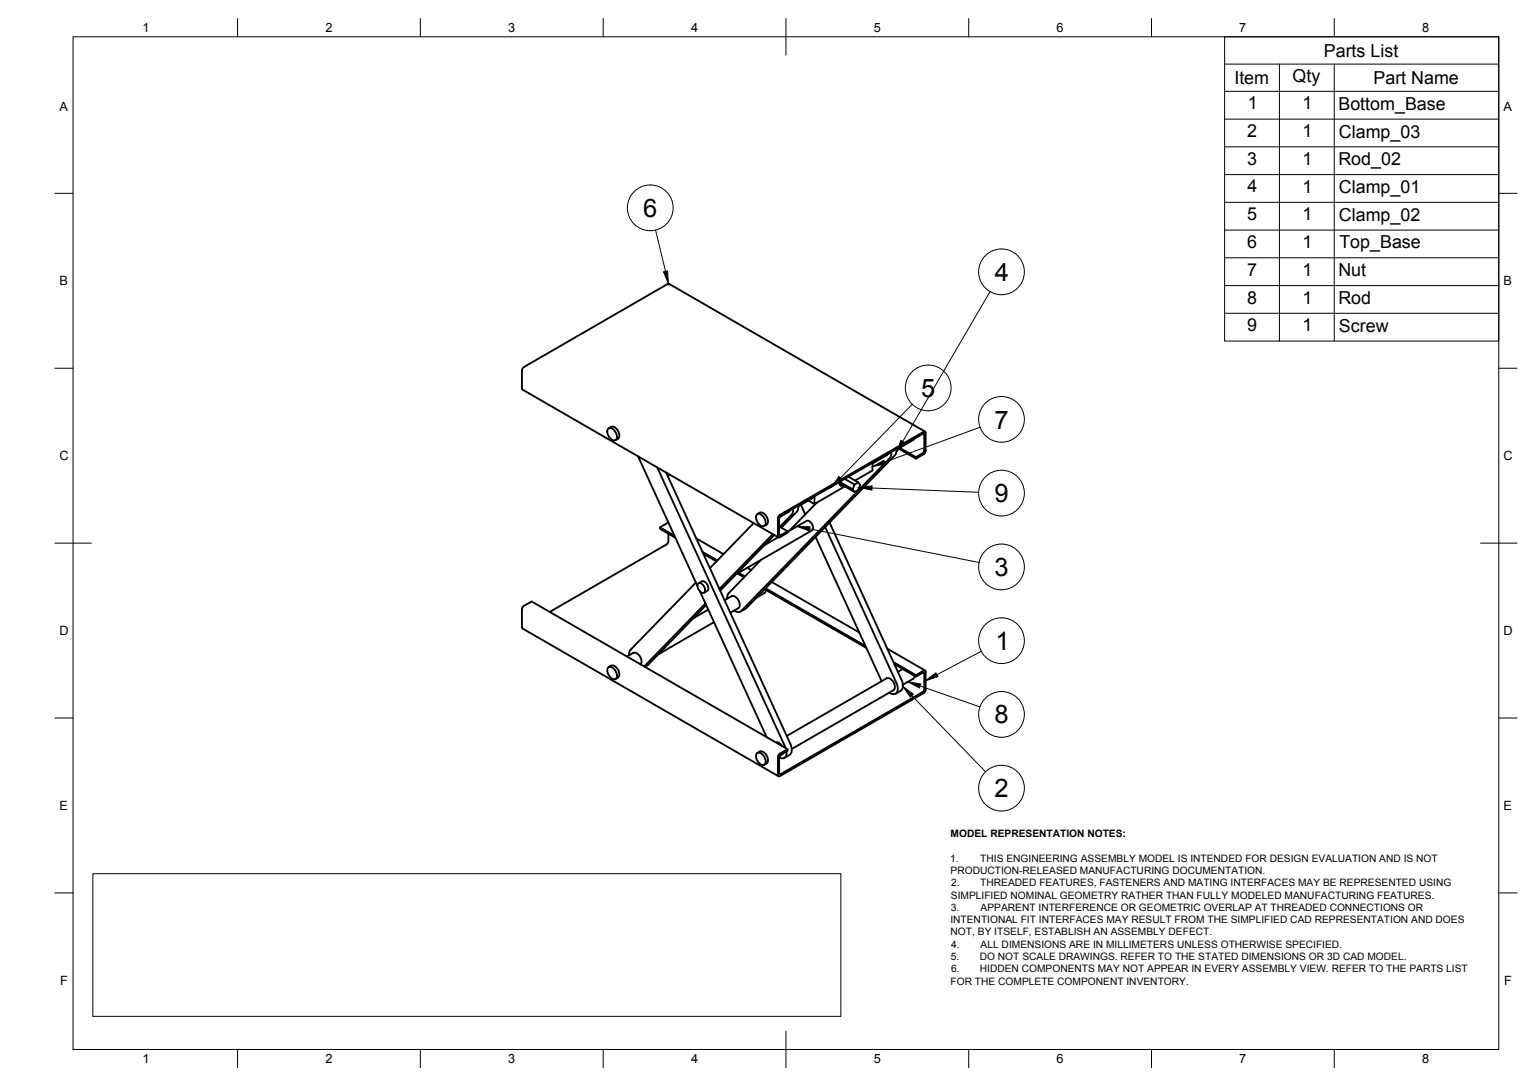
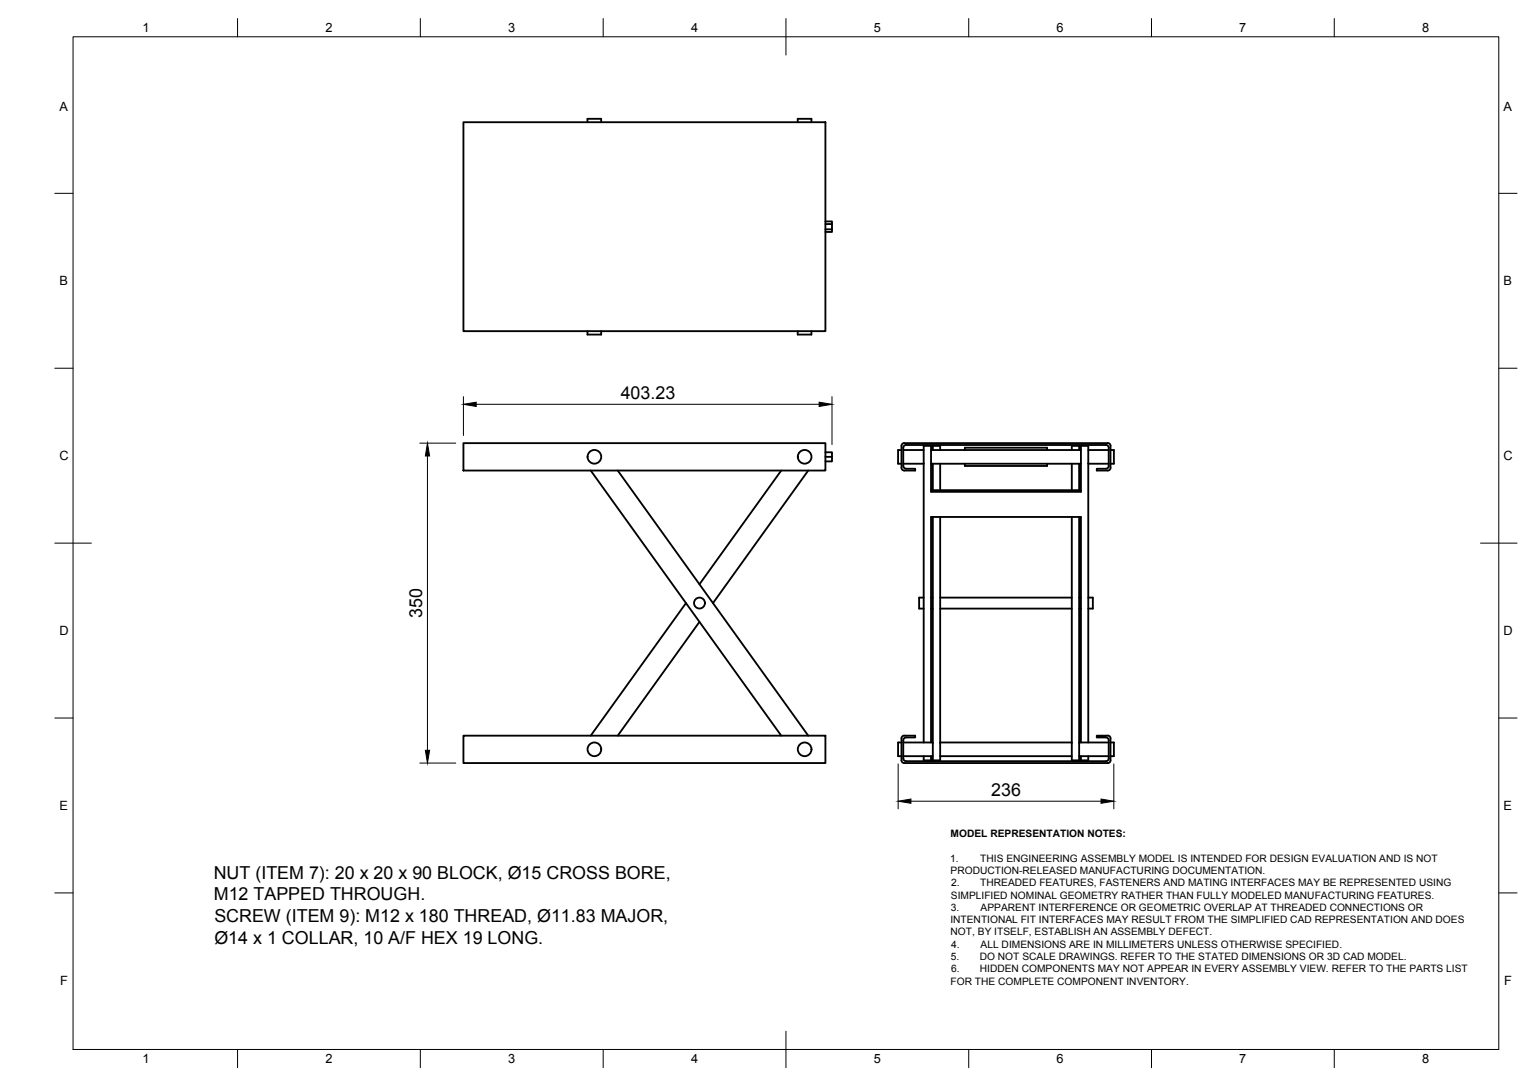
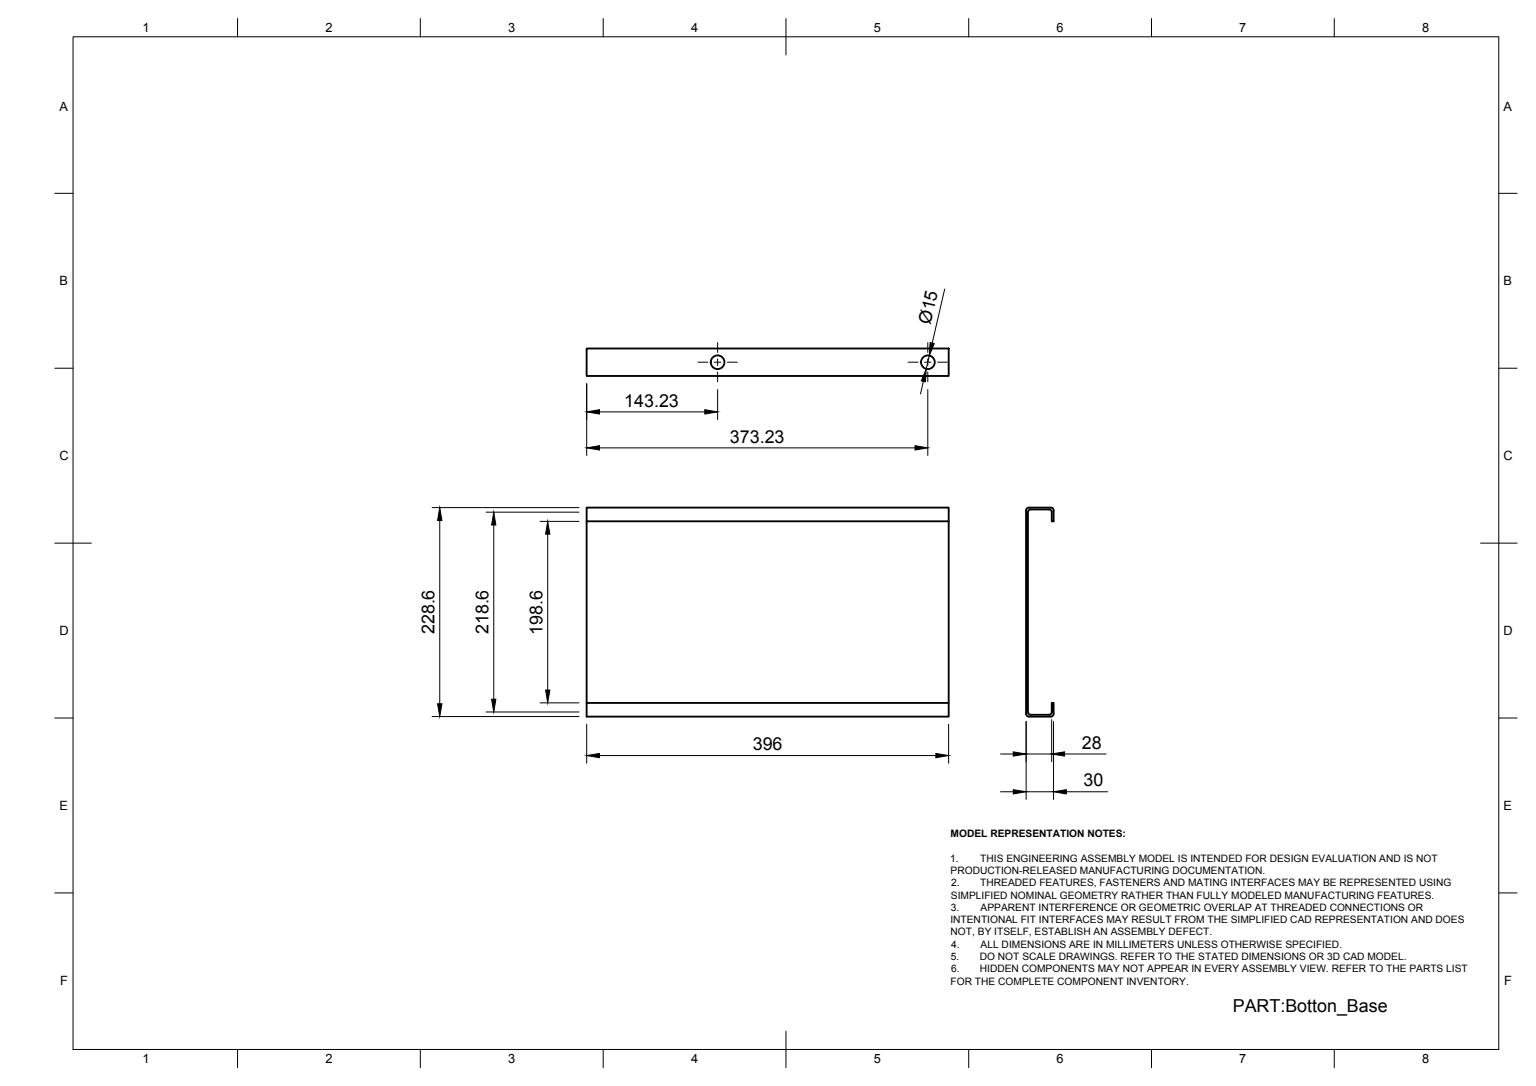
ISO-10303-21;
HEADER;
/* Generated by software containing ST-Developer
 * from STEP Tools, Inc. (www.steptools.com) 
 */

FILE_DESCRIPTION(
/* description */ (''),
/* implementation_level */ '2;1');

FILE_NAME(
/* name */ 'BR-202',
/* time_stamp */ '2026-10-05T15:35:09-07:00',
/* author */ (''),
/* organization */ (''),
/* preprocessor_version */ 'ST-DEVELOPER v20.2',
/* originating_system */ 'Autodesk Translation Framework v15.15.0.0',
/* authorisation */ '');

FILE_SCHEMA (('AUTOMOTIVE_DESIGN { 1 0 10303 214 3 1 1 }'));
ENDSEC;

DATA;
#10=MECHANICAL_DESIGN_GEOMETRIC_PRESENTATION_REPRESENTATION('',(#543,#544,
#545,#546,#547,#548,#549,#550,#551),#74523);
#11=ITEM_DEFINED_TRANSFORMATION($,$,#4832,#5089);
#12=ITEM_DEFINED_TRANSFORMATION($,$,#4883,#5090);
#13=ITEM_DEFINED_TRANSFORMATION($,$,#4929,#5091);
#14=ITEM_DEFINED_TRANSFORMATION($,$,#4935,#5092);
#15=ITEM_DEFINED_TRANSFORMATION($,$,#4960,#5093);
#16=ITEM_DEFINED_TRANSFORMATION($,$,#4986,#5094);
#17=ITEM_DEFINED_TRANSFORMATION($,$,#5037,#5095);
#18=ITEM_DEFINED_TRANSFORMATION($,$,#5063,#5096);
#19=ITEM_DEFINED_TRANSFORMATION($,$,#5069,#5097);
#20=(
REPRESENTATION_RELATIONSHIP($,$,#74558,#74557)
REPRESENTATION_RELATIONSHIP_WITH_TRANSFORMATION(#11)
SHAPE_REPRESENTATION_RELATIONSHIP()
);
#21=(
REPRESENTATION_RELATIONSHIP($,$,#74559,#74557)
REPRESENTATION_RELATIONSHIP_WITH_TRANSFORMATION(#12)
SHAPE_REPRESENTATION_RELATIONSHIP()
);
#22=(
REPRESENTATION_RELATIONSHIP($,$,#74560,#74557)
REPRESENTATION_RELATIONSHIP_WITH_TRANSFORMATION(#13)
SHAPE_REPRESENTATION_RELATIONSHIP()
);
#23=(
REPRESENTATION_RELATIONSHIP($,$,#74561,#74557)
REPRESENTATION_RELATIONSHIP_WITH_TRANSFORMATION(#14)
SHAPE_REPRESENTATION_RELATIONSHIP()
);
#24=(
REPRESENTATION_RELATIONSHIP($,$,#74562,#74557)
REPRESENTATION_RELATIONSHIP_WITH_TRANSFORMATION(#15)
SHAPE_REPRESENTATION_RELATIONSHIP()
);
#25=(
REPRESENTATION_RELATIONSHIP($,$,#74563,#74557)
REPRESENTATION_RELATIONSHIP_WITH_TRANSFORMATION(#16)
SHAPE_REPRESENTATION_RELATIONSHIP()
);
#26=(
REPRESENTATION_RELATIONSHIP($,$,#74564,#74557)
REPRESENTATION_RELATIONSHIP_WITH_TRANSFORMATION(#17)
SHAPE_REPRESENTATION_RELATIONSHIP()
);
#27=(
REPRESENTATION_RELATIONSHIP($,$,#74565,#74557)
REPRESENTATION_RELATIONSHIP_WITH_TRANSFORMATION(#18)
SHAPE_REPRESENTATION_RELATIONSHIP()
);
#28=(
REPRESENTATION_RELATIONSHIP($,$,#74566,#74557)
REPRESENTATION_RELATIONSHIP_WITH_TRANSFORMATION(#19)
SHAPE_REPRESENTATION_RELATIONSHIP()
);
#29=CONTEXT_DEPENDENT_SHAPE_REPRESENTATION(#20,#74548);
#30=CONTEXT_DEPENDENT_SHAPE_REPRESENTATION(#21,#74549);
#31=CONTEXT_DEPENDENT_SHAPE_REPRESENTATION(#22,#74550);
#32=CONTEXT_DEPENDENT_SHAPE_REPRESENTATION(#23,#74551);
#33=CONTEXT_DEPENDENT_SHAPE_REPRESENTATION(#24,#74552);
#34=CONTEXT_DEPENDENT_SHAPE_REPRESENTATION(#25,#74553);
#35=CONTEXT_DEPENDENT_SHAPE_REPRESENTATION(#26,#74554);
#36=CONTEXT_DEPENDENT_SHAPE_REPRESENTATION(#27,#74555);
#37=CONTEXT_DEPENDENT_SHAPE_REPRESENTATION(#28,#74556);
#38=NEXT_ASSEMBLY_USAGE_OCCURRENCE('Bottom_Base:1','Bottom_Base:1',
'Bottom_Base:1',#74568,#74569,'Bottom_Base:1');
#39=NEXT_ASSEMBLY_USAGE_OCCURRENCE('Clamp_03:1','Clamp_03:1',
'Clamp_03:1',#74568,#74570,'Clamp_03:1');
#40=NEXT_ASSEMBLY_USAGE_OCCURRENCE('Rod_02:1','Rod_02:1','Rod_02:1',#74568,
#74571,'Rod_02:1');
#41=NEXT_ASSEMBLY_USAGE_OCCURRENCE('Clamp_01:1','Clamp_01:1',
'Clamp_01:1',#74568,#74572,'Clamp_01:1');
#42=NEXT_ASSEMBLY_USAGE_OCCURRENCE('Clamp_02:1','Clamp_02:1',
'Clamp_02:1',#74568,#74573,'Clamp_02:1');
#43=NEXT_ASSEMBLY_USAGE_OCCURRENCE('Top_Base:1','Top_Base:1',
'Top_Base:1',#74568,#74574,'Top_Base:1');
#44=NEXT_ASSEMBLY_USAGE_OCCURRENCE('Nut:1','Nut:1','Nut:1',#74568,#74575,
'Nut:1');
#45=NEXT_ASSEMBLY_USAGE_OCCURRENCE('Rod:1','Rod:1','Rod:1',#74568,#74576,
'Rod:1');
#46=NEXT_ASSEMBLY_USAGE_OCCURRENCE('Screw:1','Screw:1','Screw:1',#74568,
#74577,'Screw:1');
#47=ELLIPSE('',#5049,4.99855036794194,3.19830998796427);
#48=B_SPLINE_SURFACE_WITH_KNOTS('',3,3,((#6899,#6900,#6901,#6902,#6903,
#6904,#6905,#6906,#6907,#6908,#6909,#6910,#6911,#6912,#6913,#6914,#6915,
#6916,#6917,#6918,#6919,#6920,#6921,#6922,#6923,#6924,#6925,#6926,#6927,
#6928,#6929),(#6930,#6931,#6932,#6933,#6934,#6935,#6936,#6937,#6938,#6939,
#6940,#6941,#6942,#6943,#6944,#6945,#6946,#6947,#6948,#6949,#6950,#6951,
#6952,#6953,#6954,#6955,#6956,#6957,#6958,#6959,#6960),(#6961,#6962,#6963,
#6964,#6965,#6966,#6967,#6968,#6969,#6970,#6971,#6972,#6973,#6974,#6975,
#6976,#6977,#6978,#6979,#6980,#6981,#6982,#6983,#6984,#6985,#6986,#6987,
#6988,#6989,#6990,#6991),(#6992,#6993,#6994,#6995,#6996,#6997,#6998,#6999,
#7000,#7001,#7002,#7003,#7004,#7005,#7006,#7007,#7008,#7009,#7010,#7011,
#7012,#7013,#7014,#7015,#7016,#7017,#7018,#7019,#7020,#7021,#7022)),
 .UNSPECIFIED.,.F.,.F.,.F.,(4,4),(4,1,1,1,1,1,1,1,1,1,1,1,1,1,1,1,1,1,1,
1,1,1,1,1,1,1,1,1,4),(-4.22102652940044E-5,0.112813165026554),(14.3984001269721,
14.8716759259636,15.344951724955,15.8182275239465,16.2915033229379,16.7647791219294,
17.2380549209208,17.7113307199123,18.1846065189038,18.6578823178952,19.1311581168867,
19.6044339158781,20.0777097148696,20.5509855138611,21.0242613128525,21.497537111844,
21.9708129108354,22.4440887098269,22.9173645088184,23.3906403078098,23.8639161068013,
24.3371919057927,24.8104677047842,25.2837435037757,25.7570193027671,26.2302951017586,
26.70357090075,27.1768466997415,27.6501791561868),.UNSPECIFIED.);
#49=B_SPLINE_SURFACE_WITH_KNOTS('',3,3,((#7342,#7343,#7344,#7345,#7346,
#7347,#7348,#7349,#7350,#7351,#7352,#7353,#7354,#7355,#7356,#7357,#7358,
#7359,#7360,#7361,#7362,#7363,#7364,#7365,#7366,#7367,#7368,#7369,#7370),
(#7371,#7372,#7373,#7374,#7375,#7376,#7377,#7378,#7379,#7380,#7381,#7382,
#7383,#7384,#7385,#7386,#7387,#7388,#7389,#7390,#7391,#7392,#7393,#7394,
#7395,#7396,#7397,#7398,#7399),(#7400,#7401,#7402,#7403,#7404,#7405,#7406,
#7407,#7408,#7409,#7410,#7411,#7412,#7413,#7414,#7415,#7416,#7417,#7418,
#7419,#7420,#7421,#7422,#7423,#7424,#7425,#7426,#7427,#7428),(#7429,#7430,
#7431,#7432,#7433,#7434,#7435,#7436,#7437,#7438,#7439,#7440,#7441,#7442,
#7443,#7444,#7445,#7446,#7447,#7448,#7449,#7450,#7451,#7452,#7453,#7454,
#7455,#7456,#7457)),.UNSPECIFIED.,.F.,.F.,.F.,(4,4),(4,1,1,1,1,1,1,1,1,
1,1,1,1,1,1,1,1,1,1,1,1,1,1,1,1,1,4),(-6.68859175462372E-5,0.112808473639489),
(11.8516667789337,12.3448673159975,12.8380009671439,13.3311346182902,13.8242682694366,
14.3174019205829,14.8105355717293,15.3036692228756,15.796802874022,16.2899365251684,
16.7830701763147,17.2762038274611,17.7693374786074,18.2624711297538,18.7556047809001,
19.2487384320465,19.7418720831929,20.2350057343392,20.7281393854856,21.2212730366319,
21.7144066877783,22.2075403389246,22.700673990071,23.1938076412174,23.6869412923637,
24.1800749435101,24.6732085946564),.UNSPECIFIED.);
#50=B_SPLINE_SURFACE_WITH_KNOTS('',3,3,((#7678,#7679,#7680,#7681,#7682,
#7683,#7684),(#7685,#7686,#7687,#7688,#7689,#7690,#7691),(#7692,#7693,#7694,
#7695,#7696,#7697,#7698),(#7699,#7700,#7701,#7702,#7703,#7704,#7705)),
 .UNSPECIFIED.,.F.,.F.,.F.,(4,4),(4,1,1,1,4),(-3.56765467420186E-5,0.112774496143046),
(25.715772779332,26.1650876565626,26.614384545223,27.0636814338833,27.512996311114),
 .UNSPECIFIED.);
#51=B_SPLINE_SURFACE_WITH_KNOTS('',3,3,((#7757,#7758,#7759,#7760,#7761),
(#7762,#7763,#7764,#7765,#7766),(#7767,#7768,#7769,#7770,#7771),(#7772,
#7773,#7774,#7775,#7776)),.UNSPECIFIED.,.F.,.F.,.F.,(4,4),(4,1,4),(0.0695195007674178,
0.112756507572734),(29.185865369981,29.6029901263762,30.1591564682366),
 .UNSPECIFIED.);
#52=B_SPLINE_SURFACE_WITH_KNOTS('',3,3,((#7783,#7784,#7785,#7786,#7787),
(#7788,#7789,#7790,#7791,#7792),(#7793,#7794,#7795,#7796,#7797),(#7798,
#7799,#7800,#7801,#7802)),.UNSPECIFIED.,.F.,.F.,.F.,(4,4),(4,1,4),(0.,0.113001416241296),
(29.1062173671441,29.7730867005616,30.4397111253108),.UNSPECIFIED.);
#53=B_SPLINE_SURFACE_WITH_KNOTS('',3,3,((#69048,#69049,#69050,#69051,#69052,
#69053,#69054,#69055,#69056,#69057,#69058,#69059,#69060,#69061,#69062,#69063,
#69064,#69065,#69066,#69067,#69068,#69069,#69070,#69071,#69072,#69073,#69074,
#69075,#69076,#69077,#69078,#69079,#69080,#69081,#69082,#69083,#69084,#69085,
#69086,#69087,#69088,#69089,#69090,#69091,#69092,#69093,#69094,#69095,#69096,
#69097,#69098,#69099,#69100,#69101,#69102,#69103,#69104,#69105,#69106,#69107,
#69108,#69109,#69110,#69111,#69112,#69113,#69114,#69115,#69116,#69117,#69118,
#69119,#69120,#69121,#69122,#69123,#69124,#69125,#69126,#69127,#69128,#69129,
#69130,#69131,#69132,#69133,#69134,#69135,#69136,#69137,#69138,#69139,#69140,
#69141,#69142,#69143,#69144,#69145,#69146,#69147,#69148,#69149,#69150,#69151,
#69152,#69153,#69154,#69155,#69156,#69157,#69158,#69159,#69160,#69161,#69162,
#69163,#69164,#69165,#69166,#69167,#69168,#69169,#69170,#69171,#69172,#69173,
#69174,#69175,#69176,#69177,#69178,#69179,#69180,#69181,#69182,#69183,#69184,
#69185,#69186,#69187,#69188,#69189,#69190,#69191,#69192,#69193,#69194,#69195,
#69196,#69197,#69198,#69199,#69200,#69201,#69202,#69203,#69204,#69205,#69206,
#69207,#69208,#69209,#69210,#69211,#69212,#69213,#69214,#69215,#69216,#69217,
#69218,#69219,#69220,#69221,#69222,#69223,#69224,#69225,#69226,#69227,#69228,
#69229,#69230,#69231,#69232,#69233,#69234,#69235,#69236,#69237,#69238,#69239,
#69240,#69241,#69242,#69243,#69244,#69245,#69246,#69247,#69248,#69249,#69250,
#69251,#69252,#69253,#69254,#69255,#69256,#69257,#69258,#69259,#69260,#69261,
#69262,#69263,#69264,#69265,#69266,#69267,#69268,#69269,#69270,#69271,#69272,
#69273,#69274,#69275,#69276,#69277,#69278,#69279,#69280,#69281,#69282,#69283,
#69284,#69285,#69286,#69287,#69288,#69289,#69290,#69291,#69292,#69293,#69294,
#69295,#69296,#69297,#69298,#69299,#69300,#69301,#69302,#69303,#69304,#69305,
#69306,#69307,#69308,#69309,#69310,#69311,#69312,#69313,#69314,#69315,#69316,
#69317,#69318,#69319,#69320,#69321,#69322,#69323,#69324,#69325,#69326,#69327,
#69328,#69329,#69330,#69331,#69332,#69333,#69334,#69335,#69336,#69337,#69338,
#69339,#69340,#69341,#69342,#69343,#69344,#69345,#69346,#69347,#69348,#69349,
#69350,#69351,#69352,#69353,#69354,#69355,#69356,#69357,#69358,#69359,#69360,
#69361,#69362,#69363,#69364,#69365,#69366,#69367,#69368,#69369,#69370,#69371,
#69372,#69373,#69374,#69375,#69376,#69377,#69378,#69379,#69380,#69381,#69382,
#69383,#69384,#69385,#69386,#69387,#69388,#69389,#69390,#69391,#69392,#69393,
#69394,#69395,#69396,#69397,#69398,#69399,#69400,#69401,#69402,#69403,#69404,
#69405,#69406,#69407,#69408,#69409,#69410,#69411,#69412,#69413,#69414,#69415,
#69416,#69417,#69418,#69419,#69420,#69421,#69422,#69423,#69424,#69425,#69426,
#69427,#69428,#69429,#69430,#69431,#69432,#69433,#69434,#69435,#69436,#69437,
#69438,#69439,#69440,#69441,#69442,#69443,#69444,#69445,#69446,#69447,#69448,
#69449,#69450,#69451,#69452,#69453,#69454,#69455,#69456,#69457,#69458,#69459,
#69460,#69461,#69462,#69463,#69464,#69465,#69466,#69467,#69468,#69469,#69470,
#69471,#69472,#69473,#69474,#69475,#69476,#69477,#69478,#69479,#69480,#69481,
#69482,#69483,#69484,#69485,#69486,#69487,#69488,#69489,#69490,#69491,#69492,
#69493,#69494,#69495,#69496,#69497,#69498,#69499,#69500,#69501,#69502,#69503,
#69504,#69505,#69506,#69507,#69508,#69509,#69510,#69511,#69512,#69513,#69514,
#69515,#69516,#69517,#69518,#69519,#69520,#69521,#69522,#69523,#69524,#69525,
#69526,#69527,#69528,#69529,#69530,#69531,#69532,#69533,#69534,#69535,#69536,
#69537,#69538,#69539,#69540,#69541,#69542,#69543,#69544,#69545,#69546,#69547,
#69548,#69549,#69550,#69551,#69552,#69553,#69554,#69555,#69556,#69557,#69558,
#69559,#69560,#69561,#69562,#69563,#69564,#69565,#69566,#69567,#69568,#69569,
#69570,#69571,#69572,#69573,#69574,#69575,#69576,#69577,#69578,#69579,#69580,
#69581,#69582,#69583,#69584,#69585,#69586,#69587,#69588,#69589,#69590,#69591,
#69592,#69593,#69594,#69595,#69596,#69597,#69598,#69599,#69600,#69601,#69602,
#69603,#69604,#69605,#69606,#69607,#69608,#69609,#69610,#69611,#69612,#69613,
#69614,#69615,#69616,#69617,#69618,#69619,#69620,#69621,#69622,#69623,#69624,
#69625,#69626,#69627,#69628,#69629,#69630,#69631,#69632,#69633,#69634,#69635,
#69636,#69637,#69638,#69639,#69640,#69641,#69642,#69643,#69644,#69645,#69646,
#69647,#69648,#69649,#69650,#69651,#69652,#69653,#69654,#69655,#69656,#69657,
#69658,#69659,#69660,#69661,#69662,#69663,#69664,#69665,#69666,#69667,#69668,
#69669,#69670,#69671,#69672,#69673,#69674,#69675,#69676,#69677,#69678,#69679,
#69680,#69681,#69682,#69683,#69684,#69685,#69686,#69687,#69688,#69689,#69690,
#69691,#69692,#69693,#69694,#69695,#69696,#69697,#69698,#69699,#69700,#69701),
(#69702,#69703,#69704,#69705,#69706,#69707,#69708,#69709,#69710,#69711,
#69712,#69713,#69714,#69715,#69716,#69717,#69718,#69719,#69720,#69721,#69722,
#69723,#69724,#69725,#69726,#69727,#69728,#69729,#69730,#69731,#69732,#69733,
#69734,#69735,#69736,#69737,#69738,#69739,#69740,#69741,#69742,#69743,#69744,
#69745,#69746,#69747,#69748,#69749,#69750,#69751,#69752,#69753,#69754,#69755,
#69756,#69757,#69758,#69759,#69760,#69761,#69762,#69763,#69764,#69765,#69766,
#69767,#69768,#69769,#69770,#69771,#69772,#69773,#69774,#69775,#69776,#69777,
#69778,#69779,#69780,#69781,#69782,#69783,#69784,#69785,#69786,#69787,#69788,
#69789,#69790,#69791,#69792,#69793,#69794,#69795,#69796,#69797,#69798,#69799,
#69800,#69801,#69802,#69803,#69804,#69805,#69806,#69807,#69808,#69809,#69810,
#69811,#69812,#69813,#69814,#69815,#69816,#69817,#69818,#69819,#69820,#69821,
#69822,#69823,#69824,#69825,#69826,#69827,#69828,#69829,#69830,#69831,#69832,
#69833,#69834,#69835,#69836,#69837,#69838,#69839,#69840,#69841,#69842,#69843,
#69844,#69845,#69846,#69847,#69848,#69849,#69850,#69851,#69852,#69853,#69854,
#69855,#69856,#69857,#69858,#69859,#69860,#69861,#69862,#69863,#69864,#69865,
#69866,#69867,#69868,#69869,#69870,#69871,#69872,#69873,#69874,#69875,#69876,
#69877,#69878,#69879,#69880,#69881,#69882,#69883,#69884,#69885,#69886,#69887,
#69888,#69889,#69890,#69891,#69892,#69893,#69894,#69895,#69896,#69897,#69898,
#69899,#69900,#69901,#69902,#69903,#69904,#69905,#69906,#69907,#69908,#69909,
#69910,#69911,#69912,#69913,#69914,#69915,#69916,#69917,#69918,#69919,#69920,
#69921,#69922,#69923,#69924,#69925,#69926,#69927,#69928,#69929,#69930,#69931,
#69932,#69933,#69934,#69935,#69936,#69937,#69938,#69939,#69940,#69941,#69942,
#69943,#69944,#69945,#69946,#69947,#69948,#69949,#69950,#69951,#69952,#69953,
#69954,#69955,#69956,#69957,#69958,#69959,#69960,#69961,#69962,#69963,#69964,
#69965,#69966,#69967,#69968,#69969,#69970,#69971,#69972,#69973,#69974,#69975,
#69976,#69977,#69978,#69979,#69980,#69981,#69982,#69983,#69984,#69985,#69986,
#69987,#69988,#69989,#69990,#69991,#69992,#69993,#69994,#69995,#69996,#69997,
#69998,#69999,#70000,#70001,#70002,#70003,#70004,#70005,#70006,#70007,#70008,
#70009,#70010,#70011,#70012,#70013,#70014,#70015,#70016,#70017,#70018,#70019,
#70020,#70021,#70022,#70023,#70024,#70025,#70026,#70027,#70028,#70029,#70030,
#70031,#70032,#70033,#70034,#70035,#70036,#70037,#70038,#70039,#70040,#70041,
#70042,#70043,#70044,#70045,#70046,#70047,#70048,#70049,#70050,#70051,#70052,
#70053,#70054,#70055,#70056,#70057,#70058,#70059,#70060,#70061,#70062,#70063,
#70064,#70065,#70066,#70067,#70068,#70069,#70070,#70071,#70072,#70073,#70074,
#70075,#70076,#70077,#70078,#70079,#70080,#70081,#70082,#70083,#70084,#70085,
#70086,#70087,#70088,#70089,#70090,#70091,#70092,#70093,#70094,#70095,#70096,
#70097,#70098,#70099,#70100,#70101,#70102,#70103,#70104,#70105,#70106,#70107,
#70108,#70109,#70110,#70111,#70112,#70113,#70114,#70115,#70116,#70117,#70118,
#70119,#70120,#70121,#70122,#70123,#70124,#70125,#70126,#70127,#70128,#70129,
#70130,#70131,#70132,#70133,#70134,#70135,#70136,#70137,#70138,#70139,#70140,
#70141,#70142,#70143,#70144,#70145,#70146,#70147,#70148,#70149,#70150,#70151,
#70152,#70153,#70154,#70155,#70156,#70157,#70158,#70159,#70160,#70161,#70162,
#70163,#70164,#70165,#70166,#70167,#70168,#70169,#70170,#70171,#70172,#70173,
#70174,#70175,#70176,#70177,#70178,#70179,#70180,#70181,#70182,#70183,#70184,
#70185,#70186,#70187,#70188,#70189,#70190,#70191,#70192,#70193,#70194,#70195,
#70196,#70197,#70198,#70199,#70200,#70201,#70202,#70203,#70204,#70205,#70206,
#70207,#70208,#70209,#70210,#70211,#70212,#70213,#70214,#70215,#70216,#70217,
#70218,#70219,#70220,#70221,#70222,#70223,#70224,#70225,#70226,#70227,#70228,
#70229,#70230,#70231,#70232,#70233,#70234,#70235,#70236,#70237,#70238,#70239,
#70240,#70241,#70242,#70243,#70244,#70245,#70246,#70247,#70248,#70249,#70250,
#70251,#70252,#70253,#70254,#70255,#70256,#70257,#70258,#70259,#70260,#70261,
#70262,#70263,#70264,#70265,#70266,#70267,#70268,#70269,#70270,#70271,#70272,
#70273,#70274,#70275,#70276,#70277,#70278,#70279,#70280,#70281,#70282,#70283,
#70284,#70285,#70286,#70287,#70288,#70289,#70290,#70291,#70292,#70293,#70294,
#70295,#70296,#70297,#70298,#70299,#70300,#70301,#70302,#70303,#70304,#70305,
#70306,#70307,#70308,#70309,#70310,#70311,#70312,#70313,#70314,#70315,#70316,
#70317,#70318,#70319,#70320,#70321,#70322,#70323,#70324,#70325,#70326,#70327,
#70328,#70329,#70330,#70331,#70332,#70333,#70334,#70335,#70336,#70337,#70338,
#70339,#70340,#70341,#70342,#70343,#70344,#70345,#70346,#70347,#70348,#70349,
#70350,#70351,#70352,#70353,#70354,#70355),(#70356,#70357,#70358,#70359,
#70360,#70361,#70362,#70363,#70364,#70365,#70366,#70367,#70368,#70369,#70370,
#70371,#70372,#70373,#70374,#70375,#70376,#70377,#70378,#70379,#70380,#70381,
#70382,#70383,#70384,#70385,#70386,#70387,#70388,#70389,#70390,#70391,#70392,
#70393,#70394,#70395,#70396,#70397,#70398,#70399,#70400,#70401,#70402,#70403,
#70404,#70405,#70406,#70407,#70408,#70409,#70410,#70411,#70412,#70413,#70414,
#70415,#70416,#70417,#70418,#70419,#70420,#70421,#70422,#70423,#70424,#70425,
#70426,#70427,#70428,#70429,#70430,#70431,#70432,#70433,#70434,#70435,#70436,
#70437,#70438,#70439,#70440,#70441,#70442,#70443,#70444,#70445,#70446,#70447,
#70448,#70449,#70450,#70451,#70452,#70453,#70454,#70455,#70456,#70457,#70458,
#70459,#70460,#70461,#70462,#70463,#70464,#70465,#70466,#70467,#70468,#70469,
#70470,#70471,#70472,#70473,#70474,#70475,#70476,#70477,#70478,#70479,#70480,
#70481,#70482,#70483,#70484,#70485,#70486,#70487,#70488,#70489,#70490,#70491,
#70492,#70493,#70494,#70495,#70496,#70497,#70498,#70499,#70500,#70501,#70502,
#70503,#70504,#70505,#70506,#70507,#70508,#70509,#70510,#70511,#70512,#70513,
#70514,#70515,#70516,#70517,#70518,#70519,#70520,#70521,#70522,#70523,#70524,
#70525,#70526,#70527,#70528,#70529,#70530,#70531,#70532,#70533,#70534,#70535,
#70536,#70537,#70538,#70539,#70540,#70541,#70542,#70543,#70544,#70545,#70546,
#70547,#70548,#70549,#70550,#70551,#70552,#70553,#70554,#70555,#70556,#70557,
#70558,#70559,#70560,#70561,#70562,#70563,#70564,#70565,#70566,#70567,#70568,
#70569,#70570,#70571,#70572,#70573,#70574,#70575,#70576,#70577,#70578,#70579,
#70580,#70581,#70582,#70583,#70584,#70585,#70586,#70587,#70588,#70589,#70590,
#70591,#70592,#70593,#70594,#70595,#70596,#70597,#70598,#70599,#70600,#70601,
#70602,#70603,#70604,#70605,#70606,#70607,#70608,#70609,#70610,#70611,#70612,
#70613,#70614,#70615,#70616,#70617,#70618,#70619,#70620,#70621,#70622,#70623,
#70624,#70625,#70626,#70627,#70628,#70629,#70630,#70631,#70632,#70633,#70634,
#70635,#70636,#70637,#70638,#70639,#70640,#70641,#70642,#70643,#70644,#70645,
#70646,#70647,#70648,#70649,#70650,#70651,#70652,#70653,#70654,#70655,#70656,
#70657,#70658,#70659,#70660,#70661,#70662,#70663,#70664,#70665,#70666,#70667,
#70668,#70669,#70670,#70671,#70672,#70673,#70674,#70675,#70676,#70677,#70678,
#70679,#70680,#70681,#70682,#70683,#70684,#70685,#70686,#70687,#70688,#70689,
#70690,#70691,#70692,#70693,#70694,#70695,#70696,#70697,#70698,#70699,#70700,
#70701,#70702,#70703,#70704,#70705,#70706,#70707,#70708,#70709,#70710,#70711,
#70712,#70713,#70714,#70715,#70716,#70717,#70718,#70719,#70720,#70721,#70722,
#70723,#70724,#70725,#70726,#70727,#70728,#70729,#70730,#70731,#70732,#70733,
#70734,#70735,#70736,#70737,#70738,#70739,#70740,#70741,#70742,#70743,#70744,
#70745,#70746,#70747,#70748,#70749,#70750,#70751,#70752,#70753,#70754,#70755,
#70756,#70757,#70758,#70759,#70760,#70761,#70762,#70763,#70764,#70765,#70766,
#70767,#70768,#70769,#70770,#70771,#70772,#70773,#70774,#70775,#70776,#70777,
#70778,#70779,#70780,#70781,#70782,#70783,#70784,#70785,#70786,#70787,#70788,
#70789,#70790,#70791,#70792,#70793,#70794,#70795,#70796,#70797,#70798,#70799,
#70800,#70801,#70802,#70803,#70804,#70805,#70806,#70807,#70808,#70809,#70810,
#70811,#70812,#70813,#70814,#70815,#70816,#70817,#70818,#70819,#70820,#70821,
#70822,#70823,#70824,#70825,#70826,#70827,#70828,#70829,#70830,#70831,#70832,
#70833,#70834,#70835,#70836,#70837,#70838,#70839,#70840,#70841,#70842,#70843,
#70844,#70845,#70846,#70847,#70848,#70849,#70850,#70851,#70852,#70853,#70854,
#70855,#70856,#70857,#70858,#70859,#70860,#70861,#70862,#70863,#70864,#70865,
#70866,#70867,#70868,#70869,#70870,#70871,#70872,#70873,#70874,#70875,#70876,
#70877,#70878,#70879,#70880,#70881,#70882,#70883,#70884,#70885,#70886,#70887,
#70888,#70889,#70890,#70891,#70892,#70893,#70894,#70895,#70896,#70897,#70898,
#70899,#70900,#70901,#70902,#70903,#70904,#70905,#70906,#70907,#70908,#70909,
#70910,#70911,#70912,#70913,#70914,#70915,#70916,#70917,#70918,#70919,#70920,
#70921,#70922,#70923,#70924,#70925,#70926,#70927,#70928,#70929,#70930,#70931,
#70932,#70933,#70934,#70935,#70936,#70937,#70938,#70939,#70940,#70941,#70942,
#70943,#70944,#70945,#70946,#70947,#70948,#70949,#70950,#70951,#70952,#70953,
#70954,#70955,#70956,#70957,#70958,#70959,#70960,#70961,#70962,#70963,#70964,
#70965,#70966,#70967,#70968,#70969,#70970,#70971,#70972,#70973,#70974,#70975,
#70976,#70977,#70978,#70979,#70980,#70981,#70982,#70983,#70984,#70985,#70986,
#70987,#70988,#70989,#70990,#70991,#70992,#70993,#70994,#70995,#70996,#70997,
#70998,#70999,#71000,#71001,#71002,#71003,#71004,#71005,#71006,#71007,#71008,
#71009),(#71010,#71011,#71012,#71013,#71014,#71015,#71016,#71017,#71018,
#71019,#71020,#71021,#71022,#71023,#71024,#71025,#71026,#71027,#71028,#71029,
#71030,#71031,#71032,#71033,#71034,#71035,#71036,#71037,#71038,#71039,#71040,
#71041,#71042,#71043,#71044,#71045,#71046,#71047,#71048,#71049,#71050,#71051,
#71052,#71053,#71054,#71055,#71056,#71057,#71058,#71059,#71060,#71061,#71062,
#71063,#71064,#71065,#71066,#71067,#71068,#71069,#71070,#71071,#71072,#71073,
#71074,#71075,#71076,#71077,#71078,#71079,#71080,#71081,#71082,#71083,#71084,
#71085,#71086,#71087,#71088,#71089,#71090,#71091,#71092,#71093,#71094,#71095,
#71096,#71097,#71098,#71099,#71100,#71101,#71102,#71103,#71104,#71105,#71106,
#71107,#71108,#71109,#71110,#71111,#71112,#71113,#71114,#71115,#71116,#71117,
#71118,#71119,#71120,#71121,#71122,#71123,#71124,#71125,#71126,#71127,#71128,
#71129,#71130,#71131,#71132,#71133,#71134,#71135,#71136,#71137,#71138,#71139,
#71140,#71141,#71142,#71143,#71144,#71145,#71146,#71147,#71148,#71149,#71150,
#71151,#71152,#71153,#71154,#71155,#71156,#71157,#71158,#71159,#71160,#71161,
#71162,#71163,#71164,#71165,#71166,#71167,#71168,#71169,#71170,#71171,#71172,
#71173,#71174,#71175,#71176,#71177,#71178,#71179,#71180,#71181,#71182,#71183,
#71184,#71185,#71186,#71187,#71188,#71189,#71190,#71191,#71192,#71193,#71194,
#71195,#71196,#71197,#71198,#71199,#71200,#71201,#71202,#71203,#71204,#71205,
#71206,#71207,#71208,#71209,#71210,#71211,#71212,#71213,#71214,#71215,#71216,
#71217,#71218,#71219,#71220,#71221,#71222,#71223,#71224,#71225,#71226,#71227,
#71228,#71229,#71230,#71231,#71232,#71233,#71234,#71235,#71236,#71237,#71238,
#71239,#71240,#71241,#71242,#71243,#71244,#71245,#71246,#71247,#71248,#71249,
#71250,#71251,#71252,#71253,#71254,#71255,#71256,#71257,#71258,#71259,#71260,
#71261,#71262,#71263,#71264,#71265,#71266,#71267,#71268,#71269,#71270,#71271,
#71272,#71273,#71274,#71275,#71276,#71277,#71278,#71279,#71280,#71281,#71282,
#71283,#71284,#71285,#71286,#71287,#71288,#71289,#71290,#71291,#71292,#71293,
#71294,#71295,#71296,#71297,#71298,#71299,#71300,#71301,#71302,#71303,#71304,
#71305,#71306,#71307,#71308,#71309,#71310,#71311,#71312,#71313,#71314,#71315,
#71316,#71317,#71318,#71319,#71320,#71321,#71322,#71323,#71324,#71325,#71326,
#71327,#71328,#71329,#71330,#71331,#71332,#71333,#71334,#71335,#71336,#71337,
#71338,#71339,#71340,#71341,#71342,#71343,#71344,#71345,#71346,#71347,#71348,
#71349,#71350,#71351,#71352,#71353,#71354,#71355,#71356,#71357,#71358,#71359,
#71360,#71361,#71362,#71363,#71364,#71365,#71366,#71367,#71368,#71369,#71370,
#71371,#71372,#71373,#71374,#71375,#71376,#71377,#71378,#71379,#71380,#71381,
#71382,#71383,#71384,#71385,#71386,#71387,#71388,#71389,#71390,#71391,#71392,
#71393,#71394,#71395,#71396,#71397,#71398,#71399,#71400,#71401,#71402,#71403,
#71404,#71405,#71406,#71407,#71408,#71409,#71410,#71411,#71412,#71413,#71414,
#71415,#71416,#71417,#71418,#71419,#71420,#71421,#71422,#71423,#71424,#71425,
#71426,#71427,#71428,#71429,#71430,#71431,#71432,#71433,#71434,#71435,#71436,
#71437,#71438,#71439,#71440,#71441,#71442,#71443,#71444,#71445,#71446,#71447,
#71448,#71449,#71450,#71451,#71452,#71453,#71454,#71455,#71456,#71457,#71458,
#71459,#71460,#71461,#71462,#71463,#71464,#71465,#71466,#71467,#71468,#71469,
#71470,#71471,#71472,#71473,#71474,#71475,#71476,#71477,#71478,#71479,#71480,
#71481,#71482,#71483,#71484,#71485,#71486,#71487,#71488,#71489,#71490,#71491,
#71492,#71493,#71494,#71495,#71496,#71497,#71498,#71499,#71500,#71501,#71502,
#71503,#71504,#71505,#71506,#71507,#71508,#71509,#71510,#71511,#71512,#71513,
#71514,#71515,#71516,#71517,#71518,#71519,#71520,#71521,#71522,#71523,#71524,
#71525,#71526,#71527,#71528,#71529,#71530,#71531,#71532,#71533,#71534,#71535,
#71536,#71537,#71538,#71539,#71540,#71541,#71542,#71543,#71544,#71545,#71546,
#71547,#71548,#71549,#71550,#71551,#71552,#71553,#71554,#71555,#71556,#71557,
#71558,#71559,#71560,#71561,#71562,#71563,#71564,#71565,#71566,#71567,#71568,
#71569,#71570,#71571,#71572,#71573,#71574,#71575,#71576,#71577,#71578,#71579,
#71580,#71581,#71582,#71583,#71584,#71585,#71586,#71587,#71588,#71589,#71590,
#71591,#71592,#71593,#71594,#71595,#71596,#71597,#71598,#71599,#71600,#71601,
#71602,#71603,#71604,#71605,#71606,#71607,#71608,#71609,#71610,#71611,#71612,
#71613,#71614,#71615,#71616,#71617,#71618,#71619,#71620,#71621,#71622,#71623,
#71624,#71625,#71626,#71627,#71628,#71629,#71630,#71631,#71632,#71633,#71634,
#71635,#71636,#71637,#71638,#71639,#71640,#71641,#71642,#71643,#71644,#71645,
#71646,#71647,#71648,#71649,#71650,#71651,#71652,#71653,#71654,#71655,#71656,
#71657,#71658,#71659,#71660,#71661,#71662,#71663)),.UNSPECIFIED.,.F.,.F.,
 .F.,(4,4),(4,1,1,1,1,1,1,1,1,1,1,1,1,1,1,1,1,1,1,1,1,1,1,1,1,1,1,1,1,1,
1,1,1,1,1,1,1,1,1,1,1,1,1,1,1,1,1,1,1,1,1,1,1,1,1,1,1,1,1,1,1,1,1,1,1,1,
1,1,1,1,1,1,1,1,1,1,1,1,1,1,1,1,1,1,1,1,1,1,1,1,1,1,1,1,1,1,1,1,1,1,1,1,
1,1,1,1,1,1,1,1,1,1,1,1,1,1,1,1,1,1,1,1,1,1,1,1,1,1,1,1,1,1,1,1,1,1,1,1,
1,1,1,1,1,1,1,1,1,1,1,1,1,1,1,1,1,1,1,1,1,1,1,1,1,1,1,1,1,1,1,1,1,1,1,1,
1,1,1,1,1,1,1,1,1,1,1,1,1,1,1,1,1,1,1,1,1,1,1,1,1,1,1,1,1,1,1,1,1,1,1,1,
1,1,1,1,1,1,1,1,1,1,1,1,1,1,1,1,1,1,1,1,1,1,1,1,1,1,1,1,1,1,1,1,1,1,1,1,
1,1,1,1,1,1,1,1,1,1,1,1,1,1,1,1,1,1,1,1,1,1,1,1,1,1,1,1,1,1,1,1,1,1,1,1,
1,1,1,1,1,1,1,1,1,1,1,1,1,1,1,1,1,1,1,1,1,1,1,1,1,1,1,1,1,1,1,1,1,1,1,1,
1,1,1,1,1,1,1,1,1,1,1,1,1,1,1,1,1,1,1,1,1,1,1,1,1,1,1,1,1,1,1,1,1,1,1,1,
1,1,1,1,1,1,1,1,1,1,1,1,1,1,1,1,1,1,1,1,1,1,1,1,1,1,1,1,1,1,1,1,1,1,1,1,
1,1,1,1,1,1,1,1,1,1,1,1,1,1,1,1,1,1,1,1,1,1,1,1,1,1,1,1,1,1,1,1,1,1,1,1,
1,1,1,1,1,1,1,1,1,1,1,1,1,1,1,1,1,1,1,1,1,1,1,1,1,1,1,1,1,1,1,1,1,1,1,1,
1,1,1,1,1,1,1,1,1,1,1,1,1,1,1,1,1,1,1,1,1,1,1,1,1,1,1,1,1,1,1,1,1,1,1,1,
1,1,1,1,1,1,1,1,1,1,1,1,1,1,1,1,1,1,1,1,1,1,1,1,1,1,1,1,1,1,1,1,1,1,1,1,
1,1,1,1,1,1,1,1,1,1,1,1,1,1,1,1,1,1,1,1,1,1,1,1,1,1,1,1,1,1,1,1,1,1,1,1,
1,1,1,1,1,1,1,1,1,1,1,1,1,1,1,1,1,1,1,1,1,1,1,1,1,1,1,1,1,1,1,1,1,1,1,1,
1,1,1,1,1,1,1,1,1,1,1,1,1,1,1,1,1,1,1,1,1,1,1,1,1,1,1,1,1,1,1,1,1,1,1,1,
1,1,1,1,1,1,1,1,1,4),(-0.000582827421712283,0.115703455642263),(8.30590425142668,
8.80541461833274,9.30490636943233,10.3038898716315,11.3028733738307,12.3018568760298,
13.300840378229,14.2998238804282,15.2988073826273,16.2977908848265,17.2967743870256,
18.2957578892248,19.294741391424,20.2937248936231,21.2927083958223,22.2916918980215,
23.2906754002206,24.2896589024198,25.288642404619,26.2876259068181,27.2866094090173,
28.2855929112165,29.2845764134156,30.2835599156148,31.282543417814,32.2815269200131,
33.2805104222123,34.2794939244115,35.2784774266106,36.2774609288098,37.276444431009,
38.2754279332081,39.2744114354073,40.2733949376064,41.2723784398056,42.2713619420048,
43.2703454442039,44.2693289464031,45.2683124486023,46.2672959508014,47.2662794530006,
48.2652629551998,49.2642464573989,50.2632299595981,51.2622134617973,52.2611969639964,
53.2601804661956,54.2591639683948,55.2581474705939,56.2571309727931,57.2561144749923,
58.2550979771914,59.2540814793906,60.2530649815898,61.2520484837889,62.2510319859881,
63.2500154881873,64.2489989903864,65.2479824925856,66.2469659947847,67.2459494969839,
68.2449329991831,69.2439165013822,70.2429000035814,71.2418835057806,72.2408670079797,
73.2398505101789,74.2388340123781,75.2378175145772,76.2368010167764,77.2357845189756,
78.2347680211747,79.2337515233739,80.2327350255731,81.2317185277722,82.2307020299714,
83.2296855321705,84.2286690343697,85.2276525365689,86.226636038768,87.2256195409672,
88.2246030431664,89.2235865453655,90.2225700475647,91.2215535497639,92.220537051963,
93.2195205541622,94.2185040563614,95.2174875585605,96.2164710607597,97.2154545629589,
98.214438065158,99.2134215673572,100.212405069556,101.211388571756,102.210372073955,
103.209355576154,104.208339078353,105.207322580552,106.206306082751,107.205289584951,
108.20427308715,109.203256589349,110.202240091548,111.201223593747,112.200207095946,
113.199190598146,114.198174100345,115.197157602544,116.196141104743,117.195124606942,
118.194108109141,119.193091611341,120.19207511354,121.191058615739,122.190042117938,
123.189025620137,124.188009122336,125.186992624535,126.185976126735,127.184959628934,
128.183943131133,129.182926633332,130.181910135531,131.18089363773,132.17987713993,
133.178860642129,134.177844144328,135.176827646527,136.175811148726,137.174794650925,
138.173778153125,139.172761655324,140.171745157523,141.170728659722,142.169712161921,
143.16869566412,144.16767916632,145.166662668519,146.165646170718,147.164629672917,
148.163613175116,149.162596677315,150.161580179515,151.160563681714,152.159547183913,
153.158530686112,154.157514188311,155.15649769051,156.15548119271,157.154464694909,
158.153448197108,159.152431699307,160.151415201506,161.150398703705,162.149382205905,
163.148365708104,164.147349210303,165.146332712502,166.145316214701,167.1442997169,
168.1432832191,169.142266721299,170.141250223498,171.140233725697,172.139217227896,
173.138200730095,174.137184232295,175.136167734494,176.135151236693,177.134134738892,
178.133118241091,179.13210174329,180.13108524549,181.130068747689,182.129052249888,
183.128035752087,184.127019254286,185.126002756485,186.124986258685,187.123969760884,
188.122953263083,189.121936765282,190.120920267481,191.11990376968,192.11888727188,
193.117870774079,194.116854276278,195.115837778477,196.114821280676,197.113804782875,
198.112788285075,199.111771787274,200.110755289473,201.109738791672,202.108722293871,
203.10770579607,204.10668929827,205.105672800469,206.104656302668,207.103639804867,
208.102623307066,209.101606809265,210.100590311465,211.099573813664,212.098557315863,
213.097540818062,214.096524320261,215.09550782246,216.09449132466,217.093474826859,
218.092458329058,219.091441831257,220.090425333456,221.089408835655,222.088392337855,
223.087375840054,224.086359342253,225.085342844452,226.084326346651,227.08330984885,
228.08229335105,229.081276853249,230.080260355448,231.079243857647,232.078227359846,
233.077210862045,234.076194364245,235.075177866444,236.074161368643,237.073144870842,
238.072128373041,239.07111187524,240.070095377439,241.069078879639,242.068062381838,
243.067045884037,244.066029386236,245.065012888435,246.063996390634,247.062979892834,
248.061963395033,249.060946897232,250.059930399431,251.05891390163,252.057897403829,
253.056880906029,254.055864408228,255.054847910427,256.053831412626,257.052814914825,
258.051798417024,259.050781919224,260.049765421423,261.048748923622,262.047732425821,
263.04671592802,264.045699430219,265.044682932419,266.043666434618,267.042649936817,
268.041633439016,269.040616941215,270.039600443414,271.038583945614,272.037567447813,
273.036550950012,274.035534452211,275.03451795441,276.033501456609,277.032484958809,
278.031468461008,279.030451963207,280.029435465406,281.028418967605,282.027402469804,
283.026385972004,284.025369474203,285.024352976402,286.023336478601,287.0223199808,
288.021303482999,289.020286985199,290.019270487398,291.018253989597,292.017237491796,
293.016220993995,294.015204496194,295.014187998394,296.013171500593,297.012155002792,
298.011138504991,299.01012200719,300.009105509389,301.008089011589,302.007072513788,
303.006056015987,304.005039518186,305.004023020385,306.003006522584,307.001990024784,
308.000973526983,308.999957029182,309.998940531381,310.99792403358,311.996907535779,
312.995891037979,313.994874540178,314.993858042377,315.992841544576,316.991825046775,
317.990808548974,318.989792051174,319.988775553373,320.987759055572,321.986742557771,
322.98572605997,323.984709562169,324.983693064369,325.982676566568,326.981660068767,
327.980643570966,328.979627073165,329.978610575364,330.977594077564,331.976577579763,
332.975561081962,333.974544584161,334.97352808636,335.972511588559,336.971495090759,
337.970478592958,338.969462095157,339.968445597356,340.967429099555,341.966412601754,
342.965396103953,343.964379606153,344.963363108352,345.962346610551,346.96133011275,
347.960313614949,348.959297117148,349.958280619348,350.957264121547,351.956247623746,
352.955231125945,353.954214628144,354.953198130343,355.952181632543,356.951165134742,
357.950148636941,358.94913213914,359.948115641339,360.947099143538,361.946082645738,
362.945066147937,363.944049650136,364.943033152335,365.942016654534,366.941000156733,
367.939983658933,368.938967161132,369.937950663331,370.93693416553,371.935917667729,
372.934901169928,373.933884672128,374.932868174327,375.931851676526,376.930835178725,
377.929818680924,378.928802183123,379.927785685323,380.926769187522,381.925752689721,
382.92473619192,383.923719694119,384.922703196318,385.921686698518,386.920670200717,
387.919653702916,388.918637205115,389.917620707314,390.916604209513,391.915587711713,
392.914571213912,393.913554716111,394.91253821831,395.911521720509,396.910505222708,
397.909488724908,398.908472227107,399.907455729306,400.906439231505,401.905422733704,
402.904406235903,403.903389738103,404.902373240302,405.901356742501,406.9003402447,
407.899323746899,408.898307249098,409.897290751298,410.896274253497,411.895257755696,
412.894241257895,413.893224760094,414.892208262293,415.891191764493,416.890175266692,
417.889158768891,418.88814227109,419.887125773289,420.886109275488,421.885092777688,
422.884076279887,423.883059782086,424.882043284285,425.881026786484,426.880010288683,
427.878993790883,428.877977293082,429.876960795281,430.87594429748,431.874927799679,
432.873911301878,433.872894804078,434.871878306277,435.870861808476,436.869845310675,
437.868828812874,438.867812315073,439.866795817273,440.865779319472,441.864762821671,
442.86374632387,443.862729826069,444.861713328268,445.860696830468,446.859680332667,
447.858663834866,448.857647337065,449.856630839264,450.855614341463,451.854597843663,
452.853581345862,453.852564848061,454.85154835026,455.850531852459,456.849515354658,
457.848498856858,458.847482359057,459.846465861256,460.845449363455,461.844432865654,
462.843416367853,463.842399870052,464.841383372252,465.840366874451,466.83935037665,
467.838333878849,468.837317381048,469.836300883247,470.835284385447,471.834267887646,
472.833251389845,473.832234892044,474.831218394243,475.830201896442,476.829185398642,
477.828168900841,478.82715240304,479.826135905239,480.825119407438,481.824102909637,
482.823086411837,483.822069914036,484.821053416235,485.820036918434,486.819020420633,
487.818003922832,488.816987425032,489.815970927231,490.81495442943,491.813937931629,
492.812921433828,493.811904936027,494.810888438227,495.809871940426,496.808855442625,
497.807838944824,498.806822447023,499.805805949222,500.804789451422,501.803772953621,
502.80275645582,503.801739958019,504.800723460218,505.799706962417,506.798690464617,
507.797673966816,508.796657469015,509.795640971214,510.794624473413,511.793607975612,
512.792591477812,513.791574980011,514.79055848221,515.789541984409,516.788525486608,
517.787508988807,518.786492491007,519.785475993206,520.784459495405,521.783442997604,
522.782426499803,523.781410002002,524.780393504201,525.779377006401,526.7783605086,
527.777344010799,528.776327512998,529.775311015197,530.774294517396,531.773278019596,
532.772261521795,533.771245023994,534.770228526193,535.769212028392,536.768195530591,
537.767179032791,538.76616253499,539.765146037189,540.764129539388,541.763113041587,
542.762096543786,543.761080045986,544.760063548185,545.759047050384,546.758030552583,
547.757014054782,548.755997556981,549.754981059181,550.75396456138,551.752948063579,
552.751931565778,553.750915067977,554.749898570176,555.748882072376,556.747865574575,
557.746849076774,558.745832578973,559.744816081172,560.743799583371,561.742783085571,
562.74176658777,563.740750089969,564.739733592168,565.738717094367,566.737700596566,
567.736684098766,568.735667600965,569.734651103164,570.733634605363,571.732618107562,
572.731601609761,573.730585111961,574.72956861416,575.728552116359,576.727535618558,
577.726519120757,578.725502622956,579.724486125156,580.723469627355,581.722453129554,
582.721436631753,583.720420133952,584.719403636151,585.718387138351,586.71737064055,
587.716354142749,588.715337644948,589.714321147147,590.713304649346,591.712288151546,
592.711271653745,593.710255155944,594.709238658143,595.708222160342,596.707205662541,
597.706189164741,598.70517266694,599.704156169139,600.703139671338,601.702123173537,
602.701106675736,603.700090177936,604.699073680135,605.698057182334,606.697040684533,
607.696024186732,608.695007688931,609.693991191131,610.69297469333,611.691958195529,
612.690941697728,613.689925199927,614.688908702126,615.687892204326,616.686875706525,
617.685859208724,618.684842710923,619.683826213122,620.682809715321,621.681793217521,
622.68077671972,623.679760221919,624.678743724118,625.677727226317,626.676710728516,
627.675694230716,628.674677732915,629.673661235114,630.672644737313,631.671628239512,
632.670611741711,633.669595243911,634.66857874611,635.667562248309,636.666545750508,
637.665529252707,638.664512754906,639.663496257106,640.662479759305,641.661463261504,
642.660446763703,643.659430265902,644.658413768101,645.657397270301,646.6563807725,
647.655364274699,648.654347776898,649.653331279097,650.652314781296,651.651298283496,
652.650281785695,653.649265287894,654.648248790093,655.647232292292,656.146724043392,
656.646215794491),.UNSPECIFIED.);
#54=B_SPLINE_SURFACE_WITH_KNOTS('',3,3,((#71773,#71774,#71775,#71776,#71777,
#71778,#71779,#71780,#71781,#71782,#71783,#71784,#71785,#71786,#71787,#71788,
#71789,#71790,#71791,#71792,#71793,#71794,#71795,#71796,#71797,#71798,#71799,
#71800,#71801,#71802,#71803,#71804,#71805,#71806,#71807,#71808,#71809,#71810,
#71811,#71812,#71813,#71814,#71815,#71816,#71817,#71818,#71819,#71820,#71821,
#71822,#71823,#71824,#71825,#71826,#71827,#71828,#71829,#71830,#71831,#71832,
#71833,#71834,#71835,#71836,#71837,#71838,#71839,#71840,#71841,#71842,#71843,
#71844,#71845,#71846,#71847,#71848,#71849,#71850,#71851,#71852,#71853,#71854,
#71855,#71856,#71857,#71858,#71859,#71860,#71861,#71862,#71863,#71864,#71865,
#71866,#71867,#71868,#71869,#71870,#71871,#71872,#71873,#71874,#71875,#71876,
#71877,#71878,#71879,#71880,#71881,#71882,#71883,#71884,#71885,#71886,#71887,
#71888,#71889,#71890,#71891,#71892,#71893,#71894,#71895,#71896,#71897,#71898,
#71899,#71900,#71901,#71902,#71903,#71904,#71905,#71906,#71907,#71908,#71909,
#71910,#71911,#71912,#71913,#71914,#71915,#71916,#71917,#71918,#71919,#71920,
#71921,#71922,#71923,#71924,#71925,#71926,#71927,#71928,#71929,#71930,#71931,
#71932,#71933,#71934,#71935,#71936,#71937,#71938,#71939,#71940,#71941,#71942,
#71943,#71944,#71945,#71946,#71947,#71948,#71949,#71950,#71951,#71952,#71953,
#71954,#71955,#71956,#71957,#71958,#71959,#71960,#71961,#71962,#71963,#71964,
#71965,#71966,#71967,#71968,#71969,#71970,#71971,#71972,#71973,#71974,#71975,
#71976,#71977,#71978,#71979,#71980,#71981,#71982,#71983,#71984,#71985,#71986,
#71987,#71988,#71989,#71990,#71991,#71992,#71993,#71994,#71995,#71996,#71997,
#71998,#71999,#72000,#72001,#72002,#72003,#72004,#72005,#72006,#72007,#72008,
#72009,#72010,#72011,#72012,#72013,#72014,#72015,#72016,#72017,#72018,#72019,
#72020,#72021,#72022,#72023,#72024,#72025,#72026,#72027,#72028,#72029,#72030,
#72031,#72032,#72033,#72034,#72035,#72036,#72037,#72038,#72039,#72040,#72041,
#72042,#72043,#72044,#72045,#72046,#72047,#72048,#72049,#72050,#72051,#72052,
#72053,#72054,#72055,#72056,#72057,#72058,#72059,#72060,#72061,#72062,#72063,
#72064,#72065,#72066,#72067,#72068,#72069,#72070,#72071,#72072,#72073,#72074,
#72075,#72076,#72077,#72078,#72079,#72080,#72081,#72082,#72083,#72084,#72085,
#72086,#72087,#72088,#72089,#72090,#72091,#72092,#72093,#72094,#72095,#72096,
#72097,#72098,#72099,#72100,#72101,#72102,#72103,#72104,#72105,#72106,#72107,
#72108,#72109,#72110,#72111,#72112,#72113,#72114,#72115,#72116,#72117,#72118,
#72119,#72120,#72121,#72122,#72123,#72124,#72125,#72126,#72127,#72128,#72129,
#72130,#72131,#72132,#72133,#72134,#72135,#72136,#72137,#72138,#72139,#72140,
#72141,#72142,#72143,#72144,#72145,#72146,#72147,#72148,#72149,#72150,#72151,
#72152,#72153,#72154,#72155,#72156,#72157,#72158,#72159,#72160,#72161,#72162,
#72163,#72164,#72165,#72166,#72167,#72168,#72169,#72170,#72171,#72172,#72173,
#72174,#72175,#72176,#72177,#72178,#72179,#72180,#72181,#72182,#72183,#72184,
#72185,#72186,#72187,#72188,#72189,#72190,#72191,#72192,#72193,#72194,#72195,
#72196,#72197,#72198,#72199,#72200,#72201,#72202,#72203,#72204,#72205,#72206,
#72207,#72208,#72209,#72210,#72211,#72212,#72213,#72214,#72215,#72216,#72217,
#72218,#72219,#72220,#72221,#72222,#72223,#72224,#72225,#72226,#72227,#72228,
#72229,#72230,#72231,#72232,#72233,#72234,#72235,#72236,#72237,#72238,#72239,
#72240,#72241,#72242,#72243,#72244,#72245,#72246,#72247,#72248,#72249,#72250,
#72251,#72252,#72253,#72254,#72255,#72256,#72257,#72258,#72259,#72260,#72261,
#72262,#72263,#72264,#72265,#72266,#72267,#72268,#72269,#72270,#72271,#72272,
#72273,#72274,#72275,#72276,#72277,#72278,#72279,#72280,#72281,#72282,#72283,
#72284,#72285,#72286,#72287,#72288,#72289,#72290,#72291,#72292,#72293,#72294,
#72295,#72296,#72297,#72298,#72299,#72300,#72301,#72302,#72303,#72304,#72305,
#72306,#72307,#72308,#72309,#72310,#72311,#72312,#72313,#72314,#72315,#72316,
#72317,#72318,#72319,#72320,#72321,#72322,#72323,#72324,#72325,#72326,#72327,
#72328,#72329,#72330,#72331,#72332,#72333,#72334,#72335,#72336,#72337,#72338,
#72339,#72340,#72341,#72342,#72343,#72344,#72345,#72346,#72347,#72348,#72349,
#72350,#72351,#72352,#72353,#72354,#72355,#72356,#72357,#72358,#72359,#72360,
#72361,#72362,#72363,#72364,#72365,#72366,#72367,#72368,#72369,#72370,#72371,
#72372,#72373,#72374,#72375,#72376,#72377,#72378,#72379,#72380,#72381,#72382,
#72383,#72384,#72385,#72386,#72387,#72388,#72389,#72390,#72391,#72392,#72393,
#72394,#72395,#72396,#72397,#72398,#72399,#72400,#72401,#72402,#72403,#72404,
#72405,#72406,#72407,#72408,#72409,#72410,#72411,#72412,#72413,#72414,#72415,
#72416,#72417,#72418,#72419,#72420,#72421,#72422,#72423,#72424,#72425,#72426),
(#72427,#72428,#72429,#72430,#72431,#72432,#72433,#72434,#72435,#72436,
#72437,#72438,#72439,#72440,#72441,#72442,#72443,#72444,#72445,#72446,#72447,
#72448,#72449,#72450,#72451,#72452,#72453,#72454,#72455,#72456,#72457,#72458,
#72459,#72460,#72461,#72462,#72463,#72464,#72465,#72466,#72467,#72468,#72469,
#72470,#72471,#72472,#72473,#72474,#72475,#72476,#72477,#72478,#72479,#72480,
#72481,#72482,#72483,#72484,#72485,#72486,#72487,#72488,#72489,#72490,#72491,
#72492,#72493,#72494,#72495,#72496,#72497,#72498,#72499,#72500,#72501,#72502,
#72503,#72504,#72505,#72506,#72507,#72508,#72509,#72510,#72511,#72512,#72513,
#72514,#72515,#72516,#72517,#72518,#72519,#72520,#72521,#72522,#72523,#72524,
#72525,#72526,#72527,#72528,#72529,#72530,#72531,#72532,#72533,#72534,#72535,
#72536,#72537,#72538,#72539,#72540,#72541,#72542,#72543,#72544,#72545,#72546,
#72547,#72548,#72549,#72550,#72551,#72552,#72553,#72554,#72555,#72556,#72557,
#72558,#72559,#72560,#72561,#72562,#72563,#72564,#72565,#72566,#72567,#72568,
#72569,#72570,#72571,#72572,#72573,#72574,#72575,#72576,#72577,#72578,#72579,
#72580,#72581,#72582,#72583,#72584,#72585,#72586,#72587,#72588,#72589,#72590,
#72591,#72592,#72593,#72594,#72595,#72596,#72597,#72598,#72599,#72600,#72601,
#72602,#72603,#72604,#72605,#72606,#72607,#72608,#72609,#72610,#72611,#72612,
#72613,#72614,#72615,#72616,#72617,#72618,#72619,#72620,#72621,#72622,#72623,
#72624,#72625,#72626,#72627,#72628,#72629,#72630,#72631,#72632,#72633,#72634,
#72635,#72636,#72637,#72638,#72639,#72640,#72641,#72642,#72643,#72644,#72645,
#72646,#72647,#72648,#72649,#72650,#72651,#72652,#72653,#72654,#72655,#72656,
#72657,#72658,#72659,#72660,#72661,#72662,#72663,#72664,#72665,#72666,#72667,
#72668,#72669,#72670,#72671,#72672,#72673,#72674,#72675,#72676,#72677,#72678,
#72679,#72680,#72681,#72682,#72683,#72684,#72685,#72686,#72687,#72688,#72689,
#72690,#72691,#72692,#72693,#72694,#72695,#72696,#72697,#72698,#72699,#72700,
#72701,#72702,#72703,#72704,#72705,#72706,#72707,#72708,#72709,#72710,#72711,
#72712,#72713,#72714,#72715,#72716,#72717,#72718,#72719,#72720,#72721,#72722,
#72723,#72724,#72725,#72726,#72727,#72728,#72729,#72730,#72731,#72732,#72733,
#72734,#72735,#72736,#72737,#72738,#72739,#72740,#72741,#72742,#72743,#72744,
#72745,#72746,#72747,#72748,#72749,#72750,#72751,#72752,#72753,#72754,#72755,
#72756,#72757,#72758,#72759,#72760,#72761,#72762,#72763,#72764,#72765,#72766,
#72767,#72768,#72769,#72770,#72771,#72772,#72773,#72774,#72775,#72776,#72777,
#72778,#72779,#72780,#72781,#72782,#72783,#72784,#72785,#72786,#72787,#72788,
#72789,#72790,#72791,#72792,#72793,#72794,#72795,#72796,#72797,#72798,#72799,
#72800,#72801,#72802,#72803,#72804,#72805,#72806,#72807,#72808,#72809,#72810,
#72811,#72812,#72813,#72814,#72815,#72816,#72817,#72818,#72819,#72820,#72821,
#72822,#72823,#72824,#72825,#72826,#72827,#72828,#72829,#72830,#72831,#72832,
#72833,#72834,#72835,#72836,#72837,#72838,#72839,#72840,#72841,#72842,#72843,
#72844,#72845,#72846,#72847,#72848,#72849,#72850,#72851,#72852,#72853,#72854,
#72855,#72856,#72857,#72858,#72859,#72860,#72861,#72862,#72863,#72864,#72865,
#72866,#72867,#72868,#72869,#72870,#72871,#72872,#72873,#72874,#72875,#72876,
#72877,#72878,#72879,#72880,#72881,#72882,#72883,#72884,#72885,#72886,#72887,
#72888,#72889,#72890,#72891,#72892,#72893,#72894,#72895,#72896,#72897,#72898,
#72899,#72900,#72901,#72902,#72903,#72904,#72905,#72906,#72907,#72908,#72909,
#72910,#72911,#72912,#72913,#72914,#72915,#72916,#72917,#72918,#72919,#72920,
#72921,#72922,#72923,#72924,#72925,#72926,#72927,#72928,#72929,#72930,#72931,
#72932,#72933,#72934,#72935,#72936,#72937,#72938,#72939,#72940,#72941,#72942,
#72943,#72944,#72945,#72946,#72947,#72948,#72949,#72950,#72951,#72952,#72953,
#72954,#72955,#72956,#72957,#72958,#72959,#72960,#72961,#72962,#72963,#72964,
#72965,#72966,#72967,#72968,#72969,#72970,#72971,#72972,#72973,#72974,#72975,
#72976,#72977,#72978,#72979,#72980,#72981,#72982,#72983,#72984,#72985,#72986,
#72987,#72988,#72989,#72990,#72991,#72992,#72993,#72994,#72995,#72996,#72997,
#72998,#72999,#73000,#73001,#73002,#73003,#73004,#73005,#73006,#73007,#73008,
#73009,#73010,#73011,#73012,#73013,#73014,#73015,#73016,#73017,#73018,#73019,
#73020,#73021,#73022,#73023,#73024,#73025,#73026,#73027,#73028,#73029,#73030,
#73031,#73032,#73033,#73034,#73035,#73036,#73037,#73038,#73039,#73040,#73041,
#73042,#73043,#73044,#73045,#73046,#73047,#73048,#73049,#73050,#73051,#73052,
#73053,#73054,#73055,#73056,#73057,#73058,#73059,#73060,#73061,#73062,#73063,
#73064,#73065,#73066,#73067,#73068,#73069,#73070,#73071,#73072,#73073,#73074,
#73075,#73076,#73077,#73078,#73079,#73080),(#73081,#73082,#73083,#73084,
#73085,#73086,#73087,#73088,#73089,#73090,#73091,#73092,#73093,#73094,#73095,
#73096,#73097,#73098,#73099,#73100,#73101,#73102,#73103,#73104,#73105,#73106,
#73107,#73108,#73109,#73110,#73111,#73112,#73113,#73114,#73115,#73116,#73117,
#73118,#73119,#73120,#73121,#73122,#73123,#73124,#73125,#73126,#73127,#73128,
#73129,#73130,#73131,#73132,#73133,#73134,#73135,#73136,#73137,#73138,#73139,
#73140,#73141,#73142,#73143,#73144,#73145,#73146,#73147,#73148,#73149,#73150,
#73151,#73152,#73153,#73154,#73155,#73156,#73157,#73158,#73159,#73160,#73161,
#73162,#73163,#73164,#73165,#73166,#73167,#73168,#73169,#73170,#73171,#73172,
#73173,#73174,#73175,#73176,#73177,#73178,#73179,#73180,#73181,#73182,#73183,
#73184,#73185,#73186,#73187,#73188,#73189,#73190,#73191,#73192,#73193,#73194,
#73195,#73196,#73197,#73198,#73199,#73200,#73201,#73202,#73203,#73204,#73205,
#73206,#73207,#73208,#73209,#73210,#73211,#73212,#73213,#73214,#73215,#73216,
#73217,#73218,#73219,#73220,#73221,#73222,#73223,#73224,#73225,#73226,#73227,
#73228,#73229,#73230,#73231,#73232,#73233,#73234,#73235,#73236,#73237,#73238,
#73239,#73240,#73241,#73242,#73243,#73244,#73245,#73246,#73247,#73248,#73249,
#73250,#73251,#73252,#73253,#73254,#73255,#73256,#73257,#73258,#73259,#73260,
#73261,#73262,#73263,#73264,#73265,#73266,#73267,#73268,#73269,#73270,#73271,
#73272,#73273,#73274,#73275,#73276,#73277,#73278,#73279,#73280,#73281,#73282,
#73283,#73284,#73285,#73286,#73287,#73288,#73289,#73290,#73291,#73292,#73293,
#73294,#73295,#73296,#73297,#73298,#73299,#73300,#73301,#73302,#73303,#73304,
#73305,#73306,#73307,#73308,#73309,#73310,#73311,#73312,#73313,#73314,#73315,
#73316,#73317,#73318,#73319,#73320,#73321,#73322,#73323,#73324,#73325,#73326,
#73327,#73328,#73329,#73330,#73331,#73332,#73333,#73334,#73335,#73336,#73337,
#73338,#73339,#73340,#73341,#73342,#73343,#73344,#73345,#73346,#73347,#73348,
#73349,#73350,#73351,#73352,#73353,#73354,#73355,#73356,#73357,#73358,#73359,
#73360,#73361,#73362,#73363,#73364,#73365,#73366,#73367,#73368,#73369,#73370,
#73371,#73372,#73373,#73374,#73375,#73376,#73377,#73378,#73379,#73380,#73381,
#73382,#73383,#73384,#73385,#73386,#73387,#73388,#73389,#73390,#73391,#73392,
#73393,#73394,#73395,#73396,#73397,#73398,#73399,#73400,#73401,#73402,#73403,
#73404,#73405,#73406,#73407,#73408,#73409,#73410,#73411,#73412,#73413,#73414,
#73415,#73416,#73417,#73418,#73419,#73420,#73421,#73422,#73423,#73424,#73425,
#73426,#73427,#73428,#73429,#73430,#73431,#73432,#73433,#73434,#73435,#73436,
#73437,#73438,#73439,#73440,#73441,#73442,#73443,#73444,#73445,#73446,#73447,
#73448,#73449,#73450,#73451,#73452,#73453,#73454,#73455,#73456,#73457,#73458,
#73459,#73460,#73461,#73462,#73463,#73464,#73465,#73466,#73467,#73468,#73469,
#73470,#73471,#73472,#73473,#73474,#73475,#73476,#73477,#73478,#73479,#73480,
#73481,#73482,#73483,#73484,#73485,#73486,#73487,#73488,#73489,#73490,#73491,
#73492,#73493,#73494,#73495,#73496,#73497,#73498,#73499,#73500,#73501,#73502,
#73503,#73504,#73505,#73506,#73507,#73508,#73509,#73510,#73511,#73512,#73513,
#73514,#73515,#73516,#73517,#73518,#73519,#73520,#73521,#73522,#73523,#73524,
#73525,#73526,#73527,#73528,#73529,#73530,#73531,#73532,#73533,#73534,#73535,
#73536,#73537,#73538,#73539,#73540,#73541,#73542,#73543,#73544,#73545,#73546,
#73547,#73548,#73549,#73550,#73551,#73552,#73553,#73554,#73555,#73556,#73557,
#73558,#73559,#73560,#73561,#73562,#73563,#73564,#73565,#73566,#73567,#73568,
#73569,#73570,#73571,#73572,#73573,#73574,#73575,#73576,#73577,#73578,#73579,
#73580,#73581,#73582,#73583,#73584,#73585,#73586,#73587,#73588,#73589,#73590,
#73591,#73592,#73593,#73594,#73595,#73596,#73597,#73598,#73599,#73600,#73601,
#73602,#73603,#73604,#73605,#73606,#73607,#73608,#73609,#73610,#73611,#73612,
#73613,#73614,#73615,#73616,#73617,#73618,#73619,#73620,#73621,#73622,#73623,
#73624,#73625,#73626,#73627,#73628,#73629,#73630,#73631,#73632,#73633,#73634,
#73635,#73636,#73637,#73638,#73639,#73640,#73641,#73642,#73643,#73644,#73645,
#73646,#73647,#73648,#73649,#73650,#73651,#73652,#73653,#73654,#73655,#73656,
#73657,#73658,#73659,#73660,#73661,#73662,#73663,#73664,#73665,#73666,#73667,
#73668,#73669,#73670,#73671,#73672,#73673,#73674,#73675,#73676,#73677,#73678,
#73679,#73680,#73681,#73682,#73683,#73684,#73685,#73686,#73687,#73688,#73689,
#73690,#73691,#73692,#73693,#73694,#73695,#73696,#73697,#73698,#73699,#73700,
#73701,#73702,#73703,#73704,#73705,#73706,#73707,#73708,#73709,#73710,#73711,
#73712,#73713,#73714,#73715,#73716,#73717,#73718,#73719,#73720,#73721,#73722,
#73723,#73724,#73725,#73726,#73727,#73728,#73729,#73730,#73731,#73732,#73733,
#73734),(#73735,#73736,#73737,#73738,#73739,#73740,#73741,#73742,#73743,
#73744,#73745,#73746,#73747,#73748,#73749,#73750,#73751,#73752,#73753,#73754,
#73755,#73756,#73757,#73758,#73759,#73760,#73761,#73762,#73763,#73764,#73765,
#73766,#73767,#73768,#73769,#73770,#73771,#73772,#73773,#73774,#73775,#73776,
#73777,#73778,#73779,#73780,#73781,#73782,#73783,#73784,#73785,#73786,#73787,
#73788,#73789,#73790,#73791,#73792,#73793,#73794,#73795,#73796,#73797,#73798,
#73799,#73800,#73801,#73802,#73803,#73804,#73805,#73806,#73807,#73808,#73809,
#73810,#73811,#73812,#73813,#73814,#73815,#73816,#73817,#73818,#73819,#73820,
#73821,#73822,#73823,#73824,#73825,#73826,#73827,#73828,#73829,#73830,#73831,
#73832,#73833,#73834,#73835,#73836,#73837,#73838,#73839,#73840,#73841,#73842,
#73843,#73844,#73845,#73846,#73847,#73848,#73849,#73850,#73851,#73852,#73853,
#73854,#73855,#73856,#73857,#73858,#73859,#73860,#73861,#73862,#73863,#73864,
#73865,#73866,#73867,#73868,#73869,#73870,#73871,#73872,#73873,#73874,#73875,
#73876,#73877,#73878,#73879,#73880,#73881,#73882,#73883,#73884,#73885,#73886,
#73887,#73888,#73889,#73890,#73891,#73892,#73893,#73894,#73895,#73896,#73897,
#73898,#73899,#73900,#73901,#73902,#73903,#73904,#73905,#73906,#73907,#73908,
#73909,#73910,#73911,#73912,#73913,#73914,#73915,#73916,#73917,#73918,#73919,
#73920,#73921,#73922,#73923,#73924,#73925,#73926,#73927,#73928,#73929,#73930,
#73931,#73932,#73933,#73934,#73935,#73936,#73937,#73938,#73939,#73940,#73941,
#73942,#73943,#73944,#73945,#73946,#73947,#73948,#73949,#73950,#73951,#73952,
#73953,#73954,#73955,#73956,#73957,#73958,#73959,#73960,#73961,#73962,#73963,
#73964,#73965,#73966,#73967,#73968,#73969,#73970,#73971,#73972,#73973,#73974,
#73975,#73976,#73977,#73978,#73979,#73980,#73981,#73982,#73983,#73984,#73985,
#73986,#73987,#73988,#73989,#73990,#73991,#73992,#73993,#73994,#73995,#73996,
#73997,#73998,#73999,#74000,#74001,#74002,#74003,#74004,#74005,#74006,#74007,
#74008,#74009,#74010,#74011,#74012,#74013,#74014,#74015,#74016,#74017,#74018,
#74019,#74020,#74021,#74022,#74023,#74024,#74025,#74026,#74027,#74028,#74029,
#74030,#74031,#74032,#74033,#74034,#74035,#74036,#74037,#74038,#74039,#74040,
#74041,#74042,#74043,#74044,#74045,#74046,#74047,#74048,#74049,#74050,#74051,
#74052,#74053,#74054,#74055,#74056,#74057,#74058,#74059,#74060,#74061,#74062,
#74063,#74064,#74065,#74066,#74067,#74068,#74069,#74070,#74071,#74072,#74073,
#74074,#74075,#74076,#74077,#74078,#74079,#74080,#74081,#74082,#74083,#74084,
#74085,#74086,#74087,#74088,#74089,#74090,#74091,#74092,#74093,#74094,#74095,
#74096,#74097,#74098,#74099,#74100,#74101,#74102,#74103,#74104,#74105,#74106,
#74107,#74108,#74109,#74110,#74111,#74112,#74113,#74114,#74115,#74116,#74117,
#74118,#74119,#74120,#74121,#74122,#74123,#74124,#74125,#74126,#74127,#74128,
#74129,#74130,#74131,#74132,#74133,#74134,#74135,#74136,#74137,#74138,#74139,
#74140,#74141,#74142,#74143,#74144,#74145,#74146,#74147,#74148,#74149,#74150,
#74151,#74152,#74153,#74154,#74155,#74156,#74157,#74158,#74159,#74160,#74161,
#74162,#74163,#74164,#74165,#74166,#74167,#74168,#74169,#74170,#74171,#74172,
#74173,#74174,#74175,#74176,#74177,#74178,#74179,#74180,#74181,#74182,#74183,
#74184,#74185,#74186,#74187,#74188,#74189,#74190,#74191,#74192,#74193,#74194,
#74195,#74196,#74197,#74198,#74199,#74200,#74201,#74202,#74203,#74204,#74205,
#74206,#74207,#74208,#74209,#74210,#74211,#74212,#74213,#74214,#74215,#74216,
#74217,#74218,#74219,#74220,#74221,#74222,#74223,#74224,#74225,#74226,#74227,
#74228,#74229,#74230,#74231,#74232,#74233,#74234,#74235,#74236,#74237,#74238,
#74239,#74240,#74241,#74242,#74243,#74244,#74245,#74246,#74247,#74248,#74249,
#74250,#74251,#74252,#74253,#74254,#74255,#74256,#74257,#74258,#74259,#74260,
#74261,#74262,#74263,#74264,#74265,#74266,#74267,#74268,#74269,#74270,#74271,
#74272,#74273,#74274,#74275,#74276,#74277,#74278,#74279,#74280,#74281,#74282,
#74283,#74284,#74285,#74286,#74287,#74288,#74289,#74290,#74291,#74292,#74293,
#74294,#74295,#74296,#74297,#74298,#74299,#74300,#74301,#74302,#74303,#74304,
#74305,#74306,#74307,#74308,#74309,#74310,#74311,#74312,#74313,#74314,#74315,
#74316,#74317,#74318,#74319,#74320,#74321,#74322,#74323,#74324,#74325,#74326,
#74327,#74328,#74329,#74330,#74331,#74332,#74333,#74334,#74335,#74336,#74337,
#74338,#74339,#74340,#74341,#74342,#74343,#74344,#74345,#74346,#74347,#74348,
#74349,#74350,#74351,#74352,#74353,#74354,#74355,#74356,#74357,#74358,#74359,
#74360,#74361,#74362,#74363,#74364,#74365,#74366,#74367,#74368,#74369,#74370,
#74371,#74372,#74373,#74374,#74375,#74376,#74377,#74378,#74379,#74380,#74381,
#74382,#74383,#74384,#74385,#74386,#74387,#74388)),.UNSPECIFIED.,.F.,.F.,
 .F.,(4,4),(4,1,1,1,1,1,1,1,1,1,1,1,1,1,1,1,1,1,1,1,1,1,1,1,1,1,1,1,1,1,
1,1,1,1,1,1,1,1,1,1,1,1,1,1,1,1,1,1,1,1,1,1,1,1,1,1,1,1,1,1,1,1,1,1,1,1,
1,1,1,1,1,1,1,1,1,1,1,1,1,1,1,1,1,1,1,1,1,1,1,1,1,1,1,1,1,1,1,1,1,1,1,1,
1,1,1,1,1,1,1,1,1,1,1,1,1,1,1,1,1,1,1,1,1,1,1,1,1,1,1,1,1,1,1,1,1,1,1,1,
1,1,1,1,1,1,1,1,1,1,1,1,1,1,1,1,1,1,1,1,1,1,1,1,1,1,1,1,1,1,1,1,1,1,1,1,
1,1,1,1,1,1,1,1,1,1,1,1,1,1,1,1,1,1,1,1,1,1,1,1,1,1,1,1,1,1,1,1,1,1,1,1,
1,1,1,1,1,1,1,1,1,1,1,1,1,1,1,1,1,1,1,1,1,1,1,1,1,1,1,1,1,1,1,1,1,1,1,1,
1,1,1,1,1,1,1,1,1,1,1,1,1,1,1,1,1,1,1,1,1,1,1,1,1,1,1,1,1,1,1,1,1,1,1,1,
1,1,1,1,1,1,1,1,1,1,1,1,1,1,1,1,1,1,1,1,1,1,1,1,1,1,1,1,1,1,1,1,1,1,1,1,
1,1,1,1,1,1,1,1,1,1,1,1,1,1,1,1,1,1,1,1,1,1,1,1,1,1,1,1,1,1,1,1,1,1,1,1,
1,1,1,1,1,1,1,1,1,1,1,1,1,1,1,1,1,1,1,1,1,1,1,1,1,1,1,1,1,1,1,1,1,1,1,1,
1,1,1,1,1,1,1,1,1,1,1,1,1,1,1,1,1,1,1,1,1,1,1,1,1,1,1,1,1,1,1,1,1,1,1,1,
1,1,1,1,1,1,1,1,1,1,1,1,1,1,1,1,1,1,1,1,1,1,1,1,1,1,1,1,1,1,1,1,1,1,1,1,
1,1,1,1,1,1,1,1,1,1,1,1,1,1,1,1,1,1,1,1,1,1,1,1,1,1,1,1,1,1,1,1,1,1,1,1,
1,1,1,1,1,1,1,1,1,1,1,1,1,1,1,1,1,1,1,1,1,1,1,1,1,1,1,1,1,1,1,1,1,1,1,1,
1,1,1,1,1,1,1,1,1,1,1,1,1,1,1,1,1,1,1,1,1,1,1,1,1,1,1,1,1,1,1,1,1,1,1,1,
1,1,1,1,1,1,1,1,1,1,1,1,1,1,1,1,1,1,1,1,1,1,1,1,1,1,1,1,1,1,1,1,1,1,1,1,
1,1,1,1,1,1,1,1,1,1,1,1,1,1,1,1,1,1,1,1,1,1,1,1,1,1,1,1,1,1,1,1,1,1,1,1,
1,1,1,1,1,1,1,1,1,4),(-0.000422349804609623,0.11588507652678),(11.6153159187298,
12.114913270212,12.6144050213115,13.6133885235107,14.6123720257099,15.611355527909,
16.6103390301082,17.6093225323074,18.6083060345065,19.6072895367057,20.6062730389049,
21.605256541104,22.6042400433032,23.6032235455024,24.6022070477015,25.6011905499007,
26.6001740520998,27.599157554299,28.5981410564982,29.5971245586973,30.5961080608965,
31.5950915630957,32.5940750652948,33.593058567494,34.5920420696932,35.5910255718923,
36.5900090740915,37.5889925762907,38.5879760784898,39.586959580689,40.5859430828882,
41.5849265850873,42.5839100872865,43.5828935894856,44.5818770916848,45.580860593884,
46.5798440960831,47.5788275982823,48.5778111004815,49.5767946026806,50.5757781048798,
51.574761607079,52.5737451092781,53.5727286114773,54.5717121136765,55.5706956158756,
56.5696791180748,57.5686626202739,58.5676461224731,59.5666296246723,60.5656131268714,
61.5645966290706,62.5635801312698,63.5625636334689,64.5615471356681,65.5605306378673,
66.5595141400664,67.5584976422656,68.5574811444648,69.5564646466639,70.5554481488631,
71.5544316510623,72.5534151532614,73.5523986554606,74.5513821576597,75.5503656598589,
76.5493491620581,77.5483326642572,78.5473161664564,79.5462996686556,80.5452831708547,
81.5442666730539,82.5432501752531,83.5422336774522,84.5412171796514,85.5402006818506,
86.5391841840497,87.5381676862489,88.5371511884481,89.5361346906472,90.5351181928464,
91.5341016950455,92.5330851972447,93.5320686994439,94.531052201643,95.5300357038422,
96.5290192060414,97.5280027082405,98.5269862104397,99.5259697126389,100.524953214838,
101.523936717037,102.522920219236,103.521903721436,104.520887223635,105.519870725834,
106.518854228033,107.517837730232,108.516821232431,109.515804734631,110.51478823683,
111.513771739029,112.512755241228,113.511738743427,114.510722245626,115.509705747826,
116.508689250025,117.507672752224,118.506656254423,119.505639756622,120.504623258821,
121.50360676102,122.50259026322,123.501573765419,124.500557267618,125.499540769817,
126.498524272016,127.497507774215,128.496491276415,129.495474778614,130.494458280813,
131.493441783012,132.492425285211,133.49140878741,134.49039228961,135.489375791809,
136.488359294008,137.487342796207,138.486326298406,139.485309800605,140.484293302805,
141.483276805004,142.482260307203,143.481243809402,144.480227311601,145.4792108138,
146.478194316,147.477177818199,148.476161320398,149.475144822597,150.474128324796,
151.473111826995,152.472095329195,153.471078831394,154.470062333593,155.469045835792,
156.468029337991,157.46701284019,158.46599634239,159.464979844589,160.463963346788,
161.462946848987,162.461930351186,163.460913853385,164.459897355585,165.458880857784,
166.457864359983,167.456847862182,168.455831364381,169.45481486658,170.45379836878,
171.452781870979,172.451765373178,173.450748875377,174.449732377576,175.448715879775,
176.447699381975,177.446682884174,178.445666386373,179.444649888572,180.443633390771,
181.44261689297,182.44160039517,183.440583897369,184.439567399568,185.438550901767,
186.437534403966,187.436517906165,188.435501408365,189.434484910564,190.433468412763,
191.432451914962,192.431435417161,193.43041891936,194.429402421559,195.428385923759,
196.427369425958,197.426352928157,198.425336430356,199.424319932555,200.423303434754,
201.422286936954,202.421270439153,203.420253941352,204.419237443551,205.41822094575,
206.417204447949,207.416187950149,208.415171452348,209.414154954547,210.413138456746,
211.412121958945,212.411105461144,213.410088963344,214.409072465543,215.408055967742,
216.407039469941,217.40602297214,218.405006474339,219.403989976539,220.402973478738,
221.401956980937,222.400940483136,223.399923985335,224.398907487534,225.397890989734,
226.396874491933,227.395857994132,228.394841496331,229.39382499853,230.392808500729,
231.391792002929,232.390775505128,233.389759007327,234.388742509526,235.387726011725,
236.386709513924,237.385693016124,238.384676518323,239.383660020522,240.382643522721,
241.38162702492,242.380610527119,243.379594029319,244.378577531518,245.377561033717,
246.376544535916,247.375528038115,248.374511540314,249.373495042514,250.372478544713,
251.371462046912,252.370445549111,253.36942905131,254.368412553509,255.367396055709,
256.366379557908,257.365363060107,258.364346562306,259.363330064505,260.362313566704,
261.361297068904,262.360280571103,263.359264073302,264.358247575501,265.3572310777,
266.356214579899,267.355198082099,268.354181584298,269.353165086497,270.352148588696,
271.351132090895,272.350115593094,273.349099095293,274.348082597493,275.347066099692,
276.346049601891,277.34503310409,278.344016606289,279.343000108488,280.341983610688,
281.340967112887,282.339950615086,283.338934117285,284.337917619484,285.336901121683,
286.335884623883,287.334868126082,288.333851628281,289.33283513048,290.331818632679,
291.330802134878,292.329785637078,293.328769139277,294.327752641476,295.326736143675,
296.325719645874,297.324703148073,298.323686650273,299.322670152472,300.321653654671,
301.32063715687,302.319620659069,303.318604161268,304.317587663468,305.316571165667,
306.315554667866,307.314538170065,308.313521672264,309.312505174463,310.311488676663,
311.310472178862,312.309455681061,313.30843918326,314.307422685459,315.306406187658,
316.305389689858,317.304373192057,318.303356694256,319.302340196455,320.301323698654,
321.300307200853,322.299290703053,323.298274205252,324.297257707451,325.29624120965,
326.295224711849,327.294208214048,328.293191716248,329.292175218447,330.291158720646,
331.290142222845,332.289125725044,333.288109227243,334.287092729443,335.286076231642,
336.285059733841,337.28404323604,338.283026738239,339.282010240438,340.280993742638,
341.279977244837,342.278960747036,343.277944249235,344.276927751434,345.275911253633,
346.274894755833,347.273878258032,348.272861760231,349.27184526243,350.270828764629,
351.269812266828,352.268795769027,353.267779271227,354.266762773426,355.265746275625,
356.264729777824,357.263713280023,358.262696782222,359.261680284422,360.260663786621,
361.25964728882,362.258630791019,363.257614293218,364.256597795417,365.255581297617,
366.254564799816,367.253548302015,368.252531804214,369.251515306413,370.250498808612,
371.249482310812,372.248465813011,373.24744931521,374.246432817409,375.245416319608,
376.244399821807,377.243383324007,378.242366826206,379.241350328405,380.240333830604,
381.239317332803,382.238300835002,383.237284337202,384.236267839401,385.2352513416,
386.234234843799,387.233218345998,388.232201848197,389.231185350397,390.230168852596,
391.229152354795,392.228135856994,393.227119359193,394.226102861392,395.225086363592,
396.224069865791,397.22305336799,398.222036870189,399.221020372388,400.220003874587,
401.218987376787,402.217970878986,403.216954381185,404.215937883384,405.214921385583,
406.213904887782,407.212888389982,408.211871892181,409.21085539438,410.209838896579,
411.208822398778,412.207805900977,413.206789403177,414.205772905376,415.204756407575,
416.203739909774,417.202723411973,418.201706914172,419.200690416372,420.199673918571,
421.19865742077,422.197640922969,423.196624425168,424.195607927367,425.194591429567,
426.193574931766,427.192558433965,428.191541936164,429.190525438363,430.189508940562,
431.188492442761,432.187475944961,433.18645944716,434.185442949359,435.184426451558,
436.183409953757,437.182393455956,438.181376958156,439.180360460355,440.179343962554,
441.178327464753,442.177310966952,443.176294469151,444.175277971351,445.17426147355,
446.173244975749,447.172228477948,448.171211980147,449.170195482346,450.169178984546,
451.168162486745,452.167145988944,453.166129491143,454.165112993342,455.164096495541,
456.163079997741,457.16206349994,458.161047002139,459.160030504338,460.159014006537,
461.157997508736,462.156981010936,463.155964513135,464.154948015334,465.153931517533,
466.152915019732,467.151898521931,468.150882024131,469.14986552633,470.148849028529,
471.147832530728,472.146816032927,473.145799535126,474.144783037326,475.143766539525,
476.142750041724,477.141733543923,478.140717046122,479.139700548321,480.138684050521,
481.13766755272,482.136651054919,483.135634557118,484.134618059317,485.133601561516,
486.132585063716,487.131568565915,488.130552068114,489.129535570313,490.128519072512,
491.127502574711,492.126486076911,493.12546957911,494.124453081309,495.123436583508,
496.122420085707,497.121403587906,498.120387090106,499.119370592305,500.118354094504,
501.117337596703,502.116321098902,503.115304601101,504.114288103301,505.1132716055,
506.112255107699,507.111238609898,508.110222112097,509.109205614296,510.108189116495,
511.107172618695,512.106156120894,513.105139623093,514.104123125292,515.103106627491,
516.102090129691,517.10107363189,518.100057134089,519.099040636288,520.098024138487,
521.097007640686,522.095991142886,523.094974645085,524.093958147284,525.092941649483,
526.091925151682,527.090908653881,528.08989215608,529.08887565828,530.087859160479,
531.086842662678,532.085826164877,533.084809667076,534.083793169275,535.082776671475,
536.081760173674,537.080743675873,538.079727178072,539.078710680271,540.07769418247,
541.07667768467,542.075661186869,543.074644689068,544.073628191267,545.072611693466,
546.071595195665,547.070578697865,548.069562200064,549.068545702263,550.067529204462,
551.066512706661,552.06549620886,553.06447971106,554.063463213259,555.062446715458,
556.061430217657,557.060413719856,558.059397222055,559.058380724255,560.057364226454,
561.056347728653,562.055331230852,563.054314733051,564.05329823525,565.05228173745,
566.051265239649,567.050248741848,568.049232244047,569.048215746246,570.047199248445,
571.046182750645,572.045166252844,573.044149755043,574.043133257242,575.042116759441,
576.04110026164,577.040083763839,578.039067266039,579.038050768238,580.037034270437,
581.036017772636,582.035001274835,583.033984777034,584.032968279234,585.031951781433,
586.030935283632,587.029918785831,588.02890228803,589.027885790229,590.026869292429,
591.025852794628,592.024836296827,593.023819799026,594.022803301225,595.021786803424,
596.020770305624,597.019753807823,598.018737310022,599.017720812221,600.01670431442,
601.015687816619,602.014671318819,603.013654821018,604.012638323217,605.011621825416,
606.010605327615,607.009588829814,608.008572332014,609.007555834213,610.006539336412,
611.005522838611,612.00450634081,613.003489843009,614.002473345209,615.001456847408,
616.000440349607,616.999423851806,617.998407354005,618.997390856204,619.996374358404,
620.995357860603,621.994341362802,622.993324865001,623.9923083672,624.991291869399,
625.990275371599,626.989258873798,627.988242375997,628.987225878196,629.986209380395,
630.985192882594,631.984176384793,632.983159886993,633.982143389192,634.981126891391,
635.98011039359,636.979093895789,637.978077397988,638.977060900188,639.976044402387,
640.975027904586,641.974011406785,642.972994908984,643.971978411183,644.970961913383,
645.969945415582,646.968928917781,647.96791241998,648.966895922179,649.965879424378,
650.964862926578,651.963846428777,652.962829930976,653.961813433175,654.960796935374,
655.959780437573,656.958763939773,657.957747441972,658.956730944171,659.456222695271,
659.95571444637),.UNSPECIFIED.);
#55=B_SPLINE_CURVE_WITH_KNOTS('',3,(#6168,#6169,#6170,#6171,#6172,#6173,
#6174,#6175,#6176,#6177,#6178,#6179),.UNSPECIFIED.,.F.,.F.,(4,2,2,2,2,4),
(0.,0.123044034193907,0.246088068387815,0.492176136775629,0.730610433663304,
0.969044730550978),.UNSPECIFIED.);
#56=B_SPLINE_CURVE_WITH_KNOTS('',3,(#6180,#6181,#6182,#6183,#6184,#6185,
#6186,#6187,#6188,#6189,#6190,#6191,#6192,#6193,#6194,#6195,#6196,#6197,
#6198,#6199,#6200,#6201,#6202,#6203,#6204,#6205,#6206,#6207,#6208,#6209,
#6210,#6211),.UNSPECIFIED.,.F.,.F.,(4,2,2,2,2,2,2,2,2,2,2,2,2,2,2,4),(0.969044730550978,
1.20747902743865,1.44591332432633,1.69200139271414,1.81504542690805,1.93808946110196,
2.06113349529586,2.18417752948977,2.43026559787759,2.66869989476526,2.90713419165293,
3.14556848854061,3.38400278542828,3.6300908538161,3.75313488801,3.87617892220391),
 .UNSPECIFIED.);
#57=B_SPLINE_CURVE_WITH_KNOTS('',3,(#6215,#6216,#6217,#6218,#6219,#6220,
#6221,#6222,#6223,#6224,#6225,#6226,#6227,#6228,#6229,#6230,#6231,#6232,
#6233,#6234,#6235,#6236),.UNSPECIFIED.,.F.,.F.,(4,2,2,2,2,2,2,2,2,2,4),
(0.969044730550978,1.20747902743865,1.44591332432633,1.69200139271414,1.81504542690805,
1.93808946110196,2.06113349529586,2.18417752948977,2.43026559787759,2.66869989476526,
2.90713419165293),.UNSPECIFIED.);
#58=B_SPLINE_CURVE_WITH_KNOTS('',3,(#6238,#6239,#6240,#6241,#6242,#6243,
#6244,#6245,#6246,#6247,#6248,#6249),.UNSPECIFIED.,.F.,.F.,(4,2,2,2,2,4),
(0.,0.123044034193907,0.246088068387815,0.492176136775629,0.730610433663304,
0.969044730550978),.UNSPECIFIED.);
#59=B_SPLINE_CURVE_WITH_KNOTS('',3,(#6250,#6251,#6252,#6253,#6254,#6255,
#6256,#6257,#6258,#6259,#6260,#6261),.UNSPECIFIED.,.F.,.F.,(4,2,2,2,2,4),
(2.90713419165293,3.14556848854061,3.38400278542828,3.6300908538161,3.75313488801,
3.87617892220391),.UNSPECIFIED.);
#60=B_SPLINE_CURVE_WITH_KNOTS('',3,(#6462,#6463,#6464,#6465),
 .UNSPECIFIED.,.F.,.F.,(4,4),(24.2167824327583,24.6732085946564),
 .UNSPECIFIED.);
#61=B_SPLINE_CURVE_WITH_KNOTS('',3,(#6467,#6468,#6469,#6470,#6471,#6472),
 .UNSPECIFIED.,.F.,.F.,(4,2,4),(-0.753063156930721,-0.748287180828045,-0.713936115042439),
 .UNSPECIFIED.);
#62=B_SPLINE_CURVE_WITH_KNOTS('',3,(#6473,#6474,#6475,#6476,#6477,#6478,
#6479,#6480),.UNSPECIFIED.,.F.,.F.,(4,2,2,4),(7.54703642806723E-5,0.0982305326102068,
0.1956130339559,0.318929227615191),.UNSPECIFIED.);
#63=B_SPLINE_CURVE_WITH_KNOTS('',3,(#6486,#6487,#6488,#6489,#6490,#6491,
#6492,#6493,#6494,#6495,#6496,#6497,#6498,#6499,#6500,#6501,#6502,#6503,
#6504,#6505,#6506,#6507),.UNSPECIFIED.,.F.,.F.,(4,2,2,2,2,2,2,2,2,2,4),
(4.17196893903895,4.31793438390998,4.49439067838144,4.61169587925562,4.80346275986459,
4.92105347661489,5.03845115754435,5.15675731126169,5.34520640965897,5.44042607659759,
5.5359732292178),.UNSPECIFIED.);
#64=B_SPLINE_CURVE_WITH_KNOTS('',3,(#6509,#6510,#6511,#6512,#6513,#6514),
 .UNSPECIFIED.,.F.,.F.,(4,1,1,4),(14.3984001269721,14.8716759259636,15.344951724955,
15.707963267949),.UNSPECIFIED.);
#65=B_SPLINE_CURVE_WITH_KNOTS('',3,(#6517,#6518,#6519,#6520,#6521,#6522,
#6523,#6524,#6525,#6526,#6527,#6528,#6529,#6530,#6531,#6532,#6533,#6534,
#6535,#6536,#6537,#6538,#6539,#6540,#6541,#6542,#6543,#6544,#6545,#6546,
#6547,#6548,#6549,#6550,#6551,#6552,#6553,#6554),.UNSPECIFIED.,.F.,.F.,
(4,2,2,2,2,2,2,2,2,2,2,2,2,2,2,2,2,2,4),(8.93612119710033E-5,0.137519605080263,
0.271503523144846,0.360853537619444,0.59605291228506,0.714174537685151,
0.86920957112301,0.986431819009906,1.16462578939155,1.28180463200857,1.46548324524592,
1.58267186650919,1.82234561940174,1.9411521807847,2.05786559772135,2.17524669758369,
2.36994176720202,2.48715613899137,2.4871743415165),.UNSPECIFIED.);
#66=B_SPLINE_CURVE_WITH_KNOTS('',3,(#6560,#6561,#6562,#6563,#6564,#6565,
#6566,#6567,#6568,#6569,#6570,#6571,#6572,#6573,#6574,#6575,#6576,#6577,
#6578,#6579,#6580,#6581,#6582,#6583,#6584,#6585,#6586,#6587,#6588,#6589,
#6590,#6591,#6592,#6593,#6594,#6595,#6596,#6597),.UNSPECIFIED.,.F.,.F.,
(4,2,2,2,2,2,2,2,2,2,2,2,2,2,2,2,2,2,4),(3.44081285251957E-5,0.12033556566363,
0.23797701963383,0.316579069165278,0.52134934559798,0.620831783340204,0.72063091120251,
0.82039841485169,1.02523503080041,1.12459939419803,1.2245754078634,1.42416968131716,
1.52608431165409,1.62528028417853,1.72551932408833,1.92432671834024,2.02032569726045,
2.11939118662542,2.17146271467381),.UNSPECIFIED.);
#67=B_SPLINE_CURVE_WITH_KNOTS('',3,(#6600,#6601,#6602,#6603,#6604,#6605,
#6606,#6607,#6608,#6609,#6610,#6611,#6612,#6613,#6614,#6615,#6616,#6617,
#6618,#6619,#6620,#6621,#6622,#6623,#6624,#6625,#6626,#6627,#6628,#6629,
#6630,#6631,#6632,#6633,#6634,#6635,#6636,#6637,#6638,#6639,#6640,#6641,
#6642,#6643,#6644,#6645,#6646,#6647,#6648,#6649,#6650,#6651),
 .UNSPECIFIED.,.F.,.F.,(4,2,2,2,2,2,2,2,2,2,2,2,2,2,2,2,2,2,2,2,2,2,2,2,
2,4),(-5.78791727609175,-5.60765656906696,-5.54795034782102,-5.34916073937174,
-5.29912888856794,-5.09895513119324,-4.99903636368212,-4.90018494634977,
-4.80099712110515,-4.64008086509064,-4.54087127009457,-4.44071265045858,
-4.24069819901497,-4.13871795375788,-4.08861417004609,-3.89168204538907,
-3.8416016546448,-3.64330286264328,-3.59325472626477,-3.39352696698553,
-3.29366130100268,-3.19468247312873,-3.09545501998428,-2.89395588410736,
-2.79440271848196,-2.7332430357663),.UNSPECIFIED.);
#68=B_SPLINE_CURVE_WITH_KNOTS('',3,(#6654,#6655,#6656,#6657,#6658,#6659,
#6660,#6661,#6662,#6663,#6664,#6665,#6666,#6667,#6668,#6669,#6670,#6671,
#6672,#6673,#6674,#6675,#6676,#6677,#6678,#6679,#6680,#6681,#6682,#6683,
#6684,#6685,#6686,#6687,#6688,#6689,#6690,#6691,#6692,#6693,#6694,#6695,
#6696,#6697,#6698,#6699),.UNSPECIFIED.,.F.,.F.,(4,2,2,2,2,2,2,2,2,2,2,2,
2,2,2,2,2,2,2,2,2,2,4),(-2.7332430357663,-2.69484018883808,-2.50140826620732,
-2.45132601081293,-2.25469999769462,-2.20459657737961,-2.10261367763625,
-1.90262055882343,-1.7012130032506,-1.53229381391829,-1.43289581954836,
-1.33349729581112,-1.23385688191433,-1.03631520063649,-0.986225259842964,
-0.796325042864855,-0.746270935737797,-0.548519362328493,-0.498429295003538,
-0.308427409772446,-0.231816757097687,-0.117078636027805,-2.91462933559131E-5),
 .UNSPECIFIED.);
#69=B_SPLINE_CURVE_WITH_KNOTS('',3,(#6701,#6702,#6703,#6704,#6705,#6706),
 .UNSPECIFIED.,.F.,.F.,(4,2,4),(0.990341797688948,1.00950965231655,1.12413598826008),
 .UNSPECIFIED.);
#70=B_SPLINE_CURVE_WITH_KNOTS('',3,(#6707,#6708,#6709,#6710,#6711,#6712,
#6713,#6714,#6715,#6716,#6717,#6718,#6719,#6720,#6721,#6722,#6723,#6724,
#6725,#6726,#6727,#6728,#6729,#6730,#6731,#6732,#6733,#6734,#6735,#6736,
#6737,#6738,#6739,#6740,#6741,#6742,#6743,#6744,#6745,#6746,#6747,#6748,
#6749,#6750),.UNSPECIFIED.,.F.,.F.,(4,2,2,2,2,2,2,2,2,2,2,2,2,2,2,2,2,2,
2,2,2,4),(2.17146271467381,2.32081873718431,2.42085332522106,2.51962847719786,
2.71909167222752,2.81827420130679,2.91707565944408,3.01709099728558,3.21846106537803,
3.31753071425488,3.41512303096382,3.61371567918643,3.81514697300165,3.9170831998352,
4.11631543055948,4.21640643470696,4.3157013669682,4.52051919296804,4.72221203817467,
4.87879648597379,4.95931330752704,5.04024048342652),.UNSPECIFIED.);
#71=B_SPLINE_CURVE_WITH_KNOTS('',3,(#6753,#6754,#6755,#6756,#6757,#6758,
#6759,#6760,#6761,#6762,#6763,#6764,#6765,#6766,#6767,#6768,#6769,#6770,
#6771,#6772,#6773,#6774,#6775,#6776,#6777,#6778,#6779,#6780,#6781,#6782,
#6783,#6784,#6785,#6786),.UNSPECIFIED.,.F.,.F.,(4,2,2,2,2,2,2,2,2,2,2,2,
2,2,2,2,4),(2.4871743415165,2.7262469977791,2.84376601052792,2.96216019071238,
3.19950395965916,3.31681308535098,3.43325766283811,3.55221021297849,3.7923702493438,
3.90957368072485,4.08096889312944,4.19841225295174,4.34417466823886,4.46297946676196,
4.70267246641313,4.83714481429229,4.97526148947484),.UNSPECIFIED.);
#72=B_SPLINE_CURVE_WITH_KNOTS('',3,(#6787,#6788,#6789,#6790,#6791,#6792,
#6793,#6794,#6795),.UNSPECIFIED.,.F.,.F.,(4,1,1,1,1,1,4),(21.9911485915565,
22.2075403389246,22.700673990071,23.1938076412174,23.6869412923637,24.1800749435101,
24.2167824327583),.UNSPECIFIED.);
#73=B_SPLINE_CURVE_WITH_KNOTS('',3,(#6796,#6797,#6798,#6799,#6800,#6801,
#6802,#6803,#6804,#6805,#6806,#6807,#6808,#6809,#6810,#6811,#6812,#6813,
#6814,#6815,#6816,#6817,#6818,#6819,#6820,#6821,#6822,#6823,#6824,#6825,
#6826,#6827,#6828,#6829,#6830,#6831,#6832,#6833,#6834,#6835,#6836,#6837,
#6838,#6839,#6840,#6841,#6842,#6843,#6844,#6845,#6846,#6847,#6848,#6849),
 .UNSPECIFIED.,.F.,.F.,(4,2,2,2,2,2,2,2,2,2,2,2,2,2,2,2,2,2,2,2,2,2,2,2,
2,2,4),(0.318929227615191,0.384926038912769,0.502349680213896,0.619949001797926,
0.858373875895787,0.977114949500405,1.09371003157623,1.21105237421161,1.45123133000857,
1.57041674209182,1.69164385601961,1.80907474394577,2.04918305373556,2.29265580161209,
2.41076173271125,2.52856060749483,2.76820125234305,2.88569212998167,3.00282499176873,
3.1212892898508,3.35779947665438,3.41724850868636,3.6606559769089,3.72024554799103,
3.84139057999963,4.07822973147708,4.17196893903895),.UNSPECIFIED.);
#74=B_SPLINE_CURVE_WITH_KNOTS('',3,(#6856,#6857,#6858,#6859,#6860,#6861,
#6862,#6863,#6864,#6865,#6866,#6867,#6868,#6869,#6870,#6871,#6872,#6873,
#6874,#6875,#6876,#6877,#6878,#6879,#6880,#6881,#6882,#6883,#6884,#6885,
#6886,#6887,#6888,#6889,#6890,#6891,#6892,#6893,#6894,#6895,#6896,#6897,
#6898),.UNSPECIFIED.,.F.,.F.,(4,3,3,3,3,3,3,3,3,3,3,3,3,3,4),(-1.14369947197745,
-1.09266156206797,-1.04162734604678,-1.01275777609579,-0.99955287370654,
-0.991008573822155,-0.940790330265059,-0.890909857971607,-0.870850090088419,
-0.859711737003807,-0.8511853223161,-0.810670786438855,-0.761368249661256,
-0.712264686030117,-0.682622141321854),.UNSPECIFIED.);
#75=B_SPLINE_CURVE_WITH_KNOTS('',3,(#7024,#7025,#7026,#7027,#7028,#7029,
#7030,#7031,#7032,#7033,#7034,#7035,#7036,#7037,#7038,#7039,#7040,#7041,
#7042,#7043,#7044,#7045,#7046,#7047,#7048,#7049),.UNSPECIFIED.,.F.,.F.,
(4,2,2,2,2,2,2,2,2,2,2,2,4),(-0.514016614331628,-0.32969130617147,-0.294713516998778,
-0.279199880107329,-0.271856778418491,-0.268695348946667,-0.266392385760583,
-0.264283697040262,-0.261451067661434,-0.254187829707465,-0.238561902747748,
-0.203303015946135,-1.727286035542E-5),.UNSPECIFIED.);
#76=B_SPLINE_CURVE_WITH_KNOTS('',3,(#7051,#7052,#7053,#7054,#7055,#7056,
#7057,#7058,#7059,#7060,#7061,#7062,#7063,#7064,#7065,#7066,#7067,#7068,
#7069,#7070,#7071,#7072,#7073,#7074,#7075,#7076,#7077,#7078,#7079,#7080,
#7081,#7082,#7083,#7084,#7085,#7086,#7087,#7088,#7089,#7090,#7091,#7092,
#7093,#7094,#7095,#7096,#7097,#7098,#7099,#7100,#7101,#7102,#7103,#7104,
#7105,#7106,#7107,#7108,#7109,#7110,#7111,#7112,#7113,#7114,#7115,#7116,
#7117,#7118,#7119,#7120,#7121,#7122,#7123,#7124,#7125,#7126),
 .UNSPECIFIED.,.F.,.F.,(4,3,3,3,3,3,3,3,3,3,3,3,3,3,3,3,3,3,3,3,3,3,3,3,
3,4),(25.6488293377177,25.7363230860383,25.7570193027671,25.8403521785318,
25.9236708927411,26.006992682315,26.0903100076079,26.1736446045009,26.2302951017586,
26.3136869261066,26.397064749755,26.4804453409533,26.5638211615191,26.6472132739149,
26.70357090075,26.786786729163,26.869987834458,26.953192221565,27.0363925108091,
27.119611617046,27.1768466997415,27.2602763642278,27.3436962816524,27.4271047300443,
27.5105172922409,27.557778459707),.UNSPECIFIED.);
#77=B_SPLINE_CURVE_WITH_KNOTS('',3,(#7127,#7128,#7129,#7130,#7131,#7132),
 .UNSPECIFIED.,.F.,.F.,(4,2,4),(-0.123598918531262,-0.0618193643105504,
0.),.UNSPECIFIED.);
#78=B_SPLINE_CURVE_WITH_KNOTS('',3,(#7133,#7134,#7135,#7136,#7137,#7138,
#7139,#7140,#7141,#7142,#7143,#7144,#7145,#7146,#7147,#7148,#7149,#7150,
#7151,#7152,#7153,#7154,#7155,#7156,#7157,#7158,#7159,#7160,#7161,#7162,
#7163,#7164,#7165,#7166,#7167,#7168,#7169,#7170,#7171,#7172,#7173,#7174,
#7175,#7176,#7177,#7178,#7179,#7180,#7181,#7182,#7183,#7184,#7185,#7186,
#7187,#7188,#7189,#7190,#7191,#7192,#7193,#7194,#7195,#7196,#7197,#7198,
#7199,#7200,#7201,#7202,#7203,#7204,#7205,#7206,#7207,#7208,#7209,#7210,
#7211,#7212,#7213,#7214,#7215,#7216,#7217,#7218,#7219,#7220,#7221,#7222,
#7223,#7224,#7225,#7226,#7227,#7228,#7229,#7230,#7231,#7232,#7233,#7234,
#7235,#7236,#7237,#7238),.UNSPECIFIED.,.F.,.F.,(4,3,3,3,3,3,3,3,3,3,3,3,
3,3,3,3,3,3,3,3,3,3,3,3,3,3,3,3,3,3,3,3,3,3,3,4),(1.32259959060234E-14,
0.050745690367541,0.101728144589328,0.152317867535398,0.202221298354011,
0.223115699003081,0.233292020958922,0.239422790003241,0.28579890095029,
0.335558319036143,0.385169128031006,0.429266865985378,0.448104138024905,
0.458259185053611,0.466209278741972,0.514659008147364,0.561141261429649,
0.609757592303607,0.657860913002203,0.682148882539776,0.688028355480578,
0.735403736851129,0.782365796754906,0.825913733428173,0.873065043083829,
0.888022019180938,0.895029710778973,0.9017703672553,0.948154249761794,0.994183679961664,
1.0163582276839,1.02409536336603,1.06944623508431,1.07956252253316,1.12521097349135,
1.14790980755862),.UNSPECIFIED.);
#79=B_SPLINE_CURVE_WITH_KNOTS('',3,(#7241,#7242,#7243,#7244),
 .UNSPECIFIED.,.F.,.F.,(4,4),(-2.53462644400385,-2.50471137450691),
 .UNSPECIFIED.);
#80=B_SPLINE_CURVE_WITH_KNOTS('',3,(#7246,#7247,#7248,#7249),
 .UNSPECIFIED.,.F.,.F.,(4,4),(-1.34654518817506,-1.30462978372618),
 .UNSPECIFIED.);
#81=B_SPLINE_CURVE_WITH_KNOTS('',3,(#7250,#7251,#7252,#7253,#7254,#7255,
#7256,#7257,#7258,#7259,#7260,#7261,#7262,#7263,#7264,#7265,#7266,#7267,
#7268,#7269,#7270,#7271,#7272,#7273,#7274,#7275,#7276,#7277,#7278,#7279,
#7280,#7281,#7282,#7283,#7284,#7285,#7286,#7287,#7288,#7289,#7290,#7291,
#7292,#7293,#7294,#7295,#7296,#7297,#7298,#7299,#7300,#7301,#7302,#7303,
#7304,#7305,#7306,#7307,#7308,#7309,#7310,#7311,#7312,#7313,#7314,#7315,
#7316,#7317,#7318,#7319,#7320,#7321,#7322),.UNSPECIFIED.,.F.,.F.,(4,3,3,
3,3,3,3,3,3,3,3,3,3,3,3,3,3,3,3,3,3,3,3,3,4),(25.7157907679023,25.7998921857034,
25.8839886324584,25.9680923853322,26.0521932755846,26.1363032915209,26.1650876565626,
26.2484227066867,26.3317477086458,26.4150799956916,26.4984115627295,26.5817614677887,
26.614384545223,26.6977343289403,26.781067684511,26.8643988612109,26.9477238552507,
27.0310591851449,27.0636814338833,27.1477914052286,27.2318926685899,27.3159957185016,
27.4000927043931,27.4841941803579,27.5129783225437),.UNSPECIFIED.);
#82=B_SPLINE_CURVE_WITH_KNOTS('',3,(#7327,#7328,#7329,#7330,#7331),
 .UNSPECIFIED.,.F.,.F.,(4,1,4),(29.135142171349,29.7730867005616,30.4397111253108),
 .UNSPECIFIED.);
#83=B_SPLINE_CURVE_WITH_KNOTS('',3,(#7333,#7334,#7335,#7336),
 .UNSPECIFIED.,.F.,.F.,(4,4),(-3.54732626370964,-3.51350080410364),
 .UNSPECIFIED.);
#84=B_SPLINE_CURVE_WITH_KNOTS('',3,(#7337,#7338,#7339,#7340,#7341),
 .UNSPECIFIED.,.F.,.F.,(4,1,4),(29.185865369981,29.6029901263762,30.1591564682366),
 .UNSPECIFIED.);
#85=B_SPLINE_CURVE_WITH_KNOTS('',3,(#7459,#7460,#7461,#7462,#7463,#7464),
 .UNSPECIFIED.,.F.,.F.,(4,2,4),(-0.220733411845382,-0.110386618861819,-4.77244559407116E-5),
 .UNSPECIFIED.);
#86=B_SPLINE_CURVE_WITH_KNOTS('',3,(#7465,#7466,#7467,#7468,#7469,#7470,
#7471,#7472,#7473,#7474,#7475,#7476,#7477,#7478,#7479,#7480,#7481,#7482,
#7483,#7484,#7485,#7486,#7487,#7488,#7489,#7490,#7491,#7492,#7493,#7494,
#7495,#7496,#7497,#7498,#7499,#7500,#7501,#7502,#7503,#7504,#7505,#7506,
#7507,#7508,#7509,#7510,#7511,#7512,#7513,#7514,#7515,#7516,#7517,#7518,
#7519,#7520,#7521,#7522,#7523,#7524,#7525,#7526,#7527,#7528,#7529,#7530,
#7531,#7532,#7533,#7534,#7535,#7536,#7537,#7538,#7539,#7540,#7541,#7542,
#7543,#7544,#7545,#7546,#7547,#7548,#7549,#7550,#7551,#7552,#7553,#7554,
#7555,#7556,#7557,#7558,#7559,#7560,#7561,#7562,#7563,#7564,#7565,#7566,
#7567,#7568,#7569,#7570,#7571,#7572,#7573,#7574,#7575,#7576,#7577,#7578,
#7579),.UNSPECIFIED.,.F.,.F.,(4,3,3,3,3,3,3,3,3,3,3,3,3,3,3,3,3,3,3,3,3,
3,3,3,3,3,3,3,3,3,3,3,3,3,3,3,3,3,4),(7.86929992325189E-14,0.0451936811860495,
0.0903969215350478,0.136144750154152,0.180774724743962,0.192656156822049,
0.202437724302502,0.208102574890687,0.254797163791912,0.260907252703528,
0.307156117174411,0.353882768105037,0.400800570233627,0.407990886645808,
0.414297194758911,0.462166258294729,0.510035321830547,0.533410739071612,
0.581324090737381,0.610800619774486,0.624309700326862,0.630783725208717,
0.637288545122989,0.686044941542277,0.735263135531318,0.784542352881166,
0.81734010039149,0.836777243703415,0.85029153110938,0.857044629992751,0.907491336547556,
0.957938043102361,0.980210958730824,0.997207592144651,1.00463770128361,
1.05568876682972,1.10658093101247,1.11216107549305,1.14369466111386),
 .UNSPECIFIED.);
#87=B_SPLINE_CURVE_WITH_KNOTS('',3,(#7581,#7582,#7583,#7584,#7585,#7586,
#7587,#7588,#7589,#7590,#7591,#7592,#7593,#7594,#7595,#7596,#7597,#7598,
#7599,#7600,#7601,#7602,#7603,#7604,#7605,#7606,#7607,#7608,#7609,#7610),
 .UNSPECIFIED.,.F.,.F.,(4,2,2,2,2,2,2,2,2,2,2,2,2,2,4),(-0.515686766343526,
-0.398525158108789,-0.320476105936825,-0.276727278366829,-0.257809834269005,
-0.25033771712097,-0.246969508664653,-0.244560940095557,-0.242057971080847,
-0.238341190453125,-0.228151135260896,-0.205623012766941,-0.150948653470694,
-0.0744708908354928,0.),.UNSPECIFIED.);
#88=B_SPLINE_CURVE_WITH_KNOTS('',3,(#7611,#7612,#7613,#7614,#7615,#7616,
#7617,#7618,#7619,#7620,#7621,#7622,#7623,#7624,#7625,#7626,#7627,#7628,
#7629,#7630,#7631,#7632,#7633,#7634,#7635,#7636,#7637,#7638,#7639,#7640,
#7641,#7642,#7643,#7644,#7645,#7646,#7647,#7648,#7649,#7650,#7651,#7652,
#7653,#7654,#7655,#7656,#7657,#7658,#7659,#7660,#7661,#7662,#7663,#7664,
#7665,#7666,#7667,#7668,#7669,#7670,#7671,#7672,#7673,#7674,#7675,#7676,
#7677),.UNSPECIFIED.,.F.,.F.,(4,3,3,3,3,3,3,3,3,3,3,3,3,3,3,3,3,3,3,3,3,
3,4),(-12.4772742666219,-12.386342772875,-12.3283412786589,-12.2415409750193,
-12.1547592718571,-12.0679755292032,-11.9811970627444,-11.8943972788186,
-11.8352076275126,-11.7482147332003,-11.6612380696607,-11.5742576640307,
-11.4872820225213,-11.4002860143297,-11.3420739763662,-11.2551423602584,
-11.1682278559083,-11.0813103241984,-10.9943978098696,-10.9074647519428,
-10.8489403252199,-10.7592881888023,-10.6751012271442),.UNSPECIFIED.);
#89=B_SPLINE_CURVE_WITH_KNOTS('',3,(#7707,#7708,#7709,#7710,#7711,#7712),
 .UNSPECIFIED.,.F.,.F.,(4,2,4),(-0.270403079816102,-0.13523083141612,-1.64625206816352E-5),
 .UNSPECIFIED.);
#90=B_SPLINE_CURVE_WITH_KNOTS('',3,(#7714,#7715,#7716,#7717,#7718,#7719),
 .UNSPECIFIED.,.F.,.F.,(4,2,4),(-0.292980681038648,-0.146437065077422,0.),
 .UNSPECIFIED.);
#91=B_SPLINE_CURVE_WITH_KNOTS('',3,(#7720,#7721,#7722,#7723,#7724,#7725,
#7726,#7727,#7728,#7729,#7730,#7731,#7732,#7733,#7734,#7735,#7736,#7737,
#7738,#7739,#7740,#7741,#7742,#7743,#7744,#7745,#7746,#7747,#7748,#7749,
#7750,#7751,#7752,#7753,#7754,#7755,#7756),.UNSPECIFIED.,.F.,.F.,(4,3,3,
3,3,3,3,3,3,3,3,3,4),(-15.2154843560458,-15.2119477690322,-15.1249068169761,
-15.034342832825,-14.947305252502,-14.8602673694158,-14.7732113197559,-14.7626508803718,
-14.6757146349977,-14.5887879934978,-14.5018740211044,-14.414949455508,
-14.3463120123156),.UNSPECIFIED.);
#92=B_SPLINE_CURVE_WITH_KNOTS('',3,(#7777,#7778,#7779,#7780,#7781,#7782),
 .UNSPECIFIED.,.F.,.F.,(4,2,4),(-0.125419138950074,-0.0626178594416655,
0.),.UNSPECIFIED.);
#93=B_SPLINE_CURVE_WITH_KNOTS('',3,(#7804,#7805,#7806,#7807,#7808,#7809),
 .UNSPECIFIED.,.F.,.F.,(4,2,4),(-0.11509764486976,-0.0575516446763736,0.),
 .UNSPECIFIED.);
#94=B_SPLINE_CURVE_WITH_KNOTS('',3,(#7811,#7812,#7813,#7814,#7815,#7816,
#7817,#7818,#7819,#7820,#7821,#7822,#7823,#7824,#7825,#7826,#7827,#7828,
#7829,#7830,#7831,#7832,#7833,#7834,#7835,#7836,#7837,#7838,#7839,#7840,
#7841,#7842,#7843,#7844,#7845,#7846,#7847,#7848,#7849,#7850,#7851,#7852,
#7853,#7854,#7855,#7856,#7857,#7858,#7859),.UNSPECIFIED.,.F.,.F.,(4,3,3,
3,3,3,3,3,3,3,3,3,3,3,3,3,4),(14.7080621488406,14.7945507604512,14.8810228978745,
14.9674879490283,15.0539552968216,15.1404593843328,15.2269782020299,15.3135524038241,
15.3746865735895,15.4609099016134,15.5470903095525,15.6332384449514,15.7193649306605,
15.8054913260564,15.8916146167529,15.9777597272694,16.0055641921085),
 .UNSPECIFIED.);
#95=B_SPLINE_CURVE_WITH_KNOTS('',3,(#7860,#7861,#7862,#7863,#7864,#7865),
 .UNSPECIFIED.,.F.,.F.,(4,2,4),(-0.115233993178556,-0.0536451184811805,
0.),.UNSPECIFIED.);
#96=B_SPLINE_CURVE_WITH_KNOTS('',3,(#7872,#7873,#7874,#7875,#7876,#7877,
#7878,#7879,#7880,#7881,#7882,#7883),.UNSPECIFIED.,.F.,.F.,(4,2,2,2,2,4),
(2.90713419165293,3.14556848854061,3.38400278542828,3.6300908538161,3.75313488801,
3.87617892220391),.UNSPECIFIED.);
#97=B_SPLINE_CURVE_WITH_KNOTS('',3,(#7885,#7886,#7887,#7888,#7889,#7890,
#7891,#7892,#7893,#7894,#7895,#7896),.UNSPECIFIED.,.F.,.F.,(4,2,2,2,2,4),
(0.,0.123044034193907,0.246088068387815,0.492176136775629,0.730610433663304,
0.969044730550978),.UNSPECIFIED.);
#98=B_SPLINE_CURVE_WITH_KNOTS('',3,(#7900,#7901,#7902,#7903,#7904,#7905,
#7906,#7907,#7908,#7909,#7910,#7911,#7912,#7913,#7914,#7915,#7916,#7917,
#7918,#7919,#7920,#7921),.UNSPECIFIED.,.F.,.F.,(4,2,2,2,2,2,2,2,2,2,4),
(0.969044730550978,1.20747902743865,1.44591332432633,1.69200139271414,1.81504542690805,
1.93808946110196,2.06113349529586,2.18417752948977,2.43026559787759,2.66869989476526,
2.90713419165293),.UNSPECIFIED.);
#99=B_SPLINE_CURVE_WITH_KNOTS('',3,(#7922,#7923,#7924,#7925,#7926,#7927),
 .UNSPECIFIED.,.F.,.F.,(4,2,4),(0.381327752557984,0.406901830999469,0.5388522709963),
 .UNSPECIFIED.);
#100=B_SPLINE_CURVE_WITH_KNOTS('',3,(#7928,#7929,#7930,#7931,#7932,#7933,
#7934,#7935),.UNSPECIFIED.,.F.,.F.,(4,2,2,4),(1.43219876356662,1.61728075708837,
1.82073167258811,1.87531375049552),.UNSPECIFIED.);
#101=B_SPLINE_CURVE_WITH_KNOTS('',3,(#7936,#7937,#7938,#7939),
 .UNSPECIFIED.,.F.,.F.,(4,4),(2.83774858360888,2.94879070536832),
 .UNSPECIFIED.);
#102=B_SPLINE_CURVE_WITH_KNOTS('',3,(#7985,#7986,#7987,#7988,#7989,#7990,
#7991,#7992,#7993,#7994,#7995,#7996,#7997,#7998,#7999,#8000,#8001,#8002,
#8003,#8004,#8005,#8006,#8007,#8008,#8009,#8010,#8011,#8012,#8013,#8014,
#8015,#8016,#8017,#8018,#8019,#8020,#8021,#8022,#8023,#8024,#8025,#8026,
#8027,#8028,#8029,#8030,#8031,#8032,#8033,#8034,#8035,#8036,#8037,#8038,
#8039,#8040,#8041,#8042,#8043,#8044,#8045,#8046,#8047,#8048,#8049,#8050,
#8051,#8052,#8053,#8054,#8055,#8056,#8057,#8058,#8059,#8060,#8061,#8062,
#8063),.UNSPECIFIED.,.F.,.F.,(4,3,3,3,3,3,3,3,3,3,3,3,3,3,3,3,3,3,3,3,3,
3,3,3,3,3,4),(-4.09254174883824,-3.99593400879665,-3.91583620996095,-3.83583142168521,
-3.75590227074564,-3.67603144249985,-3.59620166787706,-3.51638411379587,
-3.43656945874385,-3.35674210619879,-3.27688645516505,-3.19694352471772,
-3.11695137442049,-3.03684665274117,-2.99695050659749,-2.91844690823361,
-2.84003781292725,-2.76170459532558,-2.68342871723619,-2.60518487891826,
-2.52695644729207,-2.44872674633489,-2.37047909991097,-2.29215102845281,
-2.21378107360774,-2.13529261516942,-2.07059485109299),.UNSPECIFIED.);
#103=B_SPLINE_CURVE_WITH_KNOTS('',3,(#8067,#8068,#8069,#8070,#8071,#8072,
#8073,#8074,#8075,#8076,#8077,#8078,#8079,#8080,#8081,#8082,#8083,#8084,
#8085,#8086,#8087,#8088,#8089,#8090,#8091,#8092,#8093,#8094,#8095,#8096,
#8097,#8098,#8099,#8100,#8101,#8102,#8103,#8104,#8105,#8106,#8107,#8108,
#8109),.UNSPECIFIED.,.F.,.F.,(4,3,3,3,3,3,3,3,3,3,3,3,3,3,4),(0.,0.0935644284073191,
0.18729632151828,0.281031513390348,0.374648205279863,0.467922871498954,
0.499491751099595,0.579460878581141,0.659419998763359,0.739384630924569,
0.819398568293176,0.899442161096395,0.979559995621145,0.998983502199193,
1.11885509353981),.UNSPECIFIED.);
#104=B_SPLINE_CURVE_WITH_KNOTS('',3,(#8111,#8112,#8113,#8114,#8115,#8116,
#8117,#8118,#8119,#8120,#8121,#8122,#8123,#8124,#8125,#8126,#8127,#8128,
#8129,#8130,#8131,#8132,#8133,#8134,#8135,#8136,#8137,#8138,#8139,#8140,
#8141,#8142,#8143,#8144,#8145,#8146,#8147,#8148,#8149,#8150,#8151,#8152,
#8153,#8154,#8155,#8156,#8157,#8158,#8159,#8160,#8161,#8162,#8163,#8164,
#8165,#8166,#8167,#8168,#8169,#8170,#8171,#8172,#8173,#8174,#8175,#8176,
#8177,#8178,#8179,#8180,#8181,#8182,#8183,#8184,#8185,#8186,#8187,#8188,
#8189,#8190,#8191,#8192,#8193,#8194,#8195,#8196,#8197,#8198,#8199,#8200,
#8201,#8202,#8203,#8204,#8205,#8206,#8207,#8208,#8209,#8210,#8211,#8212,
#8213,#8214,#8215,#8216,#8217,#8218,#8219,#8220,#8221,#8222,#8223,#8224,
#8225,#8226,#8227,#8228,#8229,#8230,#8231,#8232,#8233,#8234,#8235,#8236,
#8237,#8238,#8239,#8240,#8241,#8242,#8243,#8244,#8245,#8246,#8247,#8248,
#8249,#8250,#8251,#8252,#8253,#8254,#8255,#8256,#8257,#8258,#8259,#8260,
#8261,#8262,#8263,#8264,#8265,#8266,#8267,#8268,#8269,#8270,#8271,#8272,
#8273,#8274,#8275,#8276,#8277,#8278,#8279,#8280,#8281,#8282,#8283,#8284,
#8285,#8286,#8287,#8288,#8289,#8290,#8291,#8292,#8293,#8294,#8295,#8296,
#8297,#8298,#8299,#8300,#8301,#8302,#8303,#8304,#8305,#8306,#8307,#8308,
#8309,#8310,#8311,#8312,#8313,#8314,#8315,#8316,#8317,#8318,#8319,#8320,
#8321,#8322,#8323,#8324,#8325,#8326,#8327,#8328,#8329,#8330,#8331,#8332,
#8333,#8334,#8335,#8336,#8337,#8338,#8339,#8340,#8341,#8342,#8343,#8344,
#8345,#8346,#8347,#8348,#8349,#8350,#8351,#8352,#8353,#8354),
 .UNSPECIFIED.,.F.,.F.,(4,3,3,3,3,3,3,3,3,3,3,3,3,3,3,3,3,3,3,3,3,3,3,3,
3,3,3,3,3,3,3,3,3,3,3,3,3,3,3,3,3,3,3,3,3,3,3,3,3,3,3,3,3,3,3,3,3,3,3,3,
3,3,3,3,3,3,3,3,3,3,3,3,3,3,3,3,3,3,3,3,3,4),(1.11885509365731,1.19890888242023,
1.27890195600316,1.35885150057562,1.43878687530592,1.51871708466099,1.59865764641746,
1.67862408146344,1.7586825532862,1.8387877251625,1.91902312927819,1.99796700439835,
2.07727102857866,2.15647325956687,2.23559184022159,2.31464483775223,2.39365026085368,
2.47263617598548,2.55161468675081,2.63060203582996,2.70961446936347,2.78871342568456,
2.86785984415472,2.94712339981395,2.9969505065975,3.07705312821031,3.1570619066815,
3.23699421838189,3.31686738045404,3.39669866385784,3.47651649014003,3.55633064916348,
3.63615673738681,3.71601035527486,3.7959500957172,3.87593839432808,3.95603826859724,
3.99593400879665,4.07599768389782,4.15596874230769,4.23586459502544,4.31570259458817,
4.39550004816396,4.47528616612706,4.55506994268505,4.63486700962401,4.714693003592,
4.79460740114907,4.87457161678181,4.95464958904228,4.99491751099581,5.07478899813074,
5.15456501822308,5.23426318727578,5.3139010592233,5.39349613977932,5.47307716442314,
5.55265417799236,5.63224298538747,5.71185939566583,5.79156324137428,5.87131604149074,
5.95118306081602,5.99390101319496,6.07389207539437,6.15378892336041,6.23360904990546,
6.31336988767804,6.39308882254675,6.47279463932957,6.55249701617323,6.63221165251339,
6.71195425208848,6.79178420386357,6.87166325245412,6.9516556575512,6.99288451539411,
7.08126525070436,7.16930398900817,7.25712468236554,7.3445872388794,7.40204018941607),
 .UNSPECIFIED.);
#105=B_SPLINE_CURVE_WITH_KNOTS('',3,(#8356,#8357,#8358,#8359,#8360,#8361,
#8362,#8363,#8364,#8365),.UNSPECIFIED.,.F.,.F.,(4,1,1,1,1,1,1,4),(7.40204040071942,
7.99186801759328,8.99085151979246,9.98983502199165,10.9888185241908,11.98780202639,
12.9867855285892,13.6852257078989),.UNSPECIFIED.);
#106=B_SPLINE_CURVE_WITH_KNOTS('',3,(#8367,#8368,#8369,#8370,#8371,#8372,
#8373,#8374,#8375,#8376,#8377,#8378,#8379,#8380,#8381,#8382,#8383,#8384,
#8385,#8386,#8387,#8388,#8389,#8390,#8391,#8392,#8393,#8394,#8395,#8396,
#8397,#8398,#8399,#8400,#8401,#8402,#8403,#8404,#8405,#8406,#8407,#8408,
#8409,#8410,#8411,#8412,#8413,#8414,#8415,#8416,#8417,#8418,#8419,#8420,
#8421,#8422,#8423,#8424,#8425,#8426,#8427,#8428,#8429,#8430,#8431,#8432,
#8433,#8434,#8435,#8436,#8437,#8438,#8439,#8440,#8441,#8442,#8443,#8444,
#8445,#8446,#8447,#8448,#8449,#8450,#8451,#8452,#8453,#8454,#8455,#8456,
#8457,#8458,#8459,#8460,#8461,#8462,#8463,#8464,#8465,#8466,#8467,#8468,
#8469,#8470,#8471,#8472,#8473,#8474,#8475,#8476,#8477,#8478,#8479,#8480,
#8481,#8482,#8483,#8484,#8485,#8486,#8487,#8488,#8489,#8490,#8491,#8492,
#8493,#8494,#8495,#8496,#8497,#8498,#8499,#8500,#8501,#8502,#8503,#8504,
#8505,#8506,#8507,#8508,#8509,#8510,#8511,#8512,#8513,#8514,#8515,#8516,
#8517,#8518,#8519,#8520,#8521,#8522,#8523,#8524,#8525,#8526,#8527,#8528,
#8529,#8530,#8531,#8532,#8533,#8534,#8535,#8536,#8537,#8538,#8539,#8540,
#8541,#8542,#8543,#8544,#8545,#8546,#8547,#8548,#8549,#8550,#8551,#8552,
#8553,#8554,#8555,#8556,#8557,#8558,#8559,#8560,#8561,#8562,#8563,#8564,
#8565,#8566,#8567,#8568,#8569,#8570,#8571,#8572,#8573,#8574,#8575,#8576,
#8577,#8578,#8579,#8580,#8581,#8582,#8583,#8584,#8585,#8586,#8587,#8588,
#8589,#8590,#8591,#8592,#8593,#8594,#8595,#8596,#8597,#8598,#8599,#8600,
#8601,#8602,#8603,#8604,#8605,#8606,#8607,#8608,#8609,#8610,#8611,#8612,
#8613),.UNSPECIFIED.,.F.,.F.,(4,3,3,3,3,3,3,3,3,3,3,3,3,3,3,3,3,3,3,3,3,
3,3,3,3,3,3,3,3,3,3,3,3,3,3,3,3,3,3,3,3,3,3,3,3,3,3,3,3,3,3,3,3,3,3,3,3,
3,3,3,3,3,3,3,3,3,3,3,3,3,3,3,3,3,3,3,3,3,3,3,3,3,4),(13.6852258923761,
13.7811381458858,13.8778420020683,13.9753729543055,13.9857690307884,14.0657337088802,
14.1456040124813,14.2253974614937,14.3051315153514,14.3848235864942,14.4645025074165,
14.5441779714702,14.623865701738,14.7035814256359,14.7833846844125,14.8632371039494,
14.9432032095308,14.9847525329875,15.0647176274353,15.1445883524893,15.2243822276137,
15.3041167118116,15.3838092170969,15.4634885764725,15.5431644816131,15.6228526552282,
15.7025688243615,15.7823725290164,15.8622253954616,15.9421919457269,15.9837360351867,
16.063700994944,16.143571584348,16.2233653230009,16.3030996700424,16.3827920376221,
16.4624712589146,16.5421470257523,16.6218350609649,16.7015510917162,16.7813546587208,
16.8612073877251,16.9411738020618,16.9827195373858,17.0626844575672,17.1425550065156,
17.2223487038769,17.3020830088335,17.3817753335765,17.4614545110396,17.5411302334353,
17.6208182236289,17.7005342088199,17.7803377296644,17.8601904120997,17.9401567796245,
17.981703039585,18.0616680202291,18.1415386304136,18.2213323897207,18.3010667572697,
18.3807591451903,18.4604383865057,18.5401141731666,18.619802227984,18.6995182781033,
18.7793218640147,18.8591746116927,18.9391410441751,18.9806865417842,19.0604936907362,
19.1402065480529,19.2198427864482,19.299420016977,19.3830438917397,19.4625667314659,
19.542087693453,19.6216226370564,19.7011874271912,19.7808399463116,19.860543555116,
19.9403569248264,19.9684110150785),.UNSPECIFIED.);
#107=B_SPLINE_CURVE_WITH_KNOTS('',3,(#8615,#8616,#8617,#8618,#8619,#8620,
#8621,#8622,#8623,#8624,#8625,#8626),.UNSPECIFIED.,.F.,.F.,(4,2,1,1,1,1,
1,1,4),(19.9684110150785,19.9796700439833,20.9786535461825,21.9776370483816,
22.9766205505808,23.9756040527799,24.9745875549791,25.9735710571782,26.2515921566761),
 .UNSPECIFIED.);
#108=B_SPLINE_CURVE_WITH_KNOTS('',3,(#8628,#8629,#8630,#8631,#8632,#8633,
#8634,#8635,#8636,#8637,#8638,#8639,#8640,#8641,#8642,#8643,#8644,#8645,
#8646,#8647,#8648,#8649,#8650,#8651,#8652,#8653,#8654,#8655,#8656,#8657,
#8658,#8659,#8660,#8661,#8662,#8663,#8664,#8665,#8666,#8667,#8668,#8669,
#8670,#8671,#8672,#8673,#8674,#8675,#8676,#8677,#8678,#8679,#8680,#8681,
#8682,#8683,#8684,#8685,#8686,#8687,#8688,#8689,#8690,#8691,#8692,#8693,
#8694,#8695,#8696,#8697,#8698,#8699,#8700,#8701,#8702,#8703,#8704,#8705,
#8706,#8707,#8708,#8709,#8710,#8711,#8712,#8713,#8714,#8715,#8716,#8717,
#8718,#8719,#8720,#8721,#8722,#8723,#8724,#8725,#8726,#8727,#8728,#8729,
#8730,#8731,#8732,#8733,#8734,#8735,#8736,#8737,#8738,#8739,#8740,#8741,
#8742,#8743,#8744,#8745,#8746,#8747,#8748,#8749,#8750,#8751,#8752,#8753,
#8754,#8755,#8756,#8757,#8758,#8759,#8760,#8761,#8762,#8763,#8764,#8765,
#8766,#8767,#8768,#8769,#8770,#8771,#8772,#8773,#8774,#8775,#8776,#8777,
#8778,#8779,#8780,#8781,#8782,#8783,#8784,#8785,#8786,#8787,#8788,#8789,
#8790,#8791,#8792,#8793,#8794,#8795,#8796,#8797,#8798,#8799,#8800,#8801,
#8802,#8803,#8804,#8805,#8806,#8807,#8808,#8809,#8810,#8811,#8812,#8813,
#8814,#8815,#8816,#8817,#8818,#8819,#8820,#8821,#8822,#8823,#8824,#8825,
#8826,#8827,#8828,#8829,#8830,#8831,#8832,#8833,#8834,#8835,#8836,#8837,
#8838,#8839,#8840,#8841,#8842,#8843,#8844,#8845,#8846,#8847,#8848,#8849,
#8850,#8851,#8852,#8853,#8854,#8855,#8856,#8857,#8858,#8859,#8860,#8861,
#8862,#8863,#8864,#8865,#8866,#8867,#8868,#8869,#8870,#8871),
 .UNSPECIFIED.,.F.,.F.,(4,3,3,3,3,3,3,3,3,3,3,3,3,3,3,3,3,3,3,3,3,3,3,3,
3,3,3,3,3,3,3,3,3,3,3,3,3,3,3,3,3,3,3,3,3,3,3,3,3,3,3,3,3,3,3,3,3,3,3,3,
3,3,3,3,3,3,3,3,3,3,3,3,3,3,3,3,3,3,3,3,3,4),(26.2515963222581,26.3306329510203,
26.4108731520649,26.4898610484131,26.5688492534367,26.647854020369,26.7290291551211,
26.8081567839455,26.8903556716614,26.9725545593774,27.0525195182439,27.1323901064284,
27.2121838435362,27.2919181887089,27.3716105540985,27.4512897727228,27.5309655365955,
27.6106535685474,27.6903695957433,27.7701731587582,27.8500258835208,27.9299922932555,
27.9715380615766,28.0515030203413,28.1313736084233,28.2111673454273,28.2909016904953,
28.3705940557787,28.4502732742969,28.5299490380631,28.6096370699079,28.6893530969969,
28.7691566599045,28.8490093845593,28.9289757941872,28.9705215637758,29.0504865225538,
29.130357110649,29.2101508476663,29.2898851927477,29.3695775580446,29.4492567765757,
29.5289325403545,29.6086205722123,29.6883365993133,29.7681401622332,29.8479928869009,
29.9279592965406,29.969505065975,30.0494700247739,30.1293406128902,30.2091343499289,
30.2888686950319,30.3685610603512,30.4482402789046,30.5279160427061,30.6076040745864,
30.6873201017102,30.7671236646531,30.8469763893435,30.9269427990063,30.9684885681741,
31.0484535269574,31.1283241150579,31.2081178520804,31.2878521971676,31.3675445624705,
31.4472237810075,31.5268995447925,31.6065875766561,31.6863036037632,31.7661071666897,
31.8459598913635,31.9259263010099,31.9674720703733,32.0493953620172,32.1312078546291,
32.212922693681,32.2945286616084,32.3760709623789,32.4575526442695,32.5347816294377),
 .UNSPECIFIED.);
#109=B_SPLINE_CURVE_WITH_KNOTS('',3,(#8873,#8874,#8875,#8876,#8877,#8878,
#8879,#8880,#8881,#8882),.UNSPECIFIED.,.F.,.F.,(4,1,1,1,1,1,1,4),(32.5347869710949,
32.9664555725725,33.9654390747716,34.9644225769708,35.9634060791699,36.9623895813691,
37.9613730835682,38.8179669366173),.UNSPECIFIED.);
#110=B_SPLINE_CURVE_WITH_KNOTS('',3,(#8884,#8885,#8886,#8887,#8888,#8889,
#8890,#8891,#8892,#8893,#8894),.UNSPECIFIED.,.F.,.F.,(4,1,1,1,1,1,1,1,4),
(38.8179669366173,38.9603565857674,39.9593400879665,40.9583235901657,41.9573070923649,
42.9562905945641,43.9552740967633,44.9542575989625,45.101152243797),
 .UNSPECIFIED.);
#111=B_SPLINE_CURVE_WITH_KNOTS('',3,(#8896,#8897,#8898,#8899,#8900,#8901,
#8902,#8903,#8904,#8905),.UNSPECIFIED.,.F.,.F.,(4,1,1,1,1,1,1,4),(45.101152243797,
45.9532411011617,46.9522246033608,47.95120810556,48.9501916077592,49.9491751099583,
50.9481586121575,51.3843324992521),.UNSPECIFIED.);
#112=B_SPLINE_CURVE_WITH_KNOTS('',3,(#8907,#8908,#8909,#8910,#8911,#8912,
#8913,#8914,#8915,#8916,#8917,#8918,#8919,#8920,#8921,#8922,#8923,#8924,
#8925,#8926,#8927,#8928,#8929,#8930,#8931,#8932,#8933,#8934,#8935,#8936,
#8937,#8938,#8939,#8940,#8941,#8942,#8943,#8944,#8945,#8946,#8947,#8948,
#8949,#8950,#8951,#8952,#8953,#8954,#8955,#8956,#8957,#8958,#8959,#8960,
#8961,#8962,#8963,#8964,#8965,#8966,#8967,#8968,#8969,#8970,#8971,#8972,
#8973,#8974,#8975,#8976,#8977,#8978,#8979,#8980,#8981,#8982,#8983,#8984,
#8985,#8986,#8987,#8988,#8989,#8990,#8991,#8992,#8993,#8994,#8995,#8996,
#8997,#8998,#8999,#9000,#9001,#9002,#9003,#9004,#9005,#9006,#9007,#9008,
#9009,#9010,#9011,#9012,#9013,#9014,#9015,#9016,#9017,#9018,#9019,#9020,
#9021,#9022,#9023,#9024,#9025,#9026,#9027,#9028,#9029,#9030,#9031,#9032,
#9033,#9034,#9035,#9036,#9037,#9038,#9039,#9040,#9041,#9042,#9043,#9044,
#9045,#9046,#9047,#9048,#9049,#9050,#9051,#9052,#9053,#9054,#9055,#9056,
#9057,#9058,#9059,#9060,#9061,#9062,#9063,#9064,#9065,#9066,#9067,#9068,
#9069,#9070,#9071,#9072,#9073,#9074,#9075,#9076,#9077,#9078,#9079,#9080,
#9081,#9082,#9083,#9084,#9085,#9086,#9087,#9088,#9089,#9090,#9091,#9092,
#9093,#9094,#9095,#9096,#9097,#9098,#9099,#9100,#9101,#9102,#9103,#9104,
#9105,#9106,#9107,#9108,#9109,#9110,#9111,#9112,#9113,#9114,#9115,#9116,
#9117,#9118,#9119,#9120,#9121,#9122,#9123,#9124,#9125,#9126,#9127,#9128,
#9129,#9130,#9131,#9132,#9133,#9134,#9135,#9136,#9137,#9138,#9139,#9140,
#9141,#9142,#9143,#9144,#9145,#9146,#9147,#9148,#9149,#9150,#9151,#9152,
#9153),.UNSPECIFIED.,.F.,.F.,(4,3,3,3,3,3,3,3,3,3,3,3,3,3,3,3,3,3,3,3,3,
3,3,3,3,3,3,3,3,3,3,3,3,3,3,3,3,3,3,3,3,3,3,3,3,3,3,3,3,3,3,3,3,3,3,3,3,
3,3,3,3,3,3,3,3,3,3,3,3,3,3,3,3,3,3,3,3,3,3,3,3,3,4),(51.3843375509764,
51.4659219703665,51.5475504548222,51.6292356660958,51.711051351291,51.7929351797258,
51.8749722248705,51.9471421143566,52.0271070731438,52.1069776612481,52.1867713982747,
52.2665057433655,52.3461981086724,52.4258773272134,52.5055530910026,52.5852411228703,
52.6649571499817,52.744760712912,52.8246134375896,52.90457984724,52.9461256165558,
53.0260905753431,53.1059611634476,53.1857549004743,53.2654892455655,53.3451816108724,
53.4248608294136,53.5045365932028,53.5842246250706,53.6639406521816,53.7437442151119,
53.8235969397897,53.9035633494401,53.9451091187549,54.0250740775424,54.1049446656471,
54.1847384026741,54.2644727477653,54.3441651130724,54.4238443316137,54.503520095403,
54.5832081272712,54.6629241543834,54.7427277173139,54.8225804419923,54.9025468516429,
54.9440926209541,55.0240575797413,55.1039281678459,55.1837219048729,55.2634562499639,
55.3431486152707,55.4228278338118,55.5025035976009,55.5821916294688,55.6619076565804,
55.7417112195109,55.8215639441889,55.9015303538393,55.9430761231532,56.0230410819406,
56.1029116700452,56.1827054070721,56.2624397521628,56.3421321174705,56.4218113360118,
56.501487099801,56.5811751316687,56.6608911587802,56.7406947217107,56.8205474463889,
56.9005138560392,56.9420596253524,57.0213023256814,57.1020798922408,57.1811290941038,
57.2601247624458,57.3390832275544,57.4211931352048,57.5001424786768,57.5791007326911,
57.6581021560049,57.6675228581561),.UNSPECIFIED.);
#113=B_SPLINE_CURVE_WITH_KNOTS('',3,(#9155,#9156,#9157,#9158,#9159,#9160,
#9161,#9162,#9163,#9164,#9165),.UNSPECIFIED.,.F.,.F.,(4,1,1,1,1,1,1,1,4),
(57.6675266605331,57.9410431275516,58.9400266297507,59.9390101319499,60.9379936341491,
61.9369771363482,62.9359606385474,63.9349441407466,63.9507081653357),
 .UNSPECIFIED.);
#114=B_SPLINE_CURVE_WITH_KNOTS('',3,(#9167,#9168,#9169,#9170,#9171,#9172,
#9173,#9174,#9175,#9176,#9177,#9178,#9179,#9180,#9181,#9182,#9183,#9184,
#9185,#9186,#9187,#9188,#9189,#9190,#9191,#9192,#9193,#9194,#9195,#9196,
#9197,#9198,#9199,#9200,#9201,#9202,#9203,#9204,#9205,#9206,#9207,#9208,
#9209,#9210,#9211,#9212,#9213,#9214,#9215,#9216,#9217,#9218,#9219,#9220,
#9221,#9222,#9223,#9224,#9225,#9226,#9227,#9228,#9229,#9230,#9231,#9232,
#9233,#9234,#9235,#9236,#9237,#9238,#9239,#9240,#9241,#9242,#9243,#9244,
#9245,#9246,#9247,#9248,#9249,#9250,#9251,#9252,#9253,#9254,#9255,#9256,
#9257,#9258,#9259,#9260,#9261,#9262,#9263,#9264,#9265,#9266,#9267,#9268,
#9269,#9270,#9271,#9272,#9273,#9274,#9275,#9276,#9277,#9278,#9279,#9280,
#9281,#9282,#9283,#9284,#9285,#9286,#9287,#9288,#9289,#9290,#9291,#9292,
#9293,#9294,#9295,#9296,#9297,#9298,#9299,#9300,#9301,#9302,#9303,#9304,
#9305,#9306,#9307,#9308,#9309,#9310,#9311,#9312,#9313,#9314,#9315,#9316,
#9317,#9318,#9319,#9320,#9321,#9322,#9323,#9324,#9325,#9326,#9327,#9328,
#9329,#9330,#9331,#9332,#9333,#9334,#9335,#9336,#9337,#9338,#9339,#9340,
#9341,#9342,#9343,#9344,#9345,#9346,#9347,#9348,#9349,#9350,#9351,#9352,
#9353,#9354,#9355,#9356,#9357,#9358,#9359,#9360,#9361,#9362,#9363,#9364,
#9365,#9366,#9367,#9368,#9369,#9370,#9371,#9372,#9373,#9374,#9375,#9376,
#9377,#9378,#9379,#9380,#9381,#9382,#9383,#9384,#9385,#9386,#9387,#9388,
#9389,#9390,#9391,#9392,#9393,#9394,#9395,#9396,#9397,#9398,#9399,#9400,
#9401,#9402,#9403,#9404,#9405,#9406,#9407,#9408,#9409,#9410,#9411,#9412,
#9413),.UNSPECIFIED.,.F.,.F.,(4,3,3,3,3,3,3,3,3,3,3,3,3,3,3,3,3,3,3,3,3,
3,3,3,3,3,3,3,3,3,3,3,3,3,3,3,3,3,3,3,3,3,3,3,3,3,3,3,3,3,3,3,3,3,3,3,3,
3,3,3,3,3,3,3,3,3,3,3,3,3,3,3,3,3,3,3,3,3,3,3,3,3,4),(63.9507081653357,
64.0304540093271,64.1101058619716,64.1896814506261,64.2691984406716,64.3522895909558,
64.4317533767242,64.5112157170839,64.5906925209173,64.6701997030615,64.7497948088937,
64.8294415713291,64.9091973059203,64.9339276429458,65.0138926017331,65.0937631898377,
65.1735569268647,65.2532912719556,65.3329836372622,65.4126628558034,65.4923386195927,
65.5720266514604,65.6517426785721,65.7315462415026,65.8113989661805,65.8913653758311,
65.9329111451449,66.0128761039322,66.092746692037,66.1725404290636,66.2522747741544,
66.3319671394608,66.4116463580019,66.4913221217909,66.5710101536589,66.6507261807705,
66.7305297437008,66.8103824683786,66.890348878029,66.9318946473441,67.0118596061315,
67.091730194236,67.1715239312629,67.2512582763545,67.3309506416611,67.4106298602024,
67.4903056239916,67.5699936558595,67.6497096829711,67.7295132459017,67.8093659705799,
67.8893323802304,67.9308781495432,68.0108431083305,68.090713696435,68.1705074334619,
68.250241778553,68.3299341438601,68.4096133624013,68.4892891261903,68.5689771580581,
68.64869318517,68.7284967481004,68.8083494727784,68.888315882429,68.9298616517423,
69.0098266105296,69.089697198634,69.1694909356608,69.2492252807525,69.3289176460595,
69.4085968646007,69.4882726283898,69.5679606602578,69.6476766873696,69.7274802502999,
69.8073329749774,69.8872993846278,69.9288451539415,70.0256929206329,70.1219607775206,
70.2171816476072,70.2338932790561),.UNSPECIFIED.);
#115=B_SPLINE_CURVE_WITH_KNOTS('',3,(#9415,#9416,#9417,#9418,#9419,#9420,
#9421,#9422,#9423,#9424),.UNSPECIFIED.,.F.,.F.,(4,1,1,1,1,1,1,4),(70.2338934725153,
70.9278286561406,71.9268121583398,72.925795660539,73.9247791627382,74.9237626649374,
75.9227461671366,76.5170787796949),.UNSPECIFIED.);
#116=B_SPLINE_CURVE_WITH_KNOTS('',3,(#9426,#9427,#9428,#9429,#9430,#9431,
#9432,#9433,#9434,#9435,#9436,#9437,#9438,#9439,#9440,#9441,#9442,#9443,
#9444,#9445,#9446,#9447,#9448,#9449,#9450,#9451,#9452,#9453,#9454,#9455,
#9456,#9457,#9458,#9459,#9460,#9461,#9462,#9463,#9464,#9465,#9466,#9467,
#9468,#9469,#9470,#9471,#9472,#9473,#9474,#9475,#9476,#9477,#9478,#9479,
#9480,#9481,#9482,#9483,#9484,#9485,#9486,#9487,#9488,#9489,#9490,#9491,
#9492,#9493,#9494,#9495,#9496,#9497,#9498,#9499,#9500,#9501,#9502,#9503,
#9504,#9505,#9506,#9507,#9508,#9509,#9510,#9511,#9512,#9513,#9514,#9515,
#9516,#9517,#9518,#9519,#9520,#9521,#9522,#9523,#9524,#9525,#9526,#9527,
#9528,#9529,#9530,#9531,#9532,#9533,#9534,#9535,#9536,#9537,#9538,#9539,
#9540,#9541,#9542,#9543,#9544,#9545,#9546,#9547,#9548,#9549,#9550,#9551,
#9552,#9553,#9554,#9555,#9556,#9557,#9558,#9559,#9560,#9561,#9562,#9563,
#9564,#9565,#9566,#9567,#9568,#9569,#9570,#9571,#9572,#9573,#9574,#9575,
#9576,#9577,#9578,#9579,#9580,#9581,#9582,#9583,#9584,#9585,#9586,#9587,
#9588,#9589,#9590,#9591,#9592,#9593,#9594,#9595,#9596,#9597,#9598,#9599,
#9600,#9601,#9602,#9603,#9604,#9605,#9606,#9607,#9608,#9609,#9610,#9611,
#9612,#9613,#9614,#9615,#9616,#9617,#9618,#9619,#9620,#9621,#9622,#9623,
#9624,#9625,#9626,#9627,#9628,#9629,#9630,#9631,#9632,#9633,#9634,#9635,
#9636,#9637,#9638,#9639,#9640,#9641,#9642,#9643,#9644,#9645,#9646,#9647,
#9648,#9649,#9650,#9651,#9652,#9653,#9654,#9655,#9656,#9657,#9658,#9659,
#9660,#9661,#9662,#9663,#9664,#9665,#9666,#9667,#9668,#9669,#9670,#9671,
#9672),.UNSPECIFIED.,.F.,.F.,(4,3,3,3,3,3,3,3,3,3,3,3,3,3,3,3,3,3,3,3,3,
3,3,3,3,3,3,3,3,3,3,3,3,3,3,3,3,3,3,3,3,3,3,3,3,3,3,3,3,3,3,3,3,3,3,3,3,
3,3,3,3,3,3,3,3,3,3,3,3,3,3,3,3,3,3,3,3,3,3,3,3,3,4),(76.5170789972737,
76.604724745235,76.6928108189936,76.7811201939996,76.8697456009293,76.9217296693358,
77.0016946281234,77.0815652162282,77.1613589532554,77.2410932983468,77.3207856636539,
77.4004648821953,77.4801406459847,77.5598286778528,77.6395447049645,77.7193482678952,
77.7992009925734,77.8791674022242,77.9207131715349,78.0006781303222,78.0805487184268,
78.1603424554537,78.2400768005447,78.3197691658517,78.3994483843929,78.4791241481821,
78.55881218005,78.6385282071615,78.718331770092,78.7981844947699,78.8781509044204,
78.9196966737341,78.9996616325214,79.0795322206259,79.1593259576527,79.2390603027437,
79.3187526680505,79.3984318865917,79.4781076503808,79.5577956822486,79.63751170936,
79.7173152722904,79.7971679969683,79.8771344066187,79.9186801759332,79.9986451347205,
80.0785157228252,80.158309459852,80.2380438049431,80.31773617025,80.3974153887912,
80.4770911525804,80.5567791844482,80.6364952115598,80.7162987744902,80.7961514991682,
80.8761179088187,80.9176636781324,80.9976286369197,81.0774992250243,81.1572929620511,
81.2370273071422,81.3167196724491,81.3963988909903,81.4760746547794,81.5557626866472,
81.6354787137588,81.7152822766893,81.7951350013672,81.8751014110176,81.9166471803315,
81.9955344657586,82.0743281297056,82.1530465802032,82.2339487685371,82.3125756196587,
82.3911872681938,82.469800214983,82.5524161829559,82.6311178282799,82.7098621033094,
82.7886974136541,82.8002640868745),.UNSPECIFIED.);
#117=B_SPLINE_CURVE_WITH_KNOTS('',3,(#9674,#9675,#9676,#9677,#9678,#9679,
#9680,#9681,#9682,#9683,#9684),.UNSPECIFIED.,.F.,.F.,(4,1,1,1,1,1,1,1,4),
(82.8002640868745,82.9156306825307,83.9146141847298,84.913597686929,85.9125811891282,
86.9115646913274,87.9105481935266,88.9095316957258,89.0834493940541),
 .UNSPECIFIED.);
#118=B_SPLINE_CURVE_WITH_KNOTS('',3,(#9686,#9687,#9688,#9689,#9690,#9691,
#9692,#9693,#9694,#9695,#9696,#9697,#9698,#9699,#9700,#9701,#9702,#9703,
#9704,#9705,#9706,#9707,#9708,#9709,#9710,#9711,#9712,#9713,#9714,#9715,
#9716,#9717,#9718,#9719,#9720,#9721,#9722,#9723,#9724,#9725,#9726,#9727,
#9728,#9729,#9730,#9731,#9732,#9733,#9734,#9735,#9736,#9737,#9738,#9739,
#9740,#9741,#9742,#9743,#9744,#9745,#9746,#9747,#9748,#9749,#9750,#9751,
#9752,#9753,#9754,#9755,#9756,#9757,#9758,#9759,#9760,#9761,#9762,#9763,
#9764,#9765,#9766,#9767,#9768,#9769,#9770,#9771,#9772,#9773,#9774,#9775,
#9776,#9777,#9778,#9779,#9780,#9781,#9782,#9783,#9784,#9785,#9786,#9787,
#9788,#9789,#9790,#9791,#9792,#9793,#9794,#9795,#9796,#9797,#9798,#9799,
#9800,#9801,#9802,#9803,#9804,#9805,#9806,#9807,#9808,#9809,#9810,#9811,
#9812,#9813,#9814,#9815,#9816,#9817,#9818,#9819,#9820,#9821,#9822,#9823,
#9824,#9825,#9826,#9827,#9828,#9829,#9830,#9831,#9832,#9833,#9834,#9835,
#9836,#9837,#9838,#9839,#9840,#9841,#9842,#9843,#9844,#9845,#9846,#9847,
#9848,#9849,#9850,#9851,#9852,#9853,#9854,#9855,#9856,#9857,#9858,#9859,
#9860,#9861,#9862,#9863,#9864,#9865,#9866,#9867,#9868,#9869,#9870,#9871,
#9872,#9873,#9874,#9875,#9876,#9877,#9878,#9879,#9880,#9881,#9882,#9883,
#9884,#9885,#9886,#9887,#9888,#9889,#9890,#9891,#9892,#9893,#9894,#9895,
#9896,#9897,#9898,#9899,#9900,#9901,#9902,#9903,#9904,#9905,#9906,#9907,
#9908,#9909,#9910,#9911,#9912,#9913,#9914,#9915,#9916,#9917,#9918,#9919,
#9920,#9921,#9922,#9923,#9924,#9925,#9926,#9927,#9928,#9929,#9930,#9931,
#9932),.UNSPECIFIED.,.F.,.F.,(4,3,3,3,3,3,3,3,3,3,3,3,3,3,3,3,3,3,3,3,3,
3,3,3,3,3,3,3,3,3,3,3,3,3,3,3,3,3,3,3,3,3,3,3,3,3,3,3,3,3,3,3,3,3,3,3,3,
3,3,3,3,3,3,3,3,3,3,3,3,3,3,3,3,3,3,3,3,3,3,3,3,3,4),(89.0834493940541,
89.162104822173,89.24069050899,89.319224841056,89.3977345280541,89.4762339591774,
89.5547396989003,89.6332683149672,89.7118787705787,89.7905353918081,89.8693023315089,
89.9085151979249,89.9884801567122,90.0683507448169,90.1481444818438,90.2278788269349,
90.3075711922417,90.387250410783,90.4669261745722,90.54661420644,90.6263302335514,
90.7061337964818,90.7859865211597,90.8659529308102,90.9074987001241,90.9874636589114,
91.067334247016,91.1471279840428,91.2268623291339,91.306554694441,91.3862339129823,
91.4659096767714,91.5455977086393,91.6253137357504,91.7051172986808,91.7849700233589,
91.8649364330094,91.9064822023232,91.9864471611105,92.0663177492151,92.1461114862419,
92.2258458313331,92.3055381966401,92.3852174151813,92.4648931789704,92.5445812108382,
92.6242972379498,92.7041008008802,92.7839535255579,92.8639199352083,92.9054657045224,
92.9854306633098,93.0653012514141,93.1450949884408,93.2248293335317,93.304521698839,
93.3842009173802,93.4638766811693,93.5435647130373,93.6232807401489,93.7030843030794,
93.7829370277574,93.862903437408,93.9044492067215,93.9844141655087,94.0642847536132,
94.1440784906401,94.2238128357304,94.3035052010373,94.3831844195783,94.4628601833674,
94.5425482152353,94.6222642423477,94.7020678052781,94.7819205299559,94.8618869396063,
94.9034327089207,94.9890127520186,95.0744296002041,95.1596141447421,95.2446560142868,
95.3294979157902,95.3666345040236),.UNSPECIFIED.);
#119=B_SPLINE_CURVE_WITH_KNOTS('',3,(#9934,#9935,#9936,#9937,#9938,#9939,
#9940,#9941,#9942,#9943),.UNSPECIFIED.,.F.,.F.,(4,1,1,1,1,1,1,4),(95.3666347012337,
95.9024162111198,96.901399713319,97.9003832155182,98.8993667177174,99.8983502199165,
100.897333722116,101.649820008413),.UNSPECIFIED.);
#120=B_SPLINE_CURVE_WITH_KNOTS('',3,(#9945,#9946,#9947,#9948,#9949,#9950,
#9951,#9952,#9953,#9954,#9955,#9956,#9957,#9958,#9959,#9960,#9961,#9962,
#9963,#9964,#9965,#9966,#9967,#9968,#9969,#9970,#9971,#9972,#9973,#9974,
#9975,#9976,#9977,#9978,#9979,#9980,#9981,#9982,#9983,#9984,#9985,#9986,
#9987,#9988,#9989,#9990,#9991,#9992,#9993,#9994,#9995,#9996,#9997,#9998,
#9999,#10000,#10001,#10002,#10003,#10004,#10005,#10006,#10007,#10008,#10009,
#10010,#10011,#10012,#10013,#10014,#10015,#10016,#10017,#10018,#10019,#10020,
#10021,#10022,#10023,#10024,#10025,#10026,#10027,#10028,#10029,#10030,#10031,
#10032,#10033,#10034,#10035,#10036,#10037,#10038,#10039,#10040,#10041,#10042,
#10043,#10044,#10045,#10046,#10047,#10048,#10049,#10050,#10051,#10052,#10053,
#10054,#10055,#10056,#10057,#10058,#10059,#10060,#10061,#10062,#10063,#10064,
#10065,#10066,#10067,#10068,#10069,#10070,#10071,#10072,#10073,#10074,#10075,
#10076,#10077,#10078,#10079,#10080,#10081,#10082,#10083,#10084,#10085,#10086,
#10087,#10088,#10089,#10090,#10091,#10092,#10093,#10094,#10095,#10096,#10097,
#10098,#10099,#10100,#10101,#10102,#10103,#10104,#10105,#10106,#10107,#10108,
#10109,#10110,#10111,#10112,#10113,#10114,#10115,#10116,#10117,#10118,#10119,
#10120,#10121,#10122,#10123,#10124,#10125,#10126,#10127,#10128,#10129,#10130,
#10131,#10132,#10133,#10134,#10135,#10136,#10137,#10138,#10139,#10140,#10141,
#10142,#10143,#10144,#10145,#10146,#10147,#10148,#10149,#10150,#10151,#10152,
#10153,#10154,#10155,#10156,#10157,#10158,#10159,#10160,#10161,#10162,#10163,
#10164,#10165,#10166,#10167,#10168,#10169,#10170,#10171,#10172,#10173,#10174,
#10175,#10176,#10177,#10178,#10179,#10180,#10181,#10182,#10183,#10184,#10185,
#10186,#10187,#10188,#10189,#10190,#10191),.UNSPECIFIED.,.F.,.F.,(4,3,3,
3,3,3,3,3,3,3,3,3,3,3,3,3,3,3,3,3,3,3,3,3,3,3,3,3,3,3,3,3,3,3,3,3,3,3,3,
3,3,3,3,3,3,3,3,3,3,3,3,3,3,3,3,3,3,3,3,3,3,3,3,3,3,3,3,3,3,3,3,3,3,3,3,
3,3,3,3,3,3,3,4),(101.649820096463,101.752700226976,101.857939430541,101.896317224315,
101.976282183101,102.056152771205,102.135946508231,102.215680853322,102.295373218628,
102.375052437168,102.454728200956,102.534416232823,102.614132259934,102.693935822864,
102.773788547541,102.85375495719,102.895300726514,102.975265685301,103.055136273406,
103.134930010433,103.214664355524,103.294356720831,103.374035939372,103.453711703162,
103.533399735029,103.613115762141,103.692919325071,103.772772049749,103.8527384594,
103.894284228713,103.9742491875,104.054119775605,104.133913512632,104.213647857723,
104.29334022303,104.373019441571,104.452695205361,104.532383237229,104.61209926434,
104.691902827271,104.771755551949,104.851721961599,104.893267730912,104.973232689699,
105.053103277804,105.132897014831,105.212631359922,105.292323725229,105.37200294377,
105.451678707559,105.531366739427,105.611082766539,105.690886329469,105.770739054147,
105.850705463798,105.892251233112,105.972216191899,106.052086780004,106.131880517031,
106.211614862122,106.291307227429,106.370986445971,106.45066220976,106.530350241628,
106.610066268739,106.68986983167,106.769722556348,106.849688965998,106.891234735311,
106.971199694098,107.051070282203,107.130864019229,107.21059836432,107.290290729627,
107.369969948168,107.449645711957,107.529333743825,107.609049770937,107.688853333867,
107.768706058545,107.848672468195,107.89021823751,107.933005315593),
 .UNSPECIFIED.);
#121=B_SPLINE_CURVE_WITH_KNOTS('',3,(#10193,#10194,#10195,#10196,#10197,
#10198,#10199,#10200,#10201,#10202),.UNSPECIFIED.,.F.,.F.,(4,1,1,1,1,1,
1,4),(107.933011045732,108.889201739709,109.888185241908,110.887168744107,
111.886152246307,112.885135748506,113.884119250705,114.216183287294),
 .UNSPECIFIED.);
#122=B_SPLINE_CURVE_WITH_KNOTS('',3,(#10204,#10205,#10206,#10207,#10208,
#10209,#10210,#10211,#10212,#10213,#10214,#10215,#10216,#10217,#10218,#10219,
#10220,#10221,#10222,#10223,#10224,#10225,#10226,#10227,#10228,#10229,#10230,
#10231,#10232,#10233,#10234,#10235,#10236,#10237,#10238,#10239,#10240,#10241,
#10242,#10243,#10244,#10245,#10246,#10247,#10248,#10249,#10250,#10251,#10252,
#10253,#10254,#10255,#10256,#10257,#10258,#10259,#10260,#10261,#10262,#10263,
#10264,#10265,#10266,#10267,#10268,#10269,#10270,#10271,#10272,#10273,#10274,
#10275,#10276,#10277,#10278,#10279,#10280,#10281,#10282,#10283,#10284,#10285,
#10286,#10287,#10288,#10289,#10290,#10291,#10292,#10293,#10294,#10295,#10296,
#10297,#10298,#10299,#10300,#10301,#10302,#10303,#10304,#10305,#10306,#10307,
#10308,#10309,#10310,#10311,#10312,#10313,#10314,#10315,#10316,#10317,#10318,
#10319,#10320,#10321,#10322,#10323,#10324,#10325,#10326,#10327,#10328,#10329,
#10330,#10331,#10332,#10333,#10334,#10335,#10336,#10337,#10338,#10339,#10340,
#10341,#10342,#10343,#10344,#10345,#10346,#10347,#10348,#10349,#10350,#10351,
#10352,#10353,#10354,#10355,#10356,#10357,#10358,#10359,#10360,#10361,#10362,
#10363,#10364,#10365,#10366,#10367,#10368,#10369,#10370,#10371,#10372,#10373,
#10374,#10375,#10376,#10377,#10378,#10379,#10380,#10381,#10382,#10383,#10384,
#10385,#10386,#10387,#10388,#10389,#10390,#10391,#10392,#10393,#10394,#10395,
#10396,#10397,#10398,#10399,#10400,#10401,#10402,#10403,#10404,#10405,#10406,
#10407,#10408,#10409,#10410,#10411,#10412,#10413,#10414,#10415,#10416,#10417,
#10418,#10419,#10420,#10421,#10422,#10423,#10424,#10425,#10426,#10427,#10428,
#10429,#10430,#10431,#10432,#10433,#10434,#10435,#10436,#10437,#10438,#10439,
#10440,#10441,#10442,#10443,#10444,#10445,#10446,#10447,#10448,#10449,#10450),
 .UNSPECIFIED.,.F.,.F.,(4,3,3,3,3,3,3,3,3,3,3,3,3,3,3,3,3,3,3,3,3,3,3,3,
3,3,3,3,3,3,3,3,3,3,3,3,3,3,3,3,3,3,3,3,3,3,3,3,3,3,3,3,3,3,3,3,3,3,3,3,
3,3,3,3,3,3,3,3,3,3,3,3,3,3,3,3,3,3,3,3,3,3,4),(114.216190622772,114.299554639039,
114.3791579932,114.458764847072,114.538390929541,114.618051978097,114.69780744092,
114.777618197829,114.857543217377,114.883102752904,114.963067711691,115.042938299796,
115.122732036823,115.202466381914,115.28215874722,115.361837965761,115.441513729551,
115.521201761419,115.60091778853,115.68072135146,115.760574076138,115.840540485788,
115.882086255103,115.96205121389,116.041921801995,116.121715539022,116.201449884113,
116.281142249419,116.36082146796,116.44049723175,116.520185263617,116.599901290729,
116.679704853659,116.759557578337,116.839523987988,116.881069757302,116.961034716089,
117.040905304194,117.120699041221,117.200433386311,117.280125751618,117.359804970159,
117.439480733948,117.519168765816,117.598884792928,117.678688355858,117.758541080536,
117.838507490186,117.880053259501,117.960018218289,118.039888806393,118.11968254342,
118.199416888512,118.279109253818,118.35878847236,118.438464236149,118.518152268017,
118.597868295129,118.677671858059,118.757524582737,118.837490992388,118.879036761701,
118.959001720488,119.038872308593,119.11866604562,119.198400390711,119.278092756017,
119.357771974558,119.437447738347,119.517135770216,119.596851797327,119.676655360257,
119.756508084935,119.836474494585,119.8780202639,119.958699782841,120.039280820086,
120.119778432003,120.20020762007,120.280577914094,120.360913170741,120.441236174366,
120.499375929952),.UNSPECIFIED.);
#123=B_SPLINE_CURVE_WITH_KNOTS('',3,(#10452,#10453,#10454,#10455,#10456,
#10457,#10458,#10459,#10460,#10461),.UNSPECIFIED.,.F.,.F.,(4,1,1,1,1,1,
1,4),(120.499383484016,120.877003766099,121.875987268298,122.874970770497,
123.873954272696,124.872937774896,125.871921277095,126.782552527095),
 .UNSPECIFIED.);
#124=B_SPLINE_CURVE_WITH_KNOTS('',3,(#10463,#10464,#10465,#10466,#10467,
#10468,#10469,#10470,#10471,#10472,#10473,#10474,#10475,#10476,#10477,#10478,
#10479,#10480,#10481,#10482,#10483,#10484,#10485,#10486,#10487,#10488,#10489,
#10490,#10491,#10492,#10493,#10494,#10495,#10496,#10497,#10498,#10499,#10500,
#10501,#10502,#10503,#10504,#10505,#10506,#10507,#10508,#10509,#10510,#10511,
#10512,#10513,#10514,#10515,#10516,#10517,#10518,#10519,#10520,#10521,#10522,
#10523,#10524,#10525,#10526,#10527,#10528,#10529,#10530,#10531,#10532,#10533,
#10534,#10535,#10536,#10537,#10538,#10539,#10540,#10541,#10542,#10543,#10544,
#10545,#10546,#10547,#10548,#10549,#10550,#10551,#10552,#10553,#10554,#10555,
#10556,#10557,#10558,#10559,#10560,#10561,#10562,#10563,#10564,#10565,#10566,
#10567,#10568,#10569,#10570,#10571,#10572,#10573,#10574,#10575,#10576,#10577,
#10578,#10579,#10580,#10581,#10582,#10583,#10584,#10585,#10586,#10587,#10588,
#10589,#10590,#10591,#10592,#10593,#10594,#10595,#10596,#10597,#10598,#10599,
#10600,#10601,#10602,#10603,#10604,#10605,#10606,#10607,#10608,#10609,#10610,
#10611,#10612,#10613,#10614,#10615,#10616,#10617,#10618,#10619,#10620,#10621,
#10622,#10623,#10624,#10625,#10626,#10627,#10628,#10629,#10630,#10631,#10632,
#10633,#10634,#10635,#10636,#10637,#10638,#10639,#10640,#10641,#10642,#10643,
#10644,#10645,#10646,#10647,#10648,#10649,#10650,#10651,#10652,#10653,#10654,
#10655,#10656,#10657,#10658,#10659,#10660,#10661,#10662,#10663,#10664,#10665,
#10666,#10667,#10668,#10669,#10670,#10671,#10672,#10673,#10674,#10675,#10676,
#10677,#10678,#10679,#10680,#10681,#10682,#10683,#10684,#10685,#10686,#10687,
#10688,#10689,#10690,#10691,#10692,#10693,#10694,#10695,#10696,#10697,#10698,
#10699,#10700,#10701,#10702,#10703,#10704,#10705,#10706),.UNSPECIFIED.,
 .F.,.F.,(4,3,3,3,3,3,3,3,3,3,3,3,3,3,3,3,3,3,3,3,3,3,3,3,3,3,3,3,3,3,3,
3,3,3,3,3,3,3,3,3,3,3,3,3,3,3,3,3,3,3,3,3,3,3,3,3,3,3,3,3,3,3,3,3,3,3,3,
3,3,3,3,3,3,3,3,3,3,3,3,3,3,4),(126.782561237132,126.870904779294,126.950869738081,
127.030740326186,127.110534063213,127.190268408304,127.269960773611,127.349639992152,
127.429315755941,127.509003787809,127.588719814921,127.668523377851,127.748376102529,
127.82834251218,127.869888281493,127.94985324028,128.029723828385,128.109517565412,
128.189251910503,128.26894427581,128.348623494351,128.42829925814,128.507987290008,
128.587703317119,128.66750688005,128.747359604728,128.827326014378,128.868871783692,
128.948836742479,129.028707330584,129.10850106761,129.188235412701,129.267927778008,
129.347606996549,129.427282760338,129.506970792206,129.586686819317,129.666490382248,
129.746343106926,129.826309516576,129.867855285891,129.947820244679,130.027690832783,
130.10748456981,130.187218914902,130.266911280209,130.34659049875,130.42626626254,
130.505954294408,130.585670321519,130.66547388445,130.745326609128,130.825293018779,
130.866838788091,130.946803746878,131.026674334983,131.10646807201,131.186202417101,
131.265894782408,131.345574000949,131.425249764738,131.504937796606,131.584653823718,
131.664457386648,131.744310111326,131.824276520976,131.86582229029,131.945787249077,
132.025657837182,132.105451574209,132.1851859193,132.264878284606,132.344557503148,
132.424233266937,132.503921298804,132.583637325916,132.663440888846,132.743293613524,
132.823260023174,132.864805792489,132.979172254981,133.065746544311),
 .UNSPECIFIED.);
#125=B_SPLINE_CURVE_WITH_KNOTS('',3,(#10708,#10709,#10710,#10711,#10712,
#10713,#10714,#10715,#10716,#10717,#10718,#10719,#10720,#10721,#10722,#10723,
#10724,#10725,#10726,#10727,#10728,#10729,#10730,#10731,#10732,#10733,#10734,
#10735,#10736,#10737,#10738,#10739,#10740,#10741,#10742,#10743,#10744,#10745,
#10746,#10747,#10748,#10749,#10750,#10751,#10752,#10753,#10754,#10755,#10756,
#10757,#10758,#10759,#10760,#10761,#10762,#10763,#10764,#10765,#10766,#10767,
#10768,#10769,#10770,#10771,#10772,#10773,#10774,#10775,#10776,#10777,#10778,
#10779,#10780,#10781,#10782,#10783,#10784,#10785,#10786,#10787,#10788,#10789,
#10790,#10791,#10792,#10793,#10794,#10795,#10796,#10797,#10798,#10799,#10800,
#10801,#10802,#10803,#10804,#10805,#10806,#10807,#10808,#10809,#10810,#10811,
#10812,#10813,#10814,#10815,#10816,#10817,#10818,#10819,#10820,#10821,#10822,
#10823,#10824,#10825,#10826,#10827,#10828,#10829,#10830,#10831,#10832,#10833,
#10834,#10835,#10836,#10837,#10838,#10839,#10840,#10841,#10842,#10843,#10844,
#10845,#10846,#10847,#10848,#10849,#10850,#10851,#10852,#10853,#10854,#10855,
#10856,#10857,#10858,#10859,#10860,#10861,#10862,#10863,#10864,#10865,#10866,
#10867,#10868,#10869,#10870,#10871,#10872,#10873,#10874,#10875,#10876,#10877,
#10878,#10879,#10880,#10881,#10882,#10883,#10884,#10885,#10886,#10887,#10888,
#10889,#10890,#10891,#10892,#10893,#10894,#10895,#10896,#10897,#10898,#10899,
#10900,#10901,#10902,#10903,#10904,#10905,#10906,#10907,#10908,#10909,#10910,
#10911,#10912,#10913,#10914,#10915,#10916,#10917,#10918,#10919,#10920,#10921,
#10922,#10923,#10924,#10925,#10926,#10927,#10928,#10929,#10930,#10931,#10932,
#10933,#10934,#10935,#10936,#10937,#10938,#10939,#10940,#10941,#10942,#10943,
#10944,#10945,#10946,#10947,#10948,#10949,#10950,#10951),.UNSPECIFIED.,
 .F.,.F.,(4,3,3,3,3,3,3,3,3,3,3,3,3,3,3,3,3,3,3,3,3,3,3,3,3,3,3,3,3,3,3,
3,3,3,3,3,3,3,3,3,3,3,3,3,3,3,3,3,3,3,3,3,3,3,3,3,3,3,3,3,3,3,3,3,3,3,3,
3,3,3,3,3,3,3,3,3,3,3,3,3,3,4),(133.065746544471,133.144414831246,133.223020181614,
133.303116320748,133.381660781291,133.460201368281,133.538754623018,133.620013290935,
133.698682056643,133.781235675665,133.863789294688,133.943754253475,134.02362484158,
134.103418578607,134.183152923698,134.262845289004,134.342524507545,134.422200271334,
134.501888303202,134.581604330314,134.661407893244,134.741260617922,134.821227027572,
134.862772796887,134.942737755674,135.022608343779,135.102402080806,135.182136425896,
135.261828791203,135.341508009744,135.421183773533,135.500871805401,135.580587832512,
135.660391395442,135.74024412012,135.820210529771,135.861756299086,135.941721257874,
136.021591845978,136.101385583006,136.181119928097,136.260812293404,136.340491511945,
136.420167275735,136.499855307603,136.579571334715,136.659374897646,136.739227622324,
136.819194031975,136.860739801286,136.940704760073,137.020575348178,137.100369085205,
137.180103430296,137.259795795603,137.339475014144,137.419150777933,137.498838809801,
137.578554836913,137.658358399843,137.738211124521,137.818177534172,137.859723303485,
137.939688262272,138.019558850377,138.099352587403,138.179086932494,138.258779297802,
138.338458516343,138.418134280132,138.497822311999,138.577538339111,138.657341902041,
138.737194626718,138.817161036368,138.858706805684,138.943144794911,139.027438869103,
139.111535628609,139.195515746164,139.279334149676,139.34893185139),
 .UNSPECIFIED.);
#126=B_SPLINE_CURVE_WITH_KNOTS('',3,(#10953,#10954,#10955,#10956,#10957,
#10958,#10959,#10960,#10961,#10962,#10963,#10964,#10965,#10966,#10967,#10968,
#10969,#10970,#10971,#10972,#10973,#10974,#10975,#10976,#10977,#10978,#10979,
#10980,#10981,#10982,#10983,#10984,#10985,#10986,#10987,#10988,#10989,#10990,
#10991,#10992,#10993,#10994,#10995,#10996,#10997,#10998,#10999,#11000,#11001,
#11002,#11003,#11004,#11005,#11006,#11007,#11008,#11009,#11010,#11011,#11012,
#11013,#11014,#11015,#11016,#11017,#11018,#11019,#11020,#11021,#11022,#11023,
#11024,#11025,#11026,#11027,#11028,#11029,#11030,#11031,#11032,#11033,#11034,
#11035,#11036,#11037,#11038,#11039,#11040,#11041,#11042,#11043,#11044,#11045,
#11046,#11047,#11048,#11049,#11050,#11051,#11052,#11053,#11054,#11055,#11056,
#11057,#11058,#11059,#11060,#11061,#11062,#11063,#11064,#11065,#11066,#11067,
#11068,#11069,#11070,#11071,#11072,#11073,#11074,#11075,#11076,#11077,#11078,
#11079,#11080,#11081,#11082,#11083,#11084,#11085,#11086,#11087,#11088,#11089,
#11090,#11091,#11092,#11093,#11094,#11095,#11096,#11097,#11098,#11099,#11100,
#11101,#11102,#11103,#11104,#11105,#11106,#11107,#11108,#11109,#11110,#11111,
#11112,#11113,#11114,#11115,#11116,#11117,#11118,#11119,#11120,#11121,#11122,
#11123,#11124,#11125,#11126,#11127,#11128,#11129,#11130,#11131,#11132,#11133,
#11134,#11135,#11136,#11137,#11138,#11139,#11140,#11141,#11142,#11143,#11144,
#11145,#11146,#11147,#11148,#11149,#11150,#11151,#11152,#11153,#11154,#11155,
#11156,#11157,#11158,#11159,#11160,#11161,#11162,#11163,#11164,#11165,#11166,
#11167,#11168,#11169,#11170,#11171,#11172,#11173,#11174,#11175,#11176,#11177,
#11178,#11179,#11180,#11181,#11182,#11183,#11184,#11185,#11186,#11187,#11188,
#11189,#11190,#11191,#11192,#11193,#11194,#11195,#11196),.UNSPECIFIED.,
 .F.,.F.,(4,3,3,3,3,3,3,3,3,3,3,3,3,3,3,3,3,3,3,3,3,3,3,3,3,3,3,3,3,3,3,
3,3,3,3,3,3,3,3,3,3,3,3,3,3,3,3,3,3,3,3,3,3,3,3,3,3,3,3,3,3,3,3,3,3,3,3,
3,3,3,3,3,3,3,3,3,3,3,3,3,3,4),(139.348931851491,139.432079150989,139.515320103915,
139.600912654907,139.684429370585,139.771059839234,139.857690307883,139.93765526667,
140.017525854775,140.097319591802,140.177053936893,140.256746302201,140.336425520742,
140.416101284531,140.495789316399,140.575505343511,140.655308906441,140.735161631119,
140.81512804077,140.856673810082,140.936638768869,141.016509356974,141.096303094,
141.176037439091,141.255729804398,141.335409022939,141.415084786728,141.494772818596,
141.574488845707,141.654292408638,141.734145133316,141.814111542966,141.855657312281,
141.935622271068,142.015492859173,142.0952865962,142.175020941292,142.254713306599,
142.33439252514,142.41406828893,142.493756320798,142.573472347909,142.65327591084,
142.733128635518,142.813095045169,142.854640814481,142.934605773268,143.014476361373,
143.0942700984,143.174004443491,143.253696808799,143.33337602734,143.413051791129,
143.492739822997,143.572455850108,143.652259413038,143.732112137716,143.812078547367,
143.85362431668,143.933589275467,144.013459863571,144.093253600598,144.172987945689,
144.252680310997,144.332359529538,144.412035293327,144.491723325195,144.571439352307,
144.651242915237,144.731095639916,144.811062049566,144.852607818879,144.931490161362,
145.010277469427,145.08897511628,145.167622082638,145.24623491863,145.324830146253,
145.403451165995,145.482083209498,145.560786285368,145.63211715867),
 .UNSPECIFIED.);
#127=B_SPLINE_CURVE_WITH_KNOTS('',3,(#11198,#11199,#11200,#11201,#11202,
#11203,#11204,#11205,#11206,#11207,#11208),.UNSPECIFIED.,.F.,.F.,(4,1,1,
1,1,1,1,1,4),(145.63211715867,145.851591321078,146.850574823277,147.849558325476,
148.848541827676,149.847525329875,150.846508832074,151.845492334273,151.91530246585),
 .UNSPECIFIED.);
#128=B_SPLINE_CURVE_WITH_KNOTS('',3,(#11210,#11211,#11212,#11213,#11214,
#11215,#11216,#11217,#11218,#11219,#11220,#11221,#11222,#11223,#11224,#11225,
#11226,#11227,#11228,#11229,#11230,#11231,#11232,#11233,#11234,#11235,#11236,
#11237,#11238,#11239,#11240,#11241,#11242,#11243,#11244,#11245,#11246,#11247,
#11248,#11249,#11250,#11251,#11252,#11253,#11254,#11255,#11256,#11257,#11258,
#11259,#11260,#11261,#11262,#11263,#11264,#11265,#11266,#11267,#11268,#11269,
#11270,#11271,#11272,#11273,#11274,#11275,#11276,#11277,#11278,#11279,#11280,
#11281,#11282,#11283,#11284,#11285,#11286,#11287,#11288,#11289,#11290,#11291,
#11292,#11293,#11294,#11295,#11296,#11297,#11298,#11299,#11300,#11301,#11302,
#11303,#11304,#11305,#11306,#11307,#11308,#11309,#11310,#11311,#11312,#11313,
#11314,#11315,#11316,#11317,#11318,#11319,#11320,#11321,#11322,#11323,#11324,
#11325,#11326,#11327,#11328,#11329,#11330,#11331,#11332,#11333,#11334,#11335,
#11336,#11337,#11338,#11339,#11340,#11341,#11342,#11343,#11344,#11345,#11346,
#11347,#11348,#11349,#11350,#11351,#11352,#11353,#11354,#11355,#11356,#11357,
#11358,#11359,#11360,#11361,#11362,#11363,#11364,#11365,#11366,#11367,#11368,
#11369,#11370,#11371,#11372,#11373,#11374,#11375,#11376,#11377,#11378,#11379,
#11380,#11381,#11382,#11383,#11384,#11385,#11386,#11387,#11388,#11389,#11390,
#11391,#11392,#11393,#11394,#11395,#11396,#11397,#11398,#11399,#11400,#11401,
#11402,#11403,#11404,#11405,#11406,#11407,#11408,#11409,#11410,#11411,#11412,
#11413,#11414,#11415,#11416,#11417,#11418,#11419,#11420,#11421,#11422,#11423,
#11424,#11425,#11426,#11427,#11428,#11429,#11430,#11431,#11432,#11433,#11434,
#11435,#11436,#11437,#11438,#11439,#11440,#11441,#11442,#11443,#11444,#11445,
#11446,#11447,#11448,#11449,#11450,#11451,#11452,#11453),.UNSPECIFIED.,
 .F.,.F.,(4,3,3,3,3,3,3,3,3,3,3,3,3,3,3,3,3,3,3,3,3,3,3,3,3,3,3,3,3,3,3,
3,3,3,3,3,3,3,3,3,3,3,3,3,3,3,3,3,3,3,3,3,3,3,3,3,3,3,3,3,3,3,3,3,3,3,3,
3,3,3,3,3,3,3,3,3,3,3,3,3,3,4),(151.91530246585,151.994451245667,152.073510801261,
152.152499317386,152.231434913233,152.310343716248,152.389240399023,152.468141288704,
152.547062713042,152.626066282013,152.705113451247,152.784277825896,152.844475836472,
152.924440795259,153.004311383364,153.08410512039,153.163839465482,153.243531830788,
153.323211049329,153.402886813118,153.482574844986,153.562290872097,153.642094435027,
153.721947159705,153.801913569355,153.843459338671,153.923424297459,154.003294885564,
154.083088622591,154.162822967682,154.242515332989,154.32219455153,154.401870315319,
154.481558347188,154.5612743743,154.641077937231,154.720930661909,154.800897071559,
154.842442840871,154.922407799658,155.002278387763,155.08207212479,155.161806469881,
155.241498835188,155.321178053729,155.400853817518,155.480541849386,155.560257876498,
155.640061439428,155.719914164106,155.799880573757,155.84142634307,155.921391301857,
156.001261889962,156.081055626988,156.160789972079,156.240482337386,156.320161555927,
156.399837319716,156.479525351584,156.559241378695,156.639044941626,156.718897666304,
156.798864075954,156.840409845269,156.920374804056,157.000245392161,157.080039129188,
157.159773474279,157.239465839586,157.319145058127,157.398820821916,157.478508853784,
157.558224880895,157.638028443826,157.717881168503,157.797847578154,157.839393347468,
157.931101851476,158.022495910503,158.113268253516,158.198487526203),
 .UNSPECIFIED.);
#129=B_SPLINE_CURVE_WITH_KNOTS('',3,(#11455,#11456,#11457,#11458,#11459,
#11460,#11461,#11462,#11463,#11464),.UNSPECIFIED.,.F.,.F.,(4,1,1,1,1,1,
1,4),(158.198487773029,158.838376849667,159.837360351866,160.836343854066,
161.835327356265,162.834310858464,163.833294360663,164.481673080209),
 .UNSPECIFIED.);
#130=B_SPLINE_CURVE_WITH_KNOTS('',3,(#11466,#11467,#11468,#11469,#11470,
#11471,#11472,#11473,#11474,#11475,#11476,#11477,#11478,#11479,#11480,#11481,
#11482,#11483,#11484,#11485,#11486,#11487,#11488,#11489,#11490,#11491,#11492,
#11493,#11494,#11495,#11496,#11497,#11498,#11499,#11500,#11501,#11502,#11503,
#11504,#11505,#11506,#11507,#11508,#11509,#11510,#11511,#11512,#11513,#11514,
#11515,#11516,#11517,#11518,#11519,#11520,#11521,#11522,#11523,#11524,#11525,
#11526,#11527,#11528,#11529,#11530,#11531,#11532,#11533,#11534,#11535,#11536,
#11537,#11538,#11539,#11540,#11541,#11542,#11543,#11544,#11545,#11546,#11547,
#11548,#11549,#11550,#11551,#11552,#11553,#11554,#11555,#11556,#11557,#11558,
#11559,#11560,#11561,#11562,#11563,#11564,#11565,#11566,#11567,#11568,#11569,
#11570,#11571,#11572,#11573,#11574,#11575,#11576,#11577,#11578,#11579,#11580,
#11581,#11582,#11583,#11584,#11585,#11586,#11587,#11588,#11589,#11590,#11591,
#11592,#11593,#11594,#11595,#11596,#11597,#11598,#11599,#11600,#11601,#11602,
#11603,#11604,#11605,#11606,#11607,#11608,#11609,#11610,#11611,#11612,#11613,
#11614,#11615,#11616,#11617,#11618,#11619,#11620,#11621,#11622,#11623,#11624,
#11625,#11626,#11627,#11628,#11629,#11630,#11631,#11632,#11633,#11634,#11635,
#11636,#11637,#11638,#11639,#11640,#11641,#11642,#11643,#11644,#11645,#11646,
#11647,#11648,#11649,#11650,#11651,#11652,#11653,#11654,#11655,#11656,#11657,
#11658,#11659,#11660,#11661,#11662,#11663,#11664,#11665,#11666,#11667,#11668,
#11669,#11670,#11671,#11672,#11673,#11674,#11675,#11676,#11677,#11678,#11679,
#11680,#11681,#11682,#11683,#11684,#11685,#11686,#11687,#11688,#11689,#11690,
#11691,#11692,#11693,#11694,#11695,#11696,#11697,#11698,#11699,#11700,#11701,
#11702,#11703,#11704,#11705,#11706,#11707,#11708,#11709),.UNSPECIFIED.,
 .F.,.F.,(4,3,3,3,3,3,3,3,3,3,3,3,3,3,3,3,3,3,3,3,3,3,3,3,3,3,3,3,3,3,3,
3,3,3,3,3,3,3,3,3,3,3,3,3,3,3,3,3,3,3,3,3,3,3,3,3,3,3,3,3,3,3,3,3,3,3,3,
3,3,3,3,3,3,3,3,3,3,3,3,3,3,4),(164.481673325019,164.573090933397,164.66493832906,
164.757357139414,164.832277862862,164.91224282165,164.992113409754,165.071907146782,
165.151641491873,165.23133385718,165.311013075721,165.390688839511,165.470376871379,
165.550092898491,165.629896461422,165.7097491861,165.789715595751,165.831261365061,
165.911226323848,165.991096911953,166.07089064898,166.150624994072,166.230317359378,
166.30999657792,166.389672341709,166.469360373577,166.549076400689,166.628879963619,
166.708732688298,166.788699097948,166.830244867261,166.910209826048,166.990080414153,
167.06987415118,167.149608496271,167.229300861577,167.308980080119,167.388655843908,
167.468343875776,167.548059902887,167.627863465818,167.707716190495,167.787682600146,
167.82922836946,167.909193328247,167.989063916352,168.068857653378,168.148591998469,
168.228284363776,168.307963582317,168.387639346106,168.467327377974,168.547043405086,
168.626846968016,168.706699692694,168.786666102344,168.828211871659,168.908176830446,
168.988047418551,169.067841155578,169.147575500669,169.227267865975,169.306947084517,
169.386622848306,169.466310880174,169.546026907285,169.625830470216,169.705683194894,
169.785649604544,169.827195373858,169.906442099061,169.985594953595,170.064672086523,
170.143691578133,170.222677307682,170.301646466472,170.380615335551,170.45960019336,
170.53866168693,170.617762731622,170.696978651885,170.764858387389),
 .UNSPECIFIED.);
#131=B_SPLINE_CURVE_WITH_KNOTS('',3,(#11711,#11712,#11713,#11714,#11715,
#11716,#11717,#11718,#11719,#11720,#11721,#11722),.UNSPECIFIED.,.F.,.F.,
(4,2,1,1,1,1,1,1,4),(170.764858387389,170.826178876057,171.825162378256,
172.824145880456,173.823129382655,174.822112884854,175.821096387053,176.820079889252,
177.048043694568),.UNSPECIFIED.);
#132=B_SPLINE_CURVE_WITH_KNOTS('',3,(#11724,#11725,#11726,#11727,#11728,
#11729,#11730,#11731,#11732,#11733),.UNSPECIFIED.,.F.,.F.,(4,1,1,1,1,1,
1,4),(177.048043694568,177.819063391451,178.818046893651,179.81703039585,
180.816013898049,181.814997400248,182.813980902447,183.331229001748),
 .UNSPECIFIED.);
#133=B_SPLINE_CURVE_WITH_KNOTS('',3,(#11735,#11736,#11737,#11738,#11739,
#11740,#11741,#11742,#11743,#11744),.UNSPECIFIED.,.F.,.F.,(4,1,1,1,1,1,
1,4),(183.331229001748,183.812964404646,184.811947906846,185.810931409045,
186.809914911244,187.808898413443,188.807881915642,189.614410347781),
 .UNSPECIFIED.);
#134=B_SPLINE_CURVE_WITH_KNOTS('',3,(#11746,#11747,#11748,#11749,#11750,
#11751,#11752,#11753,#11754,#11755,#11756,#11757,#11758,#11759,#11760,#11761,
#11762,#11763,#11764,#11765,#11766,#11767,#11768,#11769,#11770,#11771,#11772,
#11773,#11774,#11775,#11776,#11777,#11778,#11779,#11780,#11781,#11782,#11783,
#11784,#11785,#11786,#11787,#11788,#11789,#11790,#11791,#11792,#11793,#11794,
#11795,#11796,#11797,#11798,#11799,#11800,#11801,#11802,#11803,#11804,#11805,
#11806,#11807,#11808,#11809,#11810,#11811,#11812,#11813,#11814,#11815,#11816,
#11817,#11818,#11819,#11820,#11821,#11822,#11823,#11824,#11825,#11826,#11827,
#11828,#11829,#11830,#11831,#11832,#11833,#11834,#11835,#11836,#11837,#11838,
#11839,#11840,#11841,#11842,#11843,#11844,#11845,#11846,#11847,#11848,#11849,
#11850,#11851,#11852,#11853,#11854,#11855,#11856,#11857,#11858,#11859,#11860,
#11861,#11862,#11863,#11864,#11865,#11866,#11867,#11868,#11869,#11870,#11871,
#11872,#11873,#11874,#11875,#11876,#11877,#11878,#11879,#11880,#11881,#11882,
#11883,#11884,#11885,#11886,#11887,#11888,#11889,#11890,#11891,#11892,#11893,
#11894,#11895,#11896,#11897,#11898,#11899,#11900,#11901,#11902,#11903,#11904,
#11905,#11906,#11907,#11908,#11909,#11910,#11911,#11912,#11913,#11914,#11915,
#11916,#11917,#11918,#11919,#11920,#11921,#11922,#11923,#11924,#11925,#11926,
#11927,#11928,#11929,#11930,#11931,#11932,#11933,#11934,#11935,#11936,#11937,
#11938,#11939,#11940,#11941,#11942,#11943,#11944,#11945,#11946,#11947,#11948,
#11949,#11950,#11951,#11952,#11953,#11954,#11955,#11956,#11957,#11958,#11959,
#11960,#11961,#11962,#11963,#11964,#11965,#11966,#11967,#11968,#11969,#11970,
#11971,#11972,#11973,#11974,#11975,#11976,#11977,#11978,#11979,#11980,#11981,
#11982,#11983,#11984,#11985,#11986,#11987,#11988,#11989),.UNSPECIFIED.,
 .F.,.F.,(4,3,3,3,3,3,3,3,3,3,3,3,3,3,3,3,3,3,3,3,3,3,3,3,3,3,3,3,3,3,3,
3,3,3,3,3,3,3,3,3,3,3,3,3,3,3,3,3,3,3,3,3,3,3,3,3,3,3,3,3,3,3,3,3,3,3,3,
3,3,3,3,3,3,3,3,3,3,3,3,3,3,4),(189.614414308927,189.731351580901,189.806865417841,
189.886830376629,189.966700964734,190.046494701761,190.126229046853,190.20592141216,
190.285600630701,190.365276394491,190.444964426359,190.524680453471,190.604484016402,
190.68433674108,190.764303150731,190.805848920041,190.885813878828,190.965684466933,
191.04547820396,191.125212549051,191.204904914357,191.284584132899,191.364259896688,
191.443947928555,191.523663955667,191.603467518597,191.683320243275,191.763286652926,
191.80483242224,191.884797381027,191.964667969132,192.044461706159,192.12419605125,
192.203888416556,192.283567635098,192.363243398887,192.442931430754,192.522647457866,
192.602451020796,192.682303745474,192.762270155124,192.803815924439,192.883780883226,
192.963651471331,193.043445208358,193.123179553449,193.202871918756,193.282551137297,
193.362226901086,193.441914932954,193.521630960065,193.601434522996,193.681287247674,
193.761253657324,193.802799426638,193.882764385425,193.96263497353,194.042428710557,
194.122163055648,194.201855420955,194.281534639496,194.361210403285,194.440898435153,
194.520614462264,194.600418025195,194.680270749873,194.760237159523,194.801782928837,
194.881747887624,194.961618475729,195.041412212755,195.121146557846,195.200838923153,
195.280518141694,195.360193905483,195.439881937351,195.519597964462,195.599401527393,
195.679254252071,195.759220661721,195.800766431036,195.897599616107),
 .UNSPECIFIED.);
#135=B_SPLINE_CURVE_WITH_KNOTS('',3,(#11991,#11992,#11993,#11994,#11995,
#11996,#11997,#11998,#11999,#12000),.UNSPECIFIED.,.F.,.F.,(4,1,1,1,1,1,
1,4),(195.897608625592,196.799749933236,197.798733435435,198.797716937634,
199.796700439833,200.795683942032,201.794667444231,202.180777541694),
 .UNSPECIFIED.);
#136=B_SPLINE_CURVE_WITH_KNOTS('',3,(#12002,#12003,#12004,#12005,#12006,
#12007,#12008,#12009,#12010,#12011,#12012,#12013,#12014,#12015,#12016,#12017,
#12018,#12019,#12020,#12021,#12022,#12023,#12024,#12025,#12026,#12027,#12028,
#12029,#12030,#12031,#12032,#12033,#12034,#12035,#12036,#12037,#12038,#12039,
#12040,#12041,#12042,#12043,#12044,#12045,#12046,#12047,#12048,#12049,#12050,
#12051,#12052,#12053,#12054,#12055,#12056,#12057,#12058,#12059,#12060,#12061,
#12062,#12063,#12064,#12065,#12066,#12067,#12068,#12069,#12070,#12071,#12072,
#12073,#12074,#12075,#12076,#12077,#12078,#12079,#12080,#12081,#12082,#12083,
#12084,#12085,#12086,#12087,#12088,#12089,#12090,#12091,#12092,#12093,#12094,
#12095,#12096,#12097,#12098,#12099,#12100,#12101,#12102,#12103,#12104,#12105,
#12106,#12107,#12108,#12109,#12110,#12111,#12112,#12113,#12114,#12115,#12116,
#12117,#12118,#12119,#12120,#12121,#12122,#12123,#12124,#12125,#12126,#12127,
#12128,#12129,#12130,#12131,#12132,#12133,#12134,#12135,#12136,#12137,#12138,
#12139,#12140,#12141,#12142,#12143,#12144,#12145,#12146,#12147,#12148,#12149,
#12150,#12151,#12152,#12153,#12154,#12155,#12156,#12157,#12158,#12159,#12160,
#12161,#12162,#12163,#12164,#12165,#12166,#12167,#12168,#12169,#12170,#12171,
#12172,#12173,#12174,#12175,#12176,#12177,#12178,#12179,#12180,#12181,#12182,
#12183,#12184,#12185,#12186,#12187,#12188,#12189,#12190,#12191,#12192,#12193,
#12194,#12195,#12196,#12197,#12198,#12199,#12200,#12201,#12202,#12203,#12204,
#12205,#12206,#12207,#12208,#12209,#12210,#12211,#12212,#12213,#12214,#12215,
#12216,#12217,#12218,#12219,#12220,#12221,#12222,#12223,#12224,#12225,#12226,
#12227,#12228,#12229,#12230,#12231,#12232,#12233,#12234,#12235,#12236,#12237,
#12238,#12239,#12240,#12241,#12242,#12243,#12244,#12245,#12246,#12247,#12248),
 .UNSPECIFIED.,.F.,.F.,(4,3,3,3,3,3,3,3,3,3,3,3,3,3,3,3,3,3,3,3,3,3,3,3,
3,3,3,3,3,3,3,3,3,3,3,3,3,3,3,3,3,3,3,3,3,3,3,3,3,3,3,3,3,3,3,3,3,3,3,3,
3,3,3,3,3,3,3,3,3,3,3,3,3,3,3,3,3,3,3,3,3,3,4),(202.180784923286,202.261270285153,
202.341767965932,202.422292615556,202.502858897515,202.583532018821,202.664264123885,
202.745126086351,202.793650946431,202.873615905218,202.953486493322,203.033280230349,
203.11301457544,203.192706940747,203.272386159288,203.352061923077,203.431749954945,
203.511465982056,203.591269544986,203.671122269664,203.751088679314,203.79263444863,
203.872599407417,203.952469995522,204.032263732548,204.111998077639,204.191690442946,
204.271369661487,204.351045425276,204.430733457144,204.510449484255,204.590253047186,
204.670105771864,204.750072181514,204.791617950829,204.871582909616,204.951453497721,
205.031247234748,205.110981579839,205.190673945146,205.270353163687,205.350028927476,
205.429716959344,205.509432986456,205.589236549387,205.669089274065,205.749055683715,
205.790601453028,205.870566411815,205.95043699992,206.030230736947,206.109965082037,
206.189657447344,206.269336665885,206.349012429674,206.428700461542,206.508416488653,
206.588220051583,206.668072776261,206.748039185911,206.789584955227,206.869549914014,
206.949420502119,207.029214239145,207.108948584236,207.188640949543,207.268320168084,
207.347995931873,207.427683963741,207.507399990853,207.587203553783,207.667056278461,
207.747022688111,207.788568457426,207.8683838667,207.948070824655,208.027682813139,
208.107235768938,208.186745588199,208.266236013343,208.345714799917,208.425214991925,
208.463970230466),.UNSPECIFIED.);
#137=B_SPLINE_CURVE_WITH_KNOTS('',3,(#12250,#12251,#12252,#12253,#12254,
#12255,#12256,#12257,#12258,#12259),.UNSPECIFIED.,.F.,.F.,(4,1,1,1,1,1,
1,4),(208.463977261698,208.787551959626,209.786535461825,210.785518964024,
211.784502466223,212.783485968422,213.782469470621,214.747150895081),
 .UNSPECIFIED.);
#138=B_SPLINE_CURVE_WITH_KNOTS('',3,(#12261,#12262,#12263,#12264,#12265,
#12266,#12267,#12268,#12269,#12270,#12271,#12272,#12273,#12274,#12275,#12276,
#12277,#12278,#12279,#12280,#12281,#12282,#12283,#12284,#12285,#12286,#12287,
#12288,#12289,#12290,#12291,#12292,#12293,#12294,#12295,#12296,#12297,#12298,
#12299,#12300,#12301,#12302,#12303,#12304,#12305,#12306,#12307,#12308,#12309,
#12310,#12311,#12312,#12313,#12314,#12315,#12316,#12317,#12318,#12319,#12320,
#12321,#12322,#12323,#12324,#12325,#12326,#12327,#12328,#12329,#12330,#12331,
#12332,#12333,#12334,#12335,#12336,#12337,#12338,#12339,#12340,#12341,#12342,
#12343,#12344,#12345,#12346,#12347,#12348,#12349,#12350,#12351,#12352,#12353,
#12354,#12355,#12356,#12357,#12358,#12359,#12360,#12361,#12362,#12363,#12364,
#12365,#12366,#12367,#12368,#12369,#12370,#12371,#12372,#12373,#12374,#12375,
#12376,#12377,#12378,#12379,#12380,#12381,#12382,#12383,#12384,#12385,#12386,
#12387,#12388,#12389,#12390,#12391,#12392,#12393,#12394,#12395,#12396,#12397,
#12398,#12399,#12400,#12401,#12402,#12403,#12404,#12405,#12406,#12407,#12408,
#12409,#12410,#12411,#12412,#12413,#12414,#12415,#12416,#12417,#12418,#12419,
#12420,#12421,#12422,#12423,#12424,#12425,#12426,#12427,#12428,#12429,#12430,
#12431,#12432,#12433,#12434,#12435,#12436,#12437,#12438,#12439,#12440,#12441,
#12442,#12443,#12444,#12445,#12446,#12447,#12448,#12449,#12450,#12451,#12452,
#12453,#12454,#12455,#12456,#12457,#12458,#12459,#12460,#12461,#12462,#12463,
#12464,#12465,#12466,#12467,#12468,#12469,#12470,#12471,#12472,#12473,#12474,
#12475,#12476,#12477,#12478,#12479,#12480,#12481,#12482,#12483,#12484,#12485,
#12486,#12487,#12488,#12489,#12490,#12491,#12492,#12493,#12494,#12495,#12496,
#12497,#12498,#12499,#12500,#12501,#12502,#12503,#12504,#12505,#12506,#12507),
 .UNSPECIFIED.,.F.,.F.,(4,3,3,3,3,3,3,3,3,3,3,3,3,3,3,3,3,3,3,3,3,3,3,3,
3,3,3,3,3,3,3,3,3,3,3,3,3,3,3,3,3,3,3,3,3,3,3,3,3,3,3,3,3,3,3,3,3,3,3,3,
3,3,3,3,3,3,3,3,3,3,3,3,3,3,3,3,3,3,3,3,3,3,4),(214.747155537646,214.781452972821,
214.861417931608,214.941288519713,215.02108225674,215.100816601831,215.180508967138,
215.260188185679,215.339863949469,215.419551981337,215.499268008448,215.579071571379,
215.658924296057,215.738890705707,215.78043647502,215.860401433807,215.940272021912,
216.020065758939,216.09980010403,216.179492469337,216.259171687878,216.338847451667,
216.418535483535,216.498251510646,216.578055073577,216.657907798255,216.737874207905,
216.779419977219,216.859384936006,216.939255524111,217.019049261138,217.098783606229,
217.178475971535,217.258155190077,217.337830953866,217.417518985733,217.497235012845,
217.577038575775,217.656891300453,217.736857710104,217.778403479418,217.858368438205,
217.93823902631,218.018032763337,218.097767108428,218.177459473735,218.257138692276,
218.336814456065,218.416502487933,218.496218515044,218.576022077975,218.655874802653,
218.735841212303,218.777386981617,218.857351940404,218.937222528509,219.017016265535,
219.096750610627,219.176442975933,219.256122194474,219.335797958263,219.415485990131,
219.495202017243,219.575005580173,219.654858304851,219.734824714501,219.776370483816,
219.856335442603,219.936206030708,220.015999767735,220.095734112826,220.175426478133,
220.255105696675,220.334781460464,220.414469492332,220.494185519444,220.573989082374,
220.653841807052,220.733808216703,220.775353986016,220.87922915492,220.981055161892,
221.03034077524),.UNSPECIFIED.);
#139=B_SPLINE_CURVE_WITH_KNOTS('',3,(#12509,#12510,#12511,#12512,#12513,
#12514,#12515,#12516,#12517,#12518),.UNSPECIFIED.,.F.,.F.,(4,1,1,1,1,1,
1,4),(221.030340844825,221.774337488215,222.773320990414,223.772304492613,
224.771287994812,225.770271497011,226.76925499921,227.313526152005),
 .UNSPECIFIED.);
#140=B_SPLINE_CURVE_WITH_KNOTS('',3,(#12520,#12521,#12522,#12523,#12524,
#12525,#12526,#12527,#12528,#12529),.UNSPECIFIED.,.F.,.F.,(4,1,1,1,1,1,
1,4),(227.313526152005,227.76823850141,228.767222003609,229.766205505808,
230.765189008007,231.764172510206,232.763156012406,233.596711459184),
 .UNSPECIFIED.);
#141=B_SPLINE_CURVE_WITH_KNOTS('',3,(#12531,#12532,#12533,#12534,#12535,
#12536,#12537,#12538,#12539,#12540,#12541),.UNSPECIFIED.,.F.,.F.,(4,1,1,
1,1,1,1,1,4),(233.596711459184,233.762139514605,234.761123016804,235.760106519003,
236.759090021202,237.758073523401,238.7570570256,239.7560405278,239.879896766364),
 .UNSPECIFIED.);
#142=B_SPLINE_CURVE_WITH_KNOTS('',3,(#12543,#12544,#12545,#12546,#12547,
#12548,#12549,#12550,#12551,#12552,#12553,#12554,#12555,#12556,#12557,#12558,
#12559,#12560,#12561,#12562,#12563,#12564,#12565,#12566,#12567,#12568,#12569,
#12570,#12571,#12572,#12573,#12574,#12575,#12576,#12577,#12578,#12579,#12580,
#12581,#12582,#12583,#12584,#12585,#12586,#12587,#12588,#12589,#12590,#12591,
#12592,#12593,#12594,#12595,#12596,#12597,#12598,#12599,#12600,#12601,#12602,
#12603,#12604,#12605,#12606,#12607,#12608,#12609,#12610,#12611,#12612,#12613,
#12614,#12615,#12616,#12617,#12618,#12619,#12620,#12621,#12622,#12623,#12624,
#12625,#12626,#12627,#12628,#12629,#12630,#12631,#12632,#12633,#12634,#12635,
#12636,#12637,#12638,#12639,#12640,#12641,#12642,#12643,#12644,#12645,#12646,
#12647,#12648,#12649,#12650,#12651,#12652,#12653,#12654,#12655,#12656,#12657,
#12658,#12659,#12660,#12661,#12662,#12663,#12664,#12665,#12666,#12667,#12668,
#12669,#12670,#12671,#12672,#12673,#12674,#12675,#12676,#12677,#12678,#12679,
#12680,#12681,#12682,#12683,#12684,#12685,#12686,#12687,#12688,#12689,#12690,
#12691,#12692,#12693,#12694,#12695,#12696,#12697,#12698,#12699,#12700,#12701,
#12702,#12703,#12704,#12705,#12706,#12707,#12708,#12709,#12710,#12711,#12712,
#12713,#12714,#12715,#12716,#12717,#12718,#12719,#12720,#12721,#12722,#12723,
#12724,#12725,#12726,#12727,#12728,#12729,#12730,#12731,#12732,#12733,#12734,
#12735,#12736,#12737,#12738,#12739,#12740,#12741,#12742,#12743,#12744,#12745,
#12746,#12747,#12748,#12749,#12750,#12751,#12752,#12753,#12754,#12755,#12756,
#12757,#12758,#12759,#12760,#12761,#12762,#12763,#12764,#12765,#12766,#12767,
#12768,#12769,#12770,#12771,#12772,#12773,#12774,#12775,#12776,#12777,#12778,
#12779,#12780,#12781,#12782,#12783,#12784,#12785,#12786),.UNSPECIFIED.,
 .F.,.F.,(4,3,3,3,3,3,3,3,3,3,3,3,3,3,3,3,3,3,3,3,3,3,3,3,3,3,3,3,3,3,3,
3,3,3,3,3,3,3,3,3,3,3,3,3,3,3,3,3,3,3,3,3,3,3,3,3,3,3,3,3,3,3,3,3,3,3,3,
3,3,3,3,3,3,3,3,3,3,3,3,3,3,4),(239.879896766364,239.958682331775,240.03738738754,
240.116030307585,240.195904522887,240.274488338953,240.353068882816,240.431662673636,
240.512503012727,240.591212968301,240.67311849915,240.755024029999,240.834988988786,
240.914859576891,240.994653313918,241.074387659009,241.154080024316,241.233759242857,
241.313435006646,241.393123038514,241.472839065625,241.552642628555,241.632495353233,
241.712461762884,241.754007532198,241.833972490985,241.91384307909,241.993636816117,
242.073371161208,242.153063526515,242.232742745056,242.312418508845,242.392106540713,
242.471822567825,242.551626130756,242.631478855433,242.711445265084,242.752991034397,
242.832955993184,242.912826581289,242.992620318316,243.072354663407,243.152047028714,
243.231726247255,243.311402011045,243.391090042912,243.470806070024,243.550609632955,
243.630462357633,243.710428767283,243.751974536596,243.831939495383,243.911810083488,
243.991603820514,244.071338165605,244.151030530912,244.230709749453,244.310385513242,
244.39007354511,244.469789572222,244.549593135152,244.629445859829,244.70941226948,
244.750958038795,244.830922997583,244.910793585687,244.990587322714,245.070321667805,
245.150014033113,245.229693251654,245.309369015444,245.389057047312,245.468773074424,
245.548576637355,245.628429362033,245.708395771684,245.749941540995,245.838109597556,
245.925942288221,246.013563054025,246.100834313321,246.163081868327),
 .UNSPECIFIED.);
#143=B_SPLINE_CURVE_WITH_KNOTS('',3,(#12788,#12789,#12790,#12791,#12792,
#12793,#12794,#12795,#12796,#12797),.UNSPECIFIED.,.F.,.F.,(4,1,1,1,1,1,
1,4),(246.163082073543,246.748925043194,247.747908545393,248.746892047592,
249.745875549791,250.74485905199,251.74384255419,252.446267380723),
 .UNSPECIFIED.);
#144=B_SPLINE_CURVE_WITH_KNOTS('',3,(#12799,#12800,#12801,#12802,#12803,
#12804,#12805,#12806,#12807,#12808,#12809,#12810,#12811,#12812,#12813,#12814,
#12815,#12816,#12817,#12818,#12819,#12820,#12821,#12822,#12823,#12824,#12825,
#12826,#12827,#12828,#12829,#12830,#12831,#12832,#12833,#12834,#12835,#12836,
#12837,#12838,#12839,#12840,#12841,#12842,#12843,#12844,#12845,#12846,#12847,
#12848,#12849,#12850,#12851,#12852,#12853,#12854,#12855,#12856,#12857,#12858,
#12859,#12860,#12861,#12862,#12863,#12864,#12865,#12866,#12867,#12868,#12869,
#12870,#12871,#12872,#12873,#12874,#12875,#12876,#12877,#12878,#12879,#12880,
#12881,#12882,#12883,#12884,#12885,#12886,#12887,#12888,#12889,#12890,#12891,
#12892,#12893,#12894,#12895,#12896,#12897,#12898,#12899,#12900,#12901,#12902,
#12903,#12904,#12905,#12906,#12907,#12908,#12909,#12910,#12911,#12912,#12913,
#12914,#12915,#12916,#12917,#12918,#12919,#12920,#12921,#12922,#12923,#12924,
#12925,#12926,#12927,#12928,#12929,#12930,#12931,#12932,#12933,#12934,#12935,
#12936,#12937,#12938,#12939,#12940,#12941,#12942,#12943,#12944,#12945,#12946,
#12947,#12948,#12949,#12950,#12951,#12952,#12953,#12954,#12955,#12956,#12957,
#12958,#12959,#12960,#12961,#12962,#12963,#12964,#12965,#12966,#12967,#12968,
#12969,#12970,#12971,#12972,#12973,#12974,#12975,#12976,#12977,#12978,#12979,
#12980,#12981,#12982,#12983,#12984,#12985,#12986,#12987,#12988,#12989,#12990,
#12991,#12992,#12993,#12994,#12995,#12996,#12997,#12998,#12999,#13000,#13001,
#13002,#13003,#13004,#13005,#13006,#13007,#13008,#13009,#13010,#13011,#13012,
#13013,#13014,#13015,#13016,#13017,#13018,#13019,#13020,#13021,#13022,#13023,
#13024,#13025,#13026,#13027,#13028,#13029,#13030,#13031,#13032,#13033,#13034,
#13035,#13036,#13037,#13038,#13039,#13040,#13041,#13042),.UNSPECIFIED.,
 .F.,.F.,(4,3,3,3,3,3,3,3,3,3,3,3,3,3,3,3,3,3,3,3,3,3,3,3,3,3,3,3,3,3,3,
3,3,3,3,3,3,3,3,3,3,3,3,3,3,3,3,3,3,3,3,3,3,3,3,3,3,3,3,3,3,3,3,3,3,3,3,
3,3,3,3,3,3,3,3,3,3,3,3,3,3,4),(252.446267557126,252.542602672679,252.642714364534,
252.742826056389,252.822791015176,252.902661603281,252.982455340307,253.062189685399,
253.141882050706,253.221561269247,253.301237033036,253.380925064903,253.460641092015,
253.540444654945,253.620297379623,253.700263789274,253.741809558588,253.821774517375,
253.90164510548,253.981438842507,254.061173187598,254.140865552905,254.220544771446,
254.300220535235,254.379908567103,254.459624594215,254.539428157145,254.619280881823,
254.699247291473,254.740793060787,254.820758019574,254.900628607679,254.980422344706,
255.060156689796,255.139849055103,255.219528273644,255.299204037433,255.378892069301,
255.458608096413,255.538411659343,255.618264384021,255.698230793671,255.739776562986,
255.819741521773,255.899612109878,255.979405846905,256.059140191996,256.138832557302,
256.218511775844,256.298187539633,256.377875571501,256.457591598612,256.537395161543,
256.617247886221,256.697214295871,256.738760065185,256.818725023972,256.898595612077,
256.978389349104,257.058123694196,257.137816059503,257.217495278044,257.297171041834,
257.376859073702,257.456575100814,257.536378663744,257.616231388422,257.696197798073,
257.737743567385,257.817605191863,257.897372494987,257.977063097636,258.056694559483,
258.136284392802,258.215861564402,258.295435783951,258.375022864638,258.454638624457,
258.534341873629,258.614095072686,258.693960146717,258.729452687902),
 .UNSPECIFIED.);
#145=B_SPLINE_CURVE_WITH_KNOTS('',3,(#13044,#13045,#13046,#13047,#13048,
#13049,#13050,#13051,#13052,#13053,#13054,#13055,#13056),.UNSPECIFIED.,
 .F.,.F.,(4,3,1,1,1,1,1,1,4),(258.729452687902,258.736727069584,259.735710571783,
260.734694073982,261.733677576181,262.73266107838,263.73164458058,264.730628082779,
265.012633520022),.UNSPECIFIED.);
#146=B_SPLINE_CURVE_WITH_KNOTS('',3,(#13058,#13059,#13060,#13061,#13062,
#13063,#13064,#13065,#13066,#13067,#13068,#13069,#13070,#13071,#13072,#13073,
#13074,#13075,#13076,#13077,#13078,#13079,#13080,#13081,#13082,#13083,#13084,
#13085,#13086,#13087,#13088,#13089,#13090,#13091,#13092,#13093,#13094,#13095,
#13096,#13097,#13098,#13099,#13100,#13101,#13102,#13103,#13104,#13105,#13106,
#13107,#13108,#13109,#13110,#13111,#13112,#13113,#13114,#13115,#13116,#13117,
#13118,#13119,#13120,#13121,#13122,#13123,#13124,#13125,#13126,#13127,#13128,
#13129,#13130,#13131,#13132,#13133,#13134,#13135,#13136,#13137,#13138,#13139,
#13140,#13141,#13142,#13143,#13144,#13145,#13146,#13147,#13148,#13149,#13150,
#13151,#13152,#13153,#13154,#13155,#13156,#13157,#13158,#13159,#13160,#13161,
#13162,#13163,#13164,#13165,#13166,#13167,#13168,#13169,#13170,#13171,#13172,
#13173,#13174,#13175,#13176,#13177,#13178,#13179,#13180,#13181,#13182,#13183,
#13184,#13185,#13186,#13187,#13188,#13189,#13190,#13191,#13192,#13193,#13194,
#13195,#13196,#13197,#13198,#13199,#13200,#13201,#13202,#13203,#13204,#13205,
#13206,#13207,#13208,#13209,#13210,#13211,#13212,#13213,#13214,#13215,#13216,
#13217,#13218,#13219,#13220,#13221,#13222,#13223,#13224,#13225,#13226,#13227,
#13228,#13229,#13230,#13231,#13232,#13233,#13234,#13235,#13236,#13237,#13238,
#13239,#13240,#13241,#13242,#13243,#13244,#13245,#13246,#13247,#13248,#13249,
#13250,#13251,#13252,#13253,#13254,#13255,#13256,#13257,#13258,#13259,#13260,
#13261,#13262,#13263,#13264,#13265,#13266,#13267,#13268,#13269,#13270,#13271,
#13272,#13273,#13274,#13275,#13276,#13277,#13278,#13279,#13280,#13281,#13282,
#13283,#13284,#13285,#13286,#13287,#13288,#13289,#13290,#13291,#13292,#13293,
#13294,#13295,#13296,#13297,#13298,#13299,#13300,#13301),.UNSPECIFIED.,
 .F.,.F.,(4,3,3,3,3,3,3,3,3,3,3,3,3,3,3,3,3,3,3,3,3,3,3,3,3,3,3,3,3,3,3,
3,3,3,3,3,3,3,3,3,3,3,3,3,3,3,3,3,3,3,3,3,3,3,3,3,3,3,3,3,3,3,3,3,3,3,3,
3,3,3,3,3,3,3,3,3,3,3,3,3,3,4),(265.012637995082,265.091707545985,265.171445550859,
265.250469629238,265.329495139418,265.408538307972,265.488806627223,265.567973819963,
265.64879270247,265.729611584978,265.809576543765,265.88944713187,265.969240868897,
266.048975213988,266.128667579295,266.208346797836,266.288022561625,266.367710593493,
266.447426620605,266.527230183535,266.607082908213,266.687049317863,266.728595087177,
266.808560045964,266.888430634069,266.968224371096,267.047958716187,267.127651081494,
267.207330300035,267.287006063824,267.366694095692,267.446410122803,267.526213685734,
267.606066410411,267.686032820062,267.727578589376,267.807543548163,267.887414136268,
267.967207873295,268.046942218386,268.126634583692,268.206313802234,268.285989566023,
268.36567759789,268.445393625002,268.525197187932,268.60504991261,268.68501632226,
268.726562091575,268.806527050362,268.886397638467,268.966191375494,269.045925720585,
269.125618085892,269.205297304433,269.284973068223,269.364661100091,269.444377127202,
269.524180690133,269.604033414811,269.683999824461,269.725545593775,269.805510552562,
269.885381140667,269.965174877694,270.044909222784,270.124601588092,270.204280806633,
270.283956570422,270.36364460229,270.443360629401,270.523164192332,270.603016917009,
270.68298332666,270.724529095974,270.806347626139,270.888056489702,270.969669026202,
271.051207595217,271.132651579875,271.214237441069,271.295823302262),
 .UNSPECIFIED.);
#147=B_SPLINE_CURVE_WITH_KNOTS('',3,(#13303,#13304,#13305,#13306,#13307,
#13308,#13309,#13310,#13311,#13312),.UNSPECIFIED.,.F.,.F.,(4,1,1,1,1,1,
1,4),(271.295828888875,271.723512598173,272.722496100372,273.721479602571,
274.72046310477,275.71944660697,276.718430109169,277.579008609441),
 .UNSPECIFIED.);
#148=B_SPLINE_CURVE_WITH_KNOTS('',3,(#13314,#13315,#13316,#13317,#13318,
#13319,#13320,#13321,#13322,#13323,#13324),.UNSPECIFIED.,.F.,.F.,(4,1,1,
1,1,1,1,1,4),(277.579008609441,277.717413611368,278.716397113567,279.715380615766,
280.714364117965,281.713347620165,282.712331122364,283.711314624563,283.862193916621),
 .UNSPECIFIED.);
#149=B_SPLINE_CURVE_WITH_KNOTS('',3,(#13326,#13327,#13328,#13329,#13330,
#13331,#13332,#13333,#13334,#13335),.UNSPECIFIED.,.F.,.F.,(4,1,1,1,1,1,
1,4),(283.862193916621,284.710298126762,285.709281628961,286.70826513116,
287.70724863336,288.706232135559,289.705215637758,290.14537443941),
 .UNSPECIFIED.);
#150=B_SPLINE_CURVE_WITH_KNOTS('',3,(#13337,#13338,#13339,#13340,#13341,
#13342,#13343,#13344,#13345,#13346,#13347,#13348,#13349,#13350,#13351,#13352,
#13353,#13354,#13355,#13356,#13357,#13358,#13359,#13360,#13361,#13362,#13363,
#13364,#13365,#13366,#13367,#13368,#13369,#13370,#13371,#13372,#13373,#13374,
#13375,#13376,#13377,#13378,#13379,#13380,#13381,#13382,#13383,#13384,#13385,
#13386,#13387,#13388,#13389,#13390,#13391,#13392,#13393,#13394,#13395,#13396,
#13397,#13398,#13399,#13400,#13401,#13402,#13403,#13404,#13405,#13406,#13407,
#13408,#13409,#13410,#13411,#13412,#13413,#13414,#13415,#13416,#13417,#13418,
#13419,#13420,#13421,#13422,#13423,#13424,#13425,#13426,#13427,#13428,#13429,
#13430,#13431,#13432,#13433,#13434,#13435,#13436,#13437,#13438,#13439,#13440,
#13441,#13442,#13443,#13444,#13445,#13446,#13447,#13448,#13449,#13450,#13451,
#13452,#13453,#13454,#13455,#13456,#13457,#13458,#13459,#13460,#13461,#13462,
#13463,#13464,#13465,#13466,#13467,#13468,#13469,#13470,#13471,#13472,#13473,
#13474,#13475,#13476,#13477,#13478,#13479,#13480,#13481,#13482,#13483,#13484,
#13485,#13486,#13487,#13488,#13489,#13490,#13491,#13492,#13493,#13494,#13495,
#13496,#13497,#13498,#13499,#13500,#13501,#13502,#13503,#13504,#13505,#13506,
#13507,#13508,#13509,#13510,#13511,#13512,#13513,#13514,#13515,#13516,#13517,
#13518,#13519,#13520,#13521,#13522,#13523,#13524,#13525,#13526,#13527,#13528,
#13529,#13530,#13531,#13532,#13533,#13534,#13535,#13536,#13537,#13538,#13539,
#13540,#13541,#13542,#13543,#13544,#13545,#13546,#13547,#13548,#13549,#13550,
#13551,#13552,#13553,#13554,#13555,#13556,#13557,#13558,#13559,#13560,#13561,
#13562,#13563,#13564,#13565,#13566,#13567,#13568,#13569,#13570,#13571,#13572,
#13573,#13574,#13575,#13576,#13577,#13578,#13579,#13580,#13581,#13582,#13583),
 .UNSPECIFIED.,.F.,.F.,(4,3,3,3,3,3,3,3,3,3,3,3,3,3,3,3,3,3,3,3,3,3,3,3,
3,3,3,3,3,3,3,3,3,3,3,3,3,3,3,3,3,3,3,3,3,3,3,3,3,3,3,3,3,3,3,3,3,3,3,3,
3,3,3,3,3,3,3,3,3,3,3,3,3,3,3,3,3,3,3,3,3,3,4),(290.1453792238,290.227064665826,
290.308797183107,290.390589213631,290.472514284967,290.55450951901,290.636657890419,
290.704199139957,290.784164098744,290.864034686849,290.943828423876,291.023562768967,
291.103255134273,291.182934352814,291.262610116604,291.342298148471,291.422014175583,
291.501817738513,291.581670463191,291.661636872841,291.703182642156,291.783147600943,
291.863018189048,291.942811926074,292.022546271165,292.102238636472,292.181917855013,
292.261593618802,292.34128165067,292.420997677781,292.500801240712,292.58065396539,
292.66062037504,292.702166144355,292.782131103142,292.862001691247,292.941795428274,
293.021529773366,293.101222138672,293.180901357214,293.260577121003,293.340265152871,
293.419981179983,293.499784742913,293.579637467591,293.659603877242,293.701149646555,
293.781114605343,293.860985193447,293.940778930474,294.020513275565,294.100205640872,
294.179884859414,294.259560623203,294.339248655071,294.418964682182,294.498768245113,
294.578620969791,294.658587379441,294.700133148754,294.780098107541,294.859968695646,
294.939762432672,295.019496777763,295.09918914307,295.178868361611,295.2585441254,
295.338232157267,295.417948184378,295.497751747308,295.577604471986,295.657570881637,
295.699116650953,295.77832390399,295.859603982364,295.938618021358,296.017578945768,
296.096503109002,296.179518464496,296.258435225525,296.337361479172,296.416332651885,
296.42856453098),.UNSPECIFIED.);
#151=B_SPLINE_CURVE_WITH_KNOTS('',3,(#13585,#13586,#13587,#13588,#13589,
#13590,#13591,#13592,#13593,#13594,#13595),.UNSPECIFIED.,.F.,.F.,(4,1,1,
1,1,1,1,1,4),(296.428568001001,296.698100153152,297.697083655351,298.69606715755,
299.69505065975,300.694034161949,301.693017664148,302.692001166347,302.711749838159),
 .UNSPECIFIED.);
#152=B_SPLINE_CURVE_WITH_KNOTS('',3,(#13597,#13598,#13599,#13600,#13601,
#13602,#13603,#13604,#13605,#13606,#13607,#13608,#13609,#13610,#13611,#13612,
#13613,#13614,#13615,#13616,#13617,#13618,#13619,#13620,#13621,#13622,#13623,
#13624,#13625,#13626,#13627,#13628,#13629,#13630,#13631,#13632,#13633,#13634,
#13635,#13636,#13637,#13638,#13639,#13640,#13641,#13642,#13643,#13644,#13645,
#13646,#13647,#13648,#13649,#13650,#13651,#13652,#13653,#13654,#13655,#13656,
#13657,#13658,#13659,#13660,#13661,#13662,#13663,#13664,#13665,#13666,#13667,
#13668,#13669,#13670,#13671,#13672,#13673,#13674,#13675,#13676,#13677,#13678,
#13679,#13680,#13681,#13682,#13683,#13684,#13685,#13686,#13687,#13688,#13689,
#13690,#13691,#13692,#13693,#13694,#13695,#13696,#13697,#13698,#13699,#13700,
#13701,#13702,#13703,#13704,#13705,#13706,#13707,#13708,#13709,#13710,#13711,
#13712,#13713,#13714,#13715,#13716,#13717,#13718,#13719,#13720,#13721,#13722,
#13723,#13724,#13725,#13726,#13727,#13728,#13729,#13730,#13731,#13732,#13733,
#13734,#13735,#13736,#13737,#13738,#13739,#13740,#13741,#13742,#13743,#13744,
#13745,#13746,#13747,#13748,#13749,#13750,#13751,#13752,#13753,#13754,#13755,
#13756,#13757,#13758,#13759,#13760,#13761,#13762,#13763,#13764,#13765,#13766,
#13767,#13768,#13769,#13770,#13771,#13772,#13773,#13774,#13775,#13776,#13777,
#13778,#13779,#13780,#13781,#13782,#13783,#13784,#13785,#13786,#13787,#13788,
#13789,#13790,#13791,#13792,#13793,#13794,#13795,#13796,#13797,#13798,#13799,
#13800,#13801,#13802,#13803,#13804,#13805,#13806,#13807,#13808,#13809,#13810,
#13811,#13812,#13813,#13814,#13815,#13816,#13817,#13818,#13819,#13820,#13821,
#13822,#13823,#13824,#13825,#13826,#13827,#13828,#13829,#13830,#13831,#13832,
#13833,#13834,#13835,#13836,#13837,#13838,#13839,#13840,#13841,#13842,#13843),
 .UNSPECIFIED.,.F.,.F.,(4,3,3,3,3,3,3,3,3,3,3,3,3,3,3,3,3,3,3,3,3,3,3,3,
3,3,3,3,3,3,3,3,3,3,3,3,3,3,3,3,3,3,3,3,3,3,3,3,3,3,3,3,3,3,3,3,3,3,3,3,
3,3,3,3,3,3,3,3,3,3,3,3,3,3,3,3,3,3,3,3,3,3,4),(302.711749838159,302.79144354471,
302.871043439066,302.950567294797,303.030032823128,303.112651803805,303.19206492816,
303.271476895875,303.350903657371,303.430361169323,303.509906619331,303.589504139084,
303.669209793545,303.690984668546,303.770949627333,303.850820215438,303.930613952464,
304.010348297555,304.090040662862,304.169719881403,304.249395645192,304.32908367706,
304.408799704171,304.488603267101,304.568455991779,304.64842240143,304.689968170745,
304.769933129532,304.849803717637,304.929597454664,305.009331799755,305.089024165062,
305.168703383603,305.248379147393,305.328067179261,305.407783206372,305.487586769303,
305.567439493981,305.647405903632,305.688951672945,305.768916631732,305.848787219837,
305.928580956864,306.008315301954,306.088007667261,306.167686885802,306.247362649592,
306.32705068146,306.406766708571,306.486570271502,306.566422996179,306.64638940583,
306.687935175144,306.767900133931,306.847770722036,306.927564459062,307.007298804153,
307.08699116946,307.166670388001,307.24634615179,307.326034183658,307.405750210769,
307.4855537737,307.565406498377,307.645372908027,307.686918677343,307.76688363613,
307.846754224235,307.926547961262,308.006282306353,308.085974671658,308.165653890199,
308.245329653989,308.325017685856,308.404733712967,308.484537275898,308.564390000576,
308.644356410227,308.685902179542,308.782302303291,308.878151809102,308.972997791882,
308.99493494478),.UNSPECIFIED.);
#153=B_SPLINE_CURVE_WITH_KNOTS('',3,(#13845,#13846,#13847,#13848,#13849,
#13850,#13851,#13852,#13853,#13854),.UNSPECIFIED.,.F.,.F.,(4,1,1,1,1,1,
1,4),(308.994935145339,309.684885681741,310.68386918394,311.682852686139,
312.681836188339,313.680819690538,314.679803192737,315.278120452519),
 .UNSPECIFIED.);
#154=B_SPLINE_CURVE_WITH_KNOTS('',3,(#13856,#13857,#13858,#13859,#13860,
#13861,#13862,#13863,#13864,#13865),.UNSPECIFIED.,.F.,.F.,(4,1,1,1,1,1,
1,4),(315.278120452519,315.678786694936,316.677770197135,317.676753699334,
318.675737201534,319.674720703733,320.673704205932,321.561305759698),
 .UNSPECIFIED.);
#155=B_SPLINE_CURVE_WITH_KNOTS('',3,(#13867,#13868,#13869,#13870,#13871,
#13872,#13873,#13874,#13875,#13876,#13877),.UNSPECIFIED.,.F.,.F.,(4,1,1,
1,1,1,1,1,4),(321.561305759698,321.672687708131,322.67167121033,323.67065471253,
324.669638214729,325.668621716928,326.667605219127,327.666588721326,327.844491066878),
 .UNSPECIFIED.);
#156=B_SPLINE_CURVE_WITH_KNOTS('',3,(#13879,#13880,#13881,#13882,#13883,
#13884,#13885,#13886,#13887,#13888,#13889,#13890,#13891,#13892,#13893,#13894,
#13895,#13896,#13897,#13898,#13899,#13900,#13901,#13902,#13903,#13904,#13905,
#13906,#13907,#13908,#13909,#13910,#13911,#13912,#13913,#13914,#13915,#13916,
#13917,#13918,#13919,#13920,#13921,#13922,#13923,#13924,#13925,#13926,#13927,
#13928,#13929,#13930,#13931,#13932,#13933,#13934,#13935,#13936,#13937,#13938,
#13939,#13940,#13941,#13942,#13943,#13944,#13945,#13946,#13947,#13948,#13949,
#13950,#13951,#13952,#13953,#13954,#13955,#13956,#13957,#13958,#13959,#13960,
#13961,#13962,#13963,#13964,#13965,#13966,#13967,#13968,#13969,#13970,#13971,
#13972,#13973,#13974,#13975,#13976,#13977,#13978,#13979,#13980,#13981,#13982,
#13983,#13984,#13985,#13986,#13987,#13988,#13989,#13990,#13991,#13992,#13993,
#13994,#13995,#13996,#13997,#13998,#13999,#14000,#14001,#14002,#14003,#14004,
#14005,#14006,#14007,#14008,#14009,#14010,#14011,#14012,#14013,#14014,#14015,
#14016,#14017,#14018,#14019,#14020,#14021,#14022,#14023,#14024,#14025,#14026,
#14027,#14028,#14029,#14030,#14031,#14032,#14033,#14034,#14035,#14036,#14037,
#14038,#14039,#14040,#14041,#14042,#14043,#14044,#14045,#14046,#14047,#14048,
#14049,#14050,#14051,#14052,#14053,#14054,#14055,#14056,#14057,#14058,#14059,
#14060,#14061,#14062,#14063,#14064,#14065,#14066,#14067,#14068,#14069,#14070,
#14071,#14072,#14073,#14074,#14075,#14076,#14077,#14078,#14079,#14080,#14081,
#14082,#14083,#14084,#14085,#14086,#14087,#14088,#14089,#14090,#14091,#14092,
#14093,#14094,#14095,#14096,#14097,#14098,#14099,#14100,#14101,#14102,#14103,
#14104,#14105,#14106,#14107,#14108,#14109,#14110,#14111,#14112,#14113,#14114,
#14115,#14116,#14117,#14118,#14119,#14120,#14121,#14122,#14123,#14124,#14125),
 .UNSPECIFIED.,.F.,.F.,(4,3,3,3,3,3,3,3,3,3,3,3,3,3,3,3,3,3,3,3,3,3,3,3,
3,3,3,3,3,3,3,3,3,3,3,3,3,3,3,3,3,3,3,3,3,3,3,3,3,3,3,3,3,3,3,3,3,3,3,3,
3,3,3,3,3,3,3,3,3,3,3,3,3,3,3,3,3,3,3,3,3,3,4),(327.844491066878,327.923144699921,
328.001729551288,328.080264002823,328.15877503681,328.237276674429,328.315785478742,
328.39431801673,328.472932791003,328.551594499629,328.630365503201,328.665572223525,
328.745537182313,328.825407770417,328.905201507444,328.984935852536,329.064628217843,
329.144307436384,329.223983200174,329.303671232042,329.383387259154,329.463190822085,
329.543043546763,329.623009956414,329.664555725725,329.744520684512,329.824391272617,
329.904185009644,329.983919354735,330.063611720042,330.143290938583,330.222966702372,
330.30265473424,330.382370761351,330.462174324282,330.542027048959,330.62199345861,
330.663539227924,330.743504186711,330.823374774816,330.903168511842,330.982902856933,
331.062595222239,331.142274440781,331.22195020457,331.301638236437,331.381354263548,
331.461157826479,331.541010551156,331.620976960807,331.662522730123,331.74248768891,
331.822358277015,331.902152014042,331.981886359133,332.06157872444,332.141257942982,
332.220933706771,332.300621738639,332.380337765751,332.460141328681,332.539994053359,
332.61996046301,332.661506232322,332.741471191109,332.821341779214,332.901135516241,
332.980869861331,333.060562226638,333.140241445179,333.219917208968,333.299605240835,
333.379321267947,333.459124830878,333.538977555556,333.618943965207,333.660489734521,
333.74589133337,333.831132944262,333.916147981114,334.001024756027,334.085707551949,
334.127676197482),.UNSPECIFIED.);
#157=B_SPLINE_CURVE_WITH_KNOTS('',3,(#14127,#14128,#14129,#14130,#14131,
#14132,#14133,#14134,#14135,#14136),.UNSPECIFIED.,.F.,.F.,(4,1,1,1,1,1,
1,4),(334.127676374057,334.65947323672,335.65845673892,336.657440241119,
337.656423743318,338.655407245517,339.654390747716,340.410861681237),
 .UNSPECIFIED.);
#158=B_SPLINE_CURVE_WITH_KNOTS('',3,(#14138,#14139,#14140,#14141,#14142,
#14143,#14144,#14145,#14146,#14147,#14148,#14149,#14150,#14151,#14152,#14153,
#14154,#14155,#14156,#14157,#14158,#14159,#14160,#14161,#14162,#14163,#14164,
#14165,#14166,#14167,#14168,#14169,#14170,#14171,#14172,#14173,#14174,#14175,
#14176,#14177,#14178,#14179,#14180,#14181,#14182,#14183,#14184,#14185,#14186,
#14187,#14188,#14189,#14190,#14191,#14192,#14193,#14194,#14195,#14196,#14197,
#14198,#14199,#14200,#14201,#14202,#14203,#14204,#14205,#14206,#14207,#14208,
#14209,#14210,#14211,#14212,#14213,#14214,#14215,#14216,#14217,#14218,#14219,
#14220,#14221,#14222,#14223,#14224,#14225,#14226,#14227,#14228,#14229,#14230,
#14231,#14232,#14233,#14234,#14235,#14236,#14237,#14238,#14239,#14240,#14241,
#14242,#14243,#14244,#14245,#14246,#14247,#14248,#14249,#14250,#14251,#14252,
#14253,#14254,#14255,#14256,#14257,#14258,#14259,#14260,#14261,#14262,#14263,
#14264,#14265,#14266,#14267,#14268,#14269,#14270,#14271,#14272,#14273,#14274,
#14275,#14276,#14277,#14278,#14279,#14280,#14281,#14282,#14283,#14284,#14285,
#14286,#14287,#14288,#14289,#14290,#14291,#14292,#14293,#14294,#14295,#14296,
#14297,#14298,#14299,#14300,#14301,#14302,#14303,#14304,#14305,#14306,#14307,
#14308,#14309,#14310,#14311,#14312,#14313,#14314,#14315,#14316,#14317,#14318,
#14319,#14320,#14321,#14322,#14323,#14324,#14325,#14326,#14327,#14328,#14329,
#14330,#14331,#14332,#14333,#14334,#14335,#14336,#14337,#14338,#14339,#14340,
#14341,#14342,#14343,#14344,#14345,#14346,#14347,#14348,#14349,#14350,#14351,
#14352,#14353,#14354,#14355,#14356,#14357,#14358,#14359,#14360,#14361,#14362,
#14363,#14364,#14365,#14366,#14367,#14368,#14369,#14370,#14371,#14372,#14373,
#14374,#14375,#14376,#14377,#14378,#14379,#14380,#14381,#14382,#14383,#14384),
 .UNSPECIFIED.,.F.,.F.,(4,3,3,3,3,3,3,3,3,3,3,3,3,3,3,3,3,3,3,3,3,3,3,3,
3,3,3,3,3,3,3,3,3,3,3,3,3,3,3,3,3,3,3,3,3,3,3,3,3,3,3,3,3,3,3,3,3,3,3,3,
3,3,3,3,3,3,3,3,3,3,3,3,3,3,3,3,3,3,3,3,3,3,4),(340.410861744717,340.5143839423,
340.620403447411,340.653374249915,340.733339208702,340.813209796807,340.893003533834,
340.972737878925,341.052430244232,341.132109462773,341.211785226562,341.29147325843,
341.371189285542,341.450992848473,341.530845573151,341.610811982801,341.652357752114,
341.732322710902,341.812193299006,341.891987036033,341.971721381125,342.051413746432,
342.131092964973,342.210768728762,342.29045676063,342.370172787742,342.449976350673,
342.529829075351,342.609795485001,342.651341254314,342.731306213101,342.811176801206,
342.890970538233,342.970704883324,343.050397248631,343.130076467172,343.209752230961,
343.289440262829,343.369156289941,343.448959852871,343.528812577549,343.6087789872,
343.650324756513,343.7302897153,343.810160303405,343.889954040431,343.969688385522,
344.049380750829,344.12905996937,344.208735733159,344.288423765027,344.368139792138,
344.447943355068,344.527796079746,344.607762489396,344.649308258712,344.729273217499,
344.809143805604,344.888937542631,344.968671887722,345.048364253029,345.12804347157,
345.207719235359,345.287407267227,345.367123294339,345.446926857269,345.526779581947,
345.606745991598,345.648291760911,345.728256719698,345.808127307803,345.88792104483,
345.967655389921,346.047347755228,346.127026973769,346.206702737558,346.286390769426,
346.366106796537,346.445910359467,346.525763084145,346.605729493796,346.64727526311,
346.694046988416),.UNSPECIFIED.);
#159=B_SPLINE_CURVE_WITH_KNOTS('',3,(#14386,#14387,#14388,#14389,#14390,
#14391,#14392,#14393,#14394,#14395),.UNSPECIFIED.,.F.,.F.,(4,1,1,1,1,1,
1,4),(346.694053119753,347.64625876531,348.645242267509,349.644225769708,
350.643209271907,351.642192774106,352.641176276305,352.977224842988),
 .UNSPECIFIED.);
#160=B_SPLINE_CURVE_WITH_KNOTS('',3,(#14397,#14398,#14399,#14400,#14401,
#14402,#14403,#14404,#14405,#14406,#14407,#14408,#14409,#14410,#14411,#14412,
#14413,#14414,#14415,#14416,#14417,#14418,#14419,#14420,#14421,#14422,#14423,
#14424,#14425,#14426,#14427,#14428,#14429,#14430,#14431,#14432,#14433,#14434,
#14435,#14436,#14437,#14438,#14439,#14440,#14441,#14442,#14443,#14444,#14445,
#14446,#14447,#14448,#14449,#14450,#14451,#14452,#14453,#14454,#14455,#14456,
#14457,#14458,#14459,#14460,#14461,#14462,#14463,#14464,#14465,#14466,#14467,
#14468,#14469,#14470,#14471,#14472,#14473,#14474,#14475,#14476,#14477,#14478,
#14479,#14480,#14481,#14482,#14483,#14484,#14485,#14486,#14487,#14488,#14489,
#14490,#14491,#14492,#14493,#14494,#14495,#14496,#14497,#14498,#14499,#14500,
#14501,#14502,#14503,#14504,#14505,#14506,#14507,#14508,#14509,#14510,#14511,
#14512,#14513,#14514,#14515,#14516,#14517,#14518,#14519,#14520,#14521,#14522,
#14523,#14524,#14525,#14526,#14527,#14528,#14529,#14530,#14531,#14532,#14533,
#14534,#14535,#14536,#14537,#14538,#14539,#14540,#14541,#14542,#14543,#14544,
#14545,#14546,#14547,#14548,#14549,#14550,#14551,#14552,#14553,#14554,#14555,
#14556,#14557,#14558,#14559,#14560,#14561,#14562,#14563,#14564,#14565,#14566,
#14567,#14568,#14569,#14570,#14571,#14572,#14573,#14574,#14575,#14576,#14577,
#14578,#14579,#14580,#14581,#14582,#14583,#14584,#14585,#14586,#14587,#14588,
#14589,#14590,#14591,#14592,#14593,#14594,#14595,#14596,#14597,#14598,#14599,
#14600,#14601,#14602,#14603,#14604,#14605,#14606,#14607,#14608,#14609,#14610,
#14611,#14612,#14613,#14614,#14615,#14616,#14617,#14618,#14619,#14620,#14621,
#14622,#14623,#14624,#14625,#14626,#14627,#14628,#14629,#14630,#14631,#14632,
#14633,#14634,#14635,#14636,#14637,#14638,#14639,#14640,#14641,#14642,#14643),
 .UNSPECIFIED.,.F.,.F.,(4,3,3,3,3,3,3,3,3,3,3,3,3,3,3,3,3,3,3,3,3,3,3,3,
3,3,3,3,3,3,3,3,3,3,3,3,3,3,3,3,3,3,3,3,3,3,3,3,3,3,3,3,3,3,3,3,3,3,3,3,
3,3,3,3,3,3,3,3,3,3,3,3,3,3,3,3,3,3,3,3,3,3,4),(352.977232295596,353.06009823096,
353.139757082557,353.219420900244,353.299105357425,353.378826136887,353.458642309883,
353.538514879143,353.618501117166,353.640159778504,353.720124737292,353.799995325396,
353.879789062424,353.959523407515,354.039215772822,354.118894991363,354.198570755153,
354.278258787021,354.357974814133,354.437778377064,354.517631101742,354.597597511393,
354.639143280704,354.719108239491,354.798978827596,354.878772564623,354.958506909714,
355.038199275021,355.117878493562,355.197554257351,355.277242289219,355.35695831633,
355.436761879261,355.516614603939,355.596581013589,355.638126782903,355.71809174169,
355.797962329795,355.877756066821,355.957490411912,356.037182777219,356.11686199576,
356.196537759549,356.276225791417,356.355941818528,356.435745381459,356.515598106136,
356.595564515787,356.637110285102,356.717075243889,356.796945831994,356.876739569021,
356.956473914113,357.03616627942,357.115845497961,357.19552126175,357.275209293618,
357.35492532073,357.43472888366,357.514581608338,357.594548017989,357.636093787301,
357.716058746088,357.795929334193,357.875723071219,357.95545741631,358.035149781616,
358.114829000158,358.194504763947,358.274192795815,358.353908822926,358.433712385856,
358.513565110534,358.593531520184,358.6350772895,358.715679342861,358.796183603853,
358.876605222163,358.956959293157,359.03725629139,359.117519135194,359.197772296352,
359.260417602776),.UNSPECIFIED.);
#161=B_SPLINE_CURVE_WITH_KNOTS('',3,(#14645,#14646,#14647,#14648,#14649,
#14650,#14651,#14652,#14653,#14654),.UNSPECIFIED.,.F.,.F.,(4,1,1,1,1,1,
1,4),(359.260425213007,359.634060791699,360.633044293899,361.632027796098,
362.631011298297,363.629994800496,364.628978302695,365.543602909955),
 .UNSPECIFIED.);
#162=B_SPLINE_CURVE_WITH_KNOTS('',3,(#14656,#14657,#14658,#14659,#14660,
#14661,#14662,#14663,#14664,#14665,#14666,#14667),.UNSPECIFIED.,.F.,.F.,
(4,2,1,1,1,1,1,1,4),(365.543602909955,365.627961804895,366.626945307094,
367.625928809293,368.624912311492,369.623895813691,370.62287931589,371.62186281809,
371.826788217135),.UNSPECIFIED.);
#163=B_SPLINE_CURVE_WITH_KNOTS('',3,(#14669,#14670,#14671,#14672,#14673,
#14674,#14675,#14676,#14677,#14678,#14679,#14680,#14681,#14682,#14683,#14684,
#14685,#14686,#14687,#14688,#14689,#14690,#14691,#14692,#14693,#14694,#14695,
#14696,#14697,#14698,#14699,#14700,#14701,#14702,#14703,#14704,#14705,#14706,
#14707,#14708,#14709,#14710,#14711,#14712,#14713,#14714,#14715,#14716,#14717,
#14718,#14719,#14720,#14721,#14722,#14723,#14724,#14725,#14726,#14727,#14728,
#14729,#14730,#14731,#14732,#14733,#14734,#14735,#14736,#14737,#14738,#14739,
#14740,#14741,#14742,#14743,#14744,#14745,#14746,#14747,#14748,#14749,#14750,
#14751,#14752,#14753,#14754,#14755,#14756,#14757,#14758,#14759,#14760,#14761,
#14762,#14763,#14764,#14765,#14766,#14767,#14768,#14769,#14770,#14771,#14772,
#14773,#14774,#14775,#14776,#14777,#14778,#14779,#14780,#14781,#14782,#14783,
#14784,#14785,#14786,#14787,#14788,#14789,#14790,#14791,#14792,#14793,#14794,
#14795,#14796,#14797,#14798,#14799,#14800,#14801,#14802,#14803,#14804,#14805,
#14806,#14807,#14808,#14809,#14810,#14811,#14812,#14813,#14814,#14815,#14816,
#14817,#14818,#14819,#14820,#14821,#14822,#14823,#14824,#14825,#14826,#14827,
#14828,#14829,#14830,#14831,#14832,#14833,#14834,#14835,#14836,#14837,#14838,
#14839,#14840,#14841,#14842,#14843,#14844,#14845,#14846,#14847,#14848,#14849,
#14850,#14851,#14852,#14853,#14854,#14855,#14856,#14857,#14858,#14859,#14860,
#14861,#14862,#14863,#14864,#14865,#14866,#14867,#14868,#14869,#14870,#14871,
#14872,#14873,#14874,#14875,#14876,#14877,#14878,#14879,#14880,#14881,#14882,
#14883,#14884,#14885,#14886,#14887,#14888,#14889,#14890,#14891,#14892,#14893,
#14894,#14895,#14896,#14897,#14898,#14899,#14900,#14901,#14902,#14903,#14904,
#14905,#14906,#14907,#14908,#14909,#14910,#14911,#14912),.UNSPECIFIED.,
 .F.,.F.,(4,3,3,3,3,3,3,3,3,3,3,3,3,3,3,3,3,3,3,3,3,3,3,3,3,3,3,3,3,3,3,
3,3,3,3,3,3,3,3,3,3,3,3,3,3,3,3,3,3,3,3,3,3,3,3,3,3,3,3,3,3,3,3,3,3,3,3,
3,3,3,3,3,3,3,3,3,3,3,3,3,3,4),(371.826788217135,371.905463396283,371.984076702167,
372.063672904432,372.142227785294,372.220779624991,372.299344958611,372.37972029903,
372.458401859117,372.539624089703,372.620846320289,372.700811279076,372.780681867181,
372.860475604208,372.940209949299,373.019902314605,373.099581533147,373.179257296936,
373.258945328804,373.338661355915,373.418464918845,373.498317643523,373.578284053174,
373.619829822488,373.699794781275,373.77966536938,373.859459106407,373.939193451498,
374.018885816805,374.098565035346,374.178240799135,374.257928831003,374.337644858115,
374.417448421046,374.497301145723,374.577267555374,374.618813324687,374.698778283474,
374.778648871579,374.858442608606,374.938176953697,375.017869319004,375.097548537545,
375.177224301335,375.256912333203,375.336628360314,375.416431923245,375.496284647923,
375.576251057573,375.617796826886,375.697761785673,375.777632373778,375.857426110805,
375.937160455896,376.016852821203,376.096532039744,376.176207803533,376.255895835401,
376.335611862512,376.415415425443,376.49526815012,376.575234559771,376.616780329085,
376.696745287872,376.776615875977,376.856409613004,376.936143958095,377.015836323402,
377.095515541943,377.175191305732,377.2548793376,377.334595364712,377.414398927642,
377.49425165232,377.57421806197,377.615763831284,377.700046285104,377.784187229288,
377.868135337036,377.951969959806,378.035648096222,378.109973524199),
 .UNSPECIFIED.);
#164=B_SPLINE_CURVE_WITH_KNOTS('',3,(#14914,#14915,#14916,#14917,#14918,
#14919,#14920,#14921,#14922,#14923,#14924,#14925,#14926,#14927,#14928,#14929,
#14930,#14931,#14932,#14933,#14934,#14935,#14936,#14937,#14938,#14939,#14940,
#14941,#14942,#14943,#14944,#14945,#14946,#14947,#14948,#14949,#14950,#14951,
#14952,#14953,#14954,#14955,#14956,#14957,#14958,#14959,#14960,#14961,#14962,
#14963,#14964,#14965,#14966,#14967,#14968,#14969,#14970,#14971,#14972,#14973,
#14974,#14975,#14976,#14977,#14978,#14979,#14980,#14981,#14982,#14983,#14984,
#14985,#14986,#14987,#14988,#14989,#14990,#14991,#14992,#14993,#14994,#14995,
#14996,#14997,#14998,#14999,#15000,#15001,#15002,#15003,#15004,#15005,#15006,
#15007,#15008,#15009,#15010,#15011,#15012,#15013,#15014,#15015,#15016,#15017,
#15018,#15019,#15020,#15021,#15022,#15023,#15024,#15025,#15026,#15027,#15028,
#15029,#15030,#15031,#15032,#15033,#15034,#15035,#15036,#15037,#15038,#15039,
#15040,#15041,#15042,#15043,#15044,#15045,#15046,#15047,#15048,#15049,#15050,
#15051,#15052,#15053,#15054,#15055,#15056,#15057,#15058,#15059,#15060,#15061,
#15062,#15063,#15064,#15065,#15066,#15067,#15068,#15069,#15070,#15071,#15072,
#15073,#15074,#15075,#15076,#15077,#15078,#15079,#15080,#15081,#15082,#15083,
#15084,#15085,#15086,#15087,#15088,#15089,#15090,#15091,#15092,#15093,#15094,
#15095,#15096,#15097,#15098,#15099,#15100,#15101,#15102,#15103,#15104,#15105,
#15106,#15107,#15108,#15109,#15110,#15111,#15112,#15113,#15114,#15115,#15116,
#15117,#15118,#15119,#15120,#15121,#15122,#15123,#15124,#15125,#15126,#15127,
#15128,#15129,#15130,#15131,#15132,#15133,#15134,#15135,#15136,#15137,#15138,
#15139,#15140,#15141,#15142,#15143,#15144,#15145,#15146,#15147,#15148,#15149,
#15150,#15151,#15152,#15153,#15154,#15155,#15156,#15157),.UNSPECIFIED.,
 .F.,.F.,(4,3,3,3,3,3,3,3,3,3,3,3,3,3,3,3,3,3,3,3,3,3,3,3,3,3,3,3,3,3,3,
3,3,3,3,3,3,3,3,3,3,3,3,3,3,3,3,3,3,3,3,3,3,3,3,3,3,3,3,3,3,3,3,3,3,3,3,
3,3,3,3,3,3,3,3,3,3,3,3,3,3,4),(378.109973524314,378.193253743236,378.276632185242,
378.361160972303,378.444821525,378.529784429242,378.614747333484,378.694712292271,
378.774582880375,378.854376617402,378.934110962492,379.013803327799,379.09348254634,
379.173158310129,379.252846341996,379.332562369107,379.412365932038,379.492218656715,
379.572185066365,379.613730835683,379.69369579447,379.773566382575,379.853360119602,
379.933094464692,380.012786829999,380.092466048541,380.17214181233,380.251829844198,
380.331545871309,380.411349434239,380.491202158917,380.571168568568,380.612714337882,
380.692679296669,380.772549884774,380.852343621801,380.932077966892,381.011770332199,
381.09144955074,381.171125314529,381.250813346397,381.330529373509,381.41033293644,
381.490185661118,381.570152070768,381.611697840081,381.691662798868,381.771533386973,
381.851327123999,381.93106146909,382.010753834398,382.090433052939,382.170108816728,
382.249796848595,382.329512875706,382.409316438637,382.489169163314,382.569135572965,
382.61068134228,382.690646301067,382.770516889172,382.850310626199,382.93004497129,
383.009737336597,383.089416555138,383.169092318928,383.248780350796,383.328496377907,
383.408299940838,383.488152665516,383.568119075167,383.60966484448,383.688530682252,
383.767301609312,383.845983160986,383.924614195004,384.00321127053,384.081790918647,
384.160397349559,384.239014939738,384.317705749996,384.393158831494),
 .UNSPECIFIED.);
#165=B_SPLINE_CURVE_WITH_KNOTS('',3,(#15159,#15160,#15161,#15162,#15163,
#15164,#15165,#15166,#15167,#15168,#15169),.UNSPECIFIED.,.F.,.F.,(4,1,1,
1,1,1,1,1,4),(384.393158831494,384.608648346679,385.607631848878,386.606615351077,
387.605598853276,388.604582355475,389.603565857674,390.602549359874,390.676344138673),
 .UNSPECIFIED.);
#166=B_SPLINE_CURVE_WITH_KNOTS('',3,(#15171,#15172,#15173,#15174,#15175,
#15176,#15177,#15178,#15179,#15180),.UNSPECIFIED.,.F.,.F.,(4,1,1,1,1,1,
1,4),(390.676344138673,391.601532862073,392.600516364272,393.599499866471,
394.59848336867,395.597466870869,396.596450373069,396.959529445853),
 .UNSPECIFIED.);
#167=B_SPLINE_CURVE_WITH_KNOTS('',3,(#15182,#15183,#15184,#15185,#15186,
#15187,#15188,#15189,#15190,#15191),.UNSPECIFIED.,.F.,.F.,(4,1,1,1,1,1,
1,4),(396.959529445853,397.595433875268,398.594417377467,399.593400879666,
400.592384381865,401.591367884064,402.590351386264,403.242714753032),
 .UNSPECIFIED.);
#168=B_SPLINE_CURVE_WITH_KNOTS('',3,(#15193,#15194,#15195,#15196,#15197,
#15198,#15199,#15200,#15201,#15202,#15203,#15204,#15205,#15206,#15207,#15208,
#15209,#15210,#15211,#15212,#15213,#15214,#15215,#15216,#15217,#15218,#15219,
#15220,#15221,#15222,#15223,#15224,#15225,#15226,#15227,#15228,#15229,#15230,
#15231,#15232,#15233,#15234,#15235,#15236,#15237,#15238,#15239,#15240,#15241,
#15242,#15243,#15244,#15245,#15246,#15247,#15248,#15249,#15250,#15251,#15252,
#15253,#15254,#15255,#15256,#15257,#15258,#15259,#15260,#15261,#15262,#15263,
#15264,#15265,#15266,#15267,#15268,#15269,#15270,#15271,#15272,#15273,#15274,
#15275,#15276,#15277,#15278,#15279,#15280,#15281,#15282,#15283,#15284,#15285,
#15286,#15287,#15288,#15289,#15290,#15291,#15292,#15293,#15294,#15295,#15296,
#15297,#15298,#15299,#15300,#15301,#15302,#15303,#15304,#15305,#15306,#15307,
#15308,#15309,#15310,#15311,#15312,#15313,#15314,#15315,#15316,#15317,#15318,
#15319,#15320,#15321,#15322,#15323,#15324,#15325,#15326,#15327,#15328,#15329,
#15330,#15331,#15332,#15333,#15334,#15335,#15336,#15337,#15338,#15339,#15340,
#15341,#15342,#15343,#15344,#15345,#15346,#15347,#15348,#15349,#15350,#15351,
#15352,#15353,#15354,#15355,#15356,#15357,#15358,#15359,#15360,#15361,#15362,
#15363,#15364,#15365,#15366,#15367,#15368,#15369,#15370,#15371,#15372,#15373,
#15374,#15375,#15376,#15377,#15378,#15379,#15380,#15381,#15382,#15383,#15384,
#15385,#15386,#15387,#15388,#15389,#15390,#15391,#15392,#15393,#15394,#15395,
#15396,#15397,#15398,#15399,#15400,#15401,#15402,#15403,#15404,#15405,#15406,
#15407,#15408,#15409,#15410,#15411,#15412,#15413,#15414,#15415,#15416,#15417,
#15418,#15419,#15420,#15421,#15422,#15423,#15424,#15425,#15426,#15427,#15428,
#15429,#15430,#15431,#15432,#15433,#15434,#15435,#15436),.UNSPECIFIED.,
 .F.,.F.,(4,3,3,3,3,3,3,3,3,3,3,3,3,3,3,3,3,3,3,3,3,3,3,3,3,3,3,3,3,3,3,
3,3,3,3,3,3,3,3,3,3,3,3,3,3,3,3,3,3,3,3,3,3,3,3,3,3,3,3,3,3,3,3,3,3,3,3,
3,3,3,3,3,3,3,3,3,3,3,3,3,3,4),(403.24271487461,403.334441411454,403.426617865222,
403.519381278125,403.589334888463,403.66929984725,403.749170435354,403.82896417238,
403.908698517471,403.988390882778,404.068070101318,404.147745865107,404.227433896974,
404.307149924086,404.386953487016,404.466806211693,404.546772621343,404.588318390662,
404.668283349449,404.748153937554,404.827947674581,404.907682019672,404.987374384979,
405.06705360352,405.146729367309,405.226417399177,405.306133426288,405.385936989219,
405.465789713897,405.545756123547,405.587301892861,405.667266851648,405.747137439753,
405.82693117678,405.906665521871,405.986357887178,406.06603710572,406.145712869509,
406.225400901377,406.305116928489,406.384920491419,406.464773216097,406.544739625748,
406.58628539506,406.666250353847,406.746120941952,406.825914678978,406.905649024069,
406.985341389376,407.065020607917,407.144696371706,407.224384403574,407.304100430685,
407.383903993615,407.463756718293,407.543723127943,407.585268897259,407.665233856046,
407.745104444151,407.824898181178,407.904632526269,407.984324891576,408.064004110118,
408.143679873907,408.223367905775,408.303083932887,408.382887495817,408.462740220496,
408.542706630146,408.584252399459,408.663535534452,408.742724767276,408.821838218944,
408.900893942308,408.979915849117,409.058921070256,409.137925862554,409.216946480107,
409.296044176676,409.375181216383,409.454434737698,409.525900060212),
 .UNSPECIFIED.);
#169=B_SPLINE_CURVE_WITH_KNOTS('',3,(#15438,#15439,#15440,#15441,#15442,
#15443,#15444,#15445,#15446,#15447,#15448,#15449),.UNSPECIFIED.,.F.,.F.,
(4,2,1,1,1,1,1,1,4),(409.525900060212,409.583235901658,410.582219403857,
411.581202906056,412.580186408255,413.579169910454,414.578153412654,415.577136914853,
415.809085367392),.UNSPECIFIED.);
#170=B_SPLINE_CURVE_WITH_KNOTS('',3,(#15451,#15452,#15453,#15454,#15455,
#15456,#15457,#15458,#15459,#15460),.UNSPECIFIED.,.F.,.F.,(4,1,1,1,1,1,
1,4),(415.809085367392,416.576120417052,417.575103919251,418.57408742145,
419.573070923649,420.572054425849,421.571037928048,422.092270674571),
 .UNSPECIFIED.);
#171=B_SPLINE_CURVE_WITH_KNOTS('',3,(#15462,#15463,#15464,#15465,#15466,
#15467,#15468,#15469,#15470,#15471),.UNSPECIFIED.,.F.,.F.,(4,1,1,1,1,1,
1,4),(422.092270674571,422.570021430247,423.569004932446,424.567988434645,
425.566971936844,426.565955439044,427.564938941243,428.375451647274),
 .UNSPECIFIED.);
#172=B_SPLINE_CURVE_WITH_KNOTS('',3,(#15473,#15474,#15475,#15476,#15477,
#15478,#15479,#15480,#15481,#15482,#15483,#15484,#15485,#15486,#15487,#15488,
#15489,#15490,#15491,#15492,#15493,#15494,#15495,#15496,#15497,#15498,#15499,
#15500,#15501,#15502,#15503,#15504,#15505,#15506,#15507,#15508,#15509,#15510,
#15511,#15512,#15513,#15514,#15515,#15516,#15517,#15518,#15519,#15520,#15521,
#15522,#15523,#15524,#15525,#15526,#15527,#15528,#15529,#15530,#15531,#15532,
#15533,#15534,#15535,#15536,#15537,#15538,#15539,#15540,#15541,#15542,#15543,
#15544,#15545,#15546,#15547,#15548,#15549,#15550,#15551,#15552,#15553,#15554,
#15555,#15556,#15557,#15558,#15559,#15560,#15561,#15562,#15563,#15564,#15565,
#15566,#15567,#15568,#15569,#15570,#15571,#15572,#15573,#15574,#15575,#15576,
#15577,#15578,#15579,#15580,#15581,#15582,#15583,#15584,#15585,#15586,#15587,
#15588,#15589,#15590,#15591,#15592,#15593,#15594,#15595,#15596,#15597,#15598,
#15599,#15600,#15601,#15602,#15603,#15604,#15605,#15606,#15607,#15608,#15609,
#15610,#15611,#15612,#15613,#15614,#15615,#15616,#15617,#15618,#15619,#15620,
#15621,#15622,#15623,#15624,#15625,#15626,#15627,#15628,#15629,#15630,#15631,
#15632,#15633,#15634,#15635,#15636,#15637,#15638,#15639,#15640,#15641,#15642,
#15643,#15644,#15645,#15646,#15647,#15648,#15649,#15650,#15651,#15652,#15653,
#15654,#15655,#15656,#15657,#15658,#15659,#15660,#15661,#15662,#15663,#15664,
#15665,#15666,#15667,#15668,#15669,#15670,#15671,#15672,#15673,#15674,#15675,
#15676,#15677,#15678,#15679,#15680,#15681,#15682,#15683,#15684,#15685,#15686,
#15687,#15688,#15689,#15690,#15691,#15692,#15693,#15694,#15695,#15696,#15697,
#15698,#15699,#15700,#15701,#15702,#15703,#15704,#15705,#15706,#15707,#15708,
#15709,#15710,#15711,#15712,#15713,#15714,#15715,#15716),.UNSPECIFIED.,
 .F.,.F.,(4,3,3,3,3,3,3,3,3,3,3,3,3,3,3,3,3,3,3,3,3,3,3,3,3,3,3,3,3,3,3,
3,3,3,3,3,3,3,3,3,3,3,3,3,3,3,3,3,3,3,3,3,3,3,3,3,3,3,3,3,3,3,3,3,3,3,3,
3,3,3,3,3,3,3,3,3,3,3,3,3,3,4),(428.375455981751,428.493703066263,428.563922443442,
428.64388740223,428.723757990335,428.803551727362,428.883286072453,428.962978437761,
429.042657656303,429.122333420092,429.202021451961,429.281737479072,429.361541042003,
429.441393766682,429.521360176333,429.562905945641,429.642870904428,429.722741492533,
429.802535229559,429.88226957465,429.961961939957,430.041641158498,430.121316922287,
430.201004954155,430.280720981267,430.360524544197,430.440377268875,430.520343678525,
430.56188944784,430.641854406627,430.721724994732,430.801518731758,430.881253076849,
430.960945442156,431.040624660697,431.120300424486,431.199988456354,431.279704483466,
431.359508046396,431.439360771074,431.519327180724,431.560872950039,431.640837908826,
431.720708496931,431.800502233958,431.880236579049,431.959928944356,432.039608162897,
432.119283926686,432.198971958554,432.278687985665,432.358491548595,432.438344273273,
432.518310682924,432.559856452238,432.639821411026,432.71969199913,432.799485736157,
432.879220081249,432.958912446556,433.038591665097,433.118267428886,433.197955460754,
433.277671487866,433.357475050797,433.437327775475,433.517294185126,433.558839954438,
433.638804913225,433.71867550133,433.798469238357,433.878203583448,433.957895948755,
434.037575167297,434.117250931086,434.196938962954,434.276654990065,434.356458552996,
434.436311277674,434.516277687325,434.557823456637,434.65864128893),
 .UNSPECIFIED.);
#173=B_SPLINE_CURVE_WITH_KNOTS('',3,(#15718,#15719,#15720,#15721,#15722,
#15723,#15724,#15725,#15726,#15727),.UNSPECIFIED.,.F.,.F.,(4,1,1,1,1,1,
1,4),(434.658650333521,435.556806958836,436.555790461035,437.554773963234,
438.553757465434,439.552740967633,440.551724469832,440.94182659611),
 .UNSPECIFIED.);
#174=B_SPLINE_CURVE_WITH_KNOTS('',3,(#15729,#15730,#15731,#15732,#15733,
#15734,#15735,#15736,#15737,#15738),.UNSPECIFIED.,.F.,.F.,(4,1,1,1,1,1,
1,4),(440.94182659611,441.550707972031,442.54969147423,443.548674976429,
444.547658478629,445.546641980828,446.545625483027,447.225011903289),
 .UNSPECIFIED.);
#175=B_SPLINE_CURVE_WITH_KNOTS('',3,(#15740,#15741,#15742,#15743,#15744,
#15745,#15746,#15747,#15748,#15749),.UNSPECIFIED.,.F.,.F.,(4,1,1,1,1,1,
1,4),(447.225011903289,447.544608985226,448.543592487425,449.542575989624,
450.541559491824,451.540542994023,452.539526496222,453.50819303157),
 .UNSPECIFIED.);
#176=B_SPLINE_CURVE_WITH_KNOTS('',3,(#15751,#15752,#15753,#15754,#15755,
#15756,#15757,#15758,#15759,#15760,#15761,#15762,#15763,#15764,#15765,#15766,
#15767,#15768,#15769,#15770,#15771,#15772,#15773,#15774,#15775,#15776,#15777,
#15778,#15779,#15780,#15781,#15782,#15783,#15784,#15785,#15786,#15787,#15788,
#15789,#15790,#15791,#15792,#15793,#15794,#15795,#15796,#15797,#15798,#15799,
#15800,#15801,#15802,#15803,#15804,#15805,#15806,#15807,#15808,#15809,#15810,
#15811,#15812,#15813,#15814,#15815,#15816,#15817,#15818,#15819,#15820,#15821,
#15822,#15823,#15824,#15825,#15826,#15827,#15828,#15829,#15830,#15831,#15832,
#15833,#15834,#15835,#15836,#15837,#15838,#15839,#15840,#15841,#15842,#15843,
#15844,#15845,#15846,#15847,#15848,#15849,#15850,#15851,#15852,#15853,#15854,
#15855,#15856,#15857,#15858,#15859,#15860,#15861,#15862,#15863,#15864,#15865,
#15866,#15867,#15868,#15869,#15870,#15871,#15872,#15873,#15874,#15875,#15876,
#15877,#15878,#15879,#15880,#15881,#15882,#15883,#15884,#15885,#15886,#15887,
#15888,#15889,#15890,#15891,#15892,#15893,#15894,#15895,#15896,#15897,#15898,
#15899,#15900,#15901,#15902,#15903,#15904,#15905,#15906,#15907,#15908,#15909,
#15910,#15911,#15912,#15913,#15914,#15915,#15916,#15917,#15918,#15919,#15920,
#15921,#15922,#15923,#15924,#15925,#15926,#15927,#15928,#15929,#15930,#15931,
#15932,#15933,#15934,#15935,#15936,#15937,#15938,#15939,#15940,#15941,#15942,
#15943,#15944,#15945,#15946,#15947,#15948,#15949,#15950,#15951,#15952,#15953,
#15954,#15955,#15956,#15957,#15958,#15959,#15960,#15961,#15962,#15963,#15964,
#15965,#15966,#15967,#15968,#15969,#15970,#15971,#15972,#15973,#15974,#15975,
#15976,#15977,#15978,#15979,#15980,#15981,#15982,#15983,#15984,#15985,#15986,
#15987,#15988,#15989,#15990,#15991,#15992,#15993,#15994,#15995,#15996,#15997),
 .UNSPECIFIED.,.F.,.F.,(4,3,3,3,3,3,3,3,3,3,3,3,3,3,3,3,3,3,3,3,3,3,3,3,
3,3,3,3,3,3,3,3,3,3,3,3,3,3,3,3,3,3,3,3,3,3,3,3,3,3,3,3,3,3,3,3,3,3,3,3,
3,3,3,3,3,3,3,3,3,3,3,3,3,3,3,3,3,3,3,3,3,3,4),(453.508197210469,453.538509998421,
453.618474957208,453.698345545313,453.778139282339,453.85787362743,453.937565992737,
454.017245211278,454.096920975067,454.176609006935,454.256325034046,454.336128596977,
454.415981321654,454.495947731305,454.53749350062,454.617458459407,454.697329047512,
454.777122784539,454.85685712963,454.936549494937,455.016228713478,455.095904477267,
455.175592509135,455.255308536247,455.335112099177,455.414964823855,455.494931233505,
455.536477002819,455.616441961606,455.696312549711,455.776106286738,455.855840631829,
455.935532997136,456.015212215677,456.094887979466,456.174576011334,456.254292038446,
456.334095601376,456.413948326054,456.493914735704,456.535460505018,456.615425463805,
456.69529605191,456.775089788937,456.854824134028,456.934516499335,457.014195717876,
457.093871481666,457.173559513534,457.253275540645,457.333079103576,457.412931828254,
457.492898237904,457.534444007218,457.614408966005,457.69427955411,457.774073291137,
457.853807636228,457.933500001535,458.013179220076,458.092854983865,458.172543015733,
458.252259042845,458.332062605775,458.411915330453,458.491881740104,458.533427509417,
458.613392468204,458.693263056309,458.773056793335,458.852791138426,458.932483503733,
459.012162722274,459.091838486063,459.171526517931,459.251242545042,459.331046107972,
459.41089883265,459.4908652423,459.532411011616,459.635607913994,459.736866594815,
459.791382436132),.UNSPECIFIED.);
#177=B_SPLINE_CURVE_WITH_KNOTS('',3,(#15999,#16000,#16001,#16002,#16003,
#16004,#16005,#16006,#16007,#16008),.UNSPECIFIED.,.F.,.F.,(4,1,1,1,1,1,
1,4),(459.791382517649,460.531394513815,461.530378016014,462.529361518214,
463.528345020413,464.527328522612,465.526312024811,466.074567824828),
 .UNSPECIFIED.);
#178=B_SPLINE_CURVE_WITH_KNOTS('',3,(#16010,#16011,#16012,#16013,#16014,
#16015,#16016,#16017,#16018,#16019),.UNSPECIFIED.,.F.,.F.,(4,1,1,1,1,1,
1,4),(466.074567824828,466.52529552701,467.524279029209,468.523262531408,
469.522246033608,470.521229535807,471.520213038006,472.357753132008),
 .UNSPECIFIED.);
#179=B_SPLINE_CURVE_WITH_KNOTS('',3,(#16021,#16022,#16023,#16024,#16025,
#16026,#16027,#16028,#16029,#16030,#16031),.UNSPECIFIED.,.F.,.F.,(4,1,1,
1,1,1,1,1,4),(472.357753132008,472.519196540205,473.518180042404,474.517163544603,
475.516147046803,476.515130549002,477.514114051201,478.5130975534,478.640938439187),
 .UNSPECIFIED.);
#180=B_SPLINE_CURVE_WITH_KNOTS('',3,(#16033,#16034,#16035,#16036,#16037,
#16038,#16039,#16040,#16041,#16042,#16043,#16044,#16045,#16046,#16047,#16048,
#16049,#16050,#16051,#16052,#16053,#16054,#16055,#16056,#16057,#16058,#16059,
#16060,#16061,#16062,#16063,#16064,#16065,#16066,#16067,#16068,#16069,#16070,
#16071,#16072,#16073,#16074,#16075,#16076,#16077,#16078,#16079,#16080,#16081,
#16082,#16083,#16084,#16085,#16086,#16087,#16088,#16089,#16090,#16091,#16092,
#16093,#16094,#16095,#16096,#16097,#16098,#16099,#16100,#16101,#16102,#16103,
#16104,#16105,#16106,#16107,#16108,#16109,#16110,#16111,#16112,#16113,#16114,
#16115,#16116,#16117,#16118,#16119,#16120,#16121,#16122,#16123,#16124,#16125,
#16126,#16127,#16128,#16129,#16130,#16131,#16132,#16133,#16134,#16135,#16136,
#16137,#16138,#16139,#16140,#16141,#16142,#16143,#16144,#16145,#16146,#16147,
#16148,#16149,#16150,#16151,#16152,#16153,#16154,#16155,#16156,#16157,#16158,
#16159,#16160,#16161,#16162,#16163,#16164,#16165,#16166,#16167,#16168,#16169,
#16170,#16171,#16172,#16173,#16174,#16175,#16176,#16177,#16178,#16179,#16180,
#16181,#16182,#16183,#16184,#16185,#16186,#16187,#16188,#16189,#16190,#16191,
#16192,#16193,#16194,#16195,#16196,#16197,#16198,#16199,#16200,#16201,#16202,
#16203,#16204,#16205,#16206,#16207,#16208,#16209,#16210,#16211,#16212,#16213,
#16214,#16215,#16216,#16217,#16218,#16219,#16220,#16221,#16222,#16223,#16224,
#16225,#16226,#16227,#16228,#16229,#16230,#16231,#16232,#16233,#16234,#16235,
#16236,#16237,#16238,#16239,#16240,#16241,#16242,#16243,#16244,#16245,#16246,
#16247,#16248,#16249,#16250,#16251,#16252,#16253,#16254,#16255,#16256,#16257,
#16258,#16259,#16260,#16261,#16262,#16263,#16264,#16265,#16266,#16267,#16268,
#16269,#16270,#16271,#16272,#16273,#16274,#16275,#16276),.UNSPECIFIED.,
 .F.,.F.,(4,3,3,3,3,3,3,3,3,3,3,3,3,3,3,3,3,3,3,3,3,3,3,3,3,3,3,3,3,3,3,
3,3,3,3,3,3,3,3,3,3,3,3,3,3,3,3,3,3,3,3,3,3,3,3,3,3,3,3,3,3,3,3,3,3,3,3,
3,3,3,3,3,3,3,3,3,3,3,3,3,3,4),(478.640938439187,478.719706377143,478.798394573331,
478.877021407815,478.956403863788,479.034973428448,479.113540340611,479.19212112738,
479.272111109435,479.350808436616,479.431444746107,479.512081055599,479.592046014386,
479.671916602491,479.751710339518,479.831444684608,479.911137049915,479.990816268456,
480.070492032245,480.150180064113,480.229896091225,480.309699654155,480.389552378833,
480.469518788483,480.511064557798,480.591029516586,480.670900104691,480.750693841718,
480.830428186809,480.910120552116,480.989799770658,481.069475534447,481.149163566315,
481.228879593427,481.308683156358,481.388535881036,481.468502290686,481.510048059998,
481.590013018785,481.66988360689,481.749677343917,481.829411689009,481.909104054315,
481.988783272857,482.068459036646,482.148147068514,482.227863095625,482.307666658556,
482.387519383234,482.467485792884,482.509031562197,482.588996520984,482.668867109089,
482.748660846115,482.828395191206,482.908087556513,482.987766775054,483.067442538843,
483.147130570711,483.226846597823,483.306650160753,483.386502885431,483.466469295081,
483.508015064396,483.587980023183,483.667850611288,483.747644348314,483.827378693406,
483.907071058712,483.986750277253,484.066426041042,484.14611407291,484.225830100022,
484.305633662952,484.38548638763,484.465452797281,484.506998566595,484.594934491268,
484.682543461914,484.769947617553,484.857012922915,484.924123547619),
 .UNSPECIFIED.);
#181=B_SPLINE_CURVE_WITH_KNOTS('',3,(#16278,#16279,#16280,#16281,#16282,
#16283,#16284,#16285,#16286,#16287),.UNSPECIFIED.,.F.,.F.,(4,1,1,1,1,1,
1,4),(484.924123746367,485.505982068794,486.504965570993,487.503949073193,
488.502932575392,489.501916077591,490.50089957979,491.207309053546),
 .UNSPECIFIED.);
#182=B_SPLINE_CURVE_WITH_KNOTS('',3,(#16289,#16290,#16291,#16292,#16293,
#16294,#16295,#16296,#16297,#16298,#16299,#16300,#16301,#16302,#16303,#16304,
#16305,#16306,#16307,#16308,#16309,#16310,#16311,#16312,#16313,#16314,#16315,
#16316,#16317,#16318,#16319,#16320,#16321,#16322,#16323,#16324,#16325,#16326,
#16327,#16328,#16329,#16330,#16331,#16332,#16333,#16334,#16335,#16336,#16337,
#16338,#16339,#16340,#16341,#16342,#16343,#16344,#16345,#16346,#16347,#16348,
#16349,#16350,#16351,#16352,#16353,#16354,#16355,#16356,#16357,#16358,#16359,
#16360,#16361,#16362,#16363,#16364,#16365,#16366,#16367,#16368,#16369,#16370,
#16371,#16372,#16373,#16374,#16375,#16376,#16377,#16378,#16379,#16380,#16381,
#16382,#16383,#16384,#16385,#16386,#16387,#16388,#16389,#16390,#16391,#16392,
#16393,#16394,#16395,#16396,#16397,#16398,#16399,#16400,#16401,#16402,#16403,
#16404,#16405,#16406,#16407,#16408,#16409,#16410,#16411,#16412,#16413,#16414,
#16415,#16416,#16417,#16418,#16419,#16420,#16421,#16422,#16423,#16424,#16425,
#16426,#16427,#16428,#16429,#16430,#16431,#16432,#16433,#16434,#16435,#16436,
#16437,#16438,#16439,#16440,#16441,#16442,#16443,#16444,#16445,#16446,#16447,
#16448,#16449,#16450,#16451,#16452,#16453,#16454,#16455,#16456,#16457,#16458,
#16459,#16460,#16461,#16462,#16463,#16464,#16465,#16466,#16467,#16468,#16469,
#16470,#16471,#16472,#16473,#16474,#16475,#16476,#16477,#16478,#16479,#16480,
#16481,#16482,#16483,#16484,#16485,#16486,#16487,#16488,#16489,#16490,#16491,
#16492,#16493,#16494,#16495,#16496,#16497,#16498,#16499,#16500,#16501,#16502,
#16503,#16504,#16505,#16506,#16507,#16508,#16509,#16510,#16511,#16512,#16513,
#16514,#16515,#16516,#16517,#16518,#16519,#16520,#16521,#16522,#16523,#16524,
#16525,#16526,#16527,#16528,#16529,#16530,#16531,#16532),.UNSPECIFIED.,
 .F.,.F.,(4,3,3,3,3,3,3,3,3,3,3,3,3,3,3,3,3,3,3,3,3,3,3,3,3,3,3,3,3,3,3,
3,3,3,3,3,3,3,3,3,3,3,3,3,3,3,3,3,3,3,3,3,3,3,3,3,3,3,3,3,3,3,3,3,3,3,3,
3,3,3,3,3,3,3,3,3,3,3,3,3,3,4),(491.207309221467,491.304080701035,491.402189558315,
491.499883081989,491.579848040776,491.65971862888,491.739512365907,491.819246710998,
491.898939076304,491.978618294845,492.058294058634,492.137982090501,492.217698117612,
492.297501680543,492.37735440522,492.45732081487,492.498866584188,492.578831542976,
492.65870213108,492.738495868107,492.818230213199,492.897922578506,492.977601797047,
493.057277560837,493.136965592705,493.216681619817,493.296485182747,493.376337907425,
493.456304317076,493.497850086388,493.577815045175,493.65768563328,493.737479370307,
493.817213715398,493.896906080705,493.976585299246,494.056261063035,494.135949094903,
494.215665122015,494.295468684945,494.375321409623,494.455287819274,494.496833588587,
494.576798547374,494.656669135479,494.736462872505,494.816197217596,494.895889582903,
494.975568801444,495.055244565233,495.134932597101,495.214648624212,495.294452187142,
495.37430491182,495.454271321471,495.495817090786,495.575782049573,495.655652637678,
495.735446374705,495.815180719796,495.894873085103,495.974552303644,496.054228067433,
496.133916099301,496.213632126412,496.293435689343,496.373288414021,496.453254823671,
496.494800592985,496.57471819498,496.654541447734,496.734287917752,496.81397511075,
496.89362048528,496.973252939931,497.052882172046,497.132523946332,497.212194032043,
497.291951648498,497.37175879078,497.451678816343,497.490494360726),
 .UNSPECIFIED.);
#183=B_SPLINE_CURVE_WITH_KNOTS('',3,(#16534,#16535,#16536,#16537,#16538,
#16539,#16540,#16541,#16542,#16543,#16544,#16545),.UNSPECIFIED.,.F.,.F.,
(4,2,1,1,1,1,1,1,4),(497.490494360726,497.493784095184,498.492767597383,
499.491751099583,500.490734601782,501.489718103981,502.48870160618,503.487685108379,
503.773679667906),.UNSPECIFIED.);
#184=B_SPLINE_CURVE_WITH_KNOTS('',3,(#16547,#16548,#16549,#16550,#16551,
#16552,#16553,#16554,#16555,#16556),.UNSPECIFIED.,.F.,.F.,(4,1,1,1,1,1,
1,4),(503.773679667906,504.486668610578,505.485652112778,506.484635614977,
507.483619117176,508.482602619375,509.481586121574,510.056864975085),
 .UNSPECIFIED.);
#185=B_SPLINE_CURVE_WITH_KNOTS('',3,(#16558,#16559,#16560,#16561,#16562,
#16563,#16564,#16565,#16566,#16567),.UNSPECIFIED.,.F.,.F.,(4,1,1,1,1,1,
1,4),(510.056864975085,510.480569623773,511.479553125973,512.478536628172,
513.477520130371,514.47650363257,515.475487134769,516.340050282265),
 .UNSPECIFIED.);
#186=B_SPLINE_CURVE_WITH_KNOTS('',3,(#16569,#16570,#16571,#16572,#16573,
#16574,#16575,#16576,#16577,#16578,#16579),.UNSPECIFIED.,.F.,.F.,(4,1,1,
1,1,1,1,1,4),(516.340050282265,516.474470636968,517.473454139167,518.472437641367,
519.471421143566,520.470404645765,521.469388147964,522.468371650163,522.623235589444),
 .UNSPECIFIED.);
#187=B_SPLINE_CURVE_WITH_KNOTS('',3,(#16581,#16582,#16583,#16584,#16585,
#16586,#16587,#16588,#16589,#16590),.UNSPECIFIED.,.F.,.F.,(4,1,1,1,1,1,
1,4),(522.623235589444,523.467355152363,524.466338654562,525.465322156761,
526.46430565896,527.463289161159,528.462272663358,528.906420896624),
 .UNSPECIFIED.);
#188=B_SPLINE_CURVE_WITH_KNOTS('',3,(#16592,#16593,#16594,#16595,#16596,
#16597,#16598,#16599,#16600,#16601),.UNSPECIFIED.,.F.,.F.,(4,1,1,1,1,1,
1,4),(528.906420896624,529.461256165558,530.460239667757,531.459223169956,
532.458206672155,533.457190174354,534.456173676553,535.189606203803),
 .UNSPECIFIED.);
#189=B_SPLINE_CURVE_WITH_KNOTS('',3,(#16603,#16604,#16605,#16606,#16607,
#16608,#16609,#16610,#16611,#16612,#16613),.UNSPECIFIED.,.F.,.F.,(4,1,1,
1,1,1,1,1,4),(535.189606203803,535.455157178753,536.454140680952,537.453124183151,
538.45210768535,539.451091187549,540.450074689748,541.449058191948,541.472791510983),
 .UNSPECIFIED.);
#190=B_SPLINE_CURVE_WITH_KNOTS('',3,(#16615,#16616,#16617,#16618,#16619,
#16620,#16621,#16622,#16623,#16624,#16625,#16626,#16627,#16628,#16629,#16630,
#16631,#16632,#16633,#16634,#16635,#16636,#16637,#16638,#16639,#16640,#16641,
#16642,#16643,#16644,#16645,#16646,#16647,#16648,#16649,#16650,#16651,#16652,
#16653,#16654,#16655,#16656,#16657,#16658,#16659,#16660,#16661,#16662,#16663,
#16664,#16665,#16666,#16667,#16668,#16669,#16670,#16671,#16672,#16673,#16674,
#16675,#16676,#16677,#16678,#16679,#16680,#16681,#16682,#16683,#16684,#16685,
#16686,#16687,#16688,#16689,#16690,#16691,#16692,#16693,#16694,#16695,#16696,
#16697,#16698,#16699,#16700,#16701,#16702,#16703,#16704,#16705,#16706,#16707,
#16708,#16709,#16710,#16711,#16712,#16713,#16714,#16715,#16716,#16717,#16718,
#16719,#16720,#16721,#16722,#16723,#16724,#16725,#16726,#16727,#16728,#16729,
#16730,#16731,#16732,#16733,#16734,#16735,#16736,#16737,#16738,#16739,#16740,
#16741,#16742,#16743,#16744,#16745,#16746,#16747,#16748,#16749,#16750,#16751,
#16752,#16753,#16754,#16755,#16756,#16757,#16758,#16759,#16760,#16761,#16762,
#16763,#16764,#16765,#16766,#16767,#16768,#16769,#16770,#16771,#16772,#16773,
#16774,#16775,#16776,#16777,#16778,#16779,#16780,#16781,#16782,#16783,#16784,
#16785,#16786,#16787,#16788,#16789,#16790,#16791,#16792,#16793,#16794,#16795,
#16796,#16797,#16798,#16799,#16800,#16801,#16802,#16803,#16804,#16805,#16806,
#16807,#16808,#16809,#16810,#16811,#16812,#16813,#16814,#16815,#16816,#16817,
#16818,#16819,#16820,#16821,#16822,#16823,#16824,#16825,#16826,#16827,#16828,
#16829,#16830,#16831,#16832,#16833,#16834,#16835,#16836,#16837,#16838,#16839,
#16840,#16841,#16842,#16843,#16844,#16845,#16846,#16847,#16848,#16849,#16850,
#16851,#16852,#16853,#16854,#16855,#16856,#16857,#16858,#16859,#16860,#16861),
 .UNSPECIFIED.,.F.,.F.,(4,3,3,3,3,3,3,3,3,3,3,3,3,3,3,3,3,3,3,3,3,3,3,3,
3,3,3,3,3,3,3,3,3,3,3,3,3,3,3,3,3,3,3,3,3,3,3,3,3,3,3,3,3,3,3,3,3,3,3,3,
3,3,3,3,3,3,3,3,3,3,3,3,3,3,3,3,3,3,3,3,3,3,4),(541.472791510983,541.552434384195,
541.631983655514,541.711457142406,541.790872599625,541.87301873644,541.952382639305,
542.031745690708,542.111123880599,542.190533205499,542.270030489991,542.349580264739,
542.42923733723,542.448041694147,542.528006652934,542.607877241039,542.687670978065,
542.767405323156,542.847097688464,542.926776907005,543.006452670794,543.086140702662,
543.165856729773,543.245660292703,543.325513017381,543.405479427032,543.447025196346,
543.526990155133,543.606860743238,543.686654480265,543.766388825356,543.846081190663,
543.925760409204,544.005436172993,544.085124204861,544.164840231972,544.244643794903,
544.32449651958,544.404462929231,544.446008698545,544.525973657332,544.605844245437,
544.685637982464,544.765372327555,544.845064692863,544.924743911404,545.004419675193,
545.084107707061,545.163823734172,545.243627297103,545.32348002178,545.403446431431,
545.444992200744,545.524957159531,545.604827747636,545.684621484663,545.764355829754,
545.844048195061,545.923727413602,546.003403177391,546.083091209259,546.16280723637,
546.242610799301,546.322463523979,546.402429933629,546.443975702943,546.52394066173,
546.603811249835,546.683604986862,546.763339331953,546.84303169726,546.922710915801,
547.00238667959,547.082074711458,547.161790738569,547.2415943015,547.321447026177,
547.401413435828,547.442959205142,547.53892448688,547.634366343838,547.72884563209,
547.755976610976),.UNSPECIFIED.);
#191=B_SPLINE_CURVE_WITH_KNOTS('',3,(#16863,#16864,#16865,#16866,#16867,
#16868,#16869,#16870,#16871,#16872),.UNSPECIFIED.,.F.,.F.,(4,1,1,1,1,1,
1,4),(547.755976818162,548.441942707342,549.440926209541,550.43990971174,
551.438893213939,552.437876716138,553.436860218338,554.039162125342),
 .UNSPECIFIED.);
#192=B_SPLINE_CURVE_WITH_KNOTS('',3,(#16874,#16875,#16876,#16877,#16878,
#16879,#16880,#16881,#16882,#16883),.UNSPECIFIED.,.F.,.F.,(4,1,1,1,1,1,
1,4),(554.039162125342,554.435843720537,555.434827222736,556.433810724935,
557.432794227134,558.431777729333,559.430761231533,560.322347432522),
 .UNSPECIFIED.);
#193=B_SPLINE_CURVE_WITH_KNOTS('',3,(#16885,#16886,#16887,#16888,#16889,
#16890,#16891,#16892,#16893,#16894,#16895),.UNSPECIFIED.,.F.,.F.,(4,1,1,
1,1,1,1,1,4),(560.322347432522,560.429744733732,561.428728235931,562.42771173813,
563.426695240329,564.425678742528,565.424662244728,566.423645746927,566.605532739701),
 .UNSPECIFIED.);
#194=B_SPLINE_CURVE_WITH_KNOTS('',3,(#16897,#16898,#16899,#16900,#16901,
#16902,#16903,#16904,#16905,#16906),.UNSPECIFIED.,.F.,.F.,(4,1,1,1,1,1,
1,4),(566.605532739701,567.422629249126,568.421612751325,569.420596253524,
570.419579755723,571.418563257923,572.417546760122,572.888718046881),
 .UNSPECIFIED.);
#195=B_SPLINE_CURVE_WITH_KNOTS('',3,(#16908,#16909,#16910,#16911,#16912,
#16913,#16914,#16915,#16916,#16917),.UNSPECIFIED.,.F.,.F.,(4,1,1,1,1,1,
1,4),(572.888718046881,573.416530262321,574.41551376452,575.414497266719,
576.413480768918,577.412464271117,578.411447773317,579.17190335406),
 .UNSPECIFIED.);
#196=B_SPLINE_CURVE_WITH_KNOTS('',3,(#16919,#16920,#16921,#16922,#16923,
#16924,#16925,#16926,#16927,#16928,#16929),.UNSPECIFIED.,.F.,.F.,(4,1,1,
1,1,1,1,1,4),(579.17190335406,579.410431275516,580.409414777715,581.408398279914,
582.407381782113,583.406365284312,584.405348786512,585.404332288711,585.45508866124),
 .UNSPECIFIED.);
#197=B_SPLINE_CURVE_WITH_KNOTS('',3,(#16931,#16932,#16933,#16934,#16935,
#16936,#16937,#16938,#16939,#16940),.UNSPECIFIED.,.F.,.F.,(4,1,1,1,1,1,
1,4),(585.45508866124,586.40331579091,587.402299293109,588.401282795308,
589.400266297508,590.399249799707,591.398233301906,591.738266415292),
 .UNSPECIFIED.);
#198=B_SPLINE_CURVE_WITH_KNOTS('',3,(#16942,#16943,#16944,#16945,#16946,
#16947,#16948,#16949,#16950,#16951,#16952,#16953,#16954,#16955,#16956,#16957,
#16958,#16959,#16960,#16961,#16962,#16963,#16964,#16965,#16966,#16967,#16968,
#16969,#16970,#16971,#16972,#16973,#16974,#16975,#16976,#16977,#16978,#16979,
#16980,#16981,#16982,#16983,#16984,#16985,#16986,#16987,#16988,#16989,#16990,
#16991,#16992,#16993,#16994,#16995,#16996,#16997,#16998,#16999,#17000,#17001,
#17002,#17003,#17004,#17005,#17006,#17007,#17008,#17009,#17010,#17011,#17012,
#17013,#17014,#17015,#17016,#17017,#17018,#17019,#17020,#17021,#17022,#17023,
#17024,#17025,#17026,#17027,#17028,#17029,#17030,#17031,#17032,#17033,#17034,
#17035,#17036,#17037,#17038,#17039,#17040,#17041,#17042,#17043,#17044,#17045,
#17046,#17047,#17048,#17049,#17050,#17051,#17052,#17053,#17054,#17055,#17056,
#17057,#17058,#17059,#17060,#17061,#17062,#17063,#17064,#17065,#17066,#17067,
#17068,#17069,#17070,#17071,#17072,#17073,#17074,#17075,#17076,#17077,#17078,
#17079,#17080,#17081,#17082,#17083,#17084,#17085,#17086,#17087,#17088,#17089,
#17090,#17091,#17092,#17093,#17094,#17095,#17096,#17097,#17098,#17099,#17100,
#17101,#17102,#17103,#17104,#17105,#17106,#17107,#17108,#17109,#17110,#17111,
#17112,#17113,#17114,#17115,#17116,#17117,#17118,#17119,#17120,#17121,#17122,
#17123,#17124,#17125,#17126,#17127,#17128,#17129,#17130,#17131,#17132,#17133,
#17134,#17135,#17136,#17137,#17138,#17139,#17140,#17141,#17142,#17143,#17144,
#17145,#17146,#17147,#17148,#17149,#17150,#17151,#17152,#17153,#17154,#17155,
#17156,#17157,#17158,#17159,#17160,#17161,#17162,#17163,#17164,#17165,#17166,
#17167,#17168,#17169,#17170,#17171,#17172,#17173,#17174,#17175,#17176,#17177,
#17178,#17179,#17180,#17181,#17182,#17183,#17184,#17185,#17186,#17187,#17188),
 .UNSPECIFIED.,.F.,.F.,(4,3,3,3,3,3,3,3,3,3,3,3,3,3,3,3,3,3,3,3,3,3,3,3,
3,3,3,3,3,3,3,3,3,3,3,3,3,3,3,3,3,3,3,3,3,3,3,3,3,3,3,3,3,3,3,3,3,3,3,3,
3,3,3,3,3,3,3,3,3,3,3,3,3,3,3,3,3,3,3,3,3,3,4),(591.738273968419,591.82064182288,
591.90035776133,591.980080161589,592.059824638625,592.139606817585,592.219485387332,
592.299421470385,592.379470642451,592.397216804105,592.477181762892,592.557052350997,
592.636846088023,592.716580433114,592.796272798421,592.875952016962,592.955627780751,
593.035315812619,593.11503183973,593.194835402661,593.274688127339,593.354654536989,
593.396200306304,593.476165265091,593.556035853196,593.635829590223,593.715563935314,
593.795256300621,593.874935519162,593.954611282952,594.034299314819,594.114015341931,
594.193818904861,594.273671629539,594.35363803919,594.395183808503,594.47514876729,
594.555019355395,594.634813092421,594.714547437512,594.79423980282,594.873919021361,
594.95359478515,595.033282817018,595.112998844129,595.19280240706,595.272655131737,
595.352621541388,595.394167310702,595.474132269489,595.554002857594,595.633796594621,
595.713530939713,595.793223305019,595.872902523561,595.95257828735,596.032266319218,
596.11198234633,596.191785909261,596.271638633939,596.35160504359,596.393150812902,
596.473115771689,596.552986359794,596.632780096821,596.712514441912,596.792206807219,
596.871886025761,596.95156178955,597.031249821418,597.110965848529,597.19076941146,
597.270622136138,597.350588545789,597.392134315101,597.472660730037,597.553090017382,
597.633437415374,597.713718108436,597.793943515459,597.874135612635,597.954320611889,
598.021459275599),.UNSPECIFIED.);
#199=B_SPLINE_CURVE_WITH_KNOTS('',3,(#17190,#17191,#17192,#17193,#17194,
#17195,#17196,#17197,#17198,#17199),.UNSPECIFIED.,.F.,.F.,(4,1,1,1,1,1,
1,4),(598.021466925895,598.3911178173,599.390101319499,600.389084821698,
601.388068323897,602.387051826097,603.386035328296,604.304644582779),
 .UNSPECIFIED.);
#200=B_SPLINE_CURVE_WITH_KNOTS('',3,(#17201,#17202,#17203,#17204,#17205,
#17206,#17207,#17208,#17209,#17210,#17211,#17212),.UNSPECIFIED.,.F.,.F.,
(4,2,1,1,1,1,1,1,4),(604.304644582779,604.385018830495,605.384002332694,
606.382985834893,607.381969337092,608.380952839292,609.379936341491,610.37891984369,
610.587829889958),.UNSPECIFIED.);
#201=B_SPLINE_CURVE_WITH_KNOTS('',3,(#17214,#17215,#17216,#17217,#17218,
#17219,#17220,#17221,#17222,#17223),.UNSPECIFIED.,.F.,.F.,(4,1,1,1,1,1,
1,4),(610.587829889958,611.377903345889,612.376886848088,613.375870350287,
614.374853852486,615.373837354686,616.372820856885,616.871015197138),
 .UNSPECIFIED.);
#202=B_SPLINE_CURVE_WITH_KNOTS('',3,(#17225,#17226,#17227,#17228,#17229,
#17230,#17231,#17232,#17233,#17234),.UNSPECIFIED.,.F.,.F.,(4,1,1,1,1,1,
1,4),(616.871015197138,617.371804359084,618.370787861283,619.369771363482,
620.368754865682,621.367738367881,622.36672187008,623.154200504317),
 .UNSPECIFIED.);
#203=B_SPLINE_CURVE_WITH_KNOTS('',3,(#17236,#17237,#17238,#17239,#17240,
#17241,#17242,#17243,#17244,#17245,#17246),.UNSPECIFIED.,.F.,.F.,(4,1,1,
1,1,1,1,1,4),(623.154200504317,623.365705372279,624.364688874478,625.363672376677,
626.362655878877,627.361639381076,628.360622883275,629.359606385474,629.437385811497),
 .UNSPECIFIED.);
#204=B_SPLINE_CURVE_WITH_KNOTS('',3,(#17248,#17249,#17250,#17251,#17252,
#17253,#17254,#17255,#17256,#17257),.UNSPECIFIED.,.F.,.F.,(4,1,1,1,1,1,
1,4),(629.437385811497,630.358589887673,631.357573389873,632.356556892072,
633.355540394271,634.35452389647,635.353507398669,635.72056345413),
 .UNSPECIFIED.);
#205=B_SPLINE_CURVE_WITH_KNOTS('',3,(#17259,#17260,#17261,#17262,#17263,
#17264,#17265,#17266,#17267,#17268,#17269,#17270,#17271,#17272,#17273,#17274,
#17275,#17276,#17277,#17278,#17279,#17280,#17281,#17282,#17283,#17284,#17285,
#17286,#17287,#17288,#17289,#17290,#17291,#17292,#17293,#17294,#17295,#17296,
#17297,#17298,#17299,#17300,#17301,#17302,#17303,#17304,#17305,#17306,#17307,
#17308,#17309,#17310,#17311,#17312,#17313,#17314,#17315,#17316,#17317,#17318,
#17319,#17320,#17321,#17322,#17323,#17324,#17325,#17326,#17327,#17328,#17329,
#17330,#17331,#17332,#17333,#17334,#17335,#17336,#17337,#17338,#17339,#17340,
#17341,#17342,#17343,#17344,#17345,#17346,#17347,#17348,#17349,#17350,#17351,
#17352,#17353,#17354,#17355,#17356,#17357,#17358,#17359,#17360,#17361,#17362,
#17363,#17364,#17365,#17366,#17367,#17368,#17369,#17370,#17371,#17372,#17373,
#17374,#17375,#17376,#17377,#17378,#17379,#17380,#17381,#17382,#17383,#17384,
#17385,#17386,#17387,#17388,#17389,#17390,#17391,#17392,#17393,#17394,#17395,
#17396,#17397,#17398,#17399,#17400,#17401,#17402,#17403,#17404,#17405,#17406,
#17407,#17408,#17409,#17410,#17411,#17412,#17413,#17414,#17415,#17416,#17417,
#17418,#17419,#17420,#17421,#17422,#17423,#17424,#17425,#17426,#17427,#17428,
#17429,#17430,#17431,#17432,#17433,#17434,#17435,#17436,#17437,#17438,#17439,
#17440,#17441,#17442,#17443,#17444,#17445,#17446,#17447,#17448,#17449,#17450,
#17451,#17452,#17453,#17454,#17455,#17456,#17457,#17458,#17459,#17460,#17461,
#17462,#17463,#17464,#17465,#17466,#17467,#17468,#17469,#17470,#17471,#17472,
#17473,#17474,#17475,#17476,#17477,#17478,#17479,#17480,#17481,#17482,#17483,
#17484,#17485,#17486,#17487,#17488,#17489,#17490,#17491,#17492,#17493,#17494,
#17495,#17496,#17497,#17498,#17499,#17500,#17501,#17502,#17503,#17504,#17505),
 .UNSPECIFIED.,.F.,.F.,(4,3,3,3,3,3,3,3,3,3,3,3,3,3,3,3,3,3,3,3,3,3,3,3,
3,3,3,3,3,3,3,3,3,3,3,3,3,3,3,3,3,3,3,3,3,3,3,3,3,3,3,3,3,3,3,3,3,3,3,3,
3,3,3,3,3,3,3,3,3,3,3,3,3,3,3,3,3,3,3,3,3,3,4),(635.720571118676,635.800716360848,
635.880864171963,635.961029670184,636.041227981188,636.121525941313,636.201875952468,
636.282358567307,636.352490900868,636.432453727681,636.512322182468,636.592113786839,
636.671846001927,636.751536241864,636.831213348658,636.910887009352,636.990572948562,
637.070286895249,637.15008840676,637.229939093392,637.309903503355,637.351474403067,
637.431440742958,637.511312700702,637.591107794774,637.670843483185,637.750537176951,
637.830217697708,637.909894747326,637.989584047587,638.069301324594,638.149106103173,
638.228960025913,638.308927596002,638.350457905267,638.430427643991,638.510303040276,
638.590101608879,638.669840804149,638.749538033481,638.829222121093,638.908902756573,
638.988595658521,639.068316549863,639.148124943528,639.227982487151,639.307953655806,
639.349441407466,639.429391681465,639.509247568071,639.58902660077,639.668746252476,
639.748423949045,639.828088581936,639.907749812979,639.987423377342,640.067125014586,
640.146914377732,640.22675298909,640.306705541614,640.348424909665,640.428402857143,
640.508286367581,640.588092949365,640.66784005044,640.747545071756,640.82723675789,
640.906924871261,640.986625124445,641.066353234259,641.146168609493,641.226033010865,
641.306010786103,641.347408411864,641.429451913613,641.509413080617,641.589297472675,
641.669120771521,641.752779685104,641.832531129424,641.912269375975,641.992019605056,
642.003756425856),.UNSPECIFIED.);
#206=B_SPLINE_CURVE_WITH_KNOTS('',3,(#17507,#17508,#17509,#17510,#17511,
#17512,#17513,#17514),.UNSPECIFIED.,.F.,.F.,(4,1,1,1,1,4),(642.003763862697,
642.346391914063,643.345375416262,644.344358918462,645.343342420661,646.269689253992),
 .UNSPECIFIED.);
#207=B_SPLINE_CURVE_WITH_KNOTS('',3,(#17518,#17519,#17520,#17521,#17522,
#17523,#17524,#17525),.UNSPECIFIED.,.F.,.F.,(4,1,1,1,1,4),(-648.340292927258,
-647.840801176158,-647.341309425059,-646.342325922859,-645.34334242066,
-644.977443081154),.UNSPECIFIED.);
#208=B_SPLINE_CURVE_WITH_KNOTS('',3,(#17527,#17528,#17529,#17530,#17531,
#17532,#17533,#17534,#17535,#17536),.UNSPECIFIED.,.F.,.F.,(4,1,1,1,1,1,
1,4),(-644.977443081154,-644.344358918461,-643.345375416262,-642.346391914063,
-641.347408411864,-640.348424909664,-639.349441407465,-638.694257773975),
 .UNSPECIFIED.);
#209=B_SPLINE_CURVE_WITH_KNOTS('',3,(#17538,#17539,#17540,#17541,#17542,
#17543,#17544,#17545,#17546,#17547,#17548,#17549,#17550,#17551,#17552,#17553,
#17554,#17555,#17556,#17557,#17558,#17559,#17560,#17561,#17562,#17563,#17564,
#17565,#17566,#17567,#17568,#17569,#17570,#17571,#17572,#17573,#17574,#17575,
#17576,#17577,#17578,#17579,#17580,#17581,#17582,#17583,#17584,#17585,#17586,
#17587,#17588,#17589,#17590,#17591,#17592,#17593,#17594,#17595,#17596,#17597,
#17598,#17599,#17600,#17601,#17602,#17603,#17604,#17605,#17606,#17607,#17608,
#17609,#17610,#17611,#17612,#17613,#17614,#17615,#17616,#17617,#17618,#17619,
#17620,#17621,#17622,#17623,#17624,#17625,#17626,#17627,#17628,#17629,#17630,
#17631,#17632,#17633,#17634,#17635,#17636,#17637,#17638,#17639,#17640,#17641,
#17642,#17643,#17644,#17645,#17646,#17647,#17648,#17649,#17650,#17651,#17652,
#17653,#17654,#17655,#17656,#17657,#17658,#17659,#17660,#17661,#17662,#17663,
#17664,#17665,#17666,#17667,#17668,#17669,#17670,#17671,#17672,#17673,#17674,
#17675,#17676,#17677,#17678,#17679,#17680,#17681,#17682,#17683,#17684,#17685,
#17686,#17687,#17688,#17689,#17690,#17691,#17692,#17693,#17694,#17695,#17696,
#17697,#17698,#17699,#17700,#17701,#17702,#17703,#17704,#17705,#17706,#17707,
#17708,#17709,#17710,#17711,#17712,#17713,#17714,#17715,#17716,#17717,#17718,
#17719,#17720,#17721,#17722,#17723,#17724,#17725,#17726,#17727,#17728,#17729,
#17730,#17731,#17732,#17733,#17734,#17735,#17736,#17737,#17738,#17739,#17740,
#17741,#17742,#17743,#17744,#17745,#17746,#17747,#17748,#17749,#17750,#17751,
#17752,#17753,#17754,#17755,#17756,#17757,#17758,#17759,#17760,#17761,#17762,
#17763,#17764,#17765,#17766,#17767,#17768,#17769,#17770,#17771,#17772,#17773,
#17774,#17775,#17776,#17777,#17778,#17779,#17780,#17781),.UNSPECIFIED.,
 .F.,.F.,(4,3,3,3,3,3,3,3,3,3,3,3,3,3,3,3,3,3,3,3,3,3,3,3,3,3,3,3,3,3,3,
3,3,3,3,3,3,3,3,3,3,3,3,3,3,3,3,3,3,3,3,3,3,3,3,3,3,3,3,3,3,3,3,3,3,3,3,
3,3,3,3,3,3,3,3,3,3,3,3,3,3,4),(-638.694257653504,-638.602314147676,-638.509906521229,
-638.416901408164,-638.350457905266,-638.270491791684,-638.190620021241,
-638.110825075614,-638.031089496909,-637.951395874201,-637.871715366522,
-637.792038293996,-637.712348934841,-637.632631562926,-637.552826635138,
-637.472972532192,-637.393004735029,-637.351474403067,-637.27151143441,
-637.191642862227,-637.111851164813,-637.032118880961,-636.952428596482,
-636.872751481486,-636.793077835144,-636.713391932841,-636.633678045632,
-636.553876627634,-636.474026053943,-636.394061786297,-636.352490900868,
-636.272525125158,-636.192653713066,-636.112859145831,-636.033123965146,
-635.953430759684,-635.873750696862,-635.794074086318,-635.714385205951,
-635.634668329325,-635.554863919623,-635.475010348465,-635.395043100077,
-635.353507398669,-635.27354234991,-635.193671668647,-635.113877835379,
-635.034143391066,-634.954450923656,-634.874771599002,-634.795095726619,
-634.715407583757,-634.635691443333,-634.555887764108,-634.476034921271,
-634.396068391543,-634.354523896469,-634.274559218377,-634.194688914776,
-634.114895465763,-634.035161411905,-633.955469340762,-633.87579041984,
-633.796114955786,-633.716427225518,-633.63671150162,-633.556908242843,
-633.477055823306,-633.397089717725,-633.35554039427,-633.276230505782,
-633.197014541243,-633.117874400493,-633.038792051091,-632.959743562529,
-632.880711844586,-632.801680658467,-632.722633768204,-632.643509498184,
-632.564346038251,-632.485064970735,-632.411072466795),.UNSPECIFIED.);
#210=B_SPLINE_CURVE_WITH_KNOTS('',3,(#17783,#17784,#17785,#17786,#17787,
#17788,#17789,#17790,#17791,#17792,#17793,#17794),.UNSPECIFIED.,.F.,.F.,
(4,2,1,1,1,1,1,1,4),(-632.411072466795,-632.356556892071,-631.357573389872,
-630.358589887673,-629.359606385474,-628.360622883274,-627.361639381075,
-626.362655878876,-626.127887159616),.UNSPECIFIED.);
#211=B_SPLINE_CURVE_WITH_KNOTS('',3,(#17796,#17797,#17798,#17799,#17800,
#17801,#17802,#17803,#17804,#17805),.UNSPECIFIED.,.F.,.F.,(4,1,1,1,1,1,
1,4),(-626.127887159616,-625.363672376677,-624.364688874478,-623.365705372279,
-622.366721870079,-621.36773836788,-620.368754865681,-619.844701852436),
 .UNSPECIFIED.);
#212=B_SPLINE_CURVE_WITH_KNOTS('',3,(#17807,#17808,#17809,#17810,#17811,
#17812,#17813,#17814,#17815,#17816),.UNSPECIFIED.,.F.,.F.,(4,1,1,1,1,1,
1,4),(-619.844701852436,-619.369771363482,-618.370787861283,-617.371804359084,
-616.372820856884,-615.373837354685,-614.374853852486,-613.561521139307),
 .UNSPECIFIED.);
#213=B_SPLINE_CURVE_WITH_KNOTS('',3,(#17818,#17819,#17820,#17821,#17822,
#17823,#17824,#17825,#17826,#17827,#17828,#17829,#17830,#17831,#17832,#17833,
#17834,#17835,#17836,#17837,#17838,#17839,#17840,#17841,#17842,#17843,#17844,
#17845,#17846,#17847,#17848,#17849,#17850,#17851,#17852,#17853,#17854,#17855,
#17856,#17857,#17858,#17859,#17860,#17861,#17862,#17863,#17864,#17865,#17866,
#17867,#17868,#17869,#17870,#17871,#17872,#17873,#17874,#17875,#17876,#17877,
#17878,#17879,#17880,#17881,#17882,#17883,#17884,#17885,#17886,#17887,#17888,
#17889,#17890,#17891,#17892,#17893,#17894,#17895,#17896,#17897,#17898,#17899,
#17900,#17901,#17902,#17903,#17904,#17905,#17906,#17907,#17908,#17909,#17910,
#17911,#17912,#17913,#17914,#17915,#17916,#17917,#17918,#17919,#17920,#17921,
#17922,#17923,#17924,#17925,#17926,#17927,#17928,#17929,#17930,#17931,#17932,
#17933,#17934,#17935,#17936,#17937,#17938,#17939,#17940,#17941,#17942,#17943,
#17944,#17945,#17946,#17947,#17948,#17949,#17950,#17951,#17952,#17953,#17954,
#17955,#17956,#17957,#17958,#17959,#17960,#17961,#17962,#17963,#17964,#17965,
#17966,#17967,#17968,#17969,#17970,#17971,#17972,#17973,#17974,#17975,#17976,
#17977,#17978,#17979,#17980,#17981,#17982,#17983,#17984,#17985,#17986,#17987,
#17988,#17989,#17990,#17991,#17992,#17993,#17994,#17995,#17996,#17997,#17998,
#17999,#18000,#18001,#18002,#18003,#18004,#18005,#18006,#18007,#18008,#18009,
#18010,#18011,#18012,#18013,#18014,#18015,#18016,#18017,#18018,#18019,#18020,
#18021,#18022,#18023,#18024,#18025,#18026,#18027,#18028,#18029,#18030,#18031,
#18032,#18033,#18034,#18035,#18036,#18037,#18038,#18039,#18040,#18041,#18042,
#18043,#18044,#18045,#18046,#18047,#18048,#18049,#18050,#18051,#18052,#18053,
#18054,#18055,#18056,#18057,#18058,#18059,#18060,#18061),.UNSPECIFIED.,
 .F.,.F.,(4,3,3,3,3,3,3,3,3,3,3,3,3,3,3,3,3,3,3,3,3,3,3,3,3,3,3,3,3,3,3,
3,3,3,3,3,3,3,3,3,3,3,3,3,3,3,3,3,3,3,3,3,3,3,3,3,3,3,3,3,3,3,3,3,3,3,3,
3,3,3,3,3,3,3,3,3,3,3,3,3,3,4),(-613.561516545257,-613.442298360645,-613.375870350287,
-613.295905391501,-613.216034803397,-613.136241066371,-613.056506721281,
-612.976814355976,-612.897135137436,-612.817459373648,-612.737771341781,
-612.658055314671,-612.578251751741,-612.498399027065,-612.418432617415,
-612.376886848088,-612.2969218893,-612.217051301196,-612.137257564168,-612.057523219077,
-611.97783085377,-611.898151635228,-611.818475871439,-611.738787839571,
-611.659071812459,-611.579268249528,-611.49941552485,-611.419449115199,
-611.377903345889,-611.297938387101,-611.218067798997,-611.13827406197,
-611.058539716878,-610.978847351571,-610.89916813303,-610.81949236924,-610.739804337372,
-610.660088310261,-610.58028474733,-610.500432022652,-610.420465613001,
-610.378919843689,-610.298954884902,-610.219084296797,-610.13929055977,
-610.059556214679,-609.979863849373,-609.900184630831,-609.820508867042,
-609.740820835175,-609.661104808063,-609.581301245133,-609.501448520455,
-609.421482110805,-609.37993634149,-609.299971382703,-609.220100794598,
-609.140307057571,-609.06057271248,-608.980880347173,-608.901201128632,
-608.821525364843,-608.741837332975,-608.662121305864,-608.582317742933,
-608.502465018256,-608.422498608605,-608.380952839291,-608.300987880504,
-608.221117292399,-608.141323555372,-608.061589210281,-607.981896844975,
-607.902217626433,-607.822541862644,-607.742853830776,-607.663137803665,
-607.583334240735,-607.503481516057,-607.423515106406,-607.381969337092,
-607.278331238077),.UNSPECIFIED.);
#214=B_SPLINE_CURVE_WITH_KNOTS('',3,(#18063,#18064,#18065,#18066,#18067,
#18068,#18069,#18070,#18071,#18072),.UNSPECIFIED.,.F.,.F.,(4,1,1,1,1,1,
1,4),(-607.278322184525,-606.382985834893,-605.384002332694,-604.385018830495,
-603.386035328296,-602.387051826096,-601.388068323897,-600.995145930897),
 .UNSPECIFIED.);
#215=B_SPLINE_CURVE_WITH_KNOTS('',3,(#18074,#18075,#18076,#18077,#18078,
#18079,#18080,#18081,#18082,#18083),.UNSPECIFIED.,.F.,.F.,(4,1,1,1,1,1,
1,4),(-600.995145930897,-600.389084821698,-599.390101319499,-598.3911178173,
-597.3921343151,-596.393150812901,-595.394167310702,-594.711960623718),
 .UNSPECIFIED.);
#216=B_SPLINE_CURVE_WITH_KNOTS('',3,(#18085,#18086,#18087,#18088,#18089,
#18090,#18091,#18092,#18093,#18094),.UNSPECIFIED.,.F.,.F.,(4,1,1,1,1,1,
1,4),(-594.711960623718,-594.395183808503,-593.396200306304,-592.397216804105,
-591.398233301905,-590.399249799706,-589.400266297507,-588.428775316538),
 .UNSPECIFIED.);
#217=B_SPLINE_CURVE_WITH_KNOTS('',3,(#18096,#18097,#18098,#18099,#18100,
#18101,#18102,#18103,#18104,#18105,#18106,#18107),.UNSPECIFIED.,.F.,.F.,
(4,2,1,1,1,1,1,1,4),(-588.428775316538,-588.401282795308,-587.402299293109,
-586.40331579091,-585.40433228871,-584.405348786511,-583.406365284312,-582.407381782113,
-582.145590009359),.UNSPECIFIED.);
#218=B_SPLINE_CURVE_WITH_KNOTS('',3,(#18109,#18110,#18111,#18112,#18113,
#18114,#18115,#18116,#18117,#18118),.UNSPECIFIED.,.F.,.F.,(4,1,1,1,1,1,
1,4),(-582.145590009359,-581.408398279914,-580.409414777715,-579.410431275515,
-578.411447773316,-577.412464271117,-576.413480768918,-575.862404702179),
 .UNSPECIFIED.);
#219=B_SPLINE_CURVE_WITH_KNOTS('',3,(#18120,#18121,#18122,#18123,#18124,
#18125,#18126,#18127,#18128,#18129),.UNSPECIFIED.,.F.,.F.,(4,1,1,1,1,1,
1,4),(-575.862404702179,-575.414497266719,-574.41551376452,-573.41653026232,
-572.417546760121,-571.418563257922,-570.419579755723,-569.579219395),
 .UNSPECIFIED.);
#220=B_SPLINE_CURVE_WITH_KNOTS('',3,(#18131,#18132,#18133,#18134,#18135,
#18136,#18137,#18138,#18139,#18140,#18141),.UNSPECIFIED.,.F.,.F.,(4,1,1,
1,1,1,1,1,4),(-569.579219395,-569.420596253524,-568.421612751325,-567.422629249126,
-566.423645746926,-565.424662244727,-564.425678742528,-563.426695240329,
-563.29603408782),.UNSPECIFIED.);
#221=B_SPLINE_CURVE_WITH_KNOTS('',3,(#18143,#18144,#18145,#18146,#18147,
#18148,#18149,#18150,#18151,#18152),.UNSPECIFIED.,.F.,.F.,(4,1,1,1,1,1,
1,4),(-563.29603408782,-562.42771173813,-561.428728235931,-560.429744733731,
-559.430761231532,-558.431777729333,-557.432794227134,-557.012848780641),
 .UNSPECIFIED.);
#222=B_SPLINE_CURVE_WITH_KNOTS('',3,(#18154,#18155,#18156,#18157,#18158,
#18159,#18160,#18161,#18162,#18163),.UNSPECIFIED.,.F.,.F.,(4,1,1,1,1,1,
1,4),(-557.012848780641,-556.433810724935,-555.434827222736,-554.435843720536,
-553.436860218337,-552.437876716138,-551.438893213939,-550.729663473461),
 .UNSPECIFIED.);
#223=B_SPLINE_CURVE_WITH_KNOTS('',3,(#18165,#18166,#18167,#18168,#18169,
#18170,#18171,#18172,#18173,#18174,#18175,#18176,#18177,#18178,#18179,#18180,
#18181,#18182,#18183,#18184,#18185,#18186,#18187,#18188,#18189,#18190,#18191,
#18192,#18193,#18194,#18195,#18196,#18197,#18198,#18199,#18200,#18201,#18202,
#18203,#18204,#18205,#18206,#18207,#18208,#18209,#18210,#18211,#18212,#18213,
#18214,#18215,#18216,#18217,#18218,#18219,#18220,#18221,#18222,#18223,#18224,
#18225,#18226,#18227,#18228,#18229,#18230,#18231,#18232,#18233,#18234,#18235,
#18236,#18237,#18238,#18239,#18240,#18241,#18242,#18243,#18244,#18245,#18246,
#18247,#18248,#18249,#18250,#18251,#18252,#18253,#18254,#18255,#18256,#18257,
#18258,#18259,#18260,#18261,#18262,#18263,#18264,#18265,#18266,#18267,#18268,
#18269,#18270,#18271,#18272,#18273,#18274,#18275,#18276,#18277,#18278,#18279,
#18280,#18281,#18282,#18283,#18284,#18285,#18286,#18287,#18288,#18289,#18290,
#18291,#18292,#18293,#18294,#18295,#18296,#18297,#18298,#18299,#18300,#18301,
#18302,#18303,#18304,#18305,#18306,#18307,#18308,#18309,#18310,#18311,#18312,
#18313,#18314,#18315,#18316,#18317,#18318,#18319,#18320,#18321,#18322,#18323,
#18324,#18325,#18326,#18327,#18328,#18329,#18330,#18331,#18332,#18333,#18334,
#18335,#18336,#18337,#18338,#18339,#18340,#18341,#18342,#18343,#18344,#18345,
#18346,#18347,#18348,#18349,#18350,#18351,#18352,#18353,#18354,#18355,#18356,
#18357,#18358,#18359,#18360,#18361,#18362,#18363,#18364,#18365,#18366,#18367,
#18368,#18369,#18370,#18371,#18372,#18373,#18374,#18375,#18376,#18377,#18378,
#18379,#18380,#18381,#18382,#18383,#18384,#18385,#18386,#18387,#18388,#18389,
#18390,#18391,#18392,#18393,#18394,#18395,#18396,#18397,#18398,#18399,#18400,
#18401,#18402,#18403,#18404,#18405,#18406,#18407,#18408),.UNSPECIFIED.,
 .F.,.F.,(4,3,3,3,3,3,3,3,3,3,3,3,3,3,3,3,3,3,3,3,3,3,3,3,3,3,3,3,3,3,3,
3,3,3,3,3,3,3,3,3,3,3,3,3,3,3,3,3,3,3,3,3,3,3,3,3,3,3,3,3,3,3,3,3,3,3,3,
3,3,3,3,3,3,3,3,3,3,3,3,3,3,4),(-550.729663311796,-550.632575528383,-550.534108600299,
-550.43990971174,-550.359944752953,-550.280074164848,-550.200280427822,
-550.120546082731,-550.040853717424,-549.961174498883,-549.881498735094,
-549.801810703227,-549.722094676115,-549.642291113185,-549.562438388507,
-549.482471978857,-549.440926209541,-549.360961250753,-549.281090662649,
-549.201296925622,-549.12156258053,-549.041870215223,-548.962190996682,
-548.882515232893,-548.802827201024,-548.723111173913,-548.643307610982,
-548.563454886304,-548.483488476653,-548.441942707341,-548.361977748554,
-548.282107160449,-548.202313423422,-548.122579078331,-548.042886713024,
-547.963207494483,-547.883531730693,-547.803843698825,-547.724127671714,
-547.644324108783,-547.564471384105,-547.484504974455,-547.442959205142,
-547.362994246355,-547.28312365825,-547.203329921224,-547.123595576133,
-547.043903210826,-546.964223992285,-546.884548228496,-546.804860196628,
-546.725144169517,-546.645340606587,-546.565487881909,-546.485521472259,
-546.443975702943,-546.364010744156,-546.284140156051,-546.204346419024,
-546.124612073933,-546.044919708626,-545.965240490085,-545.885564726296,
-545.805876694428,-545.726160667317,-545.646357104386,-545.566504379708,
-545.486537970058,-545.444992200744,-545.365034063542,-545.285170294057,
-545.205383365879,-545.125655813102,-545.045970216838,-544.966297734187,
-544.886628672647,-544.806947303307,-544.727237892889,-544.647440945723,
-544.567594784061,-544.487635050059,-544.446478166396),.UNSPECIFIED.);
#224=B_SPLINE_CURVE_WITH_KNOTS('',3,(#18410,#18411,#18412,#18413,#18414,
#18415,#18416,#18417,#18418,#18419,#18420,#18421,#18422,#18423,#18424,#18425,
#18426,#18427,#18428,#18429,#18430,#18431,#18432,#18433,#18434,#18435,#18436,
#18437,#18438,#18439,#18440,#18441,#18442,#18443,#18444,#18445,#18446,#18447,
#18448,#18449,#18450,#18451,#18452,#18453,#18454,#18455,#18456,#18457,#18458,
#18459,#18460,#18461,#18462,#18463,#18464,#18465,#18466,#18467,#18468,#18469,
#18470,#18471,#18472,#18473,#18474,#18475,#18476,#18477,#18478,#18479,#18480,
#18481,#18482,#18483,#18484,#18485,#18486,#18487,#18488,#18489,#18490,#18491,
#18492,#18493,#18494,#18495,#18496,#18497,#18498,#18499,#18500,#18501,#18502,
#18503,#18504,#18505,#18506,#18507,#18508,#18509,#18510,#18511,#18512,#18513,
#18514,#18515,#18516,#18517,#18518,#18519,#18520,#18521,#18522,#18523,#18524,
#18525,#18526,#18527,#18528,#18529,#18530,#18531,#18532,#18533,#18534,#18535,
#18536,#18537,#18538,#18539,#18540,#18541,#18542,#18543,#18544,#18545,#18546,
#18547,#18548,#18549,#18550,#18551,#18552,#18553,#18554,#18555,#18556,#18557,
#18558,#18559,#18560,#18561,#18562,#18563,#18564,#18565,#18566,#18567,#18568,
#18569,#18570,#18571,#18572,#18573,#18574,#18575,#18576,#18577,#18578,#18579,
#18580,#18581,#18582,#18583,#18584,#18585,#18586,#18587,#18588,#18589,#18590,
#18591,#18592,#18593,#18594,#18595,#18596,#18597,#18598,#18599,#18600,#18601,
#18602,#18603,#18604,#18605,#18606,#18607,#18608,#18609,#18610,#18611,#18612,
#18613,#18614,#18615,#18616,#18617,#18618,#18619,#18620,#18621,#18622,#18623,
#18624,#18625,#18626,#18627,#18628,#18629,#18630,#18631,#18632,#18633,#18634,
#18635,#18636,#18637,#18638,#18639,#18640,#18641,#18642,#18643,#18644,#18645,
#18646,#18647,#18648,#18649,#18650,#18651,#18652,#18653),.UNSPECIFIED.,
 .F.,.F.,(4,3,3,3,3,3,3,3,3,3,3,3,3,3,3,3,3,3,3,3,3,3,3,3,3,3,3,3,3,3,3,
3,3,3,3,3,3,3,3,3,3,3,3,3,3,3,3,3,3,3,3,3,3,3,3,3,3,3,3,3,3,3,3,3,3,3,3,
3,3,3,3,3,3,3,3,3,3,3,3,3,3,4),(-544.446478166281,-544.366506366184,-544.286628939455,
-544.206828373337,-544.12708721549,-544.04738806054,-543.967702085404,-543.888019598603,
-543.808324883423,-543.728602218847,-543.648792019597,-543.568932711421,
-543.48895960595,-543.447025196346,-543.367060237558,-543.287189649453,
-543.207395912426,-543.127661567335,-543.047969202028,-542.968289983486,
-542.888614219697,-542.808926187829,-542.729210160717,-542.649406597786,
-542.569553873108,-542.489587463457,-542.448041694146,-542.368076735359,
-542.288206147254,-542.208412410227,-542.128678065136,-542.048985699829,
-541.969306481288,-541.889630717499,-541.809942685631,-541.730226658519,
-541.650423095588,-541.57057037091,-541.49060396126,-541.449058191947,-541.36909323316,
-541.289222645055,-541.209428908029,-541.129694562938,-541.050002197631,
-540.97032297909,-540.890647215301,-540.810959183434,-540.731243156322,
-540.651439593392,-540.571586868714,-540.491620459064,-540.450074689748,
-540.370109730961,-540.290239142856,-540.210445405829,-540.130711060738,
-540.051018695431,-539.97133947689,-539.891663713101,-539.811975681233,
-539.732259654121,-539.652456091191,-539.572603366513,-539.492636956862,
-539.451091187549,-539.371126228762,-539.291255640657,-539.21146190363,
-539.131727558539,-539.052035193232,-538.97235597469,-538.892680210901,
-538.812992179033,-538.733276151922,-538.653472588991,-538.573619864313,
-538.493653454663,-538.45210768535,-538.353290578552,-538.255807107317,
-538.163293018638),.UNSPECIFIED.);
#225=B_SPLINE_CURVE_WITH_KNOTS('',3,(#18655,#18656,#18657,#18658,#18659,
#18660,#18661,#18662,#18663,#18664),.UNSPECIFIED.,.F.,.F.,(4,1,1,1,1,1,
1,4),(-538.163292859102,-537.453124183151,-536.454140680951,-535.455157178752,
-534.456173676553,-533.457190174354,-532.458206672155,-531.880107551922),
 .UNSPECIFIED.);
#226=B_SPLINE_CURVE_WITH_KNOTS('',3,(#18666,#18667,#18668,#18669,#18670,
#18671,#18672,#18673,#18674,#18675),.UNSPECIFIED.,.F.,.F.,(4,1,1,1,1,1,
1,4),(-531.880107551922,-531.459223169956,-530.460239667756,-529.461256165557,
-528.462272663358,-527.463289161159,-526.46430565896,-525.596922244743),
 .UNSPECIFIED.);
#227=B_SPLINE_CURVE_WITH_KNOTS('',3,(#18677,#18678,#18679,#18680,#18681,
#18682,#18683,#18684,#18685,#18686,#18687),.UNSPECIFIED.,.F.,.F.,(4,1,1,
1,1,1,1,1,4),(-525.596922244743,-525.465322156761,-524.466338654561,-523.467355152362,
-522.468371650163,-521.469388147964,-520.470404645765,-519.471421143566,
-519.313736937563),.UNSPECIFIED.);
#228=B_SPLINE_CURVE_WITH_KNOTS('',3,(#18689,#18690,#18691,#18692,#18693,
#18694,#18695,#18696,#18697,#18698),.UNSPECIFIED.,.F.,.F.,(4,1,1,1,1,1,
1,4),(-519.313736937563,-518.472437641366,-517.473454139167,-516.474470636968,
-515.475487134769,-514.47650363257,-513.477520130371,-513.030551630384),
 .UNSPECIFIED.);
#229=B_SPLINE_CURVE_WITH_KNOTS('',3,(#18700,#18701,#18702,#18703,#18704,
#18705,#18706,#18707,#18708,#18709),.UNSPECIFIED.,.F.,.F.,(4,1,1,1,1,1,
1,4),(-513.030551630384,-512.478536628171,-511.479553125972,-510.480569623773,
-509.481586121574,-508.482602619375,-507.483619117176,-506.747366323204),
 .UNSPECIFIED.);
#230=B_SPLINE_CURVE_WITH_KNOTS('',3,(#18711,#18712,#18713,#18714,#18715,
#18716,#18717,#18718,#18719,#18720,#18721),.UNSPECIFIED.,.F.,.F.,(4,1,1,
1,1,1,1,1,4),(-506.747366323204,-506.484635614976,-505.485652112777,-504.486668610578,
-503.487685108379,-502.48870160618,-501.489718103981,-500.490734601782,
-500.464181016024),.UNSPECIFIED.);
#231=B_SPLINE_CURVE_WITH_KNOTS('',3,(#18723,#18724,#18725,#18726,#18727,
#18728,#18729,#18730,#18731,#18732),.UNSPECIFIED.,.F.,.F.,(4,1,1,1,1,1,
1,4),(-500.464181016024,-499.491751099582,-498.492767597383,-497.493784095184,
-496.494800592985,-495.495817090786,-494.496833588587,-494.180995708845),
 .UNSPECIFIED.);
#232=B_SPLINE_CURVE_WITH_KNOTS('',3,(#18734,#18735,#18736,#18737,#18738,
#18739,#18740,#18741,#18742,#18743),.UNSPECIFIED.,.F.,.F.,(4,1,1,1,1,1,
1,4),(-494.180995708845,-493.497850086387,-492.498866584188,-491.499883081989,
-490.50089957979,-489.501916077591,-488.502932575392,-487.897810401665),
 .UNSPECIFIED.);
#233=B_SPLINE_CURVE_WITH_KNOTS('',3,(#18745,#18746,#18747,#18748,#18749,
#18750,#18751,#18752,#18753,#18754),.UNSPECIFIED.,.F.,.F.,(4,1,1,1,1,1,
1,4),(-487.897810401665,-487.503949073192,-486.504965570993,-485.505982068794,
-484.506998566595,-483.508015064396,-482.509031562196,-481.614625094486),
 .UNSPECIFIED.);
#234=B_SPLINE_CURVE_WITH_KNOTS('',3,(#18756,#18757,#18758,#18759,#18760,
#18761,#18762,#18763,#18764,#18765,#18766),.UNSPECIFIED.,.F.,.F.,(4,1,1,
1,1,1,1,1,4),(-481.614625094486,-481.510048059997,-480.511064557798,-479.512081055599,
-478.5130975534,-477.514114051201,-476.515130549001,-475.516147046802,-475.331439787306),
 .UNSPECIFIED.);
#235=B_SPLINE_CURVE_WITH_KNOTS('',3,(#18768,#18769,#18770,#18771,#18772,
#18773,#18774,#18775,#18776,#18777),.UNSPECIFIED.,.F.,.F.,(4,1,1,1,1,1,
1,4),(-475.331439787306,-474.517163544603,-473.518180042404,-472.519196540205,
-471.520213038006,-470.521229535807,-469.522246033607,-469.048254480127),
 .UNSPECIFIED.);
#236=B_SPLINE_CURVE_WITH_KNOTS('',3,(#18779,#18780,#18781,#18782,#18783,
#18784,#18785,#18786,#18787,#18788),.UNSPECIFIED.,.F.,.F.,(4,1,1,1,1,1,
1,4),(-469.048254480127,-468.523262531408,-467.524279029209,-466.52529552701,
-465.526312024811,-464.527328522612,-463.528345020412,-462.765069172947),
 .UNSPECIFIED.);
#237=B_SPLINE_CURVE_WITH_KNOTS('',3,(#18790,#18791,#18792,#18793,#18794,
#18795,#18796,#18797,#18798,#18799,#18800),.UNSPECIFIED.,.F.,.F.,(4,1,1,
1,1,1,1,1,4),(-462.765069172947,-462.529361518213,-461.530378016014,-460.531394513815,
-459.532411011616,-458.533427509417,-457.534444007217,-456.535460505018,
-456.481883865767),.UNSPECIFIED.);
#238=B_SPLINE_CURVE_WITH_KNOTS('',3,(#18802,#18803,#18804,#18805,#18806,
#18807,#18808,#18809,#18810,#18811),.UNSPECIFIED.,.F.,.F.,(4,1,1,1,1,1,
1,4),(-456.481883865767,-455.536477002819,-454.53749350062,-453.538509998421,
-452.539526496222,-451.540542994022,-450.541559491823,-450.198698558588),
 .UNSPECIFIED.);
#239=B_SPLINE_CURVE_WITH_KNOTS('',3,(#18813,#18814,#18815,#18816,#18817,
#18818,#18819,#18820,#18821,#18822),.UNSPECIFIED.,.F.,.F.,(4,1,1,1,1,1,
1,4),(-450.198698558588,-449.542575989624,-448.543592487425,-447.544608985226,
-446.545625483027,-445.546641980827,-444.547658478628,-443.915513251408),
 .UNSPECIFIED.);
#240=B_SPLINE_CURVE_WITH_KNOTS('',3,(#18824,#18825,#18826,#18827,#18828,
#18829,#18830,#18831,#18832,#18833),.UNSPECIFIED.,.F.,.F.,(4,1,1,1,1,1,
1,4),(-443.915513251408,-443.548674976429,-442.54969147423,-441.550707972031,
-440.551724469832,-439.552740967632,-438.553757465433,-437.632327944229),
 .UNSPECIFIED.);
#241=B_SPLINE_CURVE_WITH_KNOTS('',3,(#18835,#18836,#18837,#18838,#18839,
#18840,#18841,#18842,#18843,#18844,#18845,#18846),.UNSPECIFIED.,.F.,.F.,
(4,2,1,1,1,1,1,1,4),(-437.632327944229,-437.554773963234,-436.555790461035,
-435.556806958836,-434.557823456637,-433.558839954437,-432.559856452238,
-431.560872950039,-431.349142637049),.UNSPECIFIED.);
#242=B_SPLINE_CURVE_WITH_KNOTS('',3,(#18848,#18849,#18850,#18851,#18852,
#18853,#18854,#18855,#18856,#18857),.UNSPECIFIED.,.F.,.F.,(4,1,1,1,1,1,
1,4),(-431.349142637049,-430.56188944784,-429.562905945641,-428.563922443442,
-427.564938941242,-426.565955439043,-425.566971936844,-425.06595732987),
 .UNSPECIFIED.);
#243=B_SPLINE_CURVE_WITH_KNOTS('',3,(#18859,#18860,#18861,#18862,#18863,
#18864,#18865,#18866,#18867,#18868),.UNSPECIFIED.,.F.,.F.,(4,1,1,1,1,1,
1,4),(-425.06595732987,-424.567988434645,-423.569004932446,-422.570021430247,
-421.571037928047,-420.572054425848,-419.573070923649,-418.78277202269),
 .UNSPECIFIED.);
#244=B_SPLINE_CURVE_WITH_KNOTS('',3,(#18870,#18871,#18872,#18873,#18874,
#18875,#18876,#18877,#18878,#18879,#18880),.UNSPECIFIED.,.F.,.F.,(4,1,1,
1,1,1,1,1,4),(-418.78277202269,-418.57408742145,-417.575103919251,-416.576120417052,
-415.577136914853,-414.578153412653,-413.579169910454,-412.580186408255,
-412.499586715511),.UNSPECIFIED.);
#245=B_SPLINE_CURVE_WITH_KNOTS('',3,(#18882,#18883,#18884,#18885,#18886,
#18887,#18888,#18889,#18890,#18891),.UNSPECIFIED.,.F.,.F.,(4,1,1,1,1,1,
1,4),(-412.499586715511,-411.581202906056,-410.582219403857,-409.583235901657,
-408.584252399458,-407.585268897259,-406.58628539506,-406.216409056793),
 .UNSPECIFIED.);
#246=B_SPLINE_CURVE_WITH_KNOTS('',3,(#18893,#18894,#18895,#18896,#18897,
#18898,#18899,#18900,#18901,#18902,#18903,#18904,#18905,#18906,#18907,#18908,
#18909,#18910,#18911,#18912,#18913,#18914,#18915,#18916,#18917,#18918,#18919,
#18920,#18921,#18922,#18923,#18924,#18925,#18926,#18927,#18928,#18929,#18930,
#18931,#18932,#18933,#18934,#18935,#18936,#18937,#18938,#18939,#18940,#18941,
#18942,#18943,#18944,#18945,#18946,#18947,#18948,#18949,#18950,#18951,#18952,
#18953,#18954,#18955,#18956,#18957,#18958,#18959,#18960,#18961,#18962,#18963,
#18964,#18965,#18966,#18967,#18968,#18969,#18970,#18971,#18972,#18973,#18974,
#18975,#18976,#18977,#18978,#18979,#18980,#18981,#18982,#18983,#18984,#18985,
#18986,#18987,#18988,#18989,#18990,#18991,#18992,#18993,#18994,#18995,#18996,
#18997,#18998,#18999,#19000,#19001,#19002,#19003,#19004,#19005,#19006,#19007,
#19008,#19009,#19010,#19011,#19012,#19013,#19014,#19015,#19016,#19017,#19018,
#19019,#19020,#19021,#19022,#19023,#19024,#19025,#19026,#19027,#19028,#19029,
#19030,#19031,#19032,#19033,#19034,#19035,#19036,#19037,#19038,#19039,#19040,
#19041,#19042,#19043,#19044,#19045,#19046,#19047,#19048,#19049,#19050,#19051,
#19052,#19053,#19054,#19055,#19056,#19057,#19058,#19059,#19060,#19061,#19062,
#19063,#19064,#19065,#19066,#19067,#19068,#19069,#19070,#19071,#19072,#19073,
#19074,#19075,#19076,#19077,#19078,#19079,#19080,#19081,#19082,#19083,#19084,
#19085,#19086,#19087,#19088,#19089,#19090,#19091,#19092,#19093,#19094,#19095,
#19096,#19097,#19098,#19099,#19100,#19101,#19102,#19103,#19104,#19105,#19106,
#19107,#19108,#19109,#19110,#19111,#19112,#19113,#19114,#19115,#19116,#19117,
#19118,#19119,#19120,#19121,#19122,#19123,#19124,#19125,#19126,#19127,#19128,
#19129,#19130,#19131,#19132,#19133,#19134,#19135,#19136,#19137,#19138,#19139),
 .UNSPECIFIED.,.F.,.F.,(4,3,3,3,3,3,3,3,3,3,3,3,3,3,3,3,3,3,3,3,3,3,3,3,
3,3,3,3,3,3,3,3,3,3,3,3,3,3,3,3,3,3,3,3,3,3,3,3,3,3,3,3,3,3,3,3,3,3,3,3,
3,3,3,3,3,3,3,3,3,3,3,3,3,3,3,3,3,3,3,3,3,3,4),(-406.216401408331,-406.136209553946,
-406.05601375924,-405.975798966752,-405.895550110692,-405.81520058091,-405.73479800545,
-405.654263253984,-405.587301892861,-405.507336934074,-405.427466345969,
-405.347672608942,-405.267938263851,-405.188245898544,-405.108566680002,
-405.028890916213,-404.949202884345,-404.869486857234,-404.789683294303,
-404.709830569625,-404.629864159975,-404.588318390662,-404.508353431875,
-404.42848284377,-404.348689106743,-404.268954761652,-404.189262396345,
-404.109583177804,-404.029907414015,-403.950219382147,-403.870503355036,
-403.790699792105,-403.710847067427,-403.630880657777,-403.589334888463,
-403.509369929676,-403.429499341571,-403.349705604544,-403.269971259453,
-403.190278894146,-403.110599675605,-403.030923911816,-402.951235879948,
-402.871519852837,-402.791716289906,-402.711863565228,-402.631897155578,
-402.590351386263,-402.510386427476,-402.430515839371,-402.350722102344,
-402.270987757253,-402.191295391946,-402.111616173405,-402.031940409616,
-401.952252377748,-401.872536350636,-401.792732787706,-401.712880063028,
-401.632913653377,-401.591367884064,-401.511402925277,-401.431532337173,
-401.351738600146,-401.272004255056,-401.192311889749,-401.112632671208,
-401.032956907419,-400.953268875552,-400.87355284844,-400.79374928551,-400.713896560832,
-400.633930151182,-400.592384381865,-400.509988346776,-400.430067771627,
-400.350223801306,-400.270440715539,-400.190702835088,-400.11098969475,
-400.031290175392,-399.951577741183,-399.933216101151),.UNSPECIFIED.);
#247=B_SPLINE_CURVE_WITH_KNOTS('',3,(#19141,#19142,#19143,#19144,#19145,
#19146,#19147,#19148,#19149,#19150),.UNSPECIFIED.,.F.,.F.,(4,1,1,1,1,1,
1,4),(-399.933208553266,-399.593400879666,-398.594417377467,-397.595433875268,
-396.596450373068,-395.597466870869,-394.59848336867,-393.650030793972),
 .UNSPECIFIED.);
#248=B_SPLINE_CURVE_WITH_KNOTS('',3,(#19152,#19153,#19154,#19155,#19156,
#19157,#19158,#19159,#19160,#19161,#19162),.UNSPECIFIED.,.F.,.F.,(4,1,1,
1,1,1,1,1,4),(-393.650030793972,-393.599499866471,-392.600516364272,-391.601532862073,
-390.602549359873,-389.603565857674,-388.604582355475,-387.605598853276,
-387.366845486792),.UNSPECIFIED.);
#249=B_SPLINE_CURVE_WITH_KNOTS('',3,(#19164,#19165,#19166,#19167,#19168,
#19169,#19170,#19171,#19172,#19173),.UNSPECIFIED.,.F.,.F.,(4,1,1,1,1,1,
1,4),(-387.366845486792,-386.606615351077,-385.607631848878,-384.608648346678,
-383.609664844479,-382.61068134228,-381.611697840081,-381.083660179613),
 .UNSPECIFIED.);
#250=B_SPLINE_CURVE_WITH_KNOTS('',3,(#19175,#19176,#19177,#19178,#19179,
#19180,#19181,#19182,#19183,#19184),.UNSPECIFIED.,.F.,.F.,(4,1,1,1,1,1,
1,4),(-381.083660179613,-380.612714337882,-379.613730835683,-378.614747333483,
-377.615763831284,-376.616780329085,-375.617796826886,-374.800474872433),
 .UNSPECIFIED.);
#251=B_SPLINE_CURVE_WITH_KNOTS('',3,(#19186,#19187,#19188,#19189,#19190,
#19191,#19192,#19193,#19194,#19195,#19196),.UNSPECIFIED.,.F.,.F.,(4,1,1,
1,1,1,1,1,4),(-374.800474872433,-374.618813324687,-373.619829822488,-372.620846320288,
-371.621862818089,-370.62287931589,-369.623895813691,-368.624912311492,
-368.517289565254),.UNSPECIFIED.);
#252=B_SPLINE_CURVE_WITH_KNOTS('',3,(#19198,#19199,#19200,#19201,#19202,
#19203,#19204,#19205,#19206,#19207),.UNSPECIFIED.,.F.,.F.,(4,1,1,1,1,1,
1,4),(-368.517289565254,-367.625928809293,-366.626945307093,-365.627961804894,
-364.628978302695,-363.629994800496,-362.631011298297,-362.234104258074),
 .UNSPECIFIED.);
#253=B_SPLINE_CURVE_WITH_KNOTS('',3,(#19209,#19210,#19211,#19212,#19213,
#19214,#19215,#19216,#19217,#19218),.UNSPECIFIED.,.F.,.F.,(4,1,1,1,1,1,
1,4),(-362.234104258074,-361.632027796098,-360.633044293898,-359.634060791699,
-358.6350772895,-357.636093787301,-356.637110285102,-355.950918950894),
 .UNSPECIFIED.);
#254=B_SPLINE_CURVE_WITH_KNOTS('',3,(#19220,#19221,#19222,#19223,#19224,
#19225,#19226,#19227,#19228,#19229,#19230,#19231,#19232,#19233,#19234,#19235,
#19236,#19237,#19238,#19239,#19240,#19241,#19242,#19243,#19244,#19245,#19246,
#19247,#19248,#19249,#19250,#19251,#19252,#19253,#19254,#19255,#19256,#19257,
#19258,#19259,#19260,#19261,#19262,#19263,#19264,#19265,#19266,#19267,#19268,
#19269,#19270,#19271,#19272,#19273,#19274,#19275,#19276,#19277,#19278,#19279,
#19280,#19281,#19282,#19283,#19284,#19285,#19286,#19287,#19288,#19289,#19290,
#19291,#19292,#19293,#19294,#19295,#19296,#19297,#19298,#19299,#19300,#19301,
#19302,#19303,#19304,#19305,#19306,#19307,#19308,#19309,#19310,#19311,#19312,
#19313,#19314,#19315,#19316,#19317,#19318,#19319,#19320,#19321,#19322,#19323,
#19324,#19325,#19326,#19327,#19328,#19329,#19330,#19331,#19332,#19333,#19334,
#19335,#19336,#19337,#19338,#19339,#19340,#19341,#19342,#19343,#19344,#19345,
#19346,#19347,#19348,#19349,#19350,#19351,#19352,#19353,#19354,#19355,#19356,
#19357,#19358,#19359,#19360,#19361,#19362,#19363,#19364,#19365,#19366,#19367,
#19368,#19369,#19370,#19371,#19372,#19373,#19374,#19375,#19376,#19377,#19378,
#19379,#19380,#19381,#19382,#19383,#19384,#19385,#19386,#19387,#19388,#19389,
#19390,#19391,#19392,#19393,#19394,#19395,#19396,#19397,#19398,#19399,#19400,
#19401,#19402,#19403,#19404,#19405,#19406,#19407,#19408,#19409,#19410,#19411,
#19412,#19413,#19414,#19415,#19416,#19417,#19418,#19419,#19420,#19421,#19422,
#19423,#19424,#19425,#19426,#19427,#19428,#19429,#19430,#19431,#19432,#19433,
#19434,#19435,#19436,#19437,#19438,#19439,#19440,#19441,#19442,#19443,#19444,
#19445,#19446,#19447,#19448,#19449,#19450,#19451,#19452,#19453,#19454,#19455,
#19456,#19457,#19458,#19459,#19460,#19461,#19462,#19463,#19464,#19465,#19466),
 .UNSPECIFIED.,.F.,.F.,(4,3,3,3,3,3,3,3,3,3,3,3,3,3,3,3,3,3,3,3,3,3,3,3,
3,3,3,3,3,3,3,3,3,3,3,3,3,3,3,3,3,3,3,3,3,3,3,3,3,3,3,3,3,3,3,3,3,3,3,3,
3,3,3,3,3,3,3,3,3,3,3,3,3,3,3,3,3,3,3,3,3,3,4),(-355.95091874407,-355.856243657912,
-355.760892553551,-355.664791043618,-355.638126782903,-355.558161824115,
-355.478291236009,-355.398497498981,-355.318763153889,-355.239070788581,
-355.159391570039,-355.079715806248,-355.000027774379,-354.920311747267,
-354.840508184335,-354.760655459656,-354.680689050004,-354.639143280703,
-354.559178321916,-354.479307733811,-354.399513996785,-354.319779651694,
-354.240087286387,-354.160408067846,-354.080732304057,-354.001044272189,
-353.921328245078,-353.841524682147,-353.761671957469,-353.681705547819,
-353.640159778504,-353.560194819717,-353.480324231613,-353.400530494586,
-353.320796149495,-353.241103784188,-353.161424565647,-353.081748801858,
-353.002060769991,-352.92234474288,-352.842541179949,-352.762688455272,
-352.682722045621,-352.641176276305,-352.561211317518,-352.481340729413,
-352.401546992386,-352.321812647295,-352.242120281988,-352.162441063447,
-352.082765299657,-352.003077267789,-351.923361240678,-351.843557677747,
-351.763704953069,-351.683738543418,-351.642192774106,-351.562227815319,
-351.482357227214,-351.402563490187,-351.322829145096,-351.243136779789,
-351.163457561248,-351.083781797459,-351.004093765591,-350.92437773848,
-350.844574175549,-350.764721450872,-350.684755041221,-350.643209271907,
-350.563560272858,-350.484005465922,-350.404527033761,-350.325107222228,
-350.242935524914,-350.163568756537,-350.084203390465,-350.004823439038,
-349.925412908382,-349.845915202241,-349.766365489406,-349.686709081971,
-349.667733643715),.UNSPECIFIED.);
#255=B_SPLINE_CURVE_WITH_KNOTS('',3,(#19468,#19469,#19470,#19471,#19472,
#19473,#19474,#19475,#19476,#19477,#19478,#19479),.UNSPECIFIED.,.F.,.F.,
(4,2,1,1,1,1,1,1,4),(-349.667733643715,-349.644225769708,-348.645242267508,
-347.646258765309,-346.64727526311,-345.648291760911,-344.649308258712,
-343.650324756513,-343.384548336535),.UNSPECIFIED.);
#256=B_SPLINE_CURVE_WITH_KNOTS('',3,(#19481,#19482,#19483,#19484,#19485,
#19486,#19487,#19488,#19489,#19490),.UNSPECIFIED.,.F.,.F.,(4,1,1,1,1,1,
1,4),(-343.384548336535,-342.651341254313,-341.652357752114,-340.653374249915,
-339.654390747716,-338.655407245517,-337.656423743318,-337.101363029356),
 .UNSPECIFIED.);
#257=B_SPLINE_CURVE_WITH_KNOTS('',3,(#19492,#19493,#19494,#19495,#19496,
#19497,#19498,#19499,#19500,#19501),.UNSPECIFIED.,.F.,.F.,(4,1,1,1,1,1,
1,4),(-337.101363029356,-336.657440241118,-335.658456738919,-334.65947323672,
-333.660489734521,-332.661506232322,-331.662522730123,-330.818177722176),
 .UNSPECIFIED.);
#258=B_SPLINE_CURVE_WITH_KNOTS('',3,(#19503,#19504,#19505,#19506,#19507,
#19508,#19509,#19510,#19511,#19512,#19513),.UNSPECIFIED.,.F.,.F.,(4,1,1,
1,1,1,1,1,4),(-330.818177722176,-330.663539227923,-329.664555725724,-328.665572223525,
-327.666588721326,-326.667605219127,-325.668621716928,-324.669638214728,
-324.534992414997),.UNSPECIFIED.);
#259=B_SPLINE_CURVE_WITH_KNOTS('',3,(#19515,#19516,#19517,#19518,#19519,
#19520,#19521,#19522,#19523,#19524),.UNSPECIFIED.,.F.,.F.,(4,1,1,1,1,1,
1,4),(-324.534992414997,-323.670654712529,-322.67167121033,-321.672687708131,
-320.673704205932,-319.674720703733,-318.675737201533,-318.251807107817),
 .UNSPECIFIED.);
#260=B_SPLINE_CURVE_WITH_KNOTS('',3,(#19526,#19527,#19528,#19529,#19530,
#19531,#19532,#19533,#19534,#19535),.UNSPECIFIED.,.F.,.F.,(4,1,1,1,1,1,
1,4),(-318.251807107817,-317.676753699334,-316.677770197135,-315.678786694936,
-314.679803192737,-313.680819690538,-312.681836188338,-311.968621800637),
 .UNSPECIFIED.);
#261=B_SPLINE_CURVE_WITH_KNOTS('',3,(#19537,#19538,#19539,#19540,#19541,
#19542,#19543,#19544,#19545,#19546,#19547),.UNSPECIFIED.,.F.,.F.,(4,1,1,
1,1,1,1,1,4),(-311.968621800637,-311.682852686139,-310.68386918394,-309.684885681741,
-308.685902179542,-307.686918677343,-306.687935175144,-305.688951672944,
-305.685436493458),.UNSPECIFIED.);
#262=B_SPLINE_CURVE_WITH_KNOTS('',3,(#19549,#19550,#19551,#19552,#19553,
#19554,#19555,#19556,#19557,#19558,#19559,#19560,#19561,#19562,#19563,#19564,
#19565,#19566,#19567,#19568,#19569,#19570,#19571,#19572,#19573,#19574,#19575,
#19576,#19577,#19578,#19579,#19580,#19581,#19582,#19583,#19584,#19585,#19586,
#19587,#19588,#19589,#19590,#19591,#19592,#19593,#19594,#19595,#19596,#19597,
#19598,#19599,#19600,#19601,#19602,#19603,#19604,#19605,#19606,#19607,#19608,
#19609,#19610,#19611,#19612,#19613,#19614,#19615,#19616,#19617,#19618,#19619,
#19620,#19621,#19622,#19623,#19624,#19625,#19626,#19627,#19628,#19629,#19630,
#19631,#19632,#19633,#19634,#19635,#19636,#19637,#19638,#19639,#19640,#19641,
#19642,#19643,#19644,#19645,#19646,#19647,#19648,#19649,#19650,#19651,#19652,
#19653,#19654,#19655,#19656,#19657,#19658,#19659,#19660,#19661,#19662,#19663,
#19664,#19665,#19666,#19667,#19668,#19669,#19670,#19671,#19672,#19673,#19674,
#19675,#19676,#19677,#19678,#19679,#19680,#19681,#19682,#19683,#19684,#19685,
#19686,#19687,#19688,#19689,#19690,#19691,#19692,#19693,#19694,#19695,#19696,
#19697,#19698,#19699,#19700,#19701,#19702,#19703,#19704,#19705,#19706,#19707,
#19708,#19709,#19710,#19711,#19712,#19713,#19714,#19715,#19716,#19717,#19718,
#19719,#19720,#19721,#19722,#19723,#19724,#19725,#19726,#19727,#19728,#19729,
#19730,#19731,#19732,#19733,#19734,#19735,#19736,#19737,#19738,#19739,#19740,
#19741,#19742,#19743,#19744,#19745,#19746,#19747,#19748,#19749,#19750,#19751,
#19752,#19753,#19754,#19755,#19756,#19757,#19758,#19759,#19760,#19761,#19762,
#19763,#19764,#19765,#19766,#19767,#19768,#19769,#19770,#19771,#19772,#19773,
#19774,#19775,#19776,#19777,#19778,#19779,#19780,#19781,#19782,#19783,#19784,
#19785,#19786,#19787,#19788,#19789,#19790,#19791,#19792),.UNSPECIFIED.,
 .F.,.F.,(4,3,3,3,3,3,3,3,3,3,3,3,3,3,3,3,3,3,3,3,3,3,3,3,3,3,3,3,3,3,3,
3,3,3,3,3,3,3,3,3,3,3,3,3,3,3,3,3,3,3,3,3,3,3,3,3,3,3,3,3,3,3,3,3,3,3,3,
3,3,3,3,3,3,3,3,3,3,3,3,3,3,4),(-305.685436493458,-305.605522177692,-305.525702196027,
-305.445958978862,-305.3662750174,-305.28663285001,-305.207003567203,-305.127377478755,
-305.047738817149,-304.968071810301,-304.888317255143,-304.808513138856,
-304.728596179039,-304.689968170745,-304.610003211958,-304.530132623853,
-304.450338886826,-304.370604541735,-304.290912176428,-304.211232957887,
-304.131557194098,-304.05186916223,-303.972153135118,-303.892349572188,
-303.81249684751,-303.732530437859,-303.690984668546,-303.611019709759,
-303.531149121654,-303.451355384627,-303.371621039536,-303.29192867423,
-303.212249455688,-303.132573691899,-303.052885660032,-302.973169632921,
-302.89336606999,-302.813513345312,-302.733546935662,-302.692001166347,
-302.612036207559,-302.532165619455,-302.452371882428,-302.372637537336,
-302.29294517203,-302.213265953488,-302.133590189699,-302.053902157831,
-301.97418613072,-301.89438256779,-301.814529843111,-301.734563433461,-301.693017664148,
-301.613052705361,-301.533182117256,-301.45338838023,-301.373654035139,
-301.293961669832,-301.214282451291,-301.134606687502,-301.054918655634,
-300.975202628523,-300.895399065592,-300.815546340914,-300.735579931264,
-300.694034161949,-300.614069203162,-300.534198615057,-300.454404878031,
-300.37467053294,-300.294978167632,-300.215298949091,-300.135623185302,
-300.055935153434,-299.976219126323,-299.896415563392,-299.816562838714,
-299.736596429064,-299.695050659749,-299.596740053052,-299.499495703871,
-299.40225135469),.UNSPECIFIED.);
#263=B_SPLINE_CURVE_WITH_KNOTS('',3,(#19794,#19795,#19796,#19797,#19798,
#19799,#19800,#19801,#19802,#19803),.UNSPECIFIED.,.F.,.F.,(4,1,1,1,1,1,
1,4),(-299.402251186278,-298.69606715755,-297.697083655351,-296.698100153152,
-295.699116650953,-294.700133148754,-293.701149646554,-293.119065879099),
 .UNSPECIFIED.);
#264=B_SPLINE_CURVE_WITH_KNOTS('',3,(#19805,#19806,#19807,#19808,#19809,
#19810,#19811,#19812,#19813,#19814,#19815,#19816,#19817,#19818,#19819,#19820,
#19821,#19822,#19823,#19824,#19825,#19826,#19827,#19828,#19829,#19830,#19831,
#19832,#19833,#19834,#19835,#19836,#19837,#19838,#19839,#19840,#19841,#19842,
#19843,#19844,#19845,#19846,#19847,#19848,#19849,#19850,#19851,#19852,#19853,
#19854,#19855,#19856,#19857,#19858,#19859,#19860,#19861,#19862,#19863,#19864,
#19865,#19866,#19867,#19868,#19869,#19870,#19871,#19872,#19873,#19874,#19875,
#19876,#19877,#19878,#19879,#19880,#19881,#19882,#19883,#19884,#19885,#19886,
#19887,#19888,#19889,#19890,#19891,#19892,#19893,#19894,#19895,#19896,#19897,
#19898,#19899,#19900,#19901,#19902,#19903,#19904,#19905,#19906,#19907,#19908,
#19909,#19910,#19911,#19912,#19913,#19914,#19915,#19916,#19917,#19918,#19919,
#19920,#19921,#19922,#19923,#19924,#19925,#19926,#19927,#19928,#19929,#19930,
#19931,#19932,#19933,#19934,#19935,#19936,#19937,#19938,#19939,#19940,#19941,
#19942,#19943,#19944,#19945,#19946,#19947,#19948,#19949,#19950,#19951,#19952,
#19953,#19954,#19955,#19956,#19957,#19958,#19959,#19960,#19961,#19962,#19963,
#19964,#19965,#19966,#19967,#19968,#19969,#19970,#19971,#19972,#19973,#19974,
#19975,#19976,#19977,#19978,#19979,#19980,#19981,#19982,#19983,#19984,#19985,
#19986,#19987,#19988,#19989,#19990,#19991,#19992,#19993,#19994,#19995,#19996,
#19997,#19998,#19999,#20000,#20001,#20002,#20003,#20004,#20005,#20006,#20007,
#20008,#20009,#20010,#20011,#20012,#20013,#20014,#20015,#20016,#20017,#20018,
#20019,#20020,#20021,#20022,#20023,#20024,#20025,#20026,#20027,#20028,#20029,
#20030,#20031,#20032,#20033,#20034,#20035,#20036,#20037,#20038,#20039,#20040,
#20041,#20042,#20043,#20044,#20045,#20046,#20047,#20048),.UNSPECIFIED.,
 .F.,.F.,(4,3,3,3,3,3,3,3,3,3,3,3,3,3,3,3,3,3,3,3,3,3,3,3,3,3,3,3,3,3,3,
3,3,3,3,3,3,3,3,3,3,3,3,3,3,3,3,3,3,3,3,3,3,3,3,3,3,3,3,3,3,3,3,3,3,3,3,
3,3,3,3,3,3,3,3,3,3,3,3,3,3,4),(-293.119065679974,-293.032078649479,-292.944695041724,
-292.8571122961,-292.769227567858,-292.702166144355,-292.622201185568,-292.542330597464,
-292.462536860437,-292.382802515346,-292.30311015004,-292.223430931499,
-292.14375516771,-292.064067135843,-291.984351108732,-291.904547545802,
-291.824694821124,-291.744728411474,-291.703182642156,-291.623217683369,
-291.543347095264,-291.463553358237,-291.383819013146,-291.304126647839,
-291.224447429298,-291.144771665509,-291.065083633641,-290.98536760653,
-290.905564043599,-290.825711318921,-290.745744909271,-290.704199139957,
-290.62423418117,-290.544363593065,-290.464569856038,-290.384835510947,
-290.30514314564,-290.225463927099,-290.14578816331,-290.066100131442,-289.986384104331,
-289.9065805414,-289.826727816722,-289.746761407072,-289.705215637758,-289.625250678971,
-289.545380090866,-289.465586353839,-289.385852008748,-289.306159643442,
-289.2264804249,-289.146804661111,-289.067116629244,-288.987400602132,-288.907597039202,
-288.827744314524,-288.747777904873,-288.706232135559,-288.626267176772,
-288.546396588667,-288.46660285164,-288.386868506549,-288.307176141241,
-288.2274969227,-288.147821158911,-288.068133127043,-287.988417099931,-287.908613537,
-287.828760812322,-287.748794402672,-287.707248633359,-287.628408648173,
-287.549662294741,-287.470991132852,-287.391602312736,-287.313022569158,
-287.234458300051,-287.155892977823,-287.075889876347,-286.997239478252,
-286.916560025085,-286.835880571919),.UNSPECIFIED.);
#265=B_SPLINE_CURVE_WITH_KNOTS('',3,(#20050,#20051,#20052,#20053,#20054,
#20055,#20056,#20057,#20058,#20059,#20060),.UNSPECIFIED.,.F.,.F.,(4,1,1,
1,1,1,1,1,4),(-286.835880571919,-286.70826513116,-285.709281628961,-284.710298126762,
-283.711314624563,-282.712331122364,-281.713347620164,-280.714364117965,
-280.55269526474),.UNSPECIFIED.);
#266=B_SPLINE_CURVE_WITH_KNOTS('',3,(#20062,#20063,#20064,#20065,#20066,
#20067,#20068,#20069,#20070,#20071),.UNSPECIFIED.,.F.,.F.,(4,1,1,1,1,1,
1,4),(-280.55269526474,-279.715380615766,-278.716397113567,-277.717413611368,
-276.718430109169,-275.719446606969,-274.72046310477,-274.26950995756),
 .UNSPECIFIED.);
#267=B_SPLINE_CURVE_WITH_KNOTS('',3,(#20073,#20074,#20075,#20076,#20077,
#20078,#20079,#20080,#20081,#20082),.UNSPECIFIED.,.F.,.F.,(4,1,1,1,1,1,
1,4),(-274.26950995756,-273.721479602571,-272.722496100372,-271.723512598173,
-270.724529095974,-269.725545593774,-268.726562091575,-267.986324650381),
 .UNSPECIFIED.);
#268=B_SPLINE_CURVE_WITH_KNOTS('',3,(#20084,#20085,#20086,#20087,#20088,
#20089,#20090,#20091,#20092,#20093,#20094,#20095,#20096,#20097,#20098,#20099,
#20100,#20101,#20102,#20103,#20104,#20105,#20106,#20107,#20108,#20109,#20110,
#20111,#20112,#20113,#20114,#20115,#20116,#20117,#20118,#20119,#20120,#20121,
#20122,#20123,#20124,#20125,#20126,#20127,#20128,#20129,#20130,#20131,#20132,
#20133,#20134,#20135,#20136,#20137,#20138,#20139,#20140,#20141,#20142,#20143,
#20144,#20145,#20146,#20147,#20148,#20149,#20150,#20151,#20152,#20153,#20154,
#20155,#20156,#20157,#20158,#20159,#20160,#20161,#20162,#20163,#20164,#20165,
#20166,#20167,#20168,#20169,#20170,#20171,#20172,#20173,#20174,#20175,#20176,
#20177,#20178,#20179,#20180,#20181,#20182,#20183,#20184,#20185,#20186,#20187,
#20188,#20189,#20190,#20191,#20192,#20193,#20194,#20195,#20196,#20197,#20198,
#20199,#20200,#20201,#20202,#20203,#20204,#20205,#20206,#20207,#20208,#20209,
#20210,#20211,#20212,#20213,#20214,#20215,#20216,#20217,#20218,#20219,#20220,
#20221,#20222,#20223,#20224,#20225,#20226,#20227,#20228,#20229,#20230,#20231,
#20232,#20233,#20234,#20235,#20236,#20237,#20238,#20239,#20240,#20241,#20242,
#20243,#20244,#20245,#20246,#20247,#20248,#20249,#20250,#20251,#20252,#20253,
#20254,#20255,#20256,#20257,#20258,#20259,#20260,#20261,#20262,#20263,#20264,
#20265,#20266,#20267,#20268,#20269,#20270,#20271,#20272,#20273,#20274,#20275,
#20276,#20277,#20278,#20279,#20280,#20281,#20282,#20283,#20284,#20285,#20286,
#20287,#20288,#20289,#20290,#20291,#20292,#20293,#20294,#20295,#20296,#20297,
#20298,#20299,#20300,#20301,#20302,#20303,#20304,#20305,#20306,#20307,#20308,
#20309,#20310,#20311,#20312,#20313,#20314,#20315,#20316,#20317,#20318,#20319,
#20320,#20321,#20322,#20323,#20324,#20325,#20326,#20327,#20328,#20329,#20330),
 .UNSPECIFIED.,.F.,.F.,(4,3,3,3,3,3,3,3,3,3,3,3,3,3,3,3,3,3,3,3,3,3,3,3,
3,3,3,3,3,3,3,3,3,3,3,3,3,3,3,3,3,3,3,3,3,3,3,3,3,3,3,3,3,3,3,3,3,3,3,3,
3,3,3,3,3,3,3,3,3,3,3,3,3,3,3,3,3,3,3,3,3,3,4),(-267.986324569519,-267.885288901158,
-267.782255160134,-267.727578589376,-267.647613630589,-267.567743042484,
-267.487949305458,-267.408214960367,-267.328522595061,-267.24884337652,
-267.169167612731,-267.089479580863,-267.009763553751,-266.929959990821,
-266.850107266144,-266.770140856493,-266.728595087177,-266.64863012839,
-266.568759540285,-266.488965803258,-266.409231458167,-266.32953909286,
-266.249859874319,-266.17018411053,-266.090496078662,-266.01078005155,-265.93097648862,
-265.851123763942,-265.771157354291,-265.729611584978,-265.649646626191,
-265.569776038086,-265.48998230106,-265.410247955969,-265.330555590662,
-265.250876372121,-265.171200608332,-265.091512576464,-265.011796549353,
-264.931992986423,-264.852140261745,-264.772173852095,-264.730628082779,
-264.650663123991,-264.570792535887,-264.490998798859,-264.411264453768,
-264.331572088461,-264.25189286992,-264.17221710613,-264.092529074262,-264.01281304715,
-263.933009484219,-263.853156759541,-263.773190349891,-263.731644580579,
-263.651679621792,-263.571809033687,-263.49201529666,-263.412280951569,
-263.332588586262,-263.252909367721,-263.173233603932,-263.093545572064,
-263.013829544952,-262.934025982022,-262.854173257344,-262.774206847693,
-262.73266107838,-262.652696119593,-262.572825531488,-262.493031794462,
-262.413297449371,-262.333605084064,-262.253925865523,-262.174250101734,
-262.094562069866,-262.014846042755,-261.935042479824,-261.855189755146,
-261.775223345496,-261.733677576181,-261.703139343201),.UNSPECIFIED.);
#269=B_SPLINE_CURVE_WITH_KNOTS('',3,(#20332,#20333,#20334,#20335,#20336,
#20337,#20338,#20339,#20340,#20341),.UNSPECIFIED.,.F.,.F.,(4,1,1,1,1,1,
1,4),(-261.703135137337,-260.734694073982,-259.735710571783,-258.736727069584,
-257.737743567384,-256.738760065185,-255.739776562986,-255.419954036021),
 .UNSPECIFIED.);
#270=B_SPLINE_CURVE_WITH_KNOTS('',3,(#20343,#20344,#20345,#20346,#20347,
#20348,#20349,#20350,#20351,#20352),.UNSPECIFIED.,.F.,.F.,(4,1,1,1,1,1,
1,4),(-255.419954036021,-254.740793060787,-253.741809558588,-252.742826056389,
-251.743842554189,-250.74485905199,-249.745875549791,-249.136768728842),
 .UNSPECIFIED.);
#271=B_SPLINE_CURVE_WITH_KNOTS('',3,(#20354,#20355,#20356,#20357,#20358,
#20359,#20360,#20361,#20362,#20363),.UNSPECIFIED.,.F.,.F.,(4,1,1,1,1,1,
1,4),(-249.136768728842,-248.746892047592,-247.747908545393,-246.748925043194,
-245.749941540995,-244.750958038795,-243.751974536596,-242.853592464959),
 .UNSPECIFIED.);
#272=B_SPLINE_CURVE_WITH_KNOTS('',3,(#20365,#20366,#20367,#20368,#20369,
#20370,#20371,#20372,#20373,#20374,#20375,#20376,#20377,#20378,#20379,#20380,
#20381,#20382,#20383,#20384,#20385,#20386,#20387,#20388,#20389,#20390,#20391,
#20392,#20393,#20394,#20395,#20396,#20397,#20398,#20399,#20400,#20401,#20402,
#20403,#20404,#20405,#20406,#20407,#20408,#20409,#20410,#20411,#20412,#20413,
#20414,#20415,#20416,#20417,#20418,#20419,#20420,#20421,#20422,#20423,#20424,
#20425,#20426,#20427,#20428,#20429,#20430,#20431,#20432,#20433,#20434,#20435,
#20436,#20437,#20438,#20439,#20440,#20441,#20442,#20443,#20444,#20445,#20446,
#20447,#20448,#20449,#20450,#20451,#20452,#20453,#20454,#20455,#20456,#20457,
#20458,#20459,#20460,#20461,#20462,#20463,#20464,#20465,#20466,#20467,#20468,
#20469,#20470,#20471,#20472,#20473,#20474,#20475,#20476,#20477,#20478,#20479,
#20480,#20481,#20482,#20483,#20484,#20485,#20486,#20487,#20488,#20489,#20490,
#20491,#20492,#20493,#20494,#20495,#20496,#20497,#20498,#20499,#20500,#20501,
#20502,#20503,#20504,#20505,#20506,#20507,#20508,#20509,#20510,#20511,#20512,
#20513,#20514,#20515,#20516,#20517,#20518,#20519,#20520,#20521,#20522,#20523,
#20524,#20525,#20526,#20527,#20528,#20529,#20530,#20531,#20532,#20533,#20534,
#20535,#20536,#20537,#20538,#20539,#20540,#20541,#20542,#20543,#20544,#20545,
#20546,#20547,#20548,#20549,#20550,#20551,#20552,#20553,#20554,#20555,#20556,
#20557,#20558,#20559,#20560,#20561,#20562,#20563,#20564,#20565,#20566,#20567,
#20568,#20569,#20570,#20571,#20572,#20573,#20574,#20575,#20576,#20577,#20578,
#20579,#20580,#20581,#20582,#20583,#20584,#20585,#20586,#20587,#20588,#20589,
#20590,#20591,#20592,#20593,#20594,#20595,#20596,#20597,#20598,#20599,#20600,
#20601,#20602,#20603,#20604,#20605,#20606,#20607,#20608),.UNSPECIFIED.,
 .F.,.F.,(4,3,3,3,3,3,3,3,3,3,3,3,3,3,3,3,3,3,3,3,3,3,3,3,3,3,3,3,3,3,3,
3,3,3,3,3,3,3,3,3,3,3,3,3,3,3,3,3,3,3,3,3,3,3,3,3,3,3,3,3,3,3,3,3,3,3,3,
3,3,3,3,3,3,3,3,3,3,3,3,3,3,4),(-242.853583421662,-242.752991034397,-242.67302607561,
-242.593155487505,-242.513361750478,-242.433627405387,-242.35393504008,
-242.274255821539,-242.19458005775,-242.114892025882,-242.03517599877,-241.95537243584,
-241.875519711162,-241.795553301511,-241.754007532198,-241.674042573411,
-241.594171985306,-241.51437824828,-241.434643903188,-241.354951537882,
-241.275272319341,-241.195596555551,-241.115908523684,-241.036192496572,
-240.956388933642,-240.876536208964,-240.796569799314,-240.755024029999,
-240.675059071211,-240.595188483107,-240.51539474608,-240.435660400988,
-240.355968035681,-240.27628881714,-240.19661305335,-240.116925021482,-240.037208994371,
-239.95740543144,-239.877552706762,-239.797586297111,-239.756040527799,
-239.676075569012,-239.596204980907,-239.51641124388,-239.436676898789,
-239.356984533482,-239.277305314941,-239.197629551152,-239.117941519284,
-239.038225492173,-238.958421929242,-238.878569204564,-238.798602794914,
-238.7570570256,-238.677092066813,-238.597221478708,-238.517427741682,-238.437693396591,
-238.358001031284,-238.278321812743,-238.198646048954,-238.118958017086,
-238.039241989975,-237.959438427045,-237.879585702367,-237.799619292716,
-237.758073523401,-237.678108564614,-237.598237976509,-237.518444239482,
-237.438709894391,-237.359017529084,-237.279338310543,-237.199662546753,
-237.119974514885,-237.040258487774,-236.960454924843,-236.880602200165,
-236.800635790515,-236.759090021202,-236.640918949153,-236.570398114483),
 .UNSPECIFIED.);
#273=B_SPLINE_CURVE_WITH_KNOTS('',3,(#20610,#20611,#20612,#20613,#20614,
#20615,#20616,#20617,#20618,#20619),.UNSPECIFIED.,.F.,.F.,(4,1,1,1,1,1,
1,4),(-236.570393800933,-235.760106519003,-234.761123016804,-233.762139514604,
-232.763156012405,-231.764172510206,-230.765189008007,-230.287212807303),
 .UNSPECIFIED.);
#274=B_SPLINE_CURVE_WITH_KNOTS('',3,(#20621,#20622,#20623,#20624,#20625,
#20626,#20627,#20628,#20629,#20630),.UNSPECIFIED.,.F.,.F.,(4,1,1,1,1,1,
1,4),(-230.287212807303,-229.766205505808,-228.767222003609,-227.76823850141,
-226.76925499921,-225.770271497011,-224.771287994812,-224.004027500124),
 .UNSPECIFIED.);
#275=B_SPLINE_CURVE_WITH_KNOTS('',3,(#20632,#20633,#20634,#20635,#20636,
#20637,#20638,#20639,#20640,#20641,#20642),.UNSPECIFIED.,.F.,.F.,(4,1,1,
1,1,1,1,1,4),(-224.004027500124,-223.772304492613,-222.773320990414,-221.774337488215,
-220.775353986015,-219.776370483816,-218.777386981617,-217.778403479418,
-217.720842192944),.UNSPECIFIED.);
#276=B_SPLINE_CURVE_WITH_KNOTS('',3,(#20644,#20645,#20646,#20647,#20648,
#20649,#20650,#20651,#20652,#20653,#20654,#20655,#20656,#20657,#20658,#20659,
#20660,#20661,#20662,#20663,#20664,#20665,#20666,#20667,#20668,#20669,#20670,
#20671,#20672,#20673,#20674,#20675,#20676,#20677,#20678,#20679,#20680,#20681,
#20682,#20683,#20684,#20685,#20686,#20687,#20688,#20689,#20690,#20691,#20692,
#20693,#20694,#20695,#20696,#20697,#20698,#20699,#20700,#20701,#20702,#20703,
#20704,#20705,#20706,#20707,#20708,#20709,#20710,#20711,#20712,#20713,#20714,
#20715,#20716,#20717,#20718,#20719,#20720,#20721,#20722,#20723,#20724,#20725,
#20726,#20727,#20728,#20729,#20730,#20731,#20732,#20733,#20734,#20735,#20736,
#20737,#20738,#20739,#20740,#20741,#20742,#20743,#20744,#20745,#20746,#20747,
#20748,#20749,#20750,#20751,#20752,#20753,#20754,#20755,#20756,#20757,#20758,
#20759,#20760,#20761,#20762,#20763,#20764,#20765,#20766,#20767,#20768,#20769,
#20770,#20771,#20772,#20773,#20774,#20775,#20776,#20777,#20778,#20779,#20780,
#20781,#20782,#20783,#20784,#20785,#20786,#20787,#20788,#20789,#20790,#20791,
#20792,#20793,#20794,#20795,#20796,#20797,#20798,#20799,#20800,#20801,#20802,
#20803,#20804,#20805,#20806,#20807,#20808,#20809,#20810,#20811,#20812,#20813,
#20814,#20815,#20816,#20817,#20818,#20819,#20820,#20821,#20822,#20823,#20824,
#20825,#20826,#20827,#20828,#20829,#20830,#20831,#20832,#20833,#20834,#20835,
#20836,#20837,#20838,#20839,#20840,#20841,#20842,#20843,#20844,#20845,#20846,
#20847,#20848,#20849,#20850,#20851,#20852,#20853,#20854,#20855,#20856,#20857,
#20858,#20859,#20860,#20861,#20862,#20863,#20864,#20865,#20866,#20867,#20868,
#20869,#20870,#20871,#20872,#20873,#20874,#20875,#20876,#20877,#20878,#20879,
#20880,#20881,#20882,#20883,#20884,#20885,#20886,#20887),.UNSPECIFIED.,
 .F.,.F.,(4,3,3,3,3,3,3,3,3,3,3,3,3,3,3,3,3,3,3,3,3,3,3,3,3,3,3,3,3,3,3,
3,3,3,3,3,3,3,3,3,3,3,3,3,3,3,3,3,3,3,3,3,3,3,3,3,3,3,3,3,3,3,3,3,3,3,3,
3,3,3,3,3,3,3,3,3,3,3,3,3,3,4),(-217.720842192944,-217.641578783107,-217.562406076567,
-217.483305964034,-217.404260401362,-217.325243816638,-217.246240961083,
-217.167235577504,-217.08821140943,-217.00910557981,-216.929957857125,-216.850689582362,
-216.779419977219,-216.699455018432,-216.619584430327,-216.539790693301,
-216.46005634821,-216.380363982903,-216.300684764362,-216.221009000573,
-216.141320968705,-216.061604941594,-215.981801378664,-215.901948653986,
-215.821982244336,-215.78043647502,-215.700471516232,-215.620600928128,
-215.5408071911,-215.461072846009,-215.381380480702,-215.301701262161,-215.222025498371,
-215.142337466503,-215.062621439391,-214.98281787646,-214.902965151782,
-214.822998742131,-214.78145297282,-214.701488014033,-214.621617425928,
-214.541823688901,-214.46208934381,-214.382396978503,-214.302717759962,
-214.223041996173,-214.143353964305,-214.063637937194,-213.983834374263,
-213.903981649585,-213.824015239935,-213.782469470621,-213.702504511834,
-213.622633923729,-213.542840186703,-213.463105841612,-213.383413476305,
-213.303734257764,-213.224058493975,-213.144370462107,-213.064654434996,
-212.984850872066,-212.904998147388,-212.825031737738,-212.783485968422,
-212.703521009635,-212.62365042153,-212.543856684503,-212.464122339413,
-212.384429974106,-212.304750755564,-212.225074991775,-212.145386959907,
-212.065670932796,-211.985867369865,-211.906014645187,-211.826048235537,
-211.784502466223,-211.691784045667,-211.599421182378,-211.507751789104,
-211.4376570074),.UNSPECIFIED.);
#277=B_SPLINE_CURVE_WITH_KNOTS('',3,(#20889,#20890,#20891,#20892,#20893,
#20894,#20895,#20896,#20897,#20898),.UNSPECIFIED.,.F.,.F.,(4,1,1,1,1,1,
1,4),(-211.437656885764,-210.785518964024,-209.786535461825,-208.787551959625,
-207.788568457426,-206.789584955227,-205.790601453028,-205.154471578585),
 .UNSPECIFIED.);
#278=B_SPLINE_CURVE_WITH_KNOTS('',3,(#20900,#20901,#20902,#20903,#20904,
#20905,#20906,#20907,#20908,#20909),.UNSPECIFIED.,.F.,.F.,(4,1,1,1,1,1,
1,4),(-205.154471578585,-204.791617950829,-203.79263444863,-202.79365094643,
-201.794667444231,-200.795683942032,-199.796700439833,-198.871286271405),
 .UNSPECIFIED.);
#279=B_SPLINE_CURVE_WITH_KNOTS('',3,(#20911,#20912,#20913,#20914,#20915,
#20916,#20917,#20918,#20919,#20920,#20921,#20922),.UNSPECIFIED.,.F.,.F.,
(4,2,1,1,1,1,1,1,4),(-198.871286271405,-198.797716937634,-197.798733435435,
-196.799749933235,-195.800766431036,-194.801782928837,-193.802799426638,
-192.803815924439,-192.588100964226),.UNSPECIFIED.);
#280=B_SPLINE_CURVE_WITH_KNOTS('',3,(#20924,#20925,#20926,#20927,#20928,
#20929,#20930,#20931,#20932,#20933,#20934,#20935,#20936,#20937,#20938,#20939,
#20940,#20941,#20942,#20943,#20944,#20945,#20946,#20947,#20948,#20949,#20950,
#20951,#20952,#20953,#20954,#20955,#20956,#20957,#20958,#20959,#20960,#20961,
#20962,#20963,#20964,#20965,#20966,#20967,#20968,#20969,#20970,#20971,#20972,
#20973,#20974,#20975,#20976,#20977,#20978,#20979,#20980,#20981,#20982,#20983,
#20984,#20985,#20986,#20987,#20988,#20989,#20990,#20991,#20992,#20993,#20994,
#20995,#20996,#20997,#20998,#20999,#21000,#21001,#21002,#21003,#21004,#21005,
#21006,#21007,#21008,#21009,#21010,#21011,#21012,#21013,#21014,#21015,#21016,
#21017,#21018,#21019,#21020,#21021,#21022,#21023,#21024,#21025,#21026,#21027,
#21028,#21029,#21030,#21031,#21032,#21033,#21034,#21035,#21036,#21037,#21038,
#21039,#21040,#21041,#21042,#21043,#21044,#21045,#21046,#21047,#21048,#21049,
#21050,#21051,#21052,#21053,#21054,#21055,#21056,#21057,#21058,#21059,#21060,
#21061,#21062,#21063,#21064,#21065,#21066,#21067,#21068,#21069,#21070,#21071,
#21072,#21073,#21074,#21075,#21076,#21077,#21078,#21079,#21080,#21081,#21082,
#21083,#21084,#21085,#21086,#21087,#21088,#21089,#21090,#21091,#21092,#21093,
#21094,#21095,#21096,#21097,#21098,#21099,#21100,#21101,#21102,#21103,#21104,
#21105,#21106,#21107,#21108,#21109,#21110,#21111,#21112,#21113,#21114,#21115,
#21116,#21117,#21118,#21119,#21120,#21121,#21122,#21123,#21124,#21125,#21126,
#21127,#21128,#21129,#21130,#21131,#21132,#21133,#21134,#21135,#21136,#21137,
#21138,#21139,#21140,#21141,#21142,#21143,#21144,#21145,#21146,#21147,#21148,
#21149,#21150,#21151,#21152,#21153,#21154,#21155,#21156,#21157,#21158,#21159,
#21160,#21161,#21162,#21163,#21164,#21165,#21166,#21167),.UNSPECIFIED.,
 .F.,.F.,(4,3,3,3,3,3,3,3,3,3,3,3,3,3,3,3,3,3,3,3,3,3,3,3,3,3,3,3,3,3,3,
3,3,3,3,3,3,3,3,3,3,3,3,3,3,3,3,3,3,3,3,3,3,3,3,3,3,3,3,3,3,3,3,3,3,3,3,
3,3,3,3,3,3,3,3,3,3,3,3,3,3,4),(-192.588100964226,-192.509400610385,-192.430759171616,
-192.35215227097,-192.273562537089,-192.194973453373,-192.116368505404,
-192.037684617319,-191.958960970888,-191.880116824502,-191.80483242224,
-191.724867463453,-191.644996875348,-191.565203138321,-191.485468793229,
-191.405776427922,-191.326097209381,-191.246421445591,-191.166733413723,
-191.087017386612,-191.007213823681,-190.927361099003,-190.847394689352,
-190.80584892004,-190.725883961253,-190.646013373148,-190.566219636121,
-190.48648529103,-190.406792925724,-190.327113707182,-190.247437943393,
-190.167749911525,-190.088033884414,-190.008230321483,-189.928377596805,
-189.848411187154,-189.806865417841,-189.726900459054,-189.647029870949,
-189.567236133923,-189.487501788832,-189.407809423524,-189.328130204983,
-189.248454441194,-189.168766409327,-189.089050382215,-189.009246819285,
-188.929394094607,-188.849427684957,-188.807881915642,-188.727916956855,
-188.64804636875,-188.568252631723,-188.488518286632,-188.408825921325,
-188.329146702783,-188.249470938994,-188.169782907126,-188.090066880015,
-188.010263317085,-187.930410592407,-187.850444182757,-187.808898413443,
-187.728933454656,-187.649062866551,-187.569269129524,-187.489534784433,
-187.409842419126,-187.330163200585,-187.250487436796,-187.170799404927,
-187.091083377816,-187.011279814885,-186.931427090208,-186.851460680557,
-186.809914911244,-186.726038212122,-186.642296982965,-186.557951651485,
-186.474498477817,-186.389707067432,-186.304915657046),.UNSPECIFIED.);
#281=B_SPLINE_CURVE_WITH_KNOTS('',3,(#21169,#21170,#21171,#21172,#21173,
#21174,#21175,#21176,#21177,#21178,#21179,#21180,#21181,#21182,#21183,#21184,
#21185,#21186,#21187,#21188,#21189,#21190,#21191,#21192,#21193,#21194,#21195,
#21196,#21197,#21198,#21199,#21200,#21201,#21202,#21203,#21204,#21205,#21206,
#21207,#21208,#21209,#21210,#21211,#21212,#21213,#21214,#21215,#21216,#21217,
#21218,#21219,#21220,#21221,#21222,#21223,#21224,#21225,#21226,#21227,#21228,
#21229,#21230,#21231,#21232,#21233,#21234,#21235,#21236,#21237,#21238,#21239,
#21240,#21241,#21242,#21243,#21244,#21245,#21246,#21247,#21248,#21249,#21250,
#21251,#21252,#21253,#21254,#21255,#21256,#21257,#21258,#21259,#21260,#21261,
#21262,#21263,#21264,#21265,#21266,#21267,#21268,#21269,#21270,#21271,#21272,
#21273,#21274,#21275,#21276,#21277,#21278,#21279,#21280,#21281,#21282,#21283,
#21284,#21285,#21286,#21287,#21288,#21289,#21290,#21291,#21292,#21293,#21294,
#21295,#21296,#21297,#21298,#21299,#21300,#21301,#21302,#21303,#21304,#21305,
#21306,#21307,#21308,#21309,#21310,#21311,#21312,#21313,#21314,#21315,#21316,
#21317,#21318,#21319,#21320,#21321,#21322,#21323,#21324,#21325,#21326,#21327,
#21328,#21329,#21330,#21331,#21332,#21333,#21334,#21335,#21336,#21337,#21338,
#21339,#21340,#21341,#21342,#21343,#21344,#21345,#21346,#21347,#21348,#21349,
#21350,#21351,#21352,#21353,#21354,#21355,#21356,#21357,#21358,#21359,#21360,
#21361,#21362,#21363,#21364,#21365,#21366,#21367,#21368,#21369,#21370,#21371,
#21372,#21373,#21374,#21375,#21376,#21377,#21378,#21379,#21380,#21381,#21382,
#21383,#21384,#21385,#21386,#21387,#21388,#21389,#21390,#21391,#21392,#21393,
#21394,#21395,#21396,#21397,#21398,#21399,#21400,#21401,#21402,#21403,#21404,
#21405,#21406,#21407,#21408,#21409,#21410,#21411,#21412),.UNSPECIFIED.,
 .F.,.F.,(4,3,3,3,3,3,3,3,3,3,3,3,3,3,3,3,3,3,3,3,3,3,3,3,3,3,3,3,3,3,3,
3,3,3,3,3,3,3,3,3,3,3,3,3,3,3,3,3,3,3,3,3,3,3,3,3,3,3,3,3,3,3,3,3,3,3,3,
3,3,3,3,3,3,3,3,3,3,3,3,3,3,4),(-186.304915656926,-186.221262094494,-186.137497127184,
-186.053532146919,-185.969464210991,-185.885200182465,-185.810931409045,
-185.730966450257,-185.651095862153,-185.571302125125,-185.491567780034,
-185.411875414727,-185.332196196186,-185.252520432396,-185.172832400528,
-185.093116373417,-185.013312810486,-184.933460085808,-184.853493676157,
-184.811947906845,-184.731982948058,-184.652112359953,-184.572318622926,
-184.492584277835,-184.412891912528,-184.333212693987,-184.253536930198,
-184.17384889833,-184.094132871219,-184.014329308288,-183.93447658361,-183.85451017396,
-183.812964404646,-183.732999445859,-183.653128857754,-183.573335120728,
-183.493600775637,-183.41390841033,-183.334229191789,-183.254553428,-183.174865396132,
-183.095149369021,-183.015345806091,-182.935493081413,-182.855526671762,
-182.813980902447,-182.73401594366,-182.654145355555,-182.574351618528,
-182.494617273437,-182.41492490813,-182.335245689589,-182.2555699258,-182.175881893932,
-182.09616586682,-182.01636230389,-181.936509579212,-181.856543169561,-181.814997400248,
-181.735032441461,-181.655161853356,-181.575368116329,-181.495633771238,
-181.415941405931,-181.33626218739,-181.256586423601,-181.176898391733,
-181.097182364622,-181.017378801691,-180.937526077013,-180.857559667363,
-180.816013898049,-180.737185977964,-180.658452667959,-180.578862378197,
-180.500268342106,-180.421707645983,-180.343163738494,-180.262805391337,
-180.184219816278,-180.102975083072,-180.021730349867),.UNSPECIFIED.);
#282=B_SPLINE_CURVE_WITH_KNOTS('',3,(#21414,#21415,#21416,#21417,#21418,
#21419,#21420,#21421,#21422,#21423,#21424),.UNSPECIFIED.,.F.,.F.,(4,1,1,
1,1,1,1,1,4),(-180.021730349867,-179.81703039585,-178.81804689365,-177.819063391451,
-176.820079889252,-175.821096387053,-174.822112884854,-173.823129382655,
-173.738545042687),.UNSPECIFIED.);
#283=B_SPLINE_CURVE_WITH_KNOTS('',3,(#21426,#21427,#21428,#21429,#21430,
#21431,#21432,#21433,#21434,#21435),.UNSPECIFIED.,.F.,.F.,(4,1,1,1,1,1,
1,4),(-173.738545042687,-172.824145880455,-171.825162378256,-170.826178876057,
-169.827195373858,-168.828211871659,-167.82922836946,-167.455367342988),
 .UNSPECIFIED.);
#284=B_SPLINE_CURVE_WITH_KNOTS('',3,(#21437,#21438,#21439,#21440,#21441,
#21442,#21443,#21444,#21445,#21446,#21447,#21448,#21449,#21450,#21451,#21452,
#21453,#21454,#21455,#21456,#21457,#21458,#21459,#21460,#21461,#21462,#21463,
#21464,#21465,#21466,#21467,#21468,#21469,#21470,#21471,#21472,#21473,#21474,
#21475,#21476,#21477,#21478,#21479,#21480,#21481,#21482,#21483,#21484,#21485,
#21486,#21487,#21488,#21489,#21490,#21491,#21492,#21493,#21494,#21495,#21496,
#21497,#21498,#21499,#21500,#21501,#21502,#21503,#21504,#21505,#21506,#21507,
#21508,#21509,#21510,#21511,#21512,#21513,#21514,#21515,#21516,#21517,#21518,
#21519,#21520,#21521,#21522,#21523,#21524,#21525,#21526,#21527,#21528,#21529,
#21530,#21531,#21532,#21533,#21534,#21535,#21536,#21537,#21538,#21539,#21540,
#21541,#21542,#21543,#21544,#21545,#21546,#21547,#21548,#21549,#21550,#21551,
#21552,#21553,#21554,#21555,#21556,#21557,#21558,#21559,#21560,#21561,#21562,
#21563,#21564,#21565,#21566,#21567,#21568,#21569,#21570,#21571,#21572,#21573,
#21574,#21575,#21576,#21577,#21578,#21579,#21580,#21581,#21582,#21583,#21584,
#21585,#21586,#21587,#21588,#21589,#21590,#21591,#21592,#21593,#21594,#21595,
#21596,#21597,#21598,#21599,#21600,#21601,#21602,#21603,#21604,#21605,#21606,
#21607,#21608,#21609,#21610,#21611,#21612,#21613,#21614,#21615,#21616,#21617,
#21618,#21619,#21620,#21621,#21622,#21623,#21624,#21625,#21626,#21627,#21628,
#21629,#21630,#21631,#21632,#21633,#21634,#21635,#21636,#21637,#21638,#21639,
#21640,#21641,#21642,#21643,#21644,#21645,#21646,#21647,#21648,#21649,#21650,
#21651,#21652,#21653,#21654,#21655,#21656,#21657,#21658,#21659,#21660,#21661,
#21662,#21663,#21664,#21665,#21666,#21667,#21668,#21669,#21670,#21671,#21672,
#21673,#21674,#21675,#21676,#21677,#21678,#21679,#21680,#21681,#21682,#21683),
 .UNSPECIFIED.,.F.,.F.,(4,3,3,3,3,3,3,3,3,3,3,3,3,3,3,3,3,3,3,3,3,3,3,3,
3,3,3,3,3,3,3,3,3,3,3,3,3,3,3,3,3,3,3,3,3,3,3,3,3,3,3,3,3,3,3,3,3,3,3,3,
3,3,3,3,3,3,3,3,3,3,3,3,3,3,3,3,3,3,3,3,3,3,4),(-167.455359735507,-167.375098519079,
-167.294831376116,-167.214543341274,-167.13421943968,-167.053793393311,
-166.9733128763,-166.892700782444,-166.830244867261,-166.750279908473,-166.670409320368,
-166.590615583341,-166.510881238249,-166.431188872942,-166.3515096544,-166.271833890611,
-166.192145858742,-166.11242983163,-166.032626268699,-165.952773544021,
-165.87280713437,-165.831261365061,-165.751296406274,-165.671425818169,
-165.591632081142,-165.511897736051,-165.432205370743,-165.352526152202,
-165.272850388413,-165.193162356545,-165.113446329433,-165.033642766502,
-164.953790041824,-164.873823632174,-164.832277862862,-164.752312904075,
-164.672442315971,-164.592648578944,-164.512914233853,-164.433221868547,
-164.353542650006,-164.273866886217,-164.19417885435,-164.114462827238,
-164.034659264308,-163.954806539631,-163.87484012998,-163.833294360663,
-163.753329401876,-163.673458813771,-163.593665076744,-163.513930731653,
-163.434238366346,-163.354559147805,-163.274883384015,-163.195195352147,
-163.115479325036,-163.035675762105,-162.955823037427,-162.875856627777,
-162.834310858464,-162.754345899677,-162.674475311572,-162.594681574545,
-162.514947229455,-162.435254864148,-162.355575645607,-162.275899881818,
-162.19621184995,-162.116495822838,-162.036692259908,-161.95683953523,-161.876873125579,
-161.835327356265,-161.752433240273,-161.672573680655,-161.592790068042,
-161.513066625362,-161.433387616291,-161.353731766857,-161.274088809355,
-161.194430887686,-161.172174428328),.UNSPECIFIED.);
#285=B_SPLINE_CURVE_WITH_KNOTS('',3,(#21685,#21686,#21687,#21688,#21689,
#21690,#21691,#21692,#21693,#21694),.UNSPECIFIED.,.F.,.F.,(4,1,1,1,1,1,
1,4),(-161.172166981905,-160.836343854065,-159.837360351866,-158.838376849667,
-157.839393347468,-156.840409845269,-155.84142634307,-154.888995230419),
 .UNSPECIFIED.);
#286=B_SPLINE_CURVE_WITH_KNOTS('',3,(#21696,#21697,#21698,#21699,#21700,
#21701,#21702,#21703,#21704,#21705,#21706,#21707,#21708,#21709,#21710,#21711,
#21712,#21713,#21714,#21715,#21716,#21717,#21718,#21719,#21720,#21721,#21722,
#21723,#21724,#21725,#21726,#21727,#21728,#21729,#21730,#21731,#21732,#21733,
#21734,#21735,#21736,#21737,#21738,#21739,#21740,#21741,#21742,#21743,#21744,
#21745,#21746,#21747,#21748,#21749,#21750,#21751,#21752,#21753,#21754,#21755,
#21756,#21757,#21758,#21759,#21760,#21761,#21762,#21763,#21764,#21765,#21766,
#21767,#21768,#21769,#21770,#21771,#21772,#21773,#21774,#21775,#21776,#21777,
#21778,#21779,#21780,#21781,#21782,#21783,#21784,#21785,#21786,#21787,#21788,
#21789,#21790,#21791,#21792,#21793,#21794,#21795,#21796,#21797,#21798,#21799,
#21800,#21801,#21802,#21803,#21804,#21805,#21806,#21807,#21808,#21809,#21810,
#21811,#21812,#21813,#21814,#21815,#21816,#21817,#21818,#21819,#21820,#21821,
#21822,#21823,#21824,#21825,#21826,#21827,#21828,#21829,#21830,#21831,#21832,
#21833,#21834,#21835,#21836,#21837,#21838,#21839,#21840,#21841,#21842,#21843,
#21844,#21845,#21846,#21847,#21848,#21849,#21850,#21851,#21852,#21853,#21854,
#21855,#21856,#21857,#21858,#21859,#21860,#21861,#21862,#21863,#21864,#21865,
#21866,#21867,#21868,#21869,#21870,#21871,#21872,#21873,#21874,#21875,#21876,
#21877,#21878,#21879,#21880,#21881,#21882,#21883,#21884,#21885,#21886,#21887,
#21888,#21889,#21890,#21891,#21892,#21893,#21894,#21895,#21896,#21897,#21898,
#21899,#21900,#21901,#21902,#21903,#21904,#21905,#21906,#21907,#21908,#21909,
#21910,#21911,#21912,#21913,#21914,#21915,#21916,#21917,#21918,#21919,#21920,
#21921,#21922,#21923,#21924,#21925,#21926,#21927,#21928,#21929,#21930,#21931,
#21932,#21933,#21934,#21935,#21936,#21937,#21938,#21939,#21940,#21941,#21942),
 .UNSPECIFIED.,.F.,.F.,(4,3,3,3,3,3,3,3,3,3,3,3,3,3,3,3,3,3,3,3,3,3,3,3,
3,3,3,3,3,3,3,3,3,3,3,3,3,3,3,3,3,3,3,3,3,3,3,3,3,3,3,3,3,3,3,3,3,3,3,3,
3,3,3,3,3,3,3,3,3,3,3,3,3,3,3,3,3,3,3,3,3,3,4),(-154.888989121148,-154.84244284087,
-154.762477882083,-154.682607293978,-154.602813556951,-154.52307921186,
-154.443386846553,-154.363707628012,-154.284031864223,-154.204343832355,
-154.124627805244,-154.044824242313,-153.964971517635,-153.885005107985,
-153.843459338671,-153.763494379884,-153.683623791779,-153.603830054752,
-153.524095709661,-153.444403344354,-153.364724125813,-153.285048362024,
-153.205360330156,-153.125644303045,-153.045840740114,-152.965988015436,
-152.886021605786,-152.844475836472,-152.764510877685,-152.68464028958,
-152.604846552553,-152.525112207462,-152.445419842156,-152.365740623614,
-152.286064859825,-152.206376827958,-152.126660800846,-152.046857237916,
-151.967004513238,-151.887038103587,-151.845492334273,-151.765527375486,
-151.685656787381,-151.605863050354,-151.526128705263,-151.446436339956,
-151.366757121415,-151.287081357626,-151.207393325758,-151.127677298646,
-151.047873735716,-150.968021011038,-150.888054601387,-150.846508832074,
-150.766543873287,-150.686673285182,-150.606879548156,-150.527145203065,
-150.447452837758,-150.367773619217,-150.288097855428,-150.20840982356,
-150.128693796449,-150.048890233519,-149.969037508841,-149.88907109919,
-149.847525329875,-149.767560371087,-149.687689782982,-149.607896045955,
-149.528161700864,-149.448469335557,-149.368790117015,-149.289114353226,
-149.209426321358,-149.129710294246,-149.049906731315,-148.970054006637,
-148.890087596986,-148.848541827675,-148.742408125834,-148.638731099375,
-148.605803878848),.UNSPECIFIED.);
#287=B_SPLINE_CURVE_WITH_KNOTS('',3,(#21944,#21945,#21946,#21947,#21948,
#21949,#21950,#21951,#21952,#21953),.UNSPECIFIED.,.F.,.F.,(4,1,1,1,1,1,
1,4),(-148.605803813969,-147.849558325476,-146.850574823277,-145.851591321078,
-144.852607818879,-143.85362431668,-142.854640814481,-142.322618506789),
 .UNSPECIFIED.);
#288=B_SPLINE_CURVE_WITH_KNOTS('',3,(#21955,#21956,#21957,#21958,#21959,
#21960,#21961,#21962,#21963,#21964,#21965,#21966,#21967,#21968,#21969,#21970,
#21971,#21972,#21973,#21974,#21975,#21976,#21977,#21978,#21979,#21980,#21981,
#21982,#21983,#21984,#21985,#21986,#21987,#21988,#21989,#21990,#21991,#21992,
#21993,#21994,#21995,#21996,#21997,#21998,#21999,#22000,#22001,#22002,#22003,
#22004,#22005,#22006,#22007,#22008,#22009,#22010,#22011,#22012,#22013,#22014,
#22015,#22016,#22017,#22018,#22019,#22020,#22021,#22022,#22023,#22024,#22025,
#22026,#22027,#22028,#22029,#22030,#22031,#22032,#22033,#22034,#22035,#22036,
#22037,#22038,#22039,#22040,#22041,#22042,#22043,#22044,#22045,#22046,#22047,
#22048,#22049,#22050,#22051,#22052,#22053,#22054,#22055,#22056,#22057,#22058,
#22059,#22060,#22061,#22062,#22063,#22064,#22065,#22066,#22067,#22068,#22069,
#22070,#22071,#22072,#22073,#22074,#22075,#22076,#22077,#22078,#22079,#22080,
#22081,#22082,#22083,#22084,#22085,#22086,#22087,#22088,#22089,#22090,#22091,
#22092,#22093,#22094,#22095,#22096,#22097,#22098,#22099,#22100,#22101,#22102,
#22103,#22104,#22105,#22106,#22107,#22108,#22109,#22110,#22111,#22112,#22113,
#22114,#22115,#22116,#22117,#22118,#22119,#22120,#22121,#22122,#22123,#22124,
#22125,#22126,#22127,#22128,#22129,#22130,#22131,#22132,#22133,#22134,#22135,
#22136,#22137,#22138,#22139,#22140,#22141,#22142,#22143,#22144,#22145,#22146,
#22147,#22148,#22149,#22150,#22151,#22152,#22153,#22154,#22155,#22156,#22157,
#22158,#22159,#22160,#22161,#22162,#22163,#22164,#22165,#22166,#22167,#22168,
#22169,#22170,#22171,#22172,#22173,#22174,#22175,#22176,#22177,#22178,#22179,
#22180,#22181,#22182,#22183,#22184,#22185,#22186,#22187,#22188,#22189,#22190,
#22191,#22192,#22193,#22194,#22195,#22196,#22197,#22198,#22199,#22200,#22201),
 .UNSPECIFIED.,.F.,.F.,(4,3,3,3,3,3,3,3,3,3,3,3,3,3,3,3,3,3,3,3,3,3,3,3,
3,3,3,3,3,3,3,3,3,3,3,3,3,3,3,3,3,3,3,3,3,3,3,3,3,3,3,3,3,3,3,3,3,3,3,3,
3,3,3,3,3,3,3,3,3,3,3,3,3,3,3,3,3,3,3,3,3,3,4),(-142.322618329037,-142.23793781684,
-142.15310675734,-142.068036935033,-141.982839353648,-141.897437429691,
-141.855657312281,-141.775692353494,-141.695821765389,-141.616028028363,
-141.536293683272,-141.456601317965,-141.376922099424,-141.297246335635,
-141.217558303767,-141.137842276656,-141.058038713725,-140.978185989048,
-140.898219579397,-140.856673810082,-140.776708851295,-140.69683826319,
-140.617044526163,-140.537310181072,-140.457617815765,-140.377938597224,
-140.298262833435,-140.218574801567,-140.138858774456,-140.059055211525,
-139.979202486848,-139.899236077197,-139.857690307883,-139.777725349096,
-139.697854760991,-139.618061023964,-139.538326678873,-139.458634313566,
-139.378955095025,-139.299279331236,-139.219591299368,-139.139875272257,
-139.060071709326,-138.980218984648,-138.900252574998,-138.858706805684,
-138.778741846897,-138.698871258792,-138.619077521765,-138.539343176674,
-138.459650811367,-138.379971592826,-138.300295829037,-138.220607797169,
-138.140891770057,-138.061088207127,-137.981235482449,-137.901269072799,
-137.859723303485,-137.779758344698,-137.699887756593,-137.620094019566,
-137.540359674475,-137.460667309168,-137.380988090627,-137.301312326838,
-137.22162429497,-137.141908267858,-137.062104704928,-136.98225198025,-136.902285570599,
-136.860739801286,-136.781963863931,-136.703281982304,-136.624675669747,
-136.546130316017,-136.467617718984,-136.389121300227,-136.310624495926,
-136.232080347846,-136.153509354394,-136.074858850881,-136.03943319961),
 .UNSPECIFIED.);
#289=B_SPLINE_CURVE_WITH_KNOTS('',3,(#22203,#22204,#22205,#22206,#22207,
#22208,#22209,#22210,#22211,#22212,#22213),.UNSPECIFIED.,.F.,.F.,(4,1,1,
1,1,1,1,1,4),(-136.03943319961,-135.861756299086,-134.862772796887,-133.863789294688,
-132.864805792489,-131.86582229029,-130.866838788091,-129.867855285891,
-129.75624789243),.UNSPECIFIED.);
#290=B_SPLINE_CURVE_WITH_KNOTS('',3,(#22215,#22216,#22217,#22218,#22219,
#22220,#22221,#22222,#22223,#22224,#22225,#22226,#22227,#22228,#22229,#22230,
#22231,#22232,#22233,#22234,#22235,#22236,#22237,#22238,#22239,#22240,#22241,
#22242,#22243,#22244,#22245,#22246,#22247,#22248,#22249,#22250,#22251,#22252,
#22253,#22254,#22255,#22256,#22257,#22258,#22259,#22260,#22261,#22262,#22263,
#22264,#22265,#22266,#22267,#22268,#22269,#22270,#22271,#22272,#22273,#22274,
#22275,#22276,#22277,#22278,#22279,#22280,#22281,#22282,#22283,#22284,#22285,
#22286,#22287,#22288,#22289,#22290,#22291,#22292,#22293,#22294,#22295,#22296,
#22297,#22298,#22299,#22300,#22301,#22302,#22303,#22304,#22305,#22306,#22307,
#22308,#22309,#22310,#22311,#22312,#22313,#22314,#22315,#22316,#22317,#22318,
#22319,#22320,#22321,#22322,#22323,#22324,#22325,#22326,#22327,#22328,#22329,
#22330,#22331,#22332,#22333,#22334,#22335,#22336,#22337,#22338,#22339,#22340,
#22341,#22342,#22343,#22344,#22345,#22346,#22347,#22348,#22349,#22350,#22351,
#22352,#22353,#22354,#22355,#22356,#22357,#22358,#22359,#22360,#22361,#22362,
#22363,#22364,#22365,#22366,#22367,#22368,#22369,#22370,#22371,#22372,#22373,
#22374,#22375,#22376,#22377,#22378,#22379,#22380,#22381,#22382,#22383,#22384,
#22385,#22386,#22387,#22388,#22389,#22390,#22391,#22392,#22393,#22394,#22395,
#22396,#22397,#22398,#22399,#22400,#22401,#22402,#22403,#22404,#22405,#22406,
#22407,#22408,#22409,#22410,#22411,#22412,#22413,#22414,#22415,#22416,#22417,
#22418,#22419,#22420,#22421,#22422,#22423,#22424,#22425,#22426,#22427,#22428,
#22429,#22430,#22431,#22432,#22433,#22434,#22435,#22436,#22437,#22438,#22439,
#22440,#22441,#22442,#22443,#22444,#22445,#22446,#22447,#22448,#22449,#22450,
#22451,#22452,#22453,#22454,#22455,#22456,#22457,#22458,#22459,#22460,#22461),
 .UNSPECIFIED.,.F.,.F.,(4,3,3,3,3,3,3,3,3,3,3,3,3,3,3,3,3,3,3,3,3,3,3,3,
3,3,3,3,3,3,3,3,3,3,3,3,3,3,3,3,3,3,3,3,3,3,3,3,3,3,3,3,3,3,3,3,3,3,3,3,
3,3,3,3,3,3,3,3,3,3,3,3,3,3,3,3,3,3,3,3,3,3,4),(-129.75624789243,-129.677400284394,
-129.598635444903,-129.519935025007,-129.438552119843,-129.359916309128,
-129.281285607269,-129.20264352438,-129.123973564056,-129.04521909352,-128.96641410446,
-128.887503557997,-128.868871783692,-128.788906824905,-128.7090362368,-128.629242499773,
-128.549508154682,-128.469815789375,-128.390136570834,-128.310460807045,
-128.230772775177,-128.151056748066,-128.071253185136,-127.991400460458,
-127.911434050807,-127.869888281493,-127.789923322706,-127.710052734601,
-127.630258997574,-127.550524652483,-127.470832287177,-127.391153068636,
-127.311477304847,-127.231789272979,-127.152073245867,-127.072269682936,
-126.992416958259,-126.912450548608,-126.870904779294,-126.790939820507,
-126.711069232402,-126.631275495375,-126.551541150284,-126.471848784978,
-126.392169566436,-126.312493802647,-126.232805770779,-126.153089743668,
-126.073286180737,-125.993433456059,-125.913467046409,-125.871921277095,
-125.791956318308,-125.712085730203,-125.632291993177,-125.552557648086,
-125.47286528278,-125.393186064239,-125.31351030045,-125.233822268582,-125.15410624147,
-125.07430267854,-124.994449953862,-124.914483544212,-124.872937774896,
-124.792972816109,-124.713102228004,-124.633308490977,-124.553574145886,
-124.473881780578,-124.394202562036,-124.314526798247,-124.234838766379,
-124.155122739268,-124.075319176337,-123.99546645166,-123.915500042009,
-123.873954272696,-123.78504006974,-123.69648948946,-123.608175320554,-123.520245837753,
-123.473062807661),.UNSPECIFIED.);
#291=B_SPLINE_CURVE_WITH_KNOTS('',3,(#22463,#22464,#22465,#22466,#22467,
#22468,#22469,#22470,#22471,#22472),.UNSPECIFIED.,.F.,.F.,(4,1,1,1,1,1,
1,4),(-123.47306258525,-122.874970770497,-121.875987268298,-120.877003766099,
-119.8780202639,-118.879036761701,-117.880053259501,-117.189877278071),
 .UNSPECIFIED.);
#292=B_SPLINE_CURVE_WITH_KNOTS('',3,(#22474,#22475,#22476,#22477,#22478,
#22479,#22480,#22481,#22482,#22483,#22484,#22485,#22486,#22487,#22488,#22489,
#22490,#22491,#22492,#22493,#22494,#22495,#22496,#22497,#22498,#22499,#22500,
#22501,#22502,#22503,#22504,#22505,#22506,#22507,#22508,#22509,#22510,#22511,
#22512,#22513,#22514,#22515,#22516,#22517,#22518,#22519,#22520,#22521,#22522,
#22523,#22524,#22525,#22526,#22527,#22528,#22529,#22530,#22531,#22532,#22533,
#22534,#22535,#22536,#22537,#22538,#22539,#22540,#22541,#22542,#22543,#22544,
#22545,#22546,#22547,#22548,#22549,#22550,#22551,#22552,#22553,#22554,#22555,
#22556,#22557,#22558,#22559,#22560,#22561,#22562,#22563,#22564,#22565,#22566,
#22567,#22568,#22569,#22570,#22571,#22572,#22573,#22574,#22575,#22576,#22577,
#22578,#22579,#22580,#22581,#22582,#22583,#22584,#22585,#22586,#22587,#22588,
#22589,#22590,#22591,#22592,#22593,#22594,#22595,#22596,#22597,#22598,#22599,
#22600,#22601,#22602,#22603,#22604,#22605,#22606,#22607,#22608,#22609,#22610,
#22611,#22612,#22613,#22614,#22615,#22616,#22617,#22618,#22619,#22620,#22621,
#22622,#22623,#22624,#22625,#22626,#22627,#22628,#22629,#22630,#22631,#22632,
#22633,#22634,#22635,#22636,#22637,#22638,#22639,#22640,#22641,#22642,#22643,
#22644,#22645,#22646,#22647,#22648,#22649,#22650,#22651,#22652,#22653,#22654,
#22655,#22656,#22657,#22658,#22659,#22660,#22661,#22662,#22663,#22664,#22665,
#22666,#22667,#22668,#22669,#22670,#22671,#22672,#22673,#22674,#22675,#22676,
#22677,#22678,#22679,#22680,#22681,#22682,#22683,#22684,#22685,#22686,#22687,
#22688,#22689,#22690,#22691,#22692,#22693,#22694,#22695,#22696,#22697,#22698,
#22699,#22700,#22701,#22702,#22703,#22704,#22705,#22706,#22707,#22708,#22709,
#22710,#22711,#22712,#22713,#22714,#22715,#22716,#22717,#22718,#22719,#22720),
 .UNSPECIFIED.,.F.,.F.,(4,3,3,3,3,3,3,3,3,3,3,3,3,3,3,3,3,3,3,3,3,3,3,3,
3,3,3,3,3,3,3,3,3,3,3,3,3,3,3,3,3,3,3,3,3,3,3,3,3,3,3,3,3,3,3,3,3,3,3,3,
3,3,3,3,3,3,3,3,3,3,3,3,3,3,3,3,3,3,3,3,3,3,4),(-117.189877077901,-117.094811079126,
-116.999033985742,-116.902482779177,-116.881069757302,-116.801104798515,
-116.72123421041,-116.641440473384,-116.561706128293,-116.482013762986,
-116.402334544445,-116.322658780656,-116.242970748789,-116.163254721677,
-116.083451158747,-116.003598434069,-115.923632024419,-115.882086255103,
-115.802121296316,-115.722250708211,-115.642456971184,-115.562722626093,
-115.483030260787,-115.403351042245,-115.323675278456,-115.243987246588,
-115.164271219477,-115.084467656547,-115.004614931869,-114.924648522218,
-114.883102752904,-114.803137794117,-114.723267206012,-114.643473468985,
-114.563739123894,-114.484046758587,-114.404367540046,-114.324691776256,
-114.245003744389,-114.165287717277,-114.085484154346,-114.005631429668,
-113.925665020018,-113.884119250705,-113.804154291918,-113.724283703813,
-113.644489966787,-113.564755621696,-113.485063256389,-113.405384037848,
-113.325708274059,-113.246020242191,-113.16630421508,-113.08650065215,-113.006647927472,
-112.926681517822,-112.885135748506,-112.805170789718,-112.725300201614,
-112.645506464586,-112.565772119495,-112.486079754188,-112.406400535647,
-112.326724771857,-112.247036739989,-112.167320712878,-112.087517149947,
-112.007664425269,-111.927698015618,-111.886152246306,-111.806453328173,
-111.726848635618,-111.647320396032,-111.567850899475,-111.485206033402,
-111.405789993568,-111.326375498658,-111.246946600615,-111.16748734538,
-111.087940700449,-111.00834232955,-110.928636233749,-110.906691970891),
 .UNSPECIFIED.);
#293=B_SPLINE_CURVE_WITH_KNOTS('',3,(#22722,#22723,#22724,#22725,#22726,
#22727,#22728,#22729,#22730,#22731,#22732,#22733),.UNSPECIFIED.,.F.,.F.,
(4,2,1,1,1,1,1,1,4),(-110.906691970891,-110.887168744107,-109.888185241908,
-108.889201739709,-107.89021823751,-106.891234735311,-105.892251233111,
-104.893267730912,-104.623510152804),.UNSPECIFIED.);
#294=B_SPLINE_CURVE_WITH_KNOTS('',3,(#22735,#22736,#22737,#22738,#22739,
#22740,#22741,#22742,#22743,#22744,#22745,#22746,#22747,#22748,#22749,#22750,
#22751,#22752,#22753,#22754,#22755,#22756,#22757,#22758,#22759,#22760,#22761,
#22762,#22763,#22764,#22765,#22766,#22767,#22768,#22769,#22770,#22771,#22772,
#22773,#22774,#22775,#22776,#22777,#22778,#22779,#22780,#22781,#22782,#22783,
#22784,#22785,#22786,#22787,#22788,#22789,#22790,#22791,#22792,#22793,#22794,
#22795,#22796,#22797,#22798,#22799,#22800,#22801,#22802,#22803,#22804,#22805,
#22806,#22807,#22808,#22809,#22810,#22811,#22812,#22813,#22814,#22815,#22816,
#22817,#22818,#22819,#22820,#22821,#22822,#22823,#22824,#22825,#22826,#22827,
#22828,#22829,#22830,#22831,#22832,#22833,#22834,#22835,#22836,#22837,#22838,
#22839,#22840,#22841,#22842,#22843,#22844,#22845,#22846,#22847,#22848,#22849,
#22850,#22851,#22852,#22853,#22854,#22855,#22856,#22857,#22858,#22859,#22860,
#22861,#22862,#22863,#22864,#22865,#22866,#22867,#22868,#22869,#22870,#22871,
#22872,#22873,#22874,#22875,#22876,#22877,#22878,#22879,#22880,#22881,#22882,
#22883,#22884,#22885,#22886,#22887,#22888,#22889,#22890,#22891,#22892,#22893,
#22894,#22895,#22896,#22897,#22898,#22899,#22900,#22901,#22902,#22903,#22904,
#22905,#22906,#22907,#22908,#22909,#22910,#22911,#22912,#22913,#22914,#22915,
#22916,#22917,#22918,#22919,#22920,#22921,#22922,#22923,#22924,#22925,#22926,
#22927,#22928,#22929,#22930,#22931,#22932,#22933,#22934,#22935,#22936,#22937,
#22938,#22939,#22940,#22941,#22942,#22943,#22944,#22945,#22946,#22947,#22948,
#22949,#22950,#22951,#22952,#22953,#22954,#22955,#22956,#22957,#22958,#22959,
#22960,#22961,#22962,#22963,#22964,#22965,#22966,#22967,#22968,#22969,#22970,
#22971,#22972,#22973,#22974,#22975,#22976,#22977,#22978,#22979,#22980,#22981),
 .UNSPECIFIED.,.F.,.F.,(4,3,3,3,3,3,3,3,3,3,3,3,3,3,3,3,3,3,3,3,3,3,3,3,
3,3,3,3,3,3,3,3,3,3,3,3,3,3,3,3,3,3,3,3,3,3,3,3,3,3,3,3,3,3,3,3,3,3,3,3,
3,3,3,3,3,3,3,3,3,3,3,3,3,3,3,3,3,3,3,3,3,3,4),(-104.623506663712,-104.544533831671,
-104.463252631302,-104.384335203533,-104.305419740579,-104.226489938422,
-104.143438510995,-104.064388243244,-103.985284593363,-103.906075294704,
-103.894284228713,-103.814319269926,-103.734448681821,-103.654654944795,
-103.574920599704,-103.495228234397,-103.415549015856,-103.335873252067,
-103.256185220199,-103.176469193088,-103.096665630158,-103.01681290548,
-102.936846495829,-102.895300726514,-102.815335767727,-102.735465179622,
-102.655671442595,-102.575937097504,-102.496244732198,-102.416565513657,
-102.336889749868,-102.257201718,-102.177485690888,-102.097682127958,-102.01782940328,
-101.93786299363,-101.896317224315,-101.816352265528,-101.736481677423,
-101.656687940396,-101.576953595305,-101.497261229997,-101.417582011456,
-101.337906247667,-101.258218215799,-101.178502188688,-101.098698625757,
-101.018845901079,-100.938879491428,-100.897333722116,-100.817368763329,
-100.737498175224,-100.657704438197,-100.577970093106,-100.498277727799,
-100.418598509258,-100.338922745469,-100.259234713601,-100.17951868649,
-100.09971512356,-100.019862398881,-99.9398959892309,-99.8983502199165,
-99.8183852611291,-99.7385146730248,-99.6587209359978,-99.5789865909066,
-99.4992942255997,-99.4196150070583,-99.339939243269,-99.2602512114012,
-99.1805351842898,-99.1007316213594,-99.0208788966816,-98.9409124870312,
-98.8993667177173,-98.8172189994476,-98.7351845679469,-98.6532507164691,
-98.5714312330947,-98.4896786671188,-98.4079936626733,-98.3403213565321),
 .UNSPECIFIED.);
#295=B_SPLINE_CURVE_WITH_KNOTS('',3,(#22983,#22984,#22985,#22986,#22987,
#22988,#22989,#22990,#22991,#22992),.UNSPECIFIED.,.F.,.F.,(4,1,1,1,1,1,
1,4),(-98.3403165567537,-97.9003832155181,-96.901399713319,-95.9024162111198,
-94.9034327089206,-93.9044492067215,-92.9054657045223,-92.0571360493525),
 .UNSPECIFIED.);
#296=B_SPLINE_CURVE_WITH_KNOTS('',3,(#22994,#22995,#22996,#22997,#22998,
#22999,#23000,#23001,#23002,#23003,#23004),.UNSPECIFIED.,.F.,.F.,(4,1,1,
1,1,1,1,1,4),(-92.0571360493525,-91.9064822023231,-90.907498700124,-89.9085151979248,
-88.9095316957257,-87.9105481935265,-86.9115646913273,-85.9125811891282,
-85.7739507421729),.UNSPECIFIED.);
#297=B_SPLINE_CURVE_WITH_KNOTS('',3,(#23006,#23007,#23008,#23009,#23010,
#23011,#23012,#23013,#23014,#23015),.UNSPECIFIED.,.F.,.F.,(4,1,1,1,1,1,
1,4),(-85.7739507421729,-84.913597686929,-83.9146141847298,-82.9156306825307,
-81.9166471803315,-80.9176636781323,-79.9186801759332,-79.4907710080448),
 .UNSPECIFIED.);
#298=B_SPLINE_CURVE_WITH_KNOTS('',3,(#23017,#23018,#23019,#23020,#23021,
#23022,#23023,#23024,#23025,#23026,#23027,#23028,#23029,#23030,#23031,#23032,
#23033,#23034,#23035,#23036,#23037,#23038,#23039,#23040,#23041,#23042,#23043,
#23044,#23045,#23046,#23047,#23048,#23049,#23050,#23051,#23052,#23053,#23054,
#23055,#23056,#23057,#23058,#23059,#23060,#23061,#23062,#23063,#23064,#23065,
#23066,#23067,#23068,#23069,#23070,#23071,#23072,#23073,#23074,#23075,#23076,
#23077,#23078,#23079,#23080,#23081,#23082,#23083,#23084,#23085,#23086,#23087,
#23088,#23089,#23090,#23091,#23092,#23093,#23094,#23095,#23096,#23097,#23098,
#23099,#23100,#23101,#23102,#23103,#23104,#23105,#23106,#23107,#23108,#23109,
#23110,#23111,#23112,#23113,#23114,#23115,#23116,#23117,#23118,#23119,#23120,
#23121,#23122,#23123,#23124,#23125,#23126,#23127,#23128,#23129,#23130,#23131,
#23132,#23133,#23134,#23135,#23136,#23137,#23138,#23139,#23140,#23141,#23142,
#23143,#23144,#23145,#23146,#23147,#23148,#23149,#23150,#23151,#23152,#23153,
#23154,#23155,#23156,#23157,#23158,#23159,#23160,#23161,#23162,#23163,#23164,
#23165,#23166,#23167,#23168,#23169,#23170,#23171,#23172,#23173,#23174,#23175,
#23176,#23177,#23178,#23179,#23180,#23181,#23182,#23183,#23184,#23185,#23186,
#23187,#23188,#23189,#23190,#23191,#23192,#23193,#23194,#23195,#23196,#23197,
#23198,#23199,#23200,#23201,#23202,#23203,#23204,#23205,#23206,#23207,#23208,
#23209,#23210,#23211,#23212,#23213,#23214,#23215,#23216,#23217,#23218,#23219,
#23220,#23221,#23222,#23223,#23224,#23225,#23226,#23227,#23228,#23229,#23230,
#23231,#23232,#23233,#23234,#23235,#23236,#23237,#23238,#23239,#23240,#23241,
#23242,#23243,#23244,#23245,#23246,#23247,#23248,#23249,#23250,#23251,#23252,
#23253,#23254,#23255,#23256,#23257,#23258,#23259,#23260),.UNSPECIFIED.,
 .F.,.F.,(4,3,3,3,3,3,3,3,3,3,3,3,3,3,3,3,3,3,3,3,3,3,3,3,3,3,3,3,3,3,3,
3,3,3,3,3,3,3,3,3,3,3,3,3,3,3,3,3,3,3,3,3,3,3,3,3,3,3,3,3,3,3,3,3,3,3,3,
3,3,3,3,3,3,3,3,3,3,3,3,3,3,4),(-79.4907654349933,-79.4093838734493,-79.3279642298507,
-79.2464934153202,-79.1647942299237,-79.0831339105501,-79.0013201594021,
-78.919696673734,-78.8397317149467,-78.759861126842,-78.680067389815,-78.6003330447239,
-78.5206406794171,-78.4409614608759,-78.3612856970868,-78.2815976652188,
-78.2018816381072,-78.1220780751767,-78.0422253504988,-77.9622589408483,
-77.9207131715348,-77.8407482127475,-77.760877624643,-77.6810838876163,
-77.6013495425248,-77.5216571772175,-77.4419779586762,-77.362302194887,
-77.282614163019,-77.2028981359072,-77.1230945729766,-77.0432418482986,
-76.9632754386482,-76.9217296693357,-76.8417647105485,-76.7618941224439,
-76.6821003854173,-76.6023660403263,-76.5226736750192,-76.4429944564781,
-76.3633186926889,-76.2836306608211,-76.2039146337097,-76.1241110707792,
-76.0442583461009,-75.9642919364505,-75.9227461671365,-75.8427812083493,
-75.7629106202447,-75.6831168832177,-75.6033825381264,-75.5236901728197,
-75.4440109542785,-75.3643351904894,-75.2846471586215,-75.2049311315103,
-75.1251275685798,-75.0452748439019,-74.9653084342515,-74.9237626649374,
-74.8437977061501,-74.7639271180454,-74.6841333810186,-74.6043990359275,
-74.5247066706209,-74.4450274520797,-74.3653516882905,-74.2856636564222,
-74.2059476293107,-74.1261440663803,-74.0462913417027,-73.966324932052,
-73.9247791627382,-73.8454582994504,-73.7657235279958,-73.6865968180439,
-73.6075245531369,-73.5284904554073,-73.4482628735089,-73.3692415196554,
-73.2884108237346,-73.2075801278137),.UNSPECIFIED.);
#299=B_SPLINE_CURVE_WITH_KNOTS('',3,(#23262,#23263,#23264,#23265,#23266,
#23267,#23268,#23269,#23270,#23271,#23272),.UNSPECIFIED.,.F.,.F.,(4,1,1,
1,1,1,1,1,4),(-73.2075756699579,-72.925795660539,-71.9268121583399,-70.9278286561407,
-69.9288451539415,-68.9298616517423,-67.9308781495432,-66.931894647344,
-66.9243948206341),.UNSPECIFIED.);
#300=B_SPLINE_CURVE_WITH_KNOTS('',3,(#23274,#23275,#23276,#23277,#23278,
#23279,#23280,#23281,#23282,#23283,#23284,#23285,#23286,#23287,#23288,#23289,
#23290,#23291,#23292,#23293,#23294,#23295,#23296,#23297,#23298,#23299,#23300,
#23301,#23302,#23303,#23304,#23305,#23306,#23307,#23308,#23309,#23310,#23311,
#23312,#23313,#23314,#23315,#23316,#23317,#23318,#23319,#23320,#23321,#23322,
#23323,#23324,#23325,#23326,#23327,#23328,#23329,#23330,#23331,#23332,#23333,
#23334,#23335,#23336,#23337,#23338,#23339,#23340,#23341,#23342,#23343,#23344,
#23345,#23346,#23347,#23348,#23349,#23350,#23351,#23352,#23353,#23354,#23355,
#23356,#23357,#23358,#23359,#23360,#23361,#23362,#23363,#23364,#23365,#23366,
#23367,#23368,#23369,#23370,#23371,#23372,#23373,#23374,#23375,#23376,#23377,
#23378,#23379,#23380,#23381,#23382,#23383,#23384,#23385,#23386,#23387,#23388,
#23389,#23390,#23391,#23392,#23393,#23394,#23395,#23396,#23397,#23398,#23399,
#23400,#23401,#23402,#23403,#23404,#23405,#23406,#23407,#23408,#23409,#23410,
#23411,#23412,#23413,#23414,#23415,#23416,#23417,#23418,#23419,#23420,#23421,
#23422,#23423,#23424,#23425,#23426,#23427,#23428,#23429,#23430,#23431,#23432,
#23433,#23434,#23435,#23436,#23437,#23438,#23439,#23440,#23441,#23442,#23443,
#23444,#23445,#23446,#23447,#23448,#23449,#23450,#23451,#23452,#23453,#23454,
#23455,#23456,#23457,#23458,#23459,#23460,#23461,#23462,#23463,#23464,#23465,
#23466,#23467,#23468,#23469,#23470,#23471,#23472,#23473,#23474,#23475,#23476,
#23477,#23478,#23479,#23480,#23481,#23482,#23483,#23484,#23485,#23486,#23487,
#23488,#23489,#23490,#23491,#23492,#23493,#23494,#23495,#23496,#23497,#23498,
#23499,#23500,#23501,#23502,#23503,#23504,#23505,#23506,#23507,#23508,#23509,
#23510,#23511,#23512,#23513,#23514,#23515,#23516,#23517),.UNSPECIFIED.,
 .F.,.F.,(4,3,3,3,3,3,3,3,3,3,3,3,3,3,3,3,3,3,3,3,3,3,3,3,3,3,3,3,3,3,3,
3,3,3,3,3,3,3,3,3,3,3,3,3,3,3,3,3,3,3,3,3,3,3,3,3,3,3,3,3,3,3,3,3,3,3,3,
3,3,3,3,3,3,3,3,3,3,3,3,3,3,4),(-66.9243948206341,-66.8445366717091,-66.7647727811955,
-66.6850855254513,-66.6054573420193,-66.525870715806,-66.4462966464282,
-66.3667254575869,-66.2871413334151,-66.2075284531903,-66.1278280023542,
-66.0480775294556,-65.9682151673837,-65.9329111451448,-65.8529461863576,
-65.7730755982529,-65.6932818612262,-65.6135475161349,-65.533855150828,
-65.4541759322868,-65.3745001684976,-65.2948121366298,-65.2150961095186,
-65.1352925465881,-65.0554398219102,-64.9754734122598,-64.9339276429457,
-64.8539626841582,-64.7740920960537,-64.6942983590268,-64.6145640139359,
-64.5348716486287,-64.4551924300873,-64.3755166662981,-64.2958286344302,
-64.2161126073187,-64.1363090443881,-64.0564563197102,-63.9764899100596,
-63.9349441407465,-63.8549791819592,-63.7751085938547,-63.6953148568281,
-63.6155805117372,-63.5358881464298,-63.4562089278887,-63.3765331640996,
-63.2968451322321,-63.2171291051206,-63.1373255421901,-63.0574728175123,
-62.977506407862,-62.9359606385474,-62.85599567976,-62.7761250916552,-62.6963313546284,
-62.6165970095373,-62.53690464423,-62.4572254256887,-62.3775496618996,-62.2978616300315,
-62.21814560292,-62.1383420399896,-62.0584893153119,-61.9785229056614,-61.9369771363482,
-61.8570121775608,-61.7771415894564,-61.6973478524296,-61.6176135073379,
-61.5379211420319,-61.4582419234906,-61.3785661597014,-61.2988781278338,
-61.2191621007223,-61.1393585377919,-61.0595058131141,-60.9795394034634,
-60.937993634149,-60.8401739854018,-60.7406918378632,-60.6412096903246),
 .UNSPECIFIED.);
#301=B_SPLINE_CURVE_WITH_KNOTS('',3,(#23519,#23520,#23521,#23522,#23523,
#23524,#23525,#23526,#23527,#23528),.UNSPECIFIED.,.F.,.F.,(4,1,1,1,1,1,
1,4),(-60.6412095134546,-59.9390101319499,-58.9400266297507,-57.9410431275515,
-56.9420596253524,-55.9430761231532,-54.9440926209541,-54.358024206275),
 .UNSPECIFIED.);
#302=B_SPLINE_CURVE_WITH_KNOTS('',3,(#23530,#23531,#23532,#23533,#23534,
#23535,#23536,#23537,#23538,#23539,#23540,#23541,#23542,#23543,#23544,#23545,
#23546,#23547,#23548,#23549,#23550,#23551,#23552,#23553,#23554,#23555,#23556,
#23557,#23558,#23559,#23560,#23561,#23562,#23563,#23564,#23565,#23566,#23567,
#23568,#23569,#23570,#23571,#23572,#23573,#23574,#23575,#23576,#23577,#23578,
#23579,#23580,#23581,#23582,#23583,#23584,#23585,#23586,#23587,#23588,#23589,
#23590,#23591,#23592,#23593,#23594,#23595,#23596,#23597,#23598,#23599,#23600,
#23601,#23602,#23603,#23604,#23605,#23606,#23607,#23608,#23609,#23610,#23611,
#23612,#23613,#23614,#23615,#23616,#23617,#23618,#23619,#23620,#23621,#23622,
#23623,#23624,#23625,#23626,#23627,#23628,#23629,#23630,#23631,#23632,#23633,
#23634,#23635,#23636,#23637,#23638,#23639,#23640,#23641,#23642,#23643,#23644,
#23645,#23646,#23647,#23648,#23649,#23650,#23651,#23652,#23653,#23654,#23655,
#23656,#23657,#23658,#23659,#23660,#23661,#23662,#23663,#23664,#23665,#23666,
#23667,#23668,#23669,#23670,#23671,#23672,#23673,#23674,#23675,#23676,#23677,
#23678,#23679,#23680,#23681,#23682,#23683,#23684,#23685,#23686,#23687,#23688,
#23689,#23690,#23691,#23692,#23693,#23694,#23695,#23696,#23697,#23698,#23699,
#23700,#23701,#23702,#23703,#23704,#23705,#23706,#23707,#23708,#23709,#23710,
#23711,#23712,#23713,#23714,#23715,#23716,#23717,#23718,#23719,#23720,#23721,
#23722,#23723,#23724,#23725,#23726,#23727,#23728,#23729,#23730,#23731,#23732,
#23733,#23734,#23735,#23736,#23737,#23738,#23739,#23740,#23741,#23742,#23743,
#23744,#23745,#23746,#23747,#23748,#23749,#23750,#23751,#23752,#23753,#23754,
#23755,#23756,#23757,#23758,#23759,#23760,#23761,#23762,#23763,#23764,#23765,
#23766,#23767,#23768,#23769,#23770,#23771,#23772,#23773),.UNSPECIFIED.,
 .F.,.F.,(4,3,3,3,3,3,3,3,3,3,3,3,3,3,3,3,3,3,3,3,3,3,3,3,3,3,3,3,3,3,3,
3,3,3,3,3,3,3,3,3,3,3,3,3,3,3,3,3,3,3,3,3,3,3,3,3,3,3,3,3,3,3,3,3,3,3,3,
3,3,3,3,3,3,3,3,3,3,3,3,3,3,4),(-54.3580240007055,-54.2708272108514,-54.1832202248342,
-54.0954065611413,-54.007286490156,-53.9451091187549,-53.8651441599678,
-53.7852735718634,-53.7054798348367,-53.6257454897457,-53.5460531244392,
-53.4663739058981,-53.3866981421091,-53.3070101102414,-53.22729408313,-53.1474905201998,
-53.0676377955221,-52.9876713858718,-52.9461256165557,-52.8661606577684,
-52.7862900696638,-52.7064963326369,-52.6267619875458,-52.5470696222389,
-52.4673904036976,-52.3877146399085,-52.3080266080406,-52.2283105809291,
-52.1485070179987,-52.0686542933208,-51.9886878836703,-51.9471421143566,
-51.8671771555693,-51.7873065674647,-51.7075128304378,-51.6277784853467,
-51.5480861200399,-51.4684069014987,-51.3887311377095,-51.3090431058416,
-51.22932707873,-51.1495235157996,-51.0696707911216,-50.9897043814711,-50.9481586121574,
-50.8681936533701,-50.7883230652655,-50.7085293282386,-50.6287949831475,
-50.5491026178406,-50.4694233992994,-50.3897476355102,-50.3100596036424,
-50.2303435765308,-50.1505400136004,-50.0706872889225,-49.990720879272,
-49.9491751099582,-49.8692101511709,-49.7893395630663,-49.7095458260395,
-49.6298114809484,-49.5501191156415,-49.4704398971003,-49.3907641333111,
-49.3110761014431,-49.2313600743315,-49.151556511401,-49.0717037867231,
-48.9917373770727,-48.9501916077591,-48.8713376044971,-48.7925772262353,
-48.7138920422833,-48.6340103993848,-48.5554166786926,-48.4768383365752,
-48.3982588533269,-48.317403864769,-48.2387381062066,-48.156788502651,-48.0748388990954),
 .UNSPECIFIED.);
#303=B_SPLINE_CURVE_WITH_KNOTS('',3,(#23775,#23776,#23777,#23778,#23779,
#23780,#23781,#23782,#23783,#23784,#23785),.UNSPECIFIED.,.F.,.F.,(4,1,1,
1,1,1,1,1,4),(-48.0748388990954,-47.9512081055599,-46.9522246033607,-45.9532411011616,
-44.9542575989624,-43.9552740967632,-42.9562905945641,-41.9573070923649,
-41.7916535919158),.UNSPECIFIED.);
#304=B_SPLINE_CURVE_WITH_KNOTS('',3,(#23787,#23788,#23789,#23790,#23791,
#23792,#23793,#23794,#23795,#23796),.UNSPECIFIED.,.F.,.F.,(4,1,1,1,1,1,
1,4),(-41.7916535919158,-40.9583235901658,-39.9593400879666,-38.9603565857674,
-37.9613730835683,-36.9623895813691,-35.9634060791699,-35.5084682847362),
 .UNSPECIFIED.);
#305=B_SPLINE_CURVE_WITH_KNOTS('',3,(#23798,#23799,#23800,#23801,#23802,
#23803,#23804,#23805,#23806,#23807),.UNSPECIFIED.,.F.,.F.,(4,1,1,1,1,1,
1,4),(-35.5084682847362,-34.9644225769708,-33.9654390747716,-32.9664555725724,
-31.9674720703733,-30.9684885681741,-29.9695050659749,-29.2252829775566),
 .UNSPECIFIED.);
#306=B_SPLINE_CURVE_WITH_KNOTS('',3,(#23809,#23810,#23811,#23812,#23813,
#23814,#23815,#23816,#23817,#23818,#23819,#23820,#23821,#23822,#23823,#23824,
#23825,#23826,#23827,#23828,#23829,#23830,#23831,#23832,#23833,#23834,#23835,
#23836,#23837,#23838,#23839,#23840,#23841,#23842,#23843,#23844,#23845,#23846,
#23847,#23848,#23849,#23850,#23851,#23852,#23853,#23854,#23855,#23856,#23857,
#23858,#23859,#23860,#23861,#23862,#23863,#23864,#23865,#23866,#23867,#23868,
#23869,#23870,#23871,#23872,#23873,#23874,#23875,#23876,#23877,#23878,#23879,
#23880,#23881,#23882,#23883,#23884,#23885,#23886,#23887,#23888,#23889,#23890,
#23891,#23892,#23893,#23894,#23895,#23896,#23897,#23898,#23899,#23900,#23901,
#23902,#23903,#23904,#23905,#23906,#23907,#23908,#23909,#23910,#23911,#23912,
#23913,#23914,#23915,#23916,#23917,#23918,#23919,#23920,#23921,#23922,#23923,
#23924,#23925,#23926,#23927,#23928,#23929,#23930,#23931,#23932,#23933,#23934,
#23935,#23936,#23937,#23938,#23939,#23940,#23941,#23942,#23943,#23944,#23945,
#23946,#23947,#23948,#23949,#23950,#23951,#23952,#23953,#23954,#23955,#23956,
#23957,#23958,#23959,#23960,#23961,#23962,#23963,#23964,#23965,#23966,#23967,
#23968,#23969,#23970,#23971,#23972,#23973,#23974,#23975,#23976,#23977,#23978,
#23979,#23980,#23981,#23982,#23983,#23984,#23985,#23986,#23987,#23988,#23989,
#23990,#23991,#23992,#23993,#23994,#23995,#23996,#23997,#23998,#23999,#24000,
#24001,#24002,#24003,#24004,#24005,#24006,#24007,#24008,#24009,#24010,#24011,
#24012,#24013,#24014,#24015,#24016,#24017,#24018,#24019,#24020,#24021,#24022,
#24023,#24024,#24025,#24026,#24027,#24028,#24029,#24030,#24031,#24032,#24033,
#24034,#24035,#24036,#24037,#24038,#24039,#24040,#24041,#24042,#24043,#24044,
#24045,#24046,#24047,#24048,#24049,#24050,#24051,#24052,#24053,#24054,#24055),
 .UNSPECIFIED.,.F.,.F.,(4,3,3,3,3,3,3,3,3,3,3,3,3,3,3,3,3,3,3,3,3,3,3,3,
3,3,3,3,3,3,3,3,3,3,3,3,3,3,3,3,3,3,3,3,3,3,3,3,3,3,3,3,3,3,3,3,3,3,3,3,
3,3,3,3,3,3,3,3,3,3,3,3,3,3,3,3,3,3,3,3,3,3,4),(-29.225282908638,-29.1236675299761,
-29.019946111268,-28.9705215637758,-28.8905566050103,-28.8106860169276,
-28.7308922799228,-28.651157934854,-28.5714655695693,-28.4917863510505,
-28.4121105872837,-28.3324225554383,-28.2527065283492,-28.1729029654411,
-28.0930502407854,-28.0130838311569,-27.9715380615766,-27.8915731027056,
-27.8117025145171,-27.7319087774063,-27.6521744322314,-27.5724820668408,
-27.4928028482162,-27.413127084344,-27.3334390523934,-27.2537230251996,
-27.1739194621878,-27.094066737429,-27.0141003276991,-26.9725545593774,
-26.8925896006817,-26.8127190126685,-26.7329252757326,-26.6531909307319,
-26.5734985655149,-26.4938193470624,-26.4141435833613,-26.3344555515808,
-26.2547395245557,-26.17493596171,-26.095083237116,-26.0151168275474,-25.9735710571783,
-25.8936060985027,-25.8137355105109,-25.7339417735978,-25.6542074286215,
-25.5745150634301,-25.4948358450051,-25.4151600813326,-25.3354720495818,
-25.2557560225876,-25.1759524597742,-25.0960997352135,-25.0161333256793,
-24.9745875549791,-24.894622595637,-24.8147520069765,-24.734958269393,-24.6552239237453,
-24.575531557882,-24.495852338787,-24.4161765744455,-24.3364885420273,-24.2567725143677,
-24.176968950896,-24.0971162256796,-24.0171498154998,-23.9756040527799,
-23.8956390947281,-23.8157685073574,-23.7359747710621,-23.6562404266996,
-23.5765480621178,-23.4968688442942,-23.4171930812177,-23.3375050500571,
-23.2577890236469,-23.1779854614052,-23.09813273741,-23.0181663284267,-22.9766205505808,
-22.9420976703771),.UNSPECIFIED.);
#307=B_SPLINE_CURVE_WITH_KNOTS('',3,(#24057,#24058,#24059,#24060,#24061,
#24062,#24063,#24064,#24065,#24066),.UNSPECIFIED.,.F.,.F.,(4,1,1,1,1,1,
1,4),(-22.9420930021365,-21.9776370483816,-20.9786535461825,-19.9796700439833,
-18.9806865417841,-17.981703039585,-16.9827195373858,-16.6589194036327),
 .UNSPECIFIED.);
#308=B_SPLINE_CURVE_WITH_KNOTS('',3,(#24068,#24069,#24070,#24071,#24072,
#24073,#24074,#24075,#24076,#24077,#24078,#24079,#24080,#24081,#24082,#24083,
#24084,#24085,#24086,#24087,#24088,#24089,#24090,#24091,#24092,#24093,#24094,
#24095,#24096,#24097,#24098,#24099,#24100,#24101,#24102,#24103,#24104,#24105,
#24106,#24107,#24108,#24109,#24110,#24111,#24112,#24113,#24114,#24115,#24116,
#24117,#24118,#24119,#24120,#24121,#24122,#24123,#24124,#24125,#24126,#24127,
#24128,#24129,#24130,#24131,#24132,#24133,#24134,#24135,#24136,#24137,#24138,
#24139,#24140,#24141,#24142,#24143,#24144,#24145,#24146,#24147,#24148,#24149,
#24150,#24151,#24152,#24153,#24154,#24155,#24156,#24157,#24158,#24159,#24160,
#24161,#24162,#24163,#24164,#24165,#24166,#24167,#24168,#24169,#24170,#24171,
#24172,#24173,#24174,#24175,#24176,#24177,#24178,#24179,#24180,#24181,#24182,
#24183,#24184,#24185,#24186,#24187,#24188,#24189,#24190,#24191,#24192,#24193,
#24194,#24195,#24196,#24197,#24198,#24199,#24200,#24201,#24202,#24203,#24204,
#24205,#24206,#24207,#24208,#24209,#24210,#24211,#24212,#24213,#24214,#24215,
#24216,#24217,#24218,#24219,#24220,#24221,#24222,#24223,#24224,#24225,#24226,
#24227,#24228,#24229,#24230,#24231,#24232,#24233,#24234,#24235,#24236,#24237,
#24238,#24239,#24240,#24241,#24242,#24243,#24244,#24245,#24246,#24247,#24248,
#24249,#24250,#24251,#24252,#24253,#24254,#24255,#24256,#24257,#24258,#24259,
#24260,#24261,#24262,#24263,#24264,#24265,#24266,#24267,#24268,#24269,#24270,
#24271,#24272,#24273,#24274,#24275,#24276,#24277,#24278,#24279,#24280,#24281,
#24282,#24283,#24284,#24285,#24286,#24287,#24288,#24289,#24290,#24291,#24292,
#24293,#24294,#24295,#24296,#24297,#24298,#24299,#24300,#24301,#24302,#24303,
#24304,#24305,#24306,#24307,#24308,#24309,#24310,#24311,#24312,#24313,#24314),
 .UNSPECIFIED.,.F.,.F.,(4,3,3,3,3,3,3,3,3,3,3,3,3,3,3,3,3,3,3,3,3,3,3,3,
3,3,3,3,3,3,3,3,3,3,3,3,3,3,3,3,3,3,3,3,3,3,3,3,3,3,3,3,3,3,3,3,3,3,3,3,
3,3,3,3,3,3,3,3,3,3,3,3,3,3,3,3,3,3,3,3,3,3,4),(-16.6589123631975,-16.579410177248,
-16.4999164814568,-16.4204232135971,-16.3409145385783,-16.2613746148487,
-16.1817426099068,-16.102058428893,-16.0222573539416,-15.9837360351866,
-15.9037709364464,-15.8239002078398,-15.7441063299001,-15.6643718436215,
-15.5846793369886,-15.5049999773649,-15.4253240726587,-15.3456359001607,
-15.2659197328274,-15.1861160310025,-15.1062631679752,-15.0262966220169,
-14.9847525329875,-14.9047878768464,-14.8249175914123,-14.745124156798,
-14.6653901135813,-14.5856980493307,-14.5060191296772,-14.4263436634018,
-14.3466559274219,-14.2669401943189,-14.1871369210702,-14.1072844840547,
-14.0273183564487,-13.9857690307883,-13.9058039524718,-13.8259332467455,
-13.7461393940897,-13.6664049354483,-13.5867124587574,-13.5070331323954,
-13.4273572630035,-13.3476691278334,-13.2679529998044,-13.1881493400669,
-13.1082965207654,-13.028330020695,-12.9867855285891,-12.9068197350172,
-12.8269483081417,-12.7471537291907,-12.6674185398466,-12.5877253287758,
-12.5080452649217,-12.4283686561855,-12.3486797804667,-12.2689629113326,
-12.1891585134071,-12.1093049564721,-12.0293377260061,-11.98780202639,-11.9078391995772,
-11.8279707447898,-11.7481791404182,-11.6684469253298,-11.5887566853915,
-11.5090795785972,-11.4294059179036,-11.3497199786927,-11.2700060320064,
-11.1902045204954,-11.1103538338639,-11.0303894239007,-10.9888185241908,
-10.9079683874311,-10.8272182709324,-10.7465533331597,-10.6659587888609,
-10.5854271020028,-10.5049324535704,-10.4244554222795,-10.3757270560178),
 .UNSPECIFIED.);
#309=B_SPLINE_CURVE_WITH_KNOTS('',3,(#24315,#24316,#24317,#24318,#24319,
#24320,#24321,#24322,#24323,#24324,#24325,#24326,#24327,#24328,#24329,#24330,
#24331,#24332,#24333,#24334,#24335,#24336,#24337,#24338,#24339,#24340,#24341,
#24342,#24343,#24344,#24345,#24346,#24347,#24348,#24349,#24350,#24351,#24352,
#24353,#24354,#24355,#24356,#24357,#24358,#24359,#24360,#24361,#24362,#24363,
#24364,#24365,#24366,#24367,#24368,#24369,#24370,#24371,#24372,#24373,#24374,
#24375,#24376,#24377,#24378,#24379,#24380,#24381,#24382,#24383,#24384,#24385,
#24386,#24387,#24388,#24389,#24390,#24391,#24392,#24393,#24394,#24395,#24396,
#24397,#24398,#24399,#24400,#24401,#24402,#24403,#24404,#24405,#24406,#24407,
#24408,#24409,#24410,#24411,#24412,#24413,#24414,#24415,#24416,#24417,#24418,
#24419,#24420,#24421,#24422,#24423,#24424,#24425,#24426,#24427,#24428,#24429,
#24430,#24431,#24432,#24433,#24434,#24435,#24436,#24437,#24438,#24439,#24440,
#24441,#24442,#24443,#24444,#24445,#24446,#24447,#24448,#24449,#24450,#24451,
#24452,#24453,#24454,#24455,#24456,#24457,#24458,#24459,#24460,#24461,#24462,
#24463,#24464,#24465,#24466,#24467,#24468,#24469,#24470,#24471,#24472,#24473,
#24474,#24475,#24476,#24477,#24478,#24479,#24480,#24481,#24482,#24483,#24484,
#24485,#24486,#24487,#24488,#24489,#24490,#24491,#24492,#24493,#24494,#24495,
#24496,#24497,#24498,#24499,#24500,#24501,#24502,#24503,#24504,#24505,#24506,
#24507,#24508,#24509,#24510,#24511,#24512,#24513,#24514,#24515,#24516,#24517,
#24518,#24519,#24520,#24521,#24522,#24523,#24524,#24525,#24526,#24527,#24528,
#24529,#24530,#24531,#24532,#24533,#24534,#24535,#24536,#24537,#24538,#24539,
#24540,#24541,#24542,#24543,#24544,#24545,#24546,#24547,#24548,#24549,#24550,
#24551,#24552,#24553,#24554,#24555,#24556,#24557,#24558,#24559,#24560,#24561),
 .UNSPECIFIED.,.F.,.F.,(4,3,3,3,3,3,3,3,3,3,3,3,3,3,3,3,3,3,3,3,3,3,3,3,
3,3,3,3,3,3,3,3,3,3,3,3,3,3,3,3,3,3,3,3,3,3,3,3,3,3,3,3,3,3,3,3,3,3,3,3,
3,3,3,3,3,3,3,3,3,3,3,3,3,3,3,3,3,3,3,3,3,3,4),(-10.3757270559041,-10.2869920871581,
-10.1977381029001,-10.108217706739,-10.0183574668925,-9.98983502199165,
-9.90986528326832,-9.82998988698337,-9.75019131838053,-9.67045212311163,
-9.59075489377989,-9.51107080616828,-9.43139017068793,-9.35169726874048,
-9.27197637739935,-9.19216798373438,-9.11231044011139,-9.03233927145686,
-8.99085151979248,-8.91090124579369,-8.8310453591876,-8.75126632648789,
-8.67154667478177,-8.59186897821204,-8.51220434532162,-8.4325431142785,
-8.35286954991441,-8.27316791267112,-8.19337854952507,-8.11353993816696,
-8.03358738564243,-7.99186801759332,-7.91189007011555,-7.83200655967694,
-7.75219997789339,-7.67245287681802,-7.59274785550133,-7.51305616936823,
-7.43336805599691,-7.3536678028127,-7.27393969299786,-7.19412431776395,
-7.1142599163916,-7.03428214115358,-6.99288451539415,-6.91289368398352,
-6.83299702701498,-6.75317705182906,-6.6734163258982,-6.59369746344528,
-6.51399165994175,-6.43428925966801,-6.35457456318493,-6.27483186672925,
-6.19500176270018,-6.1151225302351,-6.03512989349482,-5.99390101319498,
-5.91403497940862,-5.83426347376325,-5.75456888393364,-5.67493365889373,
-5.59534029512317,-5.51575959094961,-5.43618203185169,-5.35659181285564,
-5.27697312429453,-5.19726569154639,-5.11750855838175,-5.03763607409116,
-4.99491751099582,-4.9158035640275,-4.83678366946472,-4.7578395671856,-4.67895306886685,
-4.60010142097271,-4.52126630226961,-4.442431337671,-4.3635801545808,-4.28465880105462,
-4.20569728010626,-4.12663765514124,-4.0925417489438),.UNSPECIFIED.);
#310=B_SPLINE_CURVE_WITH_KNOTS('',3,(#24565,#24566,#24567,#24568,#24569,
#24570,#24571,#24572,#24573,#24574,#24575,#24576,#24577,#24578,#24579,#24580,
#24581,#24582,#24583,#24584,#24585,#24586,#24587,#24588,#24589,#24590,#24591,
#24592,#24593,#24594,#24595,#24596,#24597,#24598,#24599,#24600,#24601,#24602,
#24603,#24604,#24605,#24606,#24607,#24608,#24609,#24610,#24611,#24612,#24613),
 .UNSPECIFIED.,.F.,.F.,(4,3,3,3,3,3,3,3,3,3,3,3,3,3,3,3,4),(656.592864600441,
656.688389105084,656.784357962551,656.880910721209,656.958763939773,657.040980201405,
657.123093290724,657.205124599147,657.290121131882,657.372060131357,657.453986833998,
657.535920394155,657.617879970969,657.69992876607,657.782030759269,657.864248468546,
657.885096861028),.UNSPECIFIED.);
#311=B_SPLINE_CURVE_WITH_KNOTS('',3,(#24617,#24618,#24619,#24620,#24621,
#24622,#24623,#24624,#24625,#24626,#24627,#24628),.UNSPECIFIED.,.F.,.F.,
(4,2,2,2,2,4),(1.19797002426947E-5,0.013145050983649,0.0211198128453241,
0.0241087294059435,0.0252409894393879,0.0262779747017448),.UNSPECIFIED.);
#312=B_SPLINE_CURVE_WITH_KNOTS('',3,(#24630,#24631,#24632,#24633,#24634,
#24635,#24636,#24637,#24638,#24639,#24640,#24641,#24642,#24643,#24644,#24645,
#24646,#24647,#24648,#24649,#24650,#24651,#24652,#24653,#24654,#24655,#24656,
#24657,#24658,#24659,#24660,#24661,#24662,#24663,#24664,#24665,#24666,#24667,
#24668,#24669,#24670,#24671,#24672,#24673,#24674,#24675,#24676,#24677,#24678,
#24679,#24680,#24681,#24682,#24683,#24684,#24685,#24686,#24687,#24688,#24689,
#24690,#24691,#24692,#24693,#24694,#24695,#24696,#24697,#24698,#24699,#24700,
#24701,#24702,#24703,#24704,#24705,#24706,#24707,#24708,#24709,#24710,#24711,
#24712,#24713,#24714,#24715,#24716,#24717,#24718,#24719,#24720,#24721,#24722,
#24723,#24724,#24725,#24726,#24727,#24728,#24729,#24730,#24731,#24732,#24733,
#24734,#24735,#24736,#24737,#24738,#24739,#24740,#24741,#24742,#24743,#24744,
#24745,#24746,#24747,#24748,#24749,#24750,#24751,#24752,#24753,#24754,#24755,
#24756,#24757,#24758,#24759,#24760,#24761,#24762,#24763,#24764,#24765,#24766,
#24767,#24768,#24769,#24770,#24771,#24772,#24773,#24774,#24775,#24776,#24777,
#24778,#24779,#24780,#24781,#24782,#24783,#24784,#24785,#24786,#24787,#24788,
#24789,#24790,#24791,#24792,#24793,#24794,#24795,#24796,#24797,#24798,#24799,
#24800,#24801,#24802,#24803,#24804,#24805,#24806,#24807,#24808,#24809,#24810,
#24811,#24812,#24813,#24814,#24815,#24816,#24817,#24818,#24819,#24820,#24821,
#24822,#24823,#24824,#24825,#24826,#24827,#24828,#24829,#24830,#24831,#24832,
#24833,#24834,#24835,#24836,#24837,#24838,#24839,#24840,#24841,#24842,#24843,
#24844,#24845,#24846,#24847,#24848,#24849,#24850,#24851,#24852,#24853,#24854,
#24855),.UNSPECIFIED.,.F.,.F.,(4,3,3,3,3,3,3,3,3,3,3,3,3,3,3,3,3,3,3,3,
3,3,3,3,3,3,3,3,3,3,3,3,3,3,3,3,3,3,3,3,3,3,3,3,3,3,3,3,3,3,3,3,3,3,3,3,
3,3,3,3,3,3,3,3,3,3,3,3,3,3,3,3,3,3,3,4),(650.309679293274,650.406233622475,
650.503311876305,650.601029081094,650.652314781296,650.735957910548,650.819497813811,
650.902954720291,650.986348786315,651.069707913455,651.153049944518,651.236393038061,
651.319755349584,651.403207547017,651.486704935601,651.570337997441,651.651298283496,
651.735161305775,651.81892086122,651.902596957108,651.986209529205,652.069785368016,
652.153342989141,652.236900352737,652.320475414888,652.404136776,652.487841704887,
652.571677452732,652.650281785695,652.734167640835,652.817951928372,652.901654602967,
652.985295549612,653.068902358886,653.152492521882,653.236083957684,653.3196945823,
653.403393630556,653.487137462525,653.571013769074,653.649265287894,653.732279311988,
653.815189413488,653.898016396369,653.980780982524,654.06421445847,654.146931315586,
654.229651530997,654.312393764629,654.396357520995,654.479246476447,654.56374763327,
654.648248790093,654.733255939278,654.818152347384,654.902956529104,654.987686922183,
655.072360395319,655.157002738458,655.24163054438,655.326260392304,655.410945674027,
655.495658757372,655.580466457639,655.647232292292,655.731132100585,655.814963062839,
655.898744863005,655.982495865332,656.066255250149,656.146724043392,656.24281480375,
656.339248498341,656.43578222174,656.532319067256,656.592864600267),
 .UNSPECIFIED.);
#313=B_SPLINE_CURVE_WITH_KNOTS('',3,(#24857,#24858,#24859,#24860,#24861,
#24862,#24863,#24864,#24865,#24866,#24867,#24868,#24869,#24870,#24871,#24872,
#24873,#24874,#24875,#24876,#24877,#24878,#24879,#24880,#24881,#24882,#24883,
#24884,#24885,#24886,#24887,#24888,#24889,#24890,#24891,#24892,#24893,#24894,
#24895,#24896,#24897,#24898,#24899,#24900,#24901,#24902,#24903,#24904,#24905,
#24906,#24907,#24908,#24909,#24910,#24911,#24912,#24913,#24914,#24915,#24916,
#24917,#24918,#24919,#24920,#24921,#24922,#24923,#24924,#24925,#24926,#24927,
#24928,#24929,#24930,#24931,#24932,#24933,#24934,#24935,#24936,#24937,#24938,
#24939,#24940,#24941,#24942,#24943,#24944,#24945,#24946,#24947,#24948,#24949,
#24950,#24951,#24952,#24953,#24954,#24955,#24956,#24957,#24958,#24959,#24960,
#24961,#24962,#24963,#24964,#24965,#24966,#24967,#24968,#24969,#24970,#24971,
#24972,#24973,#24974,#24975,#24976,#24977,#24978,#24979,#24980,#24981,#24982,
#24983,#24984,#24985,#24986,#24987,#24988,#24989,#24990,#24991,#24992,#24993,
#24994,#24995,#24996,#24997,#24998,#24999,#25000,#25001,#25002,#25003,#25004,
#25005,#25006,#25007,#25008,#25009,#25010,#25011,#25012,#25013,#25014,#25015,
#25016,#25017,#25018,#25019,#25020,#25021,#25022,#25023,#25024,#25025,#25026,
#25027,#25028,#25029,#25030,#25031,#25032,#25033,#25034,#25035,#25036,#25037,
#25038,#25039,#25040,#25041,#25042,#25043,#25044,#25045,#25046,#25047,#25048,
#25049,#25050,#25051,#25052,#25053,#25054,#25055,#25056,#25057,#25058,#25059,
#25060,#25061,#25062,#25063,#25064,#25065,#25066,#25067,#25068,#25069,#25070,
#25071,#25072,#25073,#25074,#25075,#25076,#25077,#25078,#25079,#25080,#25081,
#25082,#25083,#25084,#25085),.UNSPECIFIED.,.F.,.F.,(4,3,3,3,3,3,3,3,3,3,
3,3,3,3,3,3,3,3,3,3,3,3,3,3,3,3,3,3,3,3,3,3,3,3,3,3,3,3,3,3,3,3,3,3,3,3,
3,3,3,3,3,3,3,3,3,3,3,3,3,3,3,3,3,3,3,3,3,3,3,3,3,3,3,3,3,3,4),(644.026493985908,
644.110429528115,644.194368280084,644.278327608105,644.362324888035,644.446429579001,
644.530594543763,644.614894173054,644.658413768101,644.742158268002,644.825799710795,
644.909358221521,644.992853853304,645.076314136271,645.159757062121,645.243200697321,
645.326663104971,645.410214134101,645.493809825012,645.577539290062,645.657397270301,
645.741145449423,645.824790560255,645.908352724234,645.991851990903,646.075315868383,
646.158762363715,646.242209540124,646.325675457446,646.409229926937,646.492829025913,
646.576561809727,646.6563807725,646.740132511195,646.823781225058,646.907347031259,
646.990849975135,647.074317569564,647.15776780545,647.241218742351,647.32468843645,
647.408246686763,647.491849574731,647.575586122846,647.655364274699,647.739095628126,
647.8227239079,647.906269252696,647.989751729165,648.073198918806,648.156628790793,
648.240059423682,648.323508892707,648.407047156379,648.490630155869,648.5743471839,
648.654347776898,648.738108112563,648.821765319466,648.905339507456,648.988850714513,
649.072326364678,649.155784529117,649.23924326054,649.322720608183,649.406286247826,
649.489896392915,649.573639900747,649.653331279097,649.737173540448,649.820914313398,
649.904571670437,649.988163622653,650.071711157331,650.155231024935,650.238761690986,
650.309679293087),.UNSPECIFIED.);
#314=B_SPLINE_CURVE_WITH_KNOTS('',3,(#25087,#25088,#25089,#25090,#25091,
#25092,#25093,#25094,#25095,#25096,#25097,#25098,#25099,#25100,#25101,#25102,
#25103,#25104,#25105,#25106,#25107,#25108,#25109,#25110,#25111,#25112,#25113,
#25114,#25115,#25116,#25117,#25118,#25119,#25120,#25121,#25122,#25123,#25124,
#25125,#25126,#25127,#25128,#25129,#25130,#25131,#25132,#25133,#25134,#25135,
#25136,#25137,#25138,#25139,#25140,#25141,#25142,#25143,#25144,#25145,#25146,
#25147,#25148,#25149,#25150,#25151,#25152,#25153,#25154,#25155,#25156,#25157,
#25158,#25159,#25160,#25161,#25162,#25163,#25164,#25165,#25166,#25167,#25168,
#25169,#25170,#25171,#25172,#25173,#25174,#25175,#25176,#25177,#25178,#25179,
#25180,#25181,#25182,#25183,#25184,#25185,#25186,#25187,#25188,#25189,#25190,
#25191,#25192,#25193,#25194,#25195,#25196,#25197,#25198,#25199,#25200,#25201,
#25202,#25203,#25204,#25205,#25206,#25207,#25208,#25209,#25210,#25211,#25212,
#25213,#25214,#25215,#25216,#25217,#25218,#25219,#25220,#25221,#25222,#25223,
#25224,#25225,#25226,#25227,#25228,#25229,#25230,#25231,#25232,#25233,#25234,
#25235,#25236,#25237,#25238,#25239,#25240,#25241,#25242,#25243,#25244,#25245,
#25246,#25247,#25248,#25249,#25250,#25251,#25252,#25253,#25254,#25255,#25256,
#25257,#25258,#25259,#25260,#25261,#25262,#25263,#25264,#25265,#25266,#25267,
#25268,#25269,#25270,#25271,#25272,#25273,#25274,#25275,#25276,#25277,#25278,
#25279,#25280,#25281,#25282,#25283,#25284,#25285,#25286,#25287,#25288,#25289,
#25290,#25291,#25292,#25293,#25294,#25295,#25296,#25297,#25298,#25299,#25300,
#25301,#25302,#25303,#25304,#25305,#25306,#25307,#25308,#25309,#25310,#25311,
#25312),.UNSPECIFIED.,.F.,.F.,(4,3,3,3,3,3,3,3,3,3,3,3,3,3,3,3,3,3,3,3,
3,3,3,3,3,3,3,3,3,3,3,3,3,3,3,3,3,3,3,3,3,3,3,3,3,3,3,3,3,3,3,3,3,3,3,3,
3,3,3,3,3,3,3,3,3,3,3,3,3,3,3,3,3,3,3,4),(637.743308678856,637.826129299476,
637.908853701098,637.991502818153,638.075629060247,638.158199624338,638.240762291769,
638.323335862189,638.408630085369,638.491326062699,638.577919408802,638.664512754906,
638.748259443697,638.831903076827,638.915463777078,638.998961595333,639.08242405252,
639.16586914484,639.249314936754,639.332779489347,639.416332632809,639.499930424729,
639.583661946882,639.663496257106,639.747242994695,639.830886676261,639.914447424539,
639.99794529037,640.081407794284,640.164852932809,640.248298770366,640.331763367998,
640.415316555299,640.498914390473,640.58264595445,640.662479759305,640.746226638579,
640.829870462765,640.913431354442,640.996929364293,641.080392012657,641.163837295875,
641.247283278227,641.330748020618,641.414301351801,641.497899330607,641.581631036332,
641.661463261504,641.745209677247,641.828853037284,641.912413464676,641.995911010585,
642.079373197151,642.162818019937,642.246263543652,642.329727829631,642.413280710478,
642.496878241542,642.580609508471,642.660446763703,642.744193621587,642.82783742169,
642.911398286652,642.994896267213,643.078358882516,643.161804130387,643.245250075151,
643.328714777759,643.412268065945,643.495865999938,643.57959765823,643.659430265902,
643.754828788849,643.849906489669,643.94436720848,644.026493985711),
 .UNSPECIFIED.);
#315=B_SPLINE_CURVE_WITH_KNOTS('',3,(#25314,#25315,#25316,#25317,#25318,
#25319,#25320,#25321,#25322,#25323,#25324,#25325,#25326,#25327,#25328,#25329,
#25330,#25331,#25332,#25333,#25334,#25335,#25336,#25337,#25338,#25339,#25340,
#25341,#25342,#25343,#25344,#25345,#25346,#25347,#25348,#25349,#25350,#25351,
#25352,#25353,#25354,#25355,#25356,#25357,#25358,#25359,#25360,#25361,#25362,
#25363,#25364,#25365,#25366,#25367,#25368,#25369,#25370,#25371,#25372,#25373,
#25374,#25375,#25376,#25377,#25378,#25379,#25380,#25381,#25382,#25383,#25384,
#25385,#25386,#25387,#25388,#25389,#25390,#25391,#25392,#25393,#25394,#25395,
#25396,#25397,#25398,#25399,#25400,#25401,#25402,#25403,#25404,#25405,#25406,
#25407,#25408,#25409,#25410,#25411,#25412,#25413,#25414,#25415,#25416,#25417,
#25418,#25419,#25420,#25421,#25422,#25423,#25424,#25425,#25426,#25427,#25428,
#25429,#25430,#25431,#25432,#25433,#25434,#25435,#25436,#25437,#25438,#25439,
#25440,#25441,#25442,#25443,#25444,#25445,#25446,#25447,#25448,#25449,#25450,
#25451,#25452,#25453,#25454,#25455,#25456,#25457,#25458,#25459,#25460,#25461,
#25462,#25463,#25464,#25465,#25466,#25467,#25468,#25469,#25470,#25471,#25472,
#25473,#25474,#25475,#25476,#25477,#25478,#25479,#25480,#25481,#25482,#25483,
#25484,#25485,#25486,#25487,#25488,#25489,#25490,#25491,#25492,#25493,#25494,
#25495,#25496,#25497,#25498,#25499,#25500,#25501,#25502,#25503,#25504,#25505,
#25506,#25507,#25508,#25509,#25510,#25511,#25512,#25513,#25514,#25515,#25516,
#25517,#25518,#25519,#25520,#25521,#25522,#25523,#25524,#25525,#25526,#25527,
#25528,#25529,#25530,#25531,#25532,#25533,#25534,#25535,#25536,#25537,#25538,
#25539),.UNSPECIFIED.,.F.,.F.,(4,3,3,3,3,3,3,3,3,3,3,3,3,3,3,3,3,3,3,3,
3,3,3,3,3,3,3,3,3,3,3,3,3,3,3,3,3,3,3,3,3,3,3,3,3,3,3,3,3,3,3,3,3,3,3,3,
3,3,3,3,3,3,3,3,3,3,3,3,3,3,3,3,3,3,3,4),(631.460123371549,631.576925539142,
631.671628239512,631.755374972795,631.839018650393,631.922579395042,632.006077257582,
632.089539758726,632.172984894798,632.256430730218,632.339895326032,632.423448512022,
632.50704634616,632.590777909577,632.670611741711,632.754358473643,632.83800214989,
632.921562893191,633.005060754385,633.088523254193,633.171968388935,633.255414223033,
633.338878817533,633.42243200223,633.506029835084,633.589761397246,633.669595243911,
633.753341976116,633.836985652626,633.920546396179,634.004044257616,634.08750675765,
634.170951892609,634.254397726913,634.337862321609,634.421415506485,634.505013339509,
634.588744901824,634.66857874611,634.752325482574,634.835969163363,634.919529911209,
635.003027776947,635.086490281281,635.169935420539,635.253381259137,635.336845858117,
635.420399047238,635.503996884493,635.587728450971,635.667562248309,635.751308975095,
635.834952646204,635.918513384376,636.002011240459,636.085473735198,636.168918864898,
636.252364693986,636.335829283511,636.419382463317,636.50298029132,636.586711848743,
636.666545750508,636.750292481885,636.833936157522,636.917496900159,637.000994760638,
637.084457259654,637.167902393558,637.251348226774,637.334812820347,637.418366004053,
637.501963835881,637.585695396965,637.665529252707,637.743308678728),
 .UNSPECIFIED.);
#316=B_SPLINE_CURVE_WITH_KNOTS('',3,(#25541,#25542,#25543,#25544,#25545,
#25546,#25547,#25548,#25549,#25550,#25551,#25552,#25553,#25554,#25555,#25556,
#25557,#25558,#25559,#25560,#25561,#25562,#25563,#25564,#25565,#25566,#25567,
#25568,#25569,#25570,#25571,#25572,#25573,#25574,#25575,#25576,#25577,#25578,
#25579,#25580,#25581,#25582,#25583,#25584,#25585,#25586,#25587,#25588,#25589,
#25590,#25591,#25592,#25593,#25594,#25595,#25596,#25597,#25598,#25599,#25600,
#25601,#25602,#25603,#25604,#25605,#25606,#25607,#25608,#25609,#25610,#25611,
#25612,#25613,#25614,#25615,#25616,#25617,#25618,#25619,#25620,#25621,#25622,
#25623,#25624,#25625,#25626,#25627,#25628,#25629,#25630,#25631,#25632,#25633,
#25634,#25635,#25636,#25637,#25638,#25639,#25640,#25641,#25642,#25643,#25644,
#25645,#25646,#25647,#25648,#25649,#25650,#25651,#25652,#25653,#25654,#25655,
#25656,#25657,#25658,#25659,#25660,#25661,#25662,#25663,#25664,#25665,#25666,
#25667,#25668,#25669,#25670,#25671,#25672,#25673,#25674,#25675,#25676,#25677,
#25678,#25679,#25680,#25681,#25682,#25683,#25684,#25685,#25686,#25687,#25688,
#25689,#25690,#25691,#25692,#25693,#25694,#25695,#25696,#25697,#25698,#25699,
#25700,#25701,#25702,#25703,#25704,#25705,#25706,#25707,#25708,#25709,#25710,
#25711,#25712,#25713,#25714,#25715,#25716,#25717,#25718,#25719,#25720,#25721,
#25722,#25723,#25724,#25725,#25726,#25727,#25728,#25729,#25730,#25731,#25732,
#25733,#25734,#25735,#25736,#25737,#25738,#25739,#25740,#25741,#25742,#25743,
#25744,#25745,#25746,#25747,#25748,#25749,#25750,#25751,#25752,#25753,#25754,
#25755,#25756,#25757,#25758,#25759,#25760,#25761,#25762,#25763,#25764,#25765,
#25766,#25767,#25768,#25769),.UNSPECIFIED.,.F.,.F.,(4,3,3,3,3,3,3,3,3,3,
3,3,3,3,3,3,3,3,3,3,3,3,3,3,3,3,3,3,3,3,3,3,3,3,3,3,3,3,3,3,3,3,3,3,3,3,
3,3,3,3,3,3,3,3,3,3,3,3,3,3,3,3,3,3,3,3,3,3,3,3,3,3,3,3,3,3,4),(625.176938064369,
625.264298823443,625.351772685274,625.439451113209,625.52723733009,625.615223939944,
625.677727226317,625.761473959032,625.845117636061,625.92867838014,626.01217624211,
626.095638742685,626.179083878191,626.262529713046,626.345994308297,626.429547493731,
626.513145327317,626.596876890191,626.676710728516,626.760457461207,626.844101138212,
626.927661882267,627.011159744213,627.094622244765,627.178067380246,627.261513215078,
627.344977810306,627.428530995718,627.51212882928,627.595860392133,627.675694230716,
627.759440963395,627.843084640387,627.92664538443,628.010143246363,628.093605746902,
628.17705088237,628.260496717189,628.343961312403,628.427514497801,628.51111233135,
628.594843894188,628.674677732915,628.758424465705,628.842068142808,628.925628886963,
629.009126749007,629.092589249658,629.176034385237,629.259480220167,629.342944815492,
629.426498000999,629.510095834656,629.593827397601,629.673661235114,629.75740796772,
629.84105164464,629.924612388612,630.008110250474,630.091572750943,630.175017886342,
630.258463721093,630.34192831624,630.425481501573,630.509079335057,630.592810897833,
630.672644737313,630.755224498922,630.837700764635,630.920082197797,631.00241054239,
631.084704824653,631.16698403934,631.249295852495,631.331625039562,631.414029479979,
631.460123371422),.UNSPECIFIED.);
#317=B_SPLINE_CURVE_WITH_KNOTS('',3,(#25771,#25772,#25773,#25774,#25775,
#25776,#25777,#25778,#25779,#25780,#25781,#25782,#25783,#25784,#25785,#25786,
#25787,#25788,#25789,#25790,#25791,#25792,#25793,#25794,#25795,#25796,#25797,
#25798,#25799,#25800,#25801,#25802,#25803,#25804,#25805,#25806,#25807,#25808,
#25809,#25810,#25811,#25812,#25813,#25814,#25815,#25816,#25817,#25818,#25819,
#25820,#25821,#25822,#25823,#25824,#25825,#25826,#25827,#25828,#25829,#25830,
#25831,#25832,#25833,#25834,#25835,#25836,#25837,#25838,#25839,#25840,#25841,
#25842,#25843,#25844,#25845,#25846,#25847,#25848,#25849,#25850,#25851,#25852,
#25853,#25854,#25855,#25856,#25857,#25858,#25859,#25860,#25861,#25862,#25863,
#25864,#25865,#25866,#25867,#25868,#25869,#25870,#25871,#25872,#25873,#25874,
#25875,#25876,#25877,#25878,#25879,#25880,#25881,#25882,#25883,#25884,#25885,
#25886,#25887,#25888,#25889,#25890,#25891,#25892,#25893,#25894,#25895,#25896,
#25897,#25898,#25899,#25900,#25901,#25902,#25903,#25904,#25905,#25906,#25907,
#25908,#25909,#25910,#25911,#25912,#25913,#25914,#25915,#25916,#25917,#25918,
#25919,#25920,#25921,#25922,#25923,#25924,#25925,#25926,#25927,#25928,#25929,
#25930,#25931,#25932,#25933,#25934,#25935,#25936,#25937,#25938,#25939,#25940,
#25941,#25942,#25943,#25944,#25945,#25946,#25947,#25948,#25949,#25950,#25951,
#25952,#25953,#25954,#25955,#25956,#25957,#25958,#25959,#25960,#25961,#25962,
#25963,#25964,#25965,#25966,#25967,#25968,#25969,#25970,#25971,#25972,#25973,
#25974,#25975,#25976,#25977,#25978,#25979,#25980,#25981,#25982,#25983,#25984,
#25985,#25986,#25987,#25988,#25989,#25990,#25991,#25992,#25993,#25994,#25995,
#25996,#25997,#25998,#25999),.UNSPECIFIED.,.F.,.F.,(4,3,3,3,3,3,3,3,3,3,
3,3,3,3,3,3,3,3,3,3,3,3,3,3,3,3,3,3,3,3,3,3,3,3,3,3,3,3,3,3,3,3,3,3,3,3,
3,3,3,3,3,3,3,3,3,3,3,3,3,3,3,3,3,3,3,3,3,3,3,3,3,3,3,3,3,3,4),(618.893752757332,
618.976157287315,619.058495611027,619.140795072643,619.223076019747,619.305357440849,
619.387658322558,619.47004462904,619.552477968653,619.63503337098,619.683826213122,
619.767572945824,619.851216622841,619.934777366907,620.018275228864,620.101737729427,
620.18518286492,620.268628699763,620.352093295002,620.435646480424,620.519244313997,
620.602975876859,620.682809715321,620.766556448023,620.850200125039,620.933760869105,
621.017258731062,621.100721231624,621.184166367117,621.267612201959,621.351076797197,
621.434629982619,621.518227816192,621.601959379054,621.681793217521,621.765539950222,
621.849183627237,621.932744371303,622.016242233259,622.099704733821,622.183149869312,
622.266595704154,622.350060299391,622.433613484812,622.517211318384,622.600942881245,
622.68077671972,622.764523452424,622.848167129442,622.93172787351,623.015225735468,
623.098688236033,623.182133371527,623.265579206372,623.349043801612,623.432596987036,
623.51619482061,623.599926383474,623.679760221919,623.76350695462,623.847150631634,
623.930711375699,624.014209237655,624.097671738216,624.181116873707,624.264562708549,
624.348027303786,624.431580489207,624.515178322779,624.59890988564,624.678743724118,
624.766852498131,624.854808775082,624.942563062619,625.030197091654,625.117672902589,
625.176938064065),.UNSPECIFIED.);
#318=B_SPLINE_CURVE_WITH_KNOTS('',3,(#26001,#26002,#26003,#26004,#26005,
#26006,#26007,#26008,#26009,#26010,#26011,#26012,#26013,#26014,#26015,#26016,
#26017,#26018,#26019,#26020,#26021,#26022,#26023,#26024,#26025,#26026,#26027,
#26028,#26029,#26030,#26031,#26032,#26033,#26034,#26035,#26036,#26037,#26038,
#26039,#26040,#26041,#26042,#26043,#26044,#26045,#26046,#26047,#26048,#26049,
#26050,#26051,#26052,#26053,#26054,#26055,#26056,#26057,#26058,#26059,#26060,
#26061,#26062,#26063,#26064,#26065,#26066,#26067,#26068,#26069,#26070,#26071,
#26072,#26073,#26074,#26075,#26076,#26077,#26078,#26079,#26080,#26081,#26082,
#26083,#26084,#26085,#26086,#26087,#26088,#26089,#26090,#26091,#26092,#26093,
#26094,#26095,#26096,#26097,#26098,#26099,#26100,#26101,#26102,#26103,#26104,
#26105,#26106,#26107,#26108,#26109,#26110,#26111,#26112,#26113,#26114,#26115,
#26116,#26117,#26118,#26119,#26120,#26121,#26122,#26123,#26124,#26125,#26126,
#26127,#26128,#26129,#26130,#26131,#26132,#26133,#26134,#26135,#26136,#26137,
#26138,#26139,#26140,#26141,#26142,#26143,#26144,#26145,#26146,#26147,#26148,
#26149,#26150,#26151,#26152,#26153,#26154,#26155,#26156,#26157,#26158,#26159,
#26160,#26161,#26162,#26163,#26164,#26165,#26166,#26167,#26168,#26169,#26170,
#26171,#26172,#26173,#26174,#26175,#26176,#26177,#26178,#26179,#26180,#26181,
#26182,#26183,#26184,#26185,#26186,#26187,#26188,#26189,#26190,#26191,#26192,
#26193,#26194,#26195,#26196,#26197,#26198,#26199,#26200,#26201,#26202,#26203,
#26204,#26205,#26206,#26207,#26208,#26209,#26210,#26211,#26212,#26213,#26214,
#26215,#26216,#26217,#26218,#26219,#26220,#26221,#26222,#26223,#26224,#26225,
#26226),.UNSPECIFIED.,.F.,.F.,(4,3,3,3,3,3,3,3,3,3,3,3,3,3,3,3,3,3,3,3,
3,3,3,3,3,3,3,3,3,3,3,3,3,3,3,3,3,3,3,3,3,3,3,3,3,3,3,3,3,3,3,3,3,3,3,3,
3,3,3,3,3,3,3,3,3,3,3,3,3,3,3,3,3,3,3,4),(612.61056745001,612.690941697728,
612.77468843043,612.858332107446,612.941892851513,613.02539071347,613.108853214032,
613.192298349525,613.275744184368,613.359208779606,613.442761965028,613.5263597986,
613.610091361462,613.689925199927,613.773671932629,613.857315609645,613.940876353711,
614.024374215668,614.10783671623,614.191281851722,614.274727686565,614.358192281803,
614.441745467225,614.525343300797,614.609074863659,614.688908702126,614.772655434828,
614.856299111844,614.939859855911,615.023357717868,615.10682021843,615.190265353923,
615.273711188766,615.357175784004,615.440728969426,615.524326802999,615.608058365861,
615.687892204326,615.771638937028,615.855282614044,615.938843358111,616.022341220067,
616.10580372063,616.189248856123,616.272694690965,616.356159286204,616.439712471626,
616.523310305198,616.60704186806,616.686875706525,616.770622439227,616.854266116243,
616.937826860309,617.021324722265,617.104787222828,617.18823235832,617.271678193163,
617.355142788401,617.438695973823,617.522293807395,617.606025370257,617.685859208724,
617.769605941426,617.853249618442,617.936810362508,618.020308224465,618.103770725028,
618.18721586052,618.270661695363,618.354126290601,618.437679476023,618.521277309595,
618.605008872457,618.684842710923,618.802340309998,618.893752757189),
 .UNSPECIFIED.);
#319=B_SPLINE_CURVE_WITH_KNOTS('',3,(#26228,#26229,#26230,#26231,#26232,
#26233,#26234,#26235,#26236,#26237,#26238,#26239,#26240,#26241,#26242,#26243,
#26244,#26245,#26246,#26247,#26248,#26249,#26250,#26251,#26252,#26253,#26254,
#26255,#26256,#26257,#26258,#26259,#26260,#26261,#26262,#26263,#26264,#26265,
#26266,#26267,#26268,#26269,#26270,#26271,#26272,#26273,#26274,#26275,#26276,
#26277,#26278,#26279,#26280,#26281,#26282,#26283,#26284,#26285,#26286,#26287,
#26288,#26289,#26290,#26291,#26292,#26293,#26294,#26295,#26296,#26297,#26298,
#26299,#26300,#26301,#26302,#26303,#26304,#26305,#26306,#26307,#26308,#26309,
#26310,#26311,#26312,#26313,#26314,#26315,#26316,#26317,#26318,#26319,#26320,
#26321,#26322,#26323,#26324,#26325,#26326,#26327,#26328,#26329,#26330,#26331,
#26332,#26333,#26334,#26335,#26336,#26337,#26338,#26339,#26340,#26341,#26342,
#26343,#26344,#26345,#26346,#26347,#26348,#26349,#26350,#26351,#26352,#26353,
#26354,#26355,#26356,#26357,#26358,#26359,#26360,#26361,#26362,#26363,#26364,
#26365,#26366,#26367,#26368,#26369,#26370,#26371,#26372,#26373,#26374,#26375,
#26376,#26377,#26378,#26379,#26380,#26381,#26382,#26383,#26384,#26385,#26386,
#26387,#26388,#26389,#26390,#26391,#26392,#26393,#26394,#26395,#26396,#26397,
#26398,#26399,#26400,#26401,#26402,#26403,#26404,#26405,#26406,#26407,#26408,
#26409,#26410,#26411,#26412,#26413,#26414,#26415,#26416,#26417,#26418,#26419,
#26420,#26421,#26422,#26423,#26424,#26425,#26426,#26427,#26428,#26429,#26430,
#26431,#26432,#26433,#26434,#26435,#26436,#26437,#26438,#26439,#26440,#26441,
#26442,#26443,#26444,#26445,#26446,#26447,#26448,#26449,#26450,#26451,#26452,
#26453),.UNSPECIFIED.,.F.,.F.,(4,3,3,3,3,3,3,3,3,3,3,3,3,3,3,3,3,3,3,3,
3,3,3,3,3,3,3,3,3,3,3,3,3,3,3,3,3,3,3,3,3,3,3,3,3,3,3,3,3,3,3,3,3,3,3,3,
3,3,3,3,3,3,3,3,3,3,3,3,3,3,3,3,3,3,3,4),(606.32738214283,606.42167540976,
606.516348323315,606.611552029141,606.697040684533,606.780787417234,606.86443109425,
606.947991838316,607.031489700272,607.114952200834,607.198397336326,607.281843171168,
607.365307766405,607.448860951827,607.532458785399,607.61619034826,607.696024186732,
607.779770919434,607.86341459645,607.946975340516,608.030473202473,608.113935703035,
608.197380838527,608.28082667337,608.364291268608,608.44784445403,608.531442287603,
608.615173850464,608.695007688931,608.778754421633,608.86239809865,608.945958842717,
609.029456704674,609.112919205237,609.196364340729,609.279810175573,609.363274770811,
609.446827956234,609.530425789806,609.614157352669,609.693991191131,609.777737923833,
609.861381600849,609.944942344915,610.028440206872,610.111902707434,610.195347842926,
610.278793677769,610.362258273007,610.445811458429,610.529409292001,610.613140854863,
610.69297469333,610.776721426032,610.860365103047,610.943925847114,611.02742370907,
611.110886209633,611.194331345125,611.277777179968,611.361241775205,611.444794960627,
611.528392794199,611.612124357061,611.691958195529,611.774790308619,611.857520078192,
611.940168482096,612.023968353069,612.106523168124,612.189064409159,612.271610890298,
612.356350030193,612.439004220829,612.524785835355,612.61056744988),
 .UNSPECIFIED.);
#320=B_SPLINE_CURVE_WITH_KNOTS('',3,(#26455,#26456,#26457,#26458,#26459,
#26460,#26461,#26462,#26463,#26464),.UNSPECIFIED.,.F.,.F.,(4,1,1,1,1,1,
1,4),(600.044196835651,600.703139671338,601.702123173537,602.701106675736,
603.700090177936,604.699073680135,605.698057182334,606.32738214283),
 .UNSPECIFIED.);
#321=B_SPLINE_CURVE_WITH_KNOTS('',3,(#26466,#26467,#26468,#26469,#26470,
#26471,#26472,#26473,#26474,#26475,#26476,#26477,#26478,#26479,#26480,#26481,
#26482,#26483,#26484,#26485,#26486,#26487,#26488,#26489,#26490,#26491,#26492,
#26493,#26494,#26495,#26496,#26497,#26498,#26499,#26500,#26501,#26502,#26503,
#26504,#26505,#26506,#26507,#26508,#26509,#26510,#26511,#26512,#26513,#26514,
#26515,#26516,#26517,#26518,#26519,#26520,#26521,#26522,#26523,#26524,#26525,
#26526,#26527,#26528,#26529,#26530,#26531,#26532,#26533,#26534,#26535,#26536,
#26537,#26538,#26539,#26540,#26541,#26542,#26543,#26544,#26545,#26546,#26547,
#26548,#26549,#26550,#26551,#26552,#26553,#26554,#26555,#26556,#26557,#26558,
#26559,#26560,#26561,#26562,#26563,#26564,#26565,#26566,#26567,#26568,#26569,
#26570,#26571,#26572,#26573,#26574,#26575,#26576,#26577,#26578,#26579,#26580,
#26581,#26582,#26583,#26584,#26585,#26586,#26587,#26588,#26589,#26590,#26591,
#26592,#26593,#26594,#26595,#26596,#26597,#26598,#26599,#26600,#26601,#26602,
#26603,#26604,#26605,#26606,#26607,#26608,#26609,#26610,#26611,#26612,#26613,
#26614,#26615,#26616,#26617,#26618,#26619,#26620,#26621,#26622,#26623,#26624,
#26625,#26626,#26627,#26628,#26629,#26630,#26631,#26632,#26633,#26634,#26635,
#26636,#26637,#26638,#26639,#26640,#26641,#26642,#26643,#26644,#26645,#26646,
#26647,#26648,#26649,#26650,#26651,#26652,#26653,#26654,#26655,#26656,#26657,
#26658,#26659,#26660,#26661,#26662,#26663,#26664,#26665,#26666,#26667,#26668,
#26669,#26670,#26671,#26672,#26673,#26674,#26675,#26676,#26677,#26678,#26679,
#26680,#26681,#26682,#26683,#26684,#26685,#26686,#26687,#26688,#26689,#26690,
#26691,#26692,#26693,#26694),.UNSPECIFIED.,.F.,.F.,(4,3,3,3,3,3,3,3,3,3,
3,3,3,3,3,3,3,3,3,3,3,3,3,3,3,3,3,3,3,3,3,3,3,3,3,3,3,3,3,3,3,3,3,3,3,3,
3,3,3,3,3,3,3,3,3,3,3,3,3,3,3,3,3,3,3,3,3,3,3,3,3,3,3,3,3,3,4),(593.761011528671,
593.844095681974,593.927080015812,594.009985274574,594.092832125752,594.175649970121,
594.258455628379,594.341267723089,594.424104878142,594.507031806383,594.590010108476,
594.673108607956,594.709238658143,594.792985390845,594.876629067861,594.960189811927,
595.043687673884,595.127150174446,595.210595309938,595.294041144781,595.377505740019,
595.461058925441,595.544656759013,595.628388321875,595.708222160342,595.791968893044,
595.87561257006,595.959173314127,596.042671176084,596.126133676646,596.209578812139,
596.293024646982,596.37648924222,596.460042427641,596.543640261214,596.627371824076,
596.707205662541,596.790952395243,596.874596072259,596.958156816326,597.041654678282,
597.125117178845,597.208562314338,597.29200814918,597.375472744418,597.45902592984,
597.542623763413,597.626355326275,597.706189164741,597.789935897443,597.873579574459,
597.957140318525,598.040638180482,598.124100681045,598.207545816537,598.29099165138,
598.374456246618,598.45800943204,598.541607265612,598.625338828474,598.70517266694,
598.788919399642,598.872563076658,598.956123820724,599.03962168268,599.123084183243,
599.206529318735,599.289975153578,599.373439748816,599.456992934238,599.54059076781,
599.624322330672,599.704156169139,599.801883478083,599.89918974496,599.995709704988,
600.044196835651),.UNSPECIFIED.);
#322=B_SPLINE_CURVE_WITH_KNOTS('',3,(#26696,#26697,#26698,#26699,#26700,
#26701,#26702,#26703,#26704,#26705,#26706,#26707,#26708,#26709,#26710,#26711,
#26712,#26713,#26714,#26715,#26716,#26717,#26718,#26719,#26720,#26721,#26722,
#26723,#26724,#26725,#26726,#26727,#26728,#26729,#26730,#26731,#26732,#26733,
#26734,#26735,#26736,#26737,#26738,#26739,#26740,#26741,#26742,#26743,#26744,
#26745,#26746,#26747,#26748,#26749,#26750,#26751,#26752,#26753,#26754,#26755,
#26756,#26757,#26758,#26759,#26760,#26761,#26762,#26763,#26764,#26765,#26766,
#26767,#26768,#26769,#26770,#26771,#26772,#26773,#26774,#26775,#26776,#26777,
#26778,#26779,#26780,#26781,#26782,#26783,#26784,#26785,#26786,#26787,#26788,
#26789,#26790,#26791,#26792,#26793,#26794,#26795,#26796,#26797,#26798,#26799,
#26800,#26801,#26802,#26803,#26804,#26805,#26806,#26807,#26808,#26809,#26810,
#26811,#26812,#26813,#26814,#26815,#26816,#26817,#26818,#26819,#26820,#26821,
#26822,#26823,#26824,#26825,#26826,#26827,#26828,#26829,#26830,#26831,#26832,
#26833,#26834,#26835,#26836,#26837,#26838,#26839,#26840,#26841,#26842,#26843,
#26844,#26845,#26846,#26847,#26848,#26849,#26850,#26851,#26852,#26853,#26854,
#26855,#26856,#26857,#26858,#26859,#26860,#26861,#26862,#26863,#26864,#26865,
#26866,#26867,#26868,#26869,#26870,#26871,#26872,#26873,#26874,#26875,#26876,
#26877,#26878,#26879,#26880,#26881,#26882,#26883,#26884,#26885,#26886,#26887,
#26888,#26889,#26890,#26891,#26892,#26893,#26894,#26895,#26896,#26897,#26898,
#26899,#26900,#26901,#26902,#26903,#26904,#26905,#26906,#26907,#26908,#26909,
#26910,#26911,#26912,#26913,#26914,#26915,#26916,#26917,#26918,#26919,#26920,
#26921,#26922,#26923,#26924),.UNSPECIFIED.,.F.,.F.,(4,3,3,3,3,3,3,3,3,3,
3,3,3,3,3,3,3,3,3,3,3,3,3,3,3,3,3,3,3,3,3,3,3,3,3,3,3,3,3,3,3,3,3,3,3,3,
3,3,3,3,3,3,3,3,3,3,3,3,3,3,3,3,3,3,3,3,3,3,3,3,3,3,3,3,3,3,4),(587.477826221416,
587.58694029442,587.698877318794,587.716354142749,587.800100875451,587.883744552467,
587.967305296533,588.05080315849,588.134265659052,588.217710794545,588.301156629387,
588.384621224626,588.468174410047,588.55177224362,588.635503806482,588.715337644948,
588.79908437765,588.882728054666,588.966288798732,589.049786660689,589.133249161251,
589.216694296744,589.300140131586,589.383604726824,589.467157912246,589.550755745819,
589.634487308681,589.714321147147,589.798067879849,589.881711556865,589.965272300931,
590.048770162888,590.132232663451,590.215677798943,590.299123633786,590.382588229024,
590.466141414446,590.549739248018,590.63347081088,590.713304649346,590.797051382048,
590.880695059064,590.964255803131,591.047753665087,591.13121616565,591.214661301142,
591.298107135985,591.381571731223,591.465124916645,591.548722750218,591.63245431308,
591.712288151546,591.796034884248,591.879678561264,591.96323930533,592.046737167287,
592.13019966785,592.213644803342,592.297090638185,592.380555233423,592.464108418845,
592.547706252418,592.631437815279,592.711271653745,592.795018386447,592.878662063463,
592.962222807529,593.045720669486,593.129183170049,593.212628305541,593.296074140384,
593.379538735622,593.463091921044,593.546689754616,593.630421317478,593.710255155944,
593.761011528471),.UNSPECIFIED.);
#323=B_SPLINE_CURVE_WITH_KNOTS('',3,(#26926,#26927,#26928,#26929,#26930,
#26931,#26932,#26933,#26934,#26935,#26936,#26937,#26938,#26939,#26940,#26941,
#26942,#26943,#26944,#26945,#26946,#26947,#26948,#26949,#26950,#26951,#26952,
#26953,#26954,#26955,#26956,#26957,#26958,#26959,#26960,#26961,#26962,#26963,
#26964,#26965,#26966,#26967,#26968,#26969,#26970,#26971,#26972,#26973,#26974,
#26975,#26976,#26977,#26978,#26979,#26980,#26981,#26982,#26983,#26984,#26985,
#26986,#26987,#26988,#26989,#26990,#26991,#26992,#26993,#26994,#26995,#26996,
#26997,#26998,#26999,#27000,#27001,#27002,#27003,#27004,#27005,#27006,#27007,
#27008,#27009,#27010,#27011,#27012,#27013,#27014,#27015,#27016,#27017,#27018,
#27019,#27020,#27021,#27022,#27023,#27024,#27025,#27026,#27027,#27028,#27029,
#27030,#27031,#27032,#27033,#27034,#27035,#27036,#27037,#27038,#27039,#27040,
#27041,#27042,#27043,#27044,#27045,#27046,#27047,#27048,#27049,#27050,#27051,
#27052,#27053,#27054,#27055,#27056,#27057,#27058,#27059,#27060,#27061,#27062,
#27063,#27064,#27065,#27066,#27067,#27068,#27069,#27070,#27071,#27072,#27073,
#27074,#27075,#27076,#27077,#27078,#27079,#27080,#27081,#27082,#27083,#27084,
#27085,#27086,#27087,#27088,#27089,#27090,#27091,#27092,#27093,#27094,#27095,
#27096,#27097,#27098,#27099,#27100,#27101,#27102,#27103,#27104,#27105,#27106,
#27107,#27108,#27109,#27110,#27111,#27112,#27113,#27114,#27115,#27116,#27117,
#27118,#27119,#27120,#27121,#27122,#27123,#27124,#27125,#27126,#27127,#27128,
#27129,#27130,#27131,#27132,#27133,#27134,#27135,#27136,#27137,#27138,#27139,
#27140,#27141,#27142,#27143,#27144,#27145,#27146,#27147,#27148,#27149,#27150,
#27151,#27152,#27153,#27154),.UNSPECIFIED.,.F.,.F.,(4,3,3,3,3,3,3,3,3,3,
3,3,3,3,3,3,3,3,3,3,3,3,3,3,3,3,3,3,3,3,3,3,3,3,3,3,3,3,3,3,3,3,3,3,3,3,
3,3,3,3,3,3,3,3,3,3,3,3,3,3,3,3,3,3,3,3,3,3,3,3,3,3,3,3,3,3,4),(581.194640914112,
581.281091694881,581.367623639591,581.456331012082,581.543124164076,581.632788646815,
581.722453129554,581.806199862256,581.889843539272,581.973404283339,582.056902145296,
582.140364645859,582.223809781352,582.307255616195,582.390720211433,582.474273396855,
582.557871230428,582.64160279329,582.721436631753,582.805183364455,582.888827041471,
582.972387785537,583.055885647494,583.139348148056,583.222793283549,583.306239118392,
583.38970371363,583.473256899052,583.556854732624,583.640586295486,583.720420133952,
583.804166866654,583.887810543669,583.971371287735,584.054869149691,584.138331650253,
584.221776785745,584.305222620588,584.388687215826,584.472240401247,584.55583823482,
584.639569797681,584.719403636151,584.803150368853,584.886794045869,584.970354789936,
585.053852651893,585.137315152456,585.220760287949,585.304206122792,585.38767071803,
585.471223903452,585.554821737025,585.638553299887,585.718387138351,585.802133871053,
585.885777548069,585.969338292136,586.052836154092,586.136298654655,586.219743790147,
586.30318962499,586.386654220228,586.47020740565,586.553805239222,586.637536802084,
586.71737064055,586.800085950562,586.884803484403,586.967315565623,587.049773693441,
587.132196809623,587.21860416254,587.301037458573,587.383488199913,587.465999582898,
587.477826221292),.UNSPECIFIED.);
#324=B_SPLINE_CURVE_WITH_KNOTS('',3,(#27156,#27157,#27158,#27159,#27160,
#27161,#27162,#27163,#27164,#27165,#27166,#27167,#27168,#27169,#27170,#27171,
#27172,#27173,#27174,#27175,#27176,#27177,#27178,#27179,#27180,#27181,#27182,
#27183,#27184,#27185,#27186,#27187,#27188,#27189,#27190,#27191,#27192,#27193,
#27194,#27195,#27196,#27197,#27198,#27199,#27200,#27201,#27202,#27203,#27204,
#27205,#27206,#27207,#27208,#27209,#27210,#27211,#27212,#27213,#27214,#27215,
#27216,#27217,#27218,#27219,#27220,#27221,#27222,#27223,#27224,#27225,#27226,
#27227,#27228,#27229,#27230,#27231,#27232,#27233,#27234,#27235,#27236,#27237,
#27238,#27239,#27240,#27241,#27242,#27243,#27244,#27245,#27246,#27247,#27248,
#27249,#27250,#27251,#27252,#27253,#27254,#27255,#27256,#27257,#27258,#27259,
#27260,#27261,#27262,#27263,#27264,#27265,#27266,#27267,#27268,#27269,#27270,
#27271,#27272,#27273,#27274,#27275,#27276,#27277,#27278,#27279,#27280,#27281,
#27282,#27283,#27284,#27285,#27286,#27287,#27288,#27289,#27290,#27291,#27292,
#27293,#27294,#27295,#27296,#27297,#27298,#27299,#27300,#27301,#27302,#27303,
#27304,#27305,#27306,#27307,#27308,#27309,#27310,#27311,#27312,#27313,#27314,
#27315,#27316,#27317,#27318,#27319,#27320,#27321,#27322,#27323,#27324,#27325,
#27326,#27327,#27328,#27329,#27330,#27331,#27332,#27333,#27334,#27335,#27336,
#27337,#27338,#27339,#27340,#27341,#27342,#27343,#27344,#27345,#27346,#27347,
#27348,#27349,#27350,#27351,#27352,#27353,#27354,#27355,#27356,#27357,#27358,
#27359,#27360,#27361,#27362,#27363,#27364,#27365,#27366,#27367,#27368,#27369,
#27370,#27371,#27372,#27373,#27374,#27375,#27376,#27377,#27378,#27379,#27380,
#27381,#27382,#27383,#27384),.UNSPECIFIED.,.F.,.F.,(4,3,3,3,3,3,3,3,3,3,
3,3,3,3,3,3,3,3,3,3,3,3,3,3,3,3,3,3,3,3,3,3,3,3,3,3,3,3,3,3,3,3,3,3,3,3,
3,3,3,3,3,3,3,3,3,3,3,3,3,3,3,3,3,3,3,3,3,3,3,3,3,3,3,3,3,3,4),(574.911455607082,
574.993828450003,575.076127396377,575.158377281039,575.240601792619,575.322819962021,
575.40505081275,575.487363270994,575.569716742042,575.652199607108,575.728552116359,
575.812298849061,575.895942526077,575.979503270143,576.0630011321,576.146463632662,
576.229908768155,576.313354602997,576.396819198235,576.480372383657,576.56397021723,
576.647701780092,576.727535618558,576.81128235126,576.894926028276,576.978486772342,
577.061984634299,577.145447134861,577.228892270353,577.312338105196,577.395802700435,
577.479355885856,577.562953719429,577.64668528229,577.726519120757,577.810265853459,
577.893909530475,577.977470274541,578.060968136498,578.144430637061,578.227875772553,
578.311321607396,578.394786202633,578.478339388055,578.561937221628,578.64566878449,
578.725502622956,578.809249355658,578.892893032674,578.976453776741,579.059951638698,
579.143414139261,579.226859274753,579.310305109596,579.393769704834,579.477322890256,
579.560920723829,579.644652286691,579.724486125156,579.808232857858,579.891876534874,
579.97543727894,580.058935140897,580.14239764146,580.225842776952,580.309288611795,
580.392753207033,580.476306392455,580.559904226027,580.643635788889,580.723469627355,
580.812727000859,580.901812324686,580.990660382827,581.079361847327,581.167867105857,
581.194640913983),.UNSPECIFIED.);
#325=B_SPLINE_CURVE_WITH_KNOTS('',3,(#27386,#27387,#27388,#27389,#27390,
#27391,#27392,#27393,#27394,#27395,#27396,#27397,#27398,#27399,#27400,#27401,
#27402,#27403,#27404,#27405,#27406,#27407,#27408,#27409,#27410,#27411,#27412,
#27413,#27414,#27415,#27416,#27417,#27418,#27419,#27420,#27421,#27422,#27423,
#27424,#27425,#27426,#27427,#27428,#27429,#27430,#27431,#27432,#27433,#27434,
#27435,#27436,#27437,#27438,#27439,#27440,#27441,#27442,#27443,#27444,#27445,
#27446,#27447,#27448,#27449,#27450,#27451,#27452,#27453,#27454,#27455,#27456,
#27457,#27458,#27459,#27460,#27461,#27462,#27463,#27464,#27465,#27466,#27467,
#27468,#27469,#27470,#27471,#27472,#27473,#27474,#27475,#27476,#27477,#27478,
#27479,#27480,#27481,#27482,#27483,#27484,#27485,#27486,#27487,#27488,#27489,
#27490,#27491,#27492,#27493,#27494,#27495,#27496,#27497,#27498,#27499,#27500,
#27501,#27502,#27503,#27504,#27505,#27506,#27507,#27508,#27509,#27510,#27511,
#27512,#27513,#27514,#27515,#27516,#27517,#27518,#27519,#27520,#27521,#27522,
#27523,#27524,#27525,#27526,#27527,#27528,#27529,#27530,#27531,#27532,#27533,
#27534,#27535,#27536,#27537,#27538,#27539,#27540,#27541,#27542,#27543,#27544,
#27545,#27546,#27547,#27548,#27549,#27550,#27551,#27552,#27553,#27554,#27555,
#27556,#27557,#27558,#27559,#27560,#27561,#27562,#27563,#27564,#27565,#27566,
#27567,#27568,#27569,#27570,#27571,#27572,#27573,#27574,#27575,#27576,#27577,
#27578,#27579,#27580,#27581,#27582,#27583,#27584,#27585,#27586,#27587,#27588,
#27589,#27590,#27591,#27592,#27593,#27594,#27595,#27596,#27597,#27598,#27599,
#27600,#27601,#27602,#27603,#27604,#27605,#27606,#27607,#27608,#27609,#27610,
#27611),.UNSPECIFIED.,.F.,.F.,(4,3,3,3,3,3,3,3,3,3,3,3,3,3,3,3,3,3,3,3,
3,3,3,3,3,3,3,3,3,3,3,3,3,3,3,3,3,3,3,3,3,3,3,3,3,3,3,3,3,3,3,3,3,3,3,3,
3,3,3,3,3,3,3,3,3,3,3,3,3,3,3,3,3,3,3,4),(568.628270299753,568.735667600965,
568.819414333667,568.903058010683,568.986618754749,569.070116616706,569.153579117268,
569.23702425276,569.320470087603,569.403934682841,569.487487868263,569.571085701836,
569.654817264697,569.734651103164,569.818397835866,569.902041512882,569.985602256948,
570.069100118905,570.152562619467,570.23600775496,570.319453589802,570.402918185041,
570.486471370462,570.570069204035,570.653800766897,570.733634605363,570.817381338065,
570.901025015081,570.984585759148,571.068083621104,571.151546121667,571.234991257159,
571.318437092002,571.40190168724,571.485454872662,571.569052706235,571.652784269097,
571.732618107562,571.816364840264,571.90000851728,571.983569261346,572.067067123303,
572.150529623865,572.233974759358,572.3174205942,572.400885189439,572.48443837486,
572.568036208433,572.651767771295,572.731601609761,572.815348342463,572.898992019479,
572.982552763546,573.066050625502,573.149513126065,573.232958261557,573.3164040964,
573.399868691639,573.48342187706,573.567019710633,573.650751273495,573.730585111961,
573.814331844663,573.897975521679,573.981536265745,574.065034127702,574.148496628265,
574.231941763757,574.3153875986,574.398852193838,574.48240537926,574.566003212833,
574.649734775695,574.72956861416,574.855844314663,574.911455606932),
 .UNSPECIFIED.);
#326=B_SPLINE_CURVE_WITH_KNOTS('',3,(#27613,#27614,#27615,#27616,#27617,
#27618,#27619,#27620,#27621,#27622,#27623,#27624,#27625,#27626,#27627,#27628,
#27629,#27630,#27631,#27632,#27633,#27634,#27635,#27636,#27637,#27638,#27639,
#27640,#27641,#27642,#27643,#27644,#27645,#27646,#27647,#27648,#27649,#27650,
#27651,#27652,#27653,#27654,#27655,#27656,#27657,#27658,#27659,#27660,#27661,
#27662,#27663,#27664,#27665,#27666,#27667,#27668,#27669,#27670,#27671,#27672,
#27673,#27674,#27675,#27676,#27677,#27678,#27679,#27680,#27681,#27682,#27683,
#27684,#27685,#27686,#27687,#27688,#27689,#27690,#27691,#27692,#27693,#27694,
#27695,#27696,#27697,#27698,#27699,#27700,#27701,#27702,#27703,#27704,#27705,
#27706,#27707,#27708,#27709,#27710,#27711,#27712,#27713,#27714,#27715,#27716,
#27717,#27718,#27719,#27720,#27721,#27722,#27723,#27724,#27725,#27726,#27727,
#27728,#27729,#27730,#27731,#27732,#27733,#27734,#27735,#27736,#27737,#27738,
#27739,#27740,#27741,#27742,#27743,#27744,#27745,#27746,#27747,#27748,#27749,
#27750,#27751,#27752,#27753,#27754,#27755,#27756,#27757,#27758,#27759,#27760,
#27761,#27762,#27763,#27764,#27765,#27766,#27767,#27768,#27769,#27770,#27771,
#27772,#27773,#27774,#27775,#27776,#27777,#27778,#27779,#27780,#27781,#27782,
#27783,#27784,#27785,#27786,#27787,#27788,#27789,#27790,#27791,#27792,#27793,
#27794,#27795,#27796,#27797,#27798,#27799,#27800,#27801,#27802,#27803,#27804,
#27805,#27806,#27807,#27808,#27809,#27810,#27811,#27812,#27813,#27814,#27815,
#27816,#27817,#27818,#27819,#27820,#27821,#27822,#27823,#27824,#27825,#27826,
#27827,#27828,#27829,#27830,#27831,#27832,#27833,#27834,#27835,#27836,#27837,
#27838,#27839,#27840,#27841),.UNSPECIFIED.,.F.,.F.,(4,3,3,3,3,3,3,3,3,3,
3,3,3,3,3,3,3,3,3,3,3,3,3,3,3,3,3,3,3,3,3,3,3,3,3,3,3,3,3,3,3,3,3,3,3,3,
3,3,3,3,3,3,3,3,3,3,3,3,3,3,3,3,3,3,3,3,3,3,3,3,3,3,3,3,3,3,4),(562.345084992753,
562.437348628487,562.530118911342,562.623151742719,562.716522454311,562.74176658777,
562.825513320472,562.909156997488,562.992717741554,563.076215603511,563.159678104074,
563.243123239566,563.326569074409,563.410033669647,563.493586855069,563.577184688641,
563.660916251503,563.740750089969,563.824496822671,563.908140499687,563.991701243753,
564.07519910571,564.158661606272,564.242106741765,564.325552576607,564.409017171846,
564.492570357267,564.57616819084,564.659899753702,564.739733592168,564.82348032487,
564.907124001886,564.990684745952,565.074182607909,565.157645108472,565.241090243964,
565.324536078807,565.408000674045,565.491553859467,565.575151693039,565.658883255901,
565.738717094367,565.822463827069,565.906107504085,565.989668248151,566.073166110108,
566.156628610671,566.240073746163,566.323519581006,566.406984176244,566.490537361666,
566.574135195238,566.6578667581,566.737700596566,566.821447329268,566.905091006284,
566.988651750351,567.072149612307,567.15561211287,567.239057248362,567.322503083205,
567.405967678443,567.489520863865,567.573118697438,567.6568502603,567.736684098766,
567.819341452811,567.901896585442,567.98437060958,568.066783877203,568.149164799221,
568.231532317683,568.313905361203,568.396346362416,568.478822157388,568.561411095726,
568.628270299618),.UNSPECIFIED.);
#327=B_SPLINE_CURVE_WITH_KNOTS('',3,(#27843,#27844,#27845,#27846,#27847,
#27848,#27849,#27850,#27851,#27852,#27853,#27854,#27855,#27856,#27857,#27858,
#27859,#27860,#27861,#27862,#27863,#27864,#27865,#27866,#27867,#27868,#27869,
#27870,#27871,#27872,#27873,#27874,#27875,#27876,#27877,#27878,#27879,#27880,
#27881,#27882,#27883,#27884,#27885,#27886,#27887,#27888,#27889,#27890,#27891,
#27892,#27893,#27894,#27895,#27896,#27897,#27898,#27899,#27900,#27901,#27902,
#27903,#27904,#27905,#27906,#27907,#27908,#27909,#27910,#27911,#27912,#27913,
#27914,#27915,#27916,#27917,#27918,#27919,#27920,#27921,#27922,#27923,#27924,
#27925,#27926,#27927,#27928,#27929,#27930,#27931,#27932,#27933,#27934,#27935,
#27936,#27937,#27938,#27939,#27940,#27941,#27942,#27943,#27944,#27945,#27946,
#27947,#27948,#27949,#27950,#27951,#27952,#27953,#27954,#27955,#27956,#27957,
#27958,#27959,#27960,#27961,#27962,#27963,#27964,#27965,#27966,#27967,#27968,
#27969,#27970,#27971,#27972,#27973,#27974,#27975,#27976,#27977,#27978,#27979,
#27980,#27981,#27982,#27983,#27984,#27985,#27986,#27987,#27988,#27989,#27990,
#27991,#27992,#27993,#27994,#27995,#27996,#27997,#27998,#27999,#28000,#28001,
#28002,#28003,#28004,#28005,#28006,#28007,#28008,#28009,#28010,#28011,#28012,
#28013,#28014,#28015,#28016,#28017,#28018,#28019,#28020,#28021,#28022,#28023,
#28024,#28025,#28026,#28027,#28028,#28029,#28030,#28031,#28032,#28033,#28034,
#28035,#28036,#28037,#28038,#28039,#28040,#28041,#28042,#28043,#28044,#28045,
#28046,#28047,#28048,#28049,#28050,#28051,#28052,#28053,#28054,#28055,#28056,
#28057,#28058,#28059,#28060,#28061,#28062,#28063,#28064,#28065,#28066,#28067,
#28068,#28069,#28070,#28071),.UNSPECIFIED.,.F.,.F.,(4,3,3,3,3,3,3,3,3,3,
3,3,3,3,3,3,3,3,3,3,3,3,3,3,3,3,3,3,3,3,3,3,3,3,3,3,3,3,3,3,3,3,3,3,3,3,
3,3,3,3,3,3,3,3,3,3,3,3,3,3,3,3,3,3,3,3,3,3,3,3,3,3,3,3,3,3,4),(556.061899685394,
556.147645421542,556.23075807931,556.313867712067,556.3969926505,556.480151232029,
556.563407194035,556.646721589556,556.73015545405,556.747865574575,556.831612307277,
556.915255984293,556.998816728359,557.082314590317,557.165777090879,557.249222226372,
557.332668061214,557.416132656453,557.499685841874,557.583283675447,557.667015238309,
557.746849076774,557.830595809476,557.914239486492,557.997800230558,558.081298092515,
558.164760593078,558.24820572857,558.331651563413,558.415116158651,558.498669344073,
558.582267177646,558.665998740507,558.745832578973,558.829579311675,558.913222988691,
558.996783732757,559.080281594714,559.163744095276,559.247189230768,559.330635065611,
559.414099660849,559.497652846271,559.581250679843,559.664982242705,559.744816081172,
559.828562813874,559.91220649089,559.995767234957,560.079265096913,560.162727597476,
560.246172732968,560.329618567811,560.413083163049,560.496636348471,560.580234182043,
560.663965744905,560.743799583371,560.827546316073,560.911189993089,560.994750737156,
561.078248599113,561.161711099675,561.245156235168,561.32860207001,561.412066665249,
561.49561985067,561.579217684243,561.662949247105,561.742783085571,561.827693316259,
561.912491884059,561.997195483401,562.084167860694,562.168721138886,562.256903065729,
562.345084992573),.UNSPECIFIED.);
#328=B_SPLINE_CURVE_WITH_KNOTS('',3,(#28073,#28074,#28075,#28076,#28077,
#28078,#28079,#28080,#28081,#28082),.UNSPECIFIED.,.F.,.F.,(4,1,1,1,1,1,
1,4),(549.778717730147,550.75396456138,551.752948063579,552.751931565778,
553.750915067977,554.749898570176,555.748882072376,556.061893235856),
 .UNSPECIFIED.);
#329=B_SPLINE_CURVE_WITH_KNOTS('',3,(#28084,#28085,#28086,#28087,#28088,
#28089,#28090,#28091,#28092,#28093,#28094,#28095,#28096,#28097,#28098,#28099,
#28100,#28101,#28102,#28103,#28104,#28105,#28106,#28107,#28108,#28109,#28110,
#28111,#28112,#28113,#28114,#28115,#28116,#28117,#28118,#28119,#28120,#28121,
#28122,#28123,#28124,#28125,#28126,#28127,#28128,#28129,#28130,#28131,#28132,
#28133,#28134,#28135,#28136,#28137,#28138,#28139,#28140,#28141,#28142,#28143,
#28144,#28145,#28146,#28147,#28148,#28149,#28150,#28151,#28152,#28153,#28154,
#28155,#28156,#28157,#28158,#28159,#28160,#28161,#28162,#28163,#28164,#28165,
#28166,#28167,#28168,#28169,#28170,#28171,#28172,#28173,#28174,#28175,#28176,
#28177,#28178,#28179,#28180,#28181,#28182,#28183,#28184,#28185,#28186,#28187,
#28188,#28189,#28190,#28191,#28192,#28193,#28194,#28195,#28196,#28197,#28198,
#28199,#28200,#28201,#28202,#28203,#28204,#28205,#28206,#28207,#28208,#28209,
#28210,#28211,#28212,#28213,#28214,#28215,#28216,#28217,#28218,#28219,#28220,
#28221,#28222,#28223,#28224,#28225,#28226,#28227,#28228,#28229,#28230,#28231,
#28232,#28233,#28234,#28235,#28236,#28237,#28238,#28239,#28240,#28241,#28242,
#28243,#28244,#28245,#28246,#28247,#28248,#28249,#28250,#28251,#28252,#28253,
#28254,#28255,#28256,#28257,#28258,#28259,#28260,#28261,#28262,#28263,#28264,
#28265,#28266,#28267,#28268,#28269,#28270,#28271,#28272,#28273,#28274,#28275,
#28276,#28277,#28278,#28279,#28280,#28281,#28282,#28283,#28284,#28285,#28286,
#28287,#28288,#28289,#28290,#28291,#28292,#28293,#28294,#28295,#28296,#28297,
#28298,#28299,#28300,#28301,#28302,#28303,#28304,#28305,#28306,#28307,#28308,
#28309,#28310,#28311,#28312),.UNSPECIFIED.,.F.,.F.,(4,3,3,3,3,3,3,3,3,3,
3,3,3,3,3,3,3,3,3,3,3,3,3,3,3,3,3,3,3,3,3,3,3,3,3,3,3,3,3,3,3,3,3,3,3,3,
3,3,3,3,3,3,3,3,3,3,3,3,3,3,3,3,3,3,3,3,3,3,3,3,3,3,3,3,3,3,4),(543.495529071195,
543.600349959761,543.70712252169,543.761080045986,543.844826778688,543.928470455704,
544.012031199771,544.095529061728,544.178991562291,544.262436697784,544.345882532627,
544.429347127865,544.512900313287,544.59649814686,544.680229709723,544.760063548185,
544.843810280887,544.927453957903,545.011014701969,545.094512563926,545.177975064488,
545.261420199981,545.344866034824,545.428330630062,545.511883815483,545.595481649056,
545.679213211918,545.759047050384,545.842793783086,545.926437460102,546.009998204168,
546.093496066124,546.176958566687,546.260403702179,546.343849537022,546.427314132259,
546.510867317681,546.594465151254,546.678196714115,546.758030552583,546.841777285285,
546.925420962301,547.008981706367,547.092479568324,547.175942068887,547.259387204379,
547.342833039222,547.42629763446,547.509850819882,547.593448653455,547.677180216316,
547.757014054782,547.840760787484,547.9244044645,548.007965208567,548.091463070524,
548.174925571086,548.258370706579,548.341816541422,548.42528113666,548.508834322082,
548.592432155655,548.676163718517,548.755997556982,548.839744289684,548.9233879667,
549.006948710767,549.090446572724,549.173909073286,549.257354208779,549.340800043622,
549.42426463886,549.507817824282,549.591415657855,549.675147220717,549.754981059181,
549.778714378214),.UNSPECIFIED.);
#330=B_SPLINE_CURVE_WITH_KNOTS('',3,(#28314,#28315,#28316,#28317,#28318,
#28319,#28320,#28321,#28322,#28323,#28324,#28325,#28326,#28327,#28328,#28329,
#28330,#28331,#28332,#28333,#28334,#28335,#28336,#28337,#28338,#28339,#28340,
#28341,#28342,#28343,#28344,#28345,#28346,#28347,#28348,#28349,#28350,#28351,
#28352,#28353,#28354,#28355,#28356,#28357,#28358,#28359,#28360,#28361,#28362,
#28363,#28364,#28365,#28366,#28367,#28368,#28369,#28370,#28371,#28372,#28373,
#28374,#28375,#28376,#28377,#28378,#28379,#28380,#28381,#28382,#28383,#28384,
#28385,#28386,#28387,#28388,#28389,#28390,#28391,#28392,#28393,#28394,#28395,
#28396,#28397,#28398,#28399,#28400,#28401,#28402,#28403,#28404,#28405,#28406,
#28407,#28408,#28409,#28410,#28411,#28412,#28413,#28414,#28415,#28416,#28417,
#28418,#28419,#28420,#28421,#28422,#28423,#28424,#28425,#28426,#28427,#28428,
#28429,#28430,#28431,#28432,#28433,#28434,#28435,#28436,#28437,#28438,#28439,
#28440,#28441,#28442,#28443,#28444,#28445,#28446,#28447,#28448,#28449,#28450,
#28451,#28452,#28453,#28454,#28455,#28456,#28457,#28458,#28459,#28460,#28461,
#28462,#28463,#28464,#28465,#28466,#28467,#28468,#28469,#28470,#28471,#28472,
#28473,#28474,#28475,#28476,#28477,#28478,#28479,#28480,#28481,#28482,#28483,
#28484,#28485,#28486,#28487,#28488,#28489,#28490,#28491,#28492,#28493,#28494,
#28495,#28496,#28497,#28498,#28499,#28500,#28501,#28502,#28503,#28504,#28505,
#28506,#28507,#28508,#28509,#28510,#28511,#28512,#28513,#28514,#28515,#28516,
#28517,#28518,#28519,#28520,#28521,#28522,#28523,#28524,#28525,#28526,#28527,
#28528,#28529,#28530,#28531,#28532,#28533,#28534,#28535,#28536,#28537,#28538,
#28539,#28540,#28541,#28542),.UNSPECIFIED.,.F.,.F.,(4,3,3,3,3,3,3,3,3,3,
3,3,3,3,3,3,3,3,3,3,3,3,3,3,3,3,3,3,3,3,3,3,3,3,3,3,3,3,3,3,3,3,3,3,3,3,
3,3,3,3,3,3,3,3,3,3,3,3,3,3,3,3,3,3,3,3,3,3,3,3,3,3,3,3,3,3,4),(537.212343763855,
537.298000378494,537.383712338006,537.469493659904,537.55542022831,537.641428057268,
537.727592604259,537.767179032791,537.850925765493,537.934569442509,538.018130186575,
538.101628048532,538.185090549094,538.268535684586,538.351981519429,538.435446114667,
538.518999300089,538.602597133661,538.686328696523,538.76616253499,538.849909267692,
538.933552944708,539.017113688774,539.100611550731,539.184074051294,539.267519186786,
539.350965021629,539.434429616867,539.517982802289,539.601580635861,539.685312198723,
539.765146037189,539.848892769891,539.932536446907,540.016097190973,540.09959505293,
540.183057553493,540.266502688985,540.349948523828,540.433413119066,540.516966304488,
540.60056413806,540.684295700922,540.764129539388,540.84787627209,540.931519949106,
541.015080693172,541.098578555128,541.182041055691,541.265486191183,541.348932026026,
541.432396621264,541.515949806686,541.599547640258,541.68327920312,541.763113041587,
541.846859774289,541.930503451305,542.014064195372,542.09756205733,542.181024557892,
542.264469693385,542.347915528228,542.431380123467,542.514933308888,542.598531142461,
542.682262705323,542.762096543787,542.845014125629,542.927800991536,543.010512696025,
543.093168093423,543.175785990596,543.258405489438,543.341022571314,543.423694512478,
543.495529071035),.UNSPECIFIED.);
#331=B_SPLINE_CURVE_WITH_KNOTS('',3,(#28544,#28545,#28546,#28547,#28548,
#28549,#28550,#28551,#28552,#28553,#28554,#28555,#28556,#28557,#28558,#28559,
#28560,#28561,#28562,#28563,#28564,#28565,#28566,#28567,#28568,#28569,#28570,
#28571,#28572,#28573,#28574,#28575,#28576,#28577,#28578,#28579,#28580,#28581,
#28582,#28583,#28584,#28585,#28586,#28587,#28588,#28589,#28590,#28591,#28592,
#28593,#28594,#28595,#28596,#28597,#28598,#28599,#28600,#28601,#28602,#28603,
#28604,#28605,#28606,#28607,#28608,#28609,#28610,#28611,#28612,#28613,#28614,
#28615,#28616,#28617,#28618,#28619,#28620,#28621,#28622,#28623,#28624,#28625,
#28626,#28627,#28628,#28629,#28630,#28631,#28632,#28633,#28634,#28635,#28636,
#28637,#28638,#28639,#28640,#28641,#28642,#28643,#28644,#28645,#28646,#28647,
#28648,#28649,#28650,#28651,#28652,#28653,#28654,#28655,#28656,#28657,#28658,
#28659,#28660,#28661,#28662,#28663,#28664,#28665,#28666,#28667,#28668,#28669,
#28670,#28671,#28672,#28673,#28674,#28675,#28676,#28677,#28678,#28679,#28680,
#28681,#28682,#28683,#28684,#28685,#28686,#28687,#28688,#28689,#28690,#28691,
#28692,#28693,#28694,#28695,#28696,#28697,#28698,#28699,#28700,#28701,#28702,
#28703,#28704,#28705,#28706,#28707,#28708,#28709,#28710,#28711,#28712,#28713,
#28714,#28715,#28716,#28717,#28718,#28719,#28720,#28721,#28722,#28723,#28724,
#28725,#28726,#28727,#28728,#28729,#28730,#28731,#28732,#28733,#28734,#28735,
#28736,#28737,#28738,#28739,#28740,#28741,#28742,#28743,#28744,#28745,#28746,
#28747,#28748,#28749,#28750,#28751,#28752,#28753,#28754,#28755,#28756,#28757,
#28758,#28759,#28760,#28761,#28762,#28763,#28764,#28765,#28766,#28767,#28768,
#28769,#28770,#28771,#28772),.UNSPECIFIED.,.F.,.F.,(4,3,3,3,3,3,3,3,3,3,
3,3,3,3,3,3,3,3,3,3,3,3,3,3,3,3,3,3,3,3,3,3,3,3,3,3,3,3,3,3,3,3,3,3,3,3,
3,3,3,3,3,3,3,3,3,3,3,3,3,3,3,3,3,3,3,3,3,3,3,3,3,3,3,3,3,3,4),(530.929158456783,
531.01156105809,531.093882835983,531.178807233935,531.261038216809,531.343257242855,
531.42548333556,531.507735522145,531.590076053576,531.6724696604,531.754977052498,
531.773278019596,531.857024752298,531.940668429314,532.02422917338,532.107727035337,
532.191189535899,532.274634671391,532.358080506234,532.441545101472,532.525098286894,
532.608696120467,532.692427683329,532.772261521795,532.856008254497,532.939651931513,
533.02321267558,533.106710537537,533.190173038099,533.273618173592,533.357064008434,
533.440528603673,533.524081789094,533.607679622667,533.691411185529,533.771245023994,
533.854991756696,533.938635433712,534.022196177778,534.105694039735,534.189156540297,
534.272601675789,534.356047510632,534.43951210587,534.523065291292,534.606663124864,
534.690394687726,534.770228526193,534.853975258895,534.937618935911,535.021179679977,
535.104677541934,535.188140042496,535.271585177988,535.355031012831,535.438495608069,
535.522048793491,535.605646627064,535.689378189925,535.769212028392,535.852958761094,
535.93660243811,536.020163182177,536.103661044133,536.187123544696,536.270568680188,
536.354014515031,536.437479110269,536.521032295691,536.604630129264,536.688361692126,
536.768195530591,536.85877152174,536.949048084385,537.039143045008,537.128947971728,
537.212343763737),.UNSPECIFIED.);
#332=B_SPLINE_CURVE_WITH_KNOTS('',3,(#28774,#28775,#28776,#28777,#28778,
#28779,#28780,#28781,#28782,#28783,#28784,#28785,#28786,#28787,#28788,#28789,
#28790,#28791,#28792,#28793,#28794,#28795,#28796,#28797,#28798,#28799,#28800,
#28801,#28802,#28803,#28804,#28805,#28806,#28807,#28808,#28809,#28810,#28811,
#28812,#28813,#28814,#28815,#28816,#28817,#28818,#28819,#28820,#28821,#28822,
#28823,#28824,#28825,#28826,#28827,#28828,#28829,#28830,#28831,#28832,#28833,
#28834,#28835,#28836,#28837,#28838,#28839,#28840,#28841,#28842,#28843,#28844,
#28845,#28846,#28847,#28848,#28849,#28850,#28851,#28852,#28853,#28854,#28855,
#28856,#28857,#28858,#28859,#28860,#28861,#28862,#28863,#28864,#28865,#28866,
#28867,#28868,#28869,#28870,#28871,#28872,#28873,#28874,#28875,#28876,#28877,
#28878,#28879,#28880,#28881,#28882,#28883,#28884,#28885,#28886,#28887,#28888,
#28889,#28890,#28891,#28892,#28893,#28894,#28895,#28896,#28897,#28898,#28899,
#28900,#28901,#28902,#28903,#28904,#28905,#28906,#28907,#28908,#28909,#28910,
#28911,#28912,#28913,#28914,#28915,#28916,#28917,#28918,#28919,#28920,#28921,
#28922,#28923,#28924,#28925,#28926,#28927,#28928,#28929,#28930,#28931,#28932,
#28933,#28934,#28935,#28936,#28937,#28938,#28939,#28940,#28941,#28942,#28943,
#28944,#28945,#28946,#28947,#28948,#28949,#28950,#28951,#28952,#28953,#28954,
#28955,#28956,#28957,#28958,#28959,#28960,#28961,#28962,#28963,#28964,#28965,
#28966,#28967,#28968,#28969,#28970,#28971,#28972,#28973,#28974,#28975,#28976,
#28977,#28978,#28979,#28980,#28981,#28982,#28983,#28984,#28985,#28986,#28987,
#28988,#28989,#28990,#28991,#28992,#28993,#28994,#28995,#28996,#28997,#28998,
#28999),.UNSPECIFIED.,.F.,.F.,(4,3,3,3,3,3,3,3,3,3,3,3,3,3,3,3,3,3,3,3,
3,3,3,3,3,3,3,3,3,3,3,3,3,3,3,3,3,3,3,3,3,3,3,3,3,3,3,3,3,3,3,3,3,3,3,3,
3,3,3,3,3,3,3,3,3,3,3,3,3,3,3,3,3,3,3,4),(524.645973149496,524.780393504201,
524.864140236903,524.947783913919,525.031344657985,525.114842519942,525.198305020505,
525.281750155997,525.36519599084,525.448660586078,525.5322137715,525.615811605073,
525.699543167934,525.779377006401,525.863123739103,525.946767416119,526.030328160185,
526.113826022142,526.197288522705,526.280733658197,526.36417949304,526.447644088278,
526.5311972737,526.614795107272,526.698526670134,526.7783605086,526.862107241302,
526.945750918318,527.029311662384,527.112809524341,527.196272024904,527.279717160396,
527.363162995239,527.446627590477,527.530180775899,527.613778609471,527.697510172333,
527.777344010799,527.861090743501,527.944734420517,528.028295164583,528.11179302654,
528.195255527103,528.278700662595,528.362146497438,528.445611092676,528.529164278098,
528.61276211167,528.696493674532,528.776327512998,528.8600742457,528.943717922716,
529.027278666782,529.110776528739,529.194239029301,529.277684164794,529.361129999636,
529.444594594874,529.528147780296,529.611745613869,529.69547717673,529.775311015197,
529.859057747899,529.942701424915,530.026262168981,530.109760030938,530.193222531501,
530.276667666993,530.360113501836,530.443578097074,530.527131282496,530.610729116068,
530.69446067893,530.774294517396,530.913405606285,530.929158456676),
 .UNSPECIFIED.);
#333=B_SPLINE_CURVE_WITH_KNOTS('',3,(#29001,#29002,#29003,#29004,#29005,
#29006,#29007,#29008,#29009,#29010,#29011,#29012,#29013,#29014,#29015,#29016,
#29017,#29018,#29019,#29020,#29021,#29022,#29023,#29024,#29025,#29026,#29027,
#29028,#29029,#29030,#29031,#29032,#29033,#29034,#29035,#29036,#29037,#29038,
#29039,#29040,#29041,#29042,#29043,#29044,#29045,#29046,#29047,#29048,#29049,
#29050,#29051,#29052,#29053,#29054,#29055,#29056,#29057,#29058,#29059,#29060,
#29061,#29062,#29063,#29064,#29065,#29066,#29067,#29068,#29069,#29070,#29071,
#29072,#29073,#29074,#29075,#29076,#29077,#29078,#29079,#29080,#29081,#29082,
#29083,#29084,#29085,#29086,#29087,#29088,#29089,#29090,#29091,#29092,#29093,
#29094,#29095,#29096,#29097,#29098,#29099,#29100,#29101,#29102,#29103,#29104,
#29105,#29106,#29107,#29108,#29109,#29110,#29111,#29112,#29113,#29114,#29115,
#29116,#29117,#29118,#29119,#29120,#29121,#29122,#29123,#29124,#29125,#29126,
#29127,#29128,#29129,#29130,#29131,#29132,#29133,#29134,#29135,#29136,#29137,
#29138,#29139,#29140,#29141,#29142,#29143,#29144,#29145,#29146,#29147,#29148,
#29149,#29150,#29151,#29152,#29153,#29154,#29155,#29156,#29157,#29158,#29159,
#29160,#29161,#29162,#29163,#29164,#29165,#29166,#29167,#29168,#29169,#29170,
#29171,#29172,#29173,#29174,#29175,#29176,#29177,#29178,#29179,#29180,#29181,
#29182,#29183,#29184,#29185,#29186,#29187,#29188,#29189,#29190,#29191,#29192,
#29193,#29194,#29195,#29196,#29197,#29198,#29199,#29200,#29201,#29202,#29203,
#29204,#29205,#29206,#29207,#29208,#29209,#29210,#29211,#29212,#29213,#29214,
#29215,#29216,#29217,#29218,#29219,#29220,#29221,#29222,#29223,#29224,#29225,
#29226,#29227,#29228,#29229),.UNSPECIFIED.,.F.,.F.,(4,3,3,3,3,3,3,3,3,3,
3,3,3,3,3,3,3,3,3,3,3,3,3,3,3,3,3,3,3,3,3,3,3,3,3,3,3,3,3,3,3,3,3,3,3,3,
3,3,3,3,3,3,3,3,3,3,3,3,3,3,3,3,3,3,3,3,3,3,3,3,3,3,3,3,3,3,4),(518.362787842463,
518.453523730853,518.544661312336,518.636003322358,518.727651533168,518.786492491007,
518.870239223709,518.953882900725,519.037443644791,519.120941506748,519.204404007311,
519.287849142803,519.371294977646,519.454759572884,519.538312758306,519.621910591878,
519.70564215474,519.785475993206,519.869222725908,519.952866402924,520.03642714699,
520.119925008947,520.203387509509,520.286832645001,520.370278479844,520.453743075082,
520.537296260504,520.620894094076,520.704625656938,520.784459495405,520.868206228107,
520.951849905123,521.03541064919,521.118908511146,521.202371011709,521.285816147201,
521.369261982044,521.452726577282,521.536279762704,521.619877596277,521.703609159139,
521.783442997604,521.867189730306,521.950833407322,522.034394151388,522.117892013345,
522.201354513907,522.284799649399,522.368245484242,522.45171007948,522.535263264902,
522.618861098475,522.702592661336,522.782426499803,522.866173232505,522.949816909521,
523.033377653587,523.116875515544,523.200338016107,523.283783151599,523.367228986442,
523.45069358168,523.534246767102,523.617844600674,523.701576163536,523.781410002002,
523.863956676188,523.946401108076,524.02876449323,524.11106650296,524.193336204663,
524.275592609193,524.357854713714,524.440179777105,524.522540120567,524.605000346848,
524.645973149371),.UNSPECIFIED.);
#334=B_SPLINE_CURVE_WITH_KNOTS('',3,(#29231,#29232,#29233,#29234,#29235,
#29236,#29237,#29238,#29239,#29240,#29241,#29242,#29243,#29244,#29245,#29246,
#29247,#29248,#29249,#29250,#29251,#29252,#29253,#29254,#29255,#29256,#29257,
#29258,#29259,#29260,#29261,#29262,#29263,#29264,#29265,#29266,#29267,#29268,
#29269,#29270,#29271,#29272,#29273,#29274,#29275,#29276,#29277,#29278,#29279,
#29280,#29281,#29282,#29283,#29284,#29285,#29286,#29287,#29288,#29289,#29290,
#29291,#29292,#29293,#29294,#29295,#29296,#29297,#29298,#29299,#29300,#29301,
#29302,#29303,#29304,#29305,#29306,#29307,#29308,#29309,#29310,#29311,#29312,
#29313,#29314,#29315,#29316,#29317,#29318,#29319,#29320,#29321,#29322,#29323,
#29324,#29325,#29326,#29327,#29328,#29329,#29330,#29331,#29332,#29333,#29334,
#29335,#29336,#29337,#29338,#29339,#29340,#29341,#29342,#29343,#29344,#29345,
#29346,#29347,#29348,#29349,#29350,#29351,#29352,#29353,#29354,#29355,#29356,
#29357,#29358,#29359,#29360,#29361,#29362,#29363,#29364,#29365,#29366,#29367,
#29368,#29369,#29370,#29371,#29372,#29373,#29374,#29375,#29376,#29377,#29378,
#29379,#29380,#29381,#29382,#29383,#29384,#29385,#29386,#29387,#29388,#29389,
#29390,#29391,#29392,#29393,#29394,#29395,#29396,#29397,#29398,#29399,#29400,
#29401,#29402,#29403,#29404,#29405,#29406,#29407,#29408,#29409,#29410,#29411,
#29412,#29413,#29414,#29415,#29416,#29417,#29418,#29419,#29420,#29421,#29422,
#29423,#29424,#29425,#29426,#29427,#29428,#29429,#29430,#29431,#29432,#29433,
#29434,#29435,#29436,#29437,#29438,#29439,#29440,#29441,#29442,#29443,#29444,
#29445,#29446,#29447,#29448,#29449,#29450,#29451,#29452,#29453,#29454,#29455,
#29456,#29457,#29458,#29459),.UNSPECIFIED.,.F.,.F.,(4,3,3,3,3,3,3,3,3,3,
3,3,3,3,3,3,3,3,3,3,3,3,3,3,3,3,3,3,3,3,3,3,3,3,3,3,3,3,3,3,3,3,3,3,3,3,
3,3,3,3,3,3,3,3,3,3,3,3,3,3,3,3,3,3,3,3,3,3,3,3,3,3,3,3,3,3,4),(512.079602535137,
512.162447478009,512.245261499868,512.328061801061,512.410866989149,512.493695671928,
512.576614950116,512.659584111197,512.742679148104,512.792591477812,512.876338210514,
512.95998188753,513.043542631596,513.127040493553,513.210502994115,513.293948129608,
513.37739396445,513.460858559689,513.544411745111,513.628009578683,513.711741141545,
513.791574980011,513.875321712713,513.958965389729,514.042526133795,514.126023995752,
514.209486496315,514.292931631807,514.37637746665,514.459842061888,514.54339524731,
514.626993080883,514.710724643744,514.79055848221,514.874305214912,514.957948891928,
515.041509635994,515.125007497951,515.208469998513,515.291915134005,515.375360968848,
515.458825564086,515.542378749508,515.625976583081,515.709708145942,515.789541984409,
515.873288717111,515.956932394127,516.040493138193,516.12399100015,516.207453500713,
516.290898636205,516.374344471048,516.457809066286,516.541362251708,516.62496008528,
516.708691648142,516.788525486608,516.87227221931,516.955915896326,517.039476640392,
517.122974502349,517.206437002912,517.289882138404,517.373327973246,517.456792568485,
517.540345753906,517.623943587479,517.707675150341,517.787508988807,517.873089538018,
517.958551346935,518.043909947176,518.129158670079,518.21434289738,518.299470899801,
518.362787842316),.UNSPECIFIED.);
#335=B_SPLINE_CURVE_WITH_KNOTS('',3,(#29461,#29462,#29463,#29464,#29465,
#29466,#29467,#29468,#29469,#29470,#29471,#29472,#29473,#29474,#29475,#29476,
#29477,#29478,#29479,#29480,#29481,#29482,#29483,#29484,#29485,#29486,#29487,
#29488,#29489,#29490,#29491,#29492,#29493,#29494,#29495,#29496,#29497,#29498,
#29499,#29500,#29501,#29502,#29503,#29504,#29505,#29506,#29507,#29508,#29509,
#29510,#29511,#29512,#29513,#29514,#29515,#29516,#29517,#29518,#29519,#29520,
#29521,#29522,#29523,#29524,#29525,#29526,#29527,#29528,#29529,#29530,#29531,
#29532,#29533,#29534,#29535,#29536,#29537,#29538,#29539,#29540,#29541,#29542,
#29543,#29544,#29545,#29546,#29547,#29548,#29549,#29550,#29551,#29552,#29553,
#29554,#29555,#29556,#29557,#29558,#29559,#29560,#29561,#29562,#29563,#29564,
#29565,#29566,#29567,#29568,#29569,#29570,#29571,#29572,#29573,#29574,#29575,
#29576,#29577,#29578,#29579,#29580,#29581,#29582,#29583,#29584,#29585,#29586,
#29587,#29588,#29589,#29590,#29591,#29592,#29593,#29594,#29595,#29596,#29597,
#29598,#29599,#29600,#29601,#29602,#29603,#29604,#29605,#29606,#29607,#29608,
#29609,#29610,#29611,#29612,#29613,#29614,#29615,#29616,#29617,#29618,#29619,
#29620,#29621,#29622,#29623,#29624,#29625,#29626,#29627,#29628,#29629,#29630,
#29631,#29632,#29633,#29634,#29635,#29636,#29637,#29638,#29639,#29640,#29641,
#29642,#29643,#29644,#29645,#29646,#29647,#29648,#29649,#29650,#29651,#29652,
#29653,#29654,#29655,#29656,#29657,#29658,#29659,#29660,#29661,#29662,#29663,
#29664,#29665,#29666,#29667,#29668,#29669,#29670,#29671,#29672,#29673,#29674,
#29675,#29676,#29677,#29678,#29679,#29680,#29681,#29682,#29683,#29684,#29685,
#29686,#29687,#29688,#29689),.UNSPECIFIED.,.F.,.F.,(4,3,3,3,3,3,3,3,3,3,
3,3,3,3,3,3,3,3,3,3,3,3,3,3,3,3,3,3,3,3,3,3,3,3,3,3,3,3,3,3,3,3,3,3,3,3,
3,3,3,3,3,3,3,3,3,3,3,3,3,3,3,3,3,3,3,3,3,3,3,3,3,3,3,3,3,3,4),(505.796417227957,
505.799706962417,505.883453695119,505.967097372135,506.050658116202,506.134155978159,
506.217618478722,506.301063614214,506.384509449057,506.467974044295,506.551527229718,
506.63512506329,506.718856626153,506.798690464617,506.882437197319,506.966080874335,
507.049641618401,507.133139480358,507.21660198092,507.300047116413,507.383492951256,
507.466957546494,507.550510731915,507.634108565488,507.71784012835,507.797673966816,
507.881420699518,507.965064376533,508.0486251206,508.132122982556,508.215585483119,
508.299030618611,508.382476453454,508.465941048692,508.549494234113,508.633092067686,
508.716823630547,508.796657469015,508.880404201717,508.964047878733,509.0476086228,
509.131106484756,509.214568985319,509.298014120812,509.381459955655,509.464924550893,
509.548477736315,509.632075569888,509.71580713275,509.795640971214,509.879387703916,
509.963031380931,510.046592124998,510.130089986954,510.213552487517,510.296997623009,
510.380443457852,510.46390805309,510.547461238512,510.631059072084,510.714790634946,
510.794624473413,510.878371206115,510.962014883131,511.045575627198,511.129073489155,
511.212535989718,511.295981125211,511.379426960054,511.462891555292,511.546444740714,
511.630042574287,511.713774137149,511.793607975613,511.897484169068,511.99988621917,
512.079602535015),.UNSPECIFIED.);
#336=B_SPLINE_CURVE_WITH_KNOTS('',3,(#29691,#29692,#29693,#29694,#29695,
#29696,#29697,#29698,#29699,#29700,#29701,#29702,#29703,#29704,#29705,#29706,
#29707,#29708,#29709,#29710,#29711,#29712,#29713,#29714,#29715,#29716,#29717,
#29718,#29719,#29720,#29721,#29722,#29723,#29724,#29725,#29726,#29727,#29728,
#29729,#29730,#29731,#29732,#29733,#29734,#29735,#29736,#29737,#29738,#29739,
#29740,#29741,#29742,#29743,#29744,#29745,#29746,#29747,#29748,#29749,#29750,
#29751,#29752,#29753,#29754,#29755,#29756,#29757,#29758,#29759,#29760,#29761,
#29762,#29763,#29764,#29765,#29766,#29767,#29768,#29769,#29770,#29771,#29772,
#29773,#29774,#29775,#29776,#29777,#29778,#29779,#29780,#29781,#29782,#29783,
#29784,#29785,#29786,#29787,#29788,#29789,#29790,#29791,#29792,#29793,#29794,
#29795,#29796,#29797,#29798,#29799,#29800,#29801,#29802,#29803,#29804,#29805,
#29806,#29807,#29808,#29809,#29810,#29811,#29812,#29813,#29814,#29815,#29816,
#29817,#29818,#29819,#29820,#29821,#29822,#29823,#29824,#29825,#29826,#29827,
#29828,#29829,#29830,#29831,#29832,#29833,#29834,#29835,#29836,#29837,#29838,
#29839,#29840,#29841,#29842,#29843,#29844,#29845,#29846,#29847,#29848,#29849,
#29850,#29851,#29852,#29853,#29854,#29855,#29856,#29857,#29858,#29859,#29860,
#29861,#29862,#29863,#29864,#29865,#29866,#29867,#29868,#29869,#29870,#29871,
#29872,#29873,#29874,#29875,#29876,#29877,#29878,#29879,#29880,#29881,#29882,
#29883,#29884,#29885,#29886,#29887,#29888,#29889,#29890,#29891,#29892,#29893,
#29894,#29895,#29896,#29897,#29898,#29899,#29900,#29901,#29902,#29903,#29904,
#29905,#29906,#29907,#29908,#29909,#29910,#29911,#29912,#29913,#29914,#29915,
#29916),.UNSPECIFIED.,.F.,.F.,(4,3,3,3,3,3,3,3,3,3,3,3,3,3,3,3,3,3,3,3,
3,3,3,3,3,3,3,3,3,3,3,3,3,3,3,3,3,3,3,3,3,3,3,3,3,3,3,3,3,3,3,3,3,3,3,3,
3,3,3,3,3,3,3,3,3,3,3,3,3,3,3,3,3,3,3,4),(499.513231920912,499.614580001576,
499.717352199052,499.805805949222,499.889552681924,499.97319635894,500.056757103006,
500.140254964963,500.223717465526,500.307162601018,500.390608435861,500.474073031099,
500.557626216521,500.641224050093,500.724955612955,500.804789451422,500.888536184124,
500.97217986114,501.055740605206,501.139238467163,501.222700967726,501.306146103218,
501.389591938061,501.473056533299,501.556609718721,501.640207552293,501.723939115155,
501.803772953621,501.887519686323,501.971163363339,502.054724107405,502.138221969362,
502.221684469925,502.305129605417,502.38857544026,502.472040035498,502.55559322092,
502.639191054493,502.722922617355,502.80275645582,502.886503188522,502.970146865538,
503.053707609604,503.137205471561,503.220667972123,503.304113107615,503.387558942458,
503.471023537696,503.554576723118,503.63817455669,503.721906119552,503.801739958019,
503.885486690721,503.969130367737,504.052691111803,504.13618897376,504.219651474323,
504.303096609815,504.386542444658,504.470007039896,504.553560225318,504.63715805889,
504.720889621752,504.800723460218,504.884420596488,504.968014701809,505.051525952777,
505.134974453708,505.218387813693,505.301784027289,505.385181206877,505.468597461663,
505.552102310251,505.635652182034,505.719334882353,505.796417227828),
 .UNSPECIFIED.);
#337=B_SPLINE_CURVE_WITH_KNOTS('',3,(#29918,#29919,#29920,#29921,#29922,
#29923,#29924,#29925,#29926,#29927,#29928,#29929,#29930,#29931,#29932,#29933,
#29934,#29935,#29936,#29937,#29938,#29939,#29940,#29941,#29942,#29943,#29944,
#29945,#29946,#29947,#29948,#29949,#29950,#29951,#29952,#29953,#29954,#29955,
#29956,#29957,#29958,#29959,#29960,#29961,#29962,#29963,#29964,#29965,#29966,
#29967,#29968,#29969,#29970,#29971,#29972,#29973,#29974,#29975,#29976,#29977,
#29978,#29979,#29980,#29981,#29982,#29983,#29984,#29985,#29986,#29987,#29988,
#29989,#29990,#29991,#29992,#29993,#29994,#29995,#29996,#29997,#29998,#29999,
#30000,#30001,#30002,#30003,#30004,#30005,#30006,#30007,#30008,#30009,#30010,
#30011,#30012,#30013,#30014,#30015,#30016,#30017,#30018,#30019,#30020,#30021,
#30022,#30023,#30024,#30025,#30026,#30027,#30028,#30029,#30030,#30031,#30032,
#30033,#30034,#30035,#30036,#30037,#30038,#30039,#30040,#30041,#30042,#30043,
#30044,#30045,#30046,#30047,#30048,#30049,#30050,#30051,#30052,#30053,#30054,
#30055,#30056,#30057,#30058,#30059,#30060,#30061,#30062,#30063,#30064,#30065,
#30066,#30067,#30068,#30069,#30070,#30071,#30072,#30073,#30074,#30075,#30076,
#30077,#30078,#30079,#30080,#30081,#30082,#30083,#30084,#30085,#30086,#30087,
#30088,#30089,#30090,#30091,#30092,#30093,#30094,#30095,#30096,#30097,#30098,
#30099,#30100,#30101,#30102,#30103,#30104,#30105,#30106,#30107,#30108,#30109,
#30110,#30111,#30112,#30113,#30114,#30115,#30116,#30117,#30118,#30119,#30120,
#30121,#30122,#30123,#30124,#30125,#30126,#30127,#30128,#30129,#30130,#30131,
#30132,#30133,#30134,#30135,#30136,#30137,#30138,#30139,#30140,#30141,#30142,
#30143,#30144,#30145,#30146),.UNSPECIFIED.,.F.,.F.,(4,3,3,3,3,3,3,3,3,3,
3,3,3,3,3,3,3,3,3,3,3,3,3,3,3,3,3,3,3,3,3,3,3,3,3,3,3,3,3,3,3,3,3,3,3,3,
3,3,3,3,3,3,3,3,3,3,3,3,3,3,3,3,3,3,3,3,3,3,3,3,3,3,3,3,3,3,4),(493.230046613598,
493.315013376264,493.400014227616,493.485064766745,493.570242771312,493.655487738022,
493.740890152444,493.811904936027,493.895651668729,493.979295345745,494.062856089812,
494.146353951769,494.229816452331,494.313261587824,494.396707422666,494.480172017904,
494.563725203326,494.647323036899,494.731054599761,494.810888438227,494.894635170929,
494.978278847945,495.061839592012,495.145337453968,495.228799954531,495.312245090023,
495.395690924866,495.479155520104,495.562708705526,495.646306539099,495.73003810196,
495.809871940426,495.893618673128,495.977262350144,496.06082309421,496.144320956166,
496.227783456729,496.311228592221,496.394674427064,496.478139022302,496.561692207724,
496.645290041296,496.729021604158,496.808855442625,496.892602175327,496.976245852343,
497.059806596409,497.143304458366,497.226766958929,497.310212094421,497.393657929264,
497.477122524502,497.560675709924,497.644273543496,497.728005106358,497.807838944824,
497.891585677526,497.975229354542,498.058790098609,498.142287960565,498.225750461128,
498.30919559662,498.392641431463,498.476106026701,498.559659212123,498.643257045696,
498.726988608558,498.806822447023,498.890011507484,498.973066630021,499.056044292387,
499.138963145046,499.221841791247,499.304713405022,499.387580210261,499.470486066474,
499.513231920778),.UNSPECIFIED.);
#338=B_SPLINE_CURVE_WITH_KNOTS('',3,(#30148,#30149,#30150,#30151,#30152,
#30153,#30154,#30155,#30156,#30157,#30158,#30159,#30160,#30161,#30162,#30163,
#30164,#30165,#30166,#30167,#30168,#30169,#30170,#30171,#30172,#30173,#30174,
#30175,#30176,#30177,#30178,#30179,#30180,#30181,#30182,#30183,#30184,#30185,
#30186,#30187,#30188,#30189,#30190,#30191,#30192,#30193,#30194,#30195,#30196,
#30197,#30198,#30199,#30200,#30201,#30202,#30203,#30204,#30205,#30206,#30207,
#30208,#30209,#30210,#30211,#30212,#30213,#30214,#30215,#30216,#30217,#30218,
#30219,#30220,#30221,#30222,#30223,#30224,#30225,#30226,#30227,#30228,#30229,
#30230,#30231,#30232,#30233,#30234,#30235,#30236,#30237,#30238,#30239,#30240,
#30241,#30242,#30243,#30244,#30245,#30246,#30247,#30248,#30249,#30250,#30251,
#30252,#30253,#30254,#30255,#30256,#30257,#30258,#30259,#30260,#30261,#30262,
#30263,#30264,#30265,#30266,#30267,#30268,#30269,#30270,#30271,#30272,#30273,
#30274,#30275,#30276,#30277,#30278,#30279,#30280,#30281,#30282,#30283,#30284,
#30285,#30286,#30287,#30288,#30289,#30290,#30291,#30292,#30293,#30294,#30295,
#30296,#30297,#30298,#30299,#30300,#30301,#30302,#30303,#30304,#30305,#30306,
#30307,#30308,#30309,#30310,#30311,#30312,#30313,#30314,#30315,#30316,#30317,
#30318,#30319,#30320,#30321,#30322,#30323,#30324,#30325,#30326,#30327,#30328,
#30329,#30330,#30331,#30332,#30333,#30334,#30335,#30336,#30337,#30338,#30339,
#30340,#30341,#30342,#30343,#30344,#30345,#30346,#30347,#30348,#30349,#30350,
#30351,#30352,#30353,#30354,#30355,#30356,#30357,#30358,#30359,#30360,#30361,
#30362,#30363,#30364,#30365,#30366,#30367,#30368,#30369,#30370,#30371,#30372,
#30373,#30374,#30375,#30376),.UNSPECIFIED.,.F.,.F.,(4,3,3,3,3,3,3,3,3,3,
3,3,3,3,3,3,3,3,3,3,3,3,3,3,3,3,3,3,3,3,3,3,3,3,3,3,3,3,3,3,3,3,3,3,3,3,
3,3,3,3,3,3,3,3,3,3,3,3,3,3,3,3,3,3,3,3,3,3,3,3,3,3,3,3,3,3,4),(486.946861306547,
487.029354407844,487.111760521916,487.194100759532,487.276402556392,487.358686132498,
487.440970475139,487.523274569938,487.605664188744,487.688101102786,487.770659626157,
487.818003922832,487.901750655534,487.98539433255,488.068955076616,488.152452938574,
488.235915439136,488.319360574628,488.402806409471,488.48627100471,488.569824190132,
488.653422023704,488.737153586566,488.816987425032,488.900734157734,488.98437783475,
489.067938578817,489.151436440773,489.234898941336,489.318344076828,489.401789911671,
489.485254506909,489.568807692331,489.652405525903,489.736137088765,489.815970927231,
489.899717659933,489.983361336949,490.066922081015,490.150419942972,490.233882443535,
490.317327579027,490.40077341387,490.484238009108,490.567791194529,490.651389028102,
490.735120590964,490.81495442943,490.898701162132,490.982344839147,491.065905583214,
491.14940344517,491.232865945733,491.316311081225,491.399756916068,491.483221511306,
491.566774696728,491.6503725303,491.734104093162,491.813937931629,491.897684664331,
491.981328341347,492.064889085414,492.148386947371,492.231849447933,492.315294583426,
492.398740418269,492.482205013506,492.565758198928,492.649356032501,492.733087595363,
492.812921433828,492.905016102355,492.99675842005,493.088275305412,493.179434747582,
493.230046613438),.UNSPECIFIED.);
#339=B_SPLINE_CURVE_WITH_KNOTS('',3,(#30378,#30379,#30380,#30381,#30382,
#30383,#30384,#30385,#30386,#30387,#30388,#30389,#30390,#30391,#30392,#30393,
#30394,#30395,#30396,#30397,#30398,#30399,#30400,#30401,#30402,#30403,#30404,
#30405,#30406,#30407,#30408,#30409,#30410,#30411,#30412,#30413,#30414,#30415,
#30416,#30417,#30418,#30419,#30420,#30421,#30422,#30423,#30424,#30425,#30426,
#30427,#30428,#30429,#30430,#30431,#30432,#30433,#30434,#30435,#30436,#30437,
#30438,#30439,#30440,#30441,#30442,#30443,#30444,#30445,#30446,#30447,#30448,
#30449,#30450,#30451,#30452,#30453,#30454,#30455,#30456,#30457,#30458,#30459,
#30460,#30461,#30462,#30463,#30464,#30465,#30466,#30467,#30468,#30469,#30470,
#30471,#30472,#30473,#30474,#30475,#30476,#30477,#30478,#30479,#30480,#30481,
#30482,#30483,#30484,#30485,#30486,#30487,#30488,#30489,#30490,#30491,#30492,
#30493,#30494,#30495,#30496,#30497,#30498,#30499,#30500,#30501,#30502,#30503,
#30504,#30505,#30506,#30507,#30508,#30509,#30510,#30511,#30512,#30513,#30514,
#30515,#30516,#30517,#30518,#30519,#30520,#30521,#30522,#30523,#30524,#30525,
#30526,#30527,#30528,#30529,#30530,#30531,#30532,#30533,#30534,#30535,#30536,
#30537,#30538,#30539,#30540,#30541,#30542,#30543,#30544,#30545,#30546,#30547,
#30548,#30549,#30550,#30551,#30552,#30553,#30554,#30555,#30556,#30557,#30558,
#30559,#30560,#30561,#30562,#30563,#30564,#30565,#30566,#30567,#30568,#30569,
#30570,#30571,#30572,#30573,#30574,#30575,#30576,#30577,#30578,#30579,#30580,
#30581,#30582,#30583,#30584,#30585,#30586,#30587,#30588,#30589,#30590,#30591,
#30592,#30593,#30594,#30595,#30596,#30597,#30598,#30599,#30600,#30601,#30602,
#30603),.UNSPECIFIED.,.F.,.F.,(4,3,3,3,3,3,3,3,3,3,3,3,3,3,3,3,3,3,3,3,
3,3,3,3,3,3,3,3,3,3,3,3,3,3,3,3,3,3,3,3,3,3,3,3,3,3,3,3,3,3,3,3,3,3,3,3,
3,3,3,3,3,3,3,3,3,3,3,3,3,3,3,3,3,3,3,4),(480.663675999239,480.799184202979,
480.825119407438,480.90886614014,480.992509817156,481.076070561222,481.159568423179,
481.243030923742,481.326476059234,481.409921894077,481.493386489315,481.576939674737,
481.66053750831,481.744269071172,481.824102909637,481.907849642339,481.991493319355,
482.075054063422,482.158551925378,482.242014425941,482.325459561433,482.408905396276,
482.492369991514,482.575923176936,482.659521010509,482.743252573371,482.823086411837,
482.906833144539,482.990476821555,483.074037565621,483.157535427578,483.240997928141,
483.324443063633,483.407888898476,483.491353493714,483.574906679136,483.658504512709,
483.742236075571,483.822069914036,483.905816646738,483.989460323754,484.07302106782,
484.156518929777,484.239981430339,484.323426565832,484.406872400674,484.490336995912,
484.573890181334,484.657488014907,484.741219577769,484.821053416235,484.904800148937,
484.988443825953,485.072004570019,485.155502431976,485.238964932539,485.322410068031,
485.405855902874,485.489320498112,485.572873683533,485.656471517106,485.740203079968,
485.820036918434,485.903783651136,485.987427328152,486.070988072219,486.154485934175,
486.237948434738,486.32139357023,486.404839405073,486.488304000312,486.571857185734,
486.655455019306,486.739186582168,486.819020420633,486.946861306418),
 .UNSPECIFIED.);
#340=B_SPLINE_CURVE_WITH_KNOTS('',3,(#30605,#30606,#30607,#30608,#30609,
#30610,#30611,#30612,#30613,#30614,#30615,#30616,#30617,#30618,#30619,#30620,
#30621,#30622,#30623,#30624,#30625,#30626,#30627,#30628,#30629,#30630,#30631,
#30632,#30633,#30634,#30635,#30636,#30637,#30638,#30639,#30640,#30641,#30642,
#30643,#30644,#30645,#30646,#30647,#30648,#30649,#30650,#30651,#30652,#30653,
#30654,#30655,#30656,#30657,#30658,#30659,#30660,#30661,#30662,#30663,#30664,
#30665,#30666,#30667,#30668,#30669,#30670,#30671,#30672,#30673,#30674,#30675,
#30676,#30677,#30678,#30679,#30680,#30681,#30682,#30683,#30684,#30685,#30686,
#30687,#30688,#30689,#30690,#30691,#30692,#30693,#30694,#30695,#30696,#30697,
#30698,#30699,#30700,#30701,#30702,#30703,#30704,#30705,#30706,#30707,#30708,
#30709,#30710,#30711,#30712,#30713,#30714,#30715,#30716,#30717,#30718,#30719,
#30720,#30721,#30722,#30723,#30724,#30725,#30726,#30727,#30728,#30729,#30730,
#30731,#30732,#30733,#30734,#30735,#30736,#30737,#30738,#30739,#30740,#30741,
#30742,#30743,#30744,#30745,#30746,#30747,#30748,#30749,#30750,#30751,#30752,
#30753,#30754,#30755,#30756,#30757,#30758,#30759,#30760,#30761,#30762,#30763,
#30764,#30765,#30766,#30767,#30768,#30769,#30770,#30771,#30772,#30773,#30774,
#30775,#30776,#30777,#30778,#30779,#30780,#30781,#30782,#30783,#30784,#30785,
#30786,#30787,#30788,#30789,#30790,#30791,#30792,#30793,#30794,#30795,#30796,
#30797,#30798,#30799,#30800,#30801,#30802,#30803,#30804,#30805,#30806,#30807,
#30808,#30809,#30810,#30811,#30812,#30813,#30814,#30815,#30816,#30817,#30818,
#30819,#30820,#30821,#30822,#30823,#30824,#30825,#30826,#30827,#30828,#30829,
#30830,#30831,#30832,#30833),.UNSPECIFIED.,.F.,.F.,(4,3,3,3,3,3,3,3,3,3,
3,3,3,3,3,3,3,3,3,3,3,3,3,3,3,3,3,3,3,3,3,3,3,3,3,3,3,3,3,3,3,3,3,3,3,3,
3,3,3,3,3,3,3,3,3,3,3,3,3,3,3,3,3,3,3,3,3,3,3,3,3,3,3,3,3,3,4),(474.38049069216,
474.469894373571,474.560225378739,474.650111625864,474.740665010053,474.831218394243,
474.914965126945,474.998608803961,475.082169548027,475.165667409984,475.249129910547,
475.332575046039,475.416020880882,475.499485476121,475.583038661543,475.666636495115,
475.750368057977,475.830201896442,475.913948629144,475.99759230616,476.081153050227,
476.164650912183,476.248113412746,476.331558548238,476.415004383081,476.49846897832,
476.582022163741,476.665619997314,476.749351560176,476.829185398642,476.912932131344,
476.99657580836,477.080136552426,477.163634414383,477.247096914946,477.330542050438,
477.413987885281,477.497452480519,477.58100566594,477.664603499513,477.748335062375,
477.828168900841,477.911915633543,477.995559310559,478.079120054625,478.162617916582,
478.246080417144,478.329525552637,478.412971387479,478.496435982717,478.579989168139,
478.663587001712,478.747318564574,478.82715240304,478.910899135742,478.994542812758,
479.078103556824,479.161601418781,479.245063919344,479.328509054836,479.411954889679,
479.495419484917,479.578972670339,479.662570503911,479.746302066773,479.826135905239,
479.908635321382,479.991032287064,480.075112751061,480.157365169424,480.239585411973,
480.321792518385,480.407263388548,480.489535156797,480.571843341417,480.654237625803,
480.663675999038),.UNSPECIFIED.);
#341=B_SPLINE_CURVE_WITH_KNOTS('',3,(#30835,#30836,#30837,#30838,#30839,
#30840,#30841,#30842,#30843,#30844,#30845,#30846,#30847,#30848,#30849,#30850,
#30851,#30852,#30853,#30854,#30855,#30856,#30857,#30858,#30859,#30860,#30861,
#30862,#30863,#30864,#30865,#30866,#30867,#30868,#30869,#30870,#30871,#30872,
#30873,#30874,#30875,#30876,#30877,#30878,#30879,#30880,#30881,#30882,#30883,
#30884,#30885,#30886,#30887,#30888,#30889,#30890,#30891,#30892,#30893,#30894,
#30895,#30896,#30897,#30898,#30899,#30900,#30901,#30902,#30903,#30904,#30905,
#30906,#30907,#30908,#30909,#30910,#30911,#30912,#30913,#30914,#30915,#30916,
#30917,#30918,#30919,#30920,#30921,#30922,#30923,#30924,#30925,#30926,#30927,
#30928,#30929,#30930,#30931,#30932,#30933,#30934,#30935,#30936,#30937,#30938,
#30939,#30940,#30941,#30942,#30943,#30944,#30945,#30946,#30947,#30948,#30949,
#30950,#30951,#30952,#30953,#30954,#30955,#30956,#30957,#30958,#30959,#30960,
#30961,#30962,#30963,#30964,#30965,#30966,#30967,#30968,#30969,#30970,#30971,
#30972,#30973,#30974,#30975,#30976,#30977,#30978,#30979,#30980,#30981,#30982,
#30983,#30984,#30985,#30986,#30987,#30988,#30989,#30990,#30991,#30992,#30993,
#30994,#30995,#30996,#30997,#30998,#30999,#31000,#31001,#31002,#31003,#31004,
#31005,#31006,#31007,#31008,#31009,#31010,#31011,#31012,#31013,#31014,#31015,
#31016,#31017,#31018,#31019,#31020,#31021,#31022,#31023,#31024,#31025,#31026,
#31027,#31028,#31029,#31030,#31031,#31032,#31033,#31034,#31035,#31036,#31037,
#31038,#31039,#31040,#31041,#31042,#31043,#31044,#31045,#31046,#31047,#31048,
#31049,#31050,#31051,#31052,#31053,#31054,#31055,#31056,#31057,#31058,#31059,
#31060,#31061,#31062,#31063),.UNSPECIFIED.,.F.,.F.,(4,3,3,3,3,3,3,3,3,3,
3,3,3,3,3,3,3,3,3,3,3,3,3,3,3,3,3,3,3,3,3,3,3,3,3,3,3,3,3,3,3,3,3,3,3,3,
3,3,3,3,3,3,3,3,3,3,3,3,3,3,3,3,3,3,3,3,3,3,3,3,3,3,3,3,3,3,4),(468.09730538488,
468.179935268047,468.262520399752,468.34508270027,468.427640970441,468.510214005244,
468.592871668108,468.675571756588,468.758404179363,468.837317381048,468.92106411375,
469.004707790766,469.088268534832,469.171766396789,469.255228897352,469.338674032844,
469.422119867687,469.505584462925,469.589137648347,469.672735481919,469.756467044781,
469.836300883247,469.920047615949,470.003691292965,470.087252037032,470.170749898988,
470.254212399551,470.337657535043,470.421103369886,470.504567965124,470.588121150545,
470.671718984118,470.75545054698,470.835284385447,470.919031118149,471.002674795165,
471.086235539232,471.169733401188,471.253195901751,471.336641037243,471.420086872086,
471.503551467325,471.587104652747,471.670702486319,471.754434049181,471.834267887646,
471.918014620348,472.001658297364,472.08521904143,472.168716903387,472.252179403949,
472.335624539442,472.419070374284,472.502534969522,472.586088154944,472.669685988517,
472.753417551379,472.833251389845,472.916998122547,473.000641799562,473.084202543629,
473.167700405586,473.251162906148,473.33460804164,473.418053876483,473.501518471721,
473.585071657143,473.668669490715,473.752401053577,473.832234892044,473.918590158789,
474.004817581131,474.090930999263,474.17691500735,474.262822406883,474.348650729396,
474.380490692059),.UNSPECIFIED.);
#342=B_SPLINE_CURVE_WITH_KNOTS('',3,(#31065,#31066,#31067,#31068,#31069,
#31070,#31071,#31072,#31073,#31074,#31075),.UNSPECIFIED.,.F.,.F.,(4,1,1,
1,1,1,1,1,4),(461.8141200777,461.844432865654,462.843416367853,463.842399870052,
464.841383372252,465.840366874451,466.83935037665,467.838333878849,468.097302840225),
 .UNSPECIFIED.);
#343=B_SPLINE_CURVE_WITH_KNOTS('',3,(#31077,#31078,#31079,#31080,#31081,
#31082,#31083,#31084,#31085,#31086,#31087,#31088,#31089,#31090,#31091,#31092,
#31093,#31094,#31095,#31096,#31097,#31098,#31099,#31100,#31101,#31102,#31103,
#31104,#31105,#31106,#31107,#31108,#31109,#31110,#31111,#31112,#31113,#31114,
#31115,#31116,#31117,#31118,#31119,#31120,#31121,#31122,#31123,#31124,#31125,
#31126,#31127,#31128,#31129,#31130,#31131,#31132,#31133,#31134,#31135,#31136,
#31137,#31138,#31139,#31140,#31141,#31142,#31143,#31144,#31145,#31146,#31147,
#31148,#31149,#31150,#31151,#31152,#31153,#31154,#31155,#31156,#31157,#31158,
#31159,#31160,#31161,#31162,#31163,#31164,#31165,#31166,#31167,#31168,#31169,
#31170,#31171,#31172,#31173,#31174,#31175,#31176,#31177,#31178,#31179,#31180,
#31181,#31182,#31183,#31184,#31185,#31186,#31187,#31188,#31189,#31190,#31191,
#31192,#31193,#31194,#31195,#31196,#31197,#31198,#31199,#31200,#31201,#31202,
#31203,#31204,#31205,#31206,#31207,#31208,#31209,#31210,#31211,#31212,#31213,
#31214,#31215,#31216,#31217,#31218,#31219,#31220,#31221,#31222,#31223,#31224,
#31225,#31226,#31227,#31228,#31229,#31230,#31231,#31232,#31233,#31234,#31235,
#31236,#31237,#31238,#31239,#31240,#31241,#31242,#31243,#31244,#31245,#31246,
#31247,#31248,#31249,#31250,#31251,#31252,#31253,#31254,#31255,#31256,#31257,
#31258,#31259,#31260,#31261,#31262,#31263,#31264,#31265,#31266,#31267,#31268,
#31269,#31270,#31271,#31272,#31273,#31274,#31275,#31276,#31277,#31278,#31279,
#31280,#31281,#31282,#31283,#31284,#31285,#31286,#31287,#31288,#31289,#31290,
#31291,#31292,#31293,#31294,#31295,#31296,#31297,#31298,#31299,#31300,#31301,
#31302,#31303,#31304,#31305),.UNSPECIFIED.,.F.,.F.,(4,3,3,3,3,3,3,3,3,3,
3,3,3,3,3,3,3,3,3,3,3,3,3,3,3,3,3,3,3,3,3,3,3,3,3,3,3,3,3,3,3,3,3,3,3,3,
3,3,3,3,3,3,3,3,3,3,3,3,3,3,3,3,3,3,3,3,3,3,3,3,3,3,3,3,3,3,4),(455.530934770694,
455.629412302043,455.728568331284,455.828470220712,455.850531852459,455.934278585161,
456.017922262177,456.101483006244,456.184980868201,456.268443368763,456.351888504256,
456.435334339098,456.518798934337,456.602352119759,456.685949953331,456.769681516193,
456.849515354658,456.93326208736,457.016905764376,457.100466508443,457.183964370399,
457.267426870962,457.350872006454,457.434317841297,457.517782436535,457.601335621957,
457.68493345553,457.768665018392,457.848498856858,457.93224558956,458.015889266576,
458.099450010642,458.182947872599,458.266410373162,458.349855508654,458.433301343497,
458.516765938735,458.600319124157,458.683916957729,458.767648520591,458.847482359057,
458.931229091759,459.014872768775,459.098433512841,459.181931374798,459.265393875361,
459.348839010853,459.432284845696,459.515749440934,459.599302626355,459.682900459928,
459.76663202279,459.846465861256,459.930212593958,460.013856270974,460.09741701504,
460.180914876997,460.264377377559,460.347822513052,460.431268347895,460.514732943133,
460.598286128554,460.681883962127,460.765615524989,460.845449363455,460.92877944253,
461.012006735704,461.095151789752,461.178235075274,461.261284625204,461.344318559843,
461.427355319168,461.510413341538,461.593559004726,461.676752316929,461.760069949751,
461.814119801522),.UNSPECIFIED.);
#344=B_SPLINE_CURVE_WITH_KNOTS('',3,(#31307,#31308,#31309,#31310,#31311,
#31312,#31313,#31314,#31315,#31316,#31317,#31318,#31319,#31320,#31321,#31322,
#31323,#31324,#31325,#31326,#31327,#31328,#31329,#31330,#31331,#31332,#31333,
#31334,#31335,#31336,#31337,#31338,#31339,#31340,#31341,#31342,#31343,#31344,
#31345,#31346,#31347,#31348,#31349,#31350,#31351,#31352,#31353,#31354,#31355,
#31356,#31357,#31358,#31359,#31360,#31361,#31362,#31363,#31364,#31365,#31366,
#31367,#31368,#31369,#31370,#31371,#31372,#31373,#31374,#31375,#31376,#31377,
#31378,#31379,#31380,#31381,#31382,#31383,#31384,#31385,#31386,#31387,#31388,
#31389,#31390,#31391,#31392,#31393,#31394,#31395,#31396,#31397,#31398,#31399,
#31400,#31401,#31402,#31403,#31404,#31405,#31406,#31407,#31408,#31409,#31410,
#31411,#31412,#31413,#31414,#31415,#31416,#31417,#31418,#31419,#31420,#31421,
#31422,#31423,#31424,#31425,#31426,#31427,#31428,#31429,#31430,#31431,#31432,
#31433,#31434,#31435,#31436,#31437,#31438,#31439,#31440,#31441,#31442,#31443,
#31444,#31445,#31446,#31447,#31448,#31449,#31450,#31451,#31452,#31453,#31454,
#31455,#31456,#31457,#31458,#31459,#31460,#31461,#31462,#31463,#31464,#31465,
#31466,#31467,#31468,#31469,#31470,#31471,#31472,#31473,#31474,#31475,#31476,
#31477,#31478,#31479,#31480,#31481,#31482,#31483,#31484,#31485,#31486,#31487,
#31488,#31489,#31490,#31491,#31492,#31493,#31494,#31495,#31496,#31497,#31498,
#31499,#31500,#31501,#31502,#31503,#31504,#31505,#31506,#31507,#31508,#31509,
#31510,#31511,#31512,#31513,#31514,#31515,#31516,#31517,#31518,#31519,#31520,
#31521,#31522,#31523,#31524,#31525,#31526,#31527,#31528,#31529,#31530,#31531,
#31532,#31533,#31534,#31535,#31536,#31537,#31538),.UNSPECIFIED.,.F.,.F.,
(4,3,3,3,3,3,3,3,3,3,3,3,3,3,3,3,3,3,3,3,3,3,3,3,3,3,3,3,3,3,3,3,3,3,3,
3,3,3,3,3,3,3,3,3,3,3,3,3,3,3,3,3,3,3,3,3,3,3,3,3,3,3,3,3,3,3,3,3,3,3,3,
3,3,3,3,3,3,4),(449.247749463341,449.332121367645,449.416509550338,449.500930709019,
449.585401559849,449.669989170282,449.75464620782,449.839434812469,449.856630839264,
449.940377571966,450.024021248982,450.107581993048,450.191079855005,450.274542355568,
450.35798749106,450.441433325903,450.524897921141,450.608451106563,450.692048940136,
450.775780502997,450.855614341463,450.939361074165,451.023004751181,451.106565495247,
451.190063357204,451.273525857767,451.356970993259,451.440416828102,451.52388142334,
451.607434608761,451.691032442334,451.774764005196,451.854597843663,451.938344576365,
452.021988253381,452.105548997447,452.189046859404,452.272509359966,452.355954495459,
452.439400330302,452.52286492554,452.606418110962,452.690015944534,452.773747507396,
452.853581345862,452.937328078564,453.02097175558,453.104532499646,453.188030361602,
453.271492862165,453.354937997657,453.438383832499,453.521848427737,453.605401613159,
453.688999446732,453.772731009594,453.852564848061,453.936311580763,454.019955257779,
454.103516001846,454.187013863803,454.270476364365,454.353921499858,454.4373673347,
454.520831929939,454.604385115361,454.687982948933,454.771714511795,454.85154835026,
454.936471652793,455.019865229954,455.103178641182,455.186430241413,455.27255637369,
455.355747822368,455.438931987459,455.522140523525,455.530934770521),
 .UNSPECIFIED.);
#345=B_SPLINE_CURVE_WITH_KNOTS('',3,(#31540,#31541,#31542,#31543,#31544,
#31545,#31546,#31547,#31548,#31549,#31550,#31551,#31552,#31553,#31554,#31555,
#31556,#31557,#31558,#31559,#31560,#31561,#31562,#31563,#31564,#31565,#31566,
#31567,#31568,#31569,#31570,#31571,#31572,#31573,#31574,#31575,#31576,#31577,
#31578,#31579,#31580,#31581,#31582,#31583,#31584,#31585,#31586,#31587,#31588,
#31589,#31590,#31591,#31592,#31593,#31594,#31595,#31596,#31597,#31598,#31599,
#31600,#31601,#31602,#31603,#31604,#31605,#31606,#31607,#31608,#31609,#31610,
#31611,#31612,#31613,#31614,#31615,#31616,#31617,#31618,#31619,#31620,#31621,
#31622,#31623,#31624,#31625,#31626,#31627,#31628,#31629,#31630,#31631,#31632,
#31633,#31634,#31635,#31636,#31637,#31638,#31639,#31640,#31641,#31642,#31643,
#31644,#31645,#31646,#31647,#31648,#31649,#31650,#31651,#31652,#31653,#31654,
#31655,#31656,#31657,#31658,#31659,#31660,#31661,#31662,#31663,#31664,#31665,
#31666,#31667,#31668,#31669,#31670,#31671,#31672,#31673,#31674,#31675,#31676,
#31677,#31678,#31679,#31680,#31681,#31682,#31683,#31684,#31685,#31686,#31687,
#31688,#31689,#31690,#31691,#31692,#31693,#31694,#31695,#31696,#31697,#31698,
#31699,#31700,#31701,#31702,#31703,#31704,#31705,#31706,#31707,#31708,#31709,
#31710,#31711,#31712,#31713,#31714,#31715,#31716,#31717,#31718,#31719,#31720,
#31721,#31722,#31723,#31724,#31725,#31726,#31727,#31728,#31729,#31730,#31731,
#31732,#31733,#31734,#31735,#31736,#31737,#31738,#31739,#31740,#31741,#31742,
#31743,#31744,#31745,#31746,#31747,#31748,#31749,#31750,#31751,#31752,#31753,
#31754,#31755,#31756,#31757,#31758,#31759,#31760,#31761,#31762,#31763,#31764,
#31765,#31766,#31767,#31768),.UNSPECIFIED.,.F.,.F.,(4,3,3,3,3,3,3,3,3,3,
3,3,3,3,3,3,3,3,3,3,3,3,3,3,3,3,3,3,3,3,3,3,3,3,3,3,3,3,3,3,3,3,3,3,3,3,
3,3,3,3,3,3,3,3,3,3,3,3,3,3,3,3,3,3,3,3,3,3,3,3,3,3,3,3,3,3,4),(442.964564156297,
443.047208221643,443.129759939605,443.212240350628,443.294675061561,443.377086506837,
443.459493597428,443.541915238339,443.624420188387,443.706967604258,443.789644235641,
443.862729826069,443.946476558771,444.030120235787,444.113680979854,444.19717884181,
444.280641342373,444.364086477865,444.447532312708,444.530996907947,444.614550093369,
444.698147926941,444.781879489803,444.861713328268,444.94546006097,445.029103737986,
445.112664482052,445.19616234401,445.279624844572,445.363069980065,445.446515814908,
445.529980410146,445.613533595568,445.697131429141,445.780862992003,445.860696830468,
445.94444356317,446.028087240186,446.111647984252,446.195145846209,446.278608346771,
446.362053482264,446.445499317107,446.528963912345,446.612517097766,446.696114931339,
446.779846494201,446.859680332667,446.943427065369,447.027070742385,447.110631486451,
447.194129348408,447.27759184897,447.361036984462,447.444482819305,447.527947414543,
447.611500599965,447.695098433538,447.7788299964,447.858663834866,447.942410567568,
448.026054244584,448.10961498865,448.193112850607,448.276575351169,448.360020486662,
448.443466321505,448.526930916743,448.610484102165,448.694081935738,448.7778134986,
448.857647337065,448.955172868587,449.048592193972,449.141721584224,449.234411531842,
449.247749463153),.UNSPECIFIED.);
#346=B_SPLINE_CURVE_WITH_KNOTS('',3,(#31770,#31771,#31772,#31773,#31774,
#31775,#31776,#31777,#31778,#31779,#31780,#31781,#31782,#31783,#31784,#31785,
#31786,#31787,#31788,#31789,#31790,#31791,#31792,#31793,#31794,#31795,#31796,
#31797,#31798,#31799,#31800,#31801,#31802,#31803,#31804,#31805,#31806,#31807,
#31808,#31809,#31810,#31811,#31812,#31813,#31814,#31815,#31816,#31817,#31818,
#31819,#31820,#31821,#31822,#31823,#31824,#31825,#31826,#31827,#31828,#31829,
#31830,#31831,#31832,#31833,#31834,#31835,#31836,#31837,#31838,#31839,#31840,
#31841,#31842,#31843,#31844,#31845,#31846,#31847,#31848,#31849,#31850,#31851,
#31852,#31853,#31854,#31855,#31856,#31857,#31858,#31859,#31860,#31861,#31862,
#31863,#31864,#31865,#31866,#31867,#31868,#31869,#31870,#31871,#31872,#31873,
#31874,#31875,#31876,#31877,#31878,#31879,#31880,#31881,#31882,#31883,#31884,
#31885,#31886,#31887,#31888,#31889,#31890,#31891,#31892,#31893,#31894,#31895,
#31896,#31897,#31898,#31899,#31900,#31901,#31902,#31903,#31904,#31905,#31906,
#31907,#31908,#31909,#31910,#31911,#31912,#31913,#31914,#31915,#31916,#31917,
#31918,#31919,#31920,#31921,#31922,#31923,#31924,#31925,#31926,#31927,#31928,
#31929,#31930,#31931,#31932,#31933,#31934,#31935,#31936,#31937,#31938,#31939,
#31940,#31941,#31942,#31943,#31944,#31945,#31946,#31947,#31948,#31949,#31950,
#31951,#31952,#31953,#31954,#31955,#31956,#31957,#31958,#31959,#31960,#31961,
#31962,#31963,#31964,#31965,#31966,#31967,#31968,#31969,#31970,#31971,#31972,
#31973,#31974,#31975,#31976,#31977,#31978,#31979,#31980,#31981,#31982,#31983,
#31984,#31985,#31986,#31987,#31988,#31989,#31990,#31991,#31992,#31993,#31994,
#31995),.UNSPECIFIED.,.F.,.F.,(4,3,3,3,3,3,3,3,3,3,3,3,3,3,3,3,3,3,3,3,
3,3,3,3,3,3,3,3,3,3,3,3,3,3,3,3,3,3,3,3,3,3,3,3,3,3,3,3,3,3,3,3,3,3,3,3,
3,3,3,3,3,3,3,3,3,3,3,3,3,3,3,3,3,3,3,4),(436.681378848982,436.805218179798,
436.869845310675,436.953592043377,437.037235720393,437.12079646446,437.204294326416,
437.287756826979,437.371201962471,437.454647797314,437.538112392552,437.621665577974,
437.705263411547,437.788994974409,437.868828812874,437.952575545576,438.036219222592,
438.119779966658,438.203277828615,438.286740329178,438.37018546467,438.453631299513,
438.537095894751,438.620649080173,438.704246913745,438.787978476607,438.867812315073,
438.951559047775,439.035202724791,439.118763468857,439.202261330814,439.285723831377,
439.369168966869,439.452614801712,439.53607939695,439.619632582372,439.703230415945,
439.786961978807,439.866795817273,439.950542549975,440.034186226991,440.117746971057,
440.201244833014,440.284707333577,440.368152469069,440.451598303912,440.53506289915,
440.618616084572,440.702213918145,440.785945481007,440.865779319472,440.949526052174,
441.03316972919,441.116730473256,441.200228335213,441.283690835775,441.367135971268,
441.450581806111,441.534046401348,441.61759958677,441.701197420343,441.784928983205,
441.864762821671,441.948509554373,442.032153231388,442.115713975455,442.199211837411,
442.282674337974,442.366119473466,442.449565308309,442.533029903547,442.616583088969,
442.700180922541,442.783912485403,442.86374632387,442.964564156162),
 .UNSPECIFIED.);
#347=B_SPLINE_CURVE_WITH_KNOTS('',3,(#31997,#31998,#31999,#32000,#32001,
#32002,#32003,#32004,#32005,#32006,#32007,#32008,#32009,#32010,#32011,#32012,
#32013,#32014,#32015,#32016,#32017,#32018,#32019,#32020,#32021,#32022,#32023,
#32024,#32025,#32026,#32027,#32028,#32029,#32030,#32031,#32032,#32033,#32034,
#32035,#32036,#32037,#32038,#32039,#32040,#32041,#32042,#32043,#32044,#32045,
#32046,#32047,#32048,#32049,#32050,#32051,#32052,#32053,#32054,#32055,#32056,
#32057,#32058,#32059,#32060,#32061,#32062,#32063,#32064,#32065,#32066,#32067,
#32068,#32069,#32070,#32071,#32072,#32073,#32074,#32075,#32076,#32077,#32078,
#32079,#32080,#32081,#32082,#32083,#32084,#32085,#32086,#32087,#32088,#32089,
#32090,#32091,#32092,#32093,#32094,#32095,#32096,#32097,#32098,#32099,#32100,
#32101,#32102,#32103,#32104,#32105,#32106,#32107,#32108,#32109,#32110,#32111,
#32112,#32113,#32114,#32115,#32116,#32117,#32118,#32119,#32120,#32121,#32122,
#32123,#32124,#32125,#32126,#32127,#32128,#32129,#32130,#32131,#32132,#32133,
#32134,#32135,#32136,#32137,#32138,#32139,#32140,#32141,#32142,#32143,#32144,
#32145,#32146,#32147,#32148,#32149,#32150,#32151,#32152,#32153,#32154,#32155,
#32156,#32157,#32158,#32159,#32160,#32161,#32162,#32163,#32164,#32165,#32166,
#32167,#32168,#32169,#32170,#32171,#32172,#32173,#32174,#32175,#32176,#32177,
#32178,#32179,#32180,#32181,#32182,#32183,#32184,#32185,#32186,#32187,#32188,
#32189,#32190,#32191,#32192,#32193,#32194,#32195,#32196,#32197,#32198,#32199,
#32200,#32201,#32202,#32203,#32204,#32205,#32206,#32207,#32208,#32209,#32210,
#32211,#32212,#32213,#32214,#32215,#32216,#32217,#32218,#32219,#32220,#32221,
#32222,#32223,#32224,#32225),.UNSPECIFIED.,.F.,.F.,(4,3,3,3,3,3,3,3,3,3,
3,3,3,3,3,3,3,3,3,3,3,3,3,3,3,3,3,3,3,3,3,3,3,3,3,3,3,3,3,3,3,3,3,3,3,3,
3,3,3,3,3,3,3,3,3,3,3,3,3,3,3,3,3,3,3,3,3,3,3,3,3,3,3,3,3,3,4),(430.398193541985,
430.486432197338,430.574817646461,430.66344055964,430.752192696424,430.84115178814,
430.87594429748,430.959691030182,431.043334707198,431.126895451264,431.210393313221,
431.293855813784,431.377300949276,431.460746784119,431.544211379357,431.627764564778,
431.711362398351,431.795093961213,431.874927799679,431.958674532381,432.042318209397,
432.125878953464,432.20937681542,432.292839315983,432.376284451475,432.459730286318,
432.543194881556,432.626748066978,432.710345900551,432.794077463413,432.873911301878,
432.95765803458,433.041301711596,433.124862455662,433.208360317619,433.291822818182,
433.375267953674,433.458713788517,433.542178383755,433.625731569177,433.709329402749,
433.793060965611,433.872894804078,433.95664153678,434.040285213796,434.123845957862,
434.207343819819,434.290806320382,434.374251455874,434.457697290717,434.541161885955,
434.624715071377,434.70831290495,434.792044467812,434.871878306277,434.955625038979,
435.039268715995,435.122829460061,435.206327322018,435.289789822581,435.373234958073,
435.456680792916,435.540145388154,435.623698573575,435.707296407148,435.79102797001,
435.870861808476,435.953377350882,436.035790000206,436.118109323625,436.200376371044,
436.282610205523,436.364829859162,436.447087832864,436.529363788295,436.611727654349,
436.68137884885),.UNSPECIFIED.);
#348=B_SPLINE_CURVE_WITH_KNOTS('',3,(#32227,#32228,#32229,#32230,#32231,
#32232,#32233,#32234,#32235,#32236,#32237,#32238,#32239,#32240,#32241,#32242,
#32243,#32244,#32245,#32246,#32247,#32248,#32249,#32250,#32251,#32252,#32253,
#32254,#32255,#32256,#32257,#32258,#32259,#32260,#32261,#32262,#32263,#32264,
#32265,#32266,#32267,#32268,#32269,#32270,#32271,#32272,#32273,#32274,#32275,
#32276,#32277,#32278,#32279,#32280,#32281,#32282,#32283,#32284,#32285,#32286,
#32287,#32288,#32289,#32290,#32291,#32292,#32293,#32294,#32295,#32296,#32297,
#32298,#32299,#32300,#32301,#32302,#32303,#32304,#32305,#32306,#32307,#32308,
#32309,#32310,#32311,#32312,#32313,#32314,#32315,#32316,#32317,#32318,#32319,
#32320,#32321,#32322,#32323,#32324,#32325,#32326,#32327,#32328,#32329,#32330,
#32331,#32332,#32333,#32334,#32335,#32336,#32337,#32338,#32339,#32340,#32341,
#32342,#32343,#32344,#32345,#32346,#32347,#32348,#32349,#32350,#32351,#32352,
#32353,#32354,#32355,#32356,#32357,#32358,#32359,#32360,#32361,#32362,#32363,
#32364,#32365,#32366,#32367,#32368,#32369,#32370,#32371,#32372,#32373,#32374,
#32375,#32376,#32377,#32378,#32379,#32380,#32381,#32382,#32383,#32384,#32385,
#32386,#32387,#32388,#32389,#32390,#32391,#32392,#32393,#32394,#32395,#32396,
#32397,#32398,#32399,#32400,#32401,#32402,#32403,#32404,#32405,#32406,#32407,
#32408,#32409,#32410,#32411,#32412,#32413,#32414,#32415,#32416,#32417,#32418,
#32419,#32420,#32421,#32422,#32423,#32424,#32425,#32426,#32427,#32428,#32429,
#32430,#32431,#32432,#32433,#32434,#32435,#32436,#32437,#32438,#32439,#32440,
#32441,#32442,#32443,#32444,#32445,#32446,#32447,#32448,#32449,#32450,#32451,
#32452,#32453,#32454,#32455),.UNSPECIFIED.,.F.,.F.,(4,3,3,3,3,3,3,3,3,3,
3,3,3,3,3,3,3,3,3,3,3,3,3,3,3,3,3,3,3,3,3,3,3,3,3,3,3,3,3,3,3,3,3,3,3,3,
3,3,3,3,3,3,3,3,3,3,3,3,3,3,3,3,3,3,3,3,3,3,3,3,3,3,3,3,3,3,4),(424.1150082348,
424.197489161053,424.283058426457,424.365449984924,424.447830114361,424.530217734788,
424.612631769645,424.695135102409,424.777691588687,424.86036356663,424.882043284285,
424.965790016987,425.049433694003,425.132994438069,425.216492300025,425.299954800588,
425.38339993608,425.466845770923,425.550310366161,425.633863551583,425.717461385156,
425.801192948018,425.881026786484,425.964773519186,426.048417196202,426.131977940269,
426.215475802226,426.298938302788,426.382383438281,426.465829273124,426.549293868362,
426.632847053784,426.716444887356,426.800176450218,426.880010288683,426.963757021385,
427.047400698401,427.130961442467,427.214459304424,427.297921804987,427.381366940479,
427.464812775322,427.54827737056,427.631830555981,427.715428389554,427.799159952416,
427.878993790883,427.962740523585,428.046384200601,428.129944944667,428.213442806624,
428.296905307187,428.380350442679,428.463796277522,428.54726087276,428.630814058182,
428.714411891755,428.798143454617,428.877977293082,428.961724025784,429.0453677028,
429.128928446866,429.212426308823,429.295888809386,429.379333944878,429.462779779721,
429.546244374959,429.629797560381,429.713395393953,429.797126956815,429.876960795281,
429.96420706254,430.051313696243,430.138242590583,430.225067797765,430.311763821276,
430.398193541802),.UNSPECIFIED.);
#349=B_SPLINE_CURVE_WITH_KNOTS('',3,(#32457,#32458,#32459,#32460,#32461,
#32462,#32463,#32464,#32465,#32466,#32467,#32468,#32469,#32470,#32471,#32472,
#32473,#32474,#32475,#32476,#32477,#32478,#32479,#32480,#32481,#32482,#32483,
#32484,#32485,#32486,#32487,#32488,#32489,#32490,#32491,#32492,#32493,#32494,
#32495,#32496,#32497,#32498,#32499,#32500,#32501,#32502,#32503,#32504,#32505,
#32506,#32507,#32508,#32509,#32510,#32511,#32512,#32513,#32514,#32515,#32516,
#32517,#32518,#32519,#32520,#32521,#32522,#32523,#32524,#32525,#32526,#32527,
#32528,#32529,#32530,#32531,#32532,#32533,#32534,#32535,#32536,#32537,#32538,
#32539,#32540,#32541,#32542,#32543,#32544,#32545,#32546,#32547,#32548,#32549,
#32550,#32551,#32552,#32553,#32554,#32555,#32556,#32557,#32558,#32559,#32560,
#32561,#32562,#32563,#32564,#32565,#32566,#32567,#32568,#32569,#32570,#32571,
#32572,#32573,#32574,#32575,#32576,#32577,#32578,#32579,#32580,#32581,#32582,
#32583,#32584,#32585,#32586,#32587,#32588,#32589,#32590,#32591,#32592,#32593,
#32594,#32595,#32596,#32597,#32598,#32599,#32600,#32601,#32602,#32603,#32604,
#32605,#32606,#32607,#32608,#32609,#32610,#32611,#32612,#32613,#32614,#32615,
#32616,#32617,#32618,#32619,#32620,#32621,#32622,#32623,#32624,#32625,#32626,
#32627,#32628,#32629,#32630,#32631,#32632,#32633,#32634,#32635,#32636,#32637,
#32638,#32639,#32640,#32641,#32642,#32643,#32644,#32645,#32646,#32647,#32648,
#32649,#32650,#32651,#32652,#32653,#32654,#32655,#32656,#32657,#32658,#32659,
#32660,#32661,#32662,#32663,#32664,#32665,#32666,#32667,#32668,#32669,#32670,
#32671,#32672,#32673,#32674,#32675,#32676,#32677,#32678,#32679,#32680,#32681,
#32682),.UNSPECIFIED.,.F.,.F.,(4,3,3,3,3,3,3,3,3,3,3,3,3,3,3,3,3,3,3,3,
3,3,3,3,3,3,3,3,3,3,3,3,3,3,3,3,3,3,3,3,3,3,3,3,3,3,3,3,3,3,3,3,3,3,3,3,
3,3,3,3,3,3,3,3,3,3,3,3,3,3,3,3,3,3,3,4),(417.831822927443,417.889158768891,
417.972905501593,418.056549178609,418.140109922675,418.223607784632,418.307070285195,
418.390515420687,418.47396125553,418.557425850768,418.64097903619,418.724576869763,
418.808308432624,418.88814227109,418.971889003792,419.055532680808,419.139093424874,
419.222591286831,419.306053787393,419.389498922885,419.472944757728,419.556409352966,
419.639962538388,419.723560371961,419.807291934823,419.887125773289,419.970872505991,
420.054516183007,420.138076927073,420.22157478903,420.305037289593,420.388482425085,
420.471928259928,420.555392855166,420.638946040588,420.72254387416,420.806275437022,
420.886109275488,420.96985600819,421.053499685206,421.137060429273,421.220558291229,
421.304020791792,421.387465927284,421.470911762127,421.554376357365,421.637929542787,
421.72152737636,421.805258939222,421.885092777688,421.96883951039,422.052483187406,
422.136043931472,422.219541793429,422.303004293992,422.386449429484,422.469895264327,
422.553359859565,422.636913044987,422.72051087856,422.804242441422,422.884076279887,
422.967823012589,423.051466689605,423.135027433671,423.218525295628,423.30198779619,
423.385432931682,423.468878766525,423.552343361763,423.635896547185,423.719494380758,
423.803225943619,423.883059782086,423.999034008354,424.115008234623),
 .UNSPECIFIED.);
#350=B_SPLINE_CURVE_WITH_KNOTS('',3,(#32684,#32685,#32686,#32687,#32688,
#32689,#32690,#32691,#32692,#32693),.UNSPECIFIED.,.F.,.F.,(4,1,1,1,1,1,
1,4),(411.548645183548,411.895257755696,412.894241257895,413.893224760094,
414.892208262293,415.891191764493,416.890175266692,417.831815876483),
 .UNSPECIFIED.);
#351=B_SPLINE_CURVE_WITH_KNOTS('',3,(#32695,#32696,#32697,#32698,#32699,
#32700,#32701,#32702,#32703,#32704,#32705,#32706,#32707,#32708,#32709,#32710,
#32711,#32712,#32713,#32714,#32715,#32716,#32717,#32718,#32719,#32720,#32721,
#32722,#32723,#32724,#32725,#32726,#32727,#32728,#32729,#32730,#32731,#32732,
#32733,#32734,#32735,#32736,#32737,#32738,#32739,#32740,#32741,#32742,#32743,
#32744,#32745,#32746,#32747,#32748,#32749,#32750,#32751,#32752,#32753,#32754,
#32755,#32756,#32757,#32758,#32759,#32760,#32761,#32762,#32763,#32764,#32765,
#32766,#32767,#32768,#32769,#32770,#32771,#32772,#32773,#32774,#32775,#32776,
#32777,#32778,#32779,#32780,#32781,#32782,#32783,#32784,#32785,#32786,#32787,
#32788,#32789,#32790,#32791,#32792,#32793,#32794,#32795,#32796,#32797,#32798,
#32799,#32800,#32801,#32802,#32803,#32804,#32805,#32806,#32807,#32808,#32809,
#32810,#32811,#32812,#32813,#32814,#32815,#32816,#32817,#32818,#32819,#32820,
#32821,#32822,#32823,#32824,#32825,#32826,#32827,#32828,#32829,#32830,#32831,
#32832,#32833,#32834,#32835,#32836,#32837,#32838,#32839,#32840,#32841,#32842,
#32843,#32844,#32845,#32846,#32847,#32848,#32849,#32850,#32851,#32852,#32853,
#32854,#32855,#32856,#32857,#32858,#32859,#32860,#32861,#32862,#32863,#32864,
#32865,#32866,#32867,#32868,#32869,#32870,#32871,#32872,#32873,#32874,#32875,
#32876,#32877,#32878,#32879,#32880,#32881,#32882,#32883,#32884,#32885,#32886,
#32887,#32888,#32889,#32890,#32891,#32892,#32893,#32894,#32895,#32896,#32897,
#32898,#32899,#32900,#32901,#32902,#32903,#32904,#32905,#32906,#32907,#32908,
#32909,#32910,#32911,#32912,#32913,#32914,#32915,#32916,#32917,#32918,#32919,
#32920,#32921,#32922,#32923),.UNSPECIFIED.,.F.,.F.,(4,3,3,3,3,3,3,3,3,3,
3,3,3,3,3,3,3,3,3,3,3,3,3,3,3,3,3,3,3,3,3,3,3,3,3,3,3,3,3,3,3,3,3,3,3,3,
3,3,3,3,3,3,3,3,3,3,3,3,3,3,3,3,3,3,3,3,3,3,3,3,3,3,3,3,3,3,4),(405.265452313084,
405.34931675342,405.433182297519,405.517066410324,405.600986564986,405.685012608218,
405.769097414882,405.853317495139,405.901356742501,405.985103475203,406.068747152219,
406.152307896285,406.235805758242,406.319268258804,406.402713394296,406.486159229139,
406.569623824377,406.653177009799,406.736774843372,406.820506406234,406.9003402447,
406.984086977402,407.067730654418,407.151291398484,407.234789260441,407.318251761003,
407.401696896496,407.485142731338,407.568607326576,407.652160511998,407.735758345571,
407.819489908433,407.899323746899,407.983070479601,408.066714156617,408.150274900683,
408.23377276264,408.317235263202,408.400680398694,408.484126233537,408.567590828775,
408.651144014197,408.73474184777,408.818473410631,408.898307249098,408.9820539818,
409.065697658816,409.149258402883,409.23275626484,409.316218765402,409.399663900895,
409.483109735738,409.566574330976,409.650127516398,409.73372534997,409.817456912832,
409.897290751298,409.981037484,410.064681161016,410.148241905082,410.231739767039,
410.315202267601,410.398647403093,410.482093237936,410.565557833174,410.649111018596,
410.732708852169,410.816440415031,410.896274253497,410.980187398237,411.063998149748,
411.147724505201,411.23138439992,411.314997651452,411.398582238589,411.482174468518,
411.548637620264),.UNSPECIFIED.);
#352=B_SPLINE_CURVE_WITH_KNOTS('',3,(#32925,#32926,#32927,#32928,#32929,
#32930,#32931,#32932,#32933,#32934,#32935,#32936,#32937,#32938,#32939,#32940,
#32941,#32942,#32943,#32944,#32945,#32946,#32947,#32948,#32949,#32950,#32951,
#32952,#32953,#32954,#32955,#32956,#32957,#32958,#32959,#32960,#32961,#32962,
#32963,#32964,#32965,#32966,#32967,#32968,#32969,#32970,#32971,#32972,#32973,
#32974,#32975,#32976,#32977,#32978,#32979,#32980,#32981,#32982,#32983,#32984,
#32985,#32986,#32987,#32988,#32989,#32990,#32991,#32992,#32993,#32994,#32995,
#32996,#32997,#32998,#32999,#33000,#33001,#33002,#33003,#33004,#33005,#33006,
#33007,#33008,#33009,#33010,#33011,#33012,#33013,#33014,#33015,#33016,#33017,
#33018,#33019,#33020,#33021,#33022,#33023,#33024,#33025,#33026,#33027,#33028,
#33029,#33030,#33031,#33032,#33033,#33034,#33035,#33036,#33037,#33038,#33039,
#33040,#33041,#33042,#33043,#33044,#33045,#33046,#33047,#33048,#33049,#33050,
#33051,#33052,#33053,#33054,#33055,#33056,#33057,#33058,#33059,#33060,#33061,
#33062,#33063,#33064,#33065,#33066,#33067,#33068,#33069,#33070,#33071,#33072,
#33073,#33074,#33075,#33076,#33077,#33078,#33079,#33080,#33081,#33082,#33083,
#33084,#33085,#33086,#33087,#33088,#33089,#33090,#33091,#33092,#33093,#33094,
#33095,#33096,#33097,#33098,#33099,#33100,#33101,#33102,#33103,#33104,#33105,
#33106,#33107,#33108,#33109,#33110,#33111,#33112,#33113,#33114,#33115,#33116,
#33117,#33118,#33119,#33120,#33121,#33122,#33123,#33124,#33125,#33126,#33127,
#33128,#33129,#33130,#33131,#33132,#33133,#33134,#33135,#33136,#33137,#33138,
#33139,#33140,#33141,#33142,#33143,#33144,#33145,#33146,#33147,#33148,#33149,
#33150,#33151,#33152,#33153),.UNSPECIFIED.,.F.,.F.,(4,3,3,3,3,3,3,3,3,3,
3,3,3,3,3,3,3,3,3,3,3,3,3,3,3,3,3,3,3,3,3,3,3,3,3,3,3,3,3,3,3,3,3,3,3,3,
3,3,3,3,3,3,3,3,3,3,3,3,3,3,3,3,3,3,3,3,3,3,3,3,3,3,3,3,3,3,4),(398.98226700603,
399.065122617391,399.147881411393,399.230564299258,399.315175728014,399.397778478442,
399.480372809342,399.562977498193,399.649097055971,399.731823868288,399.81460673228,
399.897502480361,399.907455729306,399.991202462008,400.074846139024,400.15840688309,
400.241904745047,400.32536724561,400.408812381102,400.492258215945,400.575722811182,
400.659275996604,400.742873830177,400.826605393039,400.906439231505,400.990185964207,
401.073829641223,401.157390385289,401.240888247246,401.324350747808,401.407795883301,
401.491241718143,401.574706313381,401.658259498803,401.741857332376,401.825588895238,
401.905422733704,401.989169466406,402.072813143422,402.156373887489,402.239871749446,
402.323334250008,402.406779385501,402.490225220344,402.573689815582,402.657243001004,
402.740840834576,402.824572397438,402.904406235903,402.988152968605,403.071796645621,
403.155357389687,403.238855251644,403.322317752207,403.405762887699,403.489208722542,
403.57267331778,403.656226503202,403.739824336775,403.823555899637,403.903389738103,
403.987136470805,404.070780147821,404.154340891888,404.237838753845,404.321301254408,
404.4047463899,404.488192224743,404.571656819981,404.655210005403,404.738807838976,
404.822539401838,404.902373240302,404.998091733373,405.093477072523,405.188223685256,
405.265452312886),.UNSPECIFIED.);
#353=B_SPLINE_CURVE_WITH_KNOTS('',3,(#33155,#33156,#33157,#33158,#33159,
#33160,#33161,#33162,#33163,#33164,#33165,#33166,#33167,#33168,#33169,#33170,
#33171,#33172,#33173,#33174,#33175,#33176,#33177,#33178,#33179,#33180,#33181,
#33182,#33183,#33184,#33185,#33186,#33187,#33188,#33189,#33190,#33191,#33192,
#33193,#33194,#33195,#33196,#33197,#33198,#33199,#33200,#33201,#33202,#33203,
#33204,#33205,#33206,#33207,#33208,#33209,#33210,#33211,#33212,#33213,#33214,
#33215,#33216,#33217,#33218,#33219,#33220,#33221,#33222,#33223,#33224,#33225,
#33226,#33227,#33228,#33229,#33230,#33231,#33232,#33233,#33234,#33235,#33236,
#33237,#33238,#33239,#33240,#33241,#33242,#33243,#33244,#33245,#33246,#33247,
#33248,#33249,#33250,#33251,#33252,#33253,#33254,#33255,#33256,#33257,#33258,
#33259,#33260,#33261,#33262,#33263,#33264,#33265,#33266,#33267,#33268,#33269,
#33270,#33271,#33272,#33273,#33274,#33275,#33276,#33277,#33278,#33279,#33280,
#33281,#33282,#33283,#33284,#33285,#33286,#33287,#33288,#33289,#33290,#33291,
#33292,#33293,#33294,#33295,#33296,#33297,#33298,#33299,#33300,#33301,#33302,
#33303,#33304,#33305,#33306,#33307,#33308,#33309,#33310,#33311,#33312,#33313,
#33314,#33315,#33316,#33317,#33318,#33319,#33320,#33321,#33322,#33323,#33324,
#33325,#33326,#33327,#33328,#33329,#33330,#33331,#33332,#33333,#33334,#33335,
#33336,#33337,#33338,#33339,#33340,#33341,#33342,#33343,#33344,#33345,#33346,
#33347,#33348,#33349,#33350,#33351,#33352,#33353,#33354,#33355,#33356,#33357,
#33358,#33359,#33360,#33361,#33362,#33363,#33364,#33365,#33366,#33367,#33368,
#33369,#33370,#33371,#33372,#33373,#33374,#33375,#33376,#33377,#33378,#33379,
#33380),.UNSPECIFIED.,.F.,.F.,(4,3,3,3,3,3,3,3,3,3,3,3,3,3,3,3,3,3,3,3,
3,3,3,3,3,3,3,3,3,3,3,3,3,3,3,3,3,3,3,3,3,3,3,3,3,3,3,3,3,3,3,3,3,3,3,3,
3,3,3,3,3,3,3,3,3,3,3,3,3,3,3,3,3,3,3,4),(392.699081698725,392.814856252697,
392.914571213912,392.998317946614,393.08196162363,393.165522367697,393.249020229654,
393.332482730216,393.415927865709,393.499373700552,393.58283829579,393.666391481212,
393.749989314785,393.833720877646,393.913554716111,393.997301448813,394.080945125829,
394.164505869895,394.248003731852,394.331466232415,394.414911367907,394.49835720275,
394.581821797988,394.66537498341,394.748972816982,394.832704379844,394.91253821831,
394.996284951012,395.079928628028,395.163489372094,395.246987234051,395.330449734613,
395.413894870105,395.497340704948,395.580805300186,395.664358485608,395.74795631918,
395.831687882042,395.911521720509,395.995268453211,396.078912130227,396.162472874293,
396.24597073625,396.329433236813,396.412878372305,396.496324207148,396.579788802386,
396.663341987808,396.746939821381,396.830671384243,396.910505222708,396.99425195541,
397.077895632426,397.161456376492,397.244954238449,397.328416739012,397.411861874504,
397.495307709347,397.578772304585,397.662325490007,397.74592332358,397.829654886441,
397.909488724908,397.99323545761,398.076879134626,398.160439878693,398.243937740649,
398.327400241212,398.410845376704,398.494291211547,398.577755806786,398.661308992208,
398.74490682578,398.828638388642,398.908472227107,398.982267005905),
 .UNSPECIFIED.);
#354=B_SPLINE_CURVE_WITH_KNOTS('',3,(#33382,#33383,#33384,#33385,#33386,
#33387,#33388,#33389,#33390,#33391,#33392,#33393,#33394,#33395,#33396,#33397,
#33398,#33399,#33400,#33401,#33402,#33403,#33404,#33405,#33406,#33407,#33408,
#33409,#33410,#33411,#33412,#33413,#33414,#33415,#33416,#33417,#33418,#33419,
#33420,#33421,#33422,#33423,#33424,#33425,#33426,#33427,#33428,#33429,#33430,
#33431,#33432,#33433,#33434,#33435,#33436,#33437,#33438,#33439,#33440,#33441,
#33442,#33443,#33444,#33445,#33446,#33447,#33448,#33449,#33450,#33451,#33452,
#33453,#33454,#33455,#33456,#33457,#33458,#33459,#33460,#33461,#33462,#33463,
#33464,#33465,#33466,#33467,#33468,#33469,#33470,#33471,#33472,#33473,#33474,
#33475,#33476,#33477,#33478,#33479,#33480,#33481,#33482,#33483,#33484,#33485,
#33486,#33487,#33488,#33489,#33490,#33491,#33492,#33493,#33494,#33495,#33496,
#33497,#33498,#33499,#33500,#33501,#33502,#33503,#33504,#33505,#33506,#33507,
#33508,#33509,#33510,#33511,#33512,#33513,#33514,#33515,#33516,#33517,#33518,
#33519,#33520,#33521,#33522,#33523,#33524,#33525,#33526,#33527,#33528,#33529,
#33530,#33531,#33532,#33533,#33534,#33535,#33536,#33537,#33538,#33539,#33540,
#33541,#33542,#33543,#33544,#33545,#33546,#33547,#33548,#33549,#33550,#33551,
#33552,#33553,#33554,#33555,#33556,#33557,#33558,#33559,#33560,#33561,#33562,
#33563,#33564,#33565,#33566,#33567,#33568,#33569,#33570,#33571,#33572,#33573,
#33574,#33575,#33576,#33577,#33578,#33579,#33580,#33581,#33582,#33583,#33584,
#33585,#33586,#33587,#33588,#33589,#33590,#33591,#33592,#33593,#33594,#33595,
#33596,#33597,#33598,#33599,#33600,#33601,#33602,#33603,#33604,#33605,#33606,
#33607,#33608,#33609,#33610),.UNSPECIFIED.,.F.,.F.,(4,3,3,3,3,3,3,3,3,3,
3,3,3,3,3,3,3,3,3,3,3,3,3,3,3,3,3,3,3,3,3,3,3,3,3,3,3,3,3,3,3,3,3,3,3,3,
3,3,3,3,3,3,3,3,3,3,3,3,3,3,3,3,3,3,3,3,3,3,3,3,3,3,3,3,3,3,4),(386.415896391546,
386.50311517261,386.59044188571,386.677968044926,386.765598608585,386.853428582552,
386.920670200717,387.004416933419,387.088060610435,387.171621354501,387.255119216458,
387.338581717021,387.422026852513,387.505472687356,387.588937282594,387.672490468016,
387.756088301589,387.839819864451,387.919653702916,388.003400435618,388.087044112634,
388.1706048567,388.254102718657,388.33756521922,388.421010354712,388.504456189555,
388.587920784793,388.671473970215,388.755071803787,388.838803366649,388.918637205115,
389.002383937817,389.086027614833,389.169588358899,389.253086220856,389.336548721418,
389.419993856911,389.503439691753,389.586904286991,389.670457472413,389.754055305986,
389.837786868848,389.917620707314,390.001367440016,390.085011117032,390.168571861098,
390.252069723055,390.335532223617,390.41897735911,390.502423193952,390.585887789191,
390.669440974613,390.753038808186,390.836770371047,390.916604209513,391.000350942215,
391.083994619231,391.167555363297,391.251053225254,391.334515725817,391.417960861309,
391.501406696152,391.58487129139,391.668424476812,391.752022310385,391.835753873247,
391.915587711713,391.998183342791,392.080675349664,392.163072226687,392.24541584479,
392.327725220785,392.410019339919,392.492345036332,392.574687966156,392.65710402368,
392.699081698622),.UNSPECIFIED.);
#355=B_SPLINE_CURVE_WITH_KNOTS('',3,(#33612,#33613,#33614,#33615,#33616,
#33617,#33618,#33619,#33620,#33621,#33622,#33623,#33624,#33625,#33626,#33627,
#33628,#33629,#33630,#33631,#33632,#33633,#33634,#33635,#33636,#33637,#33638,
#33639,#33640,#33641,#33642,#33643,#33644,#33645,#33646,#33647,#33648,#33649,
#33650,#33651,#33652,#33653,#33654,#33655,#33656,#33657,#33658,#33659,#33660,
#33661,#33662,#33663,#33664,#33665,#33666,#33667,#33668,#33669,#33670,#33671,
#33672,#33673,#33674,#33675,#33676,#33677,#33678,#33679,#33680,#33681,#33682,
#33683,#33684,#33685,#33686,#33687,#33688,#33689,#33690,#33691,#33692,#33693,
#33694,#33695,#33696,#33697,#33698,#33699,#33700,#33701,#33702,#33703,#33704,
#33705,#33706,#33707,#33708,#33709,#33710,#33711,#33712,#33713,#33714,#33715,
#33716,#33717,#33718,#33719,#33720,#33721,#33722,#33723,#33724,#33725,#33726,
#33727,#33728,#33729,#33730,#33731,#33732,#33733,#33734,#33735,#33736,#33737,
#33738,#33739,#33740,#33741,#33742,#33743,#33744,#33745,#33746,#33747,#33748,
#33749,#33750,#33751,#33752,#33753,#33754,#33755,#33756,#33757,#33758,#33759,
#33760,#33761,#33762,#33763,#33764,#33765,#33766,#33767,#33768,#33769,#33770,
#33771,#33772,#33773,#33774,#33775,#33776,#33777,#33778,#33779,#33780,#33781,
#33782,#33783,#33784,#33785,#33786,#33787,#33788,#33789,#33790,#33791,#33792,
#33793,#33794,#33795,#33796,#33797,#33798,#33799,#33800,#33801,#33802,#33803,
#33804,#33805,#33806,#33807,#33808,#33809,#33810,#33811,#33812,#33813,#33814,
#33815,#33816,#33817,#33818,#33819,#33820,#33821,#33822,#33823,#33824,#33825,
#33826,#33827,#33828,#33829,#33830,#33831,#33832,#33833,#33834,#33835,#33836,
#33837,#33838,#33839,#33840),.UNSPECIFIED.,.F.,.F.,(4,3,3,3,3,3,3,3,3,3,
3,3,3,3,3,3,3,3,3,3,3,3,3,3,3,3,3,3,3,3,3,3,3,3,3,3,3,3,3,3,3,3,3,3,3,3,
3,3,3,3,3,3,3,3,3,3,3,3,3,3,3,3,3,3,3,3,3,3,3,3,3,3,3,3,3,3,4),(380.132711084533,
380.21510704019,380.297435606509,380.379723757588,380.461992342737,380.544260359157,
380.626546801328,380.708918082886,380.79133548327,380.873875988774,380.926769187522,
381.010515920224,381.09415959724,381.177720341306,381.261218203263,381.344680703826,
381.428125839318,381.511571674161,381.595036269399,381.678589454821,381.762187288394,
381.845918851256,381.925752689721,382.009499422423,382.093143099439,382.176703843505,
382.260201705462,382.343664206024,382.427109341516,382.510555176359,382.594019771597,
382.677572957019,382.761170790592,382.844902353453,382.92473619192,383.008482924622,
383.092126601638,383.175687345704,383.259185207661,383.342647708224,383.426092843716,
383.509538678559,383.593003273797,383.676556459219,383.760154292791,383.843885855653,
383.923719694119,384.007466426821,384.091110103837,384.174670847903,384.25816870986,
384.341631210422,384.425076345915,384.508522180758,384.591986775996,384.675539961417,
384.75913779499,384.842869357852,384.922703196318,385.00644992902,385.090093606036,
385.173654350103,385.25715221206,385.340614712623,385.424059848115,385.507505682958,
385.590970278196,385.674523463618,385.75812129719,385.841852860052,385.921686698518,
386.009955113066,386.098068483732,386.18597518154,386.273758263555,386.361377828746,
386.415896391433),.UNSPECIFIED.);
#356=B_SPLINE_CURVE_WITH_KNOTS('',3,(#33842,#33843,#33844,#33845,#33846,
#33847,#33848,#33849,#33850,#33851,#33852,#33853,#33854,#33855,#33856,#33857,
#33858,#33859,#33860,#33861,#33862,#33863,#33864,#33865,#33866,#33867,#33868,
#33869,#33870,#33871,#33872,#33873,#33874,#33875,#33876,#33877,#33878,#33879,
#33880,#33881,#33882,#33883,#33884,#33885,#33886,#33887,#33888,#33889,#33890,
#33891,#33892,#33893,#33894,#33895,#33896,#33897,#33898,#33899,#33900,#33901,
#33902,#33903,#33904,#33905,#33906,#33907,#33908,#33909,#33910,#33911,#33912,
#33913,#33914,#33915,#33916,#33917,#33918,#33919,#33920,#33921,#33922,#33923,
#33924,#33925,#33926,#33927,#33928,#33929,#33930,#33931,#33932,#33933,#33934,
#33935,#33936,#33937,#33938,#33939,#33940,#33941,#33942,#33943,#33944,#33945,
#33946,#33947,#33948,#33949,#33950,#33951,#33952,#33953,#33954,#33955,#33956,
#33957,#33958,#33959,#33960,#33961,#33962,#33963,#33964,#33965,#33966,#33967,
#33968,#33969,#33970,#33971,#33972,#33973,#33974,#33975,#33976,#33977,#33978,
#33979,#33980,#33981,#33982,#33983,#33984,#33985,#33986,#33987,#33988,#33989,
#33990,#33991,#33992,#33993,#33994,#33995,#33996,#33997,#33998,#33999,#34000,
#34001,#34002,#34003,#34004,#34005,#34006,#34007,#34008,#34009,#34010,#34011,
#34012,#34013,#34014,#34015,#34016,#34017,#34018,#34019,#34020,#34021,#34022,
#34023,#34024,#34025,#34026,#34027,#34028,#34029,#34030,#34031,#34032,#34033,
#34034,#34035,#34036,#34037,#34038,#34039,#34040,#34041,#34042,#34043,#34044,
#34045,#34046,#34047,#34048,#34049,#34050,#34051,#34052,#34053,#34054,#34055,
#34056,#34057,#34058,#34059,#34060,#34061,#34062,#34063,#34064,#34065,#34066,
#34067),.UNSPECIFIED.,.F.,.F.,(4,3,3,3,3,3,3,3,3,3,3,3,3,3,3,3,3,3,3,3,
3,3,3,3,3,3,3,3,3,3,3,3,3,3,3,3,3,3,3,3,3,3,3,3,3,3,3,3,3,3,3,3,3,3,3,3,
3,3,3,3,3,3,3,3,3,3,3,3,3,3,3,3,3,3,3,4),(373.849525777186,373.933884672128,
374.01763140483,374.101275081846,374.184835825912,374.268333687869,374.351796188432,
374.435241323924,374.518687158767,374.602151754005,374.685704939427,374.769302772999,
374.853034335861,374.932868174327,375.016614907029,375.100258584045,375.183819328111,
375.267317190068,375.35077969063,375.434224826122,375.517670660965,375.601135256203,
375.684688441625,375.768286275198,375.852017838059,375.931851676526,376.015598409228,
376.099242086244,376.18280283031,376.266300692267,376.34976319283,376.433208328322,
376.516654163165,376.600118758403,376.683671943824,376.767269777397,376.851001340259,
376.930835178725,377.014581911427,377.098225588443,377.181786332509,377.265284194466,
377.348746695028,377.432191830521,377.515637665364,377.599102260602,377.682655446023,
377.766253279596,377.849984842458,377.929818680924,378.013565413626,378.097209090642,
378.180769834708,378.264267696665,378.347730197228,378.43117533272,378.514621167563,
378.598085762801,378.681638948223,378.765236781796,378.848968344657,378.928802183123,
379.012548915825,379.096192592841,379.179753336907,379.263251198864,379.346713699427,
379.430158834919,379.513604669762,379.597069265,379.680622450422,379.764220283994,
379.847951846856,379.927785685323,380.046394219483,380.132711084366),
 .UNSPECIFIED.);
#357=B_SPLINE_CURVE_WITH_KNOTS('',3,(#34069,#34070,#34071,#34072,#34073,
#34074,#34075,#34076,#34077,#34078,#34079,#34080,#34081,#34082,#34083,#34084,
#34085,#34086,#34087,#34088,#34089,#34090,#34091,#34092,#34093,#34094,#34095,
#34096,#34097,#34098,#34099,#34100,#34101,#34102,#34103,#34104,#34105,#34106,
#34107,#34108,#34109,#34110,#34111,#34112,#34113,#34114,#34115,#34116,#34117,
#34118,#34119,#34120,#34121,#34122,#34123,#34124,#34125,#34126,#34127,#34128,
#34129,#34130,#34131,#34132,#34133,#34134,#34135,#34136,#34137,#34138,#34139,
#34140,#34141,#34142,#34143,#34144,#34145,#34146,#34147,#34148,#34149,#34150,
#34151,#34152,#34153,#34154,#34155,#34156,#34157,#34158,#34159,#34160,#34161,
#34162,#34163,#34164,#34165,#34166,#34167,#34168,#34169,#34170,#34171,#34172,
#34173,#34174,#34175,#34176,#34177,#34178,#34179,#34180,#34181,#34182,#34183,
#34184,#34185,#34186,#34187,#34188,#34189,#34190,#34191,#34192,#34193,#34194,
#34195,#34196,#34197,#34198,#34199,#34200,#34201,#34202,#34203,#34204,#34205,
#34206,#34207,#34208,#34209,#34210,#34211,#34212,#34213,#34214,#34215,#34216,
#34217,#34218,#34219,#34220,#34221,#34222,#34223,#34224,#34225,#34226,#34227,
#34228,#34229,#34230,#34231,#34232,#34233,#34234,#34235,#34236,#34237,#34238,
#34239,#34240,#34241,#34242,#34243,#34244,#34245,#34246,#34247,#34248,#34249,
#34250,#34251,#34252,#34253,#34254,#34255,#34256,#34257,#34258,#34259,#34260,
#34261,#34262,#34263,#34264,#34265,#34266,#34267,#34268,#34269,#34270,#34271,
#34272,#34273,#34274,#34275,#34276,#34277,#34278,#34279,#34280,#34281,#34282,
#34283,#34284,#34285,#34286,#34287,#34288,#34289,#34290,#34291,#34292,#34293,
#34294),.UNSPECIFIED.,.F.,.F.,(4,3,3,3,3,3,3,3,3,3,3,3,3,3,3,3,3,3,3,3,
3,3,3,3,3,3,3,3,3,3,3,3,3,3,3,3,3,3,3,3,3,3,3,3,3,3,3,3,3,3,3,3,3,3,3,3,
3,3,3,3,3,3,3,3,3,3,3,3,3,3,3,3,3,3,3,4),(367.566340470201,367.660350300293,
367.754723512711,367.849614788934,367.939983658933,368.023730391635,368.107374068651,
368.190934812717,368.274432674674,368.357895175236,368.441340310729,368.524786145571,
368.608250740809,368.691803926231,368.775401759804,368.859133322666,368.938967161132,
369.022713893834,369.10635757085,369.189918314916,369.273416176873,369.356878677436,
369.440323812928,369.523769647771,369.607234243009,369.690787428431,369.774385262003,
369.858116824865,369.937950663331,370.021697396033,370.105341073049,370.188901817115,
370.272399679072,370.355862179635,370.439307315127,370.52275314997,370.606217745208,
370.68977093063,370.773368764202,370.857100327064,370.93693416553,371.020680898232,
371.104324575248,371.187885319314,371.271383181271,371.354845681833,371.438290817326,
371.521736652168,371.605201247407,371.688754432828,371.772352266401,371.856083829263,
371.935917667729,372.019664400431,372.103308077447,372.186868821513,372.27036668347,
372.353829184033,372.437274319525,372.520720154368,372.604184749606,372.687737935028,
372.7713357686,372.855067331462,372.934901169928,373.017703443352,373.100403398518,
373.183022036849,373.266335004375,373.348860249607,373.431371904164,373.513888802314,
373.597798045999,373.680421651097,373.764973714076,373.849525777054),
 .UNSPECIFIED.);
#358=B_SPLINE_CURVE_WITH_KNOTS('',3,(#34296,#34297,#34298,#34299,#34300,
#34301,#34302,#34303,#34304,#34305,#34306,#34307,#34308,#34309,#34310,#34311,
#34312,#34313,#34314,#34315,#34316,#34317,#34318,#34319,#34320,#34321,#34322,
#34323,#34324,#34325,#34326,#34327,#34328,#34329,#34330,#34331,#34332,#34333,
#34334,#34335,#34336,#34337,#34338,#34339,#34340,#34341,#34342,#34343,#34344,
#34345,#34346,#34347,#34348,#34349,#34350,#34351,#34352,#34353,#34354,#34355,
#34356,#34357,#34358,#34359,#34360,#34361,#34362,#34363,#34364,#34365,#34366,
#34367,#34368,#34369,#34370,#34371,#34372,#34373,#34374,#34375,#34376,#34377,
#34378,#34379,#34380,#34381,#34382,#34383,#34384,#34385,#34386,#34387,#34388,
#34389,#34390,#34391,#34392,#34393,#34394,#34395,#34396,#34397,#34398,#34399,
#34400,#34401,#34402,#34403,#34404,#34405,#34406,#34407,#34408,#34409,#34410,
#34411,#34412,#34413,#34414,#34415,#34416,#34417,#34418,#34419,#34420,#34421,
#34422,#34423,#34424,#34425,#34426,#34427,#34428,#34429,#34430,#34431,#34432,
#34433,#34434,#34435,#34436,#34437,#34438,#34439,#34440,#34441,#34442,#34443,
#34444,#34445,#34446,#34447,#34448,#34449,#34450,#34451,#34452,#34453,#34454,
#34455,#34456,#34457,#34458,#34459,#34460,#34461,#34462,#34463,#34464,#34465,
#34466,#34467,#34468,#34469,#34470,#34471,#34472,#34473,#34474,#34475,#34476,
#34477,#34478,#34479,#34480,#34481,#34482,#34483,#34484,#34485,#34486,#34487,
#34488,#34489,#34490,#34491,#34492,#34493,#34494,#34495,#34496,#34497,#34498,
#34499,#34500,#34501,#34502,#34503,#34504,#34505,#34506,#34507,#34508,#34509,
#34510,#34511,#34512,#34513,#34514,#34515,#34516,#34517,#34518,#34519,#34520,
#34521,#34522,#34523,#34524),.UNSPECIFIED.,.F.,.F.,(4,3,3,3,3,3,3,3,3,3,
3,3,3,3,3,3,3,3,3,3,3,3,3,3,3,3,3,3,3,3,3,3,3,3,3,3,3,3,3,3,3,3,3,3,3,3,
3,3,3,3,3,3,3,3,3,3,3,3,3,3,3,3,3,3,3,3,3,3,3,3,3,3,3,3,3,3,4),(361.283155162827,
361.366593317698,361.450019445351,361.53345154986,361.616907635409,361.700459950804,
361.784061320472,361.867802569209,361.946082645738,362.02982937844,362.113473055456,
362.197033799522,362.280531661479,362.363994162042,362.447439297534,362.530885132377,
362.614349727615,362.697902913037,362.78150074661,362.865232309471,362.945066147937,
363.028812880639,363.112456557655,363.196017301721,363.279515163678,363.36297766424,
363.446422799733,363.529868634576,363.613333229814,363.696886415236,363.780484248808,
363.86421581167,363.944049650136,364.027796382838,364.111440059854,364.19500080392,
364.278498665877,364.361961166439,364.445406301931,364.528852136774,364.612316732012,
364.695869917434,364.779467751007,364.863199313869,364.943033152335,365.026779885037,
365.110423562053,365.193984306119,365.277482168076,365.360944668638,365.44438980413,
365.527835638973,365.611300234211,365.694853419633,365.778451253206,365.862182816068,
365.942016654534,366.025763387236,366.109407064252,366.192967808319,366.276465670276,
366.359928170838,366.443373306331,366.526819141173,366.610283736411,366.693836921833,
366.777434755406,366.861166318268,366.941000156733,367.025414114052,367.109721200961,
367.193938818128,367.27808430145,367.362170923251,367.446223229521,367.530265659005,
367.566340470007),.UNSPECIFIED.);
#359=B_SPLINE_CURVE_WITH_KNOTS('',3,(#34526,#34527,#34528,#34529,#34530,
#34531,#34532,#34533,#34534,#34535,#34536,#34537,#34538,#34539,#34540,#34541,
#34542,#34543,#34544,#34545,#34546,#34547,#34548,#34549,#34550,#34551,#34552,
#34553,#34554,#34555,#34556,#34557,#34558,#34559,#34560,#34561,#34562,#34563,
#34564,#34565,#34566,#34567,#34568,#34569,#34570,#34571,#34572,#34573,#34574,
#34575,#34576,#34577,#34578,#34579,#34580,#34581,#34582,#34583,#34584,#34585,
#34586,#34587,#34588,#34589,#34590,#34591,#34592,#34593,#34594,#34595,#34596,
#34597,#34598,#34599,#34600,#34601,#34602,#34603,#34604,#34605,#34606,#34607,
#34608,#34609,#34610,#34611,#34612,#34613,#34614,#34615,#34616,#34617,#34618,
#34619,#34620,#34621,#34622,#34623,#34624,#34625,#34626,#34627,#34628,#34629,
#34630,#34631,#34632,#34633,#34634,#34635,#34636,#34637,#34638,#34639,#34640,
#34641,#34642,#34643,#34644,#34645,#34646,#34647,#34648,#34649,#34650,#34651,
#34652,#34653,#34654,#34655,#34656,#34657,#34658,#34659,#34660,#34661,#34662,
#34663,#34664,#34665,#34666,#34667,#34668,#34669,#34670,#34671,#34672,#34673,
#34674,#34675,#34676,#34677,#34678,#34679,#34680,#34681,#34682,#34683,#34684,
#34685,#34686,#34687,#34688,#34689,#34690,#34691,#34692,#34693,#34694,#34695,
#34696,#34697,#34698,#34699,#34700,#34701,#34702,#34703,#34704,#34705,#34706,
#34707,#34708,#34709,#34710,#34711,#34712,#34713,#34714,#34715,#34716,#34717,
#34718,#34719,#34720,#34721,#34722,#34723,#34724,#34725,#34726,#34727,#34728,
#34729,#34730,#34731,#34732,#34733,#34734,#34735,#34736,#34737,#34738,#34739,
#34740,#34741,#34742,#34743,#34744,#34745,#34746,#34747,#34748,#34749,#34750,
#34751,#34752,#34753,#34754),.UNSPECIFIED.,.F.,.F.,(4,3,3,3,3,3,3,3,3,3,
3,3,3,3,3,3,3,3,3,3,3,3,3,3,3,3,3,3,3,3,3,3,3,3,3,3,3,3,3,3,3,3,3,3,3,3,
3,3,3,3,3,3,3,3,3,3,3,3,3,3,3,3,3,3,3,3,3,3,3,3,3,3,3,3,3,3,4),(354.999969855836,
355.083098070547,355.166126031582,355.249074448297,355.331963953429,355.414823775889,
355.497670893546,355.580523896995,355.663401377681,355.746368482,355.82938637503,
355.912525509817,355.952181632543,356.035928365245,356.119572042261,356.203132786327,
356.286630648284,356.370093148846,356.453538284339,356.536984119182,356.62044871442,
356.704001899842,356.787599733414,356.871331296276,356.951165134742,357.034911867444,
357.11855554446,357.202116288526,357.285614150483,357.369076651045,357.452521786538,
357.53596762138,357.619432216619,357.70298540204,357.786583235613,357.870314798475,
357.950148636941,358.033895369643,358.117539046659,358.201099790725,358.284597652682,
358.368060153244,358.451505288737,358.53495112358,358.618415718817,358.701968904239,
358.785566737812,358.869298300674,358.94913213914,359.032878871842,359.116522548858,
359.200083292924,359.283581154881,359.367043655443,359.450488790935,359.533934625778,
359.617399221016,359.700952406438,359.78455024001,359.868281802872,359.948115641339,
360.031862374041,360.115506051057,360.199066795123,360.282564657079,360.366027157642,
360.449472293134,360.532918127977,360.616382723216,360.699935908638,360.78353374221,
360.867265305072,360.947099143538,361.045204785511,361.142870607703,361.239719950613,
361.283155162638),.UNSPECIFIED.);
#360=B_SPLINE_CURVE_WITH_KNOTS('',3,(#34756,#34757,#34758,#34759,#34760,
#34761,#34762,#34763,#34764,#34765,#34766,#34767,#34768,#34769,#34770,#34771,
#34772,#34773,#34774,#34775,#34776,#34777,#34778,#34779,#34780,#34781,#34782,
#34783,#34784,#34785,#34786,#34787,#34788,#34789,#34790,#34791,#34792,#34793,
#34794,#34795,#34796,#34797,#34798,#34799,#34800,#34801,#34802,#34803,#34804,
#34805,#34806,#34807,#34808,#34809,#34810,#34811,#34812,#34813,#34814,#34815,
#34816,#34817,#34818,#34819,#34820,#34821,#34822,#34823,#34824,#34825,#34826,
#34827,#34828,#34829,#34830,#34831,#34832,#34833,#34834,#34835,#34836,#34837,
#34838,#34839,#34840,#34841,#34842,#34843,#34844,#34845,#34846,#34847,#34848,
#34849,#34850,#34851,#34852,#34853,#34854,#34855,#34856,#34857,#34858,#34859,
#34860,#34861,#34862,#34863,#34864,#34865,#34866,#34867,#34868,#34869,#34870,
#34871,#34872,#34873,#34874,#34875,#34876,#34877,#34878,#34879,#34880,#34881,
#34882,#34883,#34884,#34885,#34886,#34887,#34888,#34889,#34890,#34891,#34892,
#34893,#34894,#34895,#34896,#34897,#34898,#34899,#34900,#34901,#34902,#34903,
#34904,#34905,#34906,#34907,#34908,#34909,#34910,#34911,#34912,#34913,#34914,
#34915,#34916,#34917,#34918,#34919,#34920,#34921,#34922,#34923,#34924,#34925,
#34926,#34927,#34928,#34929,#34930,#34931,#34932,#34933,#34934,#34935,#34936,
#34937,#34938,#34939,#34940,#34941,#34942,#34943,#34944,#34945,#34946,#34947,
#34948,#34949,#34950,#34951,#34952,#34953,#34954,#34955,#34956,#34957,#34958,
#34959,#34960,#34961,#34962,#34963,#34964,#34965,#34966,#34967,#34968,#34969,
#34970,#34971,#34972,#34973,#34974,#34975,#34976,#34977,#34978,#34979,#34980,
#34981,#34982,#34983,#34984),.UNSPECIFIED.,.F.,.F.,(4,3,3,3,3,3,3,3,3,3,
3,3,3,3,3,3,3,3,3,3,3,3,3,3,3,3,3,3,3,3,3,3,3,3,3,3,3,3,3,3,3,3,3,3,3,3,
3,3,3,3,3,3,3,3,3,3,3,3,3,3,3,3,3,3,3,3,3,3,3,3,3,3,3,3,3,3,4),(348.71678454857,
348.825202608615,348.936282965072,348.959297117148,349.04304384985,349.126687526866,
349.210248270933,349.293746132889,349.377208633452,349.460653768944,349.544099603787,
349.627564199025,349.711117384447,349.79471521802,349.878446780882,349.958280619348,
350.04202735205,350.125671029066,350.209231773133,350.292729635089,350.376192135652,
350.459637271144,350.543083105987,350.626547701225,350.710100886647,350.79369872022,
350.877430283082,350.957264121547,351.041010854249,351.124654531265,351.208215275331,
351.291713137288,351.37517563785,351.458620773342,351.542066608185,351.625531203423,
351.709084388845,351.792682222418,351.876413785279,351.956247623746,352.039994356448,
352.123638033464,352.20719877753,352.290696639487,352.37415914005,352.457604275542,
352.541050110385,352.624514705623,352.708067891045,352.791665724618,352.87539728748,
352.955231125945,353.038977858647,353.122621535663,353.206182279729,353.289680141686,
353.373142642248,353.456587777741,353.540033612583,353.623498207821,353.707051393243,
353.790649226816,353.874380789678,353.954214628144,354.037961360846,354.121605037862,
354.205165781928,354.288663643885,354.372126144447,354.455571279939,354.539017114782,
354.62248171002,354.706034895442,354.789632729015,354.873364291876,354.953198130343,
354.999969855648),.UNSPECIFIED.);
#361=B_SPLINE_CURVE_WITH_KNOTS('',3,(#34986,#34987,#34988,#34989,#34990,
#34991,#34992,#34993,#34994,#34995,#34996,#34997,#34998,#34999,#35000,#35001,
#35002,#35003,#35004,#35005,#35006,#35007,#35008,#35009,#35010,#35011,#35012,
#35013,#35014,#35015,#35016,#35017,#35018,#35019,#35020,#35021,#35022,#35023,
#35024,#35025,#35026,#35027,#35028,#35029,#35030,#35031,#35032,#35033,#35034,
#35035,#35036,#35037,#35038,#35039,#35040,#35041,#35042,#35043,#35044,#35045,
#35046,#35047,#35048,#35049,#35050,#35051,#35052,#35053,#35054,#35055,#35056,
#35057,#35058,#35059,#35060,#35061,#35062,#35063,#35064,#35065,#35066,#35067,
#35068,#35069,#35070,#35071,#35072,#35073,#35074,#35075,#35076,#35077,#35078,
#35079,#35080,#35081,#35082,#35083,#35084,#35085,#35086,#35087,#35088,#35089,
#35090,#35091,#35092,#35093,#35094,#35095,#35096,#35097,#35098,#35099,#35100,
#35101,#35102,#35103,#35104,#35105,#35106,#35107,#35108,#35109,#35110,#35111,
#35112,#35113,#35114,#35115,#35116,#35117,#35118,#35119,#35120,#35121,#35122,
#35123,#35124,#35125,#35126,#35127,#35128,#35129,#35130,#35131,#35132,#35133,
#35134,#35135,#35136,#35137,#35138,#35139,#35140,#35141,#35142,#35143,#35144,
#35145,#35146,#35147,#35148,#35149,#35150,#35151,#35152,#35153,#35154,#35155,
#35156,#35157,#35158,#35159,#35160,#35161,#35162,#35163,#35164,#35165,#35166,
#35167,#35168,#35169,#35170,#35171,#35172,#35173,#35174,#35175,#35176,#35177,
#35178,#35179,#35180,#35181,#35182,#35183,#35184,#35185,#35186,#35187,#35188,
#35189,#35190,#35191,#35192,#35193,#35194,#35195,#35196,#35197,#35198,#35199,
#35200,#35201,#35202,#35203,#35204,#35205,#35206,#35207,#35208,#35209,#35210,
#35211,#35212,#35213,#35214,#35215,#35216,#35217),.UNSPECIFIED.,.F.,.F.,
(4,3,3,3,3,3,3,3,3,3,3,3,3,3,3,3,3,3,3,3,3,3,3,3,3,3,3,3,3,3,3,3,3,3,3,
3,3,3,3,3,3,3,3,3,3,3,3,3,3,3,3,3,3,3,3,3,3,3,3,3,3,3,3,3,3,3,3,3,3,3,3,
3,3,3,3,3,3,4),(342.433599241289,342.51992594412,342.606329662537,342.696096272891,
342.782755320326,342.86950763198,342.956417766365,342.965396103953,343.049142836655,
343.132786513671,343.216347257738,343.299845119694,343.383307620257,343.466752755749,
343.550198590592,343.63366318583,343.717216371252,343.800814204825,343.884545767687,
343.964379606153,344.048126338855,344.131770015871,344.215330759937,344.298828621894,
344.382291122457,344.465736257949,344.549182092792,344.63264668803,344.716199873452,
344.799797707024,344.883529269886,344.963363108352,345.047109841054,345.13075351807,
345.214314262137,345.297812124093,345.381274624656,345.464719760148,345.548165594991,
345.631630190229,345.715183375651,345.798781209223,345.882512772085,345.962346610551,
346.046093343253,346.129737020269,346.213297764335,346.296795626292,346.380258126854,
346.463703262347,346.547149097189,346.630613692427,346.714166877849,346.797764711422,
346.881496274284,346.96133011275,347.045076845452,347.128720522468,347.212281266534,
347.29577912849,347.379241629053,347.462686764545,347.546132599388,347.629597194627,
347.713150380049,347.796748213621,347.880479776483,347.960313614949,348.043054505276,
348.127270760675,348.209808258655,348.292291441905,348.374739235986,348.460250564106,
348.542706853071,348.625180065633,348.707712121519,348.716784548468),
 .UNSPECIFIED.);
#362=B_SPLINE_CURVE_WITH_KNOTS('',3,(#35219,#35220,#35221,#35222,#35223,
#35224,#35225,#35226,#35227,#35228,#35229,#35230,#35231,#35232,#35233,#35234,
#35235,#35236,#35237,#35238,#35239,#35240,#35241,#35242,#35243,#35244,#35245,
#35246,#35247,#35248,#35249,#35250,#35251,#35252,#35253,#35254,#35255,#35256,
#35257,#35258,#35259,#35260,#35261,#35262,#35263,#35264,#35265,#35266,#35267,
#35268,#35269,#35270,#35271,#35272,#35273,#35274,#35275,#35276,#35277,#35278,
#35279,#35280,#35281,#35282,#35283,#35284,#35285,#35286,#35287,#35288,#35289,
#35290,#35291,#35292,#35293,#35294,#35295,#35296,#35297,#35298,#35299,#35300,
#35301,#35302,#35303,#35304,#35305,#35306,#35307,#35308,#35309,#35310,#35311,
#35312,#35313,#35314,#35315,#35316,#35317,#35318,#35319,#35320,#35321,#35322,
#35323,#35324,#35325,#35326,#35327,#35328,#35329,#35330,#35331,#35332,#35333,
#35334,#35335,#35336,#35337,#35338,#35339,#35340,#35341,#35342,#35343,#35344,
#35345,#35346,#35347,#35348,#35349,#35350,#35351,#35352,#35353,#35354,#35355,
#35356,#35357,#35358,#35359,#35360,#35361,#35362,#35363,#35364,#35365,#35366,
#35367,#35368,#35369,#35370,#35371,#35372,#35373,#35374,#35375,#35376,#35377,
#35378,#35379,#35380,#35381,#35382,#35383,#35384,#35385,#35386,#35387,#35388,
#35389,#35390,#35391,#35392,#35393,#35394,#35395,#35396,#35397,#35398,#35399,
#35400,#35401,#35402,#35403,#35404,#35405,#35406,#35407,#35408,#35409,#35410,
#35411,#35412,#35413,#35414,#35415,#35416,#35417,#35418,#35419,#35420,#35421,
#35422,#35423,#35424,#35425,#35426,#35427,#35428,#35429,#35430,#35431,#35432,
#35433,#35434,#35435,#35436,#35437,#35438,#35439,#35440,#35441,#35442,#35443,
#35444,#35445,#35446,#35447),.UNSPECIFIED.,.F.,.F.,(4,3,3,3,3,3,3,3,3,3,
3,3,3,3,3,3,3,3,3,3,3,3,3,3,3,3,3,3,3,3,3,3,3,3,3,3,3,3,3,3,3,3,3,3,3,3,
3,3,3,3,3,3,3,3,3,3,3,3,3,3,3,3,3,3,3,3,3,3,3,3,3,3,3,3,3,3,4),(336.150413934269,
336.232787324844,336.315085749949,336.397333675145,336.479555269055,336.561769565653,
336.643995590724,336.726302690793,336.8086499515,336.891127738289,336.971495090759,
337.055241823461,337.138885500477,337.222446244543,337.3059441065,337.389406607062,
337.472851742555,337.556297577398,337.639762172636,337.723315358057,337.80691319163,
337.890644754492,337.970478592958,338.05422532566,338.137869002676,338.221429746743,
338.304927608699,338.388390109262,338.471835244754,338.555281079597,338.638745674835,
338.722298860257,338.80589669383,338.889628256692,338.969462095157,339.053208827859,
339.136852504875,339.220413248941,339.303911110898,339.38737361146,339.470818746952,
339.554264581795,339.637729177033,339.721282362455,339.804880196028,339.888611758889,
339.968445597356,340.052192330058,340.135836007074,340.21939675114,340.302894613097,
340.386357113659,340.469802249152,340.553248083995,340.636712679232,340.720265864654,
340.803863698227,340.887595261089,340.967429099555,341.051175832257,341.134819509273,
341.21838025334,341.301878115297,341.385340615859,341.468785751352,341.552231586195,
341.635696181433,341.719249366855,341.802847200427,341.886578763289,341.966412601754,
342.055853088888,342.145118135785,342.234139928017,342.323010439427,342.411678679605,
342.433599241143),.UNSPECIFIED.);
#363=B_SPLINE_CURVE_WITH_KNOTS('',3,(#35449,#35450,#35451,#35452,#35453,
#35454,#35455,#35456,#35457,#35458,#35459,#35460,#35461,#35462,#35463,#35464,
#35465,#35466,#35467,#35468,#35469,#35470,#35471,#35472,#35473,#35474,#35475,
#35476,#35477,#35478,#35479,#35480,#35481,#35482,#35483,#35484,#35485,#35486,
#35487,#35488,#35489,#35490,#35491,#35492,#35493,#35494,#35495,#35496,#35497,
#35498,#35499,#35500,#35501,#35502,#35503,#35504,#35505,#35506,#35507,#35508,
#35509,#35510,#35511,#35512,#35513,#35514,#35515,#35516,#35517,#35518,#35519,
#35520,#35521,#35522,#35523,#35524,#35525,#35526,#35527,#35528,#35529,#35530,
#35531,#35532,#35533,#35534,#35535,#35536,#35537,#35538,#35539,#35540,#35541,
#35542,#35543,#35544,#35545,#35546,#35547,#35548,#35549,#35550,#35551,#35552,
#35553,#35554,#35555,#35556,#35557,#35558,#35559,#35560,#35561,#35562,#35563,
#35564,#35565,#35566,#35567,#35568,#35569,#35570,#35571,#35572,#35573,#35574,
#35575,#35576,#35577,#35578,#35579,#35580,#35581,#35582,#35583,#35584,#35585,
#35586,#35587,#35588,#35589,#35590,#35591,#35592,#35593,#35594,#35595,#35596,
#35597,#35598,#35599,#35600,#35601,#35602,#35603,#35604,#35605,#35606,#35607,
#35608,#35609,#35610,#35611,#35612,#35613,#35614,#35615,#35616,#35617,#35618,
#35619,#35620,#35621,#35622,#35623,#35624,#35625,#35626,#35627,#35628,#35629,
#35630,#35631,#35632,#35633,#35634,#35635,#35636,#35637,#35638,#35639,#35640,
#35641,#35642,#35643,#35644,#35645,#35646,#35647,#35648,#35649,#35650,#35651,
#35652,#35653,#35654,#35655,#35656,#35657,#35658,#35659,#35660,#35661,#35662,
#35663,#35664,#35665,#35666,#35667,#35668,#35669,#35670,#35671,#35672,#35673,
#35674),.UNSPECIFIED.,.F.,.F.,(4,3,3,3,3,3,3,3,3,3,3,3,3,3,3,3,3,3,3,3,
3,3,3,3,3,3,3,3,3,3,3,3,3,3,3,3,3,3,3,3,3,3,3,3,3,3,3,3,3,3,3,3,3,3,3,3,
3,3,3,3,3,3,3,3,3,3,3,3,3,3,3,3,3,3,3,4),(329.867228626929,329.978610575364,
330.062357308066,330.146000985082,330.229561729148,330.313059591105,330.396522091667,
330.479967227159,330.563413062002,330.64687765724,330.730430842662,330.814028676234,
330.897760239096,330.977594077564,331.061340810266,331.144984487282,331.228545231348,
331.312043093305,331.395505593868,331.47895072936,331.562396564203,331.645861159441,
331.729414344863,331.813012178436,331.896743741298,331.976577579763,332.060324312465,
332.143967989481,332.227528733547,332.311026595504,332.394489096066,332.477934231559,
332.561380066401,332.64484466164,332.728397847061,332.811995680634,332.895727243496,
332.975561081962,333.059307814664,333.14295149168,333.226512235746,333.310010097703,
333.393472598265,333.476917733758,333.560363568601,333.643828163839,333.72738134926,
333.810979182833,333.894710745695,333.974544584161,334.058291316863,334.141934993879,
334.225495737945,334.308993599902,334.392456100465,334.475901235957,334.5593470708,
334.642811666038,334.72636485146,334.809962685032,334.893694247894,334.97352808636,
335.057274819062,335.140918496078,335.224479240144,335.307977102101,335.391439602663,
335.474884738155,335.558330572998,335.641795168236,335.725348353658,335.80894618723,
335.892677750092,335.972511588559,336.100376929765,336.150413934109),
 .UNSPECIFIED.);
#364=B_SPLINE_CURVE_WITH_KNOTS('',3,(#35676,#35677,#35678,#35679,#35680,
#35681,#35682,#35683,#35684,#35685,#35686,#35687,#35688,#35689,#35690,#35691,
#35692,#35693,#35694,#35695,#35696,#35697,#35698,#35699,#35700,#35701,#35702,
#35703,#35704,#35705,#35706,#35707,#35708,#35709,#35710,#35711,#35712,#35713,
#35714,#35715,#35716,#35717,#35718,#35719,#35720,#35721,#35722,#35723,#35724,
#35725,#35726,#35727,#35728,#35729,#35730,#35731,#35732,#35733,#35734,#35735,
#35736,#35737,#35738,#35739,#35740,#35741,#35742,#35743,#35744,#35745,#35746,
#35747,#35748,#35749,#35750,#35751,#35752,#35753,#35754,#35755,#35756,#35757,
#35758,#35759,#35760,#35761,#35762,#35763,#35764,#35765,#35766,#35767,#35768,
#35769,#35770,#35771,#35772,#35773,#35774,#35775,#35776,#35777,#35778,#35779,
#35780,#35781,#35782,#35783,#35784,#35785,#35786,#35787,#35788,#35789,#35790,
#35791,#35792,#35793,#35794,#35795,#35796,#35797,#35798,#35799,#35800,#35801,
#35802,#35803,#35804,#35805,#35806,#35807,#35808,#35809,#35810,#35811,#35812,
#35813,#35814,#35815,#35816,#35817,#35818,#35819,#35820,#35821,#35822,#35823,
#35824,#35825,#35826,#35827,#35828,#35829,#35830,#35831,#35832,#35833,#35834,
#35835,#35836,#35837,#35838,#35839,#35840,#35841,#35842,#35843,#35844,#35845,
#35846,#35847,#35848,#35849,#35850,#35851,#35852,#35853,#35854,#35855,#35856,
#35857,#35858,#35859,#35860,#35861,#35862,#35863,#35864,#35865,#35866,#35867,
#35868,#35869,#35870,#35871,#35872,#35873,#35874,#35875,#35876,#35877,#35878,
#35879,#35880,#35881,#35882,#35883,#35884,#35885,#35886,#35887,#35888,#35889,
#35890,#35891,#35892,#35893,#35894,#35895,#35896,#35897,#35898,#35899,#35900,
#35901,#35902,#35903,#35904),.UNSPECIFIED.,.F.,.F.,(4,3,3,3,3,3,3,3,3,3,
3,3,3,3,3,3,3,3,3,3,3,3,3,3,3,3,3,3,3,3,3,3,3,3,3,3,3,3,3,3,3,3,3,3,3,3,
3,3,3,3,3,3,3,3,3,3,3,3,3,3,3,3,3,3,3,3,3,3,3,3,3,3,3,3,3,3,4),(323.584043319926,
323.676068069459,323.768582031357,323.861348955712,323.954448704799,323.984709562169,
324.068456294871,324.152099971887,324.235660715953,324.31915857791,324.402621078473,
324.486066213965,324.569512048808,324.652976644046,324.736529829468,324.82012766304,
324.903859225902,324.983693064369,325.067439797071,325.151083474087,325.234644218154,
325.31814208011,325.401604580673,325.485049716165,325.568495551008,325.651960146246,
325.735513331668,325.819111165241,325.902842728103,325.982676566568,326.06642329927,
326.150066976286,326.233627720352,326.317125582309,326.400588082871,326.484033218363,
326.567479053206,326.650943648444,326.734496833866,326.818094667439,326.9018262303,
326.981660068767,327.065406801469,327.149050478485,327.232611222551,327.316109084508,
327.399571585071,327.483016720563,327.566462555406,327.649927150644,327.733480336066,
327.817078169638,327.9008097325,327.980643570966,328.064390303668,328.148033980684,
328.23159472475,328.315092586707,328.398555087269,328.482000222762,328.565446057604,
328.648910652842,328.732463838264,328.816061671837,328.899793234699,328.979627073165,
329.06226410214,329.144798916669,329.227252644958,329.309645552602,329.392006139001,
329.474353359022,329.556706154076,329.639126207836,329.72158115159,329.804147275148,
329.867228626794),.UNSPECIFIED.);
#365=B_SPLINE_CURVE_WITH_KNOTS('',3,(#35906,#35907,#35908,#35909,#35910,
#35911,#35912,#35913,#35914,#35915,#35916,#35917,#35918,#35919,#35920,#35921,
#35922,#35923,#35924,#35925,#35926,#35927,#35928,#35929,#35930,#35931,#35932,
#35933,#35934,#35935,#35936,#35937,#35938,#35939,#35940,#35941,#35942,#35943,
#35944,#35945,#35946,#35947,#35948,#35949,#35950,#35951,#35952,#35953,#35954,
#35955,#35956,#35957,#35958,#35959,#35960,#35961,#35962,#35963,#35964,#35965,
#35966,#35967,#35968,#35969,#35970,#35971,#35972,#35973,#35974,#35975,#35976,
#35977,#35978,#35979,#35980,#35981,#35982,#35983,#35984,#35985,#35986,#35987,
#35988,#35989,#35990,#35991,#35992,#35993,#35994,#35995,#35996,#35997,#35998,
#35999,#36000,#36001,#36002,#36003,#36004,#36005,#36006,#36007,#36008,#36009,
#36010,#36011,#36012,#36013,#36014,#36015,#36016,#36017,#36018,#36019,#36020,
#36021,#36022,#36023,#36024,#36025,#36026,#36027,#36028,#36029,#36030,#36031,
#36032,#36033,#36034,#36035,#36036,#36037,#36038,#36039,#36040,#36041,#36042,
#36043,#36044,#36045,#36046,#36047,#36048,#36049,#36050,#36051,#36052,#36053,
#36054,#36055,#36056,#36057,#36058,#36059,#36060,#36061,#36062,#36063,#36064,
#36065,#36066,#36067,#36068,#36069,#36070,#36071,#36072,#36073,#36074,#36075,
#36076,#36077,#36078,#36079,#36080,#36081,#36082,#36083,#36084,#36085,#36086,
#36087,#36088,#36089,#36090,#36091,#36092,#36093,#36094,#36095,#36096,#36097,
#36098,#36099,#36100,#36101,#36102,#36103,#36104,#36105,#36106,#36107,#36108,
#36109,#36110,#36111,#36112,#36113,#36114,#36115,#36116,#36117,#36118,#36119,
#36120,#36121,#36122,#36123,#36124,#36125,#36126,#36127,#36128,#36129,#36130,
#36131,#36132,#36133,#36134),.UNSPECIFIED.,.F.,.F.,(4,3,3,3,3,3,3,3,3,3,
3,3,3,3,3,3,3,3,3,3,3,3,3,3,3,3,3,3,3,3,3,3,3,3,3,3,3,3,3,3,3,3,3,3,3,3,
3,3,3,3,3,3,3,3,3,3,3,3,3,3,3,3,3,3,3,3,3,3,3,3,3,3,3,3,3,3,4),(317.30085801257,
317.387101829621,317.470165711623,317.553225128186,317.636298457177,317.719404082366,
317.802606138314,317.885865515104,317.96924500468,317.990808548974,318.074555281676,
318.158198958692,318.241759702758,318.325257564715,318.408720065278,318.49216520077,
318.575611035613,318.659075630852,318.742628816274,318.826226649846,318.909958212708,
318.989792051174,319.073538783876,319.157182460892,319.240743204958,319.324241066915,
319.407703567478,319.49114870297,319.574594537813,319.658059133051,319.741612318473,
319.825210152046,319.908941714908,319.988775553373,320.072522286075,320.156165963091,
320.239726707157,320.323224569114,320.406687069677,320.490132205169,320.573578040012,
320.65704263525,320.740595820671,320.824193654244,320.907925217106,320.987759055572,
321.071505788274,321.15514946529,321.238710209356,321.322208071313,321.405670571875,
321.489115707368,321.57256154221,321.656026137448,321.73957932287,321.823177156443,
321.906908719305,321.986742557771,322.070489290473,322.154132967489,322.237693711555,
322.321191573512,322.404654074075,322.488099209567,322.57154504441,322.655009639648,
322.73856282507,322.822160658643,322.905892221504,322.98572605997,323.070728963304,
323.15561926755,323.240413521352,323.326320970951,323.410962115911,323.497502717831,
323.58404331975),.UNSPECIFIED.);
#366=B_SPLINE_CURVE_WITH_KNOTS('',3,(#36136,#36137,#36138,#36139,#36140,
#36141,#36142,#36143,#36144,#36145,#36146,#36147,#36148,#36149,#36150,#36151,
#36152,#36153,#36154,#36155,#36156,#36157,#36158,#36159,#36160,#36161,#36162,
#36163,#36164,#36165,#36166,#36167,#36168,#36169,#36170,#36171,#36172,#36173,
#36174,#36175,#36176,#36177,#36178,#36179,#36180,#36181,#36182,#36183,#36184,
#36185,#36186,#36187,#36188,#36189,#36190,#36191,#36192,#36193,#36194,#36195,
#36196,#36197,#36198,#36199,#36200,#36201,#36202,#36203,#36204,#36205,#36206,
#36207,#36208,#36209,#36210,#36211,#36212,#36213,#36214,#36215,#36216,#36217,
#36218,#36219,#36220,#36221,#36222,#36223,#36224,#36225,#36226,#36227,#36228,
#36229,#36230,#36231,#36232,#36233,#36234,#36235,#36236,#36237,#36238,#36239,
#36240,#36241,#36242,#36243,#36244,#36245,#36246,#36247,#36248,#36249,#36250,
#36251,#36252,#36253,#36254,#36255,#36256,#36257,#36258,#36259,#36260,#36261,
#36262,#36263,#36264,#36265,#36266,#36267,#36268,#36269,#36270,#36271,#36272,
#36273,#36274,#36275,#36276,#36277,#36278,#36279,#36280,#36281,#36282,#36283,
#36284,#36285,#36286,#36287,#36288,#36289,#36290,#36291,#36292,#36293,#36294,
#36295,#36296,#36297,#36298,#36299,#36300,#36301,#36302,#36303,#36304,#36305,
#36306,#36307,#36308,#36309,#36310,#36311,#36312,#36313,#36314,#36315,#36316,
#36317,#36318,#36319,#36320,#36321,#36322,#36323,#36324,#36325,#36326,#36327,
#36328,#36329,#36330,#36331,#36332,#36333,#36334,#36335,#36336,#36337,#36338,
#36339,#36340,#36341,#36342,#36343,#36344,#36345,#36346,#36347,#36348,#36349,
#36350,#36351,#36352,#36353,#36354,#36355,#36356,#36357,#36358,#36359,#36360,
#36361),.UNSPECIFIED.,.F.,.F.,(4,3,3,3,3,3,3,3,3,3,3,3,3,3,3,3,3,3,3,3,
3,3,3,3,3,3,3,3,3,3,3,3,3,3,3,3,3,3,3,3,3,3,3,3,3,3,3,3,3,3,3,3,3,3,3,3,
3,3,3,3,3,3,3,3,3,3,3,3,3,3,3,3,3,3,3,4),(311.017672705574,311.101135357737,
311.184495573409,311.267773766953,311.350990278642,311.434173266364,311.517340510539,
311.600510335937,311.683701065398,311.766980643786,311.850307293392,311.933762367981,
311.996907535779,312.080654268481,312.164297945497,312.247858689563,312.33135655152,
312.414819052082,312.498264187575,312.581710022418,312.665174617655,312.748727803077,
312.83232563665,312.916057199512,312.995891037979,313.079637770681,313.163281447697,
313.246842191764,313.33034005372,313.413802554283,313.497247689775,313.580693524618,
313.664158119856,313.747711305278,313.831309138851,313.915040701713,313.994874540178,
314.07862127288,314.162264949896,314.245825693962,314.329323555919,314.412786056481,
314.496231191973,314.579677026816,314.663141622054,314.746694807476,314.830292641049,
314.914024203911,314.993858042377,315.077604775079,315.161248452095,315.244809196161,
315.328307058118,315.41176955868,315.495214694172,315.578660529015,315.662125124253,
315.745678309675,315.829276143247,315.913007706109,315.992841544576,316.076588277278,
316.160231954294,316.24379269836,316.327290560316,316.410753060879,316.494198196372,
316.577644031215,316.661108626452,316.744661811874,316.828259645447,316.911991208309,
316.991825046775,317.092784210493,317.196821111451,317.30085801241),
 .UNSPECIFIED.);
#367=B_SPLINE_CURVE_WITH_KNOTS('',3,(#36363,#36364,#36365,#36366,#36367,
#36368,#36369,#36370,#36371,#36372,#36373,#36374,#36375,#36376,#36377,#36378,
#36379,#36380,#36381,#36382,#36383,#36384,#36385,#36386,#36387,#36388,#36389,
#36390,#36391,#36392,#36393,#36394,#36395,#36396,#36397,#36398,#36399,#36400,
#36401,#36402,#36403,#36404,#36405,#36406,#36407,#36408,#36409,#36410,#36411,
#36412,#36413,#36414,#36415,#36416,#36417,#36418,#36419,#36420,#36421,#36422,
#36423,#36424,#36425,#36426,#36427,#36428,#36429,#36430,#36431,#36432,#36433,
#36434,#36435,#36436,#36437,#36438,#36439,#36440,#36441,#36442,#36443,#36444,
#36445,#36446,#36447,#36448,#36449,#36450,#36451,#36452,#36453,#36454,#36455,
#36456,#36457,#36458,#36459,#36460,#36461,#36462,#36463,#36464,#36465,#36466,
#36467,#36468,#36469,#36470,#36471,#36472,#36473,#36474,#36475,#36476,#36477,
#36478,#36479,#36480,#36481,#36482,#36483,#36484,#36485,#36486,#36487,#36488,
#36489,#36490,#36491,#36492,#36493,#36494,#36495,#36496,#36497,#36498,#36499,
#36500,#36501,#36502,#36503,#36504,#36505,#36506,#36507,#36508,#36509,#36510,
#36511,#36512,#36513,#36514,#36515,#36516,#36517,#36518,#36519,#36520,#36521,
#36522,#36523,#36524,#36525,#36526,#36527,#36528,#36529,#36530,#36531,#36532,
#36533,#36534,#36535,#36536,#36537,#36538,#36539,#36540,#36541,#36542,#36543,
#36544,#36545,#36546,#36547,#36548,#36549,#36550,#36551,#36552,#36553,#36554,
#36555,#36556,#36557,#36558,#36559,#36560,#36561,#36562,#36563,#36564,#36565,
#36566,#36567,#36568,#36569,#36570,#36571,#36572,#36573,#36574,#36575,#36576,
#36577,#36578,#36579,#36580,#36581,#36582,#36583,#36584,#36585,#36586,#36587,
#36588,#36589,#36590,#36591),.UNSPECIFIED.,.F.,.F.,(4,3,3,3,3,3,3,3,3,3,
3,3,3,3,3,3,3,3,3,3,3,3,3,3,3,3,3,3,3,3,3,3,3,3,3,3,3,3,3,3,3,3,3,3,3,3,
3,3,3,3,3,3,3,3,3,3,3,3,3,3,3,3,3,3,3,3,3,3,3,3,3,3,3,3,3,3,4),(304.734487398388,
304.838750950482,304.944872023283,305.004023020385,305.087769753087,305.171413430103,
305.25497417417,305.338472036127,305.421934536689,305.505379672182,305.588825507025,
305.672290102263,305.755843287685,305.839441121258,305.92317268412,306.003006522584,
306.086753255286,306.170396932302,306.253957676368,306.337455538325,306.420918038888,
306.50436317438,306.587809009223,306.671273604461,306.754826789883,306.838424623456,
306.922156186318,307.001990024784,307.085736757486,307.169380434502,307.252941178568,
307.336439040525,307.419901541088,307.50334667658,307.586792511423,307.670257106661,
307.753810292083,307.837408125656,307.921139688518,308.000973526983,308.084720259685,
308.168363936701,308.251924680767,308.335422542724,308.418885043286,308.502330178779,
308.585776013621,308.669240608859,308.752793794281,308.836391627854,308.920123190716,
308.999957029182,309.083703761884,309.1673474389,309.250908182966,309.334406044923,
309.417868545485,309.501313680978,309.58475951582,309.668224111058,309.75177729648,
309.835375130053,309.919106692915,309.998940531381,310.082687264083,310.166330941099,
310.249891685165,310.333389547122,310.416852047684,310.500297183177,310.583743018019,
310.667207613257,310.750760798679,310.834358632252,310.918090195114,310.99792403358,
311.017672705391),.UNSPECIFIED.);
#368=B_SPLINE_CURVE_WITH_KNOTS('',3,(#36593,#36594,#36595,#36596,#36597,
#36598,#36599,#36600,#36601,#36602,#36603,#36604,#36605,#36606,#36607,#36608,
#36609,#36610,#36611,#36612,#36613,#36614,#36615,#36616,#36617,#36618,#36619,
#36620,#36621,#36622,#36623,#36624,#36625,#36626,#36627,#36628,#36629,#36630,
#36631,#36632,#36633,#36634,#36635,#36636,#36637,#36638,#36639,#36640,#36641,
#36642,#36643,#36644,#36645,#36646,#36647,#36648,#36649,#36650,#36651,#36652,
#36653,#36654,#36655,#36656,#36657,#36658,#36659,#36660,#36661,#36662,#36663,
#36664,#36665,#36666,#36667,#36668,#36669,#36670,#36671,#36672,#36673,#36674,
#36675,#36676,#36677,#36678,#36679,#36680,#36681,#36682,#36683,#36684,#36685,
#36686,#36687,#36688,#36689,#36690,#36691,#36692,#36693,#36694,#36695,#36696,
#36697,#36698,#36699,#36700,#36701,#36702,#36703,#36704,#36705,#36706,#36707,
#36708,#36709,#36710,#36711,#36712,#36713,#36714,#36715,#36716,#36717,#36718,
#36719,#36720,#36721,#36722,#36723,#36724,#36725,#36726,#36727,#36728,#36729,
#36730,#36731,#36732,#36733,#36734,#36735,#36736,#36737,#36738,#36739,#36740,
#36741,#36742,#36743,#36744,#36745,#36746,#36747,#36748,#36749,#36750,#36751,
#36752,#36753,#36754,#36755,#36756,#36757,#36758,#36759,#36760,#36761,#36762,
#36763,#36764,#36765,#36766,#36767,#36768,#36769,#36770,#36771,#36772,#36773,
#36774,#36775,#36776,#36777,#36778,#36779,#36780,#36781,#36782,#36783,#36784,
#36785,#36786,#36787,#36788,#36789,#36790,#36791,#36792,#36793,#36794,#36795,
#36796,#36797,#36798,#36799,#36800,#36801,#36802,#36803,#36804,#36805,#36806,
#36807,#36808,#36809,#36810,#36811,#36812,#36813,#36814,#36815,#36816,#36817,
#36818,#36819,#36820,#36821),.UNSPECIFIED.,.F.,.F.,(4,3,3,3,3,3,3,3,3,3,
3,3,3,3,3,3,3,3,3,3,3,3,3,3,3,3,3,3,3,3,3,3,3,3,3,3,3,3,3,3,3,3,3,3,3,3,
3,3,3,3,3,3,3,3,3,3,3,3,3,3,3,3,3,3,3,3,3,3,3,3,3,3,3,3,3,3,4),(298.451302091032,
298.536850673596,298.622451210915,298.708117991808,298.793927219197,298.879815482329,
298.965860496585,299.01012200719,299.093868739892,299.177512416908,299.261073160974,
299.344571022931,299.428033523493,299.511478658985,299.594924493828,299.678389089066,
299.761942274488,299.845540108061,299.929271670923,300.009105509389,300.092852242091,
300.176495919107,300.260056663173,300.34355452513,300.427017025693,300.510462161185,
300.593907996028,300.677372591266,300.760925776688,300.844523610261,300.928255173123,
301.008089011589,301.091835744291,301.175479421307,301.259040165374,301.342538027331,
301.426000527893,301.509445663386,301.592891498228,301.676356093467,301.759909278889,
301.843507112461,301.927238675323,302.007072513788,302.09081924649,302.174462923506,
302.258023667572,302.341521529529,302.424984030092,302.508429165584,302.591875000427,
302.675339595664,302.758892781086,302.842490614659,302.92622217752,303.006056015987,
303.089802748689,303.173446425705,303.257007169771,303.340505031727,303.42396753229,
303.507412667782,303.590858502625,303.674323097863,303.757876283285,303.841474116858,
303.925205679719,304.005039518186,304.087992711044,304.170814757054,304.253561341555,
304.336251293512,304.418903394483,304.501555863992,304.584205613442,304.666907824822,
304.734487398211),.UNSPECIFIED.);
#369=B_SPLINE_CURVE_WITH_KNOTS('',3,(#36823,#36824,#36825,#36826,#36827,
#36828,#36829,#36830,#36831,#36832,#36833,#36834,#36835,#36836,#36837,#36838,
#36839,#36840,#36841,#36842,#36843,#36844,#36845,#36846,#36847,#36848,#36849,
#36850,#36851,#36852,#36853,#36854,#36855,#36856,#36857,#36858,#36859,#36860,
#36861,#36862,#36863,#36864,#36865,#36866,#36867,#36868,#36869,#36870,#36871,
#36872,#36873,#36874,#36875,#36876,#36877,#36878,#36879,#36880,#36881,#36882,
#36883,#36884,#36885,#36886,#36887,#36888,#36889,#36890,#36891,#36892,#36893,
#36894,#36895,#36896,#36897,#36898,#36899,#36900,#36901,#36902,#36903,#36904,
#36905,#36906,#36907,#36908,#36909,#36910,#36911,#36912,#36913,#36914,#36915,
#36916,#36917,#36918,#36919,#36920,#36921,#36922,#36923,#36924,#36925,#36926,
#36927,#36928,#36929,#36930,#36931,#36932,#36933,#36934,#36935,#36936,#36937,
#36938,#36939,#36940,#36941,#36942,#36943,#36944,#36945,#36946,#36947,#36948,
#36949,#36950,#36951,#36952,#36953,#36954,#36955,#36956,#36957,#36958,#36959,
#36960,#36961,#36962,#36963,#36964,#36965,#36966,#36967,#36968,#36969,#36970,
#36971,#36972,#36973,#36974,#36975,#36976,#36977,#36978,#36979,#36980,#36981,
#36982,#36983,#36984,#36985,#36986,#36987,#36988,#36989,#36990,#36991,#36992,
#36993,#36994,#36995,#36996,#36997,#36998,#36999,#37000,#37001,#37002,#37003,
#37004,#37005,#37006,#37007,#37008,#37009,#37010,#37011,#37012,#37013,#37014,
#37015,#37016,#37017,#37018,#37019,#37020,#37021,#37022,#37023,#37024,#37025,
#37026,#37027,#37028,#37029,#37030,#37031,#37032,#37033,#37034,#37035,#37036,
#37037,#37038,#37039,#37040,#37041,#37042,#37043,#37044,#37045,#37046,#37047,
#37048,#37049,#37050,#37051),.UNSPECIFIED.,.F.,.F.,(4,3,3,3,3,3,3,3,3,3,
3,3,3,3,3,3,3,3,3,3,3,3,3,3,3,3,3,3,3,3,3,3,3,3,3,3,3,3,3,3,3,3,3,3,3,3,
3,3,3,3,3,3,3,3,3,3,3,3,3,3,3,3,3,3,3,3,3,3,3,3,3,3,3,3,3,3,4),(292.168116783963,
292.250528923154,292.332859281583,292.418279495635,292.500516709425,292.582741209567,
292.664972016471,292.747228153625,292.829572299424,292.911968827067,292.994480032763,
293.016220993995,293.099967726697,293.183611403713,293.267172147779,293.350670009736,
293.434132510299,293.517577645791,293.601023480634,293.684488075872,293.768041261294,
293.851639094867,293.935370657729,294.015204496194,294.098951228896,294.182594905912,
294.266155649978,294.349653511935,294.433116012497,294.51656114799,294.600006982832,
294.68347157807,294.767024763492,294.850622597065,294.934354159927,295.014187998394,
295.097934731096,295.181578408112,295.265139152179,295.348637014135,295.432099514698,
295.51554465019,295.598990485033,295.682455080272,295.766008265694,295.849606099267,
295.933337662129,296.013171500593,296.096918233295,296.180561910311,296.264122654377,
296.347620516334,296.431083016896,296.514528152388,296.597973987231,296.681438582469,
296.76499176789,296.848589601463,296.932321164325,297.012155002792,297.095901735494,
297.17954541251,297.263106156576,297.346604018533,297.430066519095,297.513511654588,
297.59695748943,297.680422084669,297.76397527009,297.847573103663,297.931304666525,
298.011138504991,298.10192502492,298.192405175669,298.282698199155,298.372692110768,
298.451302090907),.UNSPECIFIED.);
#370=B_SPLINE_CURVE_WITH_KNOTS('',3,(#37053,#37054,#37055,#37056,#37057,
#37058,#37059,#37060,#37061,#37062,#37063,#37064,#37065,#37066,#37067,#37068,
#37069,#37070,#37071,#37072,#37073,#37074,#37075,#37076,#37077,#37078,#37079,
#37080,#37081,#37082,#37083,#37084,#37085,#37086,#37087,#37088,#37089,#37090,
#37091,#37092,#37093,#37094,#37095,#37096,#37097,#37098,#37099,#37100,#37101,
#37102,#37103,#37104,#37105,#37106,#37107,#37108,#37109,#37110,#37111,#37112,
#37113,#37114,#37115,#37116,#37117,#37118,#37119,#37120,#37121,#37122,#37123,
#37124,#37125,#37126,#37127,#37128,#37129,#37130,#37131,#37132,#37133,#37134,
#37135,#37136,#37137,#37138,#37139,#37140,#37141,#37142,#37143,#37144,#37145,
#37146,#37147,#37148,#37149,#37150,#37151,#37152,#37153,#37154,#37155,#37156,
#37157,#37158,#37159,#37160,#37161,#37162,#37163,#37164,#37165,#37166,#37167,
#37168,#37169,#37170,#37171,#37172,#37173,#37174,#37175,#37176,#37177,#37178,
#37179,#37180,#37181,#37182,#37183,#37184,#37185,#37186,#37187,#37188,#37189,
#37190,#37191,#37192,#37193,#37194,#37195,#37196,#37197,#37198,#37199,#37200,
#37201,#37202,#37203,#37204,#37205,#37206,#37207,#37208,#37209,#37210,#37211,
#37212,#37213,#37214,#37215,#37216,#37217,#37218,#37219,#37220,#37221,#37222,
#37223,#37224,#37225,#37226,#37227,#37228,#37229,#37230,#37231,#37232,#37233,
#37234,#37235,#37236,#37237,#37238,#37239,#37240,#37241,#37242,#37243,#37244,
#37245,#37246,#37247,#37248,#37249,#37250,#37251,#37252,#37253,#37254,#37255,
#37256,#37257,#37258,#37259,#37260,#37261,#37262,#37263,#37264,#37265,#37266,
#37267,#37268,#37269,#37270,#37271,#37272,#37273,#37274,#37275,#37276,#37277,
#37278),.UNSPECIFIED.,.F.,.F.,(4,3,3,3,3,3,3,3,3,3,3,3,3,3,3,3,3,3,3,3,
3,3,3,3,3,3,3,3,3,3,3,3,3,3,3,3,3,3,3,3,3,3,3,3,3,3,3,3,3,3,3,3,3,3,3,3,
3,3,3,3,3,3,3,3,3,3,3,3,3,3,3,3,3,3,3,4),(285.884931476672,286.023336478601,
286.107083211303,286.190726888319,286.274287632385,286.357785494342,286.441247994905,
286.524693130397,286.60813896524,286.691603560478,286.7751567459,286.858754579472,
286.942486142334,287.0223199808,287.106066713502,287.189710390518,287.273271134584,
287.356768996541,287.440231497104,287.523676632596,287.607122467439,287.690587062677,
287.774140248099,287.857738081671,287.941469644533,288.021303482999,288.105050215701,
288.188693892717,288.272254636783,288.35575249874,288.439214999303,288.522660134795,
288.606105969638,288.689570564876,288.773123750298,288.85672158387,288.940453146732,
289.020286985199,289.104033717901,289.187677394917,289.271238138984,289.35473600094,
289.438198501503,289.521643636995,289.605089471838,289.688554067076,289.772107252498,
289.855705086071,289.939436648933,290.019270487398,290.1030172201,290.186660897116,
290.270221641182,290.353719503139,290.437182003701,290.520627139194,290.604072974037,
290.687537569275,290.771090754697,290.854688588269,290.938420151131,291.018253989597,
291.102000722299,291.185644399315,291.269205143381,291.352703005338,291.4361655059,
291.519610641392,291.603056476235,291.686521071473,291.770074256895,291.853672090467,
291.937403653329,292.017237491796,292.158686771192,292.168116783852),
 .UNSPECIFIED.);
#371=B_SPLINE_CURVE_WITH_KNOTS('',3,(#37280,#37281,#37282,#37283,#37284,
#37285,#37286,#37287,#37288,#37289,#37290,#37291,#37292,#37293,#37294,#37295,
#37296,#37297,#37298,#37299,#37300,#37301,#37302,#37303,#37304,#37305,#37306,
#37307,#37308,#37309,#37310,#37311,#37312,#37313,#37314,#37315,#37316,#37317,
#37318,#37319,#37320,#37321,#37322,#37323,#37324,#37325,#37326,#37327,#37328,
#37329,#37330,#37331,#37332,#37333,#37334,#37335,#37336,#37337,#37338,#37339,
#37340,#37341,#37342,#37343,#37344,#37345,#37346,#37347,#37348,#37349,#37350,
#37351,#37352,#37353,#37354,#37355,#37356,#37357,#37358,#37359,#37360,#37361,
#37362,#37363,#37364,#37365,#37366,#37367,#37368,#37369,#37370,#37371,#37372,
#37373,#37374,#37375,#37376,#37377,#37378,#37379,#37380,#37381,#37382,#37383,
#37384,#37385,#37386,#37387,#37388,#37389,#37390,#37391,#37392,#37393,#37394,
#37395,#37396,#37397,#37398,#37399,#37400,#37401,#37402,#37403,#37404,#37405,
#37406,#37407,#37408,#37409,#37410,#37411,#37412,#37413,#37414,#37415,#37416,
#37417,#37418,#37419,#37420,#37421,#37422,#37423,#37424,#37425,#37426,#37427,
#37428,#37429,#37430,#37431,#37432,#37433,#37434,#37435,#37436,#37437,#37438,
#37439,#37440,#37441,#37442,#37443,#37444,#37445,#37446,#37447,#37448,#37449,
#37450,#37451,#37452,#37453,#37454,#37455,#37456,#37457,#37458,#37459,#37460,
#37461,#37462,#37463,#37464,#37465,#37466,#37467,#37468,#37469,#37470,#37471,
#37472,#37473,#37474,#37475,#37476,#37477,#37478,#37479,#37480,#37481,#37482,
#37483,#37484,#37485,#37486,#37487,#37488,#37489,#37490,#37491,#37492,#37493,
#37494,#37495,#37496,#37497,#37498,#37499,#37500,#37501,#37502,#37503,#37504,
#37505,#37506,#37507,#37508),.UNSPECIFIED.,.F.,.F.,(4,3,3,3,3,3,3,3,3,3,
3,3,3,3,3,3,3,3,3,3,3,3,3,3,3,3,3,3,3,3,3,3,3,3,3,3,3,3,3,3,3,3,3,3,3,3,
3,3,3,3,3,3,3,3,3,3,3,3,3,3,3,3,3,3,3,3,3,3,3,3,3,3,3,3,3,3,4),(279.601746169493,
279.692274093846,279.783190578907,279.874304142487,279.965719750968,280.029435465406,
280.113182198108,280.196825875124,280.28038661919,280.363884481147,280.447346981709,
280.530792117201,280.614237952044,280.697702547282,280.781255732704,280.864853566276,
280.948585129138,281.028418967605,281.112165700307,281.195809377323,281.279370121389,
281.362867983346,281.446330483909,281.529775619401,281.613221454244,281.696686049482,
281.780239234904,281.863837068477,281.947568631339,282.027402469804,282.111149202506,
282.194792879522,282.278353623588,282.361851485545,282.445313986108,282.5287591216,
282.612204956443,282.695669551681,282.779222737103,282.862820570676,282.946552133538,
283.026385972004,283.110132704706,283.193776381722,283.277337125788,283.360834987745,
283.444297488308,283.5277426238,283.611188458643,283.694653053881,283.778206239303,
283.861804072876,283.945535635738,284.025369474203,284.109116206905,284.192759883921,
284.276320627987,284.359818489944,284.443280990507,284.526726125999,284.610171960842,
284.69363655608,284.777189741502,284.860787575074,284.944519137936,285.024352976402,
285.106888703548,285.189322170556,285.271674581163,285.353965488497,285.436224067443,
285.518469335565,285.600720296674,285.683033431969,285.765381886047,285.847828289346,
285.88493147655),.UNSPECIFIED.);
#372=B_SPLINE_CURVE_WITH_KNOTS('',3,(#37510,#37511,#37512,#37513,#37514,
#37515,#37516,#37517,#37518,#37519),.UNSPECIFIED.,.F.,.F.,(4,1,1,1,1,1,
1,4),(273.318560862313,274.035534452211,275.03451795441,276.033501456609,
277.032484958809,278.031468461008,279.030451963207,279.601746169493),
 .UNSPECIFIED.);
#373=B_SPLINE_CURVE_WITH_KNOTS('',3,(#37521,#37522,#37523,#37524,#37525,
#37526,#37527,#37528,#37529,#37530,#37531,#37532,#37533,#37534,#37535,#37536,
#37537,#37538,#37539,#37540,#37541,#37542,#37543,#37544,#37545,#37546,#37547,
#37548,#37549,#37550,#37551,#37552,#37553,#37554,#37555,#37556,#37557,#37558,
#37559,#37560,#37561,#37562,#37563,#37564,#37565,#37566,#37567,#37568,#37569,
#37570,#37571,#37572,#37573,#37574,#37575,#37576,#37577,#37578,#37579,#37580,
#37581,#37582,#37583,#37584,#37585,#37586,#37587,#37588,#37589,#37590,#37591,
#37592,#37593,#37594,#37595,#37596,#37597,#37598,#37599,#37600,#37601,#37602,
#37603,#37604,#37605,#37606,#37607,#37608,#37609,#37610,#37611,#37612,#37613,
#37614,#37615,#37616,#37617,#37618,#37619,#37620,#37621,#37622,#37623,#37624,
#37625,#37626,#37627,#37628,#37629,#37630,#37631,#37632,#37633,#37634,#37635,
#37636,#37637,#37638,#37639,#37640,#37641,#37642,#37643,#37644,#37645,#37646,
#37647,#37648,#37649,#37650,#37651,#37652,#37653,#37654,#37655,#37656,#37657,
#37658,#37659,#37660,#37661,#37662,#37663,#37664,#37665,#37666,#37667,#37668,
#37669,#37670,#37671,#37672,#37673,#37674,#37675,#37676,#37677,#37678,#37679,
#37680,#37681,#37682,#37683,#37684,#37685,#37686,#37687,#37688,#37689,#37690,
#37691,#37692,#37693,#37694,#37695,#37696,#37697,#37698,#37699,#37700,#37701,
#37702,#37703,#37704,#37705,#37706,#37707,#37708,#37709,#37710,#37711,#37712,
#37713,#37714,#37715,#37716,#37717,#37718,#37719,#37720,#37721,#37722,#37723,
#37724,#37725,#37726,#37727,#37728,#37729,#37730,#37731,#37732,#37733,#37734,
#37735,#37736,#37737,#37738,#37739,#37740,#37741,#37742,#37743,#37744,#37745,
#37746,#37747,#37748,#37749),.UNSPECIFIED.,.F.,.F.,(4,3,3,3,3,3,3,3,3,3,
3,3,3,3,3,3,3,3,3,3,3,3,3,3,3,3,3,3,3,3,3,3,3,3,3,3,3,3,3,3,3,3,3,3,3,3,
3,3,3,3,3,3,3,3,3,3,3,3,3,3,3,3,3,3,3,3,3,3,3,3,3,3,3,3,3,3,4),(267.035375555134,
267.042649936817,267.126396669519,267.210040346535,267.293601090601,267.377098952558,
267.460561453121,267.544006588613,267.627452423456,267.710917018694,267.794470204116,
267.878068037689,267.961799600551,268.041633439016,268.125380171718,268.209023848734,
268.2925845928,268.376082454757,268.45954495532,268.542990090812,268.626435925655,
268.709900520893,268.793453706314,268.877051539887,268.960783102749,269.040616941215,
269.124363673917,269.208007350933,269.291568094999,269.375065956956,269.458528457519,
269.541973593011,269.625419427854,269.708884023092,269.792437208514,269.876035042087,
269.959766604949,270.039600443414,270.123347176116,270.206990853132,270.290551597198,
270.374049459155,270.457511959718,270.54095709521,270.624402930053,270.707867525291,
270.791420710713,270.875018544286,270.958750107147,271.038583945614,271.122330678316,
271.205974355332,271.289535099398,271.373032961355,271.456495461918,271.53994059741,
271.623386432253,271.706851027491,271.790404212913,271.874002046486,271.957733609348,
272.037567447813,272.121314180515,272.204957857531,272.288518601597,272.372016463554,
272.455478964116,272.538924099609,272.622369934452,272.70583452969,272.789387715111,
272.872985548684,272.956717111546,273.036550950012,273.140987376872,273.243878527479,
273.318560862313),.UNSPECIFIED.);
#374=B_SPLINE_CURVE_WITH_KNOTS('',3,(#37751,#37752,#37753,#37754,#37755,
#37756,#37757,#37758,#37759,#37760,#37761,#37762,#37763,#37764,#37765,#37766,
#37767,#37768,#37769,#37770,#37771,#37772,#37773,#37774,#37775,#37776,#37777,
#37778,#37779,#37780,#37781,#37782,#37783,#37784,#37785,#37786,#37787,#37788,
#37789,#37790,#37791,#37792,#37793,#37794,#37795,#37796,#37797,#37798,#37799,
#37800,#37801,#37802,#37803,#37804,#37805,#37806,#37807,#37808,#37809,#37810,
#37811,#37812,#37813,#37814,#37815,#37816,#37817,#37818,#37819,#37820,#37821,
#37822,#37823,#37824,#37825,#37826,#37827,#37828,#37829,#37830,#37831,#37832,
#37833,#37834,#37835,#37836,#37837,#37838,#37839,#37840,#37841,#37842,#37843,
#37844,#37845,#37846,#37847,#37848,#37849,#37850,#37851,#37852,#37853,#37854,
#37855,#37856,#37857,#37858,#37859,#37860,#37861,#37862,#37863,#37864,#37865,
#37866,#37867,#37868,#37869,#37870,#37871,#37872,#37873,#37874,#37875,#37876,
#37877,#37878,#37879,#37880,#37881,#37882,#37883,#37884,#37885,#37886,#37887,
#37888,#37889,#37890,#37891,#37892,#37893,#37894,#37895,#37896,#37897,#37898,
#37899,#37900,#37901,#37902,#37903,#37904,#37905,#37906,#37907,#37908,#37909,
#37910,#37911,#37912,#37913,#37914,#37915,#37916,#37917,#37918,#37919,#37920,
#37921,#37922,#37923,#37924,#37925,#37926,#37927,#37928,#37929,#37930,#37931,
#37932,#37933,#37934,#37935,#37936,#37937,#37938,#37939,#37940,#37941,#37942,
#37943,#37944,#37945,#37946,#37947,#37948,#37949,#37950,#37951,#37952,#37953,
#37954,#37955,#37956,#37957,#37958,#37959,#37960,#37961,#37962,#37963,#37964,
#37965,#37966,#37967,#37968,#37969,#37970,#37971,#37972,#37973,#37974,#37975,
#37976),.UNSPECIFIED.,.F.,.F.,(4,3,3,3,3,3,3,3,3,3,3,3,3,3,3,3,3,3,3,3,
3,3,3,3,3,3,3,3,3,3,3,3,3,3,3,3,3,3,3,3,3,3,3,3,3,3,3,3,3,3,3,3,3,3,3,3,
3,3,3,3,3,3,3,3,3,3,3,3,3,3,3,3,3,3,3,4),(260.752190248095,260.853081327826,
260.955336834719,261.048748923622,261.132495656324,261.21613933334,261.299700077406,
261.383197939363,261.466660439926,261.550105575418,261.633551410261,261.717016005499,
261.80056919092,261.884167024493,261.967898587355,262.047732425821,262.131479158523,
262.215122835539,262.298683579605,262.382181441562,262.465643942124,262.549089077617,
262.632534912459,262.715999507697,262.799552693119,262.883150526692,262.966882089554,
263.04671592802,263.130462660722,263.214106337738,263.297667081804,263.381164943761,
263.464627444324,263.548072579816,263.631518414659,263.714983009897,263.798536195319,
263.882134028891,263.965865591753,264.045699430219,264.129446162921,264.213089839937,
264.296650584003,264.38014844596,264.463610946523,264.547056082015,264.630501916858,
264.713966512096,264.797519697518,264.881117531091,264.964849093953,265.044682932419,
265.128429665121,265.212073342137,265.295634086204,265.37913194816,265.462594448723,
265.546039584215,265.629485419058,265.712950014296,265.796503199718,265.880101033291,
265.963832596153,266.043666434618,266.127304946033,266.2108404585,266.294293211055,
266.377683369963,266.461038639883,266.544377018387,266.627716673381,266.711075769832,
266.794523426635,266.878016543539,266.961641353193,267.035375554993),
 .UNSPECIFIED.);
#375=B_SPLINE_CURVE_WITH_KNOTS('',3,(#37978,#37979,#37980,#37981,#37982,
#37983,#37984,#37985,#37986,#37987,#37988,#37989,#37990,#37991,#37992,#37993,
#37994,#37995,#37996,#37997,#37998,#37999,#38000,#38001,#38002,#38003,#38004,
#38005,#38006,#38007,#38008,#38009,#38010,#38011,#38012,#38013,#38014,#38015,
#38016,#38017,#38018,#38019,#38020,#38021,#38022,#38023,#38024,#38025,#38026,
#38027,#38028,#38029,#38030,#38031,#38032,#38033,#38034,#38035,#38036,#38037,
#38038,#38039,#38040,#38041,#38042,#38043,#38044,#38045,#38046,#38047,#38048,
#38049,#38050,#38051,#38052,#38053,#38054,#38055,#38056,#38057,#38058,#38059,
#38060,#38061,#38062,#38063,#38064,#38065,#38066,#38067,#38068,#38069,#38070,
#38071,#38072,#38073,#38074,#38075,#38076,#38077,#38078,#38079,#38080,#38081,
#38082,#38083,#38084,#38085,#38086,#38087,#38088,#38089,#38090,#38091,#38092,
#38093,#38094,#38095,#38096,#38097,#38098,#38099,#38100,#38101,#38102,#38103,
#38104,#38105,#38106,#38107,#38108,#38109,#38110,#38111,#38112,#38113,#38114,
#38115,#38116,#38117,#38118,#38119,#38120,#38121,#38122,#38123,#38124,#38125,
#38126,#38127,#38128,#38129,#38130,#38131,#38132,#38133,#38134,#38135,#38136,
#38137,#38138,#38139,#38140,#38141,#38142,#38143,#38144,#38145,#38146,#38147,
#38148,#38149,#38150,#38151,#38152,#38153,#38154,#38155,#38156,#38157,#38158,
#38159,#38160,#38161,#38162,#38163,#38164,#38165,#38166,#38167,#38168,#38169,
#38170,#38171,#38172,#38173,#38174,#38175,#38176,#38177,#38178,#38179,#38180,
#38181,#38182,#38183,#38184,#38185,#38186,#38187,#38188,#38189,#38190,#38191,
#38192,#38193,#38194,#38195,#38196,#38197,#38198,#38199,#38200,#38201,#38202,
#38203,#38204,#38205,#38206),.UNSPECIFIED.,.F.,.F.,(4,3,3,3,3,3,3,3,3,3,
3,3,3,3,3,3,3,3,3,3,3,3,3,3,3,3,3,3,3,3,3,3,3,3,3,3,3,3,3,3,3,3,3,3,3,3,
3,3,3,3,3,3,3,3,3,3,3,3,3,3,3,3,3,3,3,3,3,3,3,3,3,3,3,3,3,3,4),(254.469004940775,
254.553878218561,254.638782764637,254.723734366107,254.808811034956,254.893952704628,
254.979252035181,255.054847910427,255.138594643129,255.222238320145,255.305799064211,
255.389296926168,255.47275942673,255.556204562223,255.639650397065,255.723114992303,
255.806668177725,255.890266011298,255.97399757416,256.053831412626,256.137578145328,
256.221221822344,256.30478256641,256.388280428367,256.47174292893,256.555188064422,
256.638633899265,256.722098494503,256.805651679925,256.889249513498,256.97298107636,
257.052814914825,257.136561647527,257.220205324543,257.303766068609,257.387263930566,
257.470726431129,257.554171566621,257.637617401464,257.721081996702,257.804635182123,
257.888233015696,257.971964578558,258.051798417024,258.135545149726,258.219188826742,
258.302749570808,258.386247432765,258.469709933328,258.55315506882,258.636600903663,
258.720065498901,258.803618684323,258.887216517896,258.970948080758,259.050781919224,
259.134528651926,259.218172328942,259.301733073008,259.385230934965,259.468693435527,
259.55213857102,259.635584405862,259.7190490011,259.802602186522,259.886200020095,
259.969931582957,260.049765421423,260.133000554424,260.216101211117,260.299124012296,
260.38208757138,260.465010454567,260.547924974296,260.630834260175,260.713780358084,
260.752190247954),.UNSPECIFIED.);
#376=B_SPLINE_CURVE_WITH_KNOTS('',3,(#38208,#38209,#38210,#38211,#38212,
#38213,#38214,#38215,#38216,#38217,#38218,#38219,#38220,#38221,#38222,#38223,
#38224,#38225,#38226,#38227,#38228,#38229,#38230,#38231,#38232,#38233,#38234,
#38235,#38236,#38237,#38238,#38239,#38240,#38241,#38242,#38243,#38244,#38245,
#38246,#38247,#38248,#38249,#38250,#38251,#38252,#38253,#38254,#38255,#38256,
#38257,#38258,#38259,#38260,#38261,#38262,#38263,#38264,#38265,#38266,#38267,
#38268,#38269,#38270,#38271,#38272,#38273,#38274,#38275,#38276,#38277,#38278,
#38279,#38280,#38281,#38282,#38283,#38284,#38285,#38286,#38287,#38288,#38289,
#38290,#38291,#38292,#38293,#38294,#38295,#38296,#38297,#38298,#38299,#38300,
#38301,#38302,#38303,#38304,#38305,#38306,#38307,#38308,#38309,#38310,#38311,
#38312,#38313,#38314,#38315,#38316,#38317,#38318,#38319,#38320,#38321,#38322,
#38323,#38324,#38325,#38326,#38327,#38328,#38329,#38330,#38331,#38332,#38333,
#38334,#38335,#38336,#38337,#38338,#38339,#38340,#38341,#38342,#38343,#38344,
#38345,#38346,#38347,#38348,#38349,#38350,#38351,#38352,#38353,#38354,#38355,
#38356,#38357,#38358,#38359,#38360,#38361,#38362,#38363,#38364,#38365,#38366,
#38367,#38368,#38369,#38370,#38371,#38372,#38373,#38374,#38375,#38376,#38377,
#38378,#38379,#38380,#38381,#38382,#38383,#38384,#38385,#38386,#38387,#38388,
#38389,#38390,#38391,#38392,#38393,#38394,#38395,#38396,#38397,#38398,#38399,
#38400,#38401,#38402,#38403,#38404,#38405,#38406,#38407,#38408,#38409,#38410,
#38411,#38412,#38413,#38414,#38415,#38416,#38417,#38418,#38419,#38420,#38421,
#38422,#38423,#38424,#38425,#38426,#38427,#38428,#38429,#38430,#38431,#38432,
#38433,#38434,#38435,#38436),.UNSPECIFIED.,.F.,.F.,(4,3,3,3,3,3,3,3,3,3,
3,3,3,3,3,3,3,3,3,3,3,3,3,3,3,3,3,3,3,3,3,3,3,3,3,3,3,3,3,3,3,3,3,3,3,3,
3,3,3,3,3,3,3,3,3,3,3,3,3,3,3,3,3,3,3,3,3,3,3,3,3,3,3,3,3,3,4),(248.185819633726,
248.268331196131,248.350754928891,248.433111935712,248.515429379703,248.597727820277,
248.680026236115,248.762343603558,248.844746147529,248.927195249346,249.009767054777,
249.060946897232,249.144693629934,249.22833730695,249.311898051016,249.395395912973,
249.478858413536,249.562303549028,249.645749383871,249.729213979109,249.812767164531,
249.896364998103,249.980096560965,250.059930399431,250.143677132133,250.227320809149,
250.310881553215,250.394379415172,250.477841915734,250.561287051227,250.64473288607,
250.728197481308,250.811750666729,250.895348500302,250.979080063164,251.05891390163,
251.142660634332,251.226304311348,251.309865055414,251.393362917371,251.476825417934,
251.560270553426,251.643716388268,251.727180983507,251.810734168929,251.894332002501,
251.978063565363,252.057897403829,252.141644136531,252.225287813547,252.308848557614,
252.392346419571,252.475808920134,252.559254055626,252.642699890469,252.726164485707,
252.809717671128,252.893315504701,252.977047067563,253.056880906029,253.140627638731,
253.224271315746,253.307832059813,253.39132992177,253.474792422332,253.558237557825,
253.641683392668,253.725147987906,253.808701173327,253.8922990069,253.976030569762,
254.055864408228,254.148202186826,254.240178487622,254.331921438503,254.42329568607,
254.46900494061),.UNSPECIFIED.);
#377=B_SPLINE_CURVE_WITH_KNOTS('',3,(#38438,#38439,#38440,#38441,#38442,
#38443,#38444,#38445,#38446,#38447,#38448,#38449,#38450,#38451,#38452,#38453,
#38454,#38455,#38456,#38457,#38458,#38459,#38460,#38461,#38462,#38463,#38464,
#38465,#38466,#38467,#38468,#38469,#38470,#38471,#38472,#38473,#38474,#38475,
#38476,#38477,#38478,#38479,#38480,#38481,#38482,#38483,#38484,#38485,#38486,
#38487,#38488,#38489,#38490,#38491,#38492,#38493,#38494,#38495,#38496,#38497,
#38498,#38499,#38500,#38501,#38502,#38503,#38504,#38505,#38506,#38507,#38508,
#38509,#38510,#38511,#38512,#38513,#38514,#38515,#38516,#38517,#38518,#38519,
#38520,#38521,#38522,#38523,#38524,#38525,#38526,#38527,#38528,#38529,#38530,
#38531,#38532,#38533,#38534,#38535,#38536,#38537,#38538,#38539,#38540,#38541,
#38542,#38543,#38544,#38545,#38546,#38547,#38548,#38549,#38550,#38551,#38552,
#38553,#38554,#38555,#38556,#38557,#38558,#38559,#38560,#38561,#38562,#38563,
#38564,#38565,#38566,#38567,#38568,#38569,#38570,#38571,#38572,#38573,#38574,
#38575,#38576,#38577,#38578,#38579,#38580,#38581,#38582,#38583,#38584,#38585,
#38586,#38587,#38588,#38589,#38590,#38591,#38592,#38593,#38594,#38595,#38596,
#38597,#38598,#38599,#38600,#38601,#38602,#38603,#38604,#38605,#38606,#38607,
#38608,#38609,#38610,#38611,#38612,#38613,#38614,#38615,#38616,#38617,#38618,
#38619,#38620,#38621,#38622,#38623,#38624,#38625,#38626,#38627,#38628,#38629,
#38630,#38631,#38632,#38633,#38634,#38635,#38636,#38637,#38638,#38639,#38640,
#38641,#38642,#38643,#38644,#38645,#38646,#38647,#38648,#38649,#38650,#38651,
#38652,#38653,#38654,#38655,#38656,#38657,#38658,#38659,#38660,#38661,#38662,
#38663),.UNSPECIFIED.,.F.,.F.,(4,3,3,3,3,3,3,3,3,3,3,3,3,3,3,3,3,3,3,3,
3,3,3,3,3,3,3,3,3,3,3,3,3,3,3,3,3,3,3,3,3,3,3,3,3,3,3,3,3,3,3,3,3,3,3,3,
3,3,3,3,3,3,3,3,3,3,3,3,3,3,3,3,3,3,3,4),(241.902634326415,242.036118860327,
242.068062381838,242.15180911454,242.235452791556,242.319013535622,242.402511397579,
242.485973898142,242.569419033634,242.652864868477,242.736329463715,242.819882649137,
242.903480482709,242.987212045571,243.067045884037,243.150792616739,243.234436293755,
243.317997037821,243.401494899778,243.48495740034,243.568402535833,243.651848370675,
243.735312965913,243.818866151335,243.902463984908,243.98619554777,244.066029386236,
244.149776118938,244.233419795954,244.31698054002,244.400478401977,244.483940902539,
244.567386038032,244.650831872874,244.734296468112,244.817849653534,244.901447487107,
244.985179049969,245.065012888435,245.148759621137,245.232403298153,245.315964042219,
245.399461904176,245.482924404739,245.566369540231,245.649815375074,245.733279970312,
245.816833155734,245.900430989307,245.984162552168,246.063996390634,246.147743123336,
246.231386800352,246.314947544418,246.398445406375,246.481907906938,246.56535304243,
246.648798877273,246.732263472511,246.815816657933,246.899414491506,246.983146054368,
247.062979892834,247.146726625536,247.230370302552,247.313931046619,247.397428908575,
247.480891409138,247.56433654463,247.647782379473,247.731246974711,247.814800160133,
247.898397993706,247.982129556568,248.061963395033,248.185819633595),
 .UNSPECIFIED.);
#378=B_SPLINE_CURVE_WITH_KNOTS('',3,(#38665,#38666,#38667,#38668,#38669,
#38670,#38671,#38672,#38673,#38674,#38675,#38676,#38677,#38678,#38679,#38680,
#38681,#38682,#38683,#38684,#38685,#38686,#38687,#38688,#38689,#38690,#38691,
#38692,#38693,#38694,#38695,#38696,#38697,#38698,#38699,#38700,#38701,#38702,
#38703,#38704,#38705,#38706,#38707,#38708,#38709,#38710,#38711,#38712,#38713,
#38714,#38715,#38716,#38717,#38718,#38719,#38720,#38721,#38722,#38723,#38724,
#38725,#38726,#38727,#38728,#38729,#38730,#38731,#38732,#38733,#38734,#38735,
#38736,#38737,#38738,#38739,#38740,#38741,#38742,#38743,#38744,#38745,#38746,
#38747,#38748,#38749,#38750,#38751,#38752,#38753,#38754,#38755,#38756,#38757,
#38758,#38759,#38760,#38761,#38762,#38763,#38764,#38765,#38766,#38767,#38768,
#38769,#38770,#38771,#38772,#38773,#38774,#38775,#38776,#38777,#38778,#38779,
#38780,#38781,#38782,#38783,#38784,#38785,#38786,#38787,#38788,#38789,#38790,
#38791,#38792,#38793,#38794,#38795,#38796,#38797,#38798,#38799,#38800,#38801,
#38802,#38803,#38804,#38805,#38806,#38807,#38808,#38809,#38810,#38811,#38812,
#38813,#38814,#38815,#38816,#38817,#38818,#38819,#38820,#38821,#38822,#38823,
#38824,#38825,#38826,#38827,#38828,#38829,#38830,#38831,#38832,#38833,#38834,
#38835,#38836,#38837,#38838,#38839,#38840,#38841,#38842,#38843,#38844,#38845,
#38846,#38847,#38848,#38849,#38850,#38851,#38852,#38853,#38854,#38855,#38856,
#38857,#38858,#38859,#38860,#38861,#38862,#38863,#38864,#38865,#38866,#38867,
#38868,#38869,#38870,#38871,#38872,#38873,#38874,#38875,#38876,#38877,#38878,
#38879,#38880,#38881,#38882,#38883,#38884,#38885,#38886,#38887,#38888,#38889,
#38890),.UNSPECIFIED.,.F.,.F.,(4,3,3,3,3,3,3,3,3,3,3,3,3,3,3,3,3,3,3,3,
3,3,3,3,3,3,3,3,3,3,3,3,3,3,3,3,3,3,3,3,3,3,3,3,3,3,3,3,3,3,3,3,3,3,3,3,
3,3,3,3,3,3,3,3,3,3,3,3,3,3,3,3,3,3,3,4),(235.619449019423,235.70867099603,
235.800043589183,235.889734382521,235.981947875582,236.074161368643,236.157908101345,
236.241551778361,236.325112522427,236.408610384384,236.492072884947,236.575518020439,
236.658963855282,236.74242845052,236.825981635942,236.909579469515,236.993311032377,
237.073144870842,237.156891603544,237.24053528056,237.324096024626,237.407593886583,
237.491056387145,237.574501522638,237.65794735748,237.741411952719,237.82496513814,
237.908562971713,237.992294534575,238.072128373041,238.155875105743,238.239518782759,
238.323079526825,238.406577388782,238.490039889344,238.573485024837,238.656930859679,
238.740395454917,238.823948640339,238.907546473912,238.991278036774,239.07111187524,
239.154858607942,239.238502284958,239.322063029024,239.405560890981,239.489023391544,
239.572468527036,239.655914361879,239.739378957117,239.822932142539,239.906529976112,
239.990261538974,240.070095377439,240.153842110141,240.237485787157,240.321046531223,
240.40454439318,240.488006893743,240.571452029235,240.654897864078,240.738362459316,
240.821915644738,240.90551347831,240.989245041172,241.069078879639,241.151576682586,
241.233971985748,241.317554778307,241.399805543854,241.482023949524,241.564229036275,
241.648830358762,241.731098704372,241.816866515298,241.902634326224),
 .UNSPECIFIED.);
#379=B_SPLINE_CURVE_WITH_KNOTS('',3,(#38892,#38893,#38894,#38895,#38896,
#38897,#38898,#38899,#38900,#38901,#38902,#38903,#38904,#38905,#38906,#38907,
#38908,#38909,#38910,#38911,#38912,#38913,#38914,#38915,#38916,#38917,#38918,
#38919,#38920,#38921,#38922,#38923,#38924,#38925,#38926,#38927,#38928,#38929,
#38930,#38931,#38932,#38933,#38934,#38935,#38936,#38937,#38938,#38939,#38940,
#38941,#38942,#38943,#38944,#38945,#38946,#38947,#38948,#38949,#38950,#38951,
#38952,#38953,#38954,#38955,#38956,#38957,#38958,#38959,#38960,#38961,#38962,
#38963,#38964,#38965,#38966,#38967,#38968,#38969,#38970,#38971,#38972,#38973,
#38974,#38975,#38976,#38977,#38978,#38979,#38980,#38981,#38982,#38983,#38984,
#38985,#38986,#38987,#38988,#38989,#38990,#38991,#38992,#38993,#38994,#38995,
#38996,#38997,#38998,#38999,#39000,#39001,#39002,#39003,#39004,#39005,#39006,
#39007,#39008,#39009,#39010,#39011,#39012,#39013,#39014,#39015,#39016,#39017,
#39018,#39019,#39020,#39021,#39022,#39023,#39024,#39025,#39026,#39027,#39028,
#39029,#39030,#39031,#39032,#39033,#39034,#39035,#39036,#39037,#39038,#39039,
#39040,#39041,#39042,#39043,#39044,#39045,#39046,#39047,#39048,#39049,#39050,
#39051,#39052,#39053,#39054,#39055,#39056,#39057,#39058,#39059,#39060,#39061,
#39062,#39063,#39064,#39065,#39066,#39067,#39068,#39069,#39070,#39071,#39072,
#39073,#39074,#39075,#39076,#39077,#39078,#39079,#39080,#39081,#39082,#39083,
#39084,#39085,#39086,#39087,#39088,#39089,#39090,#39091,#39092,#39093,#39094,
#39095,#39096,#39097,#39098,#39099,#39100,#39101,#39102,#39103,#39104,#39105,
#39106,#39107,#39108,#39109,#39110,#39111,#39112,#39113,#39114,#39115,#39116,
#39117,#39118,#39119,#39120),.UNSPECIFIED.,.F.,.F.,(4,3,3,3,3,3,3,3,3,3,
3,3,3,3,3,3,3,3,3,3,3,3,3,3,3,3,3,3,3,3,3,3,3,3,3,3,3,3,3,3,3,3,3,3,3,3,
3,3,3,3,3,3,3,3,3,3,3,3,3,3,3,3,3,3,3,3,3,3,3,3,3,3,3,3,3,3,4),(229.336263712056,
229.41886753326,229.501541636033,229.584074644522,229.66660240436,229.749143732478,
229.831922888221,229.914589512896,229.997424934172,230.080260355448,230.16400708815,
230.247650765166,230.331211509232,230.414709371189,230.498171871751,230.581617007243,
230.665062842086,230.748527437324,230.832080622746,230.915678456319,230.999410019181,
231.079243857647,231.162990590349,231.246634267365,231.330195011431,231.413692873388,
231.49715537395,231.580600509443,231.664046344285,231.747510939523,231.831064124945,
231.914661958518,231.99839352138,232.078227359846,232.161974092548,232.245617769564,
232.32917851363,232.412676375587,232.496138876149,232.579584011642,232.663029846485,
232.746494441723,232.830047627145,232.913645460718,232.99737702358,233.077210862045,
233.160957594747,233.244601271763,233.32816201583,233.411659877787,233.49512237835,
233.578567513842,233.662013348685,233.745477943923,233.829031129345,233.912628962918,
233.99636052578,234.076194364245,234.159941096947,234.243584773963,234.327145518029,
234.410643379986,234.494105880548,234.577551016041,234.660996850883,234.744461446121,
234.828014631543,234.911612465116,234.995344027978,235.075177866444,235.161656885001,
235.248006508427,235.334240268089,235.420341411725,235.506363821645,235.592303722112,
235.619449019236),.UNSPECIFIED.);
#380=B_SPLINE_CURVE_WITH_KNOTS('',3,(#39122,#39123,#39124,#39125,#39126,
#39127,#39128,#39129,#39130,#39131,#39132,#39133,#39134,#39135,#39136,#39137,
#39138,#39139,#39140,#39141,#39142,#39143,#39144,#39145,#39146,#39147,#39148,
#39149,#39150,#39151,#39152,#39153,#39154,#39155,#39156,#39157,#39158,#39159,
#39160,#39161,#39162,#39163,#39164,#39165,#39166,#39167,#39168,#39169,#39170,
#39171,#39172,#39173,#39174,#39175,#39176,#39177,#39178,#39179,#39180,#39181,
#39182,#39183,#39184,#39185,#39186,#39187,#39188,#39189,#39190,#39191,#39192,
#39193,#39194,#39195,#39196,#39197,#39198,#39199,#39200,#39201,#39202,#39203,
#39204,#39205,#39206,#39207,#39208,#39209,#39210,#39211,#39212,#39213,#39214,
#39215,#39216,#39217,#39218,#39219,#39220,#39221,#39222,#39223,#39224,#39225,
#39226,#39227,#39228,#39229,#39230,#39231,#39232,#39233,#39234,#39235,#39236,
#39237,#39238,#39239,#39240,#39241,#39242,#39243,#39244,#39245,#39246,#39247,
#39248,#39249,#39250,#39251,#39252,#39253,#39254,#39255,#39256,#39257,#39258,
#39259,#39260,#39261,#39262,#39263,#39264,#39265,#39266,#39267,#39268,#39269,
#39270,#39271,#39272,#39273,#39274,#39275,#39276,#39277,#39278,#39279,#39280,
#39281,#39282,#39283,#39284,#39285,#39286,#39287,#39288,#39289,#39290,#39291,
#39292,#39293,#39294,#39295,#39296,#39297,#39298,#39299,#39300,#39301,#39302,
#39303,#39304,#39305,#39306,#39307,#39308,#39309,#39310,#39311,#39312,#39313,
#39314,#39315,#39316,#39317,#39318,#39319,#39320,#39321,#39322,#39323,#39324,
#39325,#39326,#39327,#39328,#39329,#39330,#39331,#39332,#39333,#39334,#39335,
#39336,#39337,#39338,#39339,#39340,#39341,#39342,#39343,#39344,#39345,#39346,
#39347,#39348,#39349,#39350),.UNSPECIFIED.,.F.,.F.,(4,3,3,3,3,3,3,3,3,3,
3,3,3,3,3,3,3,3,3,3,3,3,3,3,3,3,3,3,3,3,3,3,3,3,3,3,3,3,3,3,3,3,3,3,3,3,
3,3,3,3,3,3,3,3,3,3,3,3,3,3,3,3,3,3,3,3,3,3,3,3,3,3,3,3,3,3,4),(223.053078404877,
223.087375840054,223.171122572756,223.254766249772,223.338326993838,223.421824855795,
223.505287356358,223.58873249185,223.672178326693,223.755642921931,223.839196107353,
223.922793940925,224.006525503787,224.086359342253,224.170106074955,224.253749751971,
224.337310496037,224.420808357994,224.504270858556,224.587715994049,224.671161828892,
224.75462642413,224.838179609551,224.921777443124,225.005509005986,225.085342844452,
225.169089577154,225.25273325417,225.336293998236,225.419791860193,225.503254360755,
225.586699496248,225.67014533109,225.753609926329,225.83716311175,225.920760945323,
226.004492508185,226.084326346651,226.168073079353,226.251716756369,226.335277500435,
226.418775362392,226.502237862955,226.585682998447,226.66912883329,226.752593428528,
226.836146613949,226.919744447522,227.003476010384,227.08330984885,227.167056581552,
227.250700258568,227.334261002635,227.417758864591,227.501221365154,227.584666500646,
227.668112335489,227.751576930728,227.835130116149,227.918727949722,228.002459512584,
228.08229335105,228.166040083752,228.249683760768,228.333244504835,228.416742366791,
228.500204867354,228.583650002846,228.667095837689,228.750560432927,228.834113618349,
228.917711451922,229.001443014784,229.081276853249,229.190064578712,229.296653912374,
229.336263711945),.UNSPECIFIED.);
#381=B_SPLINE_CURVE_WITH_KNOTS('',3,(#39352,#39353,#39354,#39355,#39356,
#39357,#39358,#39359,#39360,#39361,#39362,#39363,#39364,#39365,#39366,#39367,
#39368,#39369,#39370,#39371,#39372,#39373,#39374,#39375,#39376,#39377,#39378,
#39379,#39380,#39381,#39382,#39383,#39384,#39385,#39386,#39387,#39388,#39389,
#39390,#39391,#39392,#39393,#39394,#39395,#39396,#39397,#39398,#39399,#39400,
#39401,#39402,#39403,#39404,#39405,#39406,#39407,#39408,#39409,#39410,#39411,
#39412,#39413,#39414,#39415,#39416,#39417,#39418,#39419,#39420,#39421,#39422,
#39423,#39424,#39425,#39426,#39427,#39428,#39429,#39430,#39431,#39432,#39433,
#39434,#39435,#39436,#39437,#39438,#39439,#39440,#39441,#39442,#39443,#39444,
#39445,#39446,#39447,#39448,#39449,#39450,#39451,#39452,#39453,#39454,#39455,
#39456,#39457,#39458,#39459,#39460,#39461,#39462,#39463,#39464,#39465,#39466,
#39467,#39468,#39469,#39470,#39471,#39472,#39473,#39474,#39475,#39476,#39477,
#39478,#39479,#39480,#39481,#39482,#39483,#39484,#39485,#39486,#39487,#39488,
#39489,#39490,#39491,#39492,#39493,#39494,#39495,#39496,#39497,#39498,#39499,
#39500,#39501,#39502,#39503,#39504,#39505,#39506,#39507,#39508,#39509,#39510,
#39511,#39512,#39513,#39514,#39515,#39516,#39517,#39518,#39519,#39520,#39521,
#39522,#39523,#39524,#39525,#39526,#39527,#39528,#39529,#39530,#39531,#39532,
#39533,#39534,#39535,#39536,#39537,#39538,#39539,#39540,#39541,#39542,#39543,
#39544,#39545,#39546,#39547,#39548,#39549,#39550,#39551,#39552,#39553,#39554,
#39555,#39556,#39557,#39558,#39559,#39560,#39561,#39562,#39563,#39564,#39565,
#39566,#39567,#39568,#39569,#39570,#39571,#39572,#39573,#39574,#39575,#39576,
#39577,#39578,#39579,#39580),.UNSPECIFIED.,.F.,.F.,(4,3,3,3,3,3,3,3,3,3,
3,3,3,3,3,3,3,3,3,3,3,3,3,3,3,3,3,3,3,3,3,3,3,3,3,3,3,3,3,3,3,3,3,3,3,3,
3,3,3,3,3,3,3,3,3,3,3,3,3,3,3,3,3,3,3,3,3,3,3,3,3,3,3,3,3,3,4),(216.769893097874,
216.867988859855,216.966730771947,217.066196864284,217.093474826859,217.177221559561,
217.260865236577,217.344425980643,217.4279238426,217.511386343162,217.594831478654,
217.678277313497,217.761741908735,217.845295094157,217.928892927729,218.012624490591,
218.092458329058,218.17620506176,218.259848738776,218.343409482842,218.426907344799,
218.510369845361,218.593814980854,218.677260815696,218.760725410934,218.844278596356,
218.927876429929,219.011607992791,219.091441831257,219.175188563959,219.258832240975,
219.342392985041,219.425890846998,219.509353347561,219.592798483053,219.676244317896,
219.759708913134,219.843262098556,219.926859932128,220.01059149499,220.090425333456,
220.174172066158,220.257815743174,220.34137648724,220.424874349197,220.50833684976,
220.591781985252,220.675227820095,220.758692415333,220.842245600755,220.925843434327,
221.009574997189,221.089408835655,221.173155568357,221.256799245373,221.340359989439,
221.423857851396,221.507320351959,221.590765487451,221.674211322294,221.757675917532,
221.841229102954,221.924826936526,222.008558499388,222.088392337855,222.171674256109,
222.254853427668,222.337950444371,222.420985821213,222.503987612706,222.586973977605,
222.669963395455,222.7529743444,222.836072663398,222.919218957202,223.002488182695,
223.053078404729),.UNSPECIFIED.);
#382=B_SPLINE_CURVE_WITH_KNOTS('',3,(#39582,#39583,#39584,#39585,#39586,
#39587,#39588,#39589,#39590,#39591,#39592,#39593,#39594,#39595,#39596,#39597,
#39598,#39599,#39600,#39601,#39602,#39603,#39604,#39605,#39606,#39607,#39608,
#39609,#39610,#39611,#39612,#39613,#39614,#39615,#39616,#39617,#39618,#39619,
#39620,#39621,#39622,#39623,#39624,#39625,#39626,#39627,#39628,#39629,#39630,
#39631,#39632,#39633,#39634,#39635,#39636,#39637,#39638,#39639,#39640,#39641,
#39642,#39643,#39644,#39645,#39646,#39647,#39648,#39649,#39650,#39651,#39652,
#39653,#39654,#39655,#39656,#39657,#39658,#39659,#39660,#39661,#39662,#39663,
#39664,#39665,#39666,#39667,#39668,#39669,#39670,#39671,#39672,#39673,#39674,
#39675,#39676,#39677,#39678,#39679,#39680,#39681,#39682,#39683,#39684,#39685,
#39686,#39687,#39688,#39689,#39690,#39691,#39692,#39693,#39694,#39695,#39696,
#39697,#39698,#39699,#39700,#39701,#39702,#39703,#39704,#39705,#39706,#39707,
#39708,#39709,#39710,#39711,#39712,#39713,#39714,#39715,#39716,#39717,#39718,
#39719,#39720,#39721,#39722,#39723,#39724,#39725,#39726,#39727,#39728,#39729,
#39730,#39731,#39732,#39733,#39734,#39735,#39736,#39737,#39738,#39739,#39740,
#39741,#39742,#39743,#39744,#39745,#39746,#39747,#39748,#39749,#39750,#39751,
#39752,#39753,#39754,#39755,#39756,#39757,#39758,#39759,#39760,#39761,#39762,
#39763,#39764,#39765,#39766,#39767,#39768,#39769,#39770,#39771,#39772,#39773,
#39774,#39775,#39776,#39777,#39778,#39779,#39780,#39781,#39782,#39783,#39784,
#39785,#39786,#39787,#39788,#39789,#39790,#39791,#39792,#39793,#39794,#39795,
#39796,#39797,#39798,#39799,#39800,#39801,#39802,#39803,#39804,#39805,#39806,
#39807,#39808,#39809,#39810),.UNSPECIFIED.,.F.,.F.,(4,3,3,3,3,3,3,3,3,3,
3,3,3,3,3,3,3,3,3,3,3,3,3,3,3,3,3,3,3,3,3,3,3,3,3,3,3,3,3,3,3,3,3,3,3,3,
3,3,3,3,3,3,3,3,3,3,3,3,3,3,3,3,3,3,3,3,3,3,3,3,3,3,3,3,3,3,4),(210.486707790518,
210.570999537664,210.655305176302,210.739641535065,210.824025459423,210.908524456367,
210.993091242317,211.077790090279,211.099573813664,211.183320546366,211.266964223382,
211.350524967448,211.434022829405,211.517485329967,211.60093046546,211.684376300303,
211.767840895541,211.851394080962,211.934991914535,212.018723477397,212.098557315863,
212.182304048565,212.265947725581,212.349508469647,212.433006331604,212.516468832166,
212.599913967659,212.683359802502,212.76682439774,212.850377583162,212.933975416734,
213.017706979596,213.097540818062,213.181287550764,213.26493122778,213.348491971846,
213.431989833803,213.515452334366,213.598897469858,213.682343304701,213.765807899939,
213.849361085361,213.932958918933,214.016690481795,214.096524320261,214.180271052963,
214.263914729979,214.347475474046,214.430973336002,214.514435836565,214.597880972057,
214.6813268069,214.764791402138,214.84834458756,214.931942421133,215.015673983995,
215.09550782246,215.179254555162,215.262898232178,215.346458976244,215.4299568382,
215.513419338763,215.596864474255,215.680310309098,215.763774904336,215.847328089758,
215.930925923331,216.014657486193,216.09449132466,216.17891654629,216.262367135454,
216.345736920481,216.42904420361,216.514256427132,216.597501403593,216.683697250645,
216.769893097697),.UNSPECIFIED.);
#383=B_SPLINE_CURVE_WITH_KNOTS('',3,(#39812,#39813,#39814,#39815,#39816,
#39817,#39818,#39819,#39820,#39821,#39822,#39823,#39824,#39825,#39826,#39827,
#39828,#39829,#39830,#39831,#39832,#39833,#39834,#39835,#39836,#39837,#39838,
#39839,#39840,#39841,#39842,#39843,#39844,#39845,#39846,#39847,#39848,#39849,
#39850,#39851,#39852,#39853,#39854,#39855,#39856,#39857,#39858,#39859,#39860,
#39861,#39862,#39863,#39864,#39865,#39866,#39867,#39868,#39869,#39870,#39871,
#39872,#39873,#39874,#39875,#39876,#39877,#39878,#39879,#39880,#39881,#39882,
#39883,#39884,#39885,#39886,#39887,#39888,#39889,#39890,#39891,#39892,#39893,
#39894,#39895,#39896,#39897,#39898,#39899,#39900,#39901,#39902,#39903,#39904,
#39905,#39906,#39907,#39908,#39909,#39910,#39911,#39912,#39913,#39914,#39915,
#39916,#39917,#39918,#39919,#39920,#39921,#39922,#39923,#39924,#39925,#39926,
#39927,#39928,#39929,#39930,#39931,#39932,#39933,#39934,#39935,#39936,#39937,
#39938,#39939,#39940,#39941,#39942,#39943,#39944,#39945,#39946,#39947,#39948,
#39949,#39950,#39951,#39952,#39953,#39954,#39955,#39956,#39957,#39958,#39959,
#39960,#39961,#39962,#39963,#39964,#39965,#39966,#39967,#39968,#39969,#39970,
#39971,#39972,#39973,#39974,#39975,#39976,#39977,#39978,#39979,#39980,#39981,
#39982,#39983,#39984,#39985,#39986,#39987,#39988,#39989,#39990,#39991,#39992,
#39993,#39994,#39995,#39996,#39997,#39998,#39999,#40000,#40001,#40002,#40003,
#40004,#40005,#40006,#40007,#40008,#40009,#40010,#40011,#40012,#40013,#40014,
#40015,#40016,#40017,#40018,#40019,#40020,#40021,#40022,#40023,#40024,#40025,
#40026,#40027,#40028,#40029,#40030,#40031,#40032,#40033,#40034,#40035,#40036,
#40037,#40038,#40039,#40040),.UNSPECIFIED.,.F.,.F.,(4,3,3,3,3,3,3,3,3,3,
3,3,3,3,3,3,3,3,3,3,3,3,3,3,3,3,3,3,3,3,3,3,3,3,3,3,3,3,3,3,3,3,3,3,3,3,
3,3,3,3,3,3,3,3,3,3,3,3,3,3,3,3,3,3,3,3,3,3,3,3,3,3,3,3,3,3,4),(204.203522483473,
204.286193926472,204.368772304277,204.451278642249,204.533738282922,204.616173967715,
204.698604592558,204.781049046846,204.863576513138,204.946145767727,205.028845394083,
205.105672800469,205.189419533171,205.273063210187,205.356623954253,205.44012181621,
205.523584316772,205.607029452265,205.690475287107,205.773939882346,205.857493067767,
205.94109090134,206.024822464202,206.104656302668,206.18840303537,206.272046712386,
206.355607456452,206.439105318408,206.522567818971,206.606012954463,206.689458789306,
206.772923384544,206.856476569966,206.940074403538,207.0238059664,207.103639804867,
207.187386537569,207.271030214585,207.354590958651,207.438088820608,207.521551321171,
207.604996456663,207.688442291506,207.771906886744,207.855460072166,207.939057905738,
208.0227894686,208.102623307066,208.186370039768,208.270013716784,208.353574460851,
208.437072322808,208.52053482337,208.603979958862,208.687425793705,208.770890388943,
208.854443574365,208.938041407938,209.0217729708,209.101606809265,209.185353541967,
209.268997218983,209.35255796305,209.436055825006,209.519518325569,209.602963461062,
209.686409295904,209.769873891143,209.853427076564,209.937024910137,210.020756472999,
210.100590311465,210.197119681181,210.29081274856,210.388760269444,210.481685600267,
210.486707790327),.UNSPECIFIED.);
#384=B_SPLINE_CURVE_WITH_KNOTS('',3,(#40042,#40043,#40044,#40045,#40046,
#40047,#40048,#40049,#40050,#40051,#40052,#40053,#40054,#40055,#40056,#40057,
#40058,#40059,#40060,#40061,#40062,#40063,#40064,#40065,#40066,#40067,#40068,
#40069,#40070,#40071,#40072,#40073,#40074,#40075,#40076,#40077,#40078,#40079,
#40080,#40081,#40082,#40083,#40084,#40085,#40086,#40087,#40088,#40089,#40090,
#40091,#40092,#40093,#40094,#40095,#40096,#40097,#40098,#40099,#40100,#40101,
#40102,#40103,#40104,#40105,#40106,#40107,#40108,#40109,#40110,#40111,#40112,
#40113,#40114,#40115,#40116,#40117,#40118,#40119,#40120,#40121,#40122,#40123,
#40124,#40125,#40126,#40127,#40128,#40129,#40130,#40131,#40132,#40133,#40134,
#40135,#40136,#40137,#40138,#40139,#40140,#40141,#40142,#40143,#40144,#40145,
#40146,#40147,#40148,#40149,#40150,#40151,#40152,#40153,#40154,#40155,#40156,
#40157,#40158,#40159,#40160,#40161,#40162,#40163,#40164,#40165,#40166,#40167,
#40168,#40169,#40170,#40171,#40172,#40173,#40174,#40175,#40176,#40177,#40178,
#40179,#40180,#40181,#40182,#40183,#40184,#40185,#40186,#40187,#40188,#40189,
#40190,#40191,#40192,#40193,#40194,#40195,#40196,#40197,#40198,#40199,#40200,
#40201,#40202,#40203,#40204,#40205,#40206,#40207,#40208,#40209,#40210,#40211,
#40212,#40213,#40214,#40215,#40216,#40217,#40218,#40219,#40220,#40221,#40222,
#40223,#40224,#40225,#40226,#40227,#40228,#40229,#40230,#40231,#40232,#40233,
#40234,#40235,#40236,#40237,#40238,#40239,#40240,#40241,#40242,#40243,#40244,
#40245,#40246,#40247,#40248,#40249,#40250,#40251,#40252,#40253,#40254,#40255,
#40256,#40257,#40258,#40259,#40260,#40261,#40262,#40263,#40264,#40265,#40266,
#40267),.UNSPECIFIED.,.F.,.F.,(4,3,3,3,3,3,3,3,3,3,3,3,3,3,3,3,3,3,3,3,
3,3,3,3,3,3,3,3,3,3,3,3,3,3,3,3,3,3,3,3,3,3,3,3,3,3,3,3,3,3,3,3,3,3,3,3,
3,3,3,3,3,3,3,3,3,3,3,3,3,3,3,3,3,3,3,4),(197.920337176159,198.042804749541,
198.112788285075,198.196535017777,198.280178694793,198.363739438859,198.447237300816,
198.530699801378,198.614144936871,198.697590771713,198.781055366951,198.864608552373,
198.948206385946,199.031937948808,199.111771787274,199.195518519976,199.279162196992,
199.362722941058,199.446220803015,199.529683303578,199.61312843907,199.696574273913,
199.780038869151,199.863592054573,199.947189888145,200.030921451007,200.110755289473,
200.194502022175,200.278145699191,200.361706443257,200.445204305214,200.528666805777,
200.612111941269,200.695557776112,200.77902237135,200.862575556772,200.946173390344,
201.029904953206,201.109738791672,201.193485524374,201.27712920139,201.360689945456,
201.444187807413,201.527650307975,201.611095443468,201.694541278311,201.778005873549,
201.86155905897,201.945156892543,202.028888455405,202.108722293871,202.192469026573,
202.276112703589,202.359673447655,202.443171309612,202.526633810175,202.610078945667,
202.69352478051,202.776989375748,202.86054256117,202.944140394743,203.027871957605,
203.10770579607,203.191452528772,203.275096205788,203.358656949854,203.442154811811,
203.525617312373,203.609062447865,203.692508282708,203.775972877946,203.859526063368,
203.94312389694,204.026855459802,204.10668929827,204.203522483338),
 .UNSPECIFIED.);
#385=B_SPLINE_CURVE_WITH_KNOTS('',3,(#40269,#40270,#40271,#40272,#40273,
#40274,#40275,#40276,#40277,#40278,#40279,#40280,#40281,#40282,#40283,#40284,
#40285,#40286,#40287,#40288,#40289,#40290,#40291,#40292,#40293,#40294,#40295,
#40296,#40297,#40298,#40299,#40300,#40301,#40302,#40303,#40304,#40305,#40306,
#40307,#40308,#40309,#40310,#40311,#40312,#40313,#40314,#40315,#40316,#40317,
#40318,#40319,#40320,#40321,#40322,#40323,#40324,#40325,#40326,#40327,#40328,
#40329,#40330,#40331,#40332,#40333,#40334,#40335,#40336,#40337,#40338,#40339,
#40340,#40341,#40342,#40343,#40344,#40345,#40346,#40347,#40348,#40349,#40350,
#40351,#40352,#40353,#40354,#40355,#40356,#40357,#40358,#40359,#40360,#40361,
#40362,#40363,#40364,#40365,#40366,#40367,#40368,#40369,#40370,#40371,#40372,
#40373,#40374,#40375,#40376,#40377,#40378,#40379,#40380,#40381,#40382,#40383,
#40384,#40385,#40386,#40387,#40388,#40389,#40390,#40391,#40392,#40393,#40394,
#40395,#40396,#40397,#40398,#40399,#40400,#40401,#40402,#40403,#40404,#40405,
#40406,#40407,#40408,#40409,#40410,#40411,#40412,#40413,#40414,#40415,#40416,
#40417,#40418,#40419,#40420,#40421,#40422,#40423,#40424,#40425,#40426,#40427,
#40428,#40429,#40430,#40431,#40432,#40433,#40434,#40435,#40436,#40437,#40438,
#40439,#40440,#40441,#40442,#40443,#40444,#40445,#40446,#40447,#40448,#40449,
#40450,#40451,#40452,#40453,#40454,#40455,#40456,#40457,#40458,#40459,#40460,
#40461,#40462,#40463,#40464,#40465,#40466,#40467,#40468,#40469,#40470,#40471,
#40472,#40473,#40474,#40475,#40476,#40477,#40478,#40479,#40480,#40481,#40482,
#40483,#40484,#40485,#40486,#40487,#40488,#40489,#40490,#40491,#40492,#40493,
#40494,#40495,#40496,#40497),.UNSPECIFIED.,.F.,.F.,(4,3,3,3,3,3,3,3,3,3,
3,3,3,3,3,3,3,3,3,3,3,3,3,3,3,3,3,3,3,3,3,3,3,3,3,3,3,3,3,3,3,3,3,3,3,3,
3,3,3,3,3,3,3,3,3,3,3,3,3,3,3,3,3,3,3,3,3,3,3,3,3,3,3,3,3,3,4),(191.637151869127,
191.72523147956,191.813451550297,191.901902961679,191.9904796452,192.079262046608,
192.11888727188,192.202634004582,192.286277681598,192.369838425664,192.453336287621,
192.536798788184,192.620243923676,192.703689758519,192.787154353757,192.870707539179,
192.954305372751,193.038036935613,193.117870774079,193.201617506781,193.285261183797,
193.368821927863,193.45231978982,193.535782290382,193.619227425875,193.702673260717,
193.786137855955,193.869691041377,193.95328887495,194.037020437812,194.116854276278,
194.20060100898,194.284244685996,194.367805430062,194.451303292019,194.534765792582,
194.618210928074,194.701656762917,194.785121358155,194.868674543577,194.952272377149,
195.036003940011,195.115837778477,195.199584511179,195.283228188195,195.366788932261,
195.450286794218,195.53374929478,195.617194430272,195.700640265115,195.784104860353,
195.867658045775,195.951255879348,196.034987442209,196.114821280676,196.198568013378,
196.282211690394,196.36577243446,196.449270296417,196.53273279698,196.616177932472,
196.699623767315,196.783088362553,196.866641547975,196.950239381547,197.033970944409,
197.113804782875,197.196328092342,197.278748420473,197.361075187093,197.443349557154,
197.525590589424,197.607817311615,197.690081386651,197.772363362024,197.854731017392,
197.920337176039),.UNSPECIFIED.);
#386=B_SPLINE_CURVE_WITH_KNOTS('',3,(#40499,#40500,#40501,#40502,#40503,
#40504,#40505,#40506,#40507,#40508,#40509,#40510,#40511,#40512,#40513,#40514,
#40515,#40516,#40517,#40518,#40519,#40520,#40521,#40522,#40523,#40524,#40525,
#40526,#40527,#40528,#40529,#40530,#40531,#40532,#40533,#40534,#40535,#40536,
#40537,#40538,#40539,#40540,#40541,#40542,#40543,#40544,#40545,#40546,#40547,
#40548,#40549,#40550,#40551,#40552,#40553,#40554,#40555,#40556,#40557,#40558,
#40559,#40560,#40561,#40562,#40563,#40564,#40565,#40566,#40567,#40568,#40569,
#40570,#40571,#40572,#40573,#40574,#40575,#40576,#40577,#40578,#40579,#40580,
#40581,#40582,#40583,#40584,#40585,#40586,#40587,#40588,#40589,#40590,#40591,
#40592,#40593,#40594,#40595,#40596,#40597,#40598,#40599,#40600,#40601,#40602,
#40603,#40604,#40605,#40606,#40607,#40608,#40609,#40610,#40611,#40612,#40613,
#40614,#40615,#40616,#40617,#40618,#40619,#40620,#40621,#40622,#40623,#40624,
#40625,#40626,#40627,#40628,#40629,#40630,#40631,#40632,#40633,#40634,#40635,
#40636,#40637,#40638,#40639,#40640,#40641,#40642,#40643,#40644,#40645,#40646,
#40647,#40648,#40649,#40650,#40651,#40652,#40653,#40654,#40655,#40656,#40657,
#40658,#40659,#40660,#40661,#40662,#40663,#40664,#40665,#40666,#40667,#40668,
#40669,#40670,#40671,#40672,#40673,#40674,#40675,#40676,#40677,#40678,#40679,
#40680,#40681,#40682,#40683,#40684,#40685,#40686,#40687,#40688,#40689,#40690,
#40691,#40692,#40693,#40694,#40695,#40696,#40697,#40698,#40699,#40700,#40701,
#40702,#40703,#40704,#40705,#40706,#40707,#40708,#40709,#40710,#40711,#40712,
#40713,#40714,#40715,#40716,#40717,#40718,#40719,#40720,#40721,#40722,#40723,
#40724,#40725,#40726,#40727),.UNSPECIFIED.,.F.,.F.,(4,3,3,3,3,3,3,3,3,3,
3,3,3,3,3,3,3,3,3,3,3,3,3,3,3,3,3,3,3,3,3,3,3,3,3,3,3,3,3,3,3,3,3,3,3,3,
3,3,3,3,3,3,3,3,3,3,3,3,3,3,3,3,3,3,3,3,3,3,3,3,3,3,3,3,3,3,4),(185.353966561907,
185.436430980761,185.522500390501,185.604872317226,185.687231798795,185.769597769302,
185.851989165541,185.934469289462,186.017001705857,186.099650436777,186.124986258685,
186.208732991387,186.292376668403,186.375937412469,186.459435274426,186.542897774989,
186.626342910481,186.709788745324,186.793253340562,186.876806525984,186.960404359557,
187.044135922419,187.123969760884,187.207716493586,187.291360170601,187.374920914668,
187.458418776624,187.541881277187,187.625326412679,187.708772247522,187.79223684276,
187.875790028182,187.959387861754,188.043119424616,188.122953263083,188.206699995785,
188.290343672801,188.373904416867,188.457402278824,188.540864779386,188.624309914879,
188.707755749722,188.79122034496,188.874773530382,188.958371363954,189.042102926816,
189.121936765282,189.205683497984,189.289327175,189.372887919066,189.456385781023,
189.539848281586,189.623293417078,189.706739251921,189.790203847159,189.873757032581,
189.957354866153,190.041086429015,190.120920267481,190.204667000183,190.288310677198,
190.371871421265,190.455369283222,190.538831783784,190.622276919276,190.70572275412,
190.789187349358,190.87274053478,190.956338368352,191.040069931214,191.11990376968,
191.207292110406,191.294538799997,191.381603868696,191.468562696466,191.555387492085,
191.637151868979),.UNSPECIFIED.);
#387=B_SPLINE_CURVE_WITH_KNOTS('',3,(#40729,#40730,#40731,#40732,#40733,
#40734,#40735,#40736,#40737,#40738,#40739,#40740,#40741,#40742,#40743,#40744,
#40745,#40746,#40747,#40748,#40749,#40750,#40751,#40752,#40753,#40754,#40755,
#40756,#40757,#40758,#40759,#40760,#40761,#40762,#40763,#40764,#40765,#40766,
#40767,#40768,#40769,#40770,#40771,#40772,#40773,#40774,#40775,#40776,#40777,
#40778,#40779,#40780,#40781,#40782,#40783,#40784,#40785,#40786,#40787,#40788,
#40789,#40790,#40791,#40792,#40793,#40794,#40795,#40796,#40797,#40798,#40799,
#40800,#40801,#40802,#40803,#40804,#40805,#40806,#40807,#40808,#40809,#40810,
#40811,#40812,#40813,#40814,#40815,#40816,#40817,#40818,#40819,#40820,#40821,
#40822,#40823,#40824,#40825,#40826,#40827,#40828,#40829,#40830,#40831,#40832,
#40833,#40834,#40835,#40836,#40837,#40838,#40839,#40840,#40841,#40842,#40843,
#40844,#40845,#40846,#40847,#40848,#40849,#40850,#40851,#40852,#40853,#40854,
#40855,#40856,#40857,#40858,#40859,#40860,#40861,#40862,#40863,#40864,#40865,
#40866,#40867,#40868,#40869,#40870,#40871,#40872,#40873,#40874,#40875,#40876,
#40877,#40878,#40879,#40880,#40881,#40882,#40883,#40884,#40885,#40886,#40887,
#40888,#40889,#40890,#40891,#40892,#40893,#40894,#40895,#40896,#40897,#40898,
#40899,#40900,#40901,#40902,#40903,#40904,#40905,#40906,#40907,#40908,#40909,
#40910,#40911,#40912,#40913,#40914,#40915,#40916,#40917,#40918,#40919,#40920,
#40921,#40922,#40923,#40924,#40925,#40926,#40927,#40928,#40929,#40930,#40931,
#40932,#40933,#40934,#40935,#40936,#40937,#40938,#40939,#40940,#40941,#40942,
#40943,#40944,#40945,#40946,#40947,#40948,#40949,#40950,#40951,#40952,#40953,
#40954),.UNSPECIFIED.,.F.,.F.,(4,3,3,3,3,3,3,3,3,3,3,3,3,3,3,3,3,3,3,3,
3,3,3,3,3,3,3,3,3,3,3,3,3,3,3,3,3,3,3,3,3,3,3,3,3,3,3,3,3,3,3,3,3,3,3,3,
3,3,3,3,3,3,3,3,3,3,3,3,3,3,3,3,3,3,3,4),(179.07078125462,179.13210174329,
179.215848475992,179.299492153008,179.383052897074,179.466550759031,179.550013259594,
179.633458395086,179.716904229929,179.800368825167,179.883922010589,179.967519844162,
180.051251407024,180.13108524549,180.214831978192,180.298475655208,180.382036399274,
180.465534261231,180.548996761794,180.632441897286,180.715887732129,180.799352327367,
180.882905512789,180.966503346362,181.050234909224,181.130068747689,181.213815480391,
181.297459157407,181.381019901473,181.46451776343,181.547980263992,181.631425399484,
181.714871234327,181.798335829565,181.881889014987,181.96548684856,182.049218411421,
182.129052249888,182.21279898259,182.296442659606,182.380003403672,182.463501265629,
182.546963766192,182.630408901684,182.713854736527,182.797319331765,182.880872517187,
182.964470350759,183.048201913621,183.128035752087,183.211782484789,183.295426161805,
183.378986905871,183.462484767828,183.545947268391,183.629392403883,183.712838238726,
183.796302833964,183.879856019385,183.963453852958,184.04718541582,184.127019254286,
184.210765986988,184.294409664004,184.37797040807,184.461468270027,184.544930770589,
184.628375906081,184.711821740924,184.795286336162,184.878839521584,184.962437355157,
185.046168918018,185.126002756485,185.239984659142,185.353966561799),
 .UNSPECIFIED.);
#388=B_SPLINE_CURVE_WITH_KNOTS('',3,(#40956,#40957,#40958,#40959,#40960,
#40961,#40962,#40963,#40964,#40965,#40966,#40967,#40968,#40969,#40970,#40971,
#40972,#40973,#40974,#40975,#40976,#40977,#40978,#40979,#40980,#40981,#40982,
#40983,#40984,#40985,#40986,#40987,#40988,#40989,#40990,#40991,#40992,#40993,
#40994,#40995,#40996,#40997,#40998,#40999,#41000,#41001,#41002,#41003,#41004,
#41005,#41006,#41007,#41008,#41009,#41010,#41011,#41012,#41013,#41014,#41015,
#41016,#41017,#41018,#41019,#41020,#41021,#41022,#41023,#41024,#41025,#41026,
#41027,#41028,#41029,#41030,#41031,#41032,#41033,#41034,#41035,#41036,#41037,
#41038,#41039,#41040,#41041,#41042,#41043,#41044,#41045,#41046,#41047,#41048,
#41049,#41050,#41051,#41052,#41053,#41054,#41055,#41056,#41057,#41058,#41059,
#41060,#41061,#41062,#41063,#41064,#41065,#41066,#41067,#41068,#41069,#41070,
#41071,#41072,#41073,#41074,#41075,#41076,#41077,#41078,#41079,#41080,#41081,
#41082,#41083,#41084,#41085,#41086,#41087,#41088,#41089,#41090,#41091,#41092,
#41093,#41094,#41095,#41096,#41097,#41098,#41099,#41100,#41101,#41102,#41103,
#41104,#41105,#41106,#41107,#41108,#41109,#41110,#41111,#41112,#41113,#41114,
#41115,#41116,#41117,#41118,#41119,#41120,#41121,#41122,#41123,#41124,#41125,
#41126,#41127,#41128,#41129,#41130,#41131,#41132,#41133,#41134,#41135,#41136,
#41137,#41138,#41139,#41140,#41141,#41142,#41143,#41144,#41145,#41146,#41147,
#41148,#41149,#41150,#41151,#41152,#41153,#41154,#41155,#41156,#41157,#41158,
#41159,#41160,#41161,#41162,#41163,#41164,#41165,#41166,#41167,#41168,#41169,
#41170,#41171,#41172,#41173,#41174,#41175,#41176,#41177,#41178,#41179,#41180,
#41181,#41182,#41183,#41184),.UNSPECIFIED.,.F.,.F.,(4,3,3,3,3,3,3,3,3,3,
3,3,3,3,3,3,3,3,3,3,3,3,3,3,3,3,3,3,3,3,3,3,3,3,3,3,3,3,3,3,3,3,3,3,3,3,
3,3,3,3,3,3,3,3,3,3,3,3,3,3,3,3,3,3,3,3,3,3,3,3,3,3,3,3,3,3,4),(172.787595947634,
172.883336957541,172.979547986538,173.076358533046,173.138200730095,173.221947462797,
173.305591139813,173.389151883879,173.472649745836,173.556112246399,173.639557381891,
173.723003216734,173.806467811972,173.890020997394,173.973618830966,174.057350393828,
174.137184232295,174.220930964997,174.304574642013,174.388135386079,174.471633248036,
174.555095748599,174.638540884091,174.721986718934,174.805451314172,174.889004499594,
174.972602333167,175.056333896029,175.136167734494,175.219914467196,175.303558144212,
175.387118888278,175.470616750235,175.554079250797,175.637524386289,175.720970221132,
175.80443481637,175.887988001792,175.971585835364,176.055317398226,176.135151236693,
176.218897969395,176.302541646411,176.386102390477,176.469600252434,176.553062752997,
176.636507888489,176.719953723332,176.80341831857,176.886971503992,176.970569337564,
177.054300900426,177.134134738892,177.217881471594,177.30152514861,177.385085892676,
177.468583754633,177.552046255196,177.635491390688,177.718937225531,177.802401820769,
177.885955006191,177.969552839763,178.053284402625,178.133118241091,178.216112772867,
178.299004813803,178.381815209239,178.467935964897,178.550651613485,178.633353651688,
178.716060779604,178.79879169783,178.881607801925,178.964474423694,179.047453126179,
179.070781254507),.UNSPECIFIED.);
#389=B_SPLINE_CURVE_WITH_KNOTS('',3,(#41186,#41187,#41188,#41189,#41190,
#41191,#41192,#41193,#41194,#41195,#41196,#41197,#41198,#41199,#41200,#41201,
#41202,#41203,#41204,#41205,#41206,#41207,#41208,#41209,#41210,#41211,#41212,
#41213,#41214,#41215,#41216,#41217,#41218,#41219,#41220,#41221,#41222,#41223,
#41224,#41225,#41226,#41227,#41228,#41229,#41230,#41231,#41232,#41233,#41234,
#41235,#41236,#41237,#41238,#41239,#41240,#41241,#41242,#41243,#41244,#41245,
#41246,#41247,#41248,#41249,#41250,#41251,#41252,#41253,#41254,#41255,#41256,
#41257,#41258,#41259,#41260,#41261,#41262,#41263,#41264,#41265,#41266,#41267,
#41268,#41269,#41270,#41271,#41272,#41273,#41274,#41275,#41276,#41277,#41278,
#41279,#41280,#41281,#41282,#41283,#41284,#41285,#41286,#41287,#41288,#41289,
#41290,#41291,#41292,#41293,#41294,#41295,#41296,#41297,#41298,#41299,#41300,
#41301,#41302,#41303,#41304,#41305,#41306,#41307,#41308,#41309,#41310,#41311,
#41312,#41313,#41314,#41315,#41316,#41317,#41318,#41319,#41320,#41321,#41322,
#41323,#41324,#41325,#41326,#41327,#41328,#41329,#41330,#41331,#41332,#41333,
#41334,#41335,#41336,#41337,#41338,#41339,#41340,#41341,#41342,#41343,#41344,
#41345,#41346,#41347,#41348,#41349,#41350,#41351,#41352,#41353,#41354,#41355,
#41356,#41357,#41358,#41359,#41360,#41361,#41362,#41363,#41364,#41365,#41366,
#41367,#41368,#41369,#41370,#41371,#41372,#41373,#41374,#41375,#41376,#41377,
#41378,#41379,#41380,#41381,#41382,#41383,#41384,#41385,#41386,#41387,#41388,
#41389,#41390,#41391,#41392,#41393,#41394,#41395,#41396,#41397,#41398,#41399,
#41400,#41401,#41402,#41403,#41404,#41405,#41406,#41407,#41408,#41409,#41410,
#41411,#41412,#41413,#41414),.UNSPECIFIED.,.F.,.F.,(4,3,3,3,3,3,3,3,3,3,
3,3,3,3,3,3,3,3,3,3,3,3,3,3,3,3,3,3,3,3,3,3,3,3,3,3,3,3,3,3,3,3,3,3,3,3,
3,3,3,3,3,3,3,3,3,3,3,3,3,3,3,3,3,3,3,3,3,3,3,3,3,3,3,3,3,3,4),(166.504410640261,
166.588207254555,166.672002919908,166.755815193113,166.839661637873,166.923612475455,
167.007620588218,167.091764594634,167.1442997169,167.228046449602,167.311690126618,
167.395250870684,167.478748732641,167.562211233204,167.645656368696,167.729102203539,
167.812566798777,167.896119984199,167.979717817772,168.063449380634,168.1432832191,
168.227029951802,168.310673628818,168.394234372884,168.477732234841,168.561194735404,
168.644639870896,168.728085705739,168.811550300977,168.895103486399,168.978701319971,
169.062432882833,169.142266721299,169.226013454001,169.309657131016,169.393217875083,
169.47671573704,169.560178237602,169.643623373095,169.727069207937,169.810533803176,
169.894086988598,169.97768482217,170.061416385032,170.141250223498,170.2249969562,
170.308640633216,170.392201377282,170.475699239238,170.559161739801,170.642606875293,
170.726052710136,170.809517305374,170.893070490796,170.976668324368,171.06039988723,
171.140233725697,171.223980458399,171.307624135415,171.391184879481,171.474682741438,
171.558145242,171.641590377492,171.725036212335,171.808500807573,171.892053992995,
171.975651826568,172.05938338943,172.139217227896,172.223198945279,172.307077676614,
172.390871343758,172.474597806455,172.558275915806,172.641924630996,172.725578355938,
172.78759594744),.UNSPECIFIED.);
#390=B_SPLINE_CURVE_WITH_KNOTS('',3,(#41416,#41417,#41418,#41419,#41420,
#41421,#41422,#41423,#41424,#41425,#41426,#41427,#41428,#41429,#41430,#41431,
#41432,#41433,#41434,#41435,#41436,#41437,#41438,#41439,#41440,#41441,#41442,
#41443,#41444,#41445,#41446,#41447,#41448,#41449,#41450,#41451,#41452,#41453,
#41454,#41455,#41456,#41457,#41458,#41459,#41460,#41461,#41462,#41463,#41464,
#41465,#41466,#41467,#41468,#41469,#41470,#41471,#41472,#41473,#41474,#41475,
#41476,#41477,#41478,#41479,#41480,#41481,#41482,#41483,#41484,#41485,#41486,
#41487,#41488,#41489,#41490,#41491,#41492,#41493,#41494,#41495,#41496,#41497,
#41498,#41499,#41500,#41501,#41502,#41503,#41504,#41505,#41506,#41507,#41508,
#41509,#41510,#41511,#41512,#41513,#41514,#41515,#41516,#41517,#41518,#41519,
#41520,#41521,#41522,#41523,#41524,#41525,#41526,#41527,#41528,#41529,#41530,
#41531,#41532,#41533,#41534,#41535,#41536,#41537,#41538,#41539,#41540,#41541,
#41542,#41543,#41544,#41545,#41546,#41547,#41548,#41549,#41550,#41551,#41552,
#41553,#41554,#41555,#41556,#41557,#41558,#41559,#41560,#41561,#41562,#41563,
#41564,#41565,#41566,#41567,#41568,#41569,#41570,#41571,#41572,#41573,#41574,
#41575,#41576,#41577,#41578,#41579,#41580,#41581,#41582,#41583,#41584,#41585,
#41586,#41587,#41588,#41589,#41590,#41591,#41592,#41593,#41594,#41595,#41596,
#41597,#41598,#41599,#41600,#41601,#41602,#41603,#41604,#41605,#41606,#41607,
#41608,#41609,#41610,#41611,#41612,#41613,#41614,#41615,#41616,#41617,#41618,
#41619,#41620,#41621,#41622,#41623,#41624,#41625,#41626,#41627,#41628,#41629,
#41630,#41631,#41632,#41633,#41634,#41635,#41636,#41637,#41638,#41639,#41640,
#41641,#41642,#41643,#41644),.UNSPECIFIED.,.F.,.F.,(4,3,3,3,3,3,3,3,3,3,
3,3,3,3,3,3,3,3,3,3,3,3,3,3,3,3,3,3,3,3,3,3,3,3,3,3,3,3,3,3,3,3,3,3,3,3,
3,3,3,3,3,3,3,3,3,3,3,3,3,3,3,3,3,3,3,3,3,3,3,3,3,3,3,3,3,3,4),(160.221225333203,
160.304117287473,160.386911848399,160.469629902408,160.554726002571,160.637362369371,
160.719989807647,160.802627071407,160.889569979481,160.972329090611,161.055143868158,
161.138072213799,161.150398703705,161.234145436407,161.317789113423,161.401349857489,
161.484847719446,161.568310220008,161.6517553555,161.735201190343,161.818665785581,
161.902218971003,161.985816804576,162.069548367437,162.149382205905,162.233128938607,
162.316772615623,162.400333359689,162.483831221646,162.567293722209,162.650738857701,
162.734184692544,162.817649287782,162.901202473204,162.984800306776,163.068531869638,
163.148365708104,163.232112440806,163.315756117821,163.399316861888,163.482814723845,
163.566277224407,163.6497223599,163.733168194743,163.816632789981,163.900185975403,
163.983783808975,164.067515371837,164.147349210303,164.231095943005,164.314739620021,
164.398300364087,164.481798226044,164.565260726606,164.648705862099,164.732151696941,
164.815616292179,164.899169477601,164.982767311174,165.066498874036,165.146332712502,
165.230079445204,165.31372312222,165.397283866286,165.480781728243,165.564244228806,
165.647689364298,165.731135199141,165.81459979438,165.898152979801,165.981750813374,
166.065482376236,166.145316214701,166.24136187852,166.337061354585,166.432099443715,
166.504410640063),.UNSPECIFIED.);
#391=B_SPLINE_CURVE_WITH_KNOTS('',3,(#41646,#41647,#41648,#41649,#41650,
#41651,#41652,#41653,#41654,#41655,#41656,#41657,#41658,#41659,#41660,#41661,
#41662,#41663,#41664,#41665,#41666,#41667,#41668,#41669,#41670,#41671,#41672,
#41673,#41674,#41675,#41676,#41677,#41678,#41679,#41680,#41681,#41682,#41683,
#41684,#41685,#41686,#41687,#41688,#41689,#41690,#41691,#41692,#41693,#41694,
#41695,#41696,#41697,#41698,#41699,#41700,#41701,#41702,#41703,#41704,#41705,
#41706,#41707,#41708,#41709,#41710,#41711,#41712,#41713,#41714,#41715,#41716,
#41717,#41718,#41719,#41720,#41721,#41722,#41723,#41724,#41725,#41726,#41727,
#41728,#41729,#41730,#41731,#41732,#41733,#41734,#41735,#41736,#41737,#41738,
#41739,#41740,#41741,#41742,#41743,#41744,#41745,#41746,#41747,#41748,#41749,
#41750,#41751,#41752,#41753,#41754,#41755,#41756,#41757,#41758,#41759,#41760,
#41761,#41762,#41763,#41764,#41765,#41766,#41767,#41768,#41769,#41770,#41771,
#41772,#41773,#41774,#41775,#41776,#41777,#41778,#41779,#41780,#41781,#41782,
#41783,#41784,#41785,#41786,#41787,#41788,#41789,#41790,#41791,#41792,#41793,
#41794,#41795,#41796,#41797,#41798,#41799,#41800,#41801,#41802,#41803,#41804,
#41805,#41806,#41807,#41808,#41809,#41810,#41811,#41812,#41813,#41814,#41815,
#41816,#41817,#41818,#41819,#41820,#41821,#41822,#41823,#41824,#41825,#41826,
#41827,#41828,#41829,#41830,#41831,#41832,#41833,#41834,#41835,#41836,#41837,
#41838,#41839,#41840,#41841,#41842,#41843,#41844,#41845,#41846,#41847,#41848,
#41849,#41850,#41851,#41852,#41853,#41854,#41855,#41856,#41857,#41858,#41859,
#41860,#41861,#41862,#41863,#41864,#41865,#41866,#41867,#41868,#41869,#41870,
#41871),.UNSPECIFIED.,.F.,.F.,(4,3,3,3,3,3,3,3,3,3,3,3,3,3,3,3,3,3,3,3,
3,3,3,3,3,3,3,3,3,3,3,3,3,3,3,3,3,3,3,3,3,3,3,3,3,3,3,3,3,3,3,3,3,3,3,3,
3,3,3,3,3,3,3,3,3,3,3,3,3,3,3,3,3,3,3,4),(153.938040025902,154.052832737468,
154.157514188311,154.241260921013,154.324904598029,154.408465342096,154.491963204053,
154.575425704616,154.658870840108,154.742316674951,154.82578127019,154.909334455612,
154.992932289184,155.076663852047,155.15649769051,155.240244423212,155.323888100228,
155.407448844294,155.490946706251,155.574409206814,155.657854342306,155.741300177149,
155.824764772387,155.908317957809,155.991915791382,156.075647354244,156.15548119271,
156.239227925412,156.322871602428,156.406432346494,156.489930208451,156.573392709014,
156.656837844506,156.740283679349,156.823748274587,156.907301460009,156.990899293581,
157.074630856443,157.154464694909,157.238211427611,157.321855104627,157.405415848693,
157.48891371065,157.572376211213,157.655821346705,157.739267181548,157.822731776786,
157.906284962208,157.98988279578,158.073614358642,158.153448197108,158.23719492981,
158.320838606826,158.404399350892,158.487897212849,158.571359713412,158.654804848904,
158.738250683747,158.821715278985,158.905268464407,158.988866297979,159.072597860841,
159.152431699307,159.236178432009,159.319822109024,159.403382853091,159.486880715047,
159.57034321561,159.653788351102,159.737234185945,159.820698781183,159.904251966605,
159.987849800177,160.071581363039,160.151415201506,160.221225333081),
 .UNSPECIFIED.);
#392=B_SPLINE_CURVE_WITH_KNOTS('',3,(#41873,#41874,#41875,#41876,#41877,
#41878,#41879,#41880,#41881,#41882,#41883,#41884,#41885,#41886,#41887,#41888,
#41889,#41890,#41891,#41892,#41893,#41894,#41895,#41896,#41897,#41898,#41899,
#41900,#41901,#41902,#41903,#41904,#41905,#41906,#41907,#41908,#41909,#41910,
#41911,#41912,#41913,#41914,#41915,#41916,#41917,#41918,#41919,#41920,#41921,
#41922,#41923,#41924,#41925,#41926,#41927,#41928,#41929,#41930,#41931,#41932,
#41933,#41934,#41935,#41936,#41937,#41938,#41939,#41940,#41941,#41942,#41943,
#41944,#41945,#41946,#41947,#41948,#41949,#41950,#41951,#41952,#41953,#41954,
#41955,#41956,#41957,#41958,#41959,#41960,#41961,#41962,#41963,#41964,#41965,
#41966,#41967,#41968,#41969,#41970,#41971,#41972,#41973,#41974,#41975,#41976,
#41977,#41978,#41979,#41980,#41981,#41982,#41983,#41984,#41985,#41986,#41987,
#41988,#41989,#41990,#41991,#41992,#41993,#41994,#41995,#41996,#41997,#41998,
#41999,#42000,#42001,#42002,#42003,#42004,#42005,#42006,#42007,#42008,#42009,
#42010,#42011,#42012,#42013,#42014,#42015,#42016,#42017,#42018,#42019,#42020,
#42021,#42022,#42023,#42024,#42025,#42026,#42027,#42028,#42029,#42030,#42031,
#42032,#42033,#42034,#42035,#42036,#42037,#42038,#42039,#42040,#42041,#42042,
#42043,#42044,#42045,#42046,#42047,#42048,#42049,#42050,#42051,#42052,#42053,
#42054,#42055,#42056,#42057,#42058,#42059,#42060,#42061,#42062,#42063,#42064,
#42065,#42066,#42067,#42068,#42069,#42070,#42071,#42072,#42073,#42074,#42075,
#42076,#42077,#42078,#42079,#42080,#42081,#42082,#42083,#42084,#42085,#42086,
#42087,#42088,#42089,#42090,#42091,#42092,#42093,#42094,#42095,#42096,#42097,
#42098,#42099,#42100,#42101),.UNSPECIFIED.,.F.,.F.,(4,3,3,3,3,3,3,3,3,3,
3,3,3,3,3,3,3,3,3,3,3,3,3,3,3,3,3,3,3,3,3,3,3,3,3,3,3,3,3,3,3,3,3,3,3,3,
3,3,3,3,3,3,3,3,3,3,3,3,3,3,3,3,3,3,3,3,3,3,3,3,3,3,3,3,3,3,4),(147.654854718722,
147.741934294221,147.829116802213,147.916493787936,148.003971880025,148.091648447011,
148.163613175116,148.247359907818,148.331003584834,148.414564328901,148.498062190857,
148.58152469142,148.664969826912,148.748415661755,148.831880256993,148.915433442415,
148.999031275988,149.08276283885,149.162596677315,149.246343410017,149.329987087033,
149.413547831099,149.497045693056,149.580508193619,149.663953329111,149.747399163954,
149.830863759193,149.914416944614,149.998014778187,150.081746341049,150.161580179515,
150.245326912217,150.328970589233,150.412531333299,150.496029195256,150.579491695819,
150.662936831311,150.746382666154,150.829847261392,150.913400446814,150.996998280387,
151.080729843248,151.160563681714,151.244310414416,151.327954091431,151.411514835498,
151.495012697454,151.578475198017,151.661920333509,151.745366168352,151.82883076359,
151.912383949012,151.995981782585,152.079713345447,152.159547183913,152.243293916615,
152.326937593631,152.410498337697,152.493996199654,152.577458700216,152.660903835709,
152.744349670551,152.82781426579,152.911367451212,152.994965284784,153.078696847646,
153.158530686112,153.241143602457,153.323652758631,153.406066476268,153.488426755207,
153.570752601881,153.653062991075,153.735403927003,153.817761944655,153.900190984863,
153.938040025744),.UNSPECIFIED.);
#393=B_SPLINE_CURVE_WITH_KNOTS('',3,(#42103,#42104,#42105,#42106,#42107,
#42108,#42109,#42110,#42111,#42112,#42113,#42114,#42115,#42116,#42117,#42118,
#42119,#42120,#42121,#42122,#42123,#42124,#42125,#42126,#42127,#42128,#42129,
#42130,#42131,#42132,#42133,#42134,#42135,#42136,#42137,#42138,#42139,#42140,
#42141,#42142,#42143,#42144,#42145,#42146,#42147,#42148,#42149,#42150,#42151,
#42152,#42153,#42154,#42155,#42156,#42157,#42158,#42159,#42160,#42161,#42162,
#42163,#42164,#42165,#42166,#42167,#42168,#42169,#42170,#42171,#42172,#42173,
#42174,#42175,#42176,#42177,#42178,#42179,#42180,#42181,#42182,#42183,#42184,
#42185,#42186,#42187,#42188,#42189,#42190,#42191,#42192,#42193,#42194,#42195,
#42196,#42197,#42198,#42199,#42200,#42201,#42202,#42203,#42204,#42205,#42206,
#42207,#42208,#42209,#42210,#42211,#42212,#42213,#42214,#42215,#42216,#42217,
#42218,#42219,#42220,#42221,#42222,#42223,#42224,#42225,#42226,#42227,#42228,
#42229,#42230,#42231,#42232,#42233,#42234,#42235,#42236,#42237,#42238,#42239,
#42240,#42241,#42242,#42243,#42244,#42245,#42246,#42247,#42248,#42249,#42250,
#42251,#42252,#42253,#42254,#42255,#42256,#42257,#42258,#42259,#42260,#42261,
#42262,#42263,#42264,#42265,#42266,#42267,#42268,#42269,#42270,#42271,#42272,
#42273,#42274,#42275,#42276,#42277,#42278,#42279,#42280,#42281,#42282,#42283,
#42284,#42285,#42286,#42287,#42288,#42289,#42290,#42291,#42292,#42293,#42294,
#42295,#42296,#42297,#42298,#42299,#42300,#42301,#42302,#42303,#42304,#42305,
#42306,#42307,#42308,#42309,#42310,#42311,#42312,#42313,#42314,#42315,#42316,
#42317,#42318,#42319,#42320,#42321,#42322,#42323,#42324,#42325,#42326,#42327,
#42328,#42329,#42330,#42331),.UNSPECIFIED.,.F.,.F.,(4,3,3,3,3,3,3,3,3,3,
3,3,3,3,3,3,3,3,3,3,3,3,3,3,3,3,3,3,3,3,3,3,3,3,3,3,3,3,3,3,3,3,3,3,3,3,
3,3,3,3,3,3,3,3,3,3,3,3,3,3,3,3,3,3,3,3,3,3,3,3,3,3,3,3,3,3,4),(141.37166951201,
141.454058249237,141.536378431309,141.618656662166,141.700914289754,141.783170319096,
141.865443751679,141.947801446069,142.03020435425,142.112731423433,142.169712161921,
142.253458894623,142.337102571639,142.420663315705,142.504161177662,142.587623678225,
142.671068813717,142.75451464856,142.837979243798,142.92153242922,143.005130262793,
143.088861825655,143.16869566412,143.252442396822,143.336086073838,143.419646817905,
143.503144679862,143.586607180424,143.670052315917,143.75349815076,143.836962745998,
143.92051593142,144.004113764992,144.087845327854,144.16767916632,144.251425899022,
144.335069576038,144.418630320104,144.502128182061,144.585590682624,144.669035818116,
144.752481652958,144.835946248197,144.919499433619,145.003097267191,145.086828830053,
145.166662668519,145.250409401221,145.334053078237,145.417613822303,145.50111168426,
145.584574184822,145.668019320314,145.751465155157,145.834929750395,145.918482935817,
146.002080769389,146.085812332251,146.165646170718,146.24939290342,146.333036580436,
146.416597324503,146.50009518646,146.583557687022,146.667002822515,146.750448657358,
146.833913252596,146.917466438018,147.00106427159,147.084795834452,147.164629672917,
147.253060978591,147.341334586321,147.429396673395,147.517331621313,147.605097658525,
147.654854718538),.UNSPECIFIED.);
#394=B_SPLINE_CURVE_WITH_KNOTS('',3,(#42333,#42334,#42335,#42336,#42337,
#42338,#42339,#42340,#42341,#42342,#42343),.UNSPECIFIED.,.F.,.F.,(4,1,1,
1,1,1,1,1,4),(135.088484104363,135.176827646527,136.175811148726,137.174794650925,
138.173778153125,139.172761655324,140.171745157523,141.170728659722,141.371669411542),
 .UNSPECIFIED.);
#395=B_SPLINE_CURVE_WITH_KNOTS('',3,(#42345,#42346,#42347,#42348,#42349,
#42350,#42351,#42352,#42353,#42354,#42355,#42356,#42357,#42358,#42359,#42360,
#42361,#42362,#42363,#42364,#42365,#42366,#42367,#42368,#42369,#42370,#42371,
#42372,#42373,#42374,#42375,#42376,#42377,#42378,#42379,#42380,#42381,#42382,
#42383,#42384,#42385,#42386,#42387,#42388,#42389,#42390,#42391,#42392,#42393,
#42394,#42395,#42396,#42397,#42398,#42399,#42400,#42401,#42402,#42403,#42404,
#42405,#42406,#42407,#42408,#42409,#42410,#42411,#42412,#42413,#42414,#42415,
#42416,#42417,#42418,#42419,#42420,#42421,#42422,#42423,#42424,#42425,#42426,
#42427,#42428,#42429,#42430,#42431,#42432,#42433,#42434,#42435,#42436,#42437,
#42438,#42439,#42440,#42441,#42442,#42443,#42444,#42445,#42446,#42447,#42448,
#42449,#42450,#42451,#42452,#42453,#42454,#42455,#42456,#42457,#42458,#42459,
#42460,#42461,#42462,#42463,#42464,#42465,#42466,#42467,#42468,#42469,#42470,
#42471,#42472,#42473,#42474,#42475,#42476,#42477,#42478,#42479,#42480,#42481,
#42482,#42483,#42484,#42485,#42486,#42487,#42488,#42489,#42490,#42491,#42492,
#42493,#42494,#42495,#42496,#42497,#42498,#42499,#42500,#42501,#42502,#42503,
#42504,#42505,#42506,#42507,#42508,#42509,#42510,#42511,#42512,#42513,#42514,
#42515,#42516,#42517,#42518,#42519,#42520,#42521,#42522,#42523,#42524,#42525,
#42526,#42527,#42528,#42529,#42530,#42531,#42532,#42533,#42534,#42535,#42536,
#42537,#42538,#42539,#42540,#42541,#42542,#42543,#42544,#42545,#42546,#42547,
#42548,#42549,#42550,#42551,#42552,#42553,#42554,#42555,#42556,#42557,#42558,
#42559,#42560,#42561,#42562,#42563,#42564,#42565,#42566,#42567,#42568,#42569,
#42570),.UNSPECIFIED.,.F.,.F.,(4,3,3,3,3,3,3,3,3,3,3,3,3,3,3,3,3,3,3,3,
3,3,3,3,3,3,3,3,3,3,3,3,3,3,3,3,3,3,3,3,3,3,3,3,3,3,3,3,3,3,3,3,3,3,3,3,
3,3,3,3,3,3,3,3,3,3,3,3,3,3,3,3,3,3,3,4),(128.805298797375,128.899705756365,
128.993788658939,129.088376322271,129.182926633332,129.266673366034,129.350317043049,
129.433877787116,129.517375649072,129.600838149635,129.684283285127,129.76772911997,
129.851193715207,129.934746900629,130.018344734202,130.102076297063,130.181910135531,
130.265656868233,130.349300545249,130.432861289315,130.516359151272,130.599821651835,
130.683266787327,130.76671262217,130.850177217408,130.93373040283,131.017328236403,
131.101059799265,131.18089363773,131.264640370432,131.348284047448,131.431844791514,
131.515342653471,131.598805154033,131.682250289526,131.765696124368,131.849160719606,
131.932713905028,132.016311738601,132.100043301463,132.17987713993,132.263623872632,
132.347267549648,132.430828293715,132.514326155671,132.597788656234,132.681233791727,
132.764679626569,132.848144221808,132.93169740723,133.015295240802,133.099026803664,
133.178860642129,133.262607374831,133.346251051847,133.429811795913,133.51330965787,
133.596772158432,133.680217293925,133.763663128767,133.847127724005,133.930680909427,
134.014278743,134.098010305862,134.177844144328,134.26061799334,134.343289547075,
134.425879829208,134.508705328763,134.591202397923,134.67368585154,134.756174542847,
134.839251863547,134.921846228862,135.005165027255,135.088483825647),
 .UNSPECIFIED.);
#396=B_SPLINE_CURVE_WITH_KNOTS('',3,(#42572,#42573,#42574,#42575,#42576,
#42577,#42578,#42579,#42580,#42581,#42582,#42583,#42584,#42585,#42586,#42587,
#42588,#42589,#42590,#42591,#42592,#42593,#42594,#42595,#42596,#42597,#42598,
#42599,#42600,#42601,#42602,#42603,#42604,#42605,#42606,#42607,#42608,#42609,
#42610,#42611,#42612,#42613,#42614,#42615,#42616,#42617,#42618,#42619,#42620,
#42621,#42622,#42623,#42624,#42625,#42626,#42627,#42628,#42629,#42630,#42631,
#42632,#42633,#42634,#42635,#42636,#42637,#42638,#42639,#42640,#42641,#42642,
#42643,#42644,#42645,#42646,#42647,#42648,#42649,#42650,#42651,#42652,#42653,
#42654,#42655,#42656,#42657,#42658,#42659,#42660,#42661,#42662,#42663,#42664,
#42665,#42666,#42667,#42668,#42669,#42670,#42671,#42672,#42673,#42674,#42675,
#42676,#42677,#42678,#42679,#42680,#42681,#42682,#42683,#42684,#42685,#42686,
#42687,#42688,#42689,#42690,#42691,#42692,#42693,#42694,#42695,#42696,#42697,
#42698,#42699,#42700,#42701,#42702,#42703,#42704,#42705,#42706,#42707,#42708,
#42709,#42710,#42711,#42712,#42713,#42714,#42715,#42716,#42717,#42718,#42719,
#42720,#42721,#42722,#42723,#42724,#42725,#42726,#42727,#42728,#42729,#42730,
#42731,#42732,#42733,#42734,#42735,#42736,#42737,#42738,#42739,#42740,#42741,
#42742,#42743,#42744,#42745,#42746,#42747,#42748,#42749,#42750,#42751,#42752,
#42753,#42754,#42755,#42756,#42757,#42758,#42759,#42760,#42761,#42762,#42763,
#42764,#42765,#42766,#42767,#42768,#42769,#42770,#42771,#42772,#42773,#42774,
#42775,#42776,#42777,#42778,#42779,#42780,#42781,#42782,#42783,#42784,#42785,
#42786,#42787,#42788,#42789,#42790,#42791,#42792,#42793,#42794,#42795,#42796,
#42797,#42798,#42799,#42800),.UNSPECIFIED.,.F.,.F.,(4,3,3,3,3,3,3,3,3,3,
3,3,3,3,3,3,3,3,3,3,3,3,3,3,3,3,3,3,3,3,3,3,3,3,3,3,3,3,3,3,3,3,3,3,3,3,
3,3,3,3,3,3,3,3,3,3,3,3,3,3,3,3,3,3,3,3,3,3,3,3,3,3,3,3,3,3,4),(122.522113490004,
122.605495334217,122.688863359942,122.772235636009,122.855630230272,122.93911972146,
123.022656907832,123.106334733695,123.189025620137,123.272772352839,123.356416029855,
123.439976773921,123.523474635878,123.606937136441,123.690382271933,123.773828106776,
123.857292702013,123.940845887435,124.024443721008,124.10817528387,124.188009122336,
124.271755855038,124.355399532054,124.43896027612,124.522458138077,124.60592063864,
124.689365774132,124.772811608975,124.856276204213,124.939829389635,125.023427223208,
125.10715878607,125.186992624535,125.270739357237,125.354383034253,125.437943778319,
125.521441640276,125.604904140838,125.688349276331,125.771795111174,125.855259706412,
125.938812891834,126.022410725406,126.106142288268,126.185976126735,126.269722859437,
126.353366536453,126.436927280519,126.520425142477,126.603887643039,126.687332778532,
126.770778613374,126.854243208613,126.937796394035,127.021394227608,127.10512579047,
127.184959628934,127.268706361636,127.352350038652,127.435910782718,127.519408644675,
127.602871145237,127.68631628073,127.769762115572,127.85322671081,127.936779896232,
128.020377729805,128.104109292666,128.183943131133,128.268438217603,128.352825675139,
128.437122797182,128.521346811719,128.605510027022,128.689637939473,128.773753455852,
128.805298797183),.UNSPECIFIED.);
#397=B_SPLINE_CURVE_WITH_KNOTS('',3,(#42802,#42803,#42804,#42805,#42806,
#42807,#42808,#42809,#42810,#42811,#42812,#42813,#42814,#42815,#42816,#42817,
#42818,#42819,#42820,#42821,#42822,#42823,#42824,#42825,#42826,#42827,#42828,
#42829,#42830,#42831,#42832,#42833,#42834,#42835,#42836,#42837,#42838,#42839,
#42840,#42841,#42842,#42843,#42844,#42845,#42846,#42847,#42848,#42849,#42850,
#42851,#42852,#42853,#42854,#42855,#42856,#42857,#42858,#42859,#42860,#42861,
#42862,#42863,#42864,#42865,#42866,#42867,#42868,#42869,#42870,#42871,#42872,
#42873,#42874,#42875,#42876,#42877,#42878,#42879,#42880,#42881,#42882,#42883,
#42884,#42885,#42886,#42887,#42888,#42889,#42890,#42891,#42892,#42893,#42894,
#42895,#42896,#42897,#42898,#42899,#42900,#42901,#42902,#42903,#42904,#42905,
#42906,#42907,#42908,#42909,#42910,#42911,#42912,#42913,#42914,#42915,#42916,
#42917,#42918,#42919,#42920,#42921,#42922,#42923,#42924,#42925,#42926,#42927,
#42928,#42929,#42930,#42931,#42932,#42933,#42934,#42935,#42936,#42937,#42938,
#42939,#42940,#42941,#42942,#42943,#42944,#42945,#42946,#42947,#42948,#42949,
#42950,#42951,#42952,#42953,#42954,#42955,#42956,#42957,#42958,#42959,#42960,
#42961,#42962,#42963,#42964,#42965,#42966,#42967,#42968,#42969,#42970,#42971,
#42972,#42973,#42974,#42975,#42976,#42977,#42978,#42979,#42980,#42981,#42982,
#42983,#42984,#42985,#42986,#42987,#42988,#42989,#42990,#42991,#42992,#42993,
#42994,#42995,#42996,#42997,#42998,#42999,#43000,#43001,#43002,#43003,#43004,
#43005,#43006,#43007,#43008,#43009,#43010,#43011,#43012,#43013,#43014,#43015,
#43016,#43017,#43018,#43019,#43020,#43021,#43022,#43023,#43024,#43025,#43026,
#43027,#43028,#43029,#43030),.UNSPECIFIED.,.F.,.F.,(4,3,3,3,3,3,3,3,3,3,
3,3,3,3,3,3,3,3,3,3,3,3,3,3,3,3,3,3,3,3,3,3,3,3,3,3,3,3,3,3,3,3,3,3,3,3,
3,3,3,3,3,3,3,3,3,3,3,3,3,3,3,3,3,3,3,3,3,3,3,3,3,3,3,3,3,3,4),(116.238928183001,
116.322101803165,116.405174762509,116.488167733349,116.57110131169,116.654004557597,
116.736894597209,116.819789987459,116.902709285658,116.985718066432,117.068777060043,
117.151958344376,117.195124606942,117.278871339644,117.36251501666,117.446075760727,
117.529573622683,117.613036123246,117.696481258738,117.779927093581,117.863391688819,
117.946944874241,118.030542707814,118.114274270676,118.194108109141,118.277854841843,
118.361498518859,118.445059262926,118.528557124882,118.612019625445,118.695464760937,
118.77891059578,118.862375191018,118.94592837644,119.029526210013,119.113257772875,
119.193091611341,119.276838344043,119.360482021059,119.444042765125,119.527540627082,
119.611003127645,119.694448263137,119.77789409798,119.861358693218,119.94491187864,
120.028509712213,120.112241275075,120.19207511354,120.275821846242,120.359465523258,
120.443026267324,120.526524129281,120.609986629844,120.693431765336,120.776877600179,
120.860342195416,120.943895380838,121.027493214411,121.111224777272,121.191058615739,
121.274805348441,121.358449025457,121.442009769523,121.52550763148,121.608970132042,
121.692415267535,121.775861102378,121.859325697616,121.942878883038,122.026476716611,
122.110208279473,122.190042117938,122.288536143836,122.386570282577,122.483756133139,
122.522113489818),.UNSPECIFIED.);
#398=B_SPLINE_CURVE_WITH_KNOTS('',3,(#43032,#43033,#43034,#43035,#43036,
#43037,#43038,#43039,#43040,#43041,#43042,#43043,#43044,#43045,#43046,#43047,
#43048,#43049,#43050,#43051,#43052,#43053,#43054,#43055,#43056,#43057,#43058,
#43059,#43060,#43061,#43062,#43063,#43064,#43065,#43066,#43067,#43068,#43069,
#43070,#43071,#43072,#43073,#43074,#43075,#43076,#43077,#43078,#43079,#43080,
#43081,#43082,#43083,#43084,#43085,#43086,#43087,#43088,#43089,#43090,#43091,
#43092,#43093,#43094,#43095,#43096,#43097,#43098,#43099,#43100,#43101,#43102,
#43103,#43104,#43105,#43106,#43107,#43108,#43109,#43110,#43111,#43112,#43113,
#43114,#43115,#43116,#43117,#43118,#43119,#43120,#43121,#43122,#43123,#43124,
#43125,#43126,#43127,#43128,#43129,#43130,#43131,#43132,#43133,#43134,#43135,
#43136,#43137,#43138,#43139,#43140,#43141,#43142,#43143,#43144,#43145,#43146,
#43147,#43148,#43149,#43150,#43151,#43152,#43153,#43154,#43155,#43156,#43157,
#43158,#43159,#43160,#43161,#43162,#43163,#43164,#43165,#43166,#43167,#43168,
#43169,#43170,#43171,#43172,#43173,#43174,#43175,#43176,#43177,#43178,#43179,
#43180,#43181,#43182,#43183,#43184,#43185,#43186,#43187,#43188,#43189,#43190,
#43191,#43192,#43193,#43194,#43195,#43196,#43197,#43198,#43199,#43200,#43201,
#43202,#43203,#43204,#43205,#43206,#43207,#43208,#43209,#43210,#43211,#43212,
#43213,#43214,#43215,#43216,#43217,#43218,#43219,#43220,#43221,#43222,#43223,
#43224,#43225,#43226,#43227,#43228,#43229,#43230,#43231,#43232,#43233,#43234,
#43235,#43236,#43237,#43238,#43239,#43240,#43241,#43242,#43243,#43244,#43245,
#43246,#43247,#43248,#43249,#43250,#43251,#43252,#43253,#43254,#43255,#43256,
#43257,#43258,#43259,#43260),.UNSPECIFIED.,.F.,.F.,(4,3,3,3,3,3,3,3,3,3,
3,3,3,3,3,3,3,3,3,3,3,3,3,3,3,3,3,3,3,3,3,3,3,3,3,3,3,3,3,3,3,3,3,3,3,3,
3,3,3,3,3,3,3,3,3,3,3,3,3,3,3,3,3,3,3,3,3,3,3,3,3,3,3,3,3,3,4),(109.955742875786,
110.063488503129,110.17374886387,110.202240091548,110.28598682425,110.369630501266,
110.453191245332,110.536689107289,110.620151607852,110.703596743344,110.787042578187,
110.870507173425,110.954060358847,111.03765819242,111.121389755281,111.201223593747,
111.284970326449,111.368614003465,111.452174747531,111.535672609488,111.619135110051,
111.702580245543,111.786026080386,111.869490675624,111.953043861046,112.036641694618,
112.12037325748,112.200207095946,112.283953828648,112.367597505664,112.451158249731,
112.534656111687,112.61811861225,112.701563747742,112.785009582585,112.868474177823,
112.952027363245,113.035625196818,113.11935675968,113.199190598146,113.282937330848,
113.366581007864,113.45014175193,113.533639613887,113.61710211445,113.700547249942,
113.783993084785,113.867457680023,113.951010865445,114.034608699017,114.118340261879,
114.198174100345,114.281920833047,114.365564510063,114.449125254129,114.532623116086,
114.616085616648,114.699530752141,114.782976586983,114.866441182221,114.949994367643,
115.033592201216,115.117323764077,115.197157602544,115.280904335246,115.364548012262,
115.448108756328,115.531606618285,115.615069118848,115.69851425434,115.781960089183,
115.865424684421,115.948977869843,116.032575703416,116.116307266278,116.196141104743,
116.238928182824),.UNSPECIFIED.);
#399=B_SPLINE_CURVE_WITH_KNOTS('',3,(#43262,#43263,#43264,#43265,#43266,
#43267,#43268,#43269,#43270,#43271,#43272,#43273,#43274,#43275,#43276,#43277,
#43278,#43279,#43280,#43281,#43282,#43283,#43284,#43285,#43286,#43287,#43288,
#43289,#43290,#43291,#43292,#43293,#43294,#43295,#43296,#43297,#43298,#43299,
#43300,#43301,#43302,#43303,#43304,#43305,#43306,#43307,#43308,#43309,#43310,
#43311,#43312,#43313,#43314,#43315,#43316,#43317,#43318,#43319,#43320,#43321,
#43322,#43323,#43324,#43325,#43326,#43327,#43328,#43329,#43330,#43331,#43332,
#43333,#43334,#43335,#43336,#43337,#43338,#43339,#43340,#43341,#43342,#43343,
#43344,#43345,#43346,#43347,#43348,#43349,#43350,#43351,#43352,#43353,#43354,
#43355,#43356,#43357,#43358,#43359,#43360,#43361,#43362,#43363,#43364,#43365,
#43366,#43367,#43368,#43369,#43370,#43371,#43372,#43373,#43374,#43375,#43376,
#43377,#43378,#43379,#43380,#43381,#43382,#43383,#43384,#43385,#43386,#43387,
#43388,#43389,#43390,#43391,#43392,#43393,#43394,#43395,#43396,#43397,#43398,
#43399,#43400,#43401,#43402,#43403,#43404,#43405,#43406,#43407,#43408,#43409,
#43410,#43411,#43412,#43413,#43414,#43415,#43416,#43417,#43418,#43419,#43420,
#43421,#43422,#43423,#43424,#43425,#43426,#43427,#43428,#43429,#43430,#43431,
#43432,#43433,#43434,#43435,#43436,#43437,#43438,#43439,#43440,#43441,#43442,
#43443,#43444,#43445,#43446,#43447,#43448,#43449,#43450,#43451,#43452,#43453,
#43454,#43455,#43456,#43457,#43458,#43459,#43460,#43461,#43462,#43463,#43464,
#43465,#43466,#43467,#43468,#43469,#43470,#43471,#43472,#43473,#43474,#43475,
#43476,#43477,#43478,#43479,#43480,#43481,#43482,#43483,#43484,#43485,#43486,
#43487,#43488,#43489,#43490),.UNSPECIFIED.,.F.,.F.,(4,3,3,3,3,3,3,3,3,3,
3,3,3,3,3,3,3,3,3,3,3,3,3,3,3,3,3,3,3,3,3,3,3,3,3,3,3,3,3,3,3,3,3,3,3,3,
3,3,3,3,3,3,3,3,3,3,3,3,3,3,3,3,3,3,3,3,3,3,3,3,3,3,3,3,3,3,4),(103.672557568465,
103.758762666372,103.845040757771,103.935865337916,104.022392995456,104.109013779931,
104.195789661329,104.208339078353,104.292085811055,104.375729488071,104.459290232137,
104.542788094094,104.626250594656,104.709695730149,104.793141564991,104.876606160229,
104.960159345651,105.043757179224,105.127488742085,105.207322580552,105.291069313254,
105.37471299027,105.458273734336,105.541771596293,105.625234096856,105.708679232348,
105.792125067191,105.875589662429,105.959142847851,106.042740681423,106.126472244285,
106.206306082751,106.290052815453,106.373696492469,106.457257236535,106.540755098492,
106.624217599055,106.707662734547,106.79110856939,106.874573164628,106.95812635005,
107.041724183623,107.125455746485,107.205289584951,107.289036317653,107.372679994669,
107.456240738735,107.539738600692,107.623201101255,107.706646236747,107.79009207159,
107.873556666828,107.95710985225,108.040707685822,108.124439248684,108.20427308715,
108.288019819852,108.371663496868,108.455224240934,108.538722102891,108.622184603453,
108.705629738945,108.789075573788,108.872540169026,108.956093354448,109.03969118802,
109.123422750882,109.203256589349,109.286024516412,109.369739311316,109.452303664454,
109.534813329928,109.617287215932,109.70190113086,109.784381810341,109.870062342993,
109.955742875645),.UNSPECIFIED.);
#400=B_SPLINE_CURVE_WITH_KNOTS('',3,(#43492,#43493,#43494,#43495,#43496,
#43497,#43498,#43499,#43500,#43501,#43502,#43503,#43504,#43505,#43506,#43507,
#43508,#43509,#43510,#43511,#43512,#43513,#43514,#43515,#43516,#43517,#43518,
#43519,#43520,#43521,#43522,#43523,#43524,#43525,#43526,#43527,#43528,#43529,
#43530,#43531,#43532,#43533,#43534,#43535,#43536,#43537,#43538,#43539,#43540,
#43541,#43542,#43543,#43544,#43545,#43546,#43547,#43548,#43549,#43550,#43551,
#43552,#43553,#43554,#43555,#43556,#43557,#43558,#43559,#43560,#43561,#43562,
#43563,#43564,#43565,#43566,#43567,#43568,#43569,#43570,#43571,#43572,#43573,
#43574,#43575,#43576,#43577,#43578,#43579,#43580,#43581,#43582,#43583,#43584,
#43585,#43586,#43587,#43588,#43589,#43590,#43591,#43592,#43593,#43594,#43595,
#43596,#43597,#43598,#43599,#43600,#43601,#43602,#43603,#43604,#43605,#43606,
#43607,#43608,#43609,#43610,#43611,#43612,#43613,#43614,#43615,#43616,#43617,
#43618,#43619,#43620,#43621,#43622,#43623,#43624,#43625,#43626,#43627,#43628,
#43629,#43630,#43631,#43632,#43633,#43634,#43635,#43636,#43637,#43638,#43639,
#43640,#43641,#43642,#43643,#43644,#43645,#43646,#43647,#43648,#43649,#43650,
#43651,#43652,#43653,#43654,#43655,#43656,#43657,#43658,#43659,#43660,#43661,
#43662,#43663,#43664,#43665,#43666,#43667,#43668,#43669,#43670,#43671,#43672,
#43673,#43674,#43675,#43676,#43677,#43678,#43679,#43680,#43681,#43682,#43683,
#43684,#43685,#43686,#43687,#43688,#43689,#43690,#43691,#43692,#43693,#43694,
#43695,#43696,#43697,#43698,#43699,#43700,#43701,#43702,#43703,#43704,#43705,
#43706,#43707,#43708,#43709,#43710,#43711,#43712,#43713,#43714,#43715,#43716,
#43717,#43718,#43719,#43720),.UNSPECIFIED.,.F.,.F.,(4,3,3,3,3,3,3,3,3,3,
3,3,3,3,3,3,3,3,3,3,3,3,3,3,3,3,3,3,3,3,3,3,3,3,3,3,3,3,3,3,3,3,3,3,3,3,
3,3,3,3,3,3,3,3,3,3,3,3,3,3,3,3,3,3,3,3,3,3,3,3,3,3,3,3,3,3,4),(97.389372261456,
97.4717475320007,97.554046784624,97.6365956946908,97.718815685072,97.8010275054444,
97.8832501830832,97.9660471536019,98.0483900879616,98.1314140765598,98.214438065158,
98.2981847978599,98.3818284748756,98.4653892189419,98.5488870808986,98.6323495814612,
98.7157947169534,98.7992405517961,98.8827051470339,98.9662583324558,99.0498561660283,
99.1335877288901,99.2134215673572,99.2971683000592,99.380811977075,99.4643727211417,
99.5478705830985,99.6313330836612,99.7147782191535,99.7982240539964,99.8816886492344,
99.9652418346564,100.048839668229,100.132571231091,100.212405069556,100.296151802258,
100.379795479274,100.46335622334,100.546854085297,100.630316585859,100.713761721352,
100.797207556195,100.880672151433,100.964225336855,101.047823170427,101.131554733289,
101.211388571756,101.295135304458,101.378778981474,101.46233972554,101.545837587497,
101.629300088059,101.712745223552,101.796191058395,101.879655653632,101.963208839054,
102.046806672627,102.130538235489,102.210372073955,102.294118806657,102.377762483673,
102.46132322774,102.544821089696,102.628283590259,102.711728725751,102.795174560593,
102.878639155831,102.962192341253,103.045790174826,103.129521737688,103.209355576154,
103.298982946675,103.392376602082,103.481568554493,103.570604407169,103.659433763089,
103.672557568303),.UNSPECIFIED.);
#401=B_SPLINE_CURVE_WITH_KNOTS('',3,(#43722,#43723,#43724,#43725,#43726,
#43727,#43728,#43729,#43730,#43731,#43732,#43733,#43734,#43735,#43736,#43737,
#43738,#43739,#43740,#43741,#43742,#43743,#43744,#43745,#43746,#43747,#43748,
#43749,#43750,#43751,#43752,#43753,#43754,#43755,#43756,#43757,#43758,#43759,
#43760,#43761,#43762,#43763,#43764,#43765,#43766,#43767,#43768,#43769,#43770,
#43771,#43772,#43773,#43774,#43775,#43776,#43777,#43778,#43779,#43780,#43781,
#43782,#43783,#43784,#43785,#43786,#43787,#43788,#43789,#43790,#43791,#43792,
#43793,#43794,#43795,#43796,#43797,#43798,#43799,#43800,#43801,#43802,#43803,
#43804,#43805,#43806,#43807,#43808,#43809,#43810,#43811,#43812,#43813,#43814,
#43815,#43816,#43817,#43818,#43819,#43820,#43821,#43822,#43823,#43824,#43825,
#43826,#43827,#43828,#43829,#43830,#43831,#43832,#43833,#43834,#43835,#43836,
#43837,#43838,#43839,#43840,#43841,#43842,#43843,#43844,#43845,#43846,#43847,
#43848,#43849,#43850,#43851,#43852,#43853,#43854,#43855,#43856,#43857,#43858,
#43859,#43860,#43861,#43862,#43863,#43864,#43865,#43866,#43867,#43868,#43869,
#43870,#43871,#43872,#43873,#43874,#43875,#43876,#43877,#43878,#43879,#43880,
#43881,#43882,#43883,#43884,#43885,#43886,#43887,#43888,#43889,#43890,#43891,
#43892,#43893,#43894,#43895,#43896,#43897,#43898,#43899,#43900,#43901,#43902,
#43903,#43904,#43905,#43906,#43907,#43908,#43909,#43910,#43911,#43912,#43913,
#43914,#43915,#43916,#43917,#43918,#43919,#43920,#43921,#43922,#43923,#43924,
#43925,#43926,#43927,#43928,#43929,#43930,#43931,#43932,#43933,#43934,#43935,
#43936,#43937,#43938,#43939,#43940,#43941,#43942,#43943,#43944,#43945,#43946,
#43947),.UNSPECIFIED.,.F.,.F.,(4,3,3,3,3,3,3,3,3,3,3,3,3,3,3,3,3,3,3,3,
3,3,3,3,3,3,3,3,3,3,3,3,3,3,3,3,3,3,3,3,3,3,3,3,3,3,3,3,3,3,3,3,3,3,3,3,
3,3,3,3,3,3,3,3,3,3,3,3,3,3,3,3,3,3,3,4),(91.1061869541058,91.2215535497639,
91.3053002824658,91.3889439594816,91.4725047035478,91.5560025655045,91.6394650660671,
91.7229102015593,91.8063560364022,91.8898206316402,91.9733738170621,92.0569716506346,
92.1407032134965,92.220537051963,92.304283784665,92.3879274616808,92.4714882057472,
92.5549860677039,92.6384485682665,92.7218937037588,92.8053395386016,92.8888041338397,
92.9723573192615,93.0559551528342,93.139686715696,93.2195205541622,93.3032672868643,
93.3869109638802,93.4704717079468,93.5539695699036,93.6374320704662,93.7208772059586,
93.8043230408015,93.8877876360397,93.9713408214616,94.0549386550344,94.1386702178963,
94.2185040563614,94.3022507890633,94.385894466079,94.4694552101454,94.552953072102,
94.6364155726645,94.7198607081567,94.8033065429994,94.8867711382374,94.9703243236592,
95.0539221572317,95.1376537200934,95.2174875585605,95.3012342912625,95.3848779682784,
95.4684387123449,95.5519365743017,95.6353990748643,95.7188442103567,95.8022900451996,
95.8857546404377,95.9693078258596,96.0529056594323,96.1366372222942,96.2164710607597,
96.3002177934616,96.3838614704774,96.467422214544,96.5509200765008,96.6343825770633,
96.7178277125556,96.8012735473983,96.8847381426364,96.9682913280583,97.0518891616309,
97.1356207244927,97.2154545629589,97.3450039787278,97.3893722612854),
 .UNSPECIFIED.);
#402=B_SPLINE_CURVE_WITH_KNOTS('',3,(#43949,#43950,#43951,#43952,#43953,
#43954,#43955,#43956,#43957,#43958,#43959,#43960,#43961,#43962,#43963,#43964,
#43965,#43966,#43967,#43968,#43969,#43970,#43971,#43972,#43973,#43974,#43975,
#43976,#43977,#43978,#43979,#43980,#43981,#43982,#43983,#43984,#43985,#43986,
#43987,#43988,#43989,#43990,#43991,#43992,#43993,#43994,#43995,#43996,#43997,
#43998,#43999,#44000,#44001,#44002,#44003,#44004,#44005,#44006,#44007,#44008,
#44009,#44010,#44011,#44012,#44013,#44014,#44015,#44016,#44017,#44018,#44019,
#44020,#44021,#44022,#44023,#44024,#44025,#44026,#44027,#44028,#44029,#44030,
#44031,#44032,#44033,#44034,#44035,#44036,#44037,#44038,#44039,#44040,#44041,
#44042,#44043,#44044,#44045,#44046,#44047,#44048,#44049,#44050,#44051,#44052,
#44053,#44054,#44055,#44056,#44057,#44058,#44059,#44060,#44061,#44062,#44063,
#44064,#44065,#44066,#44067,#44068,#44069,#44070,#44071,#44072,#44073,#44074,
#44075,#44076,#44077,#44078,#44079,#44080,#44081,#44082,#44083,#44084,#44085,
#44086,#44087,#44088,#44089,#44090,#44091,#44092,#44093,#44094,#44095,#44096,
#44097,#44098,#44099,#44100,#44101,#44102,#44103,#44104,#44105,#44106,#44107,
#44108,#44109,#44110,#44111,#44112,#44113,#44114,#44115,#44116,#44117,#44118,
#44119,#44120,#44121,#44122,#44123,#44124,#44125,#44126,#44127,#44128,#44129,
#44130,#44131,#44132,#44133,#44134,#44135,#44136,#44137,#44138,#44139,#44140,
#44141,#44142,#44143,#44144,#44145,#44146,#44147,#44148,#44149,#44150,#44151,
#44152,#44153,#44154,#44155,#44156,#44157,#44158,#44159,#44160,#44161,#44162,
#44163,#44164,#44165,#44166,#44167,#44168,#44169,#44170,#44171,#44172,#44173,
#44174,#44175,#44176,#44177),.UNSPECIFIED.,.F.,.F.,(4,3,3,3,3,3,3,3,3,3,
3,3,3,3,3,3,3,3,3,3,3,3,3,3,3,3,3,3,3,3,3,3,3,3,3,3,3,3,3,3,3,3,3,3,3,3,
3,3,3,3,3,3,3,3,3,3,3,3,3,3,3,3,3,3,3,3,3,3,3,3,3,3,3,3,3,3,4),(84.8230016470981,
84.9147924149001,85.0070556960825,85.0995627342371,85.1923976742333,85.2276525365689,
85.3113992692709,85.3950429462865,85.4786036903529,85.5621015523098,85.6455640528723,
85.7290091883646,85.8124550232074,85.8959196184455,85.9794728038673,86.0630706374399,
86.1468022003017,86.226636038768,86.31038277147,86.3940264484858,86.4775871925524,
86.5610850545091,86.6445475550717,86.727992690564,86.8114385254069,86.894903120645,
86.9784563060669,87.0620541396396,87.1457857025015,87.2256195409672,87.3093662736691,
87.3930099506848,87.4765706947512,87.5600685567078,87.6435310572704,87.7269761927626,
87.8104220276053,87.8938866228433,87.9774398082651,88.0610376418377,88.1447692046995,
88.2246030431664,88.3083497758684,88.3919934528843,88.4755541969509,88.5590520589077,
88.6425145594703,88.7259596949627,88.8094055298056,88.8928701250438,88.9764233104657,
89.0600211440384,89.1437527069003,89.2235865453655,89.3073332780675,89.3909769550833,
89.4745376991498,89.5580355611065,89.6414980616691,89.7249431971614,89.8083890320042,
89.8918536272423,89.9754068126641,90.0590046462367,90.1427362090986,90.2225700475647,
90.3051881406199,90.3877040229452,90.4701388369267,90.5525127567424,90.6348543732513,
90.7171826531799,90.7995165497718,90.8819169921766,90.9643524122932,91.0468970494953,
91.106186953972),.UNSPECIFIED.);
#403=B_SPLINE_CURVE_WITH_KNOTS('',3,(#44179,#44180,#44181,#44182,#44183,
#44184,#44185,#44186,#44187,#44188,#44189,#44190,#44191,#44192,#44193,#44194,
#44195,#44196,#44197,#44198,#44199,#44200,#44201,#44202,#44203,#44204,#44205,
#44206,#44207,#44208,#44209,#44210,#44211,#44212,#44213,#44214,#44215,#44216,
#44217,#44218,#44219,#44220,#44221,#44222,#44223,#44224,#44225,#44226,#44227,
#44228,#44229,#44230,#44231,#44232,#44233,#44234,#44235,#44236,#44237,#44238,
#44239,#44240,#44241,#44242,#44243,#44244,#44245,#44246,#44247,#44248,#44249,
#44250,#44251,#44252,#44253,#44254,#44255,#44256,#44257,#44258,#44259,#44260,
#44261,#44262,#44263,#44264,#44265,#44266,#44267,#44268,#44269,#44270,#44271,
#44272,#44273,#44274,#44275,#44276,#44277,#44278,#44279,#44280,#44281,#44282,
#44283,#44284,#44285,#44286,#44287,#44288,#44289,#44290,#44291,#44292,#44293,
#44294,#44295,#44296,#44297,#44298,#44299,#44300,#44301,#44302,#44303,#44304,
#44305,#44306,#44307,#44308,#44309,#44310,#44311,#44312,#44313,#44314,#44315,
#44316,#44317,#44318,#44319,#44320,#44321,#44322,#44323,#44324,#44325,#44326,
#44327,#44328,#44329,#44330,#44331,#44332,#44333,#44334,#44335,#44336,#44337,
#44338,#44339,#44340,#44341,#44342,#44343,#44344,#44345,#44346,#44347,#44348,
#44349,#44350,#44351,#44352,#44353,#44354,#44355,#44356,#44357,#44358,#44359,
#44360,#44361,#44362,#44363,#44364,#44365,#44366,#44367,#44368,#44369,#44370,
#44371,#44372,#44373,#44374,#44375,#44376,#44377,#44378,#44379,#44380,#44381,
#44382,#44383,#44384,#44385,#44386,#44387,#44388,#44389,#44390,#44391,#44392,
#44393,#44394,#44395,#44396,#44397,#44398,#44399,#44400,#44401,#44402,#44403,
#44404,#44405,#44406,#44407),.UNSPECIFIED.,.F.,.F.,(4,3,3,3,3,3,3,3,3,3,
3,3,3,3,3,3,3,3,3,3,3,3,3,3,3,3,3,3,3,3,3,3,3,3,3,3,3,3,3,3,3,3,3,3,3,3,
3,3,3,3,3,3,3,3,3,3,3,3,3,3,3,3,3,3,3,3,3,3,3,3,3,3,3,3,3,3,4),(78.5398163397466,
78.6265582377,78.7095749161233,78.7925857145311,78.8756090555744,78.9586633669885,
79.0418131756962,79.1250192064087,79.208346008455,79.2337515233739,79.3174982560759,
79.4011419330917,79.4847026771586,79.5682005391154,79.6516630396781,79.7351081751703,
79.818554010013,79.9020186052512,79.985571790673,80.0691696242457,80.1529011871076,
80.2327350255731,80.3164817582751,80.400125435291,80.4836861793577,80.5671840413144,
80.6506465418771,80.7340916773693,80.8175375122122,80.9010021074502,80.984555292872,
81.0681531264446,81.1518846893065,81.2317185277722,81.3154652604742,81.3991089374899,
81.4826696815565,81.5661675435133,81.649630044076,81.7330751795684,81.8165210144114,
81.8999856096495,81.9835387950714,82.0671366286439,82.1508681915057,82.2307020299714,
82.3144487626733,82.3980924396891,82.4816531837558,82.5651510457127,82.6486135462753,
82.7320586817676,82.8155045166105,82.8989691118484,82.9825222972702,83.0661201308428,
83.1498516937047,83.2296855321705,83.3134322648725,83.3970759418886,83.4806366859552,
83.564134547912,83.6475970484746,83.7310421839668,83.8144880188095,83.8979526140471,
83.9815057994689,84.0651036330417,84.1488351959036,84.2286690343697,84.3137666968213,
84.3987507891206,84.4836377060624,84.5684786912783,84.6532096453913,84.7381056461587,
84.8230016469262),.UNSPECIFIED.);
#404=B_SPLINE_CURVE_WITH_KNOTS('',3,(#44409,#44410,#44411,#44412,#44413,
#44414,#44415,#44416,#44417,#44418,#44419,#44420,#44421,#44422,#44423,#44424,
#44425,#44426,#44427,#44428,#44429,#44430,#44431,#44432,#44433,#44434,#44435,
#44436,#44437,#44438,#44439,#44440,#44441,#44442,#44443,#44444,#44445,#44446,
#44447,#44448,#44449,#44450,#44451,#44452,#44453,#44454,#44455,#44456,#44457,
#44458,#44459,#44460,#44461,#44462,#44463,#44464,#44465,#44466,#44467,#44468,
#44469,#44470,#44471,#44472,#44473,#44474,#44475,#44476,#44477,#44478,#44479,
#44480,#44481,#44482,#44483,#44484,#44485,#44486,#44487,#44488,#44489,#44490,
#44491,#44492,#44493,#44494,#44495,#44496,#44497,#44498,#44499,#44500,#44501,
#44502,#44503,#44504,#44505,#44506,#44507,#44508,#44509,#44510,#44511,#44512,
#44513,#44514,#44515,#44516,#44517,#44518,#44519,#44520,#44521,#44522,#44523,
#44524,#44525,#44526,#44527,#44528,#44529,#44530,#44531,#44532,#44533,#44534,
#44535,#44536,#44537,#44538,#44539,#44540,#44541,#44542,#44543,#44544,#44545,
#44546,#44547,#44548,#44549,#44550,#44551,#44552,#44553,#44554,#44555,#44556,
#44557,#44558,#44559,#44560,#44561,#44562,#44563,#44564,#44565,#44566,#44567,
#44568,#44569,#44570,#44571,#44572,#44573,#44574,#44575,#44576,#44577,#44578,
#44579,#44580,#44581,#44582,#44583,#44584,#44585,#44586,#44587,#44588,#44589,
#44590,#44591,#44592,#44593,#44594,#44595,#44596,#44597,#44598,#44599,#44600,
#44601,#44602,#44603,#44604,#44605,#44606,#44607,#44608,#44609,#44610,#44611,
#44612,#44613,#44614,#44615,#44616,#44617,#44618,#44619,#44620,#44621,#44622,
#44623,#44624,#44625,#44626,#44627,#44628,#44629,#44630,#44631,#44632,#44633,
#44634),.UNSPECIFIED.,.F.,.F.,(4,3,3,3,3,3,3,3,3,3,3,3,3,3,3,3,3,3,3,3,
3,3,3,3,3,3,3,3,3,3,3,3,3,3,3,3,3,3,3,3,3,3,3,3,3,3,3,3,3,3,3,3,3,3,3,3,
3,3,3,3,3,3,3,3,3,3,3,3,3,3,3,3,3,3,3,4),(72.256631032715,72.3401482880491,
72.4235629091826,72.5068952574145,72.5901656203862,72.6734020156145,72.7566222960338,
72.8398447389392,72.9230876193702,73.0064192735912,73.0897974893735,73.1733051991883,
73.2398505101789,73.3235972428809,73.4072409198967,73.4908016639628,73.5742995259199,
73.6577620264825,73.7412071619747,73.8246529968176,73.9081175920556,73.9916707774774,
74.07526861105,74.1590001739119,74.2388340123781,74.3225807450801,74.4062244220959,
74.4897851661626,74.5732830281197,74.6567455286824,74.7401906641747,74.8236364990176,
74.9071010942556,74.9906542796775,75.0742521132503,75.1579836761122,75.2378175145772,
75.3215642472792,75.4052079242951,75.4887686683616,75.5722665303182,75.6557290308808,
75.739174166373,75.8226200012158,75.9060845964539,75.9896377818757,76.0732356154484,
76.1569671783103,76.2368010167764,76.3205477494783,76.4041914264938,76.4877521705604,
76.5712500325174,76.6547125330799,76.7381576685721,76.8216035034147,76.9050680986528,
76.9886212840747,77.0722191176474,77.1559506805093,77.2357845189756,77.3195312516775,
77.4031749286932,77.4867356727598,77.5702335347166,77.6536960352794,77.7371411707716,
77.8205870056145,77.9040516008525,77.9876047862744,78.0712026198471,78.1549341827089,
78.2347680211747,78.3361959981597,78.438006168876,78.5398163395922),
 .UNSPECIFIED.);
#405=B_SPLINE_CURVE_WITH_KNOTS('',3,(#44636,#44637,#44638,#44639,#44640,
#44641,#44642,#44643,#44644,#44645,#44646,#44647,#44648,#44649,#44650,#44651,
#44652,#44653,#44654,#44655,#44656,#44657,#44658,#44659,#44660,#44661,#44662,
#44663,#44664,#44665,#44666,#44667,#44668,#44669,#44670,#44671,#44672,#44673,
#44674,#44675,#44676,#44677,#44678,#44679,#44680,#44681,#44682,#44683,#44684,
#44685,#44686,#44687,#44688,#44689,#44690,#44691,#44692,#44693,#44694,#44695,
#44696,#44697,#44698,#44699,#44700,#44701,#44702,#44703,#44704,#44705,#44706,
#44707,#44708,#44709,#44710,#44711,#44712,#44713,#44714,#44715,#44716,#44717,
#44718,#44719,#44720,#44721,#44722,#44723,#44724,#44725,#44726,#44727,#44728,
#44729,#44730,#44731,#44732,#44733,#44734,#44735,#44736,#44737,#44738,#44739,
#44740,#44741,#44742,#44743,#44744,#44745,#44746,#44747,#44748,#44749,#44750,
#44751,#44752,#44753,#44754,#44755,#44756,#44757,#44758,#44759,#44760,#44761,
#44762,#44763,#44764,#44765,#44766,#44767,#44768,#44769,#44770,#44771,#44772,
#44773,#44774,#44775,#44776,#44777,#44778,#44779,#44780,#44781,#44782,#44783,
#44784,#44785,#44786,#44787,#44788,#44789,#44790,#44791,#44792,#44793,#44794,
#44795,#44796,#44797,#44798,#44799,#44800,#44801,#44802,#44803,#44804,#44805,
#44806,#44807,#44808,#44809,#44810,#44811,#44812,#44813,#44814,#44815,#44816,
#44817,#44818,#44819,#44820,#44821,#44822,#44823,#44824,#44825,#44826,#44827,
#44828,#44829,#44830,#44831,#44832,#44833,#44834,#44835,#44836,#44837,#44838,
#44839,#44840,#44841,#44842,#44843,#44844,#44845,#44846,#44847,#44848,#44849,
#44850,#44851,#44852,#44853,#44854,#44855,#44856,#44857,#44858,#44859,#44860,
#44861,#44862,#44863,#44864),.UNSPECIFIED.,.F.,.F.,(4,3,3,3,3,3,3,3,3,3,
3,3,3,3,3,3,3,3,3,3,3,3,3,3,3,3,3,3,3,3,3,3,3,3,3,3,3,3,3,3,3,3,3,3,3,3,
3,3,3,3,3,3,3,3,3,3,3,3,3,3,3,3,3,3,3,3,3,3,3,3,3,3,3,3,3,3,4),(65.9734457255818,
66.077168752151,66.1826616383644,66.2469659947847,66.3307127274868,66.4143564045027,
66.4979171485692,66.581415010526,66.6648775110887,66.748322646581,66.831768481424,
66.9152330766622,66.9987862620842,67.0823840956569,67.1661156585188,67.2459494969839,
67.3296962296859,67.4133399067017,67.4969006507683,67.5803985127249,67.6638610132875,
67.7473061487798,67.8307519836227,67.9142165788608,67.9977697642827,68.0813675978553,
68.1650991607172,68.2449329991831,68.3286797318851,68.4123234089009,68.4958841529674,
68.5793820149241,68.6628445154867,68.7462896509789,68.8297354858217,68.9132000810598,
68.9967532664816,69.0803511000543,69.1640826629161,69.2439165013822,69.3276632340842,
69.4113069111,69.4948676551665,69.5783655171233,69.6618280176859,69.7452731531782,
69.8287189880211,69.9121835832592,69.995736768681,70.0793346022537,70.1630661651156,
70.2429000035814,70.3266467362834,70.4102904132992,70.4938511573656,70.5773490193223,
70.6608115198849,70.7442566553772,70.82770249022,70.9111670854581,70.9947202708799,
71.0783181044525,71.1620496673144,71.2418835057806,71.3256302384826,71.4092739154985,
71.4928346595651,71.5763325215219,71.6597950220846,71.7432401575768,71.8266859924197,
71.9101505876577,71.9937037730796,72.0773016066523,72.1610331695142,72.2408670079797,
72.256631032567),.UNSPECIFIED.);
#406=B_SPLINE_CURVE_WITH_KNOTS('',3,(#44866,#44867,#44868,#44869,#44870,
#44871,#44872,#44873,#44874,#44875,#44876,#44877,#44878,#44879,#44880,#44881,
#44882,#44883,#44884,#44885,#44886,#44887,#44888,#44889,#44890,#44891,#44892,
#44893,#44894,#44895,#44896,#44897,#44898,#44899,#44900,#44901,#44902,#44903,
#44904,#44905,#44906,#44907,#44908,#44909,#44910,#44911,#44912,#44913,#44914,
#44915,#44916,#44917,#44918,#44919,#44920,#44921,#44922,#44923,#44924,#44925,
#44926,#44927,#44928,#44929,#44930,#44931,#44932,#44933,#44934,#44935,#44936,
#44937,#44938,#44939,#44940,#44941,#44942,#44943,#44944,#44945,#44946,#44947,
#44948,#44949,#44950,#44951,#44952,#44953,#44954,#44955,#44956,#44957,#44958,
#44959,#44960,#44961,#44962,#44963,#44964,#44965,#44966,#44967,#44968,#44969,
#44970,#44971,#44972,#44973,#44974,#44975,#44976,#44977,#44978,#44979,#44980,
#44981,#44982,#44983,#44984,#44985,#44986,#44987,#44988,#44989,#44990,#44991,
#44992,#44993,#44994,#44995,#44996,#44997,#44998,#44999,#45000,#45001,#45002,
#45003,#45004,#45005,#45006,#45007,#45008,#45009,#45010,#45011,#45012,#45013,
#45014,#45015,#45016,#45017,#45018,#45019,#45020,#45021,#45022,#45023,#45024,
#45025,#45026,#45027,#45028,#45029,#45030,#45031,#45032,#45033,#45034,#45035,
#45036,#45037,#45038,#45039,#45040,#45041,#45042,#45043,#45044,#45045,#45046,
#45047,#45048,#45049,#45050,#45051,#45052,#45053,#45054,#45055,#45056,#45057,
#45058,#45059,#45060,#45061,#45062,#45063,#45064,#45065,#45066,#45067,#45068,
#45069,#45070,#45071,#45072,#45073,#45074,#45075,#45076,#45077,#45078,#45079,
#45080,#45081,#45082,#45083,#45084,#45085,#45086,#45087,#45088,#45089,#45090,
#45091,#45092,#45093,#45094),.UNSPECIFIED.,.F.,.F.,(4,3,3,3,3,3,3,3,3,3,
3,3,3,3,3,3,3,3,3,3,3,3,3,3,3,3,3,3,3,3,3,3,3,3,3,3,3,3,3,3,3,3,3,3,3,3,
3,3,3,3,3,3,3,3,3,3,3,3,3,3,3,3,3,3,3,3,3,3,3,3,3,3,3,3,3,3,4),(59.6902604182078,
59.7757032004822,59.8611946417817,59.946749287853,60.0324436450503,60.1182148552943,
60.2041428744123,60.2530649815898,60.3368117142918,60.4204553913077,60.5040161353741,
60.5875139973306,60.6709764978933,60.7544216333856,60.8378674682284,60.9213320634666,
61.0048852488885,61.0884830824612,61.1722146453231,61.2520484837889,61.3357952164908,
61.4194388935065,61.5029996375732,61.58649749953,61.6699600000926,61.7534051355847,
61.8368509704275,61.9203155656657,62.0038687510876,62.0874665846602,62.1711981475221,
62.2510319859881,62.3347787186901,62.4184223957058,62.5019831397724,62.5854810017289,
62.6689435022915,62.7523886377836,62.8358344726266,62.9192990678649,63.0028522532868,
63.0864500868593,63.1701816497212,63.2500154881873,63.3337622208893,63.4174058979051,
63.5009666419717,63.5844645039286,63.6679270044913,63.7513721399835,63.8348179748266,
63.9182825700649,64.0018357554867,64.0854335890596,64.1691651519215,64.2489989903864,
64.3327457230884,64.4163894001042,64.4999501441702,64.5834480061277,64.6669105066903,
64.7503556421825,64.8338014770253,64.917266072263,65.0008192576848,65.0844170912573,
65.1681486541192,65.2479824925856,65.3309728091399,65.4138315333062,65.4966144831197,
65.5793404606703,65.6620282206894,65.744715102943,65.8273989459123,65.9101328758718,
65.9734457253874),.UNSPECIFIED.);
#407=B_SPLINE_CURVE_WITH_KNOTS('',3,(#45096,#45097,#45098,#45099,#45100,
#45101,#45102,#45103,#45104,#45105,#45106,#45107,#45108,#45109,#45110,#45111,
#45112,#45113,#45114,#45115,#45116,#45117,#45118,#45119,#45120,#45121,#45122,
#45123,#45124,#45125,#45126,#45127,#45128,#45129,#45130,#45131,#45132,#45133,
#45134,#45135,#45136,#45137,#45138,#45139,#45140,#45141,#45142,#45143,#45144,
#45145,#45146,#45147,#45148,#45149,#45150,#45151,#45152,#45153,#45154,#45155,
#45156,#45157,#45158,#45159,#45160,#45161,#45162,#45163,#45164,#45165,#45166,
#45167,#45168,#45169,#45170,#45171,#45172,#45173,#45174,#45175,#45176,#45177,
#45178,#45179,#45180,#45181,#45182,#45183,#45184,#45185,#45186,#45187,#45188,
#45189,#45190,#45191,#45192,#45193,#45194,#45195,#45196,#45197,#45198,#45199,
#45200,#45201,#45202,#45203,#45204,#45205,#45206,#45207,#45208,#45209,#45210,
#45211,#45212,#45213,#45214,#45215,#45216,#45217,#45218,#45219,#45220,#45221,
#45222,#45223,#45224,#45225,#45226,#45227,#45228,#45229,#45230,#45231,#45232,
#45233,#45234,#45235,#45236,#45237,#45238,#45239,#45240,#45241,#45242,#45243,
#45244,#45245,#45246,#45247,#45248,#45249,#45250,#45251,#45252,#45253,#45254,
#45255,#45256,#45257,#45258,#45259,#45260,#45261,#45262,#45263,#45264,#45265,
#45266,#45267,#45268,#45269,#45270,#45271,#45272,#45273,#45274,#45275,#45276,
#45277,#45278,#45279,#45280,#45281,#45282,#45283,#45284,#45285,#45286,#45287,
#45288,#45289,#45290,#45291,#45292,#45293,#45294,#45295,#45296,#45297,#45298,
#45299,#45300,#45301,#45302,#45303,#45304,#45305,#45306,#45307,#45308,#45309,
#45310,#45311,#45312,#45313,#45314,#45315,#45316,#45317,#45318,#45319,#45320,
#45321,#45322,#45323,#45324),.UNSPECIFIED.,.F.,.F.,(4,3,3,3,3,3,3,3,3,3,
3,3,3,3,3,3,3,3,3,3,3,3,3,3,3,3,3,3,3,3,3,3,3,3,3,3,3,3,3,3,3,3,3,3,3,3,
3,3,3,3,3,3,3,3,3,3,3,3,3,3,3,3,3,3,3,3,3,3,3,3,3,3,3,3,3,3,4),(53.4070751111433,
53.4894981066909,53.5718383807227,53.6577540791817,53.7399988815535,53.8222302256025,
53.9044671278617,53.9867286072932,54.0690777661479,54.1514786212285,54.2339950563424,
54.2591639683948,54.3429107010967,54.4265543781124,54.5101151221791,54.5936129841357,
54.6770754846984,54.7605206201908,54.8439664550337,54.9274310502718,55.0109842356937,
55.0945820692664,55.1783136321283,55.2581474705939,55.341894203296,55.4255378803119,
55.5090986243784,55.592596486335,55.6760589868977,55.75950412239,55.8429499572326,
55.9264145524706,56.0099677378925,56.0935655714652,56.177297134327,56.2571309727931,
56.3408777054951,56.4245213825109,56.5080821265771,56.5915799885338,56.6750424890964,
56.7584876245886,56.8419334594315,56.9253980546696,57.0089512400915,57.0925490736641,
57.1762806365259,57.2561144749923,57.3398612076942,57.42350488471,57.5070656287766,
57.5905634907332,57.6740259912958,57.757471126788,57.8409169616306,57.9243815568686,
58.0079347422905,58.0915325758632,58.1752641387251,58.2550979771914,58.3388447098935,
58.4224883869095,58.5060491309762,58.5895469929326,58.6730094934953,58.7564546289875,
58.8399004638304,58.9233650590685,59.0069182444905,59.0905160780629,59.1742476409249,
59.2540814793906,59.3450829724981,59.4357708837664,59.526265849522,59.6164523540533,
59.6902604180762),.UNSPECIFIED.);
#408=B_SPLINE_CURVE_WITH_KNOTS('',3,(#45326,#45327,#45328,#45329,#45330,
#45331,#45332,#45333,#45334,#45335,#45336,#45337,#45338,#45339,#45340,#45341,
#45342,#45343,#45344,#45345,#45346,#45347,#45348,#45349,#45350,#45351,#45352,
#45353,#45354,#45355,#45356,#45357,#45358,#45359,#45360,#45361,#45362,#45363,
#45364,#45365,#45366,#45367,#45368,#45369,#45370,#45371,#45372,#45373,#45374,
#45375,#45376,#45377,#45378,#45379,#45380,#45381,#45382,#45383,#45384,#45385,
#45386,#45387,#45388,#45389,#45390,#45391,#45392,#45393,#45394,#45395,#45396,
#45397,#45398,#45399,#45400,#45401,#45402,#45403,#45404,#45405,#45406,#45407,
#45408,#45409,#45410,#45411,#45412,#45413,#45414,#45415,#45416,#45417,#45418,
#45419,#45420,#45421,#45422,#45423,#45424,#45425,#45426,#45427,#45428,#45429,
#45430,#45431,#45432,#45433,#45434,#45435,#45436,#45437,#45438,#45439,#45440,
#45441,#45442,#45443,#45444,#45445,#45446,#45447,#45448,#45449,#45450,#45451,
#45452,#45453,#45454,#45455,#45456,#45457,#45458,#45459,#45460,#45461,#45462,
#45463,#45464,#45465,#45466,#45467,#45468,#45469,#45470,#45471,#45472,#45473,
#45474,#45475,#45476,#45477,#45478,#45479,#45480,#45481,#45482,#45483,#45484,
#45485,#45486,#45487,#45488,#45489,#45490,#45491,#45492,#45493,#45494,#45495,
#45496,#45497,#45498,#45499,#45500,#45501,#45502,#45503,#45504,#45505,#45506,
#45507,#45508,#45509,#45510,#45511,#45512,#45513,#45514,#45515,#45516,#45517,
#45518,#45519,#45520,#45521,#45522,#45523,#45524,#45525,#45526,#45527,#45528,
#45529,#45530,#45531,#45532,#45533,#45534,#45535,#45536,#45537,#45538,#45539,
#45540,#45541,#45542,#45543,#45544,#45545,#45546,#45547,#45548),
 .UNSPECIFIED.,.F.,.F.,(4,3,3,3,3,3,3,3,3,3,3,3,3,3,3,3,3,3,3,3,3,3,3,3,
3,3,3,3,3,3,3,3,3,3,3,3,3,3,3,3,3,3,3,3,3,3,3,3,3,3,3,3,3,3,3,3,3,3,3,3,
3,3,3,3,3,3,3,3,3,3,3,3,3,3,4),(47.1238898038487,47.2662794530006,47.3500261857027,
47.4336698627184,47.5172306067851,47.6007284687418,47.6841909693046,47.7676361047969,
47.8510819396398,47.9345465348779,48.0180997202998,48.1016975538725,48.1854291167344,
48.2652629551998,48.3490096879018,48.4326533649175,48.5162141089841,48.5997119709408,
48.6831744715034,48.7666196069956,48.8500654418384,48.9335300370765,49.0170832224984,
49.1006810560709,49.1844126189328,49.2642464573989,49.3479931901008,49.4316368671166,
49.5151976111831,49.5986954731397,49.6821579737023,49.7656031091945,49.8490489440373,
49.9325135392754,50.0160667246972,50.0996645582698,50.1833961211316,50.2632299595981,
50.3469766923001,50.4306203693159,50.5141811133825,50.5976789753392,50.6811414759019,
50.7645866113942,50.8480324462371,50.9314970414752,51.0150502268971,51.0986480604698,
51.1823796233317,51.2622134617973,51.3459601944993,51.4296038715151,51.5131646155817,
51.5966624775383,51.6801249781009,51.7635701135932,51.8470159484361,51.9304805436741,
52.014033729096,52.0976315626686,52.1813631255305,52.2611969639964,52.3449436966982,
52.4285873737139,52.5121481177803,52.5956459797368,52.6791084802993,52.7625536157914,
52.845999450634,52.9294640458718,53.0130172312935,53.0966150648661,53.1803466277278,
53.2601804661956,53.4070751110283),.UNSPECIFIED.);
#409=B_SPLINE_CURVE_WITH_KNOTS('',3,(#45550,#45551,#45552,#45553,#45554,
#45555,#45556,#45557,#45558,#45559,#45560,#45561,#45562,#45563,#45564,#45565,
#45566,#45567,#45568,#45569,#45570,#45571,#45572,#45573,#45574,#45575,#45576,
#45577,#45578,#45579,#45580,#45581,#45582,#45583,#45584,#45585,#45586,#45587,
#45588,#45589,#45590,#45591,#45592,#45593,#45594,#45595,#45596,#45597,#45598,
#45599,#45600,#45601,#45602,#45603,#45604,#45605,#45606,#45607,#45608,#45609,
#45610,#45611,#45612,#45613,#45614,#45615,#45616,#45617,#45618,#45619,#45620,
#45621,#45622,#45623,#45624,#45625,#45626,#45627,#45628,#45629,#45630,#45631,
#45632,#45633,#45634,#45635,#45636,#45637,#45638,#45639,#45640,#45641,#45642,
#45643,#45644,#45645,#45646,#45647,#45648,#45649,#45650,#45651,#45652,#45653,
#45654,#45655,#45656,#45657,#45658,#45659,#45660,#45661,#45662,#45663,#45664,
#45665,#45666,#45667,#45668,#45669,#45670,#45671,#45672,#45673,#45674,#45675,
#45676,#45677,#45678,#45679,#45680,#45681,#45682,#45683,#45684,#45685,#45686,
#45687,#45688,#45689,#45690,#45691,#45692,#45693,#45694,#45695,#45696,#45697,
#45698,#45699,#45700,#45701,#45702,#45703,#45704,#45705,#45706,#45707,#45708,
#45709,#45710,#45711,#45712,#45713,#45714,#45715,#45716,#45717,#45718,#45719,
#45720,#45721,#45722,#45723,#45724,#45725,#45726,#45727,#45728,#45729,#45730,
#45731,#45732,#45733,#45734,#45735,#45736,#45737,#45738,#45739,#45740,#45741,
#45742,#45743,#45744,#45745,#45746,#45747,#45748,#45749,#45750,#45751,#45752,
#45753,#45754,#45755,#45756,#45757,#45758,#45759,#45760,#45761,#45762,#45763,
#45764,#45765,#45766,#45767,#45768,#45769,#45770,#45771,#45772,#45773,#45774,
#45775,#45776,#45777,#45778),.UNSPECIFIED.,.F.,.F.,(4,3,3,3,3,3,3,3,3,3,
3,3,3,3,3,3,3,3,3,3,3,3,3,3,3,3,3,3,3,3,3,3,3,3,3,3,3,3,3,3,3,3,3,3,3,3,
3,3,3,3,3,3,3,3,3,3,3,3,3,3,3,3,3,3,3,3,3,3,3,3,3,3,3,3,3,3,4),(40.8407044968042,
40.9310285927585,41.0217286330852,41.1126186716987,41.2038067298644,41.2723784398056,
41.3561251725094,41.4397688495271,41.5233295935954,41.6068274555541,41.6902899561186,
41.7737350916128,41.8571809264576,41.9406455216977,42.0241987071215,42.1077965406961,
42.1915281035599,42.2713619420048,42.355108674706,42.438752351721,42.5223130957869,
42.6058109577429,42.6892734583047,42.7727185937962,42.8561644286382,42.9396290238755,
43.0231822092966,43.1067800428684,43.1905116057295,43.2703454442039,43.3540921769058,
43.4377358539216,43.521296597988,43.6047944599447,43.6882569605072,43.7717020959995,
43.8551479308422,43.9386125260803,44.0221657115021,44.1057635450746,44.1894951079364,
44.2693289464031,44.3530756791053,44.4367193561213,44.5202801001881,44.6037779621451,
44.687240462708,44.7706855982005,44.8541314330436,44.937596028282,45.0211492137041,
45.104747047277,45.1884786101391,45.2683124486023,45.3520591813042,45.4357028583199,
45.5192636023864,45.6027614643429,45.6862239649055,45.7696691003977,45.8531149352404,
45.9365795304784,46.0201327159002,46.1037305494727,46.1874621123345,46.2672959508014,
46.349822107809,46.432245982627,46.5187014602649,46.6009805544563,46.6832282441854,
46.7654635518224,46.8477054867025,46.9300093779677,47.0123494712962,47.0947847624809,
47.1238898037298),.UNSPECIFIED.);
#410=B_SPLINE_CURVE_WITH_KNOTS('',3,(#45780,#45781,#45782,#45783,#45784,
#45785,#45786,#45787,#45788,#45789,#45790,#45791,#45792,#45793,#45794,#45795,
#45796,#45797,#45798,#45799,#45800,#45801,#45802,#45803,#45804,#45805,#45806,
#45807,#45808,#45809,#45810,#45811,#45812,#45813,#45814,#45815,#45816,#45817,
#45818,#45819,#45820,#45821,#45822,#45823,#45824,#45825,#45826,#45827,#45828,
#45829,#45830,#45831,#45832,#45833,#45834,#45835,#45836,#45837,#45838,#45839,
#45840,#45841,#45842,#45843,#45844,#45845,#45846,#45847,#45848,#45849,#45850,
#45851,#45852,#45853,#45854,#45855,#45856,#45857,#45858,#45859,#45860,#45861,
#45862,#45863,#45864,#45865,#45866,#45867,#45868,#45869,#45870,#45871,#45872,
#45873,#45874,#45875,#45876,#45877,#45878,#45879,#45880,#45881,#45882,#45883,
#45884,#45885,#45886,#45887,#45888,#45889,#45890,#45891,#45892,#45893,#45894,
#45895,#45896,#45897,#45898,#45899,#45900,#45901,#45902,#45903,#45904,#45905,
#45906,#45907,#45908,#45909,#45910,#45911,#45912,#45913,#45914,#45915,#45916,
#45917,#45918,#45919,#45920,#45921,#45922,#45923,#45924,#45925,#45926,#45927,
#45928,#45929,#45930,#45931,#45932,#45933,#45934,#45935,#45936,#45937,#45938,
#45939,#45940,#45941,#45942,#45943,#45944,#45945,#45946,#45947,#45948,#45949,
#45950,#45951,#45952,#45953,#45954,#45955,#45956,#45957,#45958,#45959,#45960,
#45961,#45962,#45963,#45964,#45965,#45966,#45967,#45968,#45969,#45970,#45971,
#45972,#45973,#45974,#45975,#45976,#45977,#45978,#45979,#45980,#45981,#45982,
#45983,#45984,#45985,#45986,#45987,#45988,#45989,#45990,#45991,#45992,#45993,
#45994,#45995,#45996,#45997,#45998,#45999,#46000,#46001,#46002,#46003,#46004,
#46005,#46006,#46007,#46008),.UNSPECIFIED.,.F.,.F.,(4,3,3,3,3,3,3,3,3,3,
3,3,3,3,3,3,3,3,3,3,3,3,3,3,3,3,3,3,3,3,3,3,3,3,3,3,3,3,3,3,3,3,3,3,3,3,
3,3,3,3,3,3,3,3,3,3,3,3,3,3,3,3,3,3,3,3,3,3,3,3,3,3,3,3,3,3,4),(34.5575191894895,
34.6402936887573,34.7230330620196,34.8057559307772,34.8884809671239,34.9712268416032,
35.054061493518,35.136943771928,35.2199537508165,35.2784774266106,35.3622241593953,
35.4458678364949,35.5294285806463,35.6129264426885,35.6963889433377,35.7798340789172,
35.8632799138479,35.9467445091739,36.0302976946841,36.1138955283453,36.1976270912952,
36.2774609288098,36.3612076614882,36.4448513384802,36.5284120825231,36.6119099444563,
36.6953724449949,36.7788175804631,36.8622634152818,36.9457280104959,37.0292811958939,
37.1128790294426,37.196610592281,37.276444431009,37.3601911637012,37.4438348407069,
37.5273955847632,37.6108934467099,37.6943559472619,37.7778010827435,37.8612469175754,
37.9447115128023,38.0282646982131,38.1118625317746,38.1955940946252,38.2754279332081,
38.3591746659222,38.4428183429503,38.526379087029,38.6098769489982,38.6933394495735,
38.7767845850787,38.8602304199347,38.9436950151855,39.0272482006204,39.110846034206,
39.194577597081,39.2744114354073,39.358158168105,39.4418018451164,39.5253625891787,
39.6088604511311,39.6923229516894,39.7757680871773,39.8592139220161,39.9426785172497,
40.0262317026673,40.1098295362355,40.1935610990931,40.2733949376064,40.3591926183833,
40.4448691100682,40.5304395102994,40.6158946374186,40.7012820751929,40.7866066094072,
40.8407044966691),.UNSPECIFIED.);
#411=B_SPLINE_CURVE_WITH_KNOTS('',3,(#46010,#46011,#46012,#46013,#46014,
#46015,#46016,#46017,#46018,#46019,#46020,#46021,#46022,#46023,#46024,#46025,
#46026,#46027,#46028,#46029,#46030,#46031,#46032,#46033,#46034,#46035,#46036,
#46037,#46038,#46039,#46040,#46041,#46042,#46043,#46044,#46045,#46046,#46047,
#46048,#46049,#46050,#46051,#46052,#46053,#46054,#46055,#46056,#46057,#46058,
#46059,#46060,#46061,#46062,#46063,#46064,#46065,#46066,#46067,#46068,#46069,
#46070,#46071,#46072,#46073,#46074,#46075,#46076,#46077,#46078,#46079,#46080,
#46081,#46082,#46083,#46084,#46085,#46086,#46087,#46088,#46089,#46090,#46091,
#46092,#46093,#46094,#46095,#46096,#46097,#46098,#46099,#46100,#46101,#46102,
#46103,#46104,#46105,#46106,#46107,#46108,#46109,#46110,#46111,#46112,#46113,
#46114,#46115,#46116,#46117,#46118,#46119,#46120,#46121,#46122,#46123,#46124,
#46125,#46126,#46127,#46128,#46129,#46130,#46131,#46132,#46133,#46134,#46135,
#46136,#46137,#46138,#46139,#46140,#46141,#46142,#46143,#46144,#46145,#46146,
#46147,#46148,#46149,#46150,#46151,#46152,#46153,#46154,#46155,#46156,#46157,
#46158,#46159,#46160,#46161,#46162,#46163,#46164,#46165,#46166,#46167,#46168,
#46169,#46170,#46171,#46172,#46173,#46174,#46175,#46176,#46177,#46178,#46179,
#46180,#46181,#46182,#46183,#46184,#46185,#46186,#46187,#46188,#46189,#46190,
#46191,#46192,#46193,#46194,#46195,#46196,#46197,#46198,#46199,#46200,#46201,
#46202,#46203,#46204,#46205,#46206,#46207,#46208,#46209,#46210,#46211,#46212,
#46213,#46214,#46215,#46216,#46217,#46218,#46219,#46220,#46221,#46222,#46223,
#46224,#46225,#46226,#46227,#46228,#46229,#46230,#46231,#46232,#46233,#46234,
#46235,#46236,#46237,#46238),.UNSPECIFIED.,.F.,.F.,(4,3,3,3,3,3,3,3,3,3,
3,3,3,3,3,3,3,3,3,3,3,3,3,3,3,3,3,3,3,3,3,3,3,3,3,3,3,3,3,3,3,3,3,3,3,3,
3,3,3,3,3,3,3,3,3,3,3,3,3,3,3,3,3,3,3,3,3,3,3,3,3,3,3,3,3,3,4),(28.2743338823098,
28.2855929112165,28.3693396385187,28.4529833100496,28.5365440485524,28.6200419048725,
28.703504399708,28.7869495294187,28.8703953584308,28.9538599477941,29.0374131273048,
29.1210109549371,29.2047425118682,29.2845764134156,29.3683231497121,29.4519668303631,
29.5355275781013,29.6190254437621,29.7024879480652,29.7859330873194,29.8693789259423,
29.952843524975,30.0363967141929,30.1199945515685,30.2037261182066,30.2835599156148,
30.3673066477708,30.4509503242413,30.5345110677637,30.6180089291779,30.7014714292028,
30.7849165641603,30.8683623984718,30.9518269931825,31.0353801780864,31.1189780111453,
31.202709573506,31.282543417814,31.3662901498208,31.4499338261296,31.5334945694783,
31.616992430707,31.7004549305288,31.7839000652725,31.8673458993597,31.9508104938358,
32.0343636784899,32.1179615112904,32.2016930733804,32.2815269200131,32.3652736532667,
32.4489173308407,32.5324780754713,32.6159759379975,32.6994384391356,32.7828835752069,
32.866329410632,32.9497940064547,33.0333471924619,33.1169450266212,33.2006765900661,
33.2805104222123,33.364257154793,33.4479008316872,33.5314615756317,33.614959437466,
33.6984219379065,33.7818670732767,33.8653129079977,33.9487775031143,34.0323306884159,
34.1159285218687,34.1996600846128,34.2794939244115,34.384509295408,34.4879029932419,
34.5575191893829),.UNSPECIFIED.);
#412=B_SPLINE_CURVE_WITH_KNOTS('',3,(#46240,#46241,#46242,#46243,#46244,
#46245,#46246,#46247,#46248,#46249,#46250,#46251,#46252,#46253,#46254,#46255,
#46256,#46257,#46258,#46259,#46260,#46261,#46262,#46263,#46264,#46265,#46266,
#46267,#46268,#46269,#46270,#46271,#46272,#46273,#46274,#46275,#46276,#46277,
#46278,#46279,#46280,#46281,#46282,#46283,#46284,#46285,#46286,#46287,#46288,
#46289,#46290,#46291,#46292,#46293,#46294,#46295,#46296,#46297,#46298,#46299,
#46300,#46301,#46302,#46303,#46304,#46305,#46306,#46307,#46308,#46309,#46310,
#46311,#46312,#46313,#46314,#46315,#46316,#46317,#46318,#46319,#46320,#46321,
#46322,#46323,#46324,#46325,#46326,#46327,#46328,#46329,#46330,#46331,#46332,
#46333,#46334,#46335,#46336,#46337,#46338,#46339,#46340,#46341,#46342,#46343,
#46344,#46345,#46346,#46347,#46348,#46349,#46350,#46351,#46352,#46353,#46354,
#46355,#46356,#46357,#46358,#46359,#46360,#46361,#46362,#46363,#46364,#46365,
#46366,#46367,#46368,#46369,#46370,#46371,#46372,#46373,#46374,#46375,#46376,
#46377,#46378,#46379,#46380,#46381,#46382,#46383,#46384,#46385,#46386,#46387,
#46388,#46389,#46390,#46391,#46392,#46393,#46394,#46395,#46396,#46397,#46398,
#46399,#46400,#46401,#46402,#46403,#46404,#46405,#46406,#46407,#46408,#46409,
#46410,#46411,#46412,#46413,#46414,#46415,#46416,#46417,#46418,#46419,#46420,
#46421,#46422,#46423,#46424,#46425,#46426,#46427,#46428,#46429,#46430,#46431,
#46432,#46433,#46434,#46435,#46436,#46437,#46438,#46439,#46440,#46441,#46442,
#46443,#46444,#46445,#46446,#46447,#46448,#46449,#46450,#46451,#46452,#46453,
#46454,#46455,#46456,#46457,#46458,#46459,#46460,#46461,#46462,#46463,#46464,
#46465),.UNSPECIFIED.,.F.,.F.,(4,3,3,3,3,3,3,3,3,3,3,3,3,3,3,3,3,3,3,3,
3,3,3,3,3,3,3,3,3,3,3,3,3,3,3,3,3,3,3,3,3,3,3,3,3,3,3,3,3,3,3,3,3,3,3,3,
3,3,3,3,3,3,3,3,3,3,3,3,3,3,3,3,3,3,3,4),(21.9911485752772,22.0915967946116,
22.1933535952714,22.2916918980215,22.3754383367532,22.4590817156296,22.5426421577285,
22.6261397142248,22.7096019050848,22.7930467283347,22.8764922486856,22.9599565274714,
23.0435093951123,23.1271069096784,23.2108381546484,23.2906754002206,23.3744222749988,
23.4580660955009,23.5416269843023,23.6251249920827,23.7085876396076,23.7920329227343,
23.875478905744,23.9589436495423,24.0424969833073,24.1260949653393,24.2098266753587,
24.2896589024198,24.3734056361377,24.4570493145306,24.5406100603324,24.62410792438,
24.7075704275707,24.7910155660182,24.874461404142,24.9579260029855,25.0414791925099,
25.1250770304622,25.2088085981372,25.288642404619,25.3723890968892,25.4560327328708,
25.5395934353476,25.6230912552054,25.7065537130417,25.7899988054317,25.8734445968363,
25.9569091483397,26.040462289803,26.1240600792255,26.2077915980539,26.2876259068181,
26.3713726624105,26.4550163625608,26.5385771299799,26.6220750154812,26.7055375397974,
26.7889826991669,26.8724285579882,26.9558931772836,27.0394463867519,27.1230442444029,
27.2067758311547,27.2866094090173,27.3701908686011,27.4536693631837,27.5370651913173,
27.6203985782601,27.7036973121344,27.7869793990543,27.87026305976,27.9535665122895,
28.0369584520835,28.1203962706263,28.2039646002913,28.2743338822021),
 .UNSPECIFIED.);
#413=B_SPLINE_CURVE_WITH_KNOTS('',3,(#46467,#46468,#46469,#46470,#46471,
#46472,#46473,#46474,#46475,#46476,#46477,#46478,#46479,#46480,#46481,#46482,
#46483,#46484,#46485,#46486,#46487,#46488,#46489,#46490,#46491,#46492,#46493,
#46494,#46495,#46496,#46497,#46498,#46499,#46500,#46501,#46502,#46503,#46504,
#46505,#46506,#46507,#46508,#46509,#46510,#46511,#46512,#46513,#46514,#46515,
#46516,#46517,#46518,#46519,#46520,#46521,#46522,#46523,#46524,#46525,#46526,
#46527,#46528,#46529,#46530,#46531,#46532,#46533,#46534,#46535,#46536,#46537,
#46538,#46539,#46540,#46541,#46542,#46543,#46544,#46545,#46546,#46547,#46548,
#46549,#46550,#46551,#46552,#46553,#46554,#46555,#46556,#46557,#46558,#46559,
#46560,#46561,#46562,#46563,#46564,#46565,#46566,#46567,#46568,#46569,#46570,
#46571,#46572,#46573,#46574,#46575,#46576,#46577,#46578,#46579,#46580,#46581,
#46582,#46583,#46584,#46585,#46586,#46587,#46588,#46589,#46590,#46591,#46592,
#46593,#46594,#46595,#46596,#46597,#46598,#46599,#46600,#46601,#46602,#46603,
#46604,#46605,#46606,#46607,#46608,#46609,#46610,#46611,#46612,#46613,#46614,
#46615,#46616,#46617,#46618,#46619,#46620,#46621,#46622,#46623,#46624,#46625,
#46626,#46627,#46628,#46629,#46630,#46631,#46632,#46633,#46634,#46635,#46636,
#46637,#46638,#46639,#46640,#46641,#46642,#46643,#46644,#46645,#46646,#46647,
#46648,#46649,#46650,#46651,#46652,#46653,#46654,#46655,#46656,#46657,#46658,
#46659,#46660,#46661,#46662,#46663,#46664,#46665,#46666,#46667,#46668,#46669,
#46670,#46671,#46672,#46673,#46674,#46675,#46676,#46677,#46678,#46679,#46680,
#46681,#46682,#46683,#46684,#46685,#46686,#46687,#46688,#46689,#46690,#46691,
#46692,#46693,#46694,#46695),.UNSPECIFIED.,.F.,.F.,(4,3,3,3,3,3,3,3,3,3,
3,3,3,3,3,3,3,3,3,3,3,3,3,3,3,3,3,3,3,3,3,3,3,3,3,3,3,3,3,3,3,3,3,3,3,3,
3,3,3,3,3,3,3,3,3,3,3,3,3,3,3,3,3,3,3,3,3,3,3,3,3,3,3,3,3,3,4),(15.7079632679507,
15.7927756596227,15.8776170867123,15.9625034608706,16.0475130802455,16.132586075745,
16.2178171971746,16.2977908848265,16.3815231744717,16.4651522214982,16.5486981652632,
16.6321810729477,16.7156284375635,16.7990583285799,16.8824888246189,16.9659380008729,
17.0494757269557,17.1330580547515,17.2167741886622,17.2967743870256,17.3805260802118,
17.4641747567812,17.5477405338708,17.6312434567916,17.7147110427228,17.7981612776924,
17.8816122212571,17.9650819296005,18.0486402060587,18.1322431266918,18.2159797182806,
18.2957578892248,18.3795058313357,18.4631507479379,18.5467127602997,18.6302119178264,
18.713675751041,18.7971222415942,18.8805694526949,18.9640354441891,19.0475900498296,
19.1311893189108,19.2149223291237,19.294741391424,19.3784860398764,19.462127604408,
19.5456862101661,19.6291819103589,19.7126422210736,19.7960851499237,19.8795287633862,
19.9629911245534,20.0465420683562,20.130137652657,20.2138669758113,20.2937248936231,
20.3774724818822,20.4611170221827,20.5446786362914,20.6281773740904,20.7116407561995,
20.7950867765832,20.8785334988228,20.9619989831243,21.0455530552162,21.1291517755569,
21.2128842163817,21.2927083958223,21.3800134182358,21.4631567532187,21.5462227252512,
21.6292299062174,21.7121968214489,21.7951548997181,21.8781081024208,21.9610957726353,
21.9911485751302),.UNSPECIFIED.);
#414=B_SPLINE_CURVE_WITH_KNOTS('',3,(#46697,#46698,#46699,#46700,#46701,
#46702,#46703,#46704,#46705,#46706,#46707,#46708,#46709,#46710,#46711,#46712,
#46713,#46714,#46715,#46716,#46717,#46718,#46719,#46720,#46721,#46722,#46723,
#46724,#46725,#46726,#46727,#46728,#46729,#46730,#46731,#46732,#46733,#46734,
#46735,#46736,#46737,#46738,#46739,#46740,#46741,#46742,#46743,#46744,#46745,
#46746,#46747,#46748,#46749,#46750,#46751,#46752,#46753,#46754,#46755,#46756,
#46757,#46758,#46759,#46760,#46761,#46762,#46763,#46764,#46765,#46766,#46767,
#46768,#46769,#46770,#46771,#46772,#46773,#46774,#46775,#46776,#46777,#46778,
#46779,#46780,#46781,#46782,#46783,#46784,#46785,#46786,#46787,#46788,#46789,
#46790,#46791,#46792,#46793,#46794,#46795,#46796,#46797,#46798,#46799,#46800,
#46801,#46802,#46803,#46804,#46805,#46806,#46807,#46808,#46809,#46810,#46811,
#46812,#46813,#46814,#46815,#46816,#46817,#46818,#46819,#46820,#46821,#46822,
#46823,#46824,#46825,#46826,#46827,#46828,#46829,#46830,#46831,#46832,#46833,
#46834,#46835,#46836,#46837,#46838,#46839,#46840,#46841,#46842,#46843,#46844,
#46845,#46846,#46847,#46848,#46849,#46850,#46851,#46852,#46853,#46854,#46855,
#46856,#46857,#46858,#46859,#46860,#46861,#46862,#46863,#46864,#46865,#46866,
#46867,#46868,#46869,#46870,#46871,#46872,#46873,#46874,#46875,#46876,#46877,
#46878,#46879,#46880,#46881,#46882,#46883,#46884,#46885,#46886,#46887,#46888,
#46889,#46890,#46891,#46892),.UNSPECIFIED.,.F.,.F.,(4,3,3,3,3,3,3,3,3,3,
3,3,3,3,3,3,3,3,3,3,3,3,3,3,3,3,3,3,3,3,3,3,3,3,3,3,3,3,3,3,3,3,3,3,3,3,
3,3,3,3,3,3,3,3,3,3,3,3,3,3,3,3,3,3,3,4),(10.3765404525762,10.4587521152597,
10.5408614862217,10.6228899520007,10.7078878797294,10.7898262304058,10.8717530949992,
10.9536876277784,11.0356489885776,11.1177007597849,11.1998064288948,11.2820288092828,
11.3028733738307,11.3867642798309,11.4705527050716,11.5542586078086,11.637901875852,
11.7215096228114,11.8050998805076,11.8886905683685,11.9722996021914,12.0559957390186,
12.1397359346823,12.2236074081934,12.3018568760298,12.3857069936252,12.4694559766231,
12.5531238230789,12.6367304615285,12.7203039013286,12.8038612763562,12.8874205458847,
12.9709996665433,13.0546684603941,13.1383826733204,13.2222307644838,13.300840378229,
13.3844892187341,13.4680338034875,13.5514943658934,13.6348910655576,13.7182512639974,
13.8015934160834,13.8849356807694,13.9682962133096,14.0517451381917,14.1352384369971,
14.2188660501523,14.2998238804282,14.3835979510481,14.4672691368914,14.5508575299305,
14.6343831505939,14.7178734767581,14.8013464742856,14.8848201807277,14.9683126302487,
15.0518934838678,15.1355189278689,15.2192777222846,15.2988073826273,15.3913678981619,
15.4835597219632,15.575511367992,15.6670851757684,15.7079632677804),
 .UNSPECIFIED.);
#415=B_SPLINE_CURVE_WITH_KNOTS('',3,(#46896,#46897,#46898,#46899,#46900,
#46901,#46902,#46903,#46904,#46905,#46906,#46907,#46908,#46909,#46910,#46911,
#46912,#46913,#46914,#46915,#46916,#46917,#46918,#46919,#46920,#46921,#46922,
#46923,#46924,#46925,#46926,#46927,#46928,#46929,#46930,#46931,#46932,#46933,
#46934,#46935,#46936,#46937,#46938,#46939,#46940,#46941,#46942,#46943,#46944,
#46945,#46946,#46947,#46948,#46949,#46950,#46951,#46952,#46953,#46954,#46955,
#46956,#46957,#46958,#46959,#46960,#46961,#46962,#46963,#46964,#46965,#46966,
#46967,#46968,#46969,#46970,#46971,#46972,#46973,#46974,#46975,#46976,#46977,
#46978,#46979,#46980,#46981,#46982,#46983,#46984,#46985,#46986,#46987,#46988,
#46989,#46990,#46991,#46992,#46993,#46994,#46995,#46996,#46997,#46998,#46999,
#47000,#47001,#47002,#47003,#47004,#47005,#47006,#47007,#47008,#47009,#47010,
#47011,#47012,#47013,#47014,#47015,#47016,#47017,#47018,#47019,#47020,#47021,
#47022,#47023,#47024,#47025,#47026,#47027,#47028,#47029,#47030,#47031,#47032,
#47033,#47034,#47035,#47036,#47037,#47038,#47039,#47040),.UNSPECIFIED.,
 .F.,.F.,(4,3,3,3,3,3,3,3,3,3,3,3,3,3,3,3,3,3,3,3,3,3,3,3,3,3,3,3,3,3,3,
3,3,3,3,3,3,3,3,3,3,3,3,3,3,3,3,3,4),(11.6154215191127,11.7134108796421,
11.8137864772846,11.9119452646907,12.0134292674513,12.114913270212,12.1986643687573,
12.2824048936106,12.3661873966993,12.4499889517511,12.5338813874082,12.6144050213115,
12.6992193089131,12.7839581468896,12.8686399159733,12.9532829477551,13.0379222058963,
13.1225629256859,13.2072216877147,13.2919150812395,13.3767142872945,13.4615693245244,
13.5465638834944,13.6133885235107,13.6964430640987,13.7793864236487,13.8622394401368,
13.9450228616774,14.0284415071814,14.1111594185092,14.1938739986228,14.2766039053567,
14.360545935445,14.4434061340962,14.5278890799031,14.6123720257099,14.6962629317101,
14.7800513569509,14.8637572596879,14.9474005277315,15.031008274691,15.1145985323872,
15.1981892202482,15.281798254071,15.3654943908983,15.4492345865619,15.5331060600731,
15.611355527909,15.7079632679504),.UNSPECIFIED.);
#416=B_SPLINE_CURVE_WITH_KNOTS('',3,(#47042,#47043,#47044,#47045,#47046,
#47047,#47048,#47049,#47050,#47051,#47052,#47053,#47054,#47055,#47056,#47057,
#47058,#47059,#47060,#47061,#47062,#47063,#47064,#47065,#47066,#47067,#47068,
#47069,#47070,#47071,#47072,#47073,#47074,#47075,#47076,#47077,#47078,#47079,
#47080,#47081,#47082,#47083,#47084,#47085,#47086,#47087,#47088,#47089,#47090,
#47091,#47092,#47093,#47094,#47095,#47096,#47097,#47098,#47099,#47100,#47101,
#47102,#47103,#47104,#47105,#47106,#47107,#47108,#47109,#47110,#47111,#47112,
#47113,#47114,#47115,#47116,#47117,#47118,#47119,#47120,#47121,#47122,#47123,
#47124,#47125,#47126,#47127,#47128,#47129,#47130,#47131,#47132,#47133,#47134,
#47135,#47136,#47137,#47138,#47139,#47140,#47141,#47142,#47143,#47144,#47145,
#47146,#47147,#47148,#47149,#47150,#47151,#47152,#47153,#47154,#47155,#47156,
#47157,#47158,#47159,#47160,#47161,#47162,#47163,#47164,#47165,#47166,#47167,
#47168,#47169,#47170,#47171,#47172,#47173,#47174,#47175,#47176,#47177,#47178,
#47179,#47180,#47181,#47182,#47183,#47184,#47185,#47186,#47187,#47188,#47189,
#47190,#47191,#47192,#47193,#47194,#47195,#47196,#47197,#47198,#47199,#47200,
#47201,#47202,#47203,#47204,#47205,#47206,#47207,#47208,#47209,#47210,#47211,
#47212,#47213,#47214,#47215,#47216,#47217,#47218,#47219,#47220,#47221,#47222,
#47223,#47224,#47225,#47226,#47227,#47228,#47229,#47230,#47231,#47232,#47233,
#47234,#47235,#47236,#47237,#47238,#47239,#47240,#47241,#47242,#47243,#47244,
#47245,#47246,#47247,#47248,#47249,#47250,#47251,#47252,#47253,#47254,#47255,
#47256,#47257,#47258,#47259,#47260,#47261,#47262,#47263,#47264,#47265,#47266,
#47267,#47268,#47269,#47270),.UNSPECIFIED.,.F.,.F.,(4,3,3,3,3,3,3,3,3,3,
3,3,3,3,3,3,3,3,3,3,3,3,3,3,3,3,3,3,3,3,3,3,3,3,3,3,3,3,3,3,3,3,3,3,3,3,
3,3,3,3,3,3,3,3,3,3,3,3,3,3,3,3,3,3,3,3,3,3,3,3,3,3,3,3,3,3,4),(15.7079632680755,
15.7907619926379,15.8734692466063,15.9561059540638,16.0386978979543,16.1212670757871,
16.2038323011308,16.2864123817455,16.3690765141303,16.4517831983492,16.5346204612354,
16.6103390301082,16.6939878706133,16.7775324553667,16.8609930177726,16.9443897174368,
17.0277499158766,17.1110920679627,17.1944343326486,17.2777948651888,17.3612437900709,
17.4447370888762,17.5283647020315,17.6093225323074,17.6930966029273,17.7767677887705,
17.8603561818097,17.9438818024728,18.0273721286368,18.1108451261642,18.1943188326061,
18.2778112821271,18.3613921357462,18.4450175797472,18.5287763741629,18.6083060345065,
18.6920646129743,18.7757203799082,18.8592934438872,18.9428038418974,19.026279164037,
19.1097372932472,19.1931962821169,19.2766741799582,19.3602408292934,19.4438522358629,
19.5275974224496,19.6072895367057,19.6910218263509,19.7746508733775,19.8581968171425,
19.9416797248271,20.0251270894429,20.1085569804594,20.1919874764985,20.2754366527522,
20.3589743788349,20.4425567066307,20.5262728405414,20.6062730389049,20.6900247320912,
20.7736734086611,20.8572391857509,20.940742108672,21.0242096946032,21.1076599295729,
21.1911108731376,21.2745805814815,21.3581388579396,21.4417417785728,21.5254783701617,
21.605256541104,21.7017295495635,21.7954328009705,21.8932906879561,21.9862257175956,
21.9911485749418),.UNSPECIFIED.);
#417=B_SPLINE_CURVE_WITH_KNOTS('',3,(#47272,#47273,#47274,#47275,#47276,
#47277,#47278,#47279,#47280,#47281,#47282,#47283,#47284,#47285,#47286,#47287,
#47288,#47289,#47290,#47291,#47292,#47293,#47294,#47295,#47296,#47297,#47298,
#47299,#47300,#47301,#47302,#47303,#47304,#47305,#47306,#47307,#47308,#47309,
#47310,#47311,#47312,#47313,#47314,#47315,#47316,#47317,#47318,#47319,#47320,
#47321,#47322,#47323,#47324,#47325,#47326,#47327,#47328,#47329,#47330,#47331,
#47332,#47333,#47334,#47335,#47336,#47337,#47338,#47339,#47340,#47341,#47342,
#47343,#47344,#47345,#47346,#47347,#47348,#47349,#47350,#47351,#47352,#47353,
#47354,#47355,#47356,#47357,#47358,#47359,#47360,#47361,#47362,#47363,#47364,
#47365,#47366,#47367,#47368,#47369,#47370,#47371,#47372,#47373,#47374,#47375,
#47376,#47377,#47378,#47379,#47380,#47381,#47382,#47383,#47384,#47385,#47386,
#47387,#47388,#47389,#47390,#47391,#47392,#47393,#47394,#47395,#47396,#47397,
#47398,#47399,#47400,#47401,#47402,#47403,#47404,#47405,#47406,#47407,#47408,
#47409,#47410,#47411,#47412,#47413,#47414,#47415,#47416,#47417,#47418,#47419,
#47420,#47421,#47422,#47423,#47424,#47425,#47426,#47427,#47428,#47429,#47430,
#47431,#47432,#47433,#47434,#47435,#47436,#47437,#47438,#47439,#47440,#47441,
#47442,#47443,#47444,#47445,#47446,#47447,#47448,#47449,#47450,#47451,#47452,
#47453,#47454,#47455,#47456,#47457,#47458,#47459,#47460,#47461,#47462,#47463,
#47464,#47465,#47466,#47467,#47468,#47469,#47470,#47471,#47472,#47473,#47474,
#47475,#47476,#47477,#47478,#47479,#47480,#47481,#47482,#47483,#47484,#47485,
#47486,#47487,#47488,#47489,#47490,#47491,#47492,#47493,#47494,#47495,#47496,
#47497,#47498,#47499,#47500),.UNSPECIFIED.,.F.,.F.,(4,3,3,3,3,3,3,3,3,3,
3,3,3,3,3,3,3,3,3,3,3,3,3,3,3,3,3,3,3,3,3,3,3,3,3,3,3,3,3,3,3,3,3,3,3,3,
3,3,3,3,3,3,3,3,3,3,3,3,3,3,3,3,3,3,3,3,3,3,3,3,3,3,3,3,3,3,4),(21.99114857513,
22.0754397887712,22.1597448263936,22.2440805180614,22.3284637106311,22.4129619403789,
22.4975279040286,22.5822259836788,22.6042400433032,22.6879846917557,22.7716262562874,
22.8551848620454,22.9386805622383,23.0221408729532,23.1055838018032,23.1890274152657,
23.272489776433,23.3560407202358,23.4396363045367,23.523365627691,23.6032235455024,
23.6869711337616,23.7706156740621,23.854177288171,23.9376760259705,24.0211394080798,
24.1045854284634,24.1880321507029,24.2714976350044,24.3550517070964,24.4386504274371,
24.5223828682619,24.6022070477015,24.6859538746302,24.7695976493655,24.8531584945246,
24.9366564608302,25.020119070352,25.1035643175979,25.1870102668931,25.270474979188,
25.3540282851558,25.4376262413643,25.5213579292257,25.6011905499007,25.6849369886324,
25.7685803675088,25.8521408096079,25.935638366104,26.0191005569639,26.1025453802136,
26.1859909005645,26.2694551793504,26.3530080469912,26.4366055615576,26.5203368065275,
26.6001740520998,26.6839209268779,26.7675647473803,26.8511256361815,26.9346236439619,
27.0180862914868,27.1015315746134,27.1849775576231,27.268442301421,27.3519956351859,
27.4355936172179,27.5193253272373,27.599157554299,27.6835545953003,27.7670084084085,
27.8503813813075,27.9336918132199,28.0188523304923,28.102100334802,28.1882171085557,
28.2743338823095),.UNSPECIFIED.);
#418=B_SPLINE_CURVE_WITH_KNOTS('',3,(#47502,#47503,#47504,#47505,#47506,
#47507,#47508,#47509,#47510,#47511,#47512,#47513,#47514,#47515,#47516,#47517,
#47518,#47519,#47520,#47521,#47522,#47523,#47524,#47525,#47526,#47527,#47528,
#47529,#47530,#47531,#47532,#47533,#47534,#47535,#47536,#47537,#47538,#47539,
#47540,#47541,#47542,#47543,#47544,#47545,#47546,#47547,#47548,#47549,#47550,
#47551,#47552,#47553,#47554,#47555,#47556,#47557,#47558,#47559,#47560,#47561,
#47562,#47563,#47564,#47565,#47566,#47567,#47568,#47569,#47570,#47571,#47572,
#47573,#47574,#47575,#47576,#47577,#47578,#47579,#47580,#47581,#47582,#47583,
#47584,#47585,#47586,#47587,#47588,#47589,#47590,#47591,#47592,#47593,#47594,
#47595,#47596,#47597,#47598,#47599,#47600,#47601,#47602,#47603,#47604,#47605,
#47606,#47607,#47608,#47609,#47610,#47611,#47612,#47613,#47614,#47615,#47616,
#47617,#47618,#47619,#47620,#47621,#47622,#47623,#47624,#47625,#47626,#47627,
#47628,#47629,#47630,#47631,#47632,#47633,#47634,#47635,#47636,#47637,#47638,
#47639,#47640,#47641,#47642,#47643,#47644,#47645,#47646,#47647,#47648,#47649,
#47650,#47651,#47652,#47653,#47654,#47655,#47656,#47657,#47658,#47659,#47660,
#47661,#47662,#47663,#47664,#47665,#47666,#47667,#47668,#47669,#47670,#47671,
#47672,#47673,#47674,#47675,#47676,#47677,#47678,#47679,#47680,#47681,#47682,
#47683,#47684,#47685,#47686,#47687,#47688,#47689,#47690,#47691,#47692,#47693,
#47694,#47695,#47696,#47697,#47698,#47699,#47700,#47701,#47702,#47703,#47704,
#47705,#47706,#47707,#47708,#47709,#47710,#47711,#47712,#47713,#47714,#47715,
#47716,#47717,#47718,#47719,#47720,#47721,#47722,#47723,#47724,#47725,#47726,
#47727,#47728,#47729,#47730),.UNSPECIFIED.,.F.,.F.,(4,3,3,3,3,3,3,3,3,3,
3,3,3,3,3,3,3,3,3,3,3,3,3,3,3,3,3,3,3,3,3,3,3,3,3,3,3,3,3,3,3,3,3,3,3,3,
3,3,3,3,3,3,3,3,3,3,3,3,3,3,3,3,3,3,3,3,3,3,3,3,3,3,3,3,3,3,4),(28.2743338824874,
28.3724085420325,28.4711275974312,28.570569651084,28.5981410564982,28.6818877487685,
28.76553138475,28.8490920872268,28.9325899070845,29.016052364921,29.0994974573111,
29.1829432487156,29.2664078002192,29.3499609416825,29.433558731105,29.5172902499334,
29.5971245586973,29.6808713142898,29.7645150144402,29.8480757818592,29.9315736673606,
30.0150361916768,30.0984813510464,30.1819272098678,30.2653918291633,30.3489450386316,
30.4325428962827,30.5162744830346,30.5961080608965,30.679854791818,30.7634984670824,
30.8470592094284,30.9305570696972,31.0140195686282,31.0974647025234,31.1809105358054,
31.2643751295205,31.3479283134885,31.4315261456426,31.5152577071613,31.5950915630957,
31.6788382903979,31.7624819619288,31.8460427004316,31.9295405567519,32.0130030515874,
32.096448181298,32.1798940103101,32.2633585996735,32.3469117791842,32.4305096068163,
32.5142411637475,32.5940750652948,32.6778218015912,32.7614654822422,32.8450262299803,
32.9285240956412,33.0119865999442,33.0954317391984,33.1788775778212,33.2623421768537,
33.3458953660716,33.4294932034471,33.5132247700852,33.593058567494,33.6763378052535,
33.759514298541,33.8426086416793,33.925641352111,34.0086404852872,34.0916242022808,
34.1746109848179,34.2576193132337,34.3407149954989,34.4238586705803,34.5071251979438,
34.55751918934),.UNSPECIFIED.);
#419=B_SPLINE_CURVE_WITH_KNOTS('',3,(#47732,#47733,#47734,#47735,#47736,
#47737,#47738,#47739,#47740,#47741,#47742,#47743,#47744,#47745,#47746,#47747,
#47748,#47749,#47750,#47751,#47752,#47753,#47754,#47755,#47756,#47757,#47758,
#47759,#47760,#47761,#47762,#47763,#47764,#47765,#47766,#47767,#47768,#47769,
#47770,#47771,#47772,#47773,#47774,#47775,#47776,#47777,#47778,#47779,#47780,
#47781,#47782,#47783,#47784,#47785,#47786,#47787,#47788,#47789,#47790,#47791,
#47792,#47793,#47794,#47795,#47796,#47797,#47798,#47799,#47800,#47801,#47802,
#47803,#47804,#47805,#47806,#47807,#47808,#47809,#47810,#47811,#47812,#47813,
#47814,#47815,#47816,#47817,#47818,#47819,#47820,#47821,#47822,#47823,#47824,
#47825,#47826,#47827,#47828,#47829,#47830,#47831,#47832,#47833,#47834,#47835,
#47836,#47837,#47838,#47839,#47840,#47841,#47842,#47843,#47844,#47845,#47846,
#47847,#47848,#47849,#47850,#47851,#47852,#47853,#47854,#47855,#47856,#47857,
#47858,#47859,#47860,#47861,#47862,#47863,#47864,#47865,#47866,#47867,#47868,
#47869,#47870,#47871,#47872,#47873,#47874,#47875,#47876,#47877,#47878,#47879,
#47880,#47881,#47882,#47883,#47884,#47885,#47886,#47887,#47888,#47889,#47890,
#47891,#47892,#47893,#47894,#47895,#47896,#47897,#47898,#47899,#47900,#47901,
#47902,#47903,#47904,#47905,#47906,#47907,#47908,#47909,#47910,#47911,#47912,
#47913,#47914,#47915,#47916,#47917,#47918,#47919,#47920,#47921,#47922,#47923,
#47924,#47925,#47926,#47927,#47928,#47929,#47930,#47931,#47932,#47933,#47934,
#47935,#47936,#47937,#47938,#47939,#47940,#47941,#47942,#47943,#47944,#47945,
#47946,#47947,#47948,#47949,#47950,#47951,#47952,#47953,#47954,#47955,#47956,
#47957,#47958,#47959,#47960),.UNSPECIFIED.,.F.,.F.,(4,3,3,3,3,3,3,3,3,3,
3,3,3,3,3,3,3,3,3,3,3,3,3,3,3,3,3,3,3,3,3,3,3,3,3,3,3,3,3,3,3,3,3,3,3,3,
3,3,3,3,3,3,3,3,3,3,3,3,3,3,3,3,3,3,3,3,3,3,3,3,3,3,3,3,3,3,4),(34.5575191894891,
34.5920420696932,34.6757888017,34.7594324780089,34.8429932213576,34.9264910825864,
35.0099535824083,35.093398717152,35.1768445512393,35.2603091457156,35.3438623303698,
35.4274601631704,35.5111917252604,35.5910255718923,35.6747723051459,35.7584159827199,
35.8419767273506,35.9254745898766,36.0089370910147,36.0923822270861,36.175828062511,
36.2592926583338,36.342845844341,36.4264436785003,36.5101752419451,36.5900090740915,
36.6737558066723,36.7573994835664,36.840960227511,36.9244580893454,37.0079205897859,
37.0913657251563,37.1748115598773,37.258276154994,37.3418293402957,37.4254271737486,
37.5091587364928,37.5889925762907,37.6727393089074,37.7563829858364,37.8399437298146,
37.9234415916816,38.0069040921527,38.0903492275525,38.1737950623018,38.2572596574455,
38.340812842772,38.4244106762487,38.5081422390145,38.5879760784898,38.6717228112747,
38.7553664883743,38.8389272325257,38.922425094568,39.0058875952173,39.0893327307968,
39.1727785657275,39.2562431610538,39.339796346564,39.4233941802252,39.5071257431751,
39.586959580689,39.6707063133674,39.7543499903594,39.8379107344021,39.9214085963348,
40.0048710968733,40.0883162323415,40.1717620671603,40.2552266623743,40.3387798477722,
40.4223776813209,40.5061092441592,40.5859430828882,40.6947718105575,40.8013950654125,
40.8407044965583),.UNSPECIFIED.);
#420=B_SPLINE_CURVE_WITH_KNOTS('',3,(#47962,#47963,#47964,#47965,#47966,
#47967,#47968,#47969,#47970,#47971,#47972,#47973,#47974,#47975,#47976,#47977,
#47978,#47979,#47980,#47981,#47982,#47983,#47984,#47985,#47986,#47987,#47988,
#47989,#47990,#47991,#47992,#47993,#47994,#47995,#47996,#47997,#47998,#47999,
#48000,#48001,#48002,#48003,#48004,#48005,#48006,#48007,#48008,#48009,#48010,
#48011,#48012,#48013,#48014,#48015,#48016,#48017,#48018,#48019,#48020,#48021,
#48022,#48023,#48024,#48025,#48026,#48027,#48028,#48029,#48030,#48031,#48032,
#48033,#48034,#48035,#48036,#48037,#48038,#48039,#48040,#48041,#48042,#48043,
#48044,#48045,#48046,#48047,#48048,#48049,#48050,#48051,#48052,#48053,#48054,
#48055,#48056,#48057,#48058,#48059,#48060,#48061,#48062,#48063,#48064,#48065,
#48066,#48067,#48068,#48069,#48070,#48071,#48072,#48073,#48074,#48075,#48076,
#48077,#48078,#48079,#48080,#48081,#48082,#48083,#48084,#48085,#48086,#48087,
#48088,#48089,#48090,#48091,#48092,#48093,#48094,#48095,#48096,#48097,#48098,
#48099,#48100,#48101,#48102,#48103,#48104,#48105,#48106,#48107,#48108,#48109,
#48110,#48111,#48112,#48113,#48114,#48115,#48116,#48117,#48118,#48119,#48120,
#48121,#48122,#48123,#48124,#48125,#48126,#48127,#48128,#48129,#48130,#48131,
#48132,#48133,#48134,#48135,#48136,#48137,#48138,#48139,#48140,#48141,#48142,
#48143,#48144,#48145,#48146,#48147,#48148,#48149,#48150,#48151,#48152,#48153,
#48154,#48155,#48156,#48157,#48158,#48159,#48160,#48161,#48162,#48163,#48164,
#48165,#48166,#48167,#48168,#48169,#48170,#48171,#48172,#48173,#48174,#48175,
#48176,#48177,#48178,#48179,#48180,#48181,#48182,#48183,#48184,#48185,#48186,
#48187,#48188,#48189,#48190),.UNSPECIFIED.,.F.,.F.,(4,3,3,3,3,3,3,3,3,3,
3,3,3,3,3,3,3,3,3,3,3,3,3,3,3,3,3,3,3,3,3,3,3,3,3,3,3,3,3,3,3,3,3,3,3,3,
3,3,3,3,3,3,3,3,3,3,3,3,3,3,3,3,3,3,3,3,3,3,3,3,3,3,3,3,3,3,4),(40.8407044966687,
40.9233068860812,41.0060093484569,41.0885407393962,41.1710668185745,41.2536064041252,
41.3364364493657,41.4191012667399,41.5020139259136,41.5849265850873,41.6686733178014,
41.7523169948296,41.8358777389084,41.9193756008778,42.0028381014531,42.0862832369582,
42.169729071814,42.253193667065,42.3367468524999,42.4203446860855,42.5040762489604,
42.5839100872865,42.6676568199842,42.7513004969958,42.8348612410579,42.9183591030104,
43.0018216035687,43.0852667390566,43.1687125738951,43.2521771691288,43.3357303545463,
43.4193281881147,43.5030597509723,43.5828935894856,43.6666403221865,43.7502839992013,
43.8338447432672,43.9173426052228,44.0008051057843,44.0842502412753,44.1676960761171,
44.251160671354,44.3347138567746,44.418311690346,44.5020432532065,44.5818770916848,
44.6656238243886,44.7492675014062,44.8328282454744,44.9163261074329,44.9997886079974,
45.0832337434915,45.1666795783362,45.2501441735762,45.3336973589999,45.4172951925746,
45.5010267554384,45.580860593884,45.6646073265853,45.7482510036006,45.831811747666,
45.9153096096219,45.9987721101838,46.0822172456756,46.1656630805174,46.2491276757548,
46.332680861176,46.4162786947479,46.5000102576091,46.5798440960831,46.6663301926089,
46.7526868044835,46.8389274450679,46.9250352854062,47.0110642688329,47.0970105479747,
47.1238898038483),.UNSPECIFIED.);
#421=B_SPLINE_CURVE_WITH_KNOTS('',3,(#48192,#48193,#48194,#48195,#48196,
#48197,#48198,#48199,#48200,#48201,#48202,#48203,#48204,#48205,#48206,#48207,
#48208,#48209,#48210,#48211,#48212,#48213,#48214,#48215,#48216,#48217,#48218,
#48219,#48220,#48221,#48222,#48223,#48224,#48225,#48226,#48227,#48228,#48229,
#48230,#48231,#48232,#48233,#48234,#48235,#48236,#48237,#48238,#48239,#48240,
#48241,#48242,#48243,#48244,#48245,#48246,#48247,#48248,#48249,#48250,#48251,
#48252,#48253,#48254,#48255,#48256,#48257,#48258,#48259,#48260,#48261,#48262,
#48263,#48264,#48265,#48266,#48267,#48268,#48269,#48270,#48271,#48272,#48273,
#48274,#48275,#48276,#48277,#48278,#48279,#48280,#48281,#48282,#48283,#48284,
#48285,#48286,#48287,#48288,#48289,#48290,#48291,#48292,#48293,#48294,#48295,
#48296,#48297,#48298,#48299,#48300,#48301,#48302,#48303,#48304,#48305,#48306,
#48307,#48308,#48309,#48310,#48311,#48312,#48313,#48314,#48315,#48316,#48317,
#48318,#48319,#48320,#48321,#48322,#48323,#48324,#48325,#48326,#48327,#48328,
#48329,#48330,#48331,#48332,#48333,#48334,#48335,#48336,#48337,#48338,#48339,
#48340,#48341,#48342,#48343,#48344,#48345,#48346,#48347,#48348,#48349,#48350,
#48351,#48352,#48353,#48354,#48355,#48356,#48357,#48358,#48359,#48360,#48361,
#48362,#48363,#48364,#48365,#48366,#48367,#48368,#48369,#48370,#48371,#48372,
#48373,#48374,#48375,#48376,#48377,#48378,#48379,#48380,#48381,#48382,#48383,
#48384,#48385,#48386,#48387,#48388,#48389,#48390,#48391,#48392,#48393,#48394,
#48395,#48396,#48397,#48398,#48399,#48400,#48401,#48402,#48403,#48404,#48405,
#48406,#48407,#48408,#48409,#48410,#48411,#48412,#48413,#48414,#48415,#48416,
#48417),.UNSPECIFIED.,.F.,.F.,(4,3,3,3,3,3,3,3,3,3,3,3,3,3,3,3,3,3,3,3,
3,3,3,3,3,3,3,3,3,3,3,3,3,3,3,3,3,3,3,3,3,3,3,3,3,3,3,3,3,3,3,3,3,3,3,3,
3,3,3,3,3,3,3,3,3,3,3,3,3,3,3,3,3,3,3,4),(47.1238898040433,47.2131016067916,
47.3045331046643,47.3942129592113,47.4865202787468,47.5788275982823,47.6625743309846,
47.7462180080007,47.8297787520674,47.9132766140242,47.9967391145871,48.0801842500797,
48.163630084923,48.2470946801614,48.3306478655835,48.4142456991565,48.4979772620187,
48.5778111004815,48.6615578331834,48.7452015101991,48.8287622542655,48.9122601162221,
48.9957226167846,49.0791677522768,49.1626135871195,49.2460781823574,49.3296313677792,
49.4132292013517,49.4969607642135,49.5767946026806,49.6605413353825,49.7441850123983,
49.8277457564647,49.9112436184213,49.9947061189839,50.0781512544761,50.1615970893189,
50.2450616845569,50.3286148699787,50.4122127035513,50.4959442664131,50.5757781048798,
50.6595248375819,50.7431685145977,50.8267292586643,50.9102271206211,50.9936896211838,
51.0771347566761,51.160580591519,51.2440451867572,51.3275983721791,51.4111962057519,
51.4949277686138,51.574761607079,51.658508339781,51.7421520167969,51.8257127608633,
51.9092106228201,51.9926731233827,52.076118258875,52.1595640937179,52.2430286889561,
52.326581874378,52.4101797079507,52.4939112708126,52.5737451092781,52.6562428621318,
52.7386381122537,52.8221927370766,52.9044434497227,52.9866617918347,53.0688668044213,
53.1534188810252,53.2356870725923,53.3213810917146,53.407075110837),
 .UNSPECIFIED.);
#422=B_SPLINE_CURVE_WITH_KNOTS('',3,(#48419,#48420,#48421,#48422,#48423,
#48424,#48425,#48426,#48427,#48428,#48429,#48430,#48431,#48432,#48433,#48434,
#48435,#48436,#48437,#48438,#48439,#48440,#48441,#48442,#48443,#48444,#48445,
#48446,#48447,#48448,#48449,#48450,#48451,#48452,#48453,#48454,#48455,#48456,
#48457,#48458,#48459,#48460,#48461,#48462,#48463,#48464,#48465,#48466,#48467,
#48468,#48469,#48470,#48471,#48472,#48473,#48474,#48475,#48476,#48477,#48478,
#48479,#48480,#48481,#48482,#48483,#48484,#48485,#48486,#48487,#48488,#48489,
#48490,#48491,#48492,#48493,#48494,#48495,#48496,#48497,#48498,#48499,#48500,
#48501,#48502,#48503,#48504,#48505,#48506,#48507,#48508,#48509,#48510,#48511,
#48512,#48513,#48514,#48515,#48516,#48517,#48518,#48519,#48520,#48521,#48522,
#48523,#48524,#48525,#48526,#48527,#48528,#48529,#48530,#48531,#48532,#48533,
#48534,#48535,#48536,#48537,#48538,#48539,#48540,#48541,#48542,#48543,#48544,
#48545,#48546,#48547,#48548,#48549,#48550,#48551,#48552,#48553,#48554,#48555,
#48556,#48557,#48558,#48559,#48560,#48561,#48562,#48563,#48564,#48565,#48566,
#48567,#48568,#48569,#48570,#48571,#48572,#48573,#48574,#48575,#48576,#48577,
#48578,#48579,#48580,#48581,#48582,#48583,#48584,#48585,#48586,#48587,#48588,
#48589,#48590,#48591,#48592,#48593,#48594,#48595,#48596,#48597,#48598,#48599,
#48600,#48601,#48602,#48603,#48604,#48605,#48606,#48607,#48608,#48609,#48610,
#48611,#48612,#48613,#48614,#48615,#48616,#48617,#48618,#48619,#48620,#48621,
#48622,#48623,#48624,#48625,#48626,#48627,#48628,#48629,#48630,#48631,#48632,
#48633,#48634,#48635,#48636,#48637,#48638,#48639,#48640,#48641,#48642,#48643,
#48644),.UNSPECIFIED.,.F.,.F.,(4,3,3,3,3,3,3,3,3,3,3,3,3,3,3,3,3,3,3,3,
3,3,3,3,3,3,3,3,3,3,3,3,3,3,3,3,3,3,3,3,3,3,3,3,3,3,3,3,3,3,3,3,3,3,3,3,
3,3,3,3,3,3,3,3,3,3,3,3,3,3,3,3,3,3,3,4),(53.4070751110279,53.5404486401583,
53.5727286114773,53.6564753441794,53.7401190211952,53.8236797652618,53.9071776272187,
53.9906401277814,54.0740852632737,54.1575310981167,54.2409956933549,54.3245488787768,
54.4081467123496,54.4918782752115,54.5717121136765,54.6554588463785,54.7391025233943,
54.8226632674608,54.9061611294176,54.9896236299802,55.0730687654725,55.1565146003153,
55.2399791955534,55.3235323809753,55.4071302145479,55.4908617774098,55.5706956158756,
55.6544423485775,55.7380860255933,55.8216467696598,55.9051446316165,55.9886071321791,
56.0720522676713,56.1554981025141,56.2389626977521,56.3225158831739,56.4061137167465,
56.4898452796084,56.5696791180748,56.6534258507768,56.7370695277926,56.8206302718592,
56.9041281338159,56.9875906343785,57.0710357698708,57.1544816047136,57.2379461999517,
57.3214993853736,57.4050972189462,57.4888287818081,57.5686626202739,57.6524093529759,
57.7360530299917,57.8196137740582,57.9031116360149,57.9865741365775,58.0700192720698,
58.1534651069126,58.2369297021506,58.3204828875725,58.4040807211451,58.487812284007,
58.5676461224731,58.6513928551751,58.7350365321909,58.8185972762574,58.9020951382142,
58.9855576387768,59.069002774269,59.1524486091118,59.2359132043498,59.3194663897717,
59.4030642233443,59.4867957862062,59.5666296246723,59.6902604182075),
 .UNSPECIFIED.);
#423=B_SPLINE_CURVE_WITH_KNOTS('',3,(#48646,#48647,#48648,#48649,#48650,
#48651,#48652,#48653,#48654,#48655,#48656,#48657,#48658,#48659,#48660,#48661,
#48662,#48663,#48664,#48665,#48666,#48667,#48668,#48669,#48670,#48671,#48672,
#48673,#48674,#48675,#48676,#48677,#48678,#48679,#48680,#48681,#48682,#48683,
#48684,#48685,#48686,#48687,#48688,#48689,#48690,#48691,#48692,#48693,#48694,
#48695,#48696,#48697,#48698,#48699,#48700,#48701,#48702,#48703,#48704,#48705,
#48706,#48707,#48708,#48709,#48710,#48711,#48712,#48713,#48714,#48715,#48716,
#48717,#48718,#48719,#48720,#48721,#48722,#48723,#48724,#48725,#48726,#48727,
#48728,#48729,#48730,#48731,#48732,#48733,#48734,#48735,#48736,#48737,#48738,
#48739,#48740,#48741,#48742,#48743,#48744,#48745,#48746,#48747,#48748,#48749,
#48750,#48751,#48752,#48753,#48754,#48755,#48756,#48757,#48758,#48759,#48760,
#48761,#48762,#48763,#48764,#48765,#48766,#48767,#48768,#48769,#48770,#48771,
#48772,#48773,#48774,#48775,#48776,#48777,#48778,#48779,#48780,#48781,#48782,
#48783,#48784,#48785,#48786,#48787,#48788,#48789,#48790,#48791,#48792,#48793,
#48794,#48795,#48796,#48797,#48798,#48799,#48800,#48801,#48802,#48803,#48804,
#48805,#48806,#48807,#48808,#48809,#48810,#48811,#48812,#48813,#48814,#48815,
#48816,#48817,#48818,#48819,#48820,#48821,#48822,#48823,#48824,#48825,#48826,
#48827,#48828,#48829,#48830,#48831,#48832,#48833,#48834,#48835,#48836,#48837,
#48838,#48839,#48840,#48841,#48842,#48843,#48844,#48845,#48846,#48847,#48848,
#48849,#48850,#48851,#48852,#48853,#48854,#48855,#48856,#48857,#48858,#48859,
#48860,#48861,#48862,#48863,#48864,#48865,#48866,#48867,#48868,#48869,#48870,
#48871,#48872,#48873,#48874),.UNSPECIFIED.,.F.,.F.,(4,3,3,3,3,3,3,3,3,3,
3,3,3,3,3,3,3,3,3,3,3,3,3,3,3,3,3,3,3,3,3,3,3,3,3,3,3,3,3,3,3,3,3,3,3,3,
3,3,3,3,3,3,3,3,3,3,3,3,3,3,3,3,3,3,3,3,3,3,3,3,3,3,3,3,3,3,4),(59.6902604183383,
59.7727730645136,59.8551978339046,59.937555829786,60.0198741998651,60.1021735226374,
60.1844727762721,60.2667909365586,60.3491942539214,60.4316440876682,60.514216687236,
60.5656131268714,60.6493598595734,60.7330035365893,60.8165642806556,60.9000621426123,
60.9835246431749,61.0669697786671,61.1504156135099,61.2338802087482,61.31743339417,
61.4010312277426,61.4847627906044,61.5645966290706,61.6483433617727,61.7319870387886,
61.8155477828553,61.8990456448121,61.9825081453748,62.0659532808671,62.1493991157099,
62.232863710948,62.3164168963699,62.4000147299426,62.4837462928045,62.5635801312698,
62.6473268639717,62.7309705409874,62.8145312850538,62.8980291470104,62.981491647573,
63.0649367830651,63.148382617908,63.231847213146,63.3154003985678,63.3989982321403,
63.4827297950021,63.5625636334689,63.6463103661709,63.7299540431867,63.8135147872533,
63.89701264921,63.9804751497727,64.063920285265,64.147366120108,64.2308307153459,
64.3143839007678,64.3979817343406,64.4817132972025,64.5615471356681,64.6452938683701,
64.7289375453863,64.8124982894526,64.8959961514093,64.9794586519718,65.0629037874642,
65.1463496223072,65.2298142175456,65.3133674029674,65.39696523654,65.4806967994018,
65.5605306378673,65.652882329379,65.7448720149147,65.8366278894589,65.9280144118952,
65.9734457252248),.UNSPECIFIED.);
#424=B_SPLINE_CURVE_WITH_KNOTS('',3,(#48876,#48877,#48878,#48879,#48880,
#48881,#48882,#48883,#48884,#48885,#48886,#48887,#48888,#48889,#48890,#48891,
#48892,#48893,#48894,#48895,#48896,#48897,#48898,#48899,#48900,#48901,#48902,
#48903,#48904,#48905,#48906,#48907,#48908,#48909,#48910,#48911,#48912,#48913,
#48914,#48915,#48916,#48917,#48918,#48919,#48920,#48921,#48922,#48923,#48924,
#48925,#48926,#48927,#48928,#48929,#48930,#48931,#48932,#48933,#48934,#48935,
#48936,#48937,#48938,#48939,#48940,#48941,#48942,#48943,#48944,#48945,#48946,
#48947,#48948,#48949,#48950,#48951,#48952,#48953,#48954,#48955,#48956,#48957,
#48958,#48959,#48960,#48961,#48962,#48963,#48964,#48965,#48966,#48967,#48968,
#48969,#48970,#48971,#48972,#48973,#48974,#48975,#48976,#48977,#48978,#48979,
#48980,#48981,#48982,#48983,#48984,#48985,#48986,#48987,#48988,#48989,#48990,
#48991,#48992,#48993,#48994,#48995,#48996,#48997,#48998,#48999,#49000,#49001,
#49002,#49003,#49004,#49005,#49006,#49007,#49008,#49009,#49010,#49011,#49012,
#49013,#49014,#49015,#49016,#49017,#49018,#49019,#49020,#49021,#49022,#49023,
#49024,#49025,#49026,#49027,#49028,#49029,#49030,#49031,#49032,#49033,#49034,
#49035,#49036,#49037,#49038,#49039,#49040,#49041,#49042,#49043,#49044,#49045,
#49046,#49047,#49048,#49049,#49050,#49051,#49052,#49053,#49054,#49055,#49056,
#49057,#49058,#49059,#49060,#49061,#49062,#49063,#49064,#49065,#49066,#49067,
#49068,#49069,#49070,#49071,#49072,#49073,#49074,#49075,#49076,#49077,#49078,
#49079,#49080,#49081,#49082,#49083,#49084,#49085,#49086,#49087,#49088,#49089,
#49090,#49091,#49092,#49093,#49094,#49095,#49096,#49097,#49098,#49099,#49100,
#49101,#49102,#49103,#49104),.UNSPECIFIED.,.F.,.F.,(4,3,3,3,3,3,3,3,3,3,
3,3,3,3,3,3,3,3,3,3,3,3,3,3,3,3,3,3,3,3,3,3,3,3,3,3,3,3,3,3,3,3,3,3,3,3,
3,3,3,3,3,3,3,3,3,3,3,3,3,3,3,3,3,3,3,3,3,3,3,3,3,3,3,3,3,3,4),(65.9734457253871,
66.0583137750458,66.1432129355834,66.2281590044431,66.3132300065901,66.3983658996381,
66.4836594664784,66.5595141400664,66.6432608727684,66.7269045497842,66.8104652938508,
66.8939631558075,66.9774256563701,67.0608707918624,67.1443166267054,67.2277812219434,
67.3113344073653,67.3949322409378,67.4786638037997,67.5584976422656,67.6422443749675,
67.7258880519833,67.8094487960498,67.8929466580062,67.9764091585687,68.059854294061,
68.1433001289038,68.2267647241418,68.3103179095636,68.3939157431361,68.477647305998,
68.5574811444648,68.6412278771669,68.7248715541827,68.8084322982493,68.8919301602061,
68.9753926607689,69.0588377962614,69.1422836311044,69.2257482263426,69.3093014117645,
69.3928992453372,69.4766308081992,69.5564646466639,69.6402113793658,69.7238550563815,
69.8074158004482,69.8909136624047,69.9743761629672,70.0578212984594,70.141267133302,
70.22473172854,70.3082849139618,70.3918827475344,70.4756143103962,70.5554481488631,
70.6391948815652,70.722838558581,70.8063993026476,70.8898971646042,70.9733596651668,
71.0568048006591,71.1402506355021,71.2237152307402,71.3072684161621,71.3908662497347,
71.4745978125967,71.5544316510623,71.637669438077,71.7207727177989,71.8037981191682,
71.8867642534451,71.9696896846727,72.0526066766501,72.1355184100973,72.2184668296268,
72.2566310325666),.UNSPECIFIED.);
#425=B_SPLINE_CURVE_WITH_KNOTS('',3,(#49106,#49107,#49108,#49109,#49110,
#49111,#49112,#49113,#49114,#49115,#49116,#49117,#49118,#49119,#49120,#49121,
#49122,#49123,#49124,#49125,#49126,#49127,#49128,#49129,#49130,#49131,#49132,
#49133,#49134,#49135,#49136,#49137,#49138,#49139,#49140,#49141,#49142,#49143,
#49144,#49145,#49146,#49147,#49148,#49149,#49150,#49151,#49152,#49153,#49154,
#49155,#49156,#49157,#49158,#49159,#49160,#49161,#49162,#49163,#49164,#49165,
#49166,#49167,#49168,#49169,#49170,#49171,#49172,#49173,#49174,#49175,#49176,
#49177,#49178,#49179,#49180,#49181,#49182,#49183,#49184,#49185,#49186,#49187,
#49188,#49189,#49190,#49191,#49192,#49193,#49194,#49195,#49196,#49197,#49198,
#49199,#49200,#49201,#49202,#49203,#49204,#49205,#49206,#49207,#49208,#49209,
#49210,#49211,#49212,#49213,#49214,#49215,#49216,#49217,#49218,#49219,#49220,
#49221,#49222,#49223,#49224,#49225,#49226,#49227,#49228,#49229,#49230,#49231,
#49232,#49233,#49234,#49235,#49236,#49237,#49238,#49239,#49240,#49241,#49242,
#49243,#49244,#49245,#49246,#49247,#49248,#49249,#49250,#49251,#49252,#49253,
#49254,#49255,#49256,#49257,#49258,#49259,#49260,#49261,#49262,#49263,#49264,
#49265,#49266,#49267,#49268,#49269,#49270,#49271,#49272,#49273,#49274,#49275,
#49276,#49277,#49278,#49279,#49280,#49281,#49282,#49283,#49284,#49285,#49286,
#49287,#49288,#49289,#49290,#49291,#49292,#49293,#49294,#49295,#49296,#49297,
#49298,#49299,#49300,#49301,#49302,#49303,#49304,#49305,#49306,#49307,#49308,
#49309,#49310,#49311,#49312,#49313,#49314,#49315,#49316,#49317,#49318,#49319,
#49320,#49321,#49322,#49323,#49324,#49325,#49326,#49327,#49328,#49329,#49330,
#49331),.UNSPECIFIED.,.F.,.F.,(4,3,3,3,3,3,3,3,3,3,3,3,3,3,3,3,3,3,3,3,
3,3,3,3,3,3,3,3,3,3,3,3,3,3,3,3,3,3,3,3,3,3,3,3,3,3,3,3,3,3,3,3,3,3,3,3,
3,3,3,3,3,3,3,3,3,3,3,3,3,3,3,3,3,3,3,4),(72.256631032708,72.3574966325378,
72.4597233926165,72.5534151532614,72.6371618859633,72.720805562979,72.8043663070453,
72.8878641690021,72.9713266695647,73.0547718050569,73.1382176398997,73.2216822351377,
73.3052354205595,73.388833254132,73.4725648169938,73.5523986554606,73.6361453881625,
73.7197890651783,73.8033498092448,73.8868476712015,73.9703101717641,74.0537553072564,
74.1372011420992,74.2206657373373,74.3042189227592,74.3878167563318,74.4715483191936,
74.5513821576597,74.6351288903617,74.7187725673775,74.8023333114441,74.8858311734007,
74.9692936739634,75.0527388094557,75.1361846442986,75.2196492395367,75.3032024249585,
75.3868002585312,75.4705318213931,75.5503656598589,75.6341123925609,75.7177560695767,
75.8013168136432,75.8848146755999,75.9682771761625,76.0517223116548,76.1351681464976,
76.2186327417357,76.3021859271575,76.3857837607301,76.469515323592,76.5493491620581,
76.6330958947601,76.7167395717759,76.8003003158424,76.8837981777991,76.9672606783617,
77.050705813854,77.1341516486968,77.2176162439349,77.3011694293568,77.3847672629294,
77.4684988257913,77.5483326642572,77.6319679059608,77.7155001505879,77.7989496406175,
77.8823365457303,77.9656885756253,78.0490237282131,78.132360174458,78.2157160824001,
78.2991605475987,78.382650497063,78.466272073614,78.5398163396007),
 .UNSPECIFIED.);
#426=B_SPLINE_CURVE_WITH_KNOTS('',3,(#49333,#49334,#49335,#49336,#49337,
#49338,#49339,#49340,#49341,#49342,#49343,#49344,#49345,#49346,#49347,#49348,
#49349,#49350,#49351,#49352,#49353,#49354,#49355,#49356,#49357,#49358,#49359,
#49360,#49361,#49362,#49363,#49364,#49365,#49366,#49367,#49368,#49369,#49370,
#49371,#49372,#49373,#49374,#49375,#49376,#49377,#49378,#49379,#49380,#49381,
#49382,#49383,#49384,#49385,#49386,#49387,#49388,#49389,#49390,#49391,#49392,
#49393,#49394,#49395,#49396,#49397,#49398,#49399,#49400,#49401,#49402,#49403,
#49404,#49405,#49406,#49407,#49408,#49409,#49410,#49411,#49412,#49413,#49414,
#49415,#49416,#49417,#49418,#49419,#49420,#49421,#49422,#49423,#49424,#49425,
#49426,#49427,#49428,#49429,#49430,#49431,#49432,#49433,#49434,#49435,#49436,
#49437,#49438,#49439,#49440,#49441,#49442,#49443,#49444,#49445,#49446,#49447,
#49448,#49449,#49450,#49451,#49452,#49453,#49454,#49455,#49456,#49457,#49458,
#49459,#49460,#49461,#49462,#49463,#49464,#49465,#49466,#49467,#49468,#49469,
#49470,#49471,#49472,#49473,#49474,#49475,#49476,#49477,#49478,#49479,#49480,
#49481,#49482,#49483,#49484,#49485,#49486,#49487,#49488,#49489,#49490,#49491,
#49492,#49493,#49494,#49495,#49496,#49497,#49498,#49499,#49500,#49501,#49502,
#49503,#49504,#49505,#49506,#49507,#49508,#49509,#49510,#49511,#49512,#49513,
#49514,#49515,#49516,#49517,#49518,#49519,#49520,#49521,#49522,#49523,#49524,
#49525,#49526,#49527,#49528,#49529,#49530,#49531,#49532,#49533,#49534,#49535,
#49536,#49537,#49538,#49539,#49540,#49541,#49542,#49543,#49544,#49545,#49546,
#49547,#49548,#49549,#49550,#49551,#49552,#49553,#49554,#49555,#49556,#49557,
#49558,#49559,#49560,#49561),.UNSPECIFIED.,.F.,.F.,(4,3,3,3,3,3,3,3,3,3,
3,3,3,3,3,3,3,3,3,3,3,3,3,3,3,3,3,3,3,3,3,3,3,3,3,3,3,3,3,3,3,3,3,3,3,3,
3,3,3,3,3,3,3,3,3,3,3,3,3,3,3,3,3,3,3,3,3,3,3,3,3,3,3,3,3,3,4),(78.5398163397462,
78.5473161664564,78.6310628991584,78.7147065761743,78.7982673202406,78.8817651821975,
78.9652276827602,79.0486728182524,79.1321186530954,79.2155832483335,79.2991364337554,
79.3827342673281,79.46646583019,79.5462996686556,79.6300464013575,79.7136900783733,
79.7972508224399,79.8807486843966,79.9642111849592,80.0476563204514,80.1311021552943,
80.2145667505323,80.2981199359542,80.3817177695268,80.4654493323886,80.5452831708547,
80.6290299035567,80.7126735805725,80.796234324639,80.8797321865956,80.9631946871582,
81.0466398226505,81.1300856574933,81.2135502527314,81.2971034381532,81.3807012717259,
81.4644328345877,81.5442666730539,81.6280134057559,81.7116570827717,81.7952178268383,
81.878715688795,81.9621781893576,82.04562332485,82.1290691596928,82.2125337549309,
82.2960869403528,82.3796847739254,82.4634163367873,82.5432501752531,82.6269969079551,
82.7106405849708,82.7942013290373,82.877699190994,82.9611616915566,83.0446068270489,
83.1280526618917,83.2115172571298,83.2950704425516,83.3786682761242,83.4623998389861,
83.5422336774522,83.6259804101541,83.7096240871698,83.7931848312362,83.8766826931929,
83.9601451937554,84.0435903292477,84.1270361640904,84.2105007593285,84.2940539447503,
84.3776517783229,84.4613833411848,84.5412171796514,84.645685853533,84.748605073981,
84.8230016469258),.UNSPECIFIED.);
#427=B_SPLINE_CURVE_WITH_KNOTS('',3,(#49563,#49564,#49565,#49566,#49567,
#49568,#49569,#49570,#49571,#49572),.UNSPECIFIED.,.F.,.F.,(4,1,1,1,1,1,
1,4),(84.8230016469258,85.5402006818506,86.5391841840497,87.5381676862489,
88.5371511884481,89.5361346906472,90.5351181928464,91.1061869541054),
 .UNSPECIFIED.);
#428=B_SPLINE_CURVE_WITH_KNOTS('',3,(#49574,#49575,#49576,#49577,#49578,
#49579,#49580,#49581,#49582,#49583,#49584,#49585,#49586,#49587,#49588,#49589,
#49590,#49591,#49592,#49593,#49594,#49595,#49596,#49597,#49598,#49599,#49600,
#49601,#49602,#49603,#49604,#49605,#49606,#49607,#49608,#49609,#49610,#49611,
#49612,#49613,#49614,#49615,#49616,#49617,#49618,#49619,#49620,#49621,#49622,
#49623,#49624,#49625,#49626,#49627,#49628,#49629,#49630,#49631,#49632,#49633,
#49634,#49635,#49636,#49637,#49638,#49639,#49640,#49641,#49642,#49643,#49644,
#49645,#49646,#49647,#49648,#49649,#49650,#49651,#49652,#49653,#49654,#49655,
#49656,#49657,#49658,#49659,#49660,#49661,#49662,#49663,#49664,#49665,#49666,
#49667,#49668,#49669,#49670,#49671,#49672,#49673,#49674,#49675,#49676,#49677,
#49678,#49679,#49680,#49681,#49682,#49683,#49684,#49685,#49686,#49687,#49688,
#49689,#49690,#49691,#49692,#49693,#49694,#49695,#49696,#49697,#49698,#49699,
#49700,#49701,#49702,#49703,#49704,#49705,#49706,#49707,#49708,#49709,#49710,
#49711,#49712,#49713,#49714,#49715,#49716,#49717,#49718,#49719,#49720,#49721,
#49722,#49723,#49724,#49725,#49726,#49727,#49728,#49729,#49730,#49731,#49732,
#49733,#49734,#49735,#49736,#49737,#49738,#49739,#49740,#49741,#49742,#49743,
#49744,#49745,#49746,#49747,#49748,#49749,#49750,#49751,#49752,#49753,#49754,
#49755,#49756,#49757,#49758,#49759,#49760,#49761,#49762,#49763,#49764,#49765,
#49766,#49767,#49768,#49769,#49770,#49771,#49772,#49773,#49774,#49775,#49776,
#49777,#49778,#49779,#49780,#49781,#49782,#49783,#49784,#49785,#49786,#49787,
#49788,#49789,#49790,#49791,#49792,#49793,#49794,#49795,#49796,#49797,#49798,
#49799,#49800,#49801,#49802),.UNSPECIFIED.,.F.,.F.,(4,3,3,3,3,3,3,3,3,3,
3,3,3,3,3,3,3,3,3,3,3,3,3,3,3,3,3,3,3,3,3,3,3,3,3,3,3,3,3,3,3,3,3,3,3,3,
3,3,3,3,3,3,3,3,3,3,3,3,3,3,3,3,3,3,3,3,3,3,3,3,3,3,3,3,3,3,4),(91.1061869541054,
91.1967032367233,91.2876073527091,91.3787081395492,91.4701107400683,91.5341016950455,
91.6178484277474,91.7014921047632,91.7850528488296,91.8685507107865,91.9520132113491,
92.0354583468413,92.118904181684,92.2023687769221,92.2859219623439,92.3695197959165,
92.4532513587783,92.5330851972447,92.6168319299467,92.7004756069625,92.7840363510291,
92.8675342129859,92.9509967135485,93.0344418490408,93.1178876838837,93.2013522791218,
93.2849054645438,93.3685032981164,93.4522348609783,93.5320686994439,93.6158154321458,
93.6994591091615,93.783019853228,93.8665177151846,93.9499802157471,94.0334253512393,
94.1168711860821,94.2003357813201,94.2838889667419,94.3674868003145,94.4512183631763,
94.531052201643,94.614798934345,94.6984426113609,94.7820033554274,94.8655012173841,
94.9489637179468,95.0324088534391,95.115854688282,95.1993192835201,95.282872468942,
95.3664703025147,95.4502018653766,95.5300357038422,95.6137824365442,95.6974261135601,
95.7809868576267,95.8644847195834,95.947947220146,96.0313923556383,96.1148381904812,
96.1983027857192,96.2818559711412,96.3654538047138,96.4491853675757,96.5290192060414,
96.6115543549841,96.6939872426548,96.7763390732232,96.858629393003,96.9408873830372,
97.0231320612446,97.1053824317881,97.187694931784,97.2700427524997,97.3524884132919,
97.3893722611632),.UNSPECIFIED.);
#429=B_SPLINE_CURVE_WITH_KNOTS('',3,(#49804,#49805,#49806,#49807,#49808,
#49809,#49810,#49811,#49812,#49813,#49814,#49815,#49816,#49817,#49818,#49819,
#49820,#49821,#49822,#49823,#49824,#49825,#49826,#49827,#49828,#49829,#49830,
#49831,#49832,#49833,#49834,#49835,#49836,#49837,#49838,#49839,#49840,#49841,
#49842,#49843,#49844,#49845,#49846,#49847,#49848,#49849,#49850,#49851,#49852,
#49853,#49854,#49855,#49856,#49857,#49858,#49859,#49860,#49861,#49862,#49863,
#49864,#49865,#49866,#49867,#49868,#49869,#49870,#49871,#49872,#49873,#49874,
#49875,#49876,#49877,#49878,#49879,#49880,#49881,#49882,#49883,#49884,#49885,
#49886,#49887,#49888,#49889,#49890,#49891,#49892,#49893,#49894,#49895,#49896,
#49897,#49898,#49899,#49900,#49901,#49902,#49903,#49904,#49905,#49906,#49907,
#49908,#49909,#49910,#49911,#49912,#49913,#49914,#49915,#49916,#49917,#49918,
#49919,#49920,#49921,#49922,#49923,#49924,#49925,#49926,#49927,#49928,#49929,
#49930,#49931,#49932,#49933,#49934,#49935,#49936,#49937,#49938,#49939,#49940,
#49941,#49942,#49943,#49944,#49945,#49946,#49947,#49948,#49949,#49950,#49951,
#49952,#49953,#49954,#49955,#49956,#49957,#49958,#49959,#49960,#49961,#49962,
#49963,#49964,#49965,#49966,#49967,#49968,#49969,#49970,#49971,#49972,#49973,
#49974,#49975,#49976,#49977,#49978,#49979,#49980,#49981,#49982,#49983,#49984,
#49985,#49986,#49987,#49988,#49989,#49990,#49991,#49992,#49993,#49994,#49995,
#49996,#49997,#49998,#49999,#50000,#50001,#50002,#50003,#50004,#50005,#50006,
#50007,#50008,#50009,#50010,#50011,#50012,#50013,#50014,#50015,#50016,#50017,
#50018,#50019,#50020,#50021,#50022,#50023,#50024,#50025,#50026,#50027,#50028,
#50029),.UNSPECIFIED.,.F.,.F.,(4,3,3,3,3,3,3,3,3,3,3,3,3,3,3,3,3,3,3,3,
3,3,3,3,3,3,3,3,3,3,3,3,3,3,3,3,3,3,3,3,3,3,3,3,3,3,3,3,3,3,3,3,3,3,3,3,
3,3,3,3,3,3,3,3,3,3,3,3,3,3,3,3,3,3,3,4),(97.389372261285,97.5280027082405,
97.6117494409424,97.6953931179581,97.7789538620244,97.8624517239809,97.9459142245435,
98.0293593600356,98.1128051948784,98.1962697901164,98.2798229755382,98.3634208091107,
98.4471523719725,98.5269862104397,98.6107329431417,98.6943766201574,98.777937364224,
98.8614352261807,98.9448977267433,99.0283428622356,99.1117886970785,99.1952532923166,
99.2788064777384,99.3624043113111,99.4461358741729,99.5259697126389,99.6097164453409,
99.6933601223567,99.7769208664232,99.86041872838,99.9438812289426,100.027326364435,
100.110772199278,100.194236794516,100.277789979938,100.36138781351,100.445119376372,
100.524953214838,100.60869994754,100.692343624556,100.775904368622,100.859402230579,
100.942864731141,101.026309866633,101.109755701476,101.193220296714,101.276773482136,
101.360371315709,101.444102878571,101.523936717037,101.607683449739,101.691327126755,
101.774887870821,101.858385732778,101.941848233341,102.025293368833,102.108739203676,
102.192203798914,102.275756984336,102.359354817908,102.44308638077,102.522920219236,
102.606666951938,102.690310628954,102.77387137302,102.857369234977,102.94083173554,
103.024276871032,103.107722705875,103.191187301113,103.274740486535,103.358338320108,
103.44206988297,103.521903721436,103.663488611563,103.672557568465),
 .UNSPECIFIED.);
#430=B_SPLINE_CURVE_WITH_KNOTS('',3,(#50031,#50032,#50033,#50034,#50035,
#50036,#50037,#50038,#50039,#50040,#50041,#50042,#50043,#50044,#50045,#50046,
#50047,#50048,#50049,#50050,#50051,#50052,#50053,#50054,#50055,#50056,#50057,
#50058,#50059,#50060,#50061,#50062,#50063,#50064,#50065,#50066,#50067,#50068,
#50069,#50070,#50071,#50072,#50073,#50074,#50075,#50076,#50077,#50078,#50079,
#50080,#50081,#50082,#50083,#50084,#50085,#50086,#50087,#50088,#50089,#50090,
#50091,#50092,#50093,#50094,#50095,#50096,#50097,#50098,#50099,#50100,#50101,
#50102,#50103,#50104,#50105,#50106,#50107,#50108,#50109,#50110,#50111,#50112,
#50113,#50114,#50115,#50116,#50117,#50118,#50119,#50120,#50121,#50122,#50123,
#50124,#50125,#50126,#50127,#50128,#50129,#50130,#50131,#50132,#50133,#50134,
#50135,#50136,#50137,#50138,#50139,#50140,#50141,#50142,#50143,#50144,#50145,
#50146,#50147,#50148,#50149,#50150,#50151,#50152,#50153,#50154,#50155,#50156,
#50157,#50158,#50159,#50160,#50161,#50162,#50163,#50164,#50165,#50166,#50167,
#50168,#50169,#50170,#50171,#50172,#50173,#50174,#50175,#50176,#50177,#50178,
#50179,#50180,#50181,#50182,#50183,#50184,#50185,#50186,#50187,#50188,#50189,
#50190,#50191,#50192,#50193,#50194,#50195,#50196,#50197,#50198,#50199,#50200,
#50201,#50202,#50203,#50204,#50205,#50206,#50207,#50208,#50209,#50210,#50211,
#50212,#50213,#50214,#50215,#50216,#50217,#50218,#50219,#50220,#50221,#50222,
#50223,#50224,#50225,#50226,#50227,#50228,#50229,#50230,#50231,#50232,#50233,
#50234,#50235,#50236,#50237,#50238,#50239,#50240,#50241,#50242,#50243,#50244,
#50245,#50246,#50247,#50248,#50249,#50250,#50251,#50252,#50253,#50254,#50255,
#50256,#50257,#50258,#50259),.UNSPECIFIED.,.F.,.F.,(4,3,3,3,3,3,3,3,3,3,
3,3,3,3,3,3,3,3,3,3,3,3,3,3,3,3,3,3,3,3,3,3,3,3,3,3,3,3,3,3,3,3,3,3,3,3,
3,3,3,3,3,3,3,3,3,3,3,3,3,3,3,3,3,3,3,3,3,3,3,3,3,3,3,3,3,3,4),(103.672557568577,
103.754970286827,103.837301170646,103.92274942727,104.004987034183,104.087211884991,
104.169442999906,104.251699402181,104.334043794288,104.416440529236,104.498951993026,
104.520887223635,104.604633956337,104.688277633353,104.771838377419,104.855336239376,
104.938798739939,105.022243875431,105.105689710274,105.189154305512,105.272707490934,
105.356305324506,105.440036887368,105.519870725834,105.603617458536,105.687261135551,
105.770821879618,105.854319741575,105.937782242137,106.021227377629,106.104673212472,
106.18813780771,106.271690993132,106.355288826705,106.439020389567,106.518854228033,
106.602600960735,106.686244637751,106.769805381817,106.853303243773,106.936765744336,
107.020210879828,107.103656714671,107.187121309909,107.270674495331,107.354272328904,
107.438003891766,107.517837730232,107.601584462934,107.68522813995,107.768788884016,
107.852286745973,107.935749246536,108.019194382028,108.102640216871,108.186104812109,
108.269657997531,108.353255831104,108.436987393966,108.516821232431,108.600567965133,
108.684211642149,108.767772386215,108.851270248172,108.934732748735,109.018177884227,
109.10162371907,109.185088314308,109.26864149973,109.352239333302,109.435970896164,
109.515804734631,109.606603297722,109.697095090951,109.787399435718,109.877404147027,
109.955742875523),.UNSPECIFIED.);
#431=B_SPLINE_CURVE_WITH_KNOTS('',3,(#50261,#50262,#50263,#50264,#50265,
#50266,#50267,#50268,#50269,#50270,#50271,#50272,#50273,#50274,#50275,#50276,
#50277,#50278,#50279,#50280,#50281,#50282,#50283,#50284,#50285,#50286,#50287,
#50288,#50289,#50290,#50291,#50292,#50293,#50294,#50295,#50296,#50297,#50298,
#50299,#50300,#50301,#50302,#50303,#50304,#50305,#50306,#50307,#50308,#50309,
#50310,#50311,#50312,#50313,#50314,#50315,#50316,#50317,#50318,#50319,#50320,
#50321,#50322,#50323,#50324,#50325,#50326,#50327,#50328,#50329,#50330,#50331,
#50332,#50333,#50334,#50335,#50336,#50337,#50338,#50339,#50340,#50341,#50342,
#50343,#50344,#50345,#50346,#50347,#50348,#50349,#50350,#50351,#50352,#50353,
#50354,#50355,#50356,#50357,#50358,#50359,#50360,#50361,#50362,#50363,#50364,
#50365,#50366,#50367,#50368,#50369,#50370,#50371,#50372,#50373,#50374,#50375,
#50376,#50377,#50378,#50379,#50380,#50381,#50382,#50383,#50384,#50385,#50386,
#50387,#50388,#50389,#50390,#50391,#50392,#50393,#50394,#50395,#50396,#50397,
#50398,#50399,#50400,#50401,#50402,#50403,#50404,#50405,#50406,#50407,#50408,
#50409,#50410,#50411,#50412,#50413,#50414,#50415,#50416,#50417,#50418,#50419,
#50420,#50421,#50422,#50423,#50424,#50425,#50426,#50427,#50428,#50429,#50430,
#50431,#50432,#50433,#50434,#50435,#50436,#50437,#50438,#50439,#50440,#50441,
#50442,#50443,#50444,#50445,#50446,#50447,#50448,#50449,#50450,#50451,#50452,
#50453,#50454,#50455,#50456,#50457,#50458,#50459,#50460,#50461,#50462,#50463,
#50464,#50465,#50466,#50467,#50468,#50469,#50470,#50471,#50472,#50473,#50474,
#50475,#50476,#50477,#50478,#50479,#50480,#50481,#50482,#50483,#50484,#50485,
#50486,#50487,#50488,#50489),.UNSPECIFIED.,.F.,.F.,(4,3,3,3,3,3,3,3,3,3,
3,3,3,3,3,3,3,3,3,3,3,3,3,3,3,3,3,3,3,3,3,3,3,3,3,3,3,3,3,3,3,3,3,3,3,3,
3,3,3,3,3,3,3,3,3,3,3,3,3,3,3,3,3,3,3,3,3,3,3,3,3,3,3,3,3,3,4),(109.955742875644,
110.041285412932,110.126879716026,110.212540088657,110.298342751316,110.38422432511,
110.47026265263,110.51478823683,110.598534969532,110.682178646548,110.765739390614,
110.849237252571,110.932699753133,111.016144888626,111.099590723469,111.183055318706,
111.266608504128,111.350206337701,111.433937900563,111.513771739029,111.597518471731,
111.681162148746,111.764722892813,111.84822075477,111.931683255332,112.015128390824,
112.098574225667,112.182038820905,112.265592006327,112.3491898399,112.432921402761,
112.512755241228,112.59650197393,112.680145650946,112.763706395012,112.847204256969,
112.930666757531,113.014111893024,113.097557727867,113.181022323104,113.264575508526,
113.348173342099,113.431904904961,113.511738743427,113.595485476129,113.679129153145,
113.762689897211,113.846187759168,113.92965025973,114.013095395222,114.096541230065,
114.180005825303,114.263559010725,114.347156844298,114.43088840716,114.510722245626,
114.594468978328,114.678112655344,114.761673399411,114.845171261368,114.92863376193,
115.012078897423,115.095524732265,115.178989327504,115.262542512926,115.346140346498,
115.42987190936,115.509705747826,115.592661000623,115.675485081759,115.758233684028,
115.840925634918,115.923579714511,116.006234092482,116.08888573277,116.171589700014,
116.238928182824),.UNSPECIFIED.);
#432=B_SPLINE_CURVE_WITH_KNOTS('',3,(#50491,#50492,#50493,#50494,#50495,
#50496,#50497,#50498,#50499,#50500,#50501,#50502,#50503,#50504,#50505,#50506,
#50507,#50508,#50509,#50510,#50511,#50512,#50513,#50514,#50515,#50516,#50517,
#50518,#50519,#50520,#50521,#50522,#50523,#50524,#50525,#50526,#50527,#50528,
#50529,#50530,#50531,#50532,#50533,#50534,#50535,#50536,#50537,#50538,#50539,
#50540,#50541,#50542,#50543,#50544,#50545,#50546,#50547,#50548,#50549,#50550,
#50551,#50552,#50553,#50554,#50555,#50556,#50557,#50558,#50559,#50560,#50561,
#50562,#50563,#50564,#50565,#50566,#50567,#50568,#50569,#50570,#50571,#50572,
#50573,#50574,#50575,#50576,#50577,#50578,#50579,#50580,#50581,#50582,#50583,
#50584,#50585,#50586,#50587,#50588,#50589,#50590,#50591,#50592,#50593,#50594,
#50595,#50596,#50597,#50598,#50599,#50600,#50601,#50602,#50603,#50604,#50605,
#50606,#50607,#50608,#50609,#50610,#50611,#50612,#50613,#50614,#50615,#50616,
#50617,#50618,#50619,#50620,#50621,#50622,#50623,#50624,#50625,#50626,#50627,
#50628,#50629,#50630,#50631,#50632,#50633,#50634,#50635,#50636,#50637,#50638,
#50639,#50640,#50641,#50642,#50643,#50644,#50645,#50646,#50647,#50648,#50649,
#50650,#50651,#50652,#50653,#50654,#50655,#50656,#50657,#50658,#50659,#50660,
#50661,#50662,#50663,#50664,#50665,#50666,#50667,#50668,#50669,#50670,#50671,
#50672,#50673,#50674,#50675,#50676,#50677,#50678,#50679,#50680,#50681,#50682,
#50683,#50684,#50685,#50686,#50687,#50688,#50689,#50690,#50691,#50692,#50693,
#50694,#50695,#50696,#50697,#50698,#50699,#50700,#50701,#50702,#50703,#50704,
#50705,#50706,#50707,#50708,#50709,#50710,#50711,#50712,#50713,#50714,#50715,
#50716,#50717,#50718,#50719),.UNSPECIFIED.,.F.,.F.,(4,3,3,3,3,3,3,3,3,3,
3,3,3,3,3,3,3,3,3,3,3,3,3,3,3,3,3,3,3,3,3,3,3,3,3,3,3,3,3,3,3,3,3,3,3,3,
3,3,3,3,3,3,3,3,3,3,3,3,3,3,3,3,3,3,3,3,3,3,3,3,3,3,3,3,3,3,4),(116.238928183003,
116.343160711796,116.449245634065,116.508689250025,116.592435982727,116.676079659743,
116.759640403809,116.843138265766,116.926600766328,117.010045901821,117.093491736663,
117.176956331901,117.260509517323,117.344107350896,117.427838913757,117.507672752224,
117.591419484926,117.675063161942,117.758623906008,117.842121767965,117.925584268528,
118.00902940402,118.092475238863,118.175939834101,118.259493019523,118.343090853096,
118.426822415957,118.506656254423,118.590402987125,118.674046664141,118.757607408207,
118.841105270164,118.924567770726,119.008012906218,119.091458741061,119.174923336299,
119.258476521721,119.342074355293,119.425805918155,119.505639756622,119.589386489324,
119.67303016634,119.756590910406,119.840088772363,119.923551272925,120.006996408418,
120.090442243261,120.173906838499,120.25746002392,120.341057857493,120.424789420355,
120.504623258821,120.588369991523,120.672013668539,120.755574412605,120.839072274562,
120.922534775125,121.005979910617,121.08942574546,121.172890340698,121.25644352612,
121.340041359693,121.423772922555,121.50360676102,121.587353493722,121.670997170738,
121.754557914805,121.838055776761,121.921518277324,122.004963412816,122.088409247659,
122.171873842898,122.255427028319,122.339024861892,122.422756424754,122.50259026322,
122.522113490003),.UNSPECIFIED.);
#433=B_SPLINE_CURVE_WITH_KNOTS('',3,(#50721,#50722,#50723,#50724,#50725,
#50726,#50727,#50728,#50729,#50730,#50731,#50732,#50733,#50734,#50735,#50736,
#50737,#50738,#50739,#50740,#50741,#50742,#50743,#50744,#50745,#50746,#50747,
#50748,#50749,#50750,#50751,#50752,#50753,#50754,#50755,#50756,#50757,#50758,
#50759,#50760,#50761,#50762,#50763,#50764,#50765,#50766,#50767,#50768,#50769,
#50770,#50771,#50772,#50773,#50774,#50775,#50776,#50777,#50778,#50779,#50780,
#50781,#50782,#50783,#50784,#50785,#50786,#50787,#50788,#50789,#50790,#50791,
#50792,#50793,#50794,#50795,#50796,#50797,#50798,#50799,#50800,#50801,#50802,
#50803,#50804,#50805,#50806,#50807,#50808,#50809,#50810,#50811,#50812,#50813,
#50814,#50815,#50816,#50817,#50818,#50819,#50820,#50821,#50822,#50823,#50824,
#50825,#50826,#50827,#50828,#50829,#50830,#50831,#50832,#50833,#50834,#50835,
#50836,#50837,#50838,#50839,#50840,#50841,#50842,#50843,#50844,#50845,#50846,
#50847,#50848,#50849,#50850,#50851,#50852,#50853,#50854,#50855,#50856,#50857,
#50858,#50859,#50860,#50861,#50862,#50863,#50864,#50865,#50866,#50867,#50868,
#50869,#50870,#50871,#50872,#50873,#50874,#50875,#50876,#50877,#50878,#50879,
#50880,#50881,#50882,#50883,#50884,#50885,#50886,#50887,#50888,#50889,#50890,
#50891,#50892,#50893,#50894,#50895,#50896,#50897,#50898,#50899,#50900,#50901,
#50902,#50903,#50904,#50905,#50906,#50907,#50908,#50909,#50910,#50911,#50912,
#50913,#50914,#50915,#50916,#50917,#50918,#50919,#50920,#50921,#50922,#50923,
#50924,#50925,#50926,#50927,#50928,#50929,#50930,#50931,#50932,#50933,#50934,
#50935,#50936,#50937,#50938,#50939,#50940,#50941,#50942,#50943,#50944,#50945,
#50946),.UNSPECIFIED.,.F.,.F.,(4,3,3,3,3,3,3,3,3,3,3,3,3,3,3,3,3,3,3,3,
3,3,3,3,3,3,3,3,3,3,3,3,3,3,3,3,3,3,3,3,3,3,3,3,3,3,3,3,3,3,3,3,3,3,3,3,
3,3,3,3,3,3,3,3,3,3,3,3,3,3,3,3,3,3,3,4),(122.522113490184,122.605579195225,
122.688942451667,122.772223670943,122.855443190419,122.9386291599,123.021799364267,
123.104972125662,123.188165764287,123.271448247297,123.354777772417,123.438235782967,
123.501573765419,123.585320498121,123.668964175137,123.752524919203,123.83602278116,
123.919485281723,124.002930417215,124.086376252058,124.169840847296,124.253394032718,
124.33699186629,124.420723429152,124.500557267618,124.58430400032,124.667947677336,
124.751508421402,124.835006283359,124.918468783921,125.001913919414,125.085359754256,
125.168824349494,125.252377534916,125.335975368489,125.419706931351,125.499540769817,
125.583287502519,125.666931179535,125.750491923601,125.833989785557,125.91745228612,
126.000897421612,126.084343256455,126.167807851693,126.251361037115,126.334958870688,
126.41869043355,126.498524272016,126.582271004718,126.665914681734,126.7494754258,
126.832973287757,126.916435788319,126.999880923812,127.083326758655,127.166791353893,
127.250344539315,127.333942372887,127.417673935749,127.497507774215,127.581254506917,
127.664898183933,127.748458927999,127.831956789956,127.915419290518,127.99886442601,
128.082310260853,128.165774856091,128.249328041513,128.332925875085,128.416657437947,
128.496491276415,128.597476601312,128.701387699168,128.805298797024),
 .UNSPECIFIED.);
#434=B_SPLINE_CURVE_WITH_KNOTS('',3,(#50948,#50949,#50950,#50951,#50952,
#50953,#50954,#50955,#50956,#50957,#50958,#50959,#50960,#50961,#50962,#50963,
#50964,#50965,#50966,#50967,#50968,#50969,#50970,#50971,#50972,#50973,#50974,
#50975,#50976,#50977,#50978,#50979,#50980,#50981,#50982,#50983,#50984,#50985,
#50986,#50987,#50988,#50989,#50990,#50991,#50992,#50993,#50994,#50995,#50996,
#50997,#50998,#50999,#51000,#51001,#51002,#51003,#51004,#51005,#51006,#51007,
#51008,#51009,#51010,#51011,#51012,#51013,#51014,#51015,#51016,#51017,#51018,
#51019,#51020,#51021,#51022,#51023,#51024,#51025,#51026,#51027,#51028,#51029,
#51030,#51031,#51032,#51033,#51034,#51035,#51036,#51037,#51038,#51039,#51040,
#51041,#51042,#51043,#51044,#51045,#51046,#51047,#51048,#51049,#51050,#51051,
#51052,#51053,#51054,#51055,#51056,#51057,#51058,#51059,#51060,#51061,#51062,
#51063,#51064,#51065,#51066,#51067,#51068,#51069,#51070,#51071,#51072,#51073,
#51074,#51075,#51076,#51077,#51078,#51079,#51080,#51081,#51082,#51083,#51084,
#51085,#51086,#51087,#51088,#51089,#51090,#51091,#51092,#51093,#51094,#51095,
#51096,#51097,#51098,#51099,#51100,#51101,#51102,#51103,#51104,#51105,#51106,
#51107,#51108,#51109,#51110,#51111,#51112,#51113,#51114,#51115,#51116,#51117,
#51118,#51119,#51120,#51121,#51122,#51123,#51124,#51125,#51126,#51127,#51128,
#51129,#51130,#51131,#51132,#51133,#51134,#51135,#51136,#51137,#51138,#51139,
#51140,#51141,#51142,#51143,#51144,#51145,#51146,#51147,#51148,#51149,#51150,
#51151,#51152,#51153,#51154,#51155,#51156,#51157,#51158,#51159,#51160,#51161,
#51162,#51163,#51164,#51165,#51166,#51167,#51168,#51169,#51170,#51171,#51172,
#51173,#51174,#51175,#51176),.UNSPECIFIED.,.F.,.F.,(4,3,3,3,3,3,3,3,3,3,
3,3,3,3,3,3,3,3,3,3,3,3,3,3,3,3,3,3,3,3,3,3,3,3,3,3,3,3,3,3,3,3,3,3,3,3,
3,3,3,3,3,3,3,3,3,3,3,3,3,3,3,3,3,3,3,3,3,3,3,3,3,3,3,3,3,3,4),(128.805298797183,
128.891570794862,128.974631964316,129.057688587614,129.140759045218,129.223861723451,
129.307060779198,129.390317093249,129.473693556952,129.495474778614,129.579221511316,
129.662865188332,129.746425932398,129.829923794355,129.913386294917,129.99683143041,
130.080277265252,130.16374186049,130.247295045912,130.330892879485,130.414624442347,
130.494458280813,130.578205013515,130.661848690531,130.745409434597,130.828907296554,
130.912369797116,130.995814932609,131.079260767451,131.162725362689,131.246278548111,
131.329876381684,131.413607944546,131.493441783012,131.577188515714,131.66083219273,
131.744392936796,131.827890798753,131.911353299316,131.994798434808,132.078244269651,
132.161708864889,132.245262050311,132.328859883883,132.412591446745,132.492425285211,
132.576172017913,132.659815694929,132.743376438995,132.826874300952,132.910336801515,
132.993781937007,133.07722777185,133.160692367088,133.24424555251,133.327843386082,
133.411574948944,133.49140878741,133.575155520112,133.658799197128,133.742359941194,
133.825857803151,133.909320303714,133.992765439206,134.076211274048,134.159675869286,
134.243229054708,134.326826888281,134.410558451143,134.49039228961,134.575400498315,
134.660296053933,134.745095496624,134.830942648559,134.915588822726,135.002036463545,
135.088484104363),.UNSPECIFIED.);
#435=B_SPLINE_CURVE_WITH_KNOTS('',3,(#51178,#51179,#51180,#51181,#51182,
#51183,#51184,#51185,#51186,#51187,#51188,#51189,#51190,#51191,#51192,#51193,
#51194,#51195,#51196,#51197,#51198,#51199,#51200,#51201,#51202,#51203,#51204,
#51205,#51206,#51207,#51208,#51209,#51210,#51211,#51212,#51213,#51214,#51215,
#51216,#51217,#51218,#51219,#51220,#51221,#51222,#51223,#51224,#51225,#51226,
#51227,#51228,#51229,#51230,#51231,#51232,#51233,#51234,#51235,#51236,#51237,
#51238,#51239,#51240,#51241,#51242,#51243,#51244,#51245,#51246,#51247,#51248,
#51249,#51250,#51251,#51252,#51253,#51254,#51255,#51256,#51257,#51258,#51259,
#51260,#51261,#51262,#51263,#51264,#51265,#51266,#51267,#51268,#51269,#51270,
#51271,#51272,#51273,#51274,#51275,#51276,#51277,#51278,#51279,#51280,#51281,
#51282,#51283,#51284,#51285,#51286,#51287,#51288,#51289,#51290,#51291,#51292,
#51293,#51294,#51295,#51296,#51297,#51298,#51299,#51300,#51301,#51302,#51303,
#51304,#51305,#51306,#51307,#51308,#51309,#51310,#51311,#51312,#51313,#51314,
#51315,#51316,#51317,#51318,#51319,#51320,#51321,#51322,#51323,#51324,#51325,
#51326,#51327,#51328,#51329,#51330,#51331,#51332,#51333,#51334,#51335,#51336,
#51337,#51338,#51339,#51340,#51341,#51342,#51343,#51344,#51345,#51346,#51347,
#51348,#51349,#51350,#51351,#51352,#51353,#51354,#51355,#51356,#51357,#51358,
#51359,#51360,#51361,#51362,#51363,#51364,#51365,#51366,#51367,#51368,#51369,
#51370,#51371,#51372,#51373,#51374,#51375,#51376,#51377,#51378,#51379,#51380,
#51381,#51382,#51383,#51384,#51385,#51386,#51387,#51388,#51389,#51390,#51391,
#51392,#51393,#51394,#51395,#51396,#51397,#51398,#51399,#51400,#51401,#51402,
#51403,#51404,#51405,#51406),.UNSPECIFIED.,.F.,.F.,(4,3,3,3,3,3,3,3,3,3,
3,3,3,3,3,3,3,3,3,3,3,3,3,3,3,3,3,3,3,3,3,3,3,3,3,3,3,3,3,3,3,3,3,3,3,3,
3,3,3,3,3,3,3,3,3,3,3,3,3,3,3,3,3,3,3,3,3,3,3,3,3,3,3,3,3,3,4),(135.088484104542,
135.180495486085,135.272995115929,135.365747177429,135.458831781584,135.489375791809,
135.573122524511,135.656766201527,135.740326945593,135.82382480755,135.907287308113,
135.990732443605,136.074178278448,136.157642873686,136.241196059108,136.324793892681,
136.408525455543,136.488359294008,136.57210602671,136.655749703726,136.739310447792,
136.822808309749,136.906270810311,136.989715945804,137.073161780647,137.156626375885,
137.240179561306,137.323777394879,137.407508957741,137.487342796207,137.571089528909,
137.654733205925,137.738293949991,137.821791811948,137.90525431251,137.988699448003,
138.072145282845,138.155609878084,138.239163063505,138.322760897078,138.40649245994,
138.486326298406,138.570073031108,138.653716708124,138.73727745219,138.820775314147,
138.90423781471,138.987682950202,139.071128785045,139.154593380283,139.238146565705,
139.321744399278,139.405475962139,139.485309800605,139.569056533307,139.652700210323,
139.736260954389,139.819758816346,139.903221316909,139.986666452401,140.070112287244,
140.153576882482,140.237130067904,140.320727901477,140.404459464339,140.484293302805,
140.566929223367,140.649462929782,140.731915551088,140.814307347838,140.896666824531,
140.979012936728,141.061364626536,141.143783535083,141.226237338813,141.308802211266,
141.371669411407),.UNSPECIFIED.);
#436=B_SPLINE_CURVE_WITH_KNOTS('',3,(#51408,#51409,#51410,#51411,#51412,
#51413,#51414,#51415,#51416,#51417,#51418,#51419,#51420,#51421,#51422,#51423,
#51424,#51425,#51426,#51427,#51428,#51429,#51430,#51431,#51432,#51433,#51434,
#51435,#51436,#51437,#51438,#51439,#51440,#51441,#51442,#51443,#51444,#51445,
#51446,#51447,#51448,#51449,#51450,#51451,#51452,#51453,#51454,#51455,#51456,
#51457,#51458,#51459,#51460,#51461,#51462,#51463,#51464,#51465,#51466,#51467,
#51468,#51469,#51470,#51471,#51472,#51473,#51474,#51475,#51476,#51477,#51478,
#51479,#51480,#51481,#51482,#51483,#51484,#51485,#51486,#51487,#51488,#51489,
#51490,#51491,#51492,#51493,#51494,#51495,#51496,#51497,#51498,#51499,#51500,
#51501,#51502,#51503,#51504,#51505,#51506,#51507,#51508,#51509,#51510,#51511,
#51512,#51513,#51514,#51515,#51516,#51517,#51518,#51519,#51520,#51521,#51522,
#51523,#51524,#51525,#51526,#51527,#51528,#51529,#51530,#51531,#51532,#51533,
#51534,#51535,#51536,#51537,#51538,#51539,#51540,#51541,#51542,#51543,#51544,
#51545,#51546,#51547,#51548,#51549,#51550,#51551,#51552,#51553,#51554,#51555,
#51556,#51557,#51558,#51559,#51560,#51561,#51562,#51563,#51564,#51565,#51566,
#51567,#51568,#51569,#51570,#51571,#51572,#51573,#51574,#51575,#51576,#51577,
#51578,#51579,#51580,#51581,#51582,#51583,#51584,#51585,#51586,#51587,#51588,
#51589,#51590,#51591,#51592,#51593,#51594,#51595,#51596,#51597,#51598,#51599,
#51600,#51601,#51602,#51603,#51604,#51605,#51606,#51607,#51608,#51609,#51610,
#51611,#51612,#51613,#51614,#51615,#51616,#51617,#51618,#51619,#51620,#51621,
#51622,#51623,#51624,#51625,#51626,#51627,#51628,#51629,#51630,#51631,#51632,
#51633),.UNSPECIFIED.,.F.,.F.,(4,3,3,3,3,3,3,3,3,3,3,3,3,3,3,3,3,3,3,3,
3,3,3,3,3,3,3,3,3,3,3,3,3,3,3,3,3,3,3,3,3,3,3,3,3,3,3,3,3,3,3,3,3,3,3,3,
3,3,3,3,3,3,3,3,3,3,3,3,3,3,3,3,3,3,3,4),(141.371669411542,141.483276805004,
141.567023537706,141.650667214722,141.734227958788,141.817725820745,141.901188321307,
141.984633456799,142.068079291642,142.15154388688,142.235097072302,142.318694905875,
142.402426468736,142.482260307203,142.566007039905,142.649650716921,142.733211460987,
142.816709322944,142.900171823506,142.983616958999,143.067062793841,143.150527389079,
143.234080574501,143.317678408074,143.401409970936,143.481243809402,143.564990542104,
143.64863421912,143.732194963186,143.815692825143,143.899155325705,143.982600461198,
144.066046296041,144.149510891279,144.233064076701,144.316661910273,144.400393473135,
144.480227311601,144.563974044303,144.647617721319,144.731178465385,144.814676327342,
144.898138827905,144.981583963397,145.06502979824,145.148494393478,145.2320475789,
145.315645412473,145.399376975334,145.4792108138,145.562957546502,145.646601223518,
145.730161967584,145.813659829541,145.897122330104,145.980567465596,146.064013300439,
146.147477895677,146.231031081099,146.314628914672,146.398360477534,146.478194316,
146.561941048702,146.645584725718,146.729145469785,146.812643331741,146.896105832304,
146.979550967796,147.062996802639,147.146461397878,147.2300145833,147.313612416872,
147.397343979734,147.477177818199,147.605135855273,147.654854718722),
 .UNSPECIFIED.);
#437=B_SPLINE_CURVE_WITH_KNOTS('',3,(#51635,#51636,#51637,#51638,#51639,
#51640,#51641,#51642,#51643,#51644,#51645,#51646,#51647,#51648,#51649,#51650,
#51651,#51652,#51653,#51654,#51655,#51656,#51657,#51658,#51659,#51660,#51661,
#51662,#51663,#51664,#51665,#51666,#51667,#51668,#51669,#51670,#51671,#51672,
#51673,#51674,#51675,#51676,#51677,#51678,#51679,#51680,#51681,#51682,#51683,
#51684,#51685,#51686,#51687,#51688,#51689,#51690,#51691,#51692,#51693,#51694,
#51695,#51696,#51697,#51698,#51699,#51700,#51701,#51702,#51703,#51704,#51705,
#51706,#51707,#51708,#51709,#51710,#51711,#51712,#51713,#51714,#51715,#51716,
#51717,#51718,#51719,#51720,#51721,#51722,#51723,#51724,#51725,#51726,#51727,
#51728,#51729,#51730,#51731,#51732,#51733,#51734,#51735,#51736,#51737,#51738,
#51739,#51740,#51741,#51742,#51743,#51744,#51745,#51746,#51747,#51748,#51749,
#51750,#51751,#51752,#51753,#51754,#51755,#51756,#51757,#51758,#51759,#51760,
#51761,#51762,#51763,#51764,#51765,#51766,#51767,#51768,#51769,#51770,#51771,
#51772,#51773,#51774,#51775,#51776,#51777,#51778,#51779,#51780,#51781,#51782,
#51783,#51784,#51785,#51786,#51787,#51788,#51789,#51790,#51791,#51792,#51793,
#51794,#51795,#51796,#51797,#51798,#51799,#51800,#51801,#51802,#51803,#51804,
#51805,#51806,#51807,#51808,#51809,#51810,#51811,#51812,#51813,#51814,#51815,
#51816,#51817,#51818,#51819,#51820,#51821,#51822,#51823,#51824,#51825,#51826,
#51827,#51828,#51829,#51830,#51831,#51832,#51833,#51834,#51835,#51836,#51837,
#51838,#51839,#51840,#51841,#51842,#51843,#51844,#51845,#51846,#51847,#51848,
#51849,#51850,#51851,#51852,#51853,#51854,#51855,#51856,#51857,#51858,#51859,
#51860,#51861,#51862,#51863),.UNSPECIFIED.,.F.,.F.,(4,3,3,3,3,3,3,3,3,3,
3,3,3,3,3,3,3,3,3,3,3,3,3,3,3,3,3,3,3,3,3,3,3,3,3,3,3,3,3,3,3,3,3,3,3,3,
3,3,3,3,3,3,3,3,3,3,3,3,3,3,3,3,3,3,3,3,3,3,3,3,3,3,3,3,3,3,4),(147.654854718883,
147.737228180291,147.819526616244,147.901774471423,147.983995941504,148.066210060611,
148.148435854635,148.230742693763,148.313089645585,148.395567187923,148.476161320398,
148.5599080531,148.643551730116,148.727112474182,148.810610336139,148.894072836702,
148.977517972194,149.060963807037,149.144428402275,149.227981587696,149.311579421269,
149.395310984131,149.475144822597,149.558891555299,149.642535232315,149.726095976381,
149.809593838338,149.893056338901,149.976501474393,150.059947309236,150.143411904474,
150.226965089896,150.310562923469,150.394294486331,150.474128324796,150.557875057498,
150.641518734514,150.72507947858,150.808577340537,150.8920398411,150.975484976592,
151.058930811435,151.142395406672,151.225948592094,151.309546425667,151.393277988528,
151.473111826995,151.556858559697,151.640502236713,151.72406298078,151.807560842736,
151.891023343299,151.974468478792,152.057914313635,152.141378908873,152.224932094295,
152.308529927868,152.39226149073,152.472095329195,152.555842061897,152.639485738913,
152.723046482979,152.806544344935,152.890006845498,152.97345198099,153.056897815833,
153.140362411071,153.223915596493,153.307513430065,153.391244992927,153.471078831394,
153.560529790671,153.649805113436,153.738836835757,153.827717004931,153.916394555608,
153.938040025764),.UNSPECIFIED.);
#438=B_SPLINE_CURVE_WITH_KNOTS('',3,(#51865,#51866,#51867,#51868,#51869,
#51870,#51871,#51872,#51873,#51874,#51875,#51876,#51877,#51878,#51879,#51880,
#51881,#51882,#51883,#51884,#51885,#51886,#51887,#51888,#51889,#51890,#51891,
#51892,#51893,#51894,#51895,#51896,#51897,#51898,#51899,#51900,#51901,#51902,
#51903,#51904,#51905,#51906,#51907,#51908,#51909,#51910,#51911,#51912,#51913,
#51914,#51915,#51916,#51917,#51918,#51919,#51920,#51921,#51922,#51923,#51924,
#51925,#51926,#51927,#51928,#51929,#51930,#51931,#51932,#51933,#51934,#51935,
#51936,#51937,#51938,#51939,#51940,#51941,#51942,#51943,#51944,#51945,#51946,
#51947,#51948,#51949,#51950,#51951,#51952,#51953,#51954,#51955,#51956,#51957,
#51958,#51959,#51960,#51961,#51962,#51963,#51964,#51965,#51966,#51967,#51968,
#51969,#51970,#51971,#51972,#51973,#51974,#51975,#51976,#51977,#51978,#51979,
#51980,#51981,#51982,#51983,#51984,#51985,#51986,#51987,#51988,#51989,#51990,
#51991,#51992,#51993,#51994,#51995,#51996,#51997,#51998,#51999,#52000,#52001,
#52002,#52003,#52004,#52005,#52006,#52007,#52008,#52009,#52010,#52011,#52012,
#52013,#52014,#52015,#52016,#52017,#52018,#52019,#52020,#52021,#52022,#52023,
#52024,#52025,#52026,#52027,#52028,#52029,#52030,#52031,#52032,#52033,#52034,
#52035,#52036,#52037,#52038,#52039,#52040,#52041,#52042,#52043,#52044,#52045,
#52046,#52047,#52048,#52049,#52050,#52051,#52052,#52053,#52054,#52055,#52056,
#52057,#52058,#52059,#52060,#52061,#52062,#52063,#52064,#52065,#52066,#52067,
#52068,#52069,#52070,#52071,#52072,#52073,#52074,#52075,#52076,#52077,#52078,
#52079,#52080,#52081,#52082,#52083,#52084,#52085,#52086,#52087,#52088,#52089,
#52090,#52091,#52092,#52093,#52094,#52095,#52096),.UNSPECIFIED.,.F.,.F.,
(4,3,3,3,3,3,3,3,3,3,3,3,3,3,3,3,3,3,3,3,3,3,3,3,3,3,3,3,3,3,3,3,3,3,3,
3,3,3,3,3,3,3,3,3,3,3,3,3,3,3,3,3,3,3,3,3,3,3,3,3,3,3,3,3,3,3,3,3,3,3,3,
3,3,3,3,3,3,4),(153.938040025901,154.024359782887,154.110756324578,154.200582826831,
154.287234368446,154.373981223819,154.460883689602,154.470062333593,154.553809066295,
154.637452743311,154.721013487377,154.804511349334,154.887973849897,154.971418985389,
155.054864820232,155.13832941547,155.221882600892,155.305480434464,155.389211997326,
155.469045835792,155.552792568494,155.636436245509,155.719996989576,155.803494851533,
155.886957352095,155.970402487588,156.05384832243,156.137312917668,156.22086610309,
156.304463936663,156.388195499525,156.468029337991,156.551776070693,156.635419747709,
156.718980491775,156.802478353732,156.885940854295,156.969385989787,157.05283182463,
157.136296419867,157.219849605289,157.303447438862,157.387179001724,157.46701284019,
157.550759572892,157.634403249908,157.717963993974,157.80146185593,157.884924356493,
157.968369491985,158.051815326828,158.135279922066,158.218833107488,158.302430941061,
158.386162503922,158.46599634239,158.549743075092,158.633386752108,158.716947496174,
158.800445358131,158.883907858694,158.967352994187,159.05079882903,159.134263424268,
159.21781660969,159.301414443262,159.385146006124,159.464979844589,159.547722225675,
159.631910114101,159.714449093052,159.796933736485,159.87938296901,159.964843560028,
160.047301191615,160.129775716868,160.212308983891,160.221225333081),
 .UNSPECIFIED.);
#439=B_SPLINE_CURVE_WITH_KNOTS('',3,(#52098,#52099,#52100,#52101,#52102,
#52103,#52104,#52105,#52106,#52107,#52108,#52109,#52110,#52111,#52112,#52113,
#52114,#52115,#52116,#52117,#52118,#52119,#52120,#52121,#52122,#52123,#52124,
#52125,#52126,#52127,#52128,#52129,#52130,#52131,#52132,#52133,#52134,#52135,
#52136,#52137,#52138,#52139,#52140,#52141,#52142,#52143,#52144,#52145,#52146,
#52147,#52148,#52149,#52150,#52151,#52152,#52153,#52154,#52155,#52156,#52157,
#52158,#52159,#52160,#52161,#52162,#52163,#52164,#52165,#52166,#52167,#52168,
#52169,#52170,#52171,#52172,#52173,#52174,#52175,#52176,#52177,#52178,#52179,
#52180,#52181,#52182,#52183,#52184,#52185,#52186,#52187,#52188,#52189,#52190,
#52191,#52192,#52193,#52194,#52195,#52196,#52197,#52198,#52199,#52200,#52201,
#52202,#52203,#52204,#52205,#52206,#52207,#52208,#52209,#52210,#52211,#52212,
#52213,#52214,#52215,#52216,#52217,#52218,#52219,#52220,#52221,#52222,#52223,
#52224,#52225,#52226,#52227,#52228,#52229,#52230,#52231,#52232,#52233,#52234,
#52235,#52236,#52237,#52238,#52239,#52240,#52241,#52242,#52243,#52244,#52245,
#52246,#52247,#52248,#52249,#52250,#52251,#52252,#52253,#52254,#52255,#52256,
#52257,#52258,#52259,#52260,#52261,#52262,#52263,#52264,#52265,#52266,#52267,
#52268,#52269,#52270,#52271,#52272,#52273,#52274,#52275,#52276,#52277,#52278,
#52279,#52280,#52281,#52282,#52283,#52284,#52285,#52286,#52287,#52288,#52289,
#52290,#52291,#52292,#52293,#52294,#52295,#52296,#52297,#52298,#52299,#52300,
#52301,#52302,#52303,#52304,#52305,#52306,#52307,#52308,#52309,#52310,#52311,
#52312,#52313,#52314,#52315,#52316,#52317,#52318,#52319,#52320,#52321,#52322,
#52323,#52324,#52325,#52326),.UNSPECIFIED.,.F.,.F.,(4,3,3,3,3,3,3,3,3,3,
3,3,3,3,3,3,3,3,3,3,3,3,3,3,3,3,3,3,3,3,3,3,3,3,3,3,3,3,3,3,3,3,3,3,3,3,
3,3,3,3,3,3,3,3,3,3,3,3,3,3,3,3,3,3,3,3,3,3,3,3,3,3,3,3,3,3,4),(160.221225333185,
160.329604730348,160.44063773956,160.463963346788,160.54771007949,160.631353756506,
160.714914500572,160.798412362529,160.881874863091,160.965319998584,161.048765833426,
161.132230428665,161.215783614086,161.299381447659,161.383113010521,161.462946848987,
161.546693581689,161.630337258705,161.713898002771,161.797395864728,161.88085836529,
161.964303500783,162.047749335625,162.131213930863,162.214767116285,162.298364949858,
162.38209651272,162.461930351186,162.545677083888,162.629320760904,162.71288150497,
162.796379366927,162.87984186749,162.963287002982,163.046732837825,163.130197433063,
163.213750618485,163.297348452058,163.38108001492,163.460913853385,163.544660586087,
163.628304263103,163.711865007169,163.795362869126,163.878825369689,163.962270505181,
164.045716340024,164.129180935262,164.212734120684,164.296331954257,164.380063517119,
164.459897355585,164.543644088287,164.627287765303,164.710848509369,164.794346371326,
164.877808871889,164.961254007381,165.044699842224,165.128164437462,165.211717622884,
165.295315456457,165.379047019319,165.458880857784,165.542627590486,165.626271267502,
165.709832011568,165.793329873525,165.876792374087,165.960237509579,166.043683344422,
166.12714793966,166.210701125082,166.294298958654,166.378030521516,166.457864359983,
166.50441064026),.UNSPECIFIED.);
#440=B_SPLINE_CURVE_WITH_KNOTS('',3,(#52328,#52329,#52330,#52331,#52332,
#52333,#52334,#52335,#52336,#52337,#52338,#52339,#52340,#52341,#52342,#52343,
#52344,#52345,#52346,#52347,#52348,#52349,#52350,#52351,#52352,#52353,#52354,
#52355,#52356,#52357,#52358,#52359,#52360,#52361,#52362,#52363,#52364,#52365,
#52366,#52367,#52368,#52369,#52370,#52371,#52372,#52373,#52374,#52375,#52376,
#52377,#52378,#52379,#52380,#52381,#52382,#52383,#52384,#52385,#52386,#52387,
#52388,#52389,#52390,#52391,#52392,#52393,#52394,#52395,#52396,#52397,#52398,
#52399,#52400,#52401,#52402,#52403,#52404,#52405,#52406,#52407,#52408,#52409,
#52410,#52411,#52412,#52413,#52414,#52415,#52416,#52417,#52418,#52419,#52420,
#52421,#52422,#52423,#52424,#52425,#52426,#52427,#52428,#52429,#52430,#52431,
#52432,#52433,#52434,#52435,#52436,#52437,#52438,#52439,#52440,#52441,#52442,
#52443,#52444,#52445,#52446,#52447,#52448,#52449,#52450,#52451,#52452,#52453,
#52454,#52455,#52456,#52457,#52458,#52459,#52460,#52461,#52462,#52463,#52464,
#52465,#52466,#52467,#52468,#52469,#52470,#52471,#52472,#52473,#52474,#52475,
#52476,#52477,#52478,#52479,#52480,#52481,#52482,#52483,#52484,#52485,#52486,
#52487,#52488,#52489,#52490,#52491,#52492,#52493,#52494,#52495,#52496,#52497,
#52498,#52499,#52500,#52501,#52502,#52503,#52504,#52505,#52506,#52507,#52508,
#52509,#52510,#52511,#52512,#52513,#52514,#52515,#52516,#52517,#52518,#52519,
#52520,#52521,#52522,#52523,#52524,#52525,#52526,#52527,#52528,#52529,#52530,
#52531,#52532,#52533,#52534,#52535,#52536,#52537,#52538,#52539,#52540,#52541,
#52542,#52543,#52544,#52545,#52546,#52547,#52548,#52549,#52550,#52551,#52552,
#52553,#52554,#52555,#52556),.UNSPECIFIED.,.F.,.F.,(4,3,3,3,3,3,3,3,3,3,
3,3,3,3,3,3,3,3,3,3,3,3,3,3,3,3,3,3,3,3,3,3,3,3,3,3,3,3,3,3,3,3,3,3,3,3,
3,3,3,3,3,3,3,3,3,3,3,3,3,3,3,3,3,3,3,3,3,3,3,3,3,3,3,3,3,3,4),(166.504410640448,
166.587541388229,166.670571858568,166.753522758781,166.836414719578,166.919276960235,
167.002126467252,167.084981829367,167.167861636136,167.250831058329,167.333851236403,
167.416992715462,167.456847862182,167.540594594884,167.6242382719,167.707799015966,
167.791296877923,167.874759378485,167.958204513978,168.04165034882,168.125114944059,
168.20866812948,168.292265963053,168.375997525915,168.455831364381,168.539578097083,
168.623221774099,168.706782518165,168.790280380122,168.873742880685,168.957188016177,
169.04063385102,169.124098446258,169.20765163168,169.291249465253,169.374981028115,
169.45481486658,169.538561599282,169.622205276298,169.705766020364,169.789263882321,
169.872726382884,169.956171518376,170.039617353219,170.123081948457,170.206635133879,
170.290232967452,170.373964530313,170.45379836878,170.537545101482,170.621188778498,
170.704749522565,170.788247384521,170.871709885084,170.955155020576,171.038600855419,
171.122065450657,171.205618636079,171.289216469651,171.372948032513,171.452781870979,
171.536528603681,171.620172280696,171.703733024763,171.78723088672,171.870693387282,
171.954138522775,172.037584357617,172.121048952855,172.204602138277,172.28819997185,
172.371931534711,172.451765373178,172.549892717309,172.647579141693,172.744447331875,
172.787595947253),.UNSPECIFIED.);
#441=B_SPLINE_CURVE_WITH_KNOTS('',3,(#52558,#52559,#52560,#52561,#52562,
#52563,#52564,#52565,#52566,#52567,#52568,#52569,#52570,#52571,#52572,#52573,
#52574,#52575,#52576,#52577,#52578,#52579,#52580,#52581,#52582,#52583,#52584,
#52585,#52586,#52587,#52588,#52589,#52590,#52591,#52592,#52593,#52594,#52595,
#52596,#52597,#52598,#52599,#52600,#52601,#52602,#52603,#52604,#52605,#52606,
#52607,#52608,#52609,#52610,#52611,#52612,#52613,#52614,#52615,#52616,#52617,
#52618,#52619,#52620,#52621,#52622,#52623,#52624,#52625,#52626,#52627,#52628,
#52629,#52630,#52631,#52632,#52633,#52634,#52635,#52636,#52637,#52638,#52639,
#52640,#52641,#52642,#52643,#52644,#52645,#52646,#52647,#52648,#52649,#52650,
#52651,#52652,#52653,#52654,#52655,#52656,#52657,#52658,#52659,#52660,#52661,
#52662,#52663,#52664,#52665,#52666,#52667,#52668,#52669,#52670,#52671,#52672,
#52673,#52674,#52675,#52676,#52677,#52678,#52679,#52680,#52681,#52682,#52683,
#52684,#52685,#52686,#52687,#52688,#52689,#52690,#52691,#52692,#52693,#52694,
#52695,#52696,#52697,#52698,#52699,#52700,#52701,#52702,#52703,#52704,#52705,
#52706,#52707,#52708,#52709,#52710,#52711,#52712,#52713,#52714,#52715,#52716,
#52717,#52718,#52719,#52720,#52721,#52722,#52723,#52724,#52725,#52726,#52727,
#52728,#52729,#52730,#52731,#52732,#52733,#52734,#52735,#52736,#52737,#52738,
#52739,#52740,#52741,#52742,#52743,#52744,#52745,#52746,#52747,#52748,#52749,
#52750,#52751,#52752,#52753,#52754,#52755,#52756,#52757,#52758,#52759,#52760,
#52761,#52762,#52763,#52764,#52765,#52766,#52767,#52768,#52769,#52770,#52771,
#52772,#52773,#52774,#52775,#52776,#52777,#52778,#52779,#52780,#52781,#52782,
#52783,#52784,#52785,#52786),.UNSPECIFIED.,.F.,.F.,(4,3,3,3,3,3,3,3,3,3,
3,3,3,3,3,3,3,3,3,3,3,3,3,3,3,3,3,3,3,3,3,3,3,3,3,3,3,3,3,3,3,3,3,3,3,3,
3,3,3,3,3,3,3,3,3,3,3,3,3,3,3,3,3,3,3,3,3,3,3,3,3,3,3,3,3,3,4),(172.78759594744,
172.87103087237,172.954453667818,173.037882341608,173.121334901619,173.204883615468,
173.288481306221,173.372218918498,173.450748875377,173.534495608079,173.618139285095,
173.701700029161,173.785197891118,173.86866039168,173.952105527173,174.035551362015,
174.119015957253,174.202569142675,174.286166976248,174.36989853911,174.449732377576,
174.533479110278,174.617122787294,174.700683531361,174.784181393318,174.86764389388,
174.951089029373,175.034534864215,175.117999459453,175.201552644875,175.285150478448,
175.36888204131,175.448715879775,175.532462612477,175.616106289493,175.699667033559,
175.783164895516,175.866627396078,175.95007253157,176.033518366413,176.116982961651,
176.200536147073,176.284133980646,176.367865543508,176.447699381975,176.531446114677,
176.615089791693,176.69865053576,176.782148397717,176.865610898279,176.949056033771,
177.032501868614,177.115966463852,177.199519649274,177.283117482847,177.366849045709,
177.446682884174,177.530429616876,177.614073293892,177.697634037959,177.781131899916,
177.864594400478,177.94803953597,178.031485370813,178.114949966051,178.198503151473,
178.282100985046,178.365832547908,178.445666386373,178.530084882565,178.614396466162,
178.698618531916,178.782768409767,178.866859317495,178.950915854996,179.034962372757,
179.07078125462),.UNSPECIFIED.);
#442=B_SPLINE_CURVE_WITH_KNOTS('',3,(#52788,#52789,#52790,#52791,#52792,
#52793,#52794,#52795,#52796,#52797,#52798,#52799,#52800,#52801,#52802,#52803,
#52804,#52805,#52806,#52807,#52808,#52809,#52810,#52811,#52812,#52813,#52814,
#52815,#52816,#52817,#52818,#52819,#52820,#52821,#52822,#52823,#52824,#52825,
#52826,#52827,#52828,#52829,#52830,#52831,#52832,#52833,#52834,#52835,#52836,
#52837,#52838,#52839,#52840,#52841,#52842,#52843,#52844,#52845,#52846,#52847,
#52848,#52849,#52850,#52851,#52852,#52853,#52854,#52855,#52856,#52857,#52858,
#52859,#52860,#52861,#52862,#52863,#52864,#52865,#52866,#52867,#52868,#52869,
#52870,#52871,#52872,#52873,#52874,#52875,#52876,#52877,#52878,#52879,#52880,
#52881,#52882,#52883,#52884,#52885,#52886,#52887,#52888,#52889,#52890,#52891,
#52892,#52893,#52894,#52895,#52896,#52897,#52898,#52899,#52900,#52901,#52902,
#52903,#52904,#52905,#52906,#52907,#52908,#52909,#52910,#52911,#52912,#52913,
#52914,#52915,#52916,#52917,#52918,#52919,#52920,#52921,#52922,#52923,#52924,
#52925,#52926,#52927,#52928,#52929,#52930,#52931,#52932,#52933,#52934,#52935,
#52936,#52937,#52938,#52939,#52940,#52941,#52942,#52943,#52944,#52945,#52946,
#52947,#52948,#52949,#52950,#52951,#52952,#52953,#52954,#52955,#52956,#52957,
#52958,#52959,#52960,#52961,#52962,#52963,#52964,#52965,#52966,#52967,#52968,
#52969,#52970,#52971,#52972,#52973,#52974,#52975,#52976,#52977,#52978,#52979,
#52980,#52981,#52982,#52983,#52984,#52985,#52986,#52987,#52988,#52989,#52990,
#52991,#52992,#52993,#52994,#52995,#52996,#52997,#52998,#52999,#53000,#53001,
#53002,#53003,#53004,#53005,#53006,#53007,#53008,#53009,#53010,#53011,#53012,
#53013),.UNSPECIFIED.,.F.,.F.,(4,3,3,3,3,3,3,3,3,3,3,3,3,3,3,3,3,3,3,3,
3,3,3,3,3,3,3,3,3,3,3,3,3,3,3,3,3,3,3,3,3,3,3,3,3,3,3,3,3,3,3,3,3,3,3,3,
3,3,3,3,3,3,3,3,3,3,3,3,3,3,3,3,3,3,3,4),(179.070781254816,179.164775236396,
179.259131704028,179.354005530881,179.444649888572,179.528396621274,179.61204029829,
179.695601042356,179.779098904313,179.862561404875,179.946006540368,180.02945237521,
180.112916970448,180.19647015587,180.280067989443,180.363799552305,180.443633390771,
180.527380123473,180.611023800489,180.694584544555,180.778082406512,180.861544907075,
180.944990042567,181.02843587741,181.111900472648,181.19545365807,181.279051491642,
181.362783054504,181.44261689297,181.526363625672,181.610007302688,181.693568046755,
181.777065908711,181.860528409274,181.943973544766,182.027419379609,182.110883974847,
182.194437160269,182.278034993842,182.361766556704,182.44160039517,182.525347127872,
182.608990804888,182.692551548954,182.776049410911,182.859511911474,182.942957046966,
183.026402881809,183.109867477047,183.193420662469,183.277018496042,183.360750058903,
183.440583897369,183.524330630071,183.607974307087,183.691535051153,183.77503291311,
183.858495413673,183.941940549165,184.025386384008,184.108850979245,184.192404164667,
184.27600199824,184.359733561102,184.439567399568,184.522368027058,184.605066337652,
184.687683334069,184.770968737519,184.853492351443,184.936002373504,185.018517639074,
185.102379869722,185.185001784602,185.269484173134,185.353966561667),
 .UNSPECIFIED.);
#443=B_SPLINE_CURVE_WITH_KNOTS('',3,(#53015,#53016,#53017,#53018,#53019,
#53020,#53021,#53022,#53023,#53024,#53025,#53026,#53027,#53028,#53029,#53030,
#53031,#53032,#53033,#53034,#53035,#53036,#53037,#53038,#53039,#53040,#53041,
#53042,#53043,#53044,#53045,#53046,#53047,#53048,#53049,#53050,#53051,#53052,
#53053,#53054,#53055,#53056,#53057,#53058,#53059,#53060,#53061,#53062,#53063,
#53064,#53065,#53066,#53067,#53068,#53069,#53070,#53071,#53072,#53073,#53074,
#53075,#53076,#53077,#53078,#53079,#53080,#53081,#53082,#53083,#53084,#53085,
#53086,#53087,#53088,#53089,#53090,#53091,#53092,#53093,#53094,#53095,#53096,
#53097,#53098,#53099,#53100,#53101,#53102,#53103,#53104,#53105,#53106,#53107,
#53108,#53109,#53110,#53111,#53112,#53113,#53114,#53115,#53116,#53117,#53118,
#53119,#53120,#53121,#53122,#53123,#53124,#53125,#53126,#53127,#53128,#53129,
#53130,#53131,#53132,#53133,#53134,#53135,#53136,#53137,#53138,#53139,#53140,
#53141,#53142,#53143,#53144,#53145,#53146,#53147,#53148,#53149,#53150,#53151,
#53152,#53153,#53154,#53155,#53156,#53157,#53158,#53159,#53160,#53161,#53162,
#53163,#53164,#53165,#53166,#53167,#53168,#53169,#53170,#53171,#53172,#53173,
#53174,#53175,#53176,#53177,#53178,#53179,#53180,#53181,#53182,#53183,#53184,
#53185,#53186,#53187,#53188,#53189,#53190,#53191,#53192,#53193,#53194,#53195,
#53196,#53197,#53198,#53199,#53200,#53201,#53202,#53203,#53204,#53205,#53206,
#53207,#53208,#53209,#53210,#53211,#53212,#53213,#53214,#53215,#53216,#53217,
#53218,#53219,#53220,#53221,#53222,#53223,#53224,#53225,#53226,#53227,#53228,
#53229,#53230,#53231,#53232,#53233,#53234,#53235,#53236,#53237,#53238,#53239,
#53240),.UNSPECIFIED.,.F.,.F.,(4,3,3,3,3,3,3,3,3,3,3,3,3,3,3,3,3,3,3,3,
3,3,3,3,3,3,3,3,3,3,3,3,3,3,3,3,3,3,3,3,3,3,3,3,3,3,3,3,3,3,3,3,3,3,3,3,
3,3,3,3,3,3,3,3,3,3,3,3,3,3,3,3,3,3,3,4),(185.353966561799,185.438550901767,
185.522297634469,185.605941311485,185.689502055551,185.772999917508,185.856462418071,
185.939907553563,186.023353388406,186.106817983644,186.190371169066,186.273969002639,
186.3577005655,186.437534403966,186.521281136668,186.604924813684,186.68848555775,
186.771983419707,186.85544592027,186.938891055762,187.022336890605,187.105801485843,
187.189354671265,187.272952504837,187.356684067699,187.436517906165,187.520264638867,
187.603908315883,187.687469059949,187.770966921906,187.854429422469,187.937874557961,
188.021320392804,188.104784988042,188.188338173464,188.271936007037,188.355667569898,
188.435501408365,188.519248141067,188.602891818083,188.686452562149,188.769950424106,
188.853412924669,188.936858060161,189.020303895004,189.103768490242,189.187321675664,
189.270919509237,189.354651072098,189.434484910564,189.518231643266,189.601875320282,
189.685436064348,189.768933926305,189.852396426867,189.935841562359,190.019287397202,
190.10275199244,190.186305177862,190.269903011434,190.353634574296,190.433468412763,
190.517215145465,190.600858822481,190.684419566548,190.767917428504,190.851379929067,
190.934825064559,191.018270899402,191.10173549464,191.185288680062,191.268886513635,
191.352618076497,191.432451914962,191.551124929453,191.637151868979),
 .UNSPECIFIED.);
#444=B_SPLINE_CURVE_WITH_KNOTS('',3,(#53242,#53243,#53244,#53245,#53246,
#53247,#53248,#53249,#53250,#53251,#53252,#53253,#53254,#53255,#53256,#53257,
#53258,#53259,#53260,#53261,#53262,#53263,#53264,#53265,#53266,#53267,#53268,
#53269,#53270,#53271,#53272,#53273,#53274,#53275,#53276,#53277,#53278,#53279,
#53280,#53281,#53282,#53283,#53284,#53285,#53286,#53287,#53288,#53289,#53290,
#53291,#53292,#53293,#53294,#53295,#53296,#53297,#53298,#53299,#53300,#53301,
#53302,#53303,#53304,#53305,#53306,#53307,#53308,#53309,#53310,#53311,#53312,
#53313,#53314,#53315,#53316,#53317,#53318,#53319,#53320,#53321,#53322,#53323,
#53324,#53325,#53326,#53327,#53328,#53329,#53330,#53331,#53332,#53333,#53334,
#53335,#53336,#53337,#53338,#53339,#53340,#53341,#53342,#53343,#53344,#53345,
#53346,#53347,#53348,#53349,#53350,#53351,#53352,#53353,#53354,#53355,#53356,
#53357,#53358,#53359,#53360,#53361,#53362,#53363,#53364,#53365,#53366,#53367,
#53368,#53369,#53370,#53371,#53372,#53373,#53374,#53375,#53376,#53377,#53378,
#53379,#53380,#53381,#53382,#53383,#53384,#53385,#53386,#53387,#53388,#53389,
#53390,#53391,#53392,#53393,#53394,#53395,#53396,#53397,#53398,#53399,#53400,
#53401,#53402,#53403,#53404,#53405,#53406,#53407,#53408,#53409,#53410,#53411,
#53412,#53413,#53414,#53415,#53416,#53417,#53418,#53419,#53420,#53421,#53422,
#53423,#53424,#53425,#53426,#53427,#53428,#53429,#53430,#53431,#53432,#53433,
#53434,#53435,#53436,#53437,#53438,#53439,#53440,#53441,#53442,#53443,#53444,
#53445,#53446,#53447,#53448,#53449,#53450,#53451,#53452,#53453,#53454,#53455,
#53456,#53457,#53458,#53459,#53460,#53461,#53462,#53463,#53464,#53465,#53466,
#53467,#53468,#53469,#53470),.UNSPECIFIED.,.F.,.F.,(4,3,3,3,3,3,3,3,3,3,
3,3,3,3,3,3,3,3,3,3,3,3,3,3,3,3,3,3,3,3,3,3,3,3,3,3,3,3,3,3,3,3,3,3,3,3,
3,3,3,3,3,3,3,3,3,3,3,3,3,3,3,3,3,3,3,3,3,3,3,3,3,3,3,3,3,3,4),(191.637151869147,
191.719547380253,191.801875435602,191.884162988348,191.966430916099,192.04869821652,
192.13098388451,192.213354359001,192.295770900865,192.37831060723,192.431435417161,
192.515182149863,192.598825826879,192.682386570945,192.765884432902,192.849346933465,
192.932792068957,193.0162379038,193.099702499038,193.18325568446,193.266853518033,
193.350585080895,193.43041891936,193.514165652062,193.597809329078,193.681370073145,
193.764867935101,193.848330435664,193.931775571156,194.015221405999,194.098686001237,
194.182239186659,194.265837020232,194.349568583093,194.429402421559,194.513149154261,
194.596792831277,194.680353575344,194.7638514373,194.847313937863,194.930759073355,
195.014204908198,195.097669503436,195.181222688858,195.264820522431,195.348552085293,
195.428385923759,195.512132656461,195.595776333477,195.679337077543,195.7628349395,
195.846297440062,195.929742575555,196.013188410397,196.096653005635,196.180206191057,
196.26380402463,196.347535587492,196.427369425958,196.51111615866,196.594759835676,
196.678320579743,196.761818441699,196.845280942262,196.928726077754,197.012171912597,
197.095636507835,197.179189693257,197.262787526829,197.346519089691,197.426352928157,
197.514630471439,197.602752823588,197.690668233066,197.778459831919,197.866087611364,
197.920337175999),.UNSPECIFIED.);
#445=B_SPLINE_CURVE_WITH_KNOTS('',3,(#53472,#53473,#53474,#53475,#53476,
#53477,#53478,#53479,#53480,#53481,#53482,#53483,#53484,#53485,#53486,#53487,
#53488,#53489,#53490,#53491,#53492,#53493,#53494,#53495,#53496,#53497,#53498,
#53499,#53500,#53501,#53502,#53503,#53504,#53505,#53506,#53507,#53508,#53509,
#53510,#53511,#53512,#53513,#53514,#53515,#53516,#53517,#53518,#53519,#53520,
#53521,#53522,#53523,#53524,#53525,#53526,#53527,#53528,#53529,#53530,#53531,
#53532,#53533,#53534,#53535,#53536,#53537,#53538,#53539,#53540,#53541,#53542,
#53543,#53544,#53545,#53546,#53547,#53548,#53549,#53550,#53551,#53552,#53553,
#53554,#53555,#53556,#53557,#53558,#53559,#53560,#53561,#53562,#53563,#53564,
#53565,#53566,#53567,#53568,#53569,#53570,#53571,#53572,#53573,#53574,#53575,
#53576,#53577,#53578,#53579,#53580,#53581,#53582,#53583,#53584,#53585,#53586,
#53587,#53588,#53589,#53590,#53591,#53592,#53593,#53594,#53595,#53596,#53597,
#53598,#53599,#53600,#53601,#53602,#53603,#53604,#53605,#53606,#53607,#53608,
#53609,#53610,#53611,#53612,#53613,#53614,#53615,#53616,#53617,#53618,#53619,
#53620,#53621,#53622,#53623,#53624,#53625,#53626,#53627,#53628,#53629,#53630,
#53631,#53632,#53633,#53634,#53635,#53636,#53637,#53638,#53639,#53640,#53641,
#53642,#53643,#53644,#53645,#53646,#53647,#53648,#53649,#53650,#53651,#53652,
#53653,#53654,#53655,#53656,#53657,#53658,#53659,#53660,#53661,#53662,#53663,
#53664,#53665,#53666,#53667,#53668,#53669,#53670,#53671,#53672,#53673,#53674,
#53675,#53676,#53677,#53678,#53679,#53680,#53681,#53682,#53683,#53684,#53685,
#53686,#53687,#53688,#53689,#53690,#53691,#53692,#53693,#53694,#53695,#53696,
#53697,#53698,#53699,#53700),.UNSPECIFIED.,.F.,.F.,(4,3,3,3,3,3,3,3,3,3,
3,3,3,3,3,3,3,3,3,3,3,3,3,3,3,3,3,3,3,3,3,3,3,3,3,3,3,3,3,3,3,3,3,3,3,3,
3,3,3,3,3,3,3,3,3,3,3,3,3,3,3,3,3,3,3,3,3,3,3,3,3,3,3,3,3,3,4),(197.920337176158,
198.007548007661,198.09486648384,198.18238412104,198.270005973806,198.357827182688,
198.425336430356,198.509083163058,198.592726840074,198.67628758414,198.759785446097,
198.843247946659,198.926693082152,199.010138916995,199.093603512233,199.177156697654,
199.260754531227,199.344486094089,199.424319932555,199.508066665257,199.591710342273,
199.675271086339,199.758768948296,199.842231448859,199.925676584351,200.009122419193,
200.092587014432,200.176140199854,200.259738033426,200.343469596288,200.423303434754,
200.507050167456,200.590693844472,200.674254588539,200.757752450496,200.841214951058,
200.924660086551,201.008105921394,201.091570516632,201.175123702054,201.258721535626,
201.342453098488,201.422286936954,201.506033669656,201.589677346672,201.673238090738,
201.756735952695,201.840198453257,201.92364358875,202.007089423592,202.09055401883,
202.174107204252,202.257705037825,202.341436600687,202.421270439153,202.505017171855,
202.588660848871,202.672221592937,202.755719454895,202.839181955457,202.92262709095,
203.006072925792,203.089537521031,203.173090706453,203.256688540026,203.340420102887,
203.420253941352,203.502850512571,203.585343452099,203.667741244618,203.750085768299,
203.832396039394,203.91469104258,203.997017564991,204.079361312531,204.161778068112,
204.203522483236),.UNSPECIFIED.);
#446=B_SPLINE_CURVE_WITH_KNOTS('',3,(#53702,#53703,#53704,#53705,#53706,
#53707,#53708,#53709,#53710,#53711,#53712,#53713,#53714,#53715,#53716,#53717,
#53718,#53719,#53720,#53721,#53722,#53723,#53724,#53725,#53726,#53727,#53728,
#53729,#53730,#53731,#53732,#53733,#53734,#53735,#53736,#53737,#53738,#53739,
#53740,#53741,#53742,#53743,#53744,#53745,#53746,#53747,#53748,#53749,#53750,
#53751,#53752,#53753,#53754,#53755,#53756,#53757,#53758,#53759,#53760,#53761,
#53762,#53763,#53764,#53765,#53766,#53767,#53768,#53769,#53770,#53771,#53772,
#53773,#53774,#53775,#53776,#53777,#53778,#53779,#53780,#53781,#53782,#53783,
#53784,#53785,#53786,#53787,#53788,#53789,#53790,#53791,#53792,#53793,#53794,
#53795,#53796,#53797,#53798,#53799,#53800,#53801,#53802,#53803,#53804,#53805,
#53806,#53807,#53808,#53809,#53810,#53811,#53812,#53813,#53814,#53815,#53816,
#53817,#53818,#53819,#53820,#53821,#53822,#53823,#53824,#53825,#53826,#53827,
#53828,#53829,#53830,#53831,#53832,#53833,#53834,#53835,#53836,#53837,#53838,
#53839,#53840,#53841,#53842,#53843,#53844,#53845,#53846,#53847,#53848,#53849,
#53850,#53851,#53852,#53853,#53854,#53855,#53856,#53857,#53858,#53859,#53860,
#53861,#53862,#53863,#53864,#53865,#53866,#53867,#53868,#53869,#53870,#53871,
#53872,#53873,#53874,#53875,#53876,#53877,#53878,#53879,#53880,#53881,#53882,
#53883,#53884,#53885,#53886,#53887,#53888,#53889,#53890,#53891,#53892,#53893,
#53894,#53895,#53896,#53897,#53898,#53899,#53900,#53901,#53902,#53903,#53904,
#53905,#53906,#53907,#53908,#53909,#53910,#53911,#53912,#53913,#53914,#53915,
#53916,#53917,#53918,#53919,#53920,#53921,#53922,#53923,#53924,#53925,#53926,
#53927),.UNSPECIFIED.,.F.,.F.,(4,3,3,3,3,3,3,3,3,3,3,3,3,3,3,3,3,3,3,3,
3,3,3,3,3,3,3,3,3,3,3,3,3,3,3,3,3,3,3,3,3,3,3,3,3,3,3,3,3,3,3,3,3,3,3,3,
3,3,3,3,3,3,3,3,3,3,3,3,3,3,3,3,3,3,3,4),(204.203522483338,204.31924029561,
204.419237443551,204.502984176253,204.586627853269,204.670188597335,204.753686459292,
204.837148959855,204.920594095347,205.00403993019,205.087504525428,205.171057710849,
205.254655544422,205.338387107284,205.41822094575,205.501967678452,205.585611355468,
205.669172099535,205.752669961491,205.836132462054,205.919577597546,206.003023432389,
206.086488027627,206.170041213049,206.253639046622,206.337370609484,206.417204447949,
206.500951180651,206.584594857667,206.668155601733,206.75165346369,206.835115964253,
206.918561099745,207.002006934588,207.085471529826,207.169024715248,207.252622548821,
207.336354111683,207.416187950149,207.499934682851,207.583578359867,207.667139103933,
207.75063696589,207.834099466453,207.917544601945,208.000990436788,208.084455032026,
208.168008217448,208.251606051021,208.335337613883,208.415171452348,208.49891818505,
208.582561862066,208.666122606132,208.749620468089,208.833082968651,208.916528104144,
208.999973938986,209.083438534224,209.166991719646,209.250589553219,209.334321116081,
209.414154954547,209.497901687249,209.581545364265,209.665106108331,209.748603970288,
209.83206647085,209.915511606343,209.998957441185,210.082422036423,210.165975221845,
210.249573055418,210.33330461828,210.413138456746,210.486707790517),
 .UNSPECIFIED.);
#447=B_SPLINE_CURVE_WITH_KNOTS('',3,(#53929,#53930,#53931,#53932,#53933,
#53934,#53935,#53936,#53937,#53938,#53939,#53940,#53941,#53942,#53943,#53944,
#53945,#53946,#53947,#53948,#53949,#53950,#53951,#53952,#53953,#53954,#53955,
#53956,#53957,#53958,#53959,#53960,#53961,#53962,#53963,#53964,#53965,#53966,
#53967,#53968,#53969,#53970,#53971,#53972,#53973,#53974,#53975,#53976,#53977,
#53978,#53979,#53980,#53981,#53982,#53983,#53984,#53985,#53986,#53987,#53988,
#53989,#53990,#53991,#53992,#53993,#53994,#53995,#53996,#53997,#53998,#53999,
#54000,#54001,#54002,#54003,#54004,#54005,#54006,#54007,#54008,#54009,#54010,
#54011,#54012,#54013,#54014,#54015,#54016,#54017,#54018,#54019,#54020,#54021,
#54022,#54023,#54024,#54025,#54026,#54027,#54028,#54029,#54030,#54031,#54032,
#54033,#54034,#54035,#54036,#54037,#54038,#54039,#54040,#54041,#54042,#54043,
#54044,#54045,#54046,#54047,#54048,#54049,#54050,#54051,#54052,#54053,#54054,
#54055,#54056,#54057,#54058,#54059,#54060,#54061,#54062,#54063,#54064,#54065,
#54066,#54067,#54068,#54069,#54070,#54071,#54072,#54073,#54074,#54075,#54076,
#54077,#54078,#54079,#54080,#54081,#54082,#54083,#54084,#54085,#54086,#54087,
#54088,#54089,#54090,#54091,#54092,#54093,#54094,#54095,#54096,#54097,#54098,
#54099,#54100,#54101,#54102,#54103,#54104,#54105,#54106,#54107,#54108,#54109,
#54110,#54111,#54112,#54113,#54114,#54115,#54116,#54117,#54118,#54119,#54120,
#54121,#54122,#54123,#54124,#54125,#54126,#54127,#54128,#54129,#54130,#54131,
#54132,#54133,#54134,#54135,#54136,#54137,#54138,#54139,#54140,#54141,#54142,
#54143,#54144,#54145,#54146,#54147,#54148,#54149,#54150,#54151,#54152,#54153,
#54154,#54155,#54156,#54157),.UNSPECIFIED.,.F.,.F.,(4,3,3,3,3,3,3,3,3,3,
3,3,3,3,3,3,3,3,3,3,3,3,3,3,3,3,3,3,3,3,3,3,3,3,3,3,3,3,3,3,3,3,3,3,3,3,
3,3,3,3,3,3,3,3,3,3,3,3,3,3,3,3,3,3,3,3,3,3,3,3,3,3,3,3,3,3,4),(210.486707790642,
210.569565422792,210.652326204392,210.735011045307,210.819649909511,210.902254524363,
210.984850690515,211.067457184152,211.15362337785,211.236351979121,211.319136610094,
211.40203416377,211.412121958945,211.495868691647,211.579512368663,211.663073112729,
211.746570974686,211.830033475249,211.913478610741,211.996924445583,212.080389040822,
212.163942226243,212.247540059816,212.331271622678,212.411105461144,212.494852193846,
212.578495870862,212.662056614928,212.745554476885,212.829016977448,212.91246211294,
212.995907947783,213.079372543021,213.162925728443,213.246523562016,213.330255124878,
213.410088963344,213.493835696046,213.577479373062,213.661040117129,213.744537979085,
213.828000479648,213.91144561514,213.994891449983,214.078356045221,214.161909230643,
214.245507064216,214.329238627077,214.409072465543,214.492819198245,214.576462875261,
214.660023619327,214.743521481284,214.826983981846,214.910429117338,214.993874952181,
215.077339547419,215.160892732841,215.244490566414,215.328222129275,215.408055967742,
215.491802700444,215.57544637746,215.659007121526,215.742504983482,215.825967484045,
215.909412619537,215.99285845438,216.076323049618,216.15987623504,216.243474068613,
216.327205631475,216.407039469941,216.502776262836,216.598179185216,216.692942127072,
216.769893097501),.UNSPECIFIED.);
#448=B_SPLINE_CURVE_WITH_KNOTS('',3,(#54159,#54160,#54161,#54162,#54163,
#54164,#54165,#54166,#54167,#54168,#54169,#54170,#54171,#54172,#54173,#54174,
#54175,#54176,#54177,#54178,#54179,#54180,#54181,#54182,#54183,#54184,#54185,
#54186,#54187,#54188,#54189,#54190,#54191,#54192,#54193,#54194,#54195,#54196,
#54197,#54198,#54199,#54200,#54201,#54202,#54203,#54204,#54205,#54206,#54207,
#54208,#54209,#54210,#54211,#54212,#54213,#54214,#54215,#54216,#54217,#54218,
#54219,#54220,#54221,#54222,#54223,#54224,#54225,#54226,#54227,#54228,#54229,
#54230,#54231,#54232,#54233,#54234,#54235,#54236,#54237,#54238,#54239,#54240,
#54241,#54242,#54243,#54244,#54245,#54246,#54247,#54248,#54249,#54250,#54251,
#54252,#54253,#54254,#54255,#54256,#54257,#54258,#54259,#54260,#54261,#54262,
#54263,#54264,#54265,#54266,#54267,#54268,#54269,#54270,#54271,#54272,#54273,
#54274,#54275,#54276,#54277,#54278,#54279,#54280,#54281,#54282,#54283,#54284,
#54285,#54286,#54287,#54288,#54289,#54290,#54291,#54292,#54293,#54294,#54295,
#54296,#54297,#54298,#54299,#54300,#54301,#54302,#54303,#54304,#54305,#54306,
#54307,#54308,#54309,#54310,#54311,#54312,#54313,#54314,#54315,#54316,#54317,
#54318,#54319,#54320,#54321,#54322,#54323,#54324,#54325,#54326,#54327,#54328,
#54329,#54330,#54331,#54332,#54333,#54334,#54335,#54336,#54337,#54338,#54339,
#54340,#54341,#54342,#54343,#54344,#54345,#54346,#54347,#54348,#54349,#54350,
#54351,#54352,#54353,#54354,#54355,#54356,#54357,#54358,#54359,#54360,#54361,
#54362,#54363,#54364,#54365,#54366,#54367,#54368,#54369,#54370,#54371,#54372,
#54373,#54374,#54375,#54376,#54377,#54378,#54379,#54380,#54381,#54382,#54383,
#54384,#54385,#54386,#54387),.UNSPECIFIED.,.F.,.F.,(4,3,3,3,3,3,3,3,3,3,
3,3,3,3,3,3,3,3,3,3,3,3,3,3,3,3,3,3,3,3,3,3,3,3,3,3,3,3,3,3,3,3,3,3,3,3,
3,3,3,3,3,3,3,3,3,3,3,3,3,3,3,3,3,3,3,3,3,3,3,3,3,3,3,3,3,3,4),(216.769893097697,
216.853753653658,216.937615196081,217.021495195232,217.105411129513,217.189432867041,
217.273513283251,217.357729007605,217.40602297214,217.489769704842,217.573413381858,
217.656974125925,217.740471987882,217.823934488444,217.907379623937,217.990825458779,
218.074290054018,218.15784323944,218.241441073012,218.325172635874,218.405006474339,
218.488753207041,218.572396884057,218.655957628123,218.73945549008,218.822917990643,
218.906363126135,218.989808960978,219.073273556216,219.156826741638,219.240424575211,
219.324156138073,219.403989976539,219.487736709241,219.571380386257,219.654941130323,
219.73843899228,219.821901492842,219.905346628335,219.988792463178,220.072257058416,
220.155810243838,220.239408077411,220.323139640272,220.402973478738,220.48672021144,
220.570363888456,220.653924632522,220.737422494479,220.820884995042,220.904330130534,
220.987775965377,221.071240560615,221.154793746037,221.238391579609,221.322123142471,
221.401956980937,221.485703713639,221.569347390655,221.652908134721,221.736405996678,
221.819868497241,221.903313632733,221.986759467576,222.070224062814,222.153777248236,
222.237375081809,222.321106644671,222.400940483136,222.484857460097,222.568672010861,
222.652402128444,222.736065743995,222.819682620366,222.903270791918,222.986866456813,
223.053078404877),.UNSPECIFIED.);
#449=B_SPLINE_CURVE_WITH_KNOTS('',3,(#54389,#54390,#54391,#54392,#54393,
#54394,#54395,#54396,#54397,#54398),.UNSPECIFIED.,.F.,.F.,(4,1,1,1,1,1,
1,4),(223.05308597169,223.399923985335,224.398907487534,225.397890989734,
226.396874491933,227.395857994132,228.394841496331,229.336256643204),
 .UNSPECIFIED.);
#450=B_SPLINE_CURVE_WITH_KNOTS('',3,(#54400,#54401,#54402,#54403,#54404,
#54405,#54406,#54407,#54408,#54409,#54410,#54411,#54412,#54413,#54414,#54415,
#54416,#54417,#54418,#54419,#54420,#54421,#54422,#54423,#54424,#54425,#54426,
#54427,#54428,#54429,#54430,#54431,#54432,#54433,#54434,#54435,#54436,#54437,
#54438,#54439,#54440,#54441,#54442,#54443,#54444,#54445,#54446,#54447,#54448,
#54449,#54450,#54451,#54452,#54453,#54454,#54455,#54456,#54457,#54458,#54459,
#54460,#54461,#54462,#54463,#54464,#54465,#54466,#54467,#54468,#54469,#54470,
#54471,#54472,#54473,#54474,#54475,#54476,#54477,#54478,#54479,#54480,#54481,
#54482,#54483,#54484,#54485,#54486,#54487,#54488,#54489,#54490,#54491,#54492,
#54493,#54494,#54495,#54496,#54497,#54498,#54499,#54500,#54501,#54502,#54503,
#54504,#54505,#54506,#54507,#54508,#54509,#54510,#54511,#54512,#54513,#54514,
#54515,#54516,#54517,#54518,#54519,#54520,#54521,#54522,#54523,#54524,#54525,
#54526,#54527,#54528,#54529,#54530,#54531,#54532,#54533,#54534,#54535,#54536,
#54537,#54538,#54539,#54540,#54541,#54542,#54543,#54544,#54545,#54546,#54547,
#54548,#54549,#54550,#54551,#54552,#54553,#54554,#54555,#54556,#54557,#54558,
#54559,#54560,#54561,#54562,#54563,#54564,#54565,#54566,#54567,#54568,#54569,
#54570,#54571,#54572,#54573,#54574,#54575,#54576,#54577,#54578,#54579,#54580,
#54581,#54582,#54583,#54584,#54585,#54586,#54587,#54588,#54589,#54590,#54591,
#54592,#54593,#54594,#54595,#54596,#54597,#54598,#54599,#54600,#54601,#54602,
#54603,#54604,#54605,#54606,#54607,#54608,#54609,#54610,#54611,#54612,#54613,
#54614,#54615,#54616,#54617,#54618,#54619,#54620,#54621,#54622,#54623,#54624,
#54625),.UNSPECIFIED.,.F.,.F.,(4,3,3,3,3,3,3,3,3,3,3,3,3,3,3,3,3,3,3,3,
3,3,3,3,3,3,3,3,3,3,3,3,3,3,3,3,3,3,3,3,3,3,3,3,3,3,3,3,3,3,3,3,3,3,3,3,
3,3,3,3,3,3,3,3,3,3,3,3,3,3,3,3,3,3,3,4),(229.336263712056,229.39382499853,
229.477571731232,229.561215408248,229.644776152314,229.728274014271,229.811736514833,
229.895181650326,229.978627485168,230.062092080407,230.145645265828,230.229243099401,
230.312974662263,230.392808500729,230.476555233431,230.560198910447,230.643759654514,
230.72725751647,230.810720017033,230.894165152525,230.977610987368,231.061075582606,
231.144628768028,231.228226601601,231.311958164463,231.391792002929,231.475538735631,
231.559182412647,231.642743156713,231.72624101867,231.809703519233,231.893148654725,
231.976594489568,232.060059084806,232.143612270228,232.2272101038,232.310941666662,
232.390775505128,232.47452223783,232.558165914846,232.641726658912,232.725224520869,
232.808687021432,232.892132156924,232.975577991767,233.059042587005,233.142595772427,
233.226193605999,233.309925168861,233.389759007327,233.473505740029,233.557149417045,
233.640710161111,233.724208023068,233.80767052363,233.891115659123,233.974561493965,
234.058026089203,234.141579274625,234.225177108198,234.30890867106,234.388742509526,
234.472489242228,234.556132919244,234.63969366331,234.723191525267,234.80665402583,
234.890099161322,234.973544996165,235.057009591403,235.140562776825,235.224160610397,
235.307892173259,235.387726011725,235.50358751548,235.619449019236),
 .UNSPECIFIED.);
#451=B_SPLINE_CURVE_WITH_KNOTS('',3,(#54627,#54628,#54629,#54630,#54631,
#54632,#54633,#54634,#54635,#54636,#54637,#54638,#54639,#54640,#54641,#54642,
#54643,#54644,#54645,#54646,#54647,#54648,#54649,#54650,#54651,#54652,#54653,
#54654,#54655,#54656,#54657,#54658,#54659,#54660,#54661,#54662,#54663,#54664,
#54665,#54666,#54667,#54668,#54669,#54670,#54671,#54672,#54673,#54674,#54675,
#54676,#54677,#54678,#54679,#54680,#54681,#54682,#54683,#54684,#54685,#54686,
#54687,#54688,#54689,#54690,#54691,#54692,#54693,#54694,#54695,#54696,#54697,
#54698,#54699,#54700,#54701,#54702,#54703,#54704,#54705,#54706,#54707,#54708,
#54709,#54710,#54711,#54712,#54713,#54714,#54715,#54716,#54717,#54718,#54719,
#54720,#54721,#54722,#54723,#54724,#54725,#54726,#54727,#54728,#54729,#54730,
#54731,#54732,#54733,#54734,#54735,#54736,#54737,#54738,#54739,#54740,#54741,
#54742,#54743,#54744,#54745,#54746,#54747,#54748,#54749,#54750,#54751,#54752,
#54753,#54754,#54755,#54756,#54757,#54758,#54759,#54760,#54761,#54762,#54763,
#54764,#54765,#54766,#54767,#54768,#54769,#54770,#54771,#54772,#54773,#54774,
#54775,#54776,#54777,#54778,#54779,#54780,#54781,#54782,#54783,#54784,#54785,
#54786,#54787,#54788,#54789,#54790,#54791,#54792,#54793,#54794,#54795,#54796,
#54797,#54798,#54799,#54800,#54801,#54802,#54803,#54804,#54805,#54806,#54807,
#54808,#54809,#54810,#54811,#54812,#54813,#54814,#54815,#54816,#54817,#54818,
#54819,#54820,#54821,#54822,#54823,#54824,#54825,#54826,#54827,#54828,#54829,
#54830,#54831,#54832,#54833,#54834,#54835,#54836,#54837,#54838,#54839,#54840,
#54841,#54842,#54843,#54844,#54845,#54846,#54847,#54848,#54849,#54850,#54851,
#54852,#54853,#54854,#54855),.UNSPECIFIED.,.F.,.F.,(4,3,3,3,3,3,3,3,3,3,
3,3,3,3,3,3,3,3,3,3,3,3,3,3,3,3,3,3,3,3,3,3,3,3,3,3,3,3,3,3,3,3,3,3,3,3,
3,3,3,3,3,3,3,3,3,3,3,3,3,3,3,3,3,3,3,3,3,3,3,3,3,3,3,3,3,3,4),(235.619449019367,
235.701928974608,235.787526542023,235.869916952055,235.952295875165,236.034682232197,
236.117094947374,236.199596927949,236.282152013071,236.364822636091,236.386709513924,
236.470456246626,236.554099923642,236.637660667708,236.721158529665,236.804621030228,
236.88806616572,236.971512000563,237.054976595801,237.138529781223,237.222127614796,
237.305859177658,237.385693016124,237.469439748826,237.553083425842,237.636644169909,
237.720142031865,237.803604532428,237.88704966792,237.970495502763,238.053960098001,
238.137513283423,238.221111116996,238.304842679858,238.384676518323,238.468423251025,
238.552066928041,238.635627672107,238.719125534064,238.802588034626,238.886033170119,
238.969479004961,239.0529436002,239.136496785621,239.220094619194,239.303826182056,
239.383660020522,239.467406753224,239.55105043024,239.634611174306,239.718109036263,
239.801571536825,239.885016672318,239.968462507161,240.051927102398,240.13548028782,
240.219078121393,240.302809684255,240.382643522721,240.466390255423,240.550033932439,
240.633594676506,240.717092538462,240.800555039025,240.884000174517,240.96744600936,
241.050910604598,241.13446379002,241.218061623593,241.301793186454,241.38162702492,
241.468881254052,241.555995737591,241.642932265323,241.729764964557,241.816468207509,
241.902634326415),.UNSPECIFIED.);
#452=B_SPLINE_CURVE_WITH_KNOTS('',3,(#54857,#54858,#54859,#54860,#54861,
#54862,#54863,#54864,#54865,#54866,#54867,#54868,#54869,#54870,#54871,#54872,
#54873,#54874,#54875,#54876,#54877,#54878,#54879,#54880,#54881,#54882,#54883,
#54884,#54885,#54886,#54887,#54888,#54889,#54890,#54891,#54892,#54893,#54894,
#54895,#54896,#54897,#54898,#54899,#54900,#54901,#54902,#54903,#54904,#54905,
#54906,#54907,#54908,#54909,#54910,#54911,#54912,#54913,#54914,#54915,#54916,
#54917,#54918,#54919,#54920,#54921,#54922,#54923,#54924,#54925,#54926,#54927,
#54928,#54929,#54930,#54931,#54932,#54933,#54934,#54935,#54936,#54937,#54938,
#54939,#54940,#54941,#54942,#54943,#54944,#54945,#54946,#54947,#54948,#54949,
#54950,#54951,#54952,#54953,#54954,#54955,#54956,#54957,#54958,#54959,#54960,
#54961,#54962,#54963,#54964,#54965,#54966,#54967,#54968,#54969,#54970,#54971,
#54972,#54973,#54974,#54975,#54976,#54977,#54978,#54979,#54980,#54981,#54982,
#54983,#54984,#54985,#54986,#54987,#54988,#54989,#54990,#54991,#54992,#54993,
#54994,#54995,#54996,#54997,#54998,#54999,#55000,#55001,#55002,#55003,#55004,
#55005,#55006,#55007,#55008,#55009,#55010,#55011,#55012,#55013,#55014,#55015,
#55016,#55017,#55018,#55019,#55020,#55021,#55022,#55023,#55024,#55025,#55026,
#55027,#55028,#55029,#55030,#55031,#55032,#55033,#55034,#55035,#55036,#55037,
#55038,#55039,#55040,#55041,#55042,#55043,#55044,#55045,#55046,#55047,#55048,
#55049,#55050,#55051,#55052,#55053,#55054,#55055,#55056,#55057,#55058,#55059,
#55060,#55061,#55062,#55063,#55064,#55065,#55066,#55067,#55068,#55069,#55070,
#55071,#55072,#55073,#55074,#55075,#55076,#55077,#55078,#55079,#55080,#55081,
#55082,#55083,#55084,#55085),.UNSPECIFIED.,.F.,.F.,(4,3,3,3,3,3,3,3,3,3,
3,3,3,3,3,3,3,3,3,3,3,3,3,3,3,3,3,3,3,3,3,3,3,3,3,3,3,3,3,3,3,3,3,3,3,3,
3,3,3,3,3,3,3,3,3,3,3,3,3,3,3,3,3,3,3,3,3,3,3,3,3,3,3,3,3,3,4),(241.902634326614,
241.990863900032,242.079239902703,242.167853017759,242.256595129932,242.345544125978,
242.380610527119,242.464357259821,242.548000936837,242.631561680904,242.71505954286,
242.798522043423,242.881967178915,242.965413013758,243.048877608996,243.132430794418,
243.216028627991,243.299760190852,243.379594029319,243.463340762021,243.546984439037,
243.630545183103,243.71404304506,243.797505545623,243.880950681115,243.964396515958,
244.047861111196,244.131414296618,244.21501213019,244.298743693052,244.378577531518,
244.46232426422,244.545967941236,244.629528685302,244.713026547259,244.796489047822,
244.879934183314,244.963380018157,245.046844613395,245.130397798817,245.213995632389,
245.297727195251,245.377561033717,245.461307766419,245.544951443435,245.628512187501,
245.712010049458,245.795472550021,245.878917685513,245.962363520356,246.045828115594,
246.129381301015,246.212979134588,246.29671069745,246.376544535916,246.460291268618,
246.543934945634,246.6274956897,246.710993551657,246.79445605222,246.877901187712,
246.961347022555,247.044811617793,247.128364803215,247.211962636788,247.295694199649,
247.375528038115,247.458043982855,247.54045702969,247.622776737558,247.705044162818,
247.787278368309,247.869498385905,247.951756669092,248.034032929656,248.116396974214,
248.185819633464),.UNSPECIFIED.);
#453=B_SPLINE_CURVE_WITH_KNOTS('',3,(#55087,#55088,#55089,#55090,#55091,
#55092,#55093,#55094,#55095,#55096,#55097,#55098,#55099,#55100,#55101,#55102,
#55103,#55104,#55105,#55106,#55107,#55108,#55109,#55110,#55111,#55112,#55113,
#55114,#55115,#55116,#55117,#55118,#55119,#55120,#55121,#55122,#55123,#55124,
#55125,#55126,#55127,#55128,#55129,#55130,#55131,#55132,#55133,#55134,#55135,
#55136,#55137,#55138,#55139,#55140,#55141,#55142,#55143,#55144,#55145,#55146,
#55147,#55148,#55149,#55150,#55151,#55152,#55153,#55154,#55155,#55156,#55157,
#55158,#55159,#55160,#55161,#55162,#55163,#55164,#55165,#55166,#55167,#55168,
#55169,#55170,#55171,#55172,#55173,#55174,#55175,#55176,#55177,#55178,#55179,
#55180,#55181,#55182,#55183,#55184,#55185,#55186,#55187,#55188,#55189,#55190,
#55191,#55192,#55193,#55194,#55195,#55196,#55197,#55198,#55199,#55200,#55201,
#55202,#55203,#55204,#55205,#55206,#55207,#55208,#55209,#55210,#55211,#55212,
#55213,#55214,#55215,#55216,#55217,#55218,#55219,#55220,#55221,#55222,#55223,
#55224,#55225,#55226,#55227,#55228,#55229,#55230,#55231,#55232,#55233,#55234,
#55235,#55236,#55237,#55238,#55239,#55240,#55241,#55242,#55243,#55244,#55245,
#55246,#55247,#55248,#55249,#55250,#55251,#55252,#55253,#55254,#55255,#55256,
#55257,#55258,#55259,#55260,#55261,#55262,#55263,#55264,#55265,#55266,#55267,
#55268,#55269,#55270,#55271,#55272,#55273,#55274,#55275,#55276,#55277,#55278,
#55279,#55280,#55281,#55282,#55283,#55284,#55285,#55286,#55287,#55288,#55289,
#55290,#55291,#55292,#55293,#55294,#55295,#55296,#55297,#55298,#55299,#55300,
#55301,#55302,#55303,#55304,#55305,#55306,#55307,#55308,#55309,#55310,#55311,
#55312),.UNSPECIFIED.,.F.,.F.,(4,3,3,3,3,3,3,3,3,3,3,3,3,3,3,3,3,3,3,3,
3,3,3,3,3,3,3,3,3,3,3,3,3,3,3,3,3,3,3,3,3,3,3,3,3,3,3,3,3,3,3,3,3,3,3,3,
3,3,3,3,3,3,3,3,3,3,3,3,3,3,3,3,3,3,3,4),(248.185819633595,248.309579357114,
248.374511540314,248.458258273016,248.541901950032,248.625462694098,248.708960556055,
248.792423056618,248.87586819211,248.959314026953,249.042778622192,249.126331807613,
249.209929641186,249.293661204048,249.373495042514,249.457241775216,249.540885452232,
249.624446196298,249.707944058255,249.791406558818,249.87485169431,249.958297529153,
250.041762124391,250.125315309813,250.208913143386,250.292644706248,250.372478544713,
250.456225277415,250.539868954431,250.623429698497,250.706927560454,250.790390061016,
250.873835196508,250.957281031351,251.040745626589,251.124298812011,251.207896645583,
251.291628208445,251.371462046912,251.455208779614,251.53885245663,251.622413200696,
251.705911062653,251.789373563216,251.872818698708,251.956264533551,252.039729128789,
252.123282314211,252.206880147784,252.290611710646,252.370445549111,252.454192281813,
252.537835958829,252.621396702895,252.704894564852,252.788357065414,252.871802200907,
252.955248035749,253.038712630987,253.122265816409,253.205863649982,253.289595212844,
253.36942905131,253.453175784012,253.536819461028,253.620380205095,253.703878067051,
253.787340567614,253.870785703106,253.954231537949,254.037696133187,254.121249318609,
254.204847152182,254.288578715044,254.368412553509,254.469004940774),
 .UNSPECIFIED.);
#454=B_SPLINE_CURVE_WITH_KNOTS('',3,(#55314,#55315,#55316,#55317,#55318,
#55319,#55320,#55321,#55322,#55323,#55324,#55325,#55326,#55327,#55328,#55329,
#55330,#55331,#55332,#55333,#55334,#55335,#55336,#55337,#55338,#55339,#55340,
#55341,#55342,#55343,#55344,#55345,#55346,#55347,#55348,#55349,#55350,#55351,
#55352,#55353,#55354,#55355,#55356,#55357,#55358,#55359,#55360,#55361,#55362,
#55363,#55364,#55365,#55366,#55367,#55368,#55369,#55370,#55371,#55372,#55373,
#55374,#55375,#55376,#55377,#55378,#55379,#55380,#55381,#55382,#55383,#55384,
#55385,#55386,#55387,#55388,#55389,#55390,#55391,#55392,#55393,#55394,#55395,
#55396,#55397,#55398,#55399,#55400,#55401,#55402,#55403,#55404,#55405,#55406,
#55407,#55408,#55409,#55410,#55411,#55412,#55413,#55414,#55415,#55416,#55417,
#55418,#55419,#55420,#55421,#55422,#55423,#55424,#55425,#55426,#55427,#55428,
#55429,#55430,#55431,#55432,#55433,#55434,#55435,#55436,#55437,#55438,#55439,
#55440,#55441,#55442,#55443,#55444,#55445,#55446,#55447,#55448,#55449,#55450,
#55451,#55452,#55453,#55454,#55455,#55456,#55457,#55458,#55459,#55460,#55461,
#55462,#55463,#55464,#55465,#55466,#55467,#55468,#55469,#55470,#55471,#55472,
#55473,#55474,#55475,#55476,#55477,#55478,#55479,#55480,#55481,#55482,#55483,
#55484,#55485,#55486,#55487,#55488,#55489,#55490,#55491,#55492,#55493,#55494,
#55495,#55496,#55497,#55498,#55499,#55500,#55501,#55502,#55503,#55504,#55505,
#55506,#55507,#55508,#55509,#55510,#55511,#55512,#55513,#55514,#55515,#55516,
#55517,#55518,#55519,#55520,#55521,#55522,#55523,#55524,#55525,#55526,#55527,
#55528,#55529,#55530,#55531,#55532,#55533,#55534,#55535,#55536,#55537,#55538,
#55539,#55540,#55541,#55542),.UNSPECIFIED.,.F.,.F.,(4,3,3,3,3,3,3,3,3,3,
3,3,3,3,3,3,3,3,3,3,3,3,3,3,3,3,3,3,3,3,3,3,3,3,3,3,3,3,3,3,3,3,3,3,3,3,
3,3,3,3,3,3,3,3,3,3,3,3,3,3,3,3,3,3,3,3,3,3,3,3,3,3,3,3,3,3,4),(254.469004940909,
254.551650520092,254.634203710762,254.716685552544,254.799121637284,254.881534416937,
254.96394280165,255.046365695572,255.128871881607,255.211420494891,255.294098388882,
255.367396055709,255.451142788411,255.534786465427,255.618347209493,255.70184507145,
255.785307572013,255.868752707505,255.952198542348,256.035663137586,256.119216323008,
256.202814156581,256.286545719443,256.366379557908,256.45012629061,256.533769967626,
256.617330711692,256.700828573648,256.784291074211,256.867736209703,256.951182044546,
257.034646639784,257.118199825206,257.201797658778,257.28552922164,257.365363060107,
257.449109792809,257.532753469825,257.616314213891,257.699812075848,257.783274576411,
257.866719711903,257.950165546746,258.033630141984,258.117183327406,258.200781160979,
258.284512723841,258.364346562306,258.448093295008,258.531736972024,258.61529771609,
258.698795578046,258.782258078609,258.865703214101,258.949149048944,259.032613644182,
259.116166829604,259.199764663176,259.283496226038,259.363330064505,259.447076797207,
259.530720474223,259.614281218289,259.697779080246,259.781241580809,259.864686716301,
259.948132551144,260.031597146382,260.115150331804,260.198748165377,260.282479728238,
260.362313566704,260.45978273697,260.553217387915,260.646361478217,260.73906526939,
260.752190247769),.UNSPECIFIED.);
#455=B_SPLINE_CURVE_WITH_KNOTS('',3,(#55544,#55545,#55546,#55547,#55548,
#55549,#55550,#55551,#55552,#55553,#55554,#55555,#55556,#55557,#55558,#55559,
#55560,#55561,#55562,#55563,#55564,#55565,#55566,#55567,#55568,#55569,#55570,
#55571,#55572,#55573,#55574,#55575,#55576,#55577,#55578,#55579,#55580,#55581,
#55582,#55583,#55584,#55585,#55586,#55587,#55588,#55589,#55590,#55591,#55592,
#55593,#55594,#55595,#55596,#55597,#55598,#55599,#55600,#55601,#55602,#55603,
#55604,#55605,#55606,#55607,#55608,#55609,#55610,#55611,#55612,#55613,#55614,
#55615,#55616,#55617,#55618,#55619,#55620,#55621,#55622,#55623,#55624,#55625,
#55626,#55627,#55628,#55629,#55630,#55631,#55632,#55633,#55634,#55635,#55636,
#55637,#55638,#55639,#55640,#55641,#55642,#55643,#55644,#55645,#55646,#55647,
#55648,#55649,#55650,#55651,#55652,#55653,#55654,#55655,#55656,#55657,#55658,
#55659,#55660,#55661,#55662,#55663,#55664,#55665,#55666,#55667,#55668,#55669,
#55670,#55671,#55672,#55673,#55674,#55675,#55676,#55677,#55678,#55679,#55680,
#55681,#55682,#55683,#55684,#55685,#55686,#55687,#55688,#55689,#55690,#55691,
#55692,#55693,#55694,#55695,#55696,#55697,#55698,#55699,#55700,#55701,#55702,
#55703,#55704,#55705,#55706,#55707,#55708,#55709,#55710,#55711,#55712,#55713,
#55714,#55715,#55716,#55717,#55718,#55719,#55720,#55721,#55722,#55723,#55724,
#55725,#55726,#55727,#55728,#55729,#55730,#55731,#55732,#55733,#55734,#55735,
#55736,#55737,#55738,#55739,#55740,#55741,#55742,#55743,#55744,#55745,#55746,
#55747,#55748,#55749,#55750,#55751,#55752,#55753,#55754,#55755,#55756,#55757,
#55758,#55759,#55760,#55761,#55762,#55763,#55764,#55765,#55766,#55767,#55768,
#55769,#55770,#55771,#55772),.UNSPECIFIED.,.F.,.F.,(4,3,3,3,3,3,3,3,3,3,
3,3,3,3,3,3,3,3,3,3,3,3,3,3,3,3,3,3,3,3,3,3,3,3,3,3,3,3,3,3,3,3,3,3,3,3,
3,3,3,3,3,3,3,3,3,3,3,3,3,3,3,3,3,3,3,3,3,3,3,3,3,3,3,3,3,3,4),(260.752190247954,
260.836557566651,260.920941027191,261.005357334773,261.08982321306,261.174405754682,
261.259057630092,261.343841100169,261.361297068904,261.445043801606,261.528687478622,
261.612248222688,261.695746084645,261.779208585207,261.8626537207,261.946099555542,
262.02956415078,262.113117336202,262.196715169775,262.280446732637,262.360280571103,
262.444027303805,262.527670980821,262.611231724887,262.694729586844,262.778192087407,
262.861637222899,262.945083057742,263.02854765298,263.112100838401,263.195698671974,
263.279430234836,263.359264073302,263.443010806004,263.52665448302,263.610215227086,
263.693713089043,263.777175589605,263.860620725097,263.94406655994,264.027531155178,
264.1110843406,264.194682174172,264.278413737034,264.358247575501,264.441994308203,
264.525637985219,264.609198729286,264.692696591243,264.776159091805,264.859604227298,
264.943050062141,265.026514657379,265.110067842801,265.193665676373,265.277397239235,
265.3572310777,265.440977810402,265.524621487418,265.608182231484,265.691680093441,
265.775142594003,265.858587729496,265.942033564339,266.025498159577,266.109051344999,
266.192649178571,266.276380741433,266.356214579899,266.441109701803,266.524506460389,
266.607823017449,266.69107772501,266.777152182541,266.860346617411,266.947861086272,
267.035375555133),.UNSPECIFIED.);
#456=B_SPLINE_CURVE_WITH_KNOTS('',3,(#55774,#55775,#55776,#55777,#55778,
#55779,#55780,#55781,#55782,#55783,#55784,#55785,#55786,#55787,#55788,#55789,
#55790,#55791,#55792,#55793,#55794,#55795,#55796,#55797,#55798,#55799,#55800,
#55801,#55802,#55803,#55804,#55805,#55806,#55807,#55808,#55809,#55810,#55811,
#55812,#55813,#55814,#55815,#55816,#55817,#55818,#55819,#55820,#55821,#55822,
#55823,#55824,#55825,#55826,#55827,#55828,#55829,#55830,#55831,#55832,#55833,
#55834,#55835,#55836,#55837,#55838,#55839,#55840,#55841,#55842,#55843,#55844,
#55845,#55846,#55847,#55848,#55849,#55850,#55851,#55852,#55853,#55854,#55855,
#55856,#55857,#55858,#55859,#55860,#55861,#55862,#55863,#55864,#55865,#55866,
#55867,#55868,#55869,#55870,#55871,#55872,#55873,#55874,#55875,#55876,#55877,
#55878,#55879,#55880,#55881,#55882,#55883,#55884,#55885,#55886,#55887,#55888,
#55889,#55890,#55891,#55892,#55893,#55894,#55895,#55896,#55897,#55898,#55899,
#55900,#55901,#55902,#55903,#55904,#55905,#55906,#55907,#55908,#55909,#55910,
#55911,#55912,#55913,#55914,#55915,#55916,#55917,#55918,#55919,#55920,#55921,
#55922,#55923,#55924,#55925,#55926,#55927,#55928,#55929,#55930,#55931,#55932,
#55933,#55934,#55935,#55936,#55937,#55938,#55939,#55940,#55941,#55942,#55943,
#55944,#55945,#55946,#55947,#55948,#55949,#55950,#55951,#55952,#55953,#55954,
#55955,#55956,#55957,#55958,#55959,#55960,#55961,#55962,#55963,#55964,#55965,
#55966,#55967,#55968,#55969,#55970,#55971,#55972,#55973,#55974,#55975,#55976,
#55977,#55978,#55979,#55980,#55981,#55982,#55983,#55984,#55985,#55986,#55987,
#55988,#55989,#55990,#55991,#55992,#55993,#55994,#55995,#55996,#55997,#55998,
#55999,#56000,#56001,#56002),.UNSPECIFIED.,.F.,.F.,(4,3,3,3,3,3,3,3,3,3,
3,3,3,3,3,3,3,3,3,3,3,3,3,3,3,3,3,3,3,3,3,3,3,3,3,3,3,3,3,3,3,3,3,3,3,3,
3,3,3,3,3,3,3,3,3,3,3,3,3,3,3,3,3,3,3,3,3,3,3,3,3,3,3,3,3,3,4),(267.035375555307,
267.13383122682,267.232963513412,267.332840407885,267.355198082099,267.438944814801,
267.522588491817,267.606149235883,267.68964709784,267.773109598403,267.856554733895,
267.940000568738,268.023465163976,268.107018349398,268.19061618297,268.274347745832,
268.354181584298,268.437928317,268.521571994016,268.605132738082,268.688630600039,
268.772093100602,268.855538236094,268.938984070937,269.022448666175,269.106001851597,
269.189599685169,269.273331248031,269.353165086497,269.436911819199,269.520555496215,
269.604116240281,269.687614102238,269.7710766028,269.854521738292,269.937967573135,
270.021432168373,270.104985353795,270.188583187367,270.272314750229,270.352148588696,
270.435895321398,270.519538998414,270.60309974248,270.686597604437,270.770060105,
270.853505240492,270.936951075335,271.020415670573,271.103968855995,271.187566689568,
271.27129825243,271.351132090895,271.434878823597,271.518522500613,271.602083244679,
271.685581106636,271.769043607199,271.852488742691,271.935934577534,272.019399172772,
272.102952358194,272.186550191766,272.270281754628,272.350115593094,272.433442907024,
272.516667437266,272.599809733204,272.682890268008,272.765937076089,272.848968279795,
272.932002321396,273.015057641556,273.098200588014,273.181391202307,273.264706059386,
273.318560584361),.UNSPECIFIED.);
#457=B_SPLINE_CURVE_WITH_KNOTS('',3,(#56004,#56005,#56006,#56007,#56008,
#56009,#56010,#56011,#56012,#56013,#56014),.UNSPECIFIED.,.F.,.F.,(4,1,1,
1,1,1,1,1,4),(273.318560862313,273.349099095293,274.348082597493,275.347066099692,
276.346049601891,277.34503310409,278.344016606289,279.343000108488,279.60174364527),
 .UNSPECIFIED.);
#458=B_SPLINE_CURVE_WITH_KNOTS('',3,(#56016,#56017,#56018,#56019,#56020,
#56021,#56022,#56023,#56024,#56025,#56026,#56027,#56028,#56029,#56030,#56031,
#56032,#56033,#56034,#56035,#56036,#56037,#56038,#56039,#56040,#56041,#56042,
#56043,#56044,#56045,#56046,#56047,#56048,#56049,#56050,#56051,#56052,#56053,
#56054,#56055,#56056,#56057,#56058,#56059,#56060,#56061,#56062,#56063,#56064,
#56065,#56066,#56067,#56068,#56069,#56070,#56071,#56072,#56073,#56074,#56075,
#56076,#56077,#56078,#56079,#56080,#56081,#56082,#56083,#56084,#56085,#56086,
#56087,#56088,#56089,#56090,#56091,#56092,#56093,#56094,#56095,#56096,#56097,
#56098,#56099,#56100,#56101,#56102,#56103,#56104,#56105,#56106,#56107,#56108,
#56109,#56110,#56111,#56112,#56113,#56114,#56115,#56116,#56117,#56118,#56119,
#56120,#56121,#56122,#56123,#56124,#56125,#56126,#56127,#56128,#56129,#56130,
#56131,#56132,#56133,#56134,#56135,#56136,#56137,#56138,#56139,#56140,#56141,
#56142,#56143,#56144,#56145,#56146,#56147,#56148,#56149,#56150,#56151,#56152,
#56153,#56154,#56155,#56156,#56157,#56158,#56159,#56160,#56161,#56162,#56163,
#56164,#56165,#56166,#56167,#56168,#56169,#56170,#56171,#56172,#56173,#56174,
#56175,#56176,#56177,#56178,#56179,#56180,#56181,#56182,#56183,#56184,#56185,
#56186,#56187,#56188,#56189,#56190,#56191,#56192,#56193,#56194,#56195,#56196,
#56197,#56198,#56199,#56200,#56201,#56202,#56203,#56204,#56205,#56206,#56207,
#56208,#56209,#56210,#56211,#56212,#56213,#56214,#56215,#56216,#56217,#56218,
#56219,#56220,#56221,#56222,#56223,#56224,#56225,#56226,#56227,#56228,#56229,
#56230,#56231,#56232,#56233,#56234,#56235,#56236,#56237,#56238,#56239,#56240,
#56241,#56242,#56243,#56244),.UNSPECIFIED.,.F.,.F.,(4,3,3,3,3,3,3,3,3,3,
3,3,3,3,3,3,3,3,3,3,3,3,3,3,3,3,3,3,3,3,3,3,3,3,3,3,3,3,3,3,3,3,3,3,3,3,
3,3,3,3,3,3,3,3,3,3,3,3,3,3,3,3,3,3,3,3,3,3,3,3,3,3,3,3,3,3,4),(279.601746169493,
279.684374539858,279.766958048281,279.849518653294,279.932075157065,280.014646355849,
280.097302135208,280.180000280235,280.262830816679,280.341983610688,280.42573034339,
280.509374020406,280.592934764472,280.676432626429,280.759895126992,280.843340262484,
280.926786097327,281.010250692565,281.093803877987,281.177401711559,281.261133274421,
281.340967112887,281.424713845589,281.508357522604,281.591918266671,281.675416128628,
281.75887862919,281.842323764683,281.925769599525,282.009234194764,282.092787380185,
282.176385213758,282.26011677662,282.339950615086,282.423697347788,282.507341024804,
282.590901768871,282.674399630827,282.75786213139,282.841307266882,282.924753101725,
283.008217696963,283.091770882385,283.175368715958,283.25910027882,283.338934117285,
283.422680849987,283.506324527003,283.589885271069,283.673383133026,283.756845633589,
283.840290769081,283.923736603923,284.007201199161,284.090754384583,284.174352218155,
284.258083781017,284.337917619484,284.421664352186,284.505308029202,284.588868773268,
284.672366635225,284.755829135787,284.83927427128,284.922720106122,285.00618470136,
285.089737886782,285.173335720355,285.257067283217,285.336901121683,285.423263322375,
285.509497592493,285.595617755227,285.681608329013,285.767522176602,285.853356753516,
285.884931476672),.UNSPECIFIED.);
#459=B_SPLINE_CURVE_WITH_KNOTS('',3,(#56246,#56247,#56248,#56249,#56250,
#56251,#56252,#56253,#56254,#56255,#56256,#56257,#56258,#56259,#56260,#56261,
#56262,#56263,#56264,#56265,#56266,#56267,#56268,#56269,#56270,#56271,#56272,
#56273,#56274,#56275,#56276,#56277,#56278,#56279,#56280,#56281,#56282,#56283,
#56284,#56285,#56286,#56287,#56288,#56289,#56290,#56291,#56292,#56293,#56294,
#56295,#56296,#56297,#56298,#56299,#56300,#56301,#56302,#56303,#56304,#56305,
#56306,#56307,#56308,#56309,#56310,#56311,#56312,#56313,#56314,#56315,#56316,
#56317,#56318,#56319,#56320,#56321,#56322,#56323,#56324,#56325,#56326,#56327,
#56328,#56329,#56330,#56331,#56332,#56333,#56334,#56335,#56336,#56337,#56338,
#56339,#56340,#56341,#56342,#56343,#56344,#56345,#56346,#56347,#56348,#56349,
#56350,#56351,#56352,#56353,#56354,#56355,#56356,#56357,#56358,#56359,#56360,
#56361,#56362,#56363,#56364,#56365,#56366,#56367,#56368,#56369,#56370,#56371,
#56372,#56373,#56374,#56375,#56376,#56377,#56378,#56379,#56380,#56381,#56382,
#56383,#56384,#56385,#56386,#56387,#56388,#56389,#56390,#56391,#56392,#56393,
#56394,#56395,#56396,#56397,#56398,#56399,#56400,#56401,#56402,#56403,#56404,
#56405,#56406,#56407,#56408,#56409,#56410,#56411,#56412,#56413,#56414,#56415,
#56416,#56417,#56418,#56419,#56420,#56421,#56422,#56423,#56424,#56425,#56426,
#56427,#56428,#56429,#56430,#56431,#56432,#56433,#56434,#56435,#56436,#56437,
#56438,#56439,#56440,#56441,#56442,#56443,#56444,#56445,#56446,#56447,#56448,
#56449,#56450,#56451,#56452,#56453,#56454,#56455,#56456,#56457,#56458,#56459,
#56460,#56461,#56462,#56463,#56464,#56465,#56466,#56467,#56468,#56469,#56470,
#56471,#56472,#56473,#56474),.UNSPECIFIED.,.F.,.F.,(4,3,3,3,3,3,3,3,3,3,
3,3,3,3,3,3,3,3,3,3,3,3,3,3,3,3,3,3,3,3,3,3,3,3,3,3,3,3,3,3,3,3,3,3,3,3,
3,3,3,3,3,3,3,3,3,3,3,3,3,3,3,3,3,3,3,3,3,3,3,3,3,3,3,3,3,3,4),(285.884931476777,
285.974324781646,286.064714742205,286.154589823141,286.245237223512,286.335884623883,
286.419631356585,286.503275033601,286.586835777667,286.670333639624,286.753796140187,
286.837241275679,286.920687110522,287.00415170576,287.087704891182,287.171302724755,
287.255034287617,287.334868126082,287.418614858784,287.5022585358,287.585819279866,
287.669317141823,287.752779642385,287.836224777877,287.91967061272,288.003135207958,
288.08668839338,288.170286226953,288.254017789814,288.333851628281,288.417598360983,
288.501242037999,288.584802782065,288.668300644022,288.751763144585,288.835208280077,
288.91865411492,289.002118710158,289.08567189558,289.169269729153,289.253001292015,
289.33283513048,289.416581863182,289.500225540198,289.583786284264,289.667284146221,
289.750746646783,289.834191782276,289.917637617118,290.001102212356,290.084655397778,
290.168253231351,290.251984794213,290.331818632679,290.415565365381,290.499209042397,
290.582769786463,290.66626764842,290.749730148983,290.833175284475,290.916621119318,
291.000085714556,291.083638899978,291.16723673355,291.250968296412,291.330802134878,
291.413301422989,291.495698257986,291.579750573694,291.662002862286,291.744222964866,
291.826429921203,291.911851636815,291.994123176061,292.076431114752,292.158825062872,
292.168116783652),.UNSPECIFIED.);
#460=B_SPLINE_CURVE_WITH_KNOTS('',3,(#56476,#56477,#56478,#56479,#56480,
#56481,#56482,#56483,#56484,#56485,#56486,#56487,#56488,#56489,#56490,#56491,
#56492,#56493,#56494,#56495,#56496,#56497,#56498,#56499,#56500,#56501,#56502,
#56503,#56504,#56505,#56506,#56507,#56508,#56509,#56510,#56511,#56512,#56513,
#56514,#56515,#56516,#56517,#56518,#56519,#56520,#56521,#56522,#56523,#56524,
#56525,#56526,#56527,#56528,#56529,#56530,#56531,#56532,#56533,#56534,#56535,
#56536,#56537,#56538,#56539,#56540,#56541,#56542,#56543,#56544,#56545,#56546,
#56547,#56548,#56549,#56550,#56551,#56552,#56553,#56554,#56555,#56556,#56557,
#56558,#56559,#56560,#56561,#56562,#56563,#56564,#56565,#56566,#56567,#56568,
#56569,#56570,#56571,#56572,#56573,#56574,#56575,#56576,#56577,#56578,#56579,
#56580,#56581,#56582,#56583,#56584,#56585,#56586,#56587,#56588,#56589,#56590,
#56591,#56592,#56593,#56594,#56595,#56596,#56597,#56598,#56599,#56600,#56601,
#56602,#56603,#56604,#56605,#56606,#56607,#56608,#56609,#56610,#56611,#56612,
#56613,#56614,#56615,#56616,#56617,#56618,#56619,#56620,#56621,#56622,#56623,
#56624,#56625,#56626,#56627,#56628,#56629,#56630,#56631,#56632,#56633,#56634,
#56635,#56636,#56637,#56638,#56639,#56640,#56641,#56642,#56643,#56644,#56645,
#56646,#56647,#56648,#56649,#56650,#56651,#56652,#56653,#56654,#56655,#56656,
#56657,#56658,#56659,#56660,#56661,#56662,#56663,#56664,#56665,#56666,#56667,
#56668,#56669,#56670,#56671,#56672,#56673,#56674,#56675,#56676,#56677,#56678,
#56679,#56680,#56681,#56682,#56683,#56684,#56685,#56686,#56687,#56688,#56689,
#56690,#56691,#56692,#56693,#56694,#56695,#56696,#56697,#56698,#56699,#56700,
#56701),.UNSPECIFIED.,.F.,.F.,(4,3,3,3,3,3,3,3,3,3,3,3,3,3,3,3,3,3,3,3,
3,3,3,3,3,3,3,3,3,3,3,3,3,3,3,3,3,3,3,3,3,3,3,3,3,3,3,3,3,3,3,3,3,3,3,3,
3,3,3,3,3,3,3,3,3,3,3,3,3,3,3,3,3,3,3,4),(292.168116783852,292.30350733608,
292.329785637078,292.41353236978,292.497176046796,292.580736790862,292.664234652819,
292.747697153381,292.831142288874,292.914588123716,292.998052718955,293.081605904376,
293.165203737949,293.248935300811,293.328769139277,293.412515871979,293.496159548995,
293.579720293061,293.663218155018,293.74668065558,293.830125791073,293.913571625915,
293.997036221153,294.080589406575,294.164187240148,294.24791880301,294.327752641476,
294.411499374178,294.495143051194,294.578703795261,294.662201657217,294.74566415778,
294.829109293272,294.912555128115,294.996019723353,295.079572908775,295.163170742348,
295.24690230521,295.326736143675,295.410482876377,295.494126553393,295.577687297459,
295.661185159416,295.744647659978,295.82809279547,295.911538630313,295.995003225551,
296.078556410973,296.162154244545,296.245885807407,296.325719645874,296.409466378576,
296.493110055592,296.576670799659,296.660168661615,296.743631162178,296.82707629767,
296.910522132513,296.993986727751,297.077539913173,297.161137746746,297.244869309608,
297.324703148073,297.408449880775,297.492093557791,297.575654301857,297.659152163814,
297.742614664376,297.826059799869,297.909505634711,297.99297022995,298.076523415372,
298.160121248944,298.243852811806,298.323686650273,298.451302091031),
 .UNSPECIFIED.);
#461=B_SPLINE_CURVE_WITH_KNOTS('',3,(#56703,#56704,#56705,#56706,#56707,
#56708,#56709,#56710,#56711,#56712,#56713,#56714,#56715,#56716,#56717,#56718,
#56719,#56720,#56721,#56722,#56723,#56724,#56725,#56726,#56727,#56728,#56729,
#56730,#56731,#56732,#56733,#56734,#56735,#56736,#56737,#56738,#56739,#56740,
#56741,#56742,#56743,#56744,#56745,#56746,#56747,#56748,#56749,#56750,#56751,
#56752,#56753,#56754,#56755,#56756,#56757,#56758,#56759,#56760,#56761,#56762,
#56763,#56764,#56765,#56766,#56767,#56768,#56769,#56770,#56771,#56772,#56773,
#56774,#56775,#56776,#56777,#56778,#56779,#56780,#56781,#56782,#56783,#56784,
#56785,#56786,#56787,#56788,#56789,#56790,#56791,#56792,#56793,#56794,#56795,
#56796,#56797,#56798,#56799,#56800,#56801,#56802,#56803,#56804,#56805,#56806,
#56807,#56808,#56809,#56810,#56811,#56812,#56813,#56814,#56815,#56816,#56817,
#56818,#56819,#56820,#56821,#56822,#56823,#56824,#56825,#56826,#56827,#56828,
#56829,#56830,#56831,#56832,#56833,#56834,#56835,#56836,#56837,#56838,#56839,
#56840,#56841,#56842,#56843,#56844,#56845,#56846,#56847,#56848,#56849,#56850,
#56851,#56852,#56853,#56854,#56855,#56856,#56857,#56858,#56859,#56860,#56861,
#56862,#56863,#56864,#56865,#56866,#56867,#56868,#56869,#56870,#56871,#56872,
#56873,#56874,#56875,#56876,#56877,#56878,#56879,#56880,#56881,#56882,#56883,
#56884,#56885,#56886,#56887,#56888,#56889,#56890,#56891,#56892,#56893,#56894,
#56895,#56896,#56897,#56898,#56899,#56900,#56901,#56902,#56903,#56904,#56905,
#56906,#56907,#56908,#56909,#56910,#56911,#56912,#56913,#56914,#56915,#56916,
#56917,#56918,#56919,#56920,#56921,#56922,#56923,#56924,#56925,#56926,#56927,
#56928,#56929,#56930,#56931),.UNSPECIFIED.,.F.,.F.,(4,3,3,3,3,3,3,3,3,3,
3,3,3,3,3,3,3,3,3,3,3,3,3,3,3,3,3,3,3,3,3,3,3,3,3,3,3,3,3,3,3,3,3,3,3,3,
3,3,3,3,3,3,3,3,3,3,3,3,3,3,3,3,3,3,3,3,3,3,3,3,3,3,3,3,3,3,4),(298.45130209116,
298.533796201892,298.61620327727,298.698544427693,298.780847073419,298.86313145376,
298.945416555541,299.027721363881,299.110111676385,299.192549242173,299.27510847894,
299.322670152472,299.406416885174,299.49006056219,299.573621306256,299.657119168213,
299.740581668776,299.824026804268,299.907472639111,299.990937234349,300.074490419771,
300.158088253344,300.241819816205,300.321653654671,300.405400387373,300.489044064389,
300.572604808455,300.656102670412,300.739565170975,300.823010306467,300.90645614131,
300.989920736548,301.07347392197,301.157071755543,301.240803318404,301.32063715687,
301.404383889572,301.488027566588,301.571588310654,301.655086172611,301.738548673173,
301.821993808665,301.905439643508,301.988904238746,302.072457424168,302.15605525774,
302.239786820602,302.319620659069,302.403367391771,302.487011068787,302.570571812853,
302.65406967481,302.737532175372,302.820977310864,302.904423145707,302.987887740945,
303.071440926367,303.15503875994,303.238770322802,303.318604161268,303.40235089397,
303.485994570986,303.569555315052,303.653053177009,303.736515677572,303.819960813064,
303.903406647907,303.986871243145,304.070424428567,304.15402226214,304.237753825002,
304.317587663468,304.409695946908,304.501451373444,304.59298093114,304.684152418828,
304.734487398054),.UNSPECIFIED.);
#462=B_SPLINE_CURVE_WITH_KNOTS('',3,(#56933,#56934,#56935,#56936,#56937,
#56938,#56939,#56940,#56941,#56942,#56943,#56944,#56945,#56946,#56947,#56948,
#56949,#56950,#56951,#56952,#56953,#56954,#56955,#56956,#56957,#56958,#56959,
#56960,#56961,#56962,#56963,#56964,#56965,#56966,#56967,#56968,#56969,#56970,
#56971,#56972,#56973,#56974,#56975,#56976,#56977,#56978,#56979,#56980,#56981,
#56982,#56983,#56984,#56985,#56986,#56987,#56988,#56989,#56990,#56991,#56992,
#56993,#56994,#56995,#56996,#56997,#56998,#56999,#57000,#57001,#57002,#57003,
#57004,#57005,#57006,#57007,#57008,#57009,#57010,#57011,#57012,#57013,#57014,
#57015,#57016,#57017,#57018,#57019,#57020,#57021,#57022,#57023,#57024,#57025,
#57026,#57027,#57028,#57029,#57030,#57031,#57032,#57033,#57034,#57035,#57036,
#57037,#57038,#57039,#57040,#57041,#57042,#57043,#57044,#57045,#57046,#57047,
#57048,#57049,#57050,#57051,#57052,#57053,#57054,#57055,#57056,#57057,#57058,
#57059,#57060,#57061,#57062,#57063,#57064,#57065,#57066,#57067,#57068,#57069,
#57070,#57071,#57072,#57073,#57074,#57075,#57076,#57077,#57078,#57079,#57080,
#57081,#57082,#57083,#57084,#57085,#57086,#57087,#57088,#57089,#57090,#57091,
#57092,#57093,#57094,#57095,#57096,#57097,#57098,#57099,#57100,#57101,#57102,
#57103,#57104,#57105,#57106,#57107,#57108,#57109,#57110,#57111,#57112,#57113,
#57114,#57115,#57116,#57117,#57118,#57119,#57120,#57121,#57122,#57123,#57124,
#57125,#57126,#57127,#57128,#57129,#57130,#57131,#57132,#57133,#57134,#57135,
#57136,#57137,#57138,#57139,#57140,#57141,#57142,#57143,#57144,#57145,#57146,
#57147,#57148,#57149,#57150,#57151,#57152,#57153,#57154,#57155,#57156,#57157,
#57158,#57159,#57160,#57161),.UNSPECIFIED.,.F.,.F.,(4,3,3,3,3,3,3,3,3,3,
3,3,3,3,3,3,3,3,3,3,3,3,3,3,3,3,3,3,3,3,3,3,3,3,3,3,3,3,3,3,3,3,3,3,3,3,
3,3,3,3,3,3,3,3,3,3,3,3,3,3,3,3,3,3,3,3,3,3,3,3,3,3,3,3,3,3,4),(304.734487398211,
304.81944881686,304.904444162665,304.989489045624,305.074661256914,305.159900318433,
305.24529683897,305.316571165667,305.400317898369,305.483961575385,305.567522319451,
305.651020181408,305.734482681971,305.817927817463,305.901373652306,305.984838247544,
306.068391432966,306.151989266538,306.2357208294,306.315554667866,306.399301400568,
306.482945077584,306.566505821651,306.650003683608,306.73346618417,306.816911319663,
306.900357154506,306.983821749744,307.067374935166,307.150972768739,307.2347043316,
307.314538170065,307.398284902767,307.481928579782,307.565489323849,307.648987185805,
307.732449686368,307.81589482186,307.899340656703,307.982805251941,308.066358437362,
308.149956270935,308.233687833796,308.313521672264,308.397268404966,308.480912081982,
308.564472826049,308.647970688006,308.731433188568,308.814878324061,308.898324158904,
308.981788754142,309.065341939564,309.148939773137,309.232671335999,309.312505174463,
309.396251907165,309.479895584181,309.563456328248,309.646954190205,309.730416690767,
309.813861826259,309.897307661102,309.98077225634,310.064325441762,310.147923275334,
310.231654838196,310.311488676663,310.394680301707,310.477737958829,310.560718133827,
310.643639475125,310.726520583928,310.809394585425,310.892263754866,310.975171847956,
311.01767270539),.UNSPECIFIED.);
#463=B_SPLINE_CURVE_WITH_KNOTS('',3,(#57163,#57164,#57165,#57166,#57167,
#57168,#57169,#57170,#57171,#57172,#57173,#57174,#57175,#57176,#57177,#57178,
#57179,#57180,#57181,#57182,#57183,#57184,#57185,#57186,#57187,#57188,#57189,
#57190,#57191,#57192,#57193,#57194,#57195,#57196,#57197,#57198,#57199,#57200,
#57201,#57202,#57203,#57204,#57205,#57206,#57207,#57208,#57209,#57210,#57211,
#57212,#57213,#57214,#57215,#57216,#57217,#57218,#57219,#57220,#57221,#57222,
#57223,#57224,#57225,#57226,#57227,#57228,#57229,#57230,#57231,#57232,#57233,
#57234,#57235,#57236,#57237,#57238,#57239,#57240,#57241,#57242,#57243,#57244,
#57245,#57246,#57247,#57248,#57249,#57250,#57251,#57252,#57253,#57254,#57255,
#57256,#57257,#57258,#57259,#57260,#57261,#57262,#57263,#57264,#57265,#57266,
#57267,#57268,#57269,#57270,#57271,#57272,#57273,#57274,#57275,#57276,#57277,
#57278,#57279,#57280,#57281,#57282,#57283,#57284,#57285,#57286,#57287,#57288,
#57289,#57290,#57291,#57292,#57293,#57294,#57295,#57296,#57297,#57298,#57299,
#57300,#57301,#57302,#57303,#57304,#57305,#57306,#57307,#57308,#57309,#57310,
#57311,#57312,#57313,#57314,#57315,#57316,#57317,#57318,#57319,#57320,#57321,
#57322,#57323,#57324,#57325,#57326,#57327,#57328,#57329,#57330,#57331,#57332,
#57333,#57334,#57335,#57336,#57337,#57338,#57339,#57340,#57341,#57342,#57343,
#57344,#57345,#57346,#57347,#57348,#57349,#57350,#57351,#57352,#57353,#57354,
#57355,#57356,#57357,#57358,#57359,#57360,#57361,#57362,#57363,#57364,#57365,
#57366,#57367,#57368,#57369,#57370,#57371,#57372,#57373,#57374,#57375,#57376,
#57377,#57378,#57379,#57380,#57381,#57382,#57383,#57384,#57385,#57386,#57387,
#57388),.UNSPECIFIED.,.F.,.F.,(4,3,3,3,3,3,3,3,3,3,3,3,3,3,3,3,3,3,3,3,
3,3,3,3,3,3,3,3,3,3,3,3,3,3,3,3,3,3,3,3,3,3,3,3,3,3,3,3,3,3,3,3,3,3,3,3,
3,3,3,3,3,3,3,3,3,3,3,3,3,3,3,3,3,3,3,4),(311.017672705525,311.118994588861,
311.221737110735,311.310472178862,311.394218911564,311.47786258858,311.561423332646,
311.644921194603,311.728383695166,311.811828830658,311.895274665501,311.978739260739,
312.06229244616,312.145890279733,312.229621842595,312.309455681061,312.393202413763,
312.476846090779,312.560406834845,312.643904696802,312.727367197364,312.810812332857,
312.894258167699,312.977722762938,313.061275948359,313.144873781932,313.228605344794,
313.30843918326,313.392185915962,313.475829592978,313.559390337044,313.642888199001,
313.726350699563,313.809795835055,313.893241669898,313.976706265136,314.060259450558,
314.143857284131,314.227588846992,314.307422685459,314.391169418161,314.474813095177,
314.558373839243,314.6418717012,314.725334201763,314.808779337255,314.892225172098,
314.975689767336,315.059242952758,315.142840786331,315.226572349193,315.306406187658,
315.39015292036,315.473796597376,315.557357341442,315.640855203399,315.724317703962,
315.807762839454,315.891208674297,315.974673269535,316.058226454957,316.14182428853,
316.225555851391,316.305389689858,316.389083466982,316.472674214911,316.556182113853,
316.639627271712,316.723037303317,316.806430203246,316.889824087096,316.973237067301,
317.056738640507,317.140285262128,317.223964649307,317.300858012433),
 .UNSPECIFIED.);
#464=B_SPLINE_CURVE_WITH_KNOTS('',3,(#57390,#57391,#57392,#57393,#57394,
#57395,#57396,#57397,#57398,#57399,#57400,#57401,#57402,#57403,#57404,#57405,
#57406,#57407,#57408,#57409,#57410,#57411,#57412,#57413,#57414,#57415,#57416,
#57417,#57418,#57419,#57420,#57421,#57422,#57423,#57424,#57425,#57426,#57427,
#57428,#57429,#57430,#57431,#57432,#57433,#57434,#57435,#57436,#57437,#57438,
#57439,#57440,#57441,#57442,#57443,#57444,#57445,#57446,#57447,#57448,#57449,
#57450,#57451,#57452,#57453,#57454,#57455,#57456,#57457,#57458,#57459,#57460,
#57461,#57462,#57463,#57464,#57465,#57466,#57467,#57468,#57469,#57470,#57471,
#57472,#57473,#57474,#57475,#57476,#57477,#57478,#57479,#57480,#57481,#57482,
#57483,#57484,#57485,#57486,#57487,#57488,#57489,#57490,#57491,#57492,#57493,
#57494,#57495,#57496,#57497,#57498,#57499,#57500,#57501,#57502,#57503,#57504,
#57505,#57506,#57507,#57508,#57509,#57510,#57511,#57512,#57513,#57514,#57515,
#57516,#57517,#57518,#57519,#57520,#57521,#57522,#57523,#57524,#57525,#57526,
#57527,#57528,#57529,#57530,#57531,#57532,#57533,#57534,#57535,#57536,#57537,
#57538,#57539,#57540,#57541,#57542,#57543,#57544,#57545,#57546,#57547,#57548,
#57549,#57550,#57551,#57552,#57553,#57554,#57555,#57556,#57557,#57558,#57559,
#57560,#57561,#57562,#57563,#57564,#57565,#57566,#57567,#57568,#57569,#57570,
#57571,#57572,#57573,#57574,#57575,#57576,#57577,#57578,#57579,#57580,#57581,
#57582,#57583,#57584,#57585,#57586,#57587,#57588,#57589,#57590,#57591,#57592,
#57593,#57594,#57595,#57596,#57597,#57598,#57599,#57600,#57601,#57602,#57603,
#57604,#57605,#57606,#57607,#57608,#57609,#57610,#57611,#57612,#57613,#57614,
#57615,#57616,#57617,#57618),.UNSPECIFIED.,.F.,.F.,(4,3,3,3,3,3,3,3,3,3,
3,3,3,3,3,3,3,3,3,3,3,3,3,3,3,3,3,3,3,3,3,3,3,3,3,3,3,3,3,3,3,3,3,3,3,3,
3,3,3,3,3,3,3,3,3,3,3,3,3,3,3,3,3,3,3,3,3,3,3,3,3,3,3,3,3,3,4),(317.30085801257,
317.304373192057,317.388119924759,317.471763601775,317.555324345842,317.638822207799,
317.722284708361,317.805729843854,317.889175678697,317.972640273935,318.056193459357,
318.13979129293,318.223522855791,318.303356694256,318.387103426958,318.470747103974,
318.55430784804,318.637805709997,318.721268210559,318.804713346052,318.888159180894,
318.971623776132,319.055176961554,319.138774795127,319.222506357989,319.302340196455,
319.386086929157,319.469730606173,319.553291350239,319.636789212196,319.720251712759,
319.803696848251,319.887142683094,319.970607278332,320.054160463754,320.137758297326,
320.221489860188,320.301323698654,320.385070431356,320.468714108372,320.552274852438,
320.635772714395,320.719235214958,320.80268035045,320.886126185293,320.969590780531,
321.053143965953,321.136741799525,321.220473362387,321.300307200853,321.384053933555,
321.467697610571,321.551258354637,321.634756216594,321.718218717157,321.801663852649,
321.885109687492,321.96857428273,322.052127468152,322.135725301725,322.219456864587,
322.299290703053,322.383037435755,322.466681112771,322.550241856837,322.633739718794,
322.717202219357,322.800647354849,322.884093189692,322.96755778493,323.051110970352,
323.134708803925,323.218440366787,323.298274205252,323.402181613344,323.504610985504,
323.584043319628),.UNSPECIFIED.);
#465=B_SPLINE_CURVE_WITH_KNOTS('',3,(#57620,#57621,#57622,#57623,#57624,
#57625,#57626,#57627,#57628,#57629,#57630,#57631,#57632,#57633,#57634,#57635,
#57636,#57637,#57638,#57639,#57640,#57641,#57642,#57643,#57644,#57645,#57646,
#57647,#57648,#57649,#57650,#57651,#57652,#57653,#57654,#57655,#57656,#57657,
#57658,#57659,#57660,#57661,#57662,#57663,#57664,#57665,#57666,#57667,#57668,
#57669,#57670,#57671,#57672,#57673,#57674,#57675,#57676,#57677,#57678,#57679,
#57680,#57681,#57682,#57683,#57684,#57685,#57686,#57687,#57688,#57689,#57690,
#57691,#57692,#57693,#57694,#57695,#57696,#57697,#57698,#57699,#57700,#57701,
#57702,#57703,#57704,#57705,#57706,#57707,#57708,#57709,#57710,#57711,#57712,
#57713,#57714,#57715,#57716,#57717,#57718,#57719,#57720,#57721,#57722,#57723,
#57724,#57725,#57726,#57727,#57728,#57729,#57730,#57731,#57732,#57733,#57734,
#57735,#57736,#57737,#57738,#57739,#57740,#57741,#57742,#57743,#57744,#57745,
#57746,#57747,#57748,#57749,#57750,#57751,#57752,#57753,#57754,#57755,#57756,
#57757,#57758,#57759,#57760,#57761,#57762,#57763,#57764,#57765,#57766,#57767,
#57768,#57769,#57770,#57771,#57772,#57773,#57774,#57775,#57776,#57777,#57778,
#57779,#57780,#57781,#57782,#57783,#57784,#57785,#57786,#57787,#57788,#57789,
#57790,#57791,#57792,#57793,#57794,#57795,#57796,#57797,#57798,#57799,#57800,
#57801,#57802,#57803,#57804,#57805,#57806,#57807,#57808,#57809,#57810,#57811,
#57812,#57813,#57814,#57815,#57816,#57817,#57818,#57819,#57820,#57821,#57822,
#57823,#57824,#57825,#57826,#57827,#57828,#57829,#57830,#57831,#57832,#57833,
#57834,#57835,#57836,#57837,#57838,#57839,#57840,#57841,#57842,#57843,#57844,
#57845,#57846,#57847,#57848),.UNSPECIFIED.,.F.,.F.,(4,3,3,3,3,3,3,3,3,3,
3,3,3,3,3,3,3,3,3,3,3,3,3,3,3,3,3,3,3,3,3,3,3,3,3,3,3,3,3,3,3,3,3,3,3,3,
3,3,3,3,3,3,3,3,3,3,3,3,3,3,3,3,3,3,3,3,3,3,3,3,3,3,3,3,3,3,4),(323.58404331975,
323.666886187998,323.749698014738,323.83249604088,323.915298875906,323.998125129485,
324.081041926353,324.164008541604,324.247101083384,324.297257707451,324.381004440153,
324.464648117169,324.548208861235,324.631706723192,324.715169223755,324.798614359247,
324.88206019409,324.965524789328,325.04907797475,325.132675808322,325.216407371184,
325.29624120965,325.379987942352,325.463631619368,325.547192363434,325.630690225391,
325.714152725954,325.797597861446,325.881043696289,325.964508291527,326.048061476949,
326.131659310521,326.215390873383,326.295224711849,326.378971444551,326.462615121567,
326.546175865634,326.629673727591,326.713136228153,326.796581363646,326.880027198489,
326.963491793727,327.047044979149,327.130642812722,327.214374375583,327.294208214048,
327.37795494675,327.461598623766,327.545159367832,327.628657229789,327.712119730352,
327.795564865844,327.879010700687,327.962475295925,328.046028481347,328.129626314919,
328.213357877781,328.293191716248,328.37693844895,328.460582125966,328.544142870033,
328.627640731989,328.711103232552,328.794548368044,328.877994202887,328.961458798126,
329.045011983548,329.12860981712,329.212341379982,329.292175218447,329.377761784272,
329.463229543,329.548594014623,329.633848460025,329.71903832337,329.804171773391,
329.867228626929),.UNSPECIFIED.);
#466=B_SPLINE_CURVE_WITH_KNOTS('',3,(#57850,#57851,#57852,#57853,#57854,
#57855,#57856,#57857,#57858,#57859,#57860,#57861,#57862,#57863,#57864,#57865,
#57866,#57867,#57868,#57869,#57870,#57871,#57872,#57873,#57874,#57875,#57876,
#57877,#57878,#57879,#57880,#57881,#57882,#57883,#57884,#57885,#57886,#57887,
#57888,#57889,#57890,#57891,#57892,#57893,#57894,#57895,#57896,#57897,#57898,
#57899,#57900,#57901,#57902,#57903,#57904,#57905,#57906,#57907,#57908,#57909,
#57910,#57911,#57912,#57913,#57914,#57915,#57916,#57917,#57918,#57919,#57920,
#57921,#57922,#57923,#57924,#57925,#57926,#57927,#57928,#57929,#57930,#57931,
#57932,#57933,#57934,#57935,#57936,#57937,#57938,#57939,#57940,#57941,#57942,
#57943,#57944,#57945,#57946,#57947,#57948,#57949,#57950,#57951,#57952,#57953,
#57954,#57955,#57956,#57957,#57958,#57959,#57960,#57961,#57962,#57963,#57964,
#57965,#57966,#57967,#57968,#57969,#57970,#57971,#57972,#57973,#57974,#57975,
#57976,#57977,#57978,#57979,#57980,#57981,#57982,#57983,#57984,#57985,#57986,
#57987,#57988,#57989,#57990,#57991,#57992,#57993,#57994,#57995,#57996,#57997,
#57998,#57999,#58000,#58001,#58002,#58003,#58004,#58005,#58006,#58007,#58008,
#58009,#58010,#58011,#58012,#58013,#58014,#58015,#58016,#58017,#58018,#58019,
#58020,#58021,#58022,#58023,#58024,#58025,#58026,#58027,#58028,#58029,#58030,
#58031,#58032,#58033,#58034,#58035,#58036,#58037,#58038,#58039,#58040,#58041,
#58042,#58043,#58044,#58045,#58046,#58047,#58048,#58049,#58050,#58051,#58052,
#58053,#58054,#58055,#58056,#58057,#58058,#58059,#58060,#58061,#58062,#58063,
#58064,#58065,#58066,#58067,#58068,#58069,#58070,#58071,#58072,#58073,#58074,
#58075,#58076,#58077,#58078),.UNSPECIFIED.,.F.,.F.,(4,3,3,3,3,3,3,3,3,3,
3,3,3,3,3,3,3,3,3,3,3,3,3,3,3,3,3,3,3,3,3,3,3,3,3,3,3,3,3,3,3,3,3,3,3,3,
3,3,3,3,3,3,3,3,3,3,3,3,3,3,3,3,3,3,3,3,3,3,3,3,3,3,3,3,3,3,4),(329.86722862708,
329.957952637098,330.049077582971,330.140406534098,330.232041447377,330.291158720646,
330.374905453348,330.458549130364,330.542109874431,330.625607736387,330.70907023695,
330.792515372442,330.875961207285,330.959425802523,331.042978987945,331.126576821518,
331.21030838438,331.290142222845,331.373888955547,331.457532632563,331.541093376629,
331.624591238586,331.708053739148,331.79149887464,331.874944709483,331.958409304721,
332.041962490143,332.125560323716,332.209291886577,332.289125725044,332.372872457746,
332.456516134762,332.540076878828,332.623574740785,332.707037241348,332.79048237684,
332.873928211683,332.957392806921,333.040945992343,333.124543825916,333.208275388778,
333.288109227243,333.371855959945,333.455499636961,333.539060381027,333.622558242984,
333.706020743547,333.789465879039,333.872911713882,333.95637630912,334.039929494541,
334.123527328114,334.207258890976,334.287092729443,334.370839462145,334.454483139161,
334.538043883227,334.621541745184,334.705004245747,334.788449381239,334.871895216082,
334.95535981132,335.038912996742,335.122510830315,335.206242393176,335.286076231642,
335.368622249699,335.451066024559,335.533428752273,335.615730097583,335.697999133896,
335.780254872469,335.862516310863,335.944840664036,336.027200299695,336.109659708555,
336.150413933984),.UNSPECIFIED.);
#467=B_SPLINE_CURVE_WITH_KNOTS('',3,(#58080,#58081,#58082,#58083,#58084,
#58085,#58086,#58087,#58088,#58089,#58090,#58091,#58092,#58093,#58094,#58095,
#58096,#58097,#58098,#58099,#58100,#58101,#58102,#58103,#58104,#58105,#58106,
#58107,#58108,#58109,#58110,#58111,#58112,#58113,#58114,#58115,#58116,#58117,
#58118,#58119,#58120,#58121,#58122,#58123,#58124,#58125,#58126,#58127,#58128,
#58129,#58130,#58131,#58132,#58133,#58134,#58135,#58136,#58137,#58138,#58139,
#58140,#58141,#58142,#58143,#58144,#58145,#58146,#58147,#58148,#58149,#58150,
#58151,#58152,#58153,#58154,#58155,#58156,#58157,#58158,#58159,#58160,#58161,
#58162,#58163,#58164,#58165,#58166,#58167,#58168,#58169,#58170,#58171,#58172,
#58173,#58174,#58175,#58176,#58177,#58178,#58179,#58180,#58181,#58182,#58183,
#58184,#58185,#58186,#58187,#58188,#58189,#58190,#58191,#58192,#58193,#58194,
#58195,#58196,#58197,#58198,#58199,#58200,#58201,#58202,#58203,#58204,#58205,
#58206,#58207,#58208,#58209,#58210,#58211,#58212,#58213,#58214,#58215,#58216,
#58217,#58218,#58219,#58220,#58221,#58222,#58223,#58224,#58225,#58226,#58227,
#58228,#58229,#58230,#58231,#58232,#58233,#58234,#58235,#58236,#58237,#58238,
#58239,#58240,#58241,#58242,#58243,#58244,#58245,#58246,#58247,#58248,#58249,
#58250,#58251,#58252,#58253,#58254,#58255,#58256,#58257,#58258,#58259,#58260,
#58261,#58262,#58263,#58264,#58265,#58266,#58267,#58268,#58269,#58270,#58271,
#58272,#58273,#58274,#58275,#58276,#58277,#58278,#58279,#58280,#58281,#58282,
#58283,#58284,#58285,#58286,#58287,#58288,#58289,#58290,#58291,#58292,#58293,
#58294,#58295,#58296,#58297,#58298,#58299,#58300,#58301,#58302,#58303,#58304,
#58305),.UNSPECIFIED.,.F.,.F.,(4,3,3,3,3,3,3,3,3,3,3,3,3,3,3,3,3,3,3,3,
3,3,3,3,3,3,3,3,3,3,3,3,3,3,3,3,3,3,3,3,3,3,3,3,3,3,3,3,3,3,3,3,3,3,3,3,
3,3,3,3,3,3,3,3,3,3,3,3,3,3,3,3,3,3,3,4),(336.150413934109,336.285059733841,
336.368806466543,336.452450143559,336.536010887625,336.619508749582,336.702971250145,
336.786416385637,336.86986222048,336.953326815718,337.03688000114,337.120477834713,
337.204209397575,337.28404323604,337.367789968742,337.451433645758,337.534994389824,
337.618492251781,337.701954752344,337.785399887836,337.868845722679,337.952310317917,
338.035863503339,338.119461336911,338.203192899773,338.283026738239,338.366773470941,
338.450417147957,338.533977892023,338.61747575398,338.700938254542,338.784383390035,
338.867829224877,338.951293820115,339.034847005537,339.11844483911,339.202176401972,
339.282010240438,339.36575697314,339.449400650156,339.532961394223,339.61645925618,
339.699921756742,339.783366892235,339.866812727078,339.950277322316,340.033830507738,
340.117428341311,340.201159904173,340.280993742638,340.36474047534,340.448384152356,
340.531944896422,340.615442758379,340.698905258942,340.782350394434,340.865796229277,
340.949260824515,341.032814009937,341.11641184351,341.200143406372,341.279977244837,
341.363723977539,341.447367654555,341.530928398621,341.614426260578,341.69788876114,
341.781333896633,341.864779731475,341.948244326713,342.031797512135,342.115395345708,
342.199126908569,342.278960747036,342.418201063665,342.433599241288),
 .UNSPECIFIED.);
#468=B_SPLINE_CURVE_WITH_KNOTS('',3,(#58307,#58308,#58309,#58310,#58311,
#58312,#58313,#58314,#58315,#58316,#58317,#58318,#58319,#58320,#58321,#58322,
#58323,#58324,#58325,#58326,#58327,#58328,#58329,#58330,#58331,#58332,#58333,
#58334,#58335,#58336,#58337,#58338,#58339,#58340,#58341,#58342,#58343,#58344,
#58345,#58346,#58347,#58348,#58349,#58350,#58351,#58352,#58353,#58354,#58355,
#58356,#58357,#58358,#58359,#58360,#58361,#58362,#58363,#58364,#58365,#58366,
#58367,#58368,#58369,#58370,#58371,#58372,#58373,#58374,#58375,#58376,#58377,
#58378,#58379,#58380,#58381,#58382,#58383,#58384,#58385,#58386,#58387,#58388,
#58389,#58390,#58391,#58392,#58393,#58394,#58395,#58396,#58397,#58398,#58399,
#58400,#58401,#58402,#58403,#58404,#58405,#58406,#58407,#58408,#58409,#58410,
#58411,#58412,#58413,#58414,#58415,#58416,#58417,#58418,#58419,#58420,#58421,
#58422,#58423,#58424,#58425,#58426,#58427,#58428,#58429,#58430,#58431,#58432,
#58433,#58434,#58435,#58436,#58437,#58438,#58439,#58440,#58441,#58442,#58443,
#58444,#58445,#58446,#58447,#58448,#58449,#58450,#58451,#58452,#58453,#58454,
#58455,#58456,#58457,#58458,#58459,#58460,#58461,#58462,#58463,#58464,#58465,
#58466,#58467,#58468,#58469,#58470,#58471,#58472,#58473,#58474,#58475,#58476,
#58477,#58478,#58479,#58480,#58481,#58482,#58483,#58484,#58485,#58486,#58487,
#58488,#58489,#58490,#58491,#58492,#58493,#58494,#58495,#58496,#58497,#58498,
#58499,#58500,#58501,#58502,#58503,#58504,#58505,#58506,#58507,#58508,#58509,
#58510,#58511,#58512,#58513,#58514,#58515,#58516,#58517,#58518,#58519,#58520,
#58521,#58522,#58523,#58524,#58525,#58526,#58527,#58528,#58529,#58530,#58531,
#58532,#58533,#58534,#58535),.UNSPECIFIED.,.F.,.F.,(4,3,3,3,3,3,3,3,3,3,
3,3,3,3,3,3,3,3,3,3,3,3,3,3,3,3,3,3,3,3,3,3,3,3,3,3,3,3,3,3,3,3,3,3,3,3,
3,3,3,3,3,3,3,3,3,3,3,3,3,3,3,3,3,3,3,3,3,3,3,3,3,3,3,3,3,3,4),(342.433599241396,
342.516002347129,342.598324574841,342.68327703414,342.765508333302,342.847727632491,
342.929953955044,343.01220632799,343.094547026574,343.1769407611,343.259448331164,
343.277944249235,343.361690981937,343.445334658953,343.528895403019,343.612393264976,
343.695855765538,343.77930090103,343.862746735873,343.946211331111,344.029764516533,
344.113362350106,344.197093912967,344.276927751434,344.360674484136,344.444318161152,
344.527878905218,344.611376767175,344.694839267738,344.77828440323,344.861730238073,
344.94519483331,345.028748018732,345.112345852305,345.196077415167,345.275911253633,
345.359657986335,345.443301663351,345.526862407418,345.610360269374,345.693822769937,
345.777267905429,345.860713740272,345.94417833551,346.027731520932,346.111329354504,
346.195060917366,346.274894755833,346.358641488535,346.442285165551,346.525845909618,
346.609343771575,346.692806272137,346.77625140763,346.859697242473,346.943161837711,
347.026715023132,347.110312856705,347.194044419567,347.273878258032,347.357624990734,
347.44126866775,347.524829411816,347.608327273773,347.691789774335,347.775234909828,
347.85868074467,347.942145339908,348.02569852533,348.109296358902,348.193027921764,
348.272861760231,348.363449546096,348.453737517769,348.543843582329,348.633659106349,
348.716784548354),.UNSPECIFIED.);
#469=B_SPLINE_CURVE_WITH_KNOTS('',3,(#58537,#58538,#58539,#58540,#58541,
#58542,#58543,#58544,#58545,#58546,#58547,#58548,#58549,#58550,#58551,#58552,
#58553,#58554,#58555,#58556,#58557,#58558,#58559,#58560,#58561,#58562,#58563,
#58564,#58565,#58566,#58567,#58568,#58569,#58570,#58571,#58572,#58573,#58574,
#58575,#58576,#58577,#58578,#58579,#58580,#58581,#58582,#58583,#58584,#58585,
#58586,#58587,#58588,#58589,#58590,#58591,#58592,#58593,#58594,#58595,#58596,
#58597,#58598,#58599,#58600,#58601,#58602,#58603,#58604,#58605,#58606,#58607,
#58608,#58609,#58610,#58611,#58612,#58613,#58614,#58615,#58616,#58617,#58618,
#58619,#58620,#58621,#58622,#58623,#58624,#58625,#58626,#58627,#58628,#58629,
#58630,#58631,#58632,#58633,#58634,#58635,#58636,#58637,#58638,#58639,#58640,
#58641,#58642,#58643,#58644,#58645,#58646,#58647,#58648,#58649,#58650,#58651,
#58652,#58653,#58654,#58655,#58656,#58657,#58658,#58659,#58660,#58661,#58662,
#58663,#58664,#58665,#58666,#58667,#58668,#58669,#58670,#58671,#58672,#58673,
#58674,#58675,#58676,#58677,#58678,#58679,#58680,#58681,#58682,#58683,#58684,
#58685,#58686,#58687,#58688,#58689,#58690,#58691,#58692,#58693,#58694,#58695,
#58696,#58697,#58698,#58699,#58700,#58701,#58702,#58703,#58704,#58705,#58706,
#58707,#58708,#58709,#58710,#58711,#58712,#58713,#58714,#58715,#58716,#58717,
#58718,#58719,#58720,#58721,#58722,#58723,#58724,#58725,#58726,#58727,#58728,
#58729,#58730,#58731,#58732,#58733,#58734,#58735,#58736,#58737,#58738,#58739,
#58740,#58741,#58742,#58743,#58744,#58745,#58746,#58747,#58748,#58749,#58750,
#58751,#58752,#58753,#58754,#58755,#58756,#58757,#58758,#58759,#58760,#58761,
#58762,#58763,#58764,#58765),.UNSPECIFIED.,.F.,.F.,(4,3,3,3,3,3,3,3,3,3,
3,3,3,3,3,3,3,3,3,3,3,3,3,3,3,3,3,3,3,3,3,3,3,3,3,3,3,3,3,3,3,3,3,3,3,3,
3,3,3,3,3,3,3,3,3,3,3,3,3,3,3,3,3,3,3,3,3,3,3,3,3,3,3,3,3,3,4),(348.716784548468,
348.802434990704,348.888140583416,348.973915359868,349.059835222646,349.145836218956,
349.231993934527,349.27184526243,349.355591995132,349.439235672148,349.522796416214,
349.606294278171,349.689756778733,349.773201914226,349.856647749068,349.940112344306,
350.023665529728,350.107263363301,350.190994926162,350.270828764629,350.354575497331,
350.438219174347,350.521779918413,350.60527778037,350.688740280933,350.772185416425,
350.855631251267,350.939095846506,351.022649031927,351.1062468655,351.189978428362,
351.269812266828,351.35355899953,351.437202676546,351.520763420612,351.604261282569,
351.687723783132,351.771168918624,351.854614753467,351.938079348705,352.021632534127,
352.105230367699,352.188961930561,352.268795769027,352.352542501729,352.436186178745,
352.519746922811,352.603244784768,352.686707285331,352.770152420823,352.853598255666,
352.937062850904,353.020616036326,353.104213869899,353.187945432761,353.267779271227,
353.351526003929,353.435169680945,353.518730425011,353.602228286967,353.68569078753,
353.769135923022,353.852581757865,353.936046353103,354.019599538525,354.103197372098,
354.18692893496,354.266762773426,354.349682329874,354.432471146391,354.515184784845,
354.597842098166,354.680461891829,354.763083217737,354.845702109952,354.928375725224,
354.999969855647),.UNSPECIFIED.);
#470=B_SPLINE_CURVE_WITH_KNOTS('',3,(#58767,#58768,#58769,#58770,#58771,
#58772,#58773,#58774,#58775,#58776,#58777,#58778,#58779,#58780,#58781,#58782,
#58783,#58784,#58785,#58786,#58787,#58788,#58789,#58790,#58791,#58792,#58793,
#58794,#58795,#58796,#58797,#58798,#58799,#58800,#58801,#58802,#58803,#58804,
#58805,#58806,#58807,#58808,#58809,#58810,#58811,#58812,#58813,#58814,#58815,
#58816,#58817,#58818,#58819,#58820,#58821,#58822,#58823,#58824,#58825,#58826,
#58827,#58828,#58829,#58830,#58831,#58832,#58833,#58834,#58835,#58836,#58837,
#58838,#58839,#58840,#58841,#58842,#58843,#58844,#58845,#58846,#58847,#58848,
#58849,#58850,#58851,#58852,#58853,#58854,#58855,#58856,#58857,#58858,#58859,
#58860,#58861,#58862,#58863,#58864,#58865,#58866,#58867,#58868,#58869,#58870,
#58871,#58872,#58873,#58874,#58875,#58876,#58877,#58878,#58879,#58880,#58881,
#58882,#58883,#58884,#58885,#58886,#58887,#58888,#58889,#58890,#58891,#58892,
#58893,#58894,#58895,#58896,#58897,#58898,#58899,#58900,#58901,#58902,#58903,
#58904,#58905,#58906,#58907,#58908,#58909,#58910,#58911,#58912,#58913,#58914,
#58915,#58916,#58917,#58918,#58919,#58920,#58921,#58922,#58923,#58924,#58925,
#58926,#58927,#58928,#58929,#58930,#58931,#58932,#58933,#58934,#58935,#58936,
#58937,#58938,#58939,#58940,#58941,#58942,#58943,#58944,#58945,#58946,#58947,
#58948,#58949,#58950,#58951,#58952,#58953,#58954,#58955,#58956,#58957,#58958,
#58959,#58960,#58961,#58962,#58963,#58964,#58965,#58966,#58967,#58968,#58969,
#58970,#58971,#58972,#58973,#58974,#58975,#58976,#58977,#58978,#58979,#58980,
#58981,#58982,#58983,#58984,#58985,#58986,#58987,#58988,#58989,#58990,#58991,
#58992,#58993,#58994,#58995),.UNSPECIFIED.,.F.,.F.,(4,3,3,3,3,3,3,3,3,3,
3,3,3,3,3,3,3,3,3,3,3,3,3,3,3,3,3,3,3,3,3,3,3,3,3,3,3,3,3,3,3,3,3,3,3,3,
3,3,3,3,3,3,3,3,3,3,3,3,3,3,3,3,3,3,3,3,3,3,3,3,3,3,3,3,3,3,4),(354.999969855808,
355.104758748587,355.211493803573,355.265746275625,355.349493008327,355.433136685343,
355.516697429409,355.600195291366,355.683657791929,355.767102927421,355.850548762264,
355.934013357502,356.017566542924,356.101164376497,356.184895939358,356.264729777824,
356.348476510526,356.432120187542,356.515680931608,356.599178793565,356.682641294128,
356.76608642962,356.849532264463,356.932996859701,357.016550045122,357.100147878695,
357.183879441557,357.263713280023,357.347460012725,357.431103689741,357.514664433807,
357.598162295764,357.681624796327,357.765069931819,357.848515766662,357.9319803619,
358.015533547322,358.099131380894,358.182862943756,358.262696782222,358.346443514924,
358.43008719194,358.513647936007,358.597145797963,358.680608298526,358.764053434018,
358.847499268861,358.930963864099,359.014517049521,359.098114883094,359.181846445956,
359.261680284422,359.345427017124,359.42907069414,359.512631438206,359.596129300163,
359.679591800726,359.763036936218,359.846482771061,359.929947366299,360.013500551721,
360.097098385293,360.180829948155,360.260663786621,360.344410519323,360.428054196339,
360.511614940406,360.595112802363,360.678575302925,360.762020438418,360.845466273261,
360.928930868499,361.012484053921,361.096081887494,361.179813450356,361.25964728882,
361.283155162827),.UNSPECIFIED.);
#471=B_SPLINE_CURVE_WITH_KNOTS('',3,(#58997,#58998,#58999,#59000,#59001,
#59002,#59003,#59004,#59005,#59006),.UNSPECIFIED.,.F.,.F.,(4,1,1,1,1,1,
1,4),(361.283158485953,362.258630791019,363.257614293218,364.256597795417,
365.255581297617,366.254564799816,367.253548302015,367.566334031703),
 .UNSPECIFIED.);
#472=B_SPLINE_CURVE_WITH_KNOTS('',3,(#59008,#59009,#59010,#59011,#59012,
#59013,#59014,#59015,#59016,#59017,#59018,#59019,#59020,#59021,#59022,#59023,
#59024,#59025,#59026,#59027,#59028,#59029,#59030,#59031,#59032,#59033,#59034,
#59035,#59036,#59037,#59038,#59039,#59040,#59041,#59042,#59043,#59044,#59045,
#59046,#59047,#59048,#59049,#59050,#59051,#59052,#59053,#59054,#59055,#59056,
#59057,#59058,#59059,#59060,#59061,#59062,#59063,#59064,#59065,#59066,#59067,
#59068,#59069,#59070,#59071,#59072,#59073,#59074,#59075,#59076,#59077,#59078,
#59079,#59080,#59081,#59082,#59083,#59084,#59085,#59086,#59087,#59088,#59089,
#59090,#59091,#59092,#59093,#59094,#59095,#59096,#59097,#59098,#59099,#59100,
#59101,#59102,#59103,#59104,#59105,#59106,#59107,#59108,#59109,#59110,#59111,
#59112,#59113,#59114,#59115,#59116,#59117,#59118,#59119,#59120,#59121,#59122,
#59123,#59124,#59125,#59126,#59127,#59128,#59129,#59130,#59131,#59132,#59133,
#59134,#59135,#59136,#59137,#59138,#59139,#59140,#59141,#59142,#59143,#59144,
#59145,#59146,#59147,#59148,#59149,#59150,#59151,#59152,#59153,#59154,#59155,
#59156,#59157,#59158,#59159,#59160,#59161,#59162,#59163,#59164,#59165,#59166,
#59167,#59168,#59169,#59170,#59171,#59172,#59173,#59174,#59175,#59176,#59177,
#59178,#59179,#59180,#59181,#59182,#59183,#59184,#59185,#59186,#59187,#59188,
#59189,#59190,#59191,#59192,#59193,#59194,#59195,#59196,#59197,#59198,#59199,
#59200,#59201,#59202,#59203,#59204,#59205,#59206,#59207,#59208,#59209,#59210,
#59211,#59212,#59213,#59214,#59215,#59216,#59217,#59218,#59219,#59220,#59221,
#59222,#59223,#59224,#59225,#59226,#59227,#59228,#59229,#59230,#59231,#59232,
#59233,#59234,#59235,#59236),.UNSPECIFIED.,.F.,.F.,(4,3,3,3,3,3,3,3,3,3,
3,3,3,3,3,3,3,3,3,3,3,3,3,3,3,3,3,3,3,3,3,3,3,3,3,3,3,3,3,3,3,3,3,3,3,3,
3,3,3,3,3,3,3,3,3,3,3,3,3,3,3,3,3,3,3,3,3,3,3,3,3,3,3,3,3,3,4),(367.566340470006,
367.652114386782,367.735224242723,367.818330991452,367.90145296639,367.984608507648,
368.06786137521,368.151172612959,368.234603355717,368.252531804214,368.336278536916,
368.419922213932,368.503482957998,368.586980819955,368.670443320517,368.75388845601,
368.837334290852,368.92079888609,369.004352071512,369.087949905085,369.171681467946,
369.251515306413,369.335262039115,369.418905716131,369.502466460197,369.585964322154,
369.669426822717,369.752871958209,369.836317793052,369.91978238829,370.003335573712,
370.086933407285,370.170664970146,370.250498808612,370.334245541314,370.41788921833,
370.501449962396,370.584947824353,370.668410324916,370.751855460408,370.835301295251,
370.918765890489,371.002319075911,371.085916909484,371.169648472346,371.249482310812,
371.333229043514,371.41687272053,371.500433464596,371.583931326553,371.667393827116,
371.750838962608,371.834284797451,371.917749392689,372.001302578111,372.084900411684,
372.168631974546,372.248465813011,372.332212545713,372.415856222729,372.499416966795,
372.582914828751,372.666377329314,372.749822464806,372.833268299649,372.916732894887,
373.000286080309,373.083883913881,373.167615476743,373.24744931521,373.33236473397,
373.41716843778,373.50187711303,373.588789279069,373.673347477172,373.761436627179,
373.849525777186),.UNSPECIFIED.);
#473=B_SPLINE_CURVE_WITH_KNOTS('',3,(#59238,#59239,#59240,#59241,#59242,
#59243,#59244,#59245,#59246,#59247,#59248,#59249,#59250,#59251,#59252,#59253,
#59254,#59255,#59256,#59257,#59258,#59259,#59260,#59261,#59262,#59263,#59264,
#59265,#59266,#59267,#59268,#59269,#59270,#59271,#59272,#59273,#59274,#59275,
#59276,#59277,#59278,#59279,#59280,#59281,#59282,#59283,#59284,#59285,#59286,
#59287,#59288,#59289,#59290,#59291,#59292,#59293,#59294,#59295,#59296,#59297,
#59298,#59299,#59300,#59301,#59302,#59303,#59304,#59305,#59306,#59307,#59308,
#59309,#59310,#59311,#59312,#59313,#59314,#59315,#59316,#59317,#59318,#59319,
#59320,#59321,#59322,#59323,#59324,#59325,#59326,#59327,#59328,#59329,#59330,
#59331,#59332,#59333,#59334,#59335,#59336,#59337,#59338,#59339,#59340,#59341,
#59342,#59343,#59344,#59345,#59346,#59347,#59348,#59349,#59350,#59351,#59352,
#59353,#59354,#59355,#59356,#59357,#59358,#59359,#59360,#59361,#59362,#59363,
#59364,#59365,#59366,#59367,#59368,#59369,#59370,#59371,#59372,#59373,#59374,
#59375,#59376,#59377,#59378,#59379,#59380,#59381,#59382,#59383,#59384,#59385,
#59386,#59387,#59388,#59389,#59390,#59391,#59392,#59393,#59394,#59395,#59396,
#59397,#59398,#59399,#59400,#59401,#59402,#59403,#59404,#59405,#59406,#59407,
#59408,#59409,#59410,#59411,#59412,#59413,#59414,#59415,#59416,#59417,#59418,
#59419,#59420,#59421,#59422,#59423,#59424,#59425,#59426,#59427,#59428,#59429,
#59430,#59431,#59432,#59433,#59434,#59435,#59436,#59437,#59438,#59439,#59440,
#59441,#59442,#59443,#59444,#59445,#59446,#59447,#59448,#59449,#59450,#59451,
#59452,#59453,#59454,#59455,#59456,#59457,#59458,#59459,#59460,#59461,#59462,
#59463,#59464,#59465,#59466),.UNSPECIFIED.,.F.,.F.,(4,3,3,3,3,3,3,3,3,3,
3,3,3,3,3,3,3,3,3,3,3,3,3,3,3,3,3,3,3,3,3,3,3,3,3,3,3,3,3,3,3,3,3,3,3,3,
3,3,3,3,3,3,3,3,3,3,3,3,3,3,3,3,3,3,3,3,3,3,3,3,3,3,3,3,3,3,4),(373.849525777369,
373.94177576414,374.034531391264,374.127549014038,374.220904227471,374.246432817409,
374.330179550111,374.413823227127,374.497383971193,374.58088183315,374.664344333713,
374.747789469205,374.831235304048,374.914699899286,374.998253084708,375.081850918281,
375.165582481142,375.245416319608,375.32916305231,375.412806729326,375.496367473393,
375.579865335349,375.663327835912,375.746772971404,375.830218806247,375.913683401485,
375.997236586907,376.08083442048,376.164565983342,376.244399821807,376.328146554509,
376.411790231525,376.495350975591,376.578848837548,376.66231133811,376.745756473603,
376.829202308445,376.912666903683,376.996220089105,377.079817922678,377.16354948554,
377.243383324007,377.327130056709,377.410773733725,377.494334477792,377.577832339749,
377.661294840311,377.744739975804,377.828185810647,377.911650405885,377.995203591307,
378.078801424879,378.162532987741,378.242366826206,378.326113558908,378.409757235924,
378.49331797999,378.576815841947,378.660278342509,378.743723478002,378.827169312844,
378.910633908082,378.994187093504,379.077784927077,379.161516489938,379.241350328405,
379.324006495365,379.40656044139,379.489033280296,379.571445359309,379.653825094266,
379.736191427966,379.818563289775,379.901003070109,379.983477649875,380.066065261914,
380.132711084231),.UNSPECIFIED.);
#474=B_SPLINE_CURVE_WITH_KNOTS('',3,(#59468,#59469,#59470,#59471,#59472,
#59473,#59474,#59475,#59476,#59477,#59478,#59479,#59480,#59481,#59482,#59483,
#59484,#59485,#59486,#59487,#59488,#59489,#59490,#59491,#59492,#59493,#59494,
#59495,#59496,#59497,#59498,#59499,#59500,#59501,#59502,#59503,#59504,#59505,
#59506,#59507,#59508,#59509,#59510,#59511,#59512,#59513,#59514,#59515,#59516,
#59517,#59518,#59519,#59520,#59521,#59522,#59523,#59524,#59525,#59526,#59527,
#59528,#59529,#59530,#59531,#59532,#59533,#59534,#59535,#59536,#59537,#59538,
#59539,#59540,#59541,#59542,#59543,#59544,#59545,#59546,#59547,#59548,#59549,
#59550,#59551,#59552,#59553,#59554,#59555,#59556,#59557,#59558,#59559,#59560,
#59561,#59562,#59563,#59564,#59565,#59566,#59567,#59568,#59569,#59570,#59571,
#59572,#59573,#59574,#59575,#59576,#59577,#59578,#59579,#59580,#59581,#59582,
#59583,#59584,#59585,#59586,#59587,#59588,#59589,#59590,#59591,#59592,#59593,
#59594,#59595,#59596,#59597,#59598,#59599,#59600,#59601,#59602,#59603,#59604,
#59605,#59606,#59607,#59608,#59609,#59610,#59611,#59612,#59613,#59614,#59615,
#59616,#59617,#59618,#59619,#59620,#59621,#59622,#59623,#59624,#59625,#59626,
#59627,#59628,#59629,#59630,#59631,#59632,#59633,#59634,#59635,#59636,#59637,
#59638,#59639,#59640,#59641,#59642,#59643,#59644,#59645,#59646,#59647,#59648,
#59649,#59650,#59651,#59652,#59653,#59654,#59655,#59656,#59657,#59658,#59659,
#59660,#59661,#59662,#59663,#59664,#59665,#59666,#59667,#59668,#59669,#59670,
#59671,#59672,#59673,#59674,#59675,#59676,#59677,#59678,#59679,#59680,#59681,
#59682,#59683,#59684,#59685,#59686,#59687,#59688,#59689,#59690,#59691,#59692,
#59693),.UNSPECIFIED.,.F.,.F.,(4,3,3,3,3,3,3,3,3,3,3,3,3,3,3,3,3,3,3,3,
3,3,3,3,3,3,3,3,3,3,3,3,3,3,3,3,3,3,3,3,3,3,3,3,3,3,3,3,3,3,3,3,3,3,3,3,
3,3,3,3,3,3,3,3,3,3,3,3,3,3,3,3,3,3,3,4),(380.132711084366,380.240333830604,
380.324080563306,380.407724240322,380.491284984388,380.574782846345,380.658245346908,
380.7416904824,380.825136317243,380.908600912481,380.992154097903,381.075751931475,
381.159483494337,381.239317332803,381.323064065505,381.406707742521,381.490268486588,
381.573766348544,381.657228849107,381.740673984599,381.824119819442,381.90758441468,
381.991137600102,382.074735433675,382.158466996537,382.238300835002,382.322047567704,
382.40569124472,382.489251988787,382.572749850743,382.656212351306,382.739657486798,
382.823103321641,382.90656791688,382.990121102302,383.073718935874,383.157450498736,
383.237284337202,383.321031069904,383.40467474692,383.488235490986,383.571733352943,
383.655195853506,383.738640988998,383.822086823841,383.905551419079,383.9891046045,
384.072702438073,384.156434000935,384.236267839401,384.320014572103,384.403658249119,
384.487218993185,384.570716855142,384.654179355705,384.737624491197,384.82107032604,
384.904534921278,384.9880881067,385.071685940273,385.155417503134,385.2352513416,
385.318998074302,385.402641751318,385.486202495384,385.569700357341,385.653162857904,
385.736607993396,385.820053828239,385.903518423477,385.987071608899,386.070669442471,
386.154401005333,386.234234843799,386.360598083892,386.415896391545),
 .UNSPECIFIED.);
#475=B_SPLINE_CURVE_WITH_KNOTS('',3,(#59695,#59696,#59697,#59698,#59699,
#59700,#59701,#59702,#59703,#59704,#59705,#59706,#59707,#59708,#59709,#59710,
#59711,#59712,#59713,#59714,#59715,#59716,#59717,#59718,#59719,#59720,#59721,
#59722,#59723,#59724,#59725,#59726,#59727,#59728,#59729,#59730,#59731,#59732,
#59733,#59734,#59735,#59736,#59737,#59738,#59739,#59740,#59741,#59742,#59743,
#59744,#59745,#59746,#59747,#59748,#59749,#59750,#59751,#59752,#59753,#59754,
#59755,#59756,#59757,#59758,#59759,#59760,#59761,#59762,#59763,#59764,#59765,
#59766,#59767,#59768,#59769,#59770,#59771,#59772,#59773,#59774,#59775,#59776,
#59777,#59778,#59779,#59780,#59781,#59782,#59783,#59784,#59785,#59786,#59787,
#59788,#59789,#59790,#59791,#59792,#59793,#59794,#59795,#59796,#59797,#59798,
#59799,#59800,#59801,#59802,#59803,#59804,#59805,#59806,#59807,#59808,#59809,
#59810,#59811,#59812,#59813,#59814,#59815,#59816,#59817,#59818,#59819,#59820,
#59821,#59822,#59823,#59824,#59825,#59826,#59827,#59828,#59829,#59830,#59831,
#59832,#59833,#59834,#59835,#59836,#59837,#59838,#59839,#59840,#59841,#59842,
#59843,#59844,#59845,#59846,#59847,#59848,#59849,#59850,#59851,#59852,#59853,
#59854,#59855,#59856,#59857,#59858,#59859,#59860,#59861,#59862,#59863,#59864,
#59865,#59866,#59867,#59868,#59869,#59870,#59871,#59872,#59873,#59874,#59875,
#59876,#59877,#59878,#59879,#59880,#59881,#59882,#59883,#59884,#59885,#59886,
#59887,#59888,#59889,#59890,#59891,#59892,#59893,#59894,#59895,#59896,#59897,
#59898,#59899,#59900,#59901,#59902,#59903,#59904,#59905,#59906,#59907,#59908,
#59909,#59910,#59911,#59912,#59913,#59914,#59915,#59916,#59917,#59918,#59919,
#59920,#59921,#59922,#59923),.UNSPECIFIED.,.F.,.F.,(4,3,3,3,3,3,3,3,3,3,
3,3,3,3,3,3,3,3,3,3,3,3,3,3,3,3,3,3,3,3,3,3,3,3,3,3,3,3,3,3,3,3,3,3,3,3,
3,3,3,3,3,3,3,3,3,3,3,3,3,3,3,3,3,3,3,3,3,3,3,3,3,3,3,3,3,3,4),(386.415896391695,
386.498269229996,386.580568110831,386.662817848132,386.745042157778,386.827260070869,
386.909490611058,386.991802728423,387.074155810137,387.156638349575,387.233218345998,
387.3169650787,387.400608755716,387.484169499782,387.567667361739,387.651129862302,
387.734574997794,387.818020832637,387.901485427875,387.985038613297,388.068636446869,
388.152368009731,388.232201848197,388.315948580899,388.399592257915,388.483153001981,
388.566650863938,388.650113364501,388.733558499993,388.817004334836,388.900468930075,
388.984022115496,389.067619949069,389.151351511931,389.231185350397,389.314932083099,
389.398575760115,389.482136504181,389.565634366138,389.6490968667,389.732542002193,
389.815987837035,389.899452432273,389.983005617695,390.066603451268,390.15033501413,
390.230168852596,390.313915585298,390.397559262314,390.48112000638,390.564617868337,
390.6480803689,390.731525504392,390.814971339235,390.898435934473,390.981989119895,
391.065586953468,391.14931851633,391.229152354795,391.312899087497,391.396542764513,
391.480103508579,391.563601370536,391.647063871099,391.730509006591,391.813954841434,
391.897419436672,391.980972622094,392.064570455667,392.148302018529,392.228135856994,
392.317403491653,392.406498888698,392.495356687292,392.584067633296,392.672582033764,
392.699081698604),.UNSPECIFIED.);
#476=B_SPLINE_CURVE_WITH_KNOTS('',3,(#59925,#59926,#59927,#59928,#59929,
#59930,#59931,#59932,#59933,#59934,#59935,#59936,#59937,#59938,#59939,#59940,
#59941,#59942,#59943,#59944,#59945,#59946,#59947,#59948,#59949,#59950,#59951,
#59952,#59953,#59954,#59955,#59956,#59957,#59958,#59959,#59960,#59961,#59962,
#59963,#59964,#59965,#59966,#59967,#59968,#59969,#59970,#59971,#59972,#59973,
#59974,#59975,#59976,#59977,#59978,#59979,#59980,#59981,#59982,#59983,#59984,
#59985,#59986,#59987,#59988,#59989,#59990,#59991,#59992,#59993,#59994,#59995,
#59996,#59997,#59998,#59999,#60000,#60001,#60002,#60003,#60004,#60005,#60006,
#60007,#60008,#60009,#60010,#60011,#60012,#60013,#60014,#60015,#60016,#60017,
#60018,#60019,#60020,#60021,#60022,#60023,#60024,#60025,#60026,#60027,#60028,
#60029,#60030,#60031,#60032,#60033,#60034,#60035,#60036,#60037,#60038,#60039,
#60040,#60041,#60042,#60043,#60044,#60045,#60046,#60047,#60048,#60049,#60050,
#60051,#60052,#60053,#60054,#60055,#60056,#60057,#60058,#60059,#60060,#60061,
#60062,#60063,#60064,#60065,#60066,#60067,#60068,#60069,#60070,#60071,#60072,
#60073,#60074,#60075,#60076,#60077,#60078,#60079,#60080,#60081,#60082,#60083,
#60084,#60085,#60086,#60087,#60088,#60089,#60090,#60091,#60092,#60093,#60094,
#60095,#60096,#60097,#60098,#60099,#60100,#60101,#60102,#60103,#60104,#60105,
#60106,#60107,#60108,#60109,#60110,#60111,#60112,#60113,#60114,#60115,#60116,
#60117,#60118,#60119,#60120,#60121,#60122,#60123,#60124,#60125,#60126,#60127,
#60128,#60129,#60130,#60131,#60132,#60133,#60134,#60135,#60136,#60137,#60138,
#60139,#60140,#60141,#60142,#60143,#60144,#60145,#60146,#60147,#60148,#60149,
#60150,#60151,#60152,#60153),.UNSPECIFIED.,.F.,.F.,(4,3,3,3,3,3,3,3,3,3,
3,3,3,3,3,3,3,3,3,3,3,3,3,3,3,3,3,3,3,3,3,3,3,3,3,3,3,3,3,3,3,3,3,3,3,3,
3,3,3,3,3,3,3,3,3,3,3,3,3,3,3,3,3,3,3,3,3,3,3,3,3,3,3,3,3,3,4),(392.699081698725,
392.785525392672,392.872050012387,392.960817349088,393.04760284035,393.137361099771,
393.227119359193,393.310866091895,393.394509768911,393.478070512978,393.561568374935,
393.645030875497,393.72847601099,393.811921845832,393.895386441071,393.978939626492,
394.062537460065,394.146269022927,394.226102861392,394.309849594094,394.39349327111,
394.477054015177,394.560551877134,394.644014377697,394.727459513189,394.810905348032,
394.89436994327,394.977923128692,395.061520962265,395.145252525127,395.225086363592,
395.308833096294,395.39247677331,395.476037517376,395.559535379333,395.642997879896,
395.726443015388,395.809888850231,395.893353445469,395.976906630891,396.060504464463,
396.144236027325,396.224069865791,396.307816598493,396.391460275509,396.475021019575,
396.558518881532,396.641981382094,396.725426517586,396.808872352429,396.892336947667,
396.975890133089,397.059487966661,397.143219529523,397.22305336799,397.306800100692,
397.390443777708,397.474004521774,397.557502383731,397.640964884294,397.724410019786,
397.807855854629,397.891320449867,397.974873635289,398.058471468862,398.142203031724,
398.222036870189,398.304753588746,398.389442765891,398.471956246877,398.554415754322,
398.636840229104,398.723196923304,398.805631483041,398.888083458935,398.970595974559,
398.982267005904),.UNSPECIFIED.);
#477=B_SPLINE_CURVE_WITH_KNOTS('',3,(#60155,#60156,#60157,#60158,#60159,
#60160,#60161,#60162,#60163,#60164,#60165,#60166,#60167,#60168,#60169,#60170,
#60171,#60172,#60173,#60174,#60175,#60176,#60177,#60178,#60179,#60180,#60181,
#60182,#60183,#60184,#60185,#60186,#60187,#60188,#60189,#60190,#60191,#60192,
#60193,#60194,#60195,#60196,#60197,#60198,#60199,#60200,#60201,#60202,#60203,
#60204,#60205,#60206,#60207,#60208,#60209,#60210,#60211,#60212,#60213,#60214,
#60215,#60216,#60217,#60218,#60219,#60220,#60221,#60222,#60223,#60224,#60225,
#60226,#60227,#60228,#60229,#60230,#60231,#60232,#60233,#60234,#60235,#60236,
#60237,#60238,#60239,#60240,#60241,#60242,#60243,#60244,#60245,#60246,#60247,
#60248,#60249,#60250,#60251,#60252,#60253,#60254,#60255,#60256,#60257,#60258,
#60259,#60260,#60261,#60262,#60263,#60264,#60265,#60266,#60267,#60268,#60269,
#60270,#60271,#60272,#60273,#60274,#60275,#60276,#60277,#60278,#60279,#60280,
#60281,#60282,#60283,#60284,#60285,#60286,#60287,#60288,#60289,#60290,#60291,
#60292,#60293,#60294,#60295,#60296,#60297,#60298,#60299,#60300,#60301,#60302,
#60303,#60304,#60305,#60306,#60307,#60308,#60309,#60310,#60311,#60312,#60313,
#60314,#60315,#60316,#60317,#60318,#60319,#60320,#60321,#60322,#60323,#60324,
#60325,#60326,#60327,#60328,#60329,#60330,#60331,#60332,#60333,#60334,#60335,
#60336,#60337,#60338,#60339,#60340,#60341,#60342,#60343,#60344,#60345,#60346,
#60347,#60348,#60349,#60350,#60351,#60352,#60353,#60354,#60355,#60356,#60357,
#60358,#60359,#60360,#60361,#60362,#60363,#60364,#60365,#60366,#60367,#60368,
#60369,#60370,#60371,#60372,#60373,#60374,#60375,#60376,#60377,#60378,#60379,
#60380,#60381,#60382,#60383),.UNSPECIFIED.,.F.,.F.,(4,3,3,3,3,3,3,3,3,3,
3,3,3,3,3,3,3,3,3,3,3,3,3,3,3,3,3,3,3,3,3,3,3,3,3,3,3,3,3,3,3,3,3,3,3,3,
3,3,3,3,3,3,3,3,3,3,3,3,3,3,3,3,3,3,3,3,3,3,3,3,3,3,3,3,3,3,4),(398.982267006032,
399.091341048604,399.203228576954,399.221020372388,399.30476710509,399.388410782106,
399.471971526173,399.555469388129,399.638931888692,399.722377024185,399.805822859028,
399.889287454266,399.972840639688,400.05643847326,400.140170036122,400.220003874587,
400.303750607289,400.387394284305,400.470955028371,400.554452890328,400.637915390891,
400.721360526383,400.804806361226,400.888270956464,400.971824141886,401.055421975458,
401.13915353832,401.218987376787,401.302734109489,401.386377786505,401.469938530572,
401.553436392528,401.636898893091,401.720344028583,401.803789863426,401.887254458664,
401.970807644086,402.054405477659,402.138137040521,402.217970878986,402.301717611688,
402.385361288704,402.46892203277,402.552419894727,402.635882395289,402.719327530782,
402.802773365624,402.886237960862,402.969791146284,403.053388979857,403.137120542718,
403.216954381185,403.300701113887,403.384344790903,403.467905534969,403.551403396926,
403.634865897489,403.718311032981,403.801756867824,403.885221463062,403.968774648484,
404.052372482056,404.136104044918,404.215937883384,404.299684616086,404.383328293102,
404.466889037168,404.550386899125,404.633849399687,404.71729453518,404.800740370022,
404.88420496526,404.967758150682,405.051355984255,405.135087547117,405.214921385583,
405.265452313084),.UNSPECIFIED.);
#478=B_SPLINE_CURVE_WITH_KNOTS('',3,(#60385,#60386,#60387,#60388,#60389,
#60390,#60391,#60392,#60393,#60394,#60395,#60396,#60397,#60398,#60399,#60400,
#60401,#60402,#60403,#60404,#60405,#60406,#60407,#60408,#60409,#60410,#60411,
#60412,#60413,#60414,#60415,#60416,#60417,#60418,#60419,#60420,#60421,#60422,
#60423,#60424,#60425,#60426,#60427,#60428,#60429,#60430,#60431,#60432,#60433,
#60434,#60435,#60436,#60437,#60438,#60439,#60440,#60441,#60442,#60443,#60444,
#60445,#60446,#60447,#60448,#60449,#60450,#60451,#60452,#60453,#60454,#60455,
#60456,#60457,#60458,#60459,#60460,#60461,#60462,#60463,#60464,#60465,#60466,
#60467,#60468,#60469,#60470,#60471,#60472,#60473,#60474,#60475,#60476,#60477,
#60478,#60479,#60480,#60481,#60482,#60483,#60484,#60485,#60486,#60487,#60488,
#60489,#60490,#60491,#60492,#60493,#60494,#60495,#60496,#60497,#60498,#60499,
#60500,#60501,#60502,#60503,#60504,#60505,#60506,#60507,#60508,#60509,#60510,
#60511,#60512,#60513,#60514,#60515,#60516,#60517,#60518,#60519,#60520,#60521,
#60522,#60523,#60524,#60525,#60526,#60527,#60528,#60529,#60530,#60531,#60532,
#60533,#60534,#60535,#60536,#60537,#60538,#60539,#60540,#60541,#60542,#60543,
#60544,#60545,#60546,#60547,#60548,#60549,#60550,#60551,#60552,#60553,#60554,
#60555,#60556,#60557,#60558,#60559,#60560,#60561,#60562,#60563,#60564,#60565,
#60566,#60567,#60568,#60569,#60570,#60571,#60572,#60573,#60574,#60575,#60576,
#60577,#60578,#60579,#60580,#60581,#60582,#60583,#60584,#60585,#60586,#60587,
#60588,#60589,#60590,#60591,#60592,#60593,#60594,#60595,#60596,#60597,#60598,
#60599,#60600,#60601,#60602,#60603,#60604,#60605,#60606,#60607,#60608,#60609,
#60610,#60611,#60612,#60613),.UNSPECIFIED.,.F.,.F.,(4,3,3,3,3,3,3,3,3,3,
3,3,3,3,3,3,3,3,3,3,3,3,3,3,3,3,3,3,3,3,3,3,3,3,3,3,3,3,3,3,3,3,3,3,3,3,
3,3,3,3,3,3,3,3,3,3,3,3,3,3,3,3,3,3,3,3,3,3,3,3,3,3,3,3,3,3,4),(405.265452313283,
405.348538923691,405.431525689357,405.514433352743,405.597282579425,405.680102760379,
405.762910725424,405.845725095357,405.928564492279,406.011493653704,406.094474155631,
406.177574913904,406.213904887782,406.297651620484,406.3812952975,406.464856041566,
406.548353903523,406.631816404086,406.715261539578,406.798707374421,406.882171969659,
406.965725155081,407.049322988654,407.133054551516,407.212888389982,407.296635122684,
407.3802787997,407.463839543766,407.547337405723,407.630799906285,407.714245041778,
407.797690876621,407.881155471859,407.964708657281,408.048306490853,408.132038053715,
408.211871892181,408.295618624883,408.379262301899,408.462823045965,408.546320907922,
408.629783408484,408.713228543977,408.796674378819,408.880138974057,408.963692159479,
409.047289993052,409.131021555914,409.21085539438,409.294602127082,409.378245804098,
409.461806548164,409.545304410121,409.628766910684,409.712212046176,409.795657881019,
409.879122476257,409.962675661679,410.046273495252,410.130005058113,410.209838896579,
410.293585629281,410.377229306297,410.460790050363,410.54428791232,410.627750412883,
410.711195548375,410.794641383218,410.878105978456,410.961659163878,411.04525699745,
411.128988560312,411.208822398778,411.306570851759,411.403897232893,411.500435641759,
411.548637620263),.UNSPECIFIED.);
#479=B_SPLINE_CURVE_WITH_KNOTS('',3,(#60615,#60616,#60617,#60618,#60619,
#60620,#60621,#60622,#60623,#60624),.UNSPECIFIED.,.F.,.F.,(4,1,1,1,1,1,
1,4),(411.548637620263,412.207805900977,413.206789403177,414.205772905376,
415.204756407575,416.203739909774,417.202723411973,417.831822927443),
 .UNSPECIFIED.);
#480=B_SPLINE_CURVE_WITH_KNOTS('',3,(#60626,#60627,#60628,#60629,#60630,
#60631,#60632,#60633,#60634,#60635,#60636,#60637,#60638,#60639,#60640,#60641,
#60642,#60643,#60644,#60645,#60646,#60647,#60648,#60649,#60650,#60651,#60652,
#60653,#60654,#60655,#60656,#60657,#60658,#60659,#60660,#60661,#60662,#60663,
#60664,#60665,#60666,#60667,#60668,#60669,#60670,#60671,#60672,#60673,#60674,
#60675,#60676,#60677,#60678,#60679,#60680,#60681,#60682,#60683,#60684,#60685,
#60686,#60687,#60688,#60689,#60690,#60691,#60692,#60693,#60694,#60695,#60696,
#60697,#60698,#60699,#60700,#60701,#60702,#60703,#60704,#60705,#60706,#60707,
#60708,#60709,#60710,#60711,#60712,#60713,#60714,#60715,#60716,#60717,#60718,
#60719,#60720,#60721,#60722,#60723,#60724,#60725,#60726,#60727,#60728,#60729,
#60730,#60731,#60732,#60733,#60734,#60735,#60736,#60737,#60738,#60739,#60740,
#60741,#60742,#60743,#60744,#60745,#60746,#60747,#60748,#60749,#60750,#60751,
#60752,#60753,#60754,#60755,#60756,#60757,#60758,#60759,#60760,#60761,#60762,
#60763,#60764,#60765,#60766,#60767,#60768,#60769,#60770,#60771,#60772,#60773,
#60774,#60775,#60776,#60777,#60778,#60779,#60780,#60781,#60782,#60783,#60784,
#60785,#60786,#60787,#60788,#60789,#60790,#60791,#60792,#60793,#60794,#60795,
#60796,#60797,#60798,#60799,#60800,#60801,#60802,#60803,#60804,#60805,#60806,
#60807,#60808,#60809,#60810,#60811,#60812,#60813,#60814,#60815,#60816,#60817,
#60818,#60819,#60820,#60821,#60822,#60823,#60824,#60825,#60826,#60827,#60828,
#60829,#60830,#60831,#60832,#60833,#60834,#60835,#60836,#60837,#60838,#60839,
#60840,#60841,#60842,#60843,#60844,#60845,#60846,#60847,#60848,#60849,#60850,
#60851),.UNSPECIFIED.,.F.,.F.,(4,3,3,3,3,3,3,3,3,3,3,3,3,3,3,3,3,3,3,3,
3,3,3,3,3,3,3,3,3,3,3,3,3,3,3,3,3,3,3,3,3,3,3,3,3,3,3,3,3,3,3,3,3,3,3,3,
3,3,3,3,3,3,3,3,3,3,3,3,3,3,3,3,3,3,3,4),(417.831822927443,417.926099988475,
418.020755754091,418.115941577717,418.201706914172,418.285453646874,418.36909732389,
418.452658067957,418.536155929914,418.619618430476,418.703063565969,418.786509400811,
418.869973996049,418.953527181471,419.037125015044,419.120856577906,419.200690416372,
419.284437149074,419.36808082609,419.451641570156,419.535139432113,419.618601932676,
419.702047068168,419.785492903011,419.868957498249,419.952510683671,420.036108517243,
420.119840080105,420.199673918571,420.283420651273,420.367064328289,420.450625072355,
420.534122934312,420.617585434875,420.701030570367,420.78447640521,420.867941000448,
420.95149418587,421.035092019442,421.118823582304,421.19865742077,421.282404153472,
421.366047830488,421.449608574554,421.533106436511,421.616568937073,421.700014072566,
421.783459907408,421.866924502646,421.950477688068,422.034075521641,422.117807084503,
422.197640922969,422.281387655671,422.365031332687,422.448592076753,422.53208993871,
422.615552439273,422.698997574765,422.782443409608,422.865908004846,422.949461190268,
423.03305902384,423.116790586702,423.196624425168,423.27945481212,423.362182857043,
423.444829539153,423.52860187607,423.611154980827,423.693694510841,423.776239281408,
423.86093151968,423.94358394385,424.029296089172,424.115008234493),
 .UNSPECIFIED.);
#481=B_SPLINE_CURVE_WITH_KNOTS('',3,(#60853,#60854,#60855,#60856,#60857,
#60858,#60859,#60860,#60861,#60862,#60863,#60864,#60865,#60866,#60867,#60868,
#60869,#60870,#60871,#60872,#60873,#60874,#60875,#60876,#60877,#60878,#60879,
#60880,#60881,#60882,#60883,#60884,#60885,#60886,#60887,#60888,#60889,#60890,
#60891,#60892,#60893,#60894,#60895,#60896,#60897,#60898,#60899,#60900,#60901,
#60902,#60903,#60904,#60905,#60906,#60907,#60908,#60909,#60910,#60911,#60912,
#60913,#60914,#60915,#60916,#60917,#60918,#60919,#60920,#60921,#60922,#60923,
#60924,#60925,#60926,#60927,#60928,#60929,#60930,#60931,#60932,#60933,#60934,
#60935,#60936,#60937,#60938,#60939,#60940,#60941,#60942,#60943,#60944,#60945,
#60946,#60947,#60948,#60949,#60950,#60951,#60952,#60953,#60954,#60955,#60956,
#60957,#60958,#60959,#60960,#60961,#60962,#60963,#60964,#60965,#60966,#60967,
#60968,#60969,#60970,#60971,#60972,#60973,#60974,#60975,#60976,#60977,#60978,
#60979,#60980,#60981,#60982,#60983,#60984,#60985,#60986,#60987,#60988,#60989,
#60990,#60991,#60992,#60993,#60994,#60995,#60996,#60997,#60998,#60999,#61000,
#61001,#61002,#61003,#61004,#61005,#61006,#61007,#61008,#61009,#61010,#61011,
#61012,#61013,#61014,#61015,#61016,#61017,#61018,#61019,#61020,#61021,#61022,
#61023,#61024,#61025,#61026,#61027,#61028,#61029,#61030,#61031,#61032,#61033,
#61034,#61035,#61036,#61037,#61038,#61039,#61040,#61041,#61042,#61043,#61044,
#61045,#61046,#61047,#61048,#61049,#61050,#61051,#61052,#61053,#61054,#61055,
#61056,#61057,#61058,#61059,#61060,#61061,#61062,#61063,#61064,#61065,#61066,
#61067,#61068,#61069,#61070,#61071,#61072,#61073,#61074,#61075,#61076,#61077,
#61078),.UNSPECIFIED.,.F.,.F.,(4,3,3,3,3,3,3,3,3,3,3,3,3,3,3,3,3,3,3,3,
3,3,3,3,3,3,3,3,3,3,3,3,3,3,3,3,3,3,3,3,3,3,3,3,3,3,3,3,3,3,3,3,3,3,3,3,
3,3,3,3,3,3,3,3,3,3,3,3,3,3,3,3,3,3,3,4),(424.115008234623,424.195607927367,
424.279354660069,424.362998337085,424.446559081151,424.530056943108,424.61351944367,
424.696964579163,424.780410414005,424.863875009243,424.947428194665,425.031026028238,
425.1147575911,425.194591429567,425.278338162269,425.361981839285,425.445542583352,
425.529040445308,425.612502945871,425.695948081363,425.779393916206,425.862858511444,
425.946411696866,426.030009530439,426.113741093301,426.193574931766,426.277321664468,
426.360965341484,426.44452608555,426.528023947507,426.61148644807,426.694931583562,
426.778377418405,426.861842013643,426.945395199064,427.028993032637,427.112724595499,
427.192558433965,427.276305166667,427.359948843683,427.443509587749,427.527007449706,
427.610469950269,427.693915085761,427.777360920604,427.860825515842,427.944378701264,
428.027976534836,428.111708097698,428.191541936164,428.275288668866,428.358932345882,
428.442493089948,428.525990951905,428.609453452467,428.69289858796,428.776344422802,
428.85980901804,428.943362203462,429.026960037035,429.110691599897,429.190525438363,
429.274272171065,429.357915848081,429.441476592147,429.524974454104,429.608436954667,
429.691882090159,429.775327925002,429.85879252024,429.942345705662,430.025943539235,
430.109675102096,430.189508940562,430.307067979204,430.398193541802),
 .UNSPECIFIED.);
#482=B_SPLINE_CURVE_WITH_KNOTS('',3,(#61080,#61081,#61082,#61083,#61084,
#61085,#61086,#61087,#61088,#61089,#61090,#61091,#61092,#61093,#61094,#61095,
#61096,#61097,#61098,#61099,#61100,#61101,#61102,#61103,#61104,#61105,#61106,
#61107,#61108,#61109,#61110,#61111,#61112,#61113,#61114,#61115,#61116,#61117,
#61118,#61119,#61120,#61121,#61122,#61123,#61124,#61125,#61126,#61127,#61128,
#61129,#61130,#61131,#61132,#61133,#61134,#61135,#61136,#61137,#61138,#61139,
#61140,#61141,#61142,#61143,#61144,#61145,#61146,#61147,#61148,#61149,#61150,
#61151,#61152,#61153,#61154,#61155,#61156,#61157,#61158,#61159,#61160,#61161,
#61162,#61163,#61164,#61165,#61166,#61167,#61168,#61169,#61170,#61171,#61172,
#61173,#61174,#61175,#61176,#61177,#61178,#61179,#61180,#61181,#61182,#61183,
#61184,#61185,#61186,#61187,#61188,#61189,#61190,#61191,#61192,#61193,#61194,
#61195,#61196,#61197,#61198,#61199,#61200,#61201,#61202,#61203,#61204,#61205,
#61206,#61207,#61208,#61209,#61210,#61211,#61212,#61213,#61214,#61215,#61216,
#61217,#61218,#61219,#61220,#61221,#61222,#61223,#61224,#61225,#61226,#61227,
#61228,#61229,#61230,#61231,#61232,#61233,#61234,#61235,#61236,#61237,#61238,
#61239,#61240,#61241,#61242,#61243,#61244,#61245,#61246,#61247,#61248,#61249,
#61250,#61251,#61252,#61253,#61254,#61255,#61256,#61257,#61258,#61259,#61260,
#61261,#61262,#61263,#61264,#61265,#61266,#61267,#61268,#61269,#61270,#61271,
#61272,#61273,#61274,#61275,#61276,#61277,#61278,#61279,#61280,#61281,#61282,
#61283,#61284,#61285,#61286,#61287,#61288,#61289,#61290,#61291,#61292,#61293,
#61294,#61295,#61296,#61297,#61298,#61299,#61300,#61301,#61302,#61303,#61304,
#61305,#61306,#61307,#61308),.UNSPECIFIED.,.F.,.F.,(4,3,3,3,3,3,3,3,3,3,
3,3,3,3,3,3,3,3,3,3,3,3,3,3,3,3,3,3,3,3,3,3,3,3,3,3,3,3,3,3,3,3,3,3,3,3,
3,3,3,3,3,3,3,3,3,3,3,3,3,3,3,3,3,3,3,3,3,3,3,3,3,3,3,3,3,3,4),(430.398193541946,
430.480597550544,430.562935285471,430.645234069969,430.72751428009,430.809794904858,
430.892094931353,430.974480349292,431.056912748385,431.139467268808,431.188492442761,
431.272239175463,431.355882852479,431.439443596545,431.522941458502,431.606403959065,
431.689849094557,431.7732949294,431.856759524638,431.94031271006,432.023910543632,
432.107642106494,432.187475944961,432.271222677663,432.354866354679,432.438427098745,
432.521924960702,432.605387461264,432.688832596757,432.7722784316,432.855743026838,
432.93929621226,433.022894045833,433.106625608695,433.18645944716,433.270206179862,
433.353849856878,433.437410600944,433.5209084629,433.604370963463,433.687816098955,
433.771261933798,433.854726529036,433.938279714458,434.021877548031,434.105609110892,
434.185442949359,434.269189682061,434.352833359077,434.436394103143,434.5198919651,
434.603354465662,434.686799601155,434.770245435998,434.853710031236,434.937263216658,
435.02086105023,435.104592613092,435.184426451558,435.26817318426,435.351816861276,
435.435377605342,435.518875467299,435.602337967861,435.685783103354,435.769228938196,
435.852693533434,435.936246718856,436.019844552429,436.10357611529,436.183409953757,
436.271527674377,436.359492756615,436.447255588697,436.534897976604,436.622381849063,
436.681378848596),.UNSPECIFIED.);
#483=B_SPLINE_CURVE_WITH_KNOTS('',3,(#61310,#61311,#61312,#61313,#61314,
#61315,#61316,#61317,#61318,#61319,#61320,#61321,#61322,#61323,#61324,#61325,
#61326,#61327,#61328,#61329,#61330,#61331,#61332,#61333,#61334,#61335,#61336,
#61337,#61338,#61339,#61340,#61341,#61342,#61343,#61344,#61345,#61346,#61347,
#61348,#61349,#61350,#61351,#61352,#61353,#61354,#61355,#61356,#61357,#61358,
#61359,#61360,#61361,#61362,#61363,#61364,#61365,#61366,#61367,#61368,#61369,
#61370,#61371,#61372,#61373,#61374,#61375,#61376,#61377,#61378,#61379,#61380,
#61381,#61382,#61383,#61384,#61385,#61386,#61387,#61388,#61389,#61390,#61391,
#61392,#61393,#61394,#61395,#61396,#61397,#61398,#61399,#61400,#61401,#61402,
#61403,#61404,#61405,#61406,#61407,#61408,#61409,#61410,#61411,#61412,#61413,
#61414,#61415,#61416,#61417,#61418,#61419,#61420,#61421,#61422,#61423,#61424,
#61425,#61426,#61427,#61428,#61429,#61430,#61431,#61432,#61433,#61434,#61435,
#61436,#61437,#61438,#61439,#61440,#61441,#61442,#61443,#61444,#61445,#61446,
#61447,#61448,#61449,#61450,#61451,#61452,#61453,#61454,#61455,#61456,#61457,
#61458,#61459,#61460,#61461,#61462,#61463,#61464,#61465,#61466,#61467,#61468,
#61469,#61470,#61471,#61472,#61473,#61474,#61475,#61476,#61477,#61478,#61479,
#61480,#61481,#61482,#61483,#61484,#61485,#61486,#61487,#61488,#61489,#61490,
#61491,#61492,#61493,#61494,#61495,#61496,#61497,#61498,#61499,#61500,#61501,
#61502,#61503,#61504,#61505,#61506,#61507,#61508,#61509,#61510,#61511,#61512,
#61513,#61514,#61515,#61516,#61517,#61518,#61519,#61520,#61521,#61522,#61523,
#61524,#61525,#61526,#61527,#61528,#61529,#61530,#61531,#61532,#61533,#61534,
#61535,#61536,#61537,#61538),.UNSPECIFIED.,.F.,.F.,(4,3,3,3,3,3,3,3,3,3,
3,3,3,3,3,3,3,3,3,3,3,3,3,3,3,3,3,3,3,3,3,3,3,3,3,3,3,3,3,3,3,3,3,3,3,3,
3,3,3,3,3,3,3,3,3,3,3,3,3,3,3,3,3,3,3,3,3,3,3,3,3,3,3,3,3,3,4),(436.681378848982,
436.768731500326,436.856196957168,436.943866686287,437.031644010499,437.119621670839,
437.182393455956,437.266140188658,437.349783865674,437.43334460974,437.516842471697,
437.60030497226,437.683750107752,437.767195942595,437.850660537833,437.934213723255,
438.017811556828,438.10154311969,438.181376958156,438.265123690858,438.348767367874,
438.432328111941,438.515825973897,438.59928847446,438.682733609952,438.766179444795,
438.849644040033,438.933197225455,439.016795059028,439.10052662189,439.180360460355,
439.264107193057,439.347750870073,439.431311614139,439.514809476096,439.598271976659,
439.681717112151,439.765162946994,439.848627542231,439.932180727653,440.015778561226,
440.099510124088,440.179343962554,440.263090695256,440.346734372272,440.430295116338,
440.513792978295,440.597255478857,440.68070061435,440.764146449192,440.84761104443,
440.931164229852,441.014762063425,441.098493626287,441.178327464753,441.262074197455,
441.345717874471,441.429278618538,441.512776480494,441.596238981057,441.679684116549,
441.763129951392,441.84659454663,441.930147732052,442.013745565625,442.097477128487,
442.177310966952,442.259891588733,442.342368707561,442.424750977318,442.507080149116,
442.589375248686,442.671655270268,442.753967832792,442.836297761573,442.918702822903,
442.964564156035),.UNSPECIFIED.);
#484=B_SPLINE_CURVE_WITH_KNOTS('',3,(#61540,#61541,#61542,#61543,#61544,
#61545,#61546,#61547,#61548,#61549,#61550,#61551,#61552,#61553,#61554,#61555,
#61556,#61557,#61558,#61559,#61560,#61561,#61562,#61563,#61564,#61565,#61566,
#61567,#61568,#61569,#61570,#61571,#61572,#61573,#61574,#61575,#61576,#61577,
#61578,#61579,#61580,#61581,#61582,#61583,#61584,#61585,#61586,#61587,#61588,
#61589,#61590,#61591,#61592,#61593,#61594,#61595,#61596,#61597,#61598,#61599,
#61600,#61601,#61602,#61603,#61604,#61605,#61606,#61607,#61608,#61609,#61610,
#61611,#61612,#61613,#61614,#61615,#61616,#61617,#61618,#61619,#61620,#61621,
#61622,#61623,#61624,#61625,#61626,#61627,#61628,#61629,#61630,#61631,#61632,
#61633,#61634,#61635,#61636,#61637,#61638,#61639,#61640,#61641,#61642,#61643,
#61644,#61645,#61646,#61647,#61648,#61649,#61650,#61651,#61652,#61653,#61654,
#61655,#61656,#61657,#61658,#61659,#61660,#61661,#61662,#61663,#61664,#61665,
#61666,#61667,#61668,#61669,#61670,#61671,#61672,#61673,#61674,#61675,#61676,
#61677,#61678,#61679,#61680,#61681,#61682,#61683,#61684,#61685,#61686,#61687,
#61688,#61689,#61690,#61691,#61692,#61693,#61694,#61695,#61696,#61697,#61698,
#61699,#61700,#61701,#61702,#61703,#61704,#61705,#61706,#61707,#61708,#61709,
#61710,#61711,#61712,#61713,#61714,#61715,#61716,#61717,#61718,#61719,#61720,
#61721,#61722,#61723,#61724,#61725,#61726,#61727,#61728,#61729,#61730,#61731,
#61732,#61733,#61734,#61735,#61736,#61737,#61738,#61739,#61740,#61741,#61742,
#61743,#61744,#61745,#61746,#61747,#61748,#61749,#61750,#61751,#61752,#61753,
#61754,#61755,#61756,#61757,#61758,#61759,#61760,#61761,#61762,#61763,#61764,
#61765),.UNSPECIFIED.,.F.,.F.,(4,3,3,3,3,3,3,3,3,3,3,3,3,3,3,3,3,3,3,3,
3,3,3,3,3,3,3,3,3,3,3,3,3,3,3,3,3,3,3,3,3,3,3,3,3,3,3,3,3,3,3,3,3,3,3,3,
3,3,3,3,3,3,3,3,3,3,3,3,3,3,3,3,3,3,3,4),(442.964564156161,443.081306905342,
443.176294469151,443.260041201853,443.343684878869,443.427245622936,443.510743484892,
443.594205985455,443.677651120947,443.76109695579,443.844561551028,443.92811473645,
444.011712570023,444.095444132884,444.175277971351,444.259024704053,444.342668381069,
444.426229125136,444.509726987092,444.593189487655,444.676634623147,444.76008045799,
444.843545053228,444.92709823865,445.010696072223,445.094427635084,445.17426147355,
445.258008206252,445.341651883268,445.425212627334,445.508710489291,445.592172989853,
445.675618125346,445.759063960188,445.842528555426,445.926081740848,446.009679574421,
446.093411137283,446.173244975749,446.256991708451,446.340635385467,446.424196129533,
446.50769399149,446.591156492053,446.674601627545,446.758047462388,446.841512057626,
446.925065243048,447.00866307662,447.092394639482,447.172228477948,447.25597521065,
447.339618887666,447.423179631732,447.506677493689,447.590139994252,447.673585129744,
447.757030964587,447.840495559825,447.924048745246,448.007646578819,448.091378141681,
448.171211980147,448.254958712849,448.338602389865,448.422163133931,448.505660995888,
448.58912349645,448.672568631943,448.756014466786,448.839479062024,448.923032247446,
449.006630081018,449.09036164388,449.170195482346,449.247749463341),
 .UNSPECIFIED.);
#485=B_SPLINE_CURVE_WITH_KNOTS('',3,(#61767,#61768,#61769,#61770,#61771,
#61772,#61773,#61774,#61775,#61776,#61777,#61778,#61779,#61780,#61781,#61782,
#61783,#61784,#61785,#61786,#61787,#61788,#61789,#61790,#61791,#61792,#61793,
#61794,#61795,#61796,#61797,#61798,#61799,#61800,#61801,#61802,#61803,#61804,
#61805,#61806,#61807,#61808,#61809,#61810,#61811,#61812,#61813,#61814,#61815,
#61816,#61817,#61818,#61819,#61820,#61821,#61822,#61823,#61824,#61825,#61826,
#61827,#61828,#61829,#61830,#61831,#61832,#61833,#61834,#61835,#61836,#61837,
#61838,#61839,#61840,#61841,#61842,#61843,#61844,#61845,#61846,#61847,#61848,
#61849,#61850,#61851,#61852,#61853,#61854,#61855,#61856,#61857,#61858,#61859,
#61860,#61861,#61862,#61863,#61864,#61865,#61866,#61867,#61868,#61869,#61870,
#61871,#61872,#61873,#61874,#61875,#61876,#61877,#61878,#61879,#61880,#61881,
#61882,#61883,#61884,#61885,#61886,#61887,#61888,#61889,#61890,#61891,#61892,
#61893,#61894,#61895,#61896,#61897,#61898,#61899,#61900,#61901,#61902,#61903,
#61904,#61905,#61906,#61907,#61908,#61909,#61910,#61911,#61912,#61913,#61914,
#61915,#61916,#61917,#61918,#61919,#61920,#61921,#61922,#61923,#61924,#61925,
#61926,#61927,#61928,#61929,#61930,#61931,#61932,#61933,#61934,#61935,#61936,
#61937,#61938,#61939,#61940,#61941,#61942,#61943,#61944,#61945,#61946,#61947,
#61948,#61949,#61950,#61951,#61952,#61953,#61954,#61955,#61956,#61957,#61958,
#61959,#61960,#61961,#61962,#61963,#61964,#61965,#61966,#61967,#61968,#61969,
#61970,#61971,#61972,#61973,#61974,#61975,#61976,#61977,#61978,#61979,#61980,
#61981,#61982,#61983,#61984,#61985,#61986,#61987,#61988,#61989,#61990,#61991,
#61992),.UNSPECIFIED.,.F.,.F.,(4,3,3,3,3,3,3,3,3,3,3,3,3,3,3,3,3,3,3,3,
3,3,3,3,3,3,3,3,3,3,3,3,3,3,3,3,3,3,3,3,3,3,3,3,3,3,3,3,3,3,3,3,3,3,3,3,
3,3,3,3,3,3,3,3,3,3,3,3,3,3,3,3,3,3,3,4),(449.247749463469,449.330572004686,
449.413298292432,449.495949259883,449.580102975466,449.662675299464,449.745239696899,
449.827814966215,449.913155970798,449.995853631113,450.082516307829,450.169178984546,
450.252925717248,450.336569394264,450.42013013833,450.503628000287,450.58709050085,
450.670535636342,450.753981471185,450.837446066423,450.920999251845,451.004597085417,
451.088328648279,451.168162486745,451.251909219447,451.335552896463,451.419113640529,
451.502611502486,451.586074003048,451.669519138541,451.752964973383,451.836429568622,
451.919982754043,452.003580587616,452.087312150478,452.167145988944,452.250892721646,
452.334536398662,452.418097142728,452.501595004685,452.585057505248,452.66850264074,
452.751948475583,452.835413070821,452.918966256243,453.002564089816,453.086295652677,
453.166129491143,453.249876223845,453.333519900861,453.417080644927,453.500578506883,
453.584041007446,453.667486142938,453.750931977781,453.834396573019,453.917949758441,
454.001547592014,454.085279154875,454.165112993342,454.248859726044,454.33250340306,
454.416064147126,454.499562009083,454.583024509646,454.666469645138,454.749915479981,
454.833380075219,454.91693326064,455.000531094213,455.084262657075,455.164096495541,
455.259513492123,455.354608932559,455.449086084506,455.530934770324),
 .UNSPECIFIED.);
#486=B_SPLINE_CURVE_WITH_KNOTS('',3,(#61994,#61995,#61996,#61997,#61998,
#61999,#62000,#62001,#62002,#62003,#62004,#62005,#62006,#62007,#62008,#62009,
#62010,#62011,#62012,#62013,#62014,#62015,#62016,#62017,#62018,#62019,#62020,
#62021,#62022,#62023,#62024,#62025,#62026,#62027,#62028,#62029,#62030,#62031,
#62032,#62033,#62034,#62035,#62036,#62037,#62038,#62039,#62040,#62041,#62042,
#62043,#62044,#62045,#62046,#62047,#62048,#62049,#62050,#62051,#62052,#62053,
#62054,#62055,#62056,#62057,#62058,#62059,#62060,#62061,#62062,#62063,#62064,
#62065,#62066,#62067,#62068,#62069,#62070,#62071,#62072,#62073,#62074,#62075,
#62076,#62077,#62078,#62079,#62080,#62081,#62082,#62083,#62084,#62085,#62086,
#62087,#62088,#62089,#62090,#62091,#62092,#62093,#62094,#62095,#62096,#62097,
#62098,#62099,#62100,#62101,#62102,#62103,#62104,#62105,#62106,#62107,#62108,
#62109,#62110,#62111,#62112,#62113,#62114,#62115,#62116,#62117,#62118,#62119,
#62120,#62121,#62122,#62123,#62124,#62125,#62126,#62127,#62128,#62129,#62130,
#62131,#62132,#62133,#62134,#62135,#62136,#62137,#62138,#62139,#62140,#62141,
#62142,#62143,#62144,#62145,#62146,#62147,#62148,#62149,#62150,#62151,#62152,
#62153,#62154,#62155,#62156,#62157,#62158,#62159,#62160,#62161,#62162,#62163,
#62164,#62165,#62166,#62167,#62168,#62169,#62170,#62171,#62172,#62173,#62174,
#62175,#62176,#62177,#62178,#62179,#62180,#62181,#62182,#62183,#62184,#62185,
#62186,#62187,#62188,#62189,#62190,#62191,#62192,#62193,#62194,#62195,#62196,
#62197,#62198,#62199,#62200,#62201,#62202,#62203,#62204,#62205,#62206,#62207,
#62208,#62209,#62210,#62211,#62212,#62213,#62214,#62215,#62216,#62217,#62218,
#62219,#62220,#62221,#62222),.UNSPECIFIED.,.F.,.F.,(4,3,3,3,3,3,3,3,3,3,
3,3,3,3,3,3,3,3,3,3,3,3,3,3,3,3,3,3,3,3,3,3,3,3,3,3,3,3,3,3,3,3,3,3,3,3,
3,3,3,3,3,3,3,3,3,3,3,3,3,3,3,3,3,3,3,3,3,3,3,3,3,3,3,3,3,3,4),(455.53093477052,
455.614864815332,455.698797940928,455.782751521101,455.866742939129,455.950841680949,
456.035000609231,456.119294244176,456.163079997741,456.246826730443,456.330470407459,
456.414031151525,456.497529013482,456.580991514045,456.664436649537,456.74788248438,
456.831347079618,456.91490026504,456.998498098613,457.082229661475,457.16206349994,
457.245810232642,457.329453909658,457.413014653724,457.496512515681,457.579975016244,
457.663420151736,457.746865986578,457.830330581816,457.913883767238,457.997481600811,
458.081213163673,458.161047002139,458.244793734841,458.328437411857,458.411998155923,
458.49549601788,458.578958518442,458.662403653935,458.745849488777,458.829314084015,
458.912867269437,458.99646510301,459.080196665872,459.160030504338,459.24377723704,
459.327420914056,459.410981658123,459.494479520079,459.577942020642,459.661387156134,
459.744832990977,459.828297586215,459.911850771636,459.995448605209,460.079180168071,
460.159014006537,460.242760739239,460.326404416255,460.409965160321,460.493463022277,
460.57692552284,460.660370658332,460.743816493175,460.827281088413,460.910834273835,
460.994432107408,461.07816367027,461.157997508736,461.241847586848,461.32559581153,
461.40926024753,461.492858897943,461.57641249266,461.659938082167,461.74347381492,
461.8141200777),.UNSPECIFIED.);
#487=B_SPLINE_CURVE_WITH_KNOTS('',3,(#62224,#62225,#62226,#62227,#62228,
#62229,#62230,#62231,#62232,#62233,#62234,#62235,#62236,#62237,#62238,#62239,
#62240,#62241,#62242,#62243,#62244,#62245,#62246,#62247,#62248,#62249,#62250,
#62251,#62252,#62253,#62254,#62255,#62256,#62257,#62258,#62259,#62260,#62261,
#62262,#62263,#62264,#62265,#62266,#62267,#62268,#62269,#62270,#62271,#62272,
#62273,#62274,#62275,#62276,#62277,#62278,#62279,#62280,#62281,#62282,#62283,
#62284,#62285,#62286,#62287,#62288,#62289,#62290,#62291,#62292,#62293,#62294,
#62295,#62296,#62297,#62298,#62299,#62300,#62301,#62302,#62303,#62304,#62305,
#62306,#62307,#62308,#62309,#62310,#62311,#62312,#62313,#62314,#62315,#62316,
#62317,#62318,#62319,#62320,#62321,#62322,#62323,#62324,#62325,#62326,#62327,
#62328,#62329,#62330,#62331,#62332,#62333,#62334,#62335,#62336,#62337,#62338,
#62339,#62340,#62341,#62342,#62343,#62344,#62345,#62346,#62347,#62348,#62349,
#62350,#62351,#62352,#62353,#62354,#62355,#62356,#62357,#62358,#62359,#62360,
#62361,#62362,#62363,#62364,#62365,#62366,#62367,#62368,#62369,#62370,#62371,
#62372,#62373,#62374,#62375,#62376,#62377,#62378,#62379,#62380,#62381,#62382,
#62383,#62384,#62385,#62386,#62387,#62388,#62389,#62390,#62391,#62392,#62393,
#62394,#62395,#62396,#62397,#62398,#62399,#62400,#62401,#62402,#62403,#62404,
#62405,#62406,#62407,#62408,#62409,#62410,#62411,#62412,#62413,#62414,#62415,
#62416,#62417,#62418,#62419,#62420,#62421,#62422,#62423,#62424,#62425,#62426,
#62427,#62428,#62429,#62430,#62431,#62432,#62433,#62434,#62435,#62436,#62437,
#62438,#62439,#62440,#62441,#62442,#62443,#62444,#62445,#62446,#62447,#62448,
#62449,#62450,#62451,#62452),.UNSPECIFIED.,.F.,.F.,(4,3,3,3,3,3,3,3,3,3,
3,3,3,3,3,3,3,3,3,3,3,3,3,3,3,3,3,3,3,3,3,3,3,3,3,3,3,3,3,3,3,3,3,3,3,3,
3,3,3,3,3,3,3,3,3,3,3,3,3,3,3,3,3,3,3,3,3,3,3,3,3,3,3,3,3,3,4),(461.814120077892,
461.910496951514,462.007387650879,462.104909978552,462.156981010936,462.240727743638,
462.324371420654,462.40793216472,462.491430026677,462.57489252724,462.658337662732,
462.741783497575,462.825248092813,462.908801278235,462.992399111808,463.07613067467,
463.155964513135,463.239711245837,463.323354922853,463.406915666919,463.490413528876,
463.573876029438,463.657321164931,463.740766999773,463.824231595011,463.907784780433,
463.991382614006,464.075114176868,464.154948015334,464.238694748036,464.322338425052,
464.405899169118,464.489397031075,464.572859531638,464.65630466713,464.739750501973,
464.823215097211,464.906768282632,464.990366116205,465.074097679067,465.153931517533,
465.237678250235,465.321321927251,465.404882671317,465.488380533274,465.571843033837,
465.655288169329,465.738734004172,465.82219859941,465.905751784832,465.989349618404,
466.073081181266,466.152915019732,466.236661752434,466.32030542945,466.403866173516,
466.487364035473,466.570826536035,466.654271671528,466.737717506371,466.821182101609,
466.90473528703,466.988333120603,467.072064683465,467.151898521931,467.234968494349,
467.317935906293,467.400821539011,467.487882019731,467.57067232615,467.653448950727,
467.736230537978,467.819035732687,467.901927051323,467.984868586552,468.06792491431,
468.097305384775),.UNSPECIFIED.);
#488=B_SPLINE_CURVE_WITH_KNOTS('',3,(#62454,#62455,#62456,#62457,#62458,
#62459,#62460,#62461,#62462,#62463,#62464,#62465,#62466,#62467,#62468,#62469,
#62470,#62471,#62472,#62473,#62474,#62475,#62476,#62477,#62478,#62479,#62480,
#62481,#62482,#62483,#62484,#62485,#62486,#62487,#62488,#62489,#62490,#62491,
#62492,#62493,#62494,#62495,#62496,#62497,#62498,#62499,#62500,#62501,#62502,
#62503,#62504,#62505,#62506,#62507,#62508,#62509,#62510,#62511,#62512,#62513,
#62514,#62515,#62516,#62517,#62518,#62519,#62520,#62521,#62522,#62523,#62524,
#62525,#62526,#62527,#62528,#62529,#62530,#62531,#62532,#62533,#62534,#62535,
#62536,#62537,#62538,#62539,#62540,#62541,#62542,#62543,#62544,#62545,#62546,
#62547,#62548,#62549,#62550,#62551,#62552,#62553,#62554,#62555,#62556,#62557,
#62558,#62559,#62560,#62561,#62562,#62563,#62564,#62565,#62566,#62567,#62568,
#62569,#62570,#62571,#62572,#62573,#62574,#62575,#62576,#62577,#62578,#62579,
#62580,#62581,#62582,#62583,#62584,#62585,#62586,#62587,#62588,#62589,#62590,
#62591,#62592,#62593,#62594,#62595,#62596,#62597,#62598,#62599,#62600,#62601,
#62602,#62603,#62604,#62605,#62606,#62607,#62608,#62609,#62610,#62611,#62612,
#62613,#62614,#62615,#62616,#62617,#62618,#62619,#62620,#62621,#62622,#62623,
#62624,#62625,#62626,#62627,#62628,#62629,#62630,#62631,#62632,#62633,#62634,
#62635,#62636,#62637,#62638,#62639,#62640,#62641,#62642,#62643,#62644,#62645,
#62646,#62647,#62648,#62649,#62650,#62651,#62652,#62653,#62654,#62655,#62656,
#62657,#62658,#62659,#62660,#62661,#62662,#62663,#62664,#62665,#62666,#62667,
#62668,#62669,#62670,#62671,#62672,#62673,#62674,#62675,#62676,#62677,#62678,
#62679,#62680,#62681,#62682),.UNSPECIFIED.,.F.,.F.,(4,3,3,3,3,3,3,3,3,3,
3,3,3,3,3,3,3,3,3,3,3,3,3,3,3,3,3,3,3,3,3,3,3,3,3,3,3,3,3,3,3,3,3,3,3,3,
3,3,3,3,3,3,3,3,3,3,3,3,3,3,3,3,3,3,3,3,3,3,3,3,3,3,3,3,3,3,4),(468.097305384879,
468.150882024131,468.234628756833,468.318272433849,468.401833177915,468.485331039872,
468.568793540435,468.652238675927,468.73568451077,468.819149106008,468.90270229143,
468.986300125003,469.070031687865,469.14986552633,469.233612259032,469.317255936048,
469.400816680114,469.484314542071,469.567777042633,469.651222178125,469.734668012968,
469.818132608206,469.901685793628,469.985283627201,470.069015190063,470.148849028529,
470.232595761231,470.316239438247,470.399800182313,470.48329804427,470.566760544833,
470.650205680325,470.733651515168,470.817116110406,470.900669295827,470.9842671294,
471.067998692262,471.147832530728,471.23157926343,471.315222940446,471.398783684512,
471.482281546469,471.565744047032,471.649189182524,471.732635017367,471.816099612605,
471.899652798026,471.983250631599,472.066982194461,472.146816032927,472.230562765629,
472.314206442645,472.397767186711,472.481265048668,472.564727549231,472.648172684723,
472.731618519566,472.815083114804,472.898636300226,472.982234133799,473.06596569666,
473.145799535126,473.229546267828,473.313189944844,473.396750688911,473.480248550867,
473.56371105143,473.647156186923,473.730602021765,473.814066617004,473.897619802425,
473.981217635998,474.06494919886,474.144783037326,474.262636864626,474.372258510993,
474.380490691925),.UNSPECIFIED.);
#489=B_SPLINE_CURVE_WITH_KNOTS('',3,(#62684,#62685,#62686,#62687,#62688,
#62689,#62690,#62691,#62692,#62693,#62694,#62695,#62696,#62697,#62698,#62699,
#62700,#62701,#62702,#62703,#62704,#62705,#62706,#62707,#62708,#62709,#62710,
#62711,#62712,#62713,#62714,#62715,#62716,#62717,#62718,#62719,#62720,#62721,
#62722,#62723,#62724,#62725,#62726,#62727,#62728,#62729,#62730,#62731,#62732,
#62733,#62734,#62735,#62736,#62737,#62738,#62739,#62740,#62741,#62742,#62743,
#62744,#62745,#62746,#62747,#62748,#62749,#62750,#62751,#62752,#62753,#62754,
#62755,#62756,#62757,#62758,#62759,#62760,#62761,#62762,#62763,#62764,#62765,
#62766,#62767,#62768,#62769,#62770,#62771,#62772,#62773,#62774,#62775,#62776,
#62777,#62778,#62779,#62780,#62781,#62782,#62783,#62784,#62785,#62786,#62787,
#62788,#62789,#62790,#62791,#62792,#62793,#62794,#62795,#62796,#62797,#62798,
#62799,#62800,#62801,#62802,#62803,#62804,#62805,#62806,#62807,#62808,#62809,
#62810,#62811,#62812,#62813,#62814,#62815,#62816,#62817,#62818,#62819,#62820,
#62821,#62822,#62823,#62824,#62825,#62826,#62827,#62828,#62829,#62830,#62831,
#62832,#62833,#62834,#62835,#62836,#62837,#62838,#62839,#62840,#62841,#62842,
#62843,#62844,#62845,#62846,#62847,#62848,#62849,#62850,#62851,#62852,#62853,
#62854,#62855,#62856,#62857,#62858,#62859,#62860,#62861,#62862,#62863,#62864,
#62865,#62866,#62867,#62868,#62869,#62870,#62871,#62872,#62873,#62874,#62875,
#62876,#62877,#62878,#62879,#62880,#62881,#62882,#62883,#62884,#62885,#62886,
#62887,#62888,#62889,#62890,#62891,#62892,#62893,#62894,#62895,#62896,#62897,
#62898,#62899,#62900,#62901,#62902,#62903,#62904,#62905,#62906,#62907,#62908,
#62909,#62910,#62911,#62912),.UNSPECIFIED.,.F.,.F.,(4,3,3,3,3,3,3,3,3,3,
3,3,3,3,3,3,3,3,3,3,3,3,3,3,3,3,3,3,3,3,3,3,3,3,3,3,3,3,3,3,3,3,3,3,3,3,
3,3,3,3,3,3,3,3,3,3,3,3,3,3,3,3,3,3,3,3,3,3,3,3,3,3,3,3,3,3,4),(474.380490692059,
474.462988466164,474.548085725334,474.630497101718,474.71289802157,474.795307390673,
474.877744118907,474.96027069151,475.042851238611,475.12554651215,475.143766539525,
475.227513272227,475.311156949243,475.394717693309,475.478215555266,475.561678055828,
475.645123191321,475.728569026163,475.812033621402,475.895586806824,475.979184640396,
476.062916203258,476.142750041724,476.226496774426,476.310140451442,476.393701195508,
476.477199057465,476.560661558028,476.64410669352,476.727552528363,476.811017123601,
476.894570309023,476.978168142596,477.061899705458,477.141733543923,477.225480276625,
477.309123953641,477.392684697707,477.476182559663,477.559645060226,477.643090195718,
477.726536030561,477.810000625799,477.893553811221,477.977151644793,478.060883207655,
478.140717046122,478.224463778824,478.30810745584,478.391668199906,478.475166061863,
478.558628562425,478.642073697918,478.725519532761,478.808984127999,478.892537313421,
478.976135146994,479.059866709856,479.139700548321,479.223447281023,479.307090958039,
479.390651702105,479.474149564062,479.557612064625,479.641057200117,479.72450303496,
479.807967630198,479.89152081562,479.975118649192,480.058850212054,480.138684050521,
480.225798891272,480.31277593033,480.400500947557,480.487201398599,480.575438698919,
480.663675999239),.UNSPECIFIED.);
#490=B_SPLINE_CURVE_WITH_KNOTS('',3,(#62914,#62915,#62916,#62917,#62918,
#62919,#62920,#62921,#62922,#62923,#62924,#62925,#62926,#62927,#62928,#62929,
#62930,#62931,#62932,#62933,#62934,#62935,#62936,#62937,#62938,#62939,#62940,
#62941,#62942,#62943,#62944,#62945,#62946,#62947,#62948,#62949,#62950,#62951,
#62952,#62953,#62954,#62955,#62956,#62957,#62958,#62959,#62960,#62961,#62962,
#62963,#62964,#62965,#62966,#62967,#62968,#62969,#62970,#62971,#62972,#62973,
#62974,#62975,#62976,#62977,#62978,#62979,#62980,#62981,#62982,#62983,#62984,
#62985,#62986,#62987,#62988,#62989,#62990,#62991,#62992,#62993,#62994,#62995,
#62996,#62997,#62998,#62999,#63000,#63001,#63002,#63003,#63004,#63005,#63006,
#63007,#63008,#63009,#63010,#63011,#63012,#63013,#63014,#63015,#63016,#63017,
#63018,#63019,#63020,#63021,#63022,#63023,#63024,#63025,#63026,#63027,#63028,
#63029,#63030,#63031,#63032,#63033,#63034,#63035,#63036,#63037,#63038,#63039,
#63040,#63041,#63042,#63043,#63044,#63045,#63046,#63047,#63048,#63049,#63050,
#63051,#63052,#63053,#63054,#63055,#63056,#63057,#63058,#63059,#63060,#63061,
#63062,#63063,#63064,#63065,#63066,#63067,#63068,#63069,#63070,#63071,#63072,
#63073,#63074,#63075,#63076,#63077,#63078,#63079,#63080,#63081,#63082,#63083,
#63084,#63085,#63086,#63087,#63088,#63089,#63090,#63091,#63092,#63093,#63094,
#63095,#63096,#63097,#63098,#63099,#63100,#63101,#63102,#63103,#63104,#63105,
#63106,#63107,#63108,#63109,#63110,#63111,#63112,#63113,#63114,#63115,#63116,
#63117,#63118,#63119,#63120,#63121,#63122,#63123,#63124,#63125,#63126,#63127,
#63128,#63129,#63130,#63131,#63132,#63133,#63134,#63135,#63136,#63137,#63138,
#63139,#63140,#63141,#63142),.UNSPECIFIED.,.F.,.F.,(4,3,3,3,3,3,3,3,3,3,
3,3,3,3,3,3,3,3,3,3,3,3,3,3,3,3,3,3,3,3,3,3,3,3,3,3,3,3,3,3,3,3,3,3,3,3,
3,3,3,3,3,3,3,3,3,3,3,3,3,3,3,3,3,3,3,3,3,3,3,3,3,3,3,3,3,3,4),(480.663675999356,
480.752067585733,480.840612156768,480.929400150455,481.018321197254,481.10745040222,
481.13766755272,481.221414285422,481.305057962438,481.388618706504,481.472116568461,
481.555579069024,481.639024204516,481.722470039359,481.805934634597,481.889487820019,
481.973085653591,482.056817216453,482.136651054919,482.220397787621,482.304041464637,
482.387602208703,482.47110007066,482.554562571223,482.638007706715,482.721453541558,
482.804918136796,482.888471322218,482.972069155791,483.055800718653,483.135634557118,
483.21938128982,483.303024966836,483.386585710902,483.470083572859,483.553546073421,
483.636991208913,483.720437043756,483.803901638994,483.887454824416,483.971052657989,
484.05478422085,484.134618059317,484.218364792019,484.302008469035,484.385569213101,
484.469067075058,484.552529575621,484.635974711113,484.719420545956,484.802885141194,
484.886438326616,484.970036160189,485.053767723051,485.133601561516,485.217348294218,
485.300991971234,485.3845527153,485.468050577257,485.551513077819,485.634958213312,
485.718404048154,485.801868643393,485.885421828814,485.969019662387,486.052751225249,
486.132585063716,486.215094552444,486.297501225616,486.379814785946,486.462076176782,
486.544304464461,486.626518684454,486.708772128317,486.791043622075,486.873405145217,
486.946861306276),.UNSPECIFIED.);
#491=B_SPLINE_CURVE_WITH_KNOTS('',3,(#63144,#63145,#63146,#63147,#63148,
#63149,#63150,#63151,#63152,#63153,#63154,#63155,#63156,#63157,#63158,#63159,
#63160,#63161,#63162,#63163,#63164,#63165,#63166,#63167,#63168,#63169,#63170,
#63171,#63172,#63173,#63174,#63175,#63176,#63177,#63178,#63179,#63180,#63181,
#63182,#63183,#63184,#63185,#63186,#63187,#63188,#63189,#63190,#63191,#63192,
#63193,#63194,#63195,#63196,#63197,#63198,#63199,#63200,#63201,#63202,#63203,
#63204,#63205,#63206,#63207,#63208,#63209,#63210,#63211,#63212,#63213,#63214,
#63215,#63216,#63217,#63218,#63219,#63220,#63221,#63222,#63223,#63224,#63225,
#63226,#63227,#63228,#63229,#63230,#63231,#63232,#63233,#63234,#63235,#63236,
#63237,#63238,#63239,#63240,#63241,#63242,#63243,#63244,#63245,#63246,#63247,
#63248,#63249,#63250,#63251,#63252,#63253,#63254,#63255,#63256,#63257,#63258,
#63259,#63260,#63261,#63262,#63263,#63264,#63265,#63266,#63267,#63268,#63269,
#63270,#63271,#63272,#63273,#63274,#63275,#63276,#63277,#63278,#63279,#63280,
#63281,#63282,#63283,#63284,#63285,#63286,#63287,#63288,#63289,#63290,#63291,
#63292,#63293,#63294,#63295,#63296,#63297,#63298,#63299,#63300,#63301,#63302,
#63303,#63304,#63305,#63306,#63307,#63308,#63309,#63310,#63311,#63312,#63313,
#63314,#63315,#63316,#63317,#63318,#63319,#63320,#63321,#63322,#63323,#63324,
#63325,#63326,#63327,#63328,#63329,#63330,#63331,#63332,#63333,#63334,#63335,
#63336,#63337,#63338,#63339,#63340,#63341,#63342,#63343,#63344,#63345,#63346,
#63347,#63348,#63349,#63350,#63351,#63352,#63353,#63354,#63355,#63356,#63357,
#63358,#63359,#63360,#63361,#63362,#63363,#63364,#63365,#63366,#63367,#63368,
#63369),.UNSPECIFIED.,.F.,.F.,(4,3,3,3,3,3,3,3,3,3,3,3,3,3,3,3,3,3,3,3,
3,3,3,3,3,3,3,3,3,3,3,3,3,3,3,3,3,3,3,3,3,3,3,3,3,3,3,3,3,3,3,3,3,3,3,3,
3,3,3,3,3,3,3,3,3,3,3,3,3,3,3,3,3,3,3,4),(486.946861306418,487.07206518107,
487.131568565915,487.215315298617,487.298958975633,487.382519719699,487.466017581656,
487.549480082219,487.632925217711,487.716371052554,487.799835647792,487.883388833214,
487.966986666787,488.050718229649,488.130552068114,488.214298800816,488.297942477832,
488.381503221898,488.465001083855,488.548463584417,488.63190871991,488.715354554752,
488.79881914999,488.882372335412,488.965970168985,489.049701731847,489.129535570313,
489.213282303015,489.296925980031,489.380486724097,489.463984586054,489.547447086617,
489.630892222109,489.714338056952,489.79780265219,489.881355837612,489.964953671184,
490.048685234046,490.128519072512,490.212265805214,490.29590948223,490.379470226296,
490.462968088253,490.546430588816,490.629875724308,490.713321559151,490.796786154389,
490.880339339811,490.963937173383,491.047668736245,491.127502574711,491.211249307413,
491.294892984429,491.378453728495,491.461951590452,491.545414091015,491.628859226507,
491.71230506135,491.795769656588,491.87932284201,491.962920675583,492.046652238445,
492.126486076911,492.210232809613,492.293876486629,492.377437230695,492.460935092652,
492.544397593215,492.627842728707,492.71128856355,492.794753158788,492.87830634421,
492.961904177783,493.045635740645,493.12546957911,493.230046613598),
 .UNSPECIFIED.);
#492=B_SPLINE_CURVE_WITH_KNOTS('',3,(#63371,#63372,#63373,#63374,#63375,
#63376,#63377,#63378,#63379,#63380,#63381,#63382,#63383,#63384,#63385,#63386,
#63387,#63388,#63389,#63390,#63391,#63392,#63393,#63394,#63395,#63396,#63397,
#63398,#63399,#63400,#63401,#63402,#63403,#63404,#63405,#63406,#63407,#63408,
#63409,#63410,#63411,#63412,#63413,#63414,#63415,#63416,#63417,#63418,#63419,
#63420,#63421,#63422,#63423,#63424,#63425,#63426,#63427,#63428,#63429,#63430,
#63431,#63432,#63433,#63434,#63435,#63436,#63437,#63438,#63439,#63440,#63441,
#63442,#63443,#63444,#63445,#63446,#63447,#63448,#63449,#63450,#63451,#63452,
#63453,#63454,#63455,#63456,#63457,#63458,#63459,#63460,#63461,#63462,#63463,
#63464,#63465,#63466,#63467,#63468,#63469,#63470,#63471,#63472,#63473,#63474,
#63475,#63476,#63477,#63478,#63479,#63480,#63481,#63482,#63483,#63484,#63485,
#63486,#63487,#63488,#63489,#63490,#63491,#63492,#63493,#63494,#63495,#63496,
#63497,#63498,#63499,#63500,#63501,#63502,#63503,#63504,#63505,#63506,#63507,
#63508,#63509,#63510,#63511,#63512,#63513,#63514,#63515,#63516,#63517,#63518,
#63519,#63520,#63521,#63522,#63523,#63524,#63525,#63526,#63527,#63528,#63529,
#63530,#63531,#63532,#63533,#63534,#63535,#63536,#63537,#63538,#63539,#63540,
#63541,#63542,#63543,#63544,#63545,#63546,#63547,#63548,#63549,#63550,#63551,
#63552,#63553,#63554,#63555,#63556,#63557,#63558,#63559,#63560,#63561,#63562,
#63563,#63564,#63565,#63566,#63567,#63568,#63569,#63570,#63571,#63572,#63573,
#63574,#63575,#63576,#63577,#63578,#63579,#63580,#63581,#63582,#63583,#63584,
#63585,#63586,#63587,#63588,#63589,#63590,#63591,#63592,#63593,#63594,#63595,
#63596,#63597,#63598,#63599),.UNSPECIFIED.,.F.,.F.,(4,3,3,3,3,3,3,3,3,3,
3,3,3,3,3,3,3,3,3,3,3,3,3,3,3,3,3,3,3,3,3,3,3,3,3,3,3,3,3,3,3,3,3,3,3,3,
3,3,3,3,3,3,3,3,3,3,3,3,3,3,3,3,3,3,3,3,3,3,3,3,3,3,3,3,3,3,4),(493.230046613733,
493.312666057369,493.39519384848,493.477651040569,493.560063491413,493.642453340751,
493.7248395128,493.807240926367,493.889725936625,493.972254060176,494.054910316146,
494.124453081309,494.208199814011,494.291843491027,494.375404235093,494.45890209705,
494.542364597612,494.625809733104,494.709255567947,494.792720163185,494.876273348607,
494.95987118218,495.043602745042,495.123436583508,495.20718331621,495.290826993226,
495.374387737292,495.457885599249,495.541348099812,495.624793235304,495.708239070147,
495.791703665384,495.875256850806,495.958854684379,496.042586247241,496.122420085707,
496.206166818409,496.289810495425,496.373371239491,496.456869101448,496.540331602011,
496.623776737503,496.707222572346,496.790687167584,496.874240353006,496.957838186578,
497.04156974944,497.121403587906,497.205150320608,497.288793997624,497.37235474169,
497.455852603647,497.53931510421,497.622760239702,497.706206074545,497.789670669783,
497.873223855205,497.956821688778,498.04055325164,498.120387090106,498.204133822808,
498.287777499824,498.371338243891,498.454836105847,498.53829860641,498.621743741902,
498.705189576745,498.788654171983,498.872207357405,498.955805190978,499.03953675384,
499.119370592305,499.217835924377,499.311002515681,499.403889327138,499.496350686817,
499.513231920595),.UNSPECIFIED.);
#493=B_SPLINE_CURVE_WITH_KNOTS('',3,(#63601,#63602,#63603,#63604,#63605,
#63606,#63607,#63608,#63609,#63610,#63611,#63612,#63613,#63614,#63615,#63616,
#63617,#63618,#63619,#63620,#63621,#63622,#63623,#63624,#63625,#63626,#63627,
#63628,#63629,#63630,#63631,#63632,#63633,#63634,#63635,#63636,#63637,#63638,
#63639,#63640,#63641,#63642,#63643,#63644,#63645,#63646,#63647,#63648,#63649,
#63650,#63651,#63652,#63653,#63654,#63655,#63656,#63657,#63658,#63659,#63660,
#63661,#63662,#63663,#63664,#63665,#63666,#63667,#63668,#63669,#63670,#63671,
#63672,#63673,#63674,#63675,#63676,#63677,#63678,#63679,#63680,#63681,#63682,
#63683,#63684,#63685,#63686,#63687,#63688,#63689,#63690,#63691,#63692,#63693,
#63694,#63695,#63696,#63697,#63698,#63699,#63700,#63701,#63702,#63703,#63704,
#63705,#63706,#63707,#63708,#63709,#63710,#63711,#63712,#63713,#63714,#63715,
#63716,#63717,#63718,#63719,#63720,#63721,#63722,#63723,#63724,#63725,#63726,
#63727,#63728,#63729,#63730,#63731,#63732,#63733,#63734,#63735,#63736,#63737,
#63738,#63739,#63740,#63741,#63742,#63743,#63744,#63745,#63746,#63747,#63748,
#63749,#63750,#63751,#63752,#63753,#63754,#63755,#63756,#63757,#63758,#63759,
#63760,#63761,#63762,#63763,#63764,#63765,#63766,#63767,#63768,#63769,#63770,
#63771,#63772,#63773,#63774,#63775,#63776,#63777,#63778,#63779,#63780,#63781,
#63782,#63783,#63784,#63785,#63786,#63787,#63788,#63789,#63790,#63791,#63792,
#63793,#63794,#63795,#63796,#63797,#63798,#63799,#63800,#63801,#63802,#63803,
#63804,#63805,#63806,#63807,#63808,#63809,#63810,#63811,#63812,#63813,#63814,
#63815,#63816,#63817,#63818,#63819,#63820,#63821,#63822,#63823,#63824,#63825,
#63826,#63827,#63828,#63829,#63830,#63831,#63832),.UNSPECIFIED.,.F.,.F.,
(4,3,3,3,3,3,3,3,3,3,3,3,3,3,3,3,3,3,3,3,3,3,3,3,3,3,3,3,3,3,3,3,3,3,3,
3,3,3,3,3,3,3,3,3,3,3,3,3,3,3,3,3,3,3,3,3,3,3,3,3,3,3,3,3,3,3,3,3,3,3,3,
3,3,3,3,3,3,4),(499.513231920777,499.597681186419,499.682149034449,499.766652032328,
499.854577547872,499.939253202636,500.024000450852,500.10887777593,500.118354094504,
500.202100827206,500.285744504222,500.369305248288,500.452803110245,500.536265610808,
500.6197107463,500.703156581143,500.786621176381,500.870174361803,500.953772195375,
501.037503758237,501.117337596703,501.201084329405,501.284728006421,501.368288750487,
501.451786612444,501.535249113007,501.618694248499,501.702140083341,501.78560467858,
501.869157864001,501.952755697574,502.036487260436,502.116321098902,502.200067831604,
502.28371150862,502.367272252687,502.450770114643,502.534232615206,502.617677750698,
502.701123585541,502.784588180779,502.8681413662,502.951739199773,503.035470762635,
503.115304601101,503.199051333803,503.282695010819,503.366255754885,503.449753616842,
503.533216117404,503.616661252897,503.70010708774,503.783571682978,503.8671248684,
503.950722701972,504.034454264834,504.114288103301,504.198034836003,504.281678513019,
504.365239257085,504.448737119042,504.532199619605,504.615644755097,504.69909058994,
504.782555185178,504.8661083706,504.949706204172,505.033437767034,505.1132716055,
505.198664808307,505.282006113707,505.365267837759,505.448468382632,505.535455593963,
505.618597993435,505.701733921829,505.784896160721,505.796417227957),
 .UNSPECIFIED.);
#494=B_SPLINE_CURVE_WITH_KNOTS('',3,(#63834,#63835,#63836,#63837,#63838,
#63839,#63840,#63841,#63842,#63843,#63844,#63845,#63846,#63847,#63848,#63849,
#63850,#63851,#63852,#63853,#63854,#63855,#63856,#63857,#63858,#63859,#63860,
#63861,#63862,#63863,#63864,#63865,#63866,#63867,#63868,#63869,#63870,#63871,
#63872,#63873,#63874,#63875,#63876,#63877,#63878,#63879,#63880,#63881,#63882,
#63883,#63884,#63885,#63886,#63887,#63888,#63889,#63890,#63891,#63892,#63893,
#63894,#63895,#63896,#63897,#63898,#63899,#63900,#63901,#63902,#63903,#63904,
#63905,#63906,#63907,#63908,#63909,#63910,#63911,#63912,#63913,#63914,#63915,
#63916,#63917,#63918,#63919,#63920,#63921,#63922,#63923,#63924,#63925,#63926,
#63927,#63928,#63929,#63930,#63931,#63932,#63933,#63934,#63935,#63936,#63937,
#63938,#63939,#63940,#63941,#63942,#63943,#63944,#63945,#63946,#63947,#63948,
#63949,#63950,#63951,#63952,#63953,#63954,#63955,#63956,#63957,#63958,#63959,
#63960,#63961,#63962,#63963,#63964,#63965,#63966,#63967,#63968,#63969,#63970,
#63971,#63972,#63973,#63974,#63975,#63976,#63977,#63978,#63979,#63980,#63981,
#63982,#63983,#63984,#63985,#63986,#63987,#63988,#63989,#63990,#63991,#63992,
#63993,#63994,#63995,#63996,#63997,#63998,#63999,#64000,#64001,#64002,#64003,
#64004,#64005,#64006,#64007,#64008,#64009,#64010,#64011,#64012,#64013,#64014,
#64015,#64016,#64017,#64018,#64019,#64020,#64021,#64022,#64023,#64024,#64025,
#64026,#64027,#64028,#64029,#64030,#64031,#64032,#64033,#64034,#64035,#64036,
#64037,#64038,#64039,#64040,#64041,#64042,#64043,#64044,#64045,#64046,#64047,
#64048,#64049,#64050,#64051,#64052,#64053,#64054,#64055,#64056,#64057,#64058,
#64059,#64060,#64061,#64062),.UNSPECIFIED.,.F.,.F.,(4,3,3,3,3,3,3,3,3,3,
3,3,3,3,3,3,3,3,3,3,3,3,3,3,3,3,3,3,3,3,3,3,3,3,3,3,3,3,3,3,3,3,3,3,3,3,
3,3,3,3,3,3,3,3,3,3,3,3,3,3,3,3,3,3,3,3,3,3,3,3,3,3,3,3,3,3,4),(505.796417228126,
505.895263971297,505.994821585573,506.095146411306,506.112255107699,506.196001840401,
506.279645517416,506.363206261483,506.446704123439,506.530166624002,506.613611759494,
506.697057594336,506.780522189574,506.864075374996,506.947673208569,507.03140477143,
507.111238609898,507.1949853426,507.278629019616,507.362189763682,507.445687625639,
507.529150126201,507.612595261694,507.696041096536,507.779505691775,507.863058877196,
507.946656710769,508.030388273631,508.110222112097,508.193968844799,508.277612521815,
508.361173265881,508.444671127838,508.528133628401,508.611578763893,508.695024598736,
508.778489193974,508.862042379396,508.945640212969,509.029371775831,509.109205614296,
509.192952346998,509.276596024014,509.36015676808,509.443654630037,509.527117130599,
509.610562266092,509.694008100934,509.777472696172,509.861025881594,509.944623715167,
510.028355278029,510.108189116495,510.191935849197,510.275579526213,510.359140270279,
510.442638132236,510.526100632799,510.609545768291,510.692991603134,510.776456198372,
510.860009383794,510.943607217366,511.027338780228,511.107172618695,511.190549520313,
511.273823599296,511.357015357863,511.440145222664,511.523241197348,511.606321370413,
511.689404142631,511.772507912952,511.8556995516,511.938938518477,512.022303089775,
512.079602535017),.UNSPECIFIED.);
#495=B_SPLINE_CURVE_WITH_KNOTS('',3,(#64064,#64065,#64066,#64067,#64068,
#64069,#64070,#64071,#64072,#64073,#64074,#64075,#64076,#64077,#64078,#64079,
#64080,#64081,#64082,#64083,#64084,#64085,#64086,#64087,#64088,#64089,#64090,
#64091,#64092,#64093,#64094,#64095,#64096,#64097,#64098,#64099,#64100,#64101,
#64102,#64103,#64104,#64105,#64106,#64107,#64108,#64109,#64110,#64111,#64112,
#64113,#64114,#64115,#64116,#64117,#64118,#64119,#64120,#64121,#64122,#64123,
#64124,#64125,#64126,#64127,#64128,#64129,#64130,#64131,#64132,#64133,#64134,
#64135,#64136,#64137,#64138,#64139,#64140,#64141,#64142,#64143,#64144,#64145,
#64146,#64147,#64148,#64149,#64150,#64151,#64152,#64153,#64154,#64155,#64156,
#64157,#64158,#64159,#64160,#64161,#64162,#64163,#64164,#64165,#64166,#64167,
#64168,#64169,#64170,#64171,#64172,#64173,#64174,#64175,#64176,#64177,#64178,
#64179,#64180,#64181,#64182,#64183,#64184,#64185,#64186,#64187,#64188,#64189,
#64190,#64191,#64192,#64193,#64194,#64195,#64196,#64197,#64198,#64199,#64200,
#64201,#64202,#64203,#64204,#64205,#64206,#64207,#64208,#64209,#64210,#64211,
#64212,#64213,#64214,#64215,#64216,#64217,#64218,#64219,#64220,#64221,#64222,
#64223,#64224,#64225,#64226,#64227,#64228,#64229,#64230,#64231,#64232,#64233,
#64234,#64235,#64236,#64237,#64238,#64239,#64240,#64241,#64242,#64243,#64244,
#64245,#64246,#64247,#64248,#64249,#64250,#64251,#64252,#64253,#64254,#64255,
#64256,#64257,#64258,#64259,#64260,#64261,#64262,#64263,#64264,#64265,#64266,
#64267,#64268,#64269,#64270,#64271,#64272,#64273,#64274,#64275,#64276,#64277,
#64278,#64279,#64280,#64281,#64282,#64283,#64284,#64285,#64286,#64287,#64288,
#64289,#64290,#64291,#64292),.UNSPECIFIED.,.F.,.F.,(4,3,3,3,3,3,3,3,3,3,
3,3,3,3,3,3,3,3,3,3,3,3,3,3,3,3,3,3,3,3,3,3,3,3,3,3,3,3,3,3,3,3,3,3,3,3,
3,3,3,3,3,3,3,3,3,3,3,3,3,3,3,3,3,3,3,3,3,3,3,3,3,3,3,3,3,3,4),(512.079602535136,
512.106156120894,512.189902853596,512.273546530612,512.357107274678,512.440605136635,
512.524067637198,512.60751277269,512.690958607533,512.774423202771,512.857976388193,
512.941574221766,513.025305784627,513.105139623093,513.188886355795,513.272530032811,
513.356090776877,513.439588638834,513.523051139396,513.606496274889,513.689942109731,
513.773406704969,513.856959890391,513.940557723964,514.024289286826,514.104123125292,
514.187869857994,514.27151353501,514.355074279076,514.438572141033,514.522034641596,
514.605479777088,514.688925611931,514.772390207169,514.855943392591,514.939541226164,
515.023272789026,515.103106627491,515.186853360193,515.270497037209,515.354057781275,
515.437555643232,515.521018143795,515.604463279287,515.68790911413,515.771373709368,
515.85492689479,515.938524728363,516.022256291224,516.102090129691,516.185836862393,
516.269480539409,516.353041283475,516.436539145432,516.520001645995,516.603446781487,
516.68689261633,516.770357211568,516.85391039699,516.937508230563,517.021239793425,
517.10107363189,517.184820364592,517.268464041608,517.352024785674,517.435522647631,
517.518985148193,517.602430283686,517.685876118528,517.769340713767,517.852893899189,
517.936491732761,518.020223295623,518.100057134089,518.207488261823,518.312945017838,
518.362787842169),.UNSPECIFIED.);
#496=B_SPLINE_CURVE_WITH_KNOTS('',3,(#64294,#64295,#64296,#64297,#64298,
#64299,#64300,#64301,#64302,#64303,#64304,#64305,#64306,#64307,#64308,#64309,
#64310,#64311,#64312,#64313,#64314,#64315,#64316,#64317,#64318,#64319,#64320,
#64321,#64322,#64323,#64324,#64325,#64326,#64327,#64328,#64329,#64330,#64331,
#64332,#64333,#64334,#64335,#64336,#64337,#64338,#64339,#64340,#64341,#64342,
#64343,#64344,#64345,#64346,#64347,#64348,#64349,#64350,#64351,#64352,#64353,
#64354,#64355,#64356,#64357,#64358,#64359,#64360,#64361,#64362,#64363,#64364,
#64365,#64366,#64367,#64368,#64369,#64370,#64371,#64372,#64373,#64374,#64375,
#64376,#64377,#64378,#64379,#64380,#64381,#64382,#64383,#64384,#64385,#64386,
#64387,#64388,#64389,#64390,#64391,#64392,#64393,#64394,#64395,#64396,#64397,
#64398,#64399,#64400,#64401,#64402,#64403,#64404,#64405,#64406,#64407,#64408,
#64409,#64410,#64411,#64412,#64413,#64414,#64415,#64416,#64417,#64418,#64419,
#64420,#64421,#64422,#64423,#64424,#64425,#64426,#64427,#64428,#64429,#64430,
#64431,#64432,#64433,#64434,#64435,#64436,#64437,#64438,#64439,#64440,#64441,
#64442,#64443,#64444,#64445,#64446,#64447,#64448,#64449,#64450,#64451,#64452,
#64453,#64454,#64455,#64456,#64457,#64458,#64459,#64460,#64461,#64462,#64463,
#64464,#64465,#64466,#64467,#64468,#64469,#64470,#64471,#64472,#64473,#64474,
#64475,#64476,#64477,#64478,#64479,#64480,#64481,#64482,#64483,#64484,#64485,
#64486,#64487,#64488,#64489,#64490,#64491,#64492,#64493,#64494,#64495,#64496,
#64497,#64498,#64499,#64500,#64501,#64502,#64503,#64504,#64505,#64506,#64507,
#64508,#64509,#64510,#64511,#64512,#64513,#64514,#64515,#64516,#64517,#64518,
#64519,#64520,#64521,#64522),.UNSPECIFIED.,.F.,.F.,(4,3,3,3,3,3,3,3,3,3,
3,3,3,3,3,3,3,3,3,3,3,3,3,3,3,3,3,3,3,3,3,3,3,3,3,3,3,3,3,3,3,3,3,3,3,3,
3,3,3,3,3,3,3,3,3,3,3,3,3,3,3,3,3,3,3,3,3,3,3,3,3,3,3,3,3,3,4),(518.362787842316,
518.44544362937,518.528056518539,518.61064778964,518.693236220728,518.775840584852,
518.85853037429,518.941263594348,519.024128204109,519.099040636288,519.18278736899,
519.266431046006,519.349991790072,519.433489652029,519.516952152591,519.600397288083,
519.683843122926,519.767307718164,519.850860903586,519.934458737158,520.01819030002,
520.098024138487,520.181770871189,520.265414548205,520.348975292271,520.432473154228,
520.515935654791,520.599380790283,520.682826625126,520.766291220364,520.849844405786,
520.933442239359,521.01717380222,521.097007640686,521.180754373388,521.264398050404,
521.34795879447,521.431456656427,521.51491915699,521.598364292482,521.681810127325,
521.765274722563,521.848827907985,521.932425741557,522.016157304419,522.095991142886,
522.179737875588,522.263381552604,522.346942296671,522.430440158627,522.51390265919,
522.597347794682,522.680793629525,522.764258224764,522.847811410185,522.931409243758,
523.01514080662,523.094974645085,523.178721377787,523.262365054803,523.345925798869,
523.429423660825,523.512886161388,523.596331296881,523.679777131724,523.763241726962,
523.846794912384,523.930392745956,524.014124308818,524.093958147284,524.180198977607,
524.266313373394,524.352315450507,524.438191058093,524.523991974352,524.609717033682,
524.645973149496),.UNSPECIFIED.);
#497=B_SPLINE_CURVE_WITH_KNOTS('',3,(#64524,#64525,#64526,#64527,#64528,
#64529,#64530,#64531,#64532,#64533,#64534,#64535,#64536,#64537,#64538,#64539,
#64540,#64541,#64542,#64543,#64544,#64545,#64546,#64547,#64548,#64549,#64550,
#64551,#64552,#64553,#64554,#64555,#64556,#64557,#64558,#64559,#64560,#64561,
#64562,#64563,#64564,#64565,#64566,#64567,#64568,#64569,#64570,#64571,#64572,
#64573,#64574,#64575,#64576,#64577,#64578,#64579,#64580,#64581,#64582,#64583,
#64584,#64585,#64586,#64587,#64588,#64589,#64590,#64591,#64592,#64593,#64594,
#64595,#64596,#64597,#64598,#64599,#64600,#64601,#64602,#64603,#64604,#64605,
#64606,#64607,#64608,#64609,#64610,#64611,#64612,#64613,#64614,#64615,#64616,
#64617,#64618,#64619,#64620,#64621,#64622,#64623,#64624,#64625,#64626,#64627,
#64628,#64629,#64630,#64631,#64632,#64633,#64634,#64635,#64636,#64637,#64638,
#64639,#64640,#64641,#64642,#64643,#64644,#64645,#64646,#64647,#64648,#64649,
#64650,#64651,#64652,#64653,#64654,#64655,#64656,#64657,#64658,#64659,#64660,
#64661,#64662,#64663,#64664,#64665,#64666,#64667,#64668,#64669,#64670,#64671,
#64672,#64673,#64674,#64675,#64676,#64677,#64678,#64679,#64680,#64681,#64682,
#64683,#64684,#64685,#64686,#64687,#64688,#64689,#64690,#64691,#64692,#64693,
#64694,#64695,#64696,#64697,#64698,#64699,#64700,#64701,#64702,#64703,#64704,
#64705,#64706,#64707,#64708,#64709,#64710,#64711,#64712,#64713,#64714,#64715,
#64716,#64717,#64718,#64719,#64720,#64721,#64722,#64723,#64724,#64725,#64726,
#64727,#64728,#64729,#64730,#64731,#64732,#64733,#64734,#64735,#64736,#64737,
#64738,#64739,#64740,#64741,#64742,#64743,#64744,#64745,#64746,#64747,#64748,
#64749,#64750,#64751,#64752),.UNSPECIFIED.,.F.,.F.,(4,3,3,3,3,3,3,3,3,3,
3,3,3,3,3,3,3,3,3,3,3,3,3,3,3,3,3,3,3,3,3,3,3,3,3,3,3,3,3,3,3,3,3,3,3,3,
3,3,3,3,3,3,3,3,3,3,3,3,3,3,3,3,3,3,3,3,3,3,3,3,3,3,3,3,3,3,4),(524.645973149609,
524.735551576018,524.825461875191,524.915537276957,525.005896438371,525.092941649483,
525.176688382185,525.260332059201,525.343892803268,525.427390665224,525.510853165787,
525.594298301279,525.677744136122,525.76120873136,525.844761916782,525.928359750355,
526.012091313217,526.091925151682,526.175671884384,526.2593155614,526.342876305466,
526.426374167423,526.509836667985,526.593281803477,526.67672763832,526.760192233558,
526.84374541898,526.927343252553,527.011074815414,527.090908653881,527.174655386583,
527.258299063599,527.341859807665,527.425357669622,527.508820170185,527.592265305677,
527.67571114052,527.759175735758,527.84272892118,527.926326754752,528.010058317614,
528.08989215608,528.173638888782,528.257282565798,528.340843309865,528.424341171821,
528.507803672384,528.591248807876,528.674694642719,528.758159237957,528.841712423379,
528.925310256952,529.009041819814,529.08887565828,529.172622390982,529.256266067998,
529.339826812064,529.423324674021,529.506787174584,529.590232310076,529.673678144919,
529.757142740157,529.840695925579,529.924293759152,530.008025322014,530.087859160479,
530.170361360948,530.252761152824,530.337310815793,530.41956603867,530.50178925204,
530.583999493628,530.670289234364,530.752565445803,530.834878351078,530.917278863106,
530.929158456571),.UNSPECIFIED.);
#498=B_SPLINE_CURVE_WITH_KNOTS('',3,(#64754,#64755,#64756,#64757,#64758,
#64759,#64760,#64761,#64762,#64763,#64764,#64765,#64766,#64767,#64768,#64769,
#64770,#64771,#64772,#64773,#64774,#64775,#64776,#64777,#64778,#64779,#64780,
#64781,#64782,#64783,#64784,#64785,#64786,#64787,#64788,#64789,#64790,#64791,
#64792,#64793,#64794,#64795,#64796,#64797,#64798,#64799,#64800,#64801,#64802,
#64803,#64804,#64805,#64806,#64807,#64808,#64809,#64810,#64811,#64812,#64813,
#64814,#64815,#64816,#64817,#64818,#64819,#64820,#64821,#64822,#64823,#64824,
#64825,#64826,#64827,#64828,#64829,#64830,#64831,#64832,#64833,#64834,#64835,
#64836,#64837,#64838,#64839,#64840,#64841,#64842,#64843,#64844,#64845,#64846,
#64847,#64848,#64849,#64850,#64851,#64852,#64853,#64854,#64855,#64856,#64857,
#64858,#64859,#64860,#64861,#64862,#64863,#64864,#64865,#64866,#64867,#64868,
#64869,#64870,#64871,#64872,#64873,#64874,#64875,#64876,#64877,#64878,#64879,
#64880,#64881,#64882,#64883,#64884,#64885,#64886,#64887,#64888,#64889,#64890,
#64891,#64892,#64893,#64894,#64895,#64896,#64897,#64898,#64899,#64900,#64901,
#64902,#64903,#64904,#64905,#64906,#64907,#64908,#64909,#64910,#64911,#64912,
#64913,#64914,#64915,#64916,#64917,#64918,#64919,#64920,#64921,#64922,#64923,
#64924,#64925,#64926,#64927,#64928,#64929,#64930,#64931,#64932,#64933,#64934,
#64935,#64936,#64937,#64938,#64939,#64940,#64941,#64942,#64943,#64944,#64945,
#64946,#64947,#64948,#64949,#64950,#64951,#64952,#64953,#64954,#64955,#64956,
#64957,#64958,#64959,#64960,#64961,#64962,#64963,#64964,#64965,#64966,#64967,
#64968,#64969,#64970,#64971,#64972,#64973,#64974,#64975,#64976,#64977,#64978,
#64979),.UNSPECIFIED.,.F.,.F.,(4,3,3,3,3,3,3,3,3,3,3,3,3,3,3,3,3,3,3,3,
3,3,3,3,3,3,3,3,3,3,3,3,3,3,3,3,3,3,3,3,3,3,3,3,3,3,3,3,3,3,3,3,3,3,3,3,
3,3,3,3,3,3,3,3,3,3,3,3,3,3,3,3,3,3,3,4),(530.929158456675,531.066685078122,
531.086842662678,531.17058939538,531.254233072396,531.337793816463,531.42129167842,
531.504754178982,531.588199314475,531.671645149318,531.755109744556,531.838662929978,
531.92226076355,532.005992326412,532.085826164877,532.169572897579,532.253216574595,
532.336777318661,532.420275180618,532.50373768118,532.587182816672,532.670628651515,
532.754093246753,532.837646432175,532.921244265748,533.004975828609,533.084809667076,
533.168556399778,533.252200076794,533.335760820861,533.419258682817,533.50272118338,
533.586166318872,533.669612153715,533.753076748953,533.836629934375,533.920227767948,
534.00395933081,534.083793169275,534.167539901977,534.251183578993,534.334744323059,
534.418242185016,534.501704685579,534.585149821071,534.668595655914,534.752060251152,
534.835613436574,534.919211270147,535.002942833009,535.082776671475,535.166523404177,
535.250167081193,535.333727825259,535.417225687216,535.500688187779,535.584133323271,
535.667579158114,535.751043753352,535.834596938774,535.918194772347,536.001926335209,
536.081760173674,536.165506906376,536.249150583392,536.332711327458,536.416209189415,
536.499671689977,536.58311682547,536.666562660312,536.75002725555,536.833580440972,
536.917178274545,537.000909837407,537.080743675873,537.212343763855),
 .UNSPECIFIED.);
#499=B_SPLINE_CURVE_WITH_KNOTS('',3,(#64981,#64982,#64983,#64984,#64985,
#64986,#64987,#64988,#64989,#64990,#64991,#64992,#64993,#64994,#64995,#64996,
#64997,#64998,#64999,#65000,#65001,#65002,#65003,#65004,#65005,#65006,#65007,
#65008,#65009,#65010,#65011,#65012,#65013,#65014,#65015,#65016,#65017,#65018,
#65019,#65020,#65021,#65022,#65023,#65024,#65025,#65026,#65027,#65028,#65029,
#65030,#65031,#65032,#65033,#65034,#65035,#65036,#65037,#65038,#65039,#65040,
#65041,#65042,#65043,#65044,#65045,#65046,#65047,#65048,#65049,#65050,#65051,
#65052,#65053,#65054,#65055,#65056,#65057,#65058,#65059,#65060,#65061,#65062,
#65063,#65064,#65065,#65066,#65067,#65068,#65069,#65070,#65071,#65072,#65073,
#65074,#65075,#65076,#65077,#65078,#65079,#65080,#65081,#65082,#65083,#65084,
#65085,#65086,#65087,#65088,#65089,#65090,#65091,#65092,#65093,#65094,#65095,
#65096,#65097,#65098,#65099,#65100,#65101,#65102,#65103,#65104,#65105,#65106,
#65107,#65108,#65109,#65110,#65111,#65112,#65113,#65114,#65115,#65116,#65117,
#65118,#65119,#65120,#65121,#65122,#65123,#65124,#65125,#65126,#65127,#65128,
#65129,#65130,#65131,#65132,#65133,#65134,#65135,#65136,#65137,#65138,#65139,
#65140,#65141,#65142,#65143,#65144,#65145,#65146,#65147,#65148,#65149,#65150,
#65151,#65152,#65153,#65154,#65155,#65156,#65157,#65158,#65159,#65160,#65161,
#65162,#65163,#65164,#65165,#65166,#65167,#65168,#65169,#65170,#65171,#65172,
#65173,#65174,#65175,#65176,#65177,#65178,#65179,#65180,#65181,#65182,#65183,
#65184,#65185,#65186,#65187,#65188,#65189,#65190,#65191,#65192,#65193,#65194,
#65195,#65196,#65197,#65198,#65199,#65200,#65201,#65202,#65203,#65204,#65205,
#65206,#65207,#65208,#65209),.UNSPECIFIED.,.F.,.F.,(4,3,3,3,3,3,3,3,3,3,
3,3,3,3,3,3,3,3,3,3,3,3,3,3,3,3,3,3,3,3,3,3,3,3,3,3,3,3,3,3,3,3,3,3,3,3,
3,3,3,3,3,3,3,3,3,3,3,3,3,3,3,3,3,3,3,3,3,3,3,3,3,3,3,3,3,3,4),(537.212343763982,
537.2948206532,537.377211365898,537.459537018521,537.541825304515,537.624096120113,
537.706368459933,537.788661317575,537.871040033356,537.953466747926,538.036014048594,
538.079727178072,538.163473910774,538.24711758779,538.330678331856,538.414176193813,
538.497638694375,538.581083829868,538.66452966471,538.747994259949,538.83154744537,
538.915145278943,538.998876841805,539.078710680271,539.162457412973,539.246101089989,
539.329661834056,539.413159696012,539.496622196575,539.580067332067,539.66351316691,
539.746977762148,539.83053094757,539.914128781143,539.997860344005,540.07769418247,
540.161440915172,540.245084592188,540.328645336255,540.412143198212,540.495605698774,
540.579050834266,540.662496669109,540.745961264347,540.829514449769,540.913112283342,
540.996843846204,541.07667768467,541.160424417372,541.244068094388,541.327628838455,
541.411126700412,541.494589200974,541.578034336467,541.66148017131,541.744944766548,
541.82849795197,541.912095785542,541.995827348404,542.075661186869,542.159407919571,
542.243051596586,542.326612340653,542.41011020261,542.493572703173,542.577017838665,
542.660463673508,542.743928268745,542.827481454167,542.91107928774,542.994810850602,
543.074644689068,543.166514762158,543.258040747508,543.349348384809,543.440308855984,
543.495529070882),.UNSPECIFIED.);
#500=B_SPLINE_CURVE_WITH_KNOTS('',3,(#65211,#65212,#65213,#65214,#65215,
#65216,#65217,#65218,#65219,#65220,#65221,#65222,#65223,#65224,#65225,#65226,
#65227,#65228,#65229,#65230,#65231,#65232,#65233,#65234,#65235,#65236,#65237,
#65238,#65239,#65240,#65241,#65242,#65243,#65244,#65245,#65246,#65247,#65248,
#65249,#65250,#65251,#65252,#65253,#65254,#65255,#65256,#65257,#65258,#65259,
#65260,#65261,#65262,#65263,#65264,#65265,#65266,#65267,#65268,#65269,#65270,
#65271,#65272,#65273,#65274,#65275,#65276,#65277,#65278,#65279,#65280,#65281,
#65282,#65283,#65284,#65285,#65286,#65287,#65288,#65289,#65290,#65291,#65292,
#65293,#65294,#65295,#65296,#65297,#65298,#65299,#65300,#65301,#65302,#65303,
#65304,#65305,#65306,#65307,#65308,#65309,#65310,#65311,#65312,#65313,#65314,
#65315,#65316,#65317,#65318,#65319,#65320,#65321,#65322,#65323,#65324,#65325,
#65326,#65327,#65328,#65329,#65330,#65331,#65332,#65333,#65334,#65335,#65336,
#65337,#65338,#65339,#65340,#65341,#65342,#65343,#65344,#65345,#65346,#65347,
#65348,#65349,#65350,#65351,#65352,#65353,#65354,#65355,#65356,#65357,#65358,
#65359,#65360,#65361,#65362,#65363,#65364,#65365,#65366,#65367,#65368,#65369,
#65370,#65371,#65372,#65373,#65374,#65375,#65376,#65377,#65378,#65379,#65380,
#65381,#65382,#65383,#65384,#65385,#65386,#65387,#65388,#65389,#65390,#65391,
#65392,#65393,#65394,#65395,#65396,#65397,#65398,#65399,#65400,#65401,#65402,
#65403,#65404,#65405,#65406,#65407,#65408,#65409,#65410,#65411,#65412,#65413,
#65414,#65415,#65416,#65417,#65418,#65419,#65420,#65421,#65422,#65423,#65424,
#65425,#65426,#65427,#65428,#65429,#65430,#65431,#65432,#65433,#65434,#65435,
#65436,#65437,#65438,#65439),.UNSPECIFIED.,.F.,.F.,(4,3,3,3,3,3,3,3,3,3,
3,3,3,3,3,3,3,3,3,3,3,3,3,3,3,3,3,3,3,3,3,3,3,3,3,3,3,3,3,3,3,3,3,3,3,3,
3,3,3,3,3,3,3,3,3,3,3,3,3,3,3,3,3,3,3,3,3,3,3,3,3,3,3,3,3,3,4),(543.495529071034,
543.580585919541,543.665679585698,543.750825481719,543.836101155191,543.921445673897,
544.00694746502,544.073628191267,544.157374923969,544.241018600984,544.324579345051,
544.408077207008,544.49153970757,544.574984843062,544.658430677905,544.741895273143,
544.825448458564,544.909046292137,544.992777854998,545.072611693466,545.156358426168,
545.240002103184,545.32356284725,545.407060709207,545.490523209769,545.573968345261,
545.657414180104,545.740878775342,545.824431960764,545.908029794336,545.991761357198,
546.071595195665,546.155341928368,546.238985605384,546.322546349451,546.406044211407,
546.48950671197,546.572951847463,546.656397682306,546.739862277544,546.823415462967,
546.90701329654,546.990744859402,547.070578697865,547.154325430567,547.237969107583,
547.321529851649,547.405027713606,547.488490214169,547.571935349661,547.655381184504,
547.738845779743,547.822398965164,547.905996798737,547.989728361599,548.069562200064,
548.153308932766,548.236952609781,548.320513353848,548.404011215804,548.487473716366,
548.570918851859,548.654364686701,548.737829281939,548.821382467361,548.904980300933,
548.988711863795,549.068545702263,549.151692740348,549.234706332708,549.317642823717,
549.400520897003,549.483359188964,549.566191689685,549.649019764715,549.731889025188,
549.778714378214),.UNSPECIFIED.);
#501=B_SPLINE_CURVE_WITH_KNOTS('',3,(#65441,#65442,#65443,#65444,#65445,
#65446,#65447,#65448,#65449,#65450,#65451),.UNSPECIFIED.,.F.,.F.,(4,1,1,
1,1,1,2,4),(549.77871935695,550.067529204462,551.066512706661,552.065496208861,
553.06447971106,554.063463213259,555.062446715458,556.061899685393),
 .UNSPECIFIED.);
#502=B_SPLINE_CURVE_WITH_KNOTS('',3,(#65453,#65454,#65455,#65456,#65457,
#65458,#65459,#65460,#65461,#65462),.UNSPECIFIED.,.F.,.F.,(4,1,1,1,1,1,
1,4),(556.061899685393,557.060413719856,558.059397222055,559.058380724255,
560.057364226454,561.056347728653,562.055331230852,562.345079947443),
 .UNSPECIFIED.);
#503=B_SPLINE_CURVE_WITH_KNOTS('',3,(#65464,#65465,#65466,#65467,#65468,
#65469,#65470,#65471,#65472,#65473,#65474,#65475,#65476,#65477,#65478,#65479,
#65480,#65481,#65482,#65483,#65484,#65485,#65486,#65487,#65488,#65489,#65490,
#65491,#65492,#65493,#65494,#65495,#65496,#65497,#65498,#65499,#65500,#65501,
#65502,#65503,#65504,#65505,#65506,#65507,#65508,#65509,#65510,#65511,#65512,
#65513,#65514,#65515,#65516,#65517,#65518,#65519,#65520,#65521,#65522,#65523,
#65524,#65525,#65526,#65527,#65528,#65529,#65530,#65531,#65532,#65533,#65534,
#65535,#65536,#65537,#65538,#65539,#65540,#65541,#65542,#65543,#65544,#65545,
#65546,#65547,#65548,#65549,#65550,#65551,#65552,#65553,#65554,#65555,#65556,
#65557,#65558,#65559,#65560,#65561,#65562,#65563,#65564,#65565,#65566,#65567,
#65568,#65569,#65570,#65571,#65572,#65573,#65574,#65575,#65576,#65577,#65578,
#65579,#65580,#65581,#65582,#65583,#65584,#65585,#65586,#65587,#65588,#65589,
#65590,#65591,#65592,#65593,#65594,#65595,#65596,#65597,#65598,#65599,#65600,
#65601,#65602,#65603,#65604,#65605,#65606,#65607,#65608,#65609,#65610,#65611,
#65612,#65613,#65614,#65615,#65616,#65617,#65618,#65619,#65620,#65621,#65622,
#65623,#65624,#65625,#65626,#65627,#65628,#65629,#65630,#65631,#65632,#65633,
#65634,#65635,#65636,#65637,#65638,#65639,#65640,#65641,#65642,#65643,#65644,
#65645,#65646,#65647,#65648,#65649,#65650,#65651,#65652,#65653,#65654,#65655,
#65656,#65657,#65658,#65659,#65660,#65661,#65662,#65663,#65664,#65665,#65666,
#65667,#65668,#65669,#65670,#65671,#65672,#65673,#65674,#65675,#65676,#65677,
#65678,#65679,#65680,#65681,#65682,#65683,#65684,#65685,#65686,#65687,#65688,
#65689,#65690,#65691,#65692),.UNSPECIFIED.,.F.,.F.,(4,3,3,3,3,3,3,3,3,3,
3,3,3,3,3,3,3,3,3,3,3,3,3,3,3,3,3,3,3,3,3,3,3,3,3,3,3,3,3,3,3,3,3,3,3,3,
3,3,3,3,3,3,3,3,3,3,3,3,3,3,3,3,3,3,3,3,3,3,3,3,3,3,3,3,3,3,4),(562.345084992573,
562.427965235509,562.510816580263,562.593655547536,562.676500711991,562.759370649371,
562.842332057276,562.925344429649,563.008481840182,563.054314733051,563.138061465753,
563.221705142769,563.305265886835,563.388763748792,563.472226249355,563.555671384847,
563.63911721969,563.722581814928,563.80613500035,563.889732833922,563.973464396784,
564.05329823525,564.137044967952,564.220688644968,564.304249389034,564.387747250991,
564.471209751554,564.554654887046,564.638100721889,564.721565317127,564.805118502549,
564.888716336121,564.972447898983,565.05228173745,565.136028470152,565.219672147168,
565.303232891235,565.386730753191,565.470193253754,565.553638389247,565.63708422409,
565.720548819328,565.80410200475,565.887699838323,565.971431401185,566.051265239649,
566.135011972351,566.218655649366,566.302216393433,566.38571425539,566.469176755952,
566.552621891444,566.636067726287,566.719532321525,566.803085506947,566.886683340519,
566.970414903381,567.050248741848,567.13399547455,567.217639151566,567.301199895632,
567.384697757589,567.468160258151,567.551605393644,567.635051228487,567.718515823725,
567.802069009147,567.885666842719,567.969398405581,568.049232244047,568.134713532804,
568.220077174772,568.305338890218,568.390493180076,568.475584384095,568.560622501914,
568.628270299753),.UNSPECIFIED.);
#504=B_SPLINE_CURVE_WITH_KNOTS('',3,(#65694,#65695,#65696,#65697,#65698,
#65699,#65700,#65701,#65702,#65703,#65704,#65705,#65706,#65707,#65708,#65709,
#65710,#65711,#65712,#65713,#65714,#65715,#65716,#65717,#65718,#65719,#65720,
#65721,#65722,#65723,#65724,#65725,#65726,#65727,#65728,#65729,#65730,#65731,
#65732,#65733,#65734,#65735,#65736,#65737,#65738,#65739,#65740,#65741,#65742,
#65743,#65744,#65745,#65746,#65747,#65748,#65749,#65750,#65751,#65752,#65753,
#65754,#65755,#65756,#65757,#65758,#65759,#65760,#65761,#65762,#65763,#65764,
#65765,#65766,#65767,#65768,#65769,#65770,#65771,#65772,#65773,#65774,#65775,
#65776,#65777,#65778,#65779,#65780,#65781,#65782,#65783,#65784,#65785,#65786,
#65787,#65788,#65789,#65790,#65791,#65792,#65793,#65794,#65795,#65796,#65797,
#65798,#65799,#65800,#65801,#65802,#65803,#65804,#65805,#65806,#65807,#65808,
#65809,#65810,#65811,#65812,#65813,#65814,#65815,#65816,#65817,#65818,#65819,
#65820,#65821,#65822,#65823,#65824,#65825,#65826,#65827,#65828,#65829,#65830,
#65831,#65832,#65833,#65834,#65835,#65836,#65837,#65838,#65839,#65840,#65841,
#65842,#65843,#65844,#65845,#65846,#65847,#65848,#65849,#65850,#65851,#65852,
#65853,#65854,#65855,#65856,#65857,#65858,#65859,#65860,#65861,#65862,#65863,
#65864,#65865,#65866,#65867,#65868,#65869,#65870,#65871,#65872,#65873,#65874,
#65875,#65876,#65877,#65878,#65879,#65880,#65881,#65882,#65883,#65884,#65885,
#65886,#65887,#65888,#65889,#65890,#65891,#65892,#65893,#65894,#65895,#65896,
#65897,#65898,#65899,#65900,#65901,#65902,#65903,#65904,#65905,#65906,#65907,
#65908,#65909,#65910,#65911,#65912,#65913,#65914,#65915,#65916,#65917,#65918,
#65919,#65920,#65921,#65922),.UNSPECIFIED.,.F.,.F.,(4,3,3,3,3,3,3,3,3,3,
3,3,3,3,3,3,3,3,3,3,3,3,3,3,3,3,3,3,3,3,3,3,3,3,3,3,3,3,3,3,3,3,3,3,3,3,
3,3,3,3,3,3,3,3,3,3,3,3,3,3,3,3,3,3,3,3,3,3,3,3,3,3,3,3,3,3,4),(568.62827029991,
568.71920626783,568.810556815388,568.902118985271,568.993991397215,569.048215746246,
569.131962478948,569.215606155964,569.29916690003,569.382664761987,569.46612726255,
569.549572398042,569.633018232885,569.716482828123,569.800036013545,569.883633847117,
569.967365409979,570.047199248445,570.130945981147,570.214589658163,570.298150402229,
570.381648264186,570.465110764749,570.548555900241,570.632001735084,570.715466330322,
570.799019515744,570.882617349317,570.966348912179,571.046182750645,571.129929483347,
571.213573160363,571.29713390443,571.380631766386,571.464094266949,571.547539402442,
571.630985237284,571.714449832523,571.798003017945,571.881600851517,571.965332414379,
572.045166252844,572.128912985546,572.212556662562,572.296117406628,572.379615268585,
572.463077769147,572.546522904639,572.629968739482,572.71343333472,572.796986520142,
572.880584353715,572.964315916576,573.044149755043,573.127896487745,573.211540164761,
573.295100908827,573.378598770784,573.462061271346,573.545506406839,573.628952241681,
573.712416836919,573.795970022341,573.879567855914,573.963299418775,574.043133257242,
574.12569152221,574.208147557982,574.29052255149,574.372836281538,574.455117716533,
574.537385860219,574.619659702699,574.701997233827,574.784370000703,574.866844481791,
574.911455606805),.UNSPECIFIED.);
#505=B_SPLINE_CURVE_WITH_KNOTS('',3,(#65924,#65925,#65926,#65927,#65928,
#65929,#65930,#65931,#65932,#65933,#65934,#65935,#65936,#65937,#65938,#65939,
#65940,#65941,#65942,#65943,#65944,#65945,#65946,#65947,#65948,#65949,#65950,
#65951,#65952,#65953,#65954,#65955,#65956,#65957,#65958,#65959,#65960,#65961,
#65962,#65963,#65964,#65965,#65966,#65967,#65968,#65969,#65970,#65971,#65972,
#65973,#65974,#65975,#65976,#65977,#65978,#65979,#65980,#65981,#65982,#65983,
#65984,#65985,#65986,#65987,#65988,#65989,#65990,#65991,#65992,#65993,#65994,
#65995,#65996,#65997,#65998,#65999,#66000,#66001,#66002,#66003,#66004,#66005,
#66006,#66007,#66008,#66009,#66010,#66011,#66012,#66013,#66014,#66015,#66016,
#66017,#66018,#66019,#66020,#66021,#66022,#66023,#66024,#66025,#66026,#66027,
#66028,#66029,#66030,#66031,#66032,#66033,#66034,#66035,#66036,#66037,#66038,
#66039,#66040,#66041,#66042,#66043,#66044,#66045,#66046,#66047,#66048,#66049,
#66050,#66051,#66052,#66053,#66054,#66055,#66056,#66057,#66058,#66059,#66060,
#66061,#66062,#66063,#66064,#66065,#66066,#66067,#66068,#66069,#66070,#66071,
#66072,#66073,#66074,#66075,#66076,#66077,#66078,#66079,#66080,#66081,#66082,
#66083,#66084,#66085,#66086,#66087,#66088,#66089,#66090,#66091,#66092,#66093,
#66094,#66095,#66096,#66097,#66098,#66099,#66100,#66101,#66102,#66103,#66104,
#66105,#66106,#66107,#66108,#66109,#66110,#66111,#66112,#66113,#66114,#66115,
#66116,#66117,#66118,#66119,#66120,#66121,#66122,#66123,#66124,#66125,#66126,
#66127,#66128,#66129,#66130,#66131,#66132,#66133,#66134,#66135,#66136,#66137,
#66138,#66139,#66140,#66141,#66142,#66143,#66144,#66145,#66146,#66147,#66148,
#66149),.UNSPECIFIED.,.F.,.F.,(4,3,3,3,3,3,3,3,3,3,3,3,3,3,3,3,3,3,3,3,
3,3,3,3,3,3,3,3,3,3,3,3,3,3,3,3,3,3,3,3,3,3,3,3,3,3,3,3,3,3,3,3,3,3,3,3,
3,3,3,3,3,3,3,3,3,3,3,3,3,3,3,3,3,3,3,4),(574.911455606932,575.042116759441,
575.125863492143,575.209507169159,575.293067913225,575.376565775182,575.460028275744,
575.543473411236,575.626919246079,575.710383841317,575.793937026739,575.877534860312,
575.961266423173,576.04110026164,576.124846994342,576.208490671358,576.292051415424,
576.375549277381,576.459011777944,576.542456913436,576.625902748279,576.709367343517,
576.792920528939,576.876518362511,576.960249925373,577.040083763839,577.123830496541,
577.207474173557,577.291034917624,577.374532779581,577.457995280143,577.541440415636,
577.624886250479,577.708350845717,577.791904031139,577.875501864712,577.959233427574,
578.039067266039,578.122813998741,578.206457675757,578.290018419823,578.37351628178,
578.456978782342,578.540423917834,578.623869752677,578.707334347915,578.790887533337,
578.87448536691,578.958216929771,579.038050768238,579.12179750094,579.205441177956,
579.289001922022,579.372499783979,579.455962284542,579.539407420034,579.622853254877,
579.706317850115,579.789871035536,579.873468869109,579.957200431971,580.037034270437,
580.120781003139,580.204424680155,580.287985424221,580.371483286178,580.454945786741,
580.538390922233,580.621836757076,580.705301352314,580.788854537735,580.872452371308,
580.95618393417,581.036017772636,581.173030216201,581.194640914112),
 .UNSPECIFIED.);
#506=B_SPLINE_CURVE_WITH_KNOTS('',3,(#66151,#66152,#66153,#66154,#66155,
#66156,#66157,#66158,#66159,#66160,#66161,#66162,#66163,#66164,#66165,#66166,
#66167,#66168,#66169,#66170,#66171,#66172,#66173,#66174,#66175,#66176,#66177,
#66178,#66179,#66180,#66181,#66182,#66183,#66184,#66185,#66186,#66187,#66188,
#66189,#66190,#66191,#66192,#66193,#66194,#66195,#66196,#66197,#66198,#66199,
#66200,#66201,#66202,#66203,#66204,#66205,#66206,#66207,#66208,#66209,#66210,
#66211,#66212,#66213,#66214,#66215,#66216,#66217,#66218,#66219,#66220,#66221,
#66222,#66223,#66224,#66225,#66226,#66227,#66228,#66229,#66230,#66231,#66232,
#66233,#66234,#66235,#66236,#66237,#66238,#66239,#66240,#66241,#66242,#66243,
#66244,#66245,#66246,#66247,#66248,#66249,#66250,#66251,#66252,#66253,#66254,
#66255,#66256,#66257,#66258,#66259,#66260,#66261,#66262,#66263,#66264,#66265,
#66266,#66267,#66268,#66269,#66270,#66271,#66272,#66273,#66274,#66275,#66276,
#66277,#66278,#66279,#66280,#66281,#66282,#66283,#66284,#66285,#66286,#66287,
#66288,#66289,#66290,#66291,#66292,#66293,#66294,#66295,#66296,#66297,#66298,
#66299,#66300,#66301,#66302,#66303,#66304,#66305,#66306,#66307,#66308,#66309,
#66310,#66311,#66312,#66313,#66314,#66315,#66316,#66317,#66318,#66319,#66320,
#66321,#66322,#66323,#66324,#66325,#66326,#66327,#66328,#66329,#66330,#66331,
#66332,#66333,#66334,#66335,#66336,#66337,#66338,#66339,#66340,#66341,#66342,
#66343,#66344,#66345,#66346,#66347,#66348,#66349,#66350,#66351,#66352,#66353,
#66354,#66355,#66356,#66357,#66358,#66359,#66360,#66361,#66362,#66363,#66364,
#66365,#66366,#66367,#66368,#66369,#66370,#66371,#66372,#66373,#66374,#66375,
#66376,#66377,#66378,#66379),.UNSPECIFIED.,.F.,.F.,(4,3,3,3,3,3,3,3,3,3,
3,3,3,3,3,3,3,3,3,3,3,3,3,3,3,3,3,3,3,3,3,3,3,3,3,3,3,3,3,3,3,3,3,3,3,3,
3,3,3,3,3,3,3,3,3,3,3,3,3,3,3,3,3,3,3,3,3,3,3,3,3,3,3,3,3,3,4),(581.194640914215,
581.277035727267,581.35935063523,581.443806965181,581.526033315061,581.608248433236,
581.690471345369,581.776603827735,581.858944381822,581.941339481402,582.023846563504,
582.035001274835,582.118748007537,582.202391684552,582.285952428619,582.369450290576,
582.452912791138,582.53635792663,582.619803761473,582.703268356711,582.786821542133,
582.870419375705,582.954150938567,583.033984777034,583.117731509736,583.201375186752,
583.284935930819,583.368433792775,583.451896293338,583.535341428831,583.618787263674,
583.702251858912,583.785805044334,583.869402877907,583.953134440769,584.032968279234,
584.116715011936,584.200358688952,584.283919433019,584.367417294976,584.450879795538,
584.534324931031,584.617770765874,584.701235361112,584.784788546534,584.868386380106,
584.952117942968,585.031951781433,585.115698514135,585.19934219115,585.282902935216,
585.366400797173,585.449863297735,585.533308433227,585.61675426807,585.700218863308,
585.783772048729,585.867369882302,585.951101445163,586.030935283632,586.114682016334,
586.19832569335,586.281886437417,586.365384299373,586.448846799936,586.532291935428,
586.615737770271,586.699202365509,586.782755550931,586.866353384504,586.950084947366,
587.029918785831,587.120300133636,587.210388364691,587.300299953113,587.389929836687,
587.477826221184),.UNSPECIFIED.);
#507=B_SPLINE_CURVE_WITH_KNOTS('',3,(#66381,#66382,#66383,#66384,#66385,
#66386,#66387,#66388,#66389,#66390,#66391,#66392,#66393,#66394,#66395,#66396,
#66397,#66398,#66399,#66400,#66401,#66402,#66403,#66404,#66405,#66406,#66407,
#66408,#66409,#66410,#66411,#66412,#66413,#66414,#66415,#66416,#66417,#66418,
#66419,#66420,#66421,#66422,#66423,#66424,#66425,#66426,#66427,#66428,#66429,
#66430,#66431,#66432,#66433,#66434,#66435,#66436,#66437,#66438,#66439,#66440,
#66441,#66442,#66443,#66444,#66445,#66446,#66447,#66448,#66449,#66450,#66451,
#66452,#66453,#66454,#66455,#66456,#66457,#66458,#66459,#66460,#66461,#66462,
#66463,#66464,#66465,#66466,#66467,#66468,#66469,#66470,#66471,#66472,#66473,
#66474,#66475,#66476,#66477,#66478,#66479,#66480,#66481,#66482,#66483,#66484,
#66485,#66486,#66487,#66488,#66489,#66490,#66491,#66492,#66493,#66494,#66495,
#66496,#66497,#66498,#66499,#66500,#66501,#66502,#66503,#66504,#66505,#66506,
#66507,#66508,#66509,#66510,#66511,#66512,#66513,#66514,#66515,#66516,#66517,
#66518,#66519,#66520,#66521,#66522,#66523,#66524,#66525,#66526,#66527,#66528,
#66529,#66530,#66531,#66532,#66533,#66534,#66535,#66536,#66537,#66538,#66539,
#66540,#66541,#66542,#66543,#66544,#66545,#66546,#66547,#66548,#66549,#66550,
#66551,#66552,#66553,#66554,#66555,#66556,#66557,#66558,#66559,#66560,#66561,
#66562,#66563,#66564,#66565,#66566,#66567,#66568,#66569,#66570,#66571,#66572,
#66573,#66574,#66575,#66576,#66577,#66578,#66579,#66580,#66581,#66582,#66583,
#66584,#66585,#66586,#66587,#66588,#66589,#66590,#66591,#66592,#66593,#66594,
#66595,#66596,#66597,#66598,#66599,#66600,#66601,#66602,#66603,#66604,#66605,
#66606,#66607,#66608,#66609),.UNSPECIFIED.,.F.,.F.,(4,3,3,3,3,3,3,3,3,3,
3,3,3,3,3,3,3,3,3,3,3,3,3,3,3,3,3,3,3,3,3,3,3,3,3,3,3,3,3,3,3,3,3,3,3,3,
3,3,3,3,3,3,3,3,3,3,3,3,3,3,3,3,3,3,3,3,3,3,3,3,3,3,3,3,3,3,4),(587.477826221291,
587.563586830846,587.649406073758,587.735297697654,587.82133727072,587.907460242967,
587.993739923875,588.02890228803,588.112649020733,588.196292697749,588.279853441816,
588.363351303773,588.446813804336,588.530258939828,588.613704774672,588.69716936991,
588.780722555333,588.864320388906,588.948051951768,589.02788579023,589.111632522932,
589.195276199948,589.278836944014,589.362334805971,589.445797306534,589.529242442026,
589.612688276869,589.696152872106,589.779706057528,589.863303891101,589.947035453962,
590.026869292429,590.110616025131,590.194259702147,590.277820446213,590.36131830817,
590.444780808732,590.528225944224,590.611671779067,590.695136374305,590.778689559727,
590.8622873933,590.946018956162,591.025852794628,591.10959952733,591.193243204346,
591.276803948412,591.360301810369,591.443764310932,591.527209446424,591.610655281267,
591.694119876505,591.777673061926,591.861270895499,591.945002458361,592.024836296827,
592.108583029529,592.192226706545,592.275787450611,592.359285312567,592.44274781313,
592.526192948622,592.609638783465,592.693103378703,592.776656564124,592.860254397697,
592.943985960559,593.023819799026,593.106705162984,593.18946020447,593.272140356324,
593.354764495462,593.437351451291,593.519941160403,593.602528724221,593.685173429262,
593.761011528471),.UNSPECIFIED.);
#508=B_SPLINE_CURVE_WITH_KNOTS('',3,(#66611,#66612,#66613,#66614,#66615,
#66616,#66617,#66618,#66619,#66620,#66621,#66622,#66623,#66624,#66625,#66626,
#66627,#66628,#66629,#66630,#66631,#66632,#66633,#66634,#66635,#66636,#66637,
#66638,#66639,#66640,#66641,#66642,#66643,#66644,#66645,#66646,#66647,#66648,
#66649,#66650,#66651,#66652,#66653,#66654,#66655,#66656,#66657,#66658,#66659,
#66660,#66661,#66662,#66663,#66664,#66665,#66666,#66667,#66668,#66669,#66670,
#66671,#66672,#66673,#66674,#66675,#66676,#66677,#66678,#66679,#66680,#66681,
#66682,#66683,#66684,#66685,#66686,#66687,#66688,#66689,#66690,#66691,#66692,
#66693,#66694,#66695,#66696,#66697,#66698,#66699,#66700,#66701,#66702,#66703,
#66704,#66705,#66706,#66707,#66708,#66709,#66710,#66711,#66712,#66713,#66714,
#66715,#66716,#66717,#66718,#66719,#66720,#66721,#66722,#66723,#66724,#66725,
#66726,#66727,#66728,#66729,#66730,#66731,#66732,#66733,#66734,#66735,#66736,
#66737,#66738,#66739,#66740,#66741,#66742,#66743,#66744,#66745,#66746,#66747,
#66748,#66749,#66750,#66751,#66752,#66753,#66754,#66755,#66756,#66757,#66758,
#66759,#66760,#66761,#66762,#66763,#66764,#66765,#66766,#66767,#66768,#66769,
#66770,#66771,#66772,#66773,#66774,#66775,#66776,#66777,#66778,#66779,#66780,
#66781,#66782,#66783,#66784,#66785,#66786,#66787,#66788,#66789,#66790,#66791,
#66792,#66793,#66794,#66795,#66796,#66797,#66798,#66799,#66800,#66801,#66802,
#66803,#66804,#66805,#66806,#66807,#66808,#66809,#66810,#66811,#66812,#66813,
#66814,#66815,#66816,#66817,#66818,#66819,#66820,#66821,#66822,#66823,#66824,
#66825,#66826,#66827,#66828,#66829,#66830,#66831,#66832,#66833,#66834,#66835,
#66836,#66837,#66838,#66839),.UNSPECIFIED.,.F.,.F.,(4,3,3,3,3,3,3,3,3,3,
3,3,3,3,3,3,3,3,3,3,3,3,3,3,3,3,3,3,3,3,3,3,3,3,3,3,3,3,3,3,3,3,3,3,3,3,
3,3,3,3,3,3,3,3,3,3,3,3,3,3,3,3,3,3,3,3,3,3,3,3,3,3,3,3,3,3,4),(593.761011528614,
593.866374367455,593.973784241142,594.022803301225,594.106550033927,594.190193710943,
594.27375445501,594.357252316966,594.440714817529,594.524159953021,594.607605787864,
594.691070383102,594.774623568524,594.858221402097,594.941952964959,595.021786803424,
595.105533536126,595.189177213142,595.272737957209,595.356235819165,595.439698319728,
595.52314345522,595.606589290063,595.690053885301,595.773607070723,595.857204904296,
595.940936467158,596.020770305624,596.104517038326,596.188160715342,596.271721459408,
596.355219321365,596.438681821928,596.52212695742,596.605572792263,596.689037387501,
596.772590572923,596.856188406496,596.939919969358,597.019753807823,597.103500540525,
597.187144217541,597.270704961607,597.354202823564,597.437665324127,597.521110459619,
597.604556294462,597.6880208897,597.771574075122,597.855171908694,597.938903471556,
598.018737310022,598.102484042724,598.18612771974,598.269688463806,598.353186325763,
598.436648826325,598.520093961817,598.60353979666,598.687004391898,598.77055757732,
598.854155410893,598.937886973754,599.017720812221,599.101467544923,599.185111221939,
599.268671966005,599.352169827962,599.435632328525,599.519077464017,599.60252329886,
599.685987894098,599.76954107952,599.853138913093,599.936870475955,600.01670431442,
600.04419683565),.UNSPECIFIED.);
#509=B_SPLINE_CURVE_WITH_KNOTS('',3,(#66841,#66842,#66843,#66844,#66845,
#66846,#66847,#66848,#66849,#66850,#66851,#66852,#66853,#66854,#66855,#66856,
#66857,#66858,#66859,#66860,#66861,#66862,#66863,#66864,#66865,#66866,#66867,
#66868,#66869,#66870,#66871,#66872,#66873,#66874,#66875,#66876,#66877,#66878,
#66879,#66880,#66881,#66882,#66883,#66884,#66885,#66886,#66887,#66888,#66889,
#66890,#66891,#66892,#66893,#66894,#66895,#66896,#66897,#66898,#66899,#66900,
#66901,#66902,#66903,#66904,#66905,#66906,#66907,#66908,#66909,#66910,#66911,
#66912,#66913,#66914,#66915,#66916,#66917,#66918,#66919,#66920,#66921,#66922,
#66923,#66924,#66925,#66926,#66927,#66928,#66929,#66930,#66931,#66932,#66933,
#66934,#66935,#66936,#66937,#66938,#66939,#66940,#66941,#66942,#66943,#66944,
#66945,#66946,#66947,#66948,#66949,#66950,#66951,#66952,#66953,#66954,#66955,
#66956,#66957,#66958,#66959,#66960,#66961,#66962,#66963,#66964,#66965,#66966,
#66967,#66968,#66969,#66970,#66971,#66972,#66973,#66974,#66975,#66976,#66977,
#66978,#66979,#66980,#66981,#66982,#66983,#66984,#66985,#66986,#66987,#66988,
#66989,#66990,#66991,#66992,#66993,#66994,#66995,#66996,#66997,#66998,#66999,
#67000,#67001,#67002,#67003,#67004,#67005,#67006,#67007,#67008,#67009,#67010,
#67011,#67012,#67013,#67014,#67015,#67016,#67017,#67018,#67019,#67020,#67021,
#67022,#67023,#67024,#67025,#67026,#67027,#67028,#67029,#67030,#67031,#67032,
#67033,#67034,#67035,#67036,#67037,#67038,#67039,#67040,#67041,#67042,#67043,
#67044,#67045,#67046,#67047,#67048,#67049,#67050,#67051,#67052,#67053,#67054,
#67055,#67056,#67057,#67058,#67059,#67060,#67061,#67062,#67063,#67064,#67065,
#67066,#67067,#67068,#67069),.UNSPECIFIED.,.F.,.F.,(4,3,3,3,3,3,3,3,3,3,
3,3,3,3,3,3,3,3,3,3,3,3,3,3,3,3,3,3,3,3,3,3,3,3,3,3,3,3,3,3,3,3,3,3,3,3,
3,3,3,3,3,3,3,3,3,3,3,3,3,3,3,3,3,3,3,3,3,3,3,3,3,3,3,3,3,3,4),(600.044196835773,
600.127557274234,600.210815756894,600.293992793723,600.377108819792,600.460192280264,
600.543260777893,600.626332723164,600.709426525337,600.79260935285,600.875840271015,
600.959197541668,601.015687816619,601.099434549321,601.183078226337,601.266638970403,
601.35013683236,601.433599332922,601.517044468415,601.600490303258,601.683954898495,
601.767508083917,601.85110591749,601.934837480352,602.014671318819,602.098418051521,
602.182061728537,602.265622472603,602.34912033456,602.432582835123,602.516027970615,
602.599473805458,602.682938400697,602.766491586119,602.850089419691,602.933820982553,
603.013654821018,603.09740155372,603.181045230736,603.264605974802,603.348103836759,
603.431566337322,603.515011472814,603.598457307657,603.681921902895,603.765475088316,
603.849072921889,603.932804484751,604.012638323217,604.096385055919,604.180028732935,
604.263589477001,604.347087338958,604.43054983952,604.513994975012,604.597440809855,
604.680905405093,604.764458590515,604.848056424088,604.93178798695,605.011621825416,
605.095368558118,605.179012235134,605.262572979201,605.346070841158,605.42953334172,
605.512978477213,605.596424312055,605.679888907293,605.763442092715,605.847039926288,
605.93077148915,606.010605327615,606.110691202018,606.210226018898,606.308772913203,
606.327382142661),.UNSPECIFIED.);
#510=B_SPLINE_CURVE_WITH_KNOTS('',3,(#67071,#67072,#67073,#67074,#67075,
#67076,#67077,#67078,#67079,#67080,#67081,#67082,#67083,#67084,#67085,#67086,
#67087,#67088,#67089,#67090,#67091,#67092,#67093,#67094,#67095,#67096,#67097,
#67098,#67099,#67100,#67101,#67102,#67103,#67104,#67105,#67106,#67107,#67108,
#67109,#67110,#67111,#67112,#67113,#67114,#67115,#67116,#67117,#67118,#67119,
#67120,#67121,#67122,#67123,#67124,#67125,#67126,#67127,#67128,#67129,#67130,
#67131,#67132,#67133,#67134,#67135,#67136,#67137,#67138,#67139,#67140,#67141,
#67142,#67143,#67144,#67145,#67146,#67147,#67148,#67149,#67150,#67151,#67152,
#67153,#67154,#67155,#67156,#67157,#67158,#67159,#67160,#67161,#67162,#67163,
#67164,#67165,#67166,#67167,#67168,#67169,#67170,#67171,#67172,#67173,#67174,
#67175,#67176,#67177,#67178,#67179,#67180,#67181,#67182,#67183,#67184,#67185,
#67186,#67187,#67188,#67189,#67190,#67191,#67192,#67193,#67194,#67195,#67196,
#67197,#67198,#67199,#67200,#67201,#67202,#67203,#67204,#67205,#67206,#67207,
#67208,#67209,#67210,#67211,#67212,#67213,#67214,#67215,#67216,#67217,#67218,
#67219,#67220,#67221,#67222,#67223,#67224,#67225,#67226,#67227,#67228,#67229,
#67230,#67231,#67232,#67233,#67234,#67235,#67236,#67237,#67238,#67239,#67240,
#67241,#67242,#67243,#67244,#67245,#67246,#67247,#67248,#67249,#67250,#67251,
#67252,#67253,#67254,#67255,#67256,#67257,#67258,#67259,#67260,#67261,#67262,
#67263,#67264,#67265,#67266,#67267,#67268,#67269,#67270,#67271,#67272,#67273,
#67274,#67275,#67276,#67277,#67278,#67279,#67280,#67281,#67282,#67283,#67284,
#67285,#67286,#67287,#67288,#67289,#67290,#67291,#67292,#67293,#67294,#67295,
#67296,#67297,#67298,#67299,#67300,#67301,#67302),.UNSPECIFIED.,.F.,.F.,
(4,3,3,3,3,3,3,3,3,3,3,3,3,3,3,3,3,3,3,3,3,3,3,3,3,3,3,3,3,3,3,3,3,3,3,
3,3,3,3,3,3,3,3,3,3,3,3,3,3,3,3,3,3,3,3,3,3,3,3,3,3,3,3,3,3,3,3,3,3,3,3,
3,3,3,3,3,3,4),(606.32738214283,606.412657978703,606.495818105016,606.578976589673,
606.662151716541,606.749010994859,606.832321608991,606.915692440895,606.999181171714,
607.009588829814,607.093335562516,607.176979239532,607.260539983599,607.344037845556,
607.427500346118,607.510945481611,607.594391316454,607.677855911692,607.761409097114,
607.845006930686,607.928738493548,608.008572332014,608.092319064716,608.175962741732,
608.259523485799,608.343021347755,608.426483848318,608.50992898381,608.593374818653,
608.676839413891,608.760392599313,608.843990432886,608.927721995748,609.007555834213,
609.091302566915,609.174946243931,609.258506987997,609.342004849953,609.425467350516,
609.508912486008,609.592358320851,609.675822916089,609.759376101511,609.842973935084,
609.926705497945,610.006539336412,610.090286069114,610.173929746129,610.257490490196,
610.340988352152,610.424450852715,610.507895988207,610.59134182305,610.674806418288,
610.75835960371,610.841957437283,610.925689000145,611.005522838611,611.089269571313,
611.172913248329,611.256473992395,611.339971854352,611.423434354915,611.506879490407,
611.59032532525,611.673789920488,611.75734310591,611.840940939483,611.924672502345,
612.00450634081,612.089331029797,612.174044908342,612.25866480143,612.346640463575,
612.431112606904,612.515545829306,612.599957555231,612.61056745001),
 .UNSPECIFIED.);
#511=B_SPLINE_CURVE_WITH_KNOTS('',3,(#67304,#67305,#67306,#67307,#67308,
#67309,#67310,#67311,#67312,#67313,#67314,#67315,#67316,#67317,#67318,#67319,
#67320,#67321,#67322,#67323,#67324,#67325,#67326,#67327,#67328,#67329,#67330,
#67331,#67332,#67333,#67334,#67335,#67336,#67337,#67338,#67339,#67340,#67341,
#67342,#67343,#67344,#67345,#67346,#67347,#67348,#67349,#67350,#67351,#67352,
#67353,#67354,#67355,#67356,#67357,#67358,#67359,#67360,#67361,#67362,#67363,
#67364,#67365,#67366,#67367,#67368,#67369,#67370,#67371,#67372,#67373,#67374,
#67375,#67376,#67377,#67378,#67379,#67380,#67381,#67382,#67383,#67384,#67385,
#67386,#67387,#67388,#67389,#67390,#67391,#67392,#67393,#67394,#67395,#67396,
#67397,#67398,#67399,#67400,#67401,#67402,#67403,#67404,#67405,#67406,#67407,
#67408,#67409,#67410,#67411,#67412,#67413,#67414,#67415,#67416,#67417,#67418,
#67419,#67420,#67421,#67422,#67423,#67424,#67425,#67426,#67427,#67428,#67429,
#67430,#67431,#67432,#67433,#67434,#67435,#67436,#67437,#67438,#67439,#67440,
#67441,#67442,#67443,#67444,#67445,#67446,#67447,#67448,#67449,#67450,#67451,
#67452,#67453,#67454,#67455,#67456,#67457,#67458,#67459,#67460,#67461,#67462,
#67463,#67464,#67465,#67466,#67467,#67468,#67469,#67470,#67471,#67472,#67473,
#67474,#67475,#67476,#67477,#67478,#67479,#67480,#67481,#67482,#67483,#67484,
#67485,#67486,#67487,#67488,#67489,#67490,#67491,#67492,#67493,#67494,#67495,
#67496,#67497,#67498,#67499,#67500,#67501,#67502,#67503,#67504,#67505,#67506,
#67507,#67508,#67509,#67510,#67511,#67512,#67513,#67514,#67515,#67516,#67517,
#67518,#67519,#67520,#67521,#67522,#67523,#67524,#67525,#67526,#67527,#67528,
#67529,#67530,#67531,#67532),.UNSPECIFIED.,.F.,.F.,(4,3,3,3,3,3,3,3,3,3,
3,3,3,3,3,3,3,3,3,3,3,3,3,3,3,3,3,3,3,3,3,3,3,3,3,3,3,3,3,3,3,3,3,3,3,3,
3,3,3,3,3,3,3,3,3,3,3,3,3,3,3,3,3,3,3,3,3,3,3,3,3,3,3,3,3,3,4),(612.610567450196,
612.703061071577,612.796078500098,612.889367888172,612.983000046674,613.003489843009,
613.087236575711,613.170880252728,613.254440996794,613.337938858751,613.421401359314,
613.504846494807,613.58829232965,613.671756924889,613.755310110311,613.838907943884,
613.922639506746,614.002473345209,614.086220077911,614.169863754927,614.253424498993,
614.33692236095,614.420384861513,614.503829997005,614.587275831848,614.670740427086,
614.754293612508,614.83789144608,614.921623008942,615.001456847408,615.08520358011,
615.168847257126,615.252408001192,615.335905863149,615.419368363711,615.502813499204,
615.586259334046,615.669723929284,615.753277114706,615.836874948279,615.920606511141,
616.000440349607,616.084187082309,616.167830759325,616.251391503391,616.334889365348,
616.41835186591,616.501797001402,616.585242836245,616.668707431483,616.752260616905,
616.835858450478,616.919590013339,616.999423851806,617.083170584508,617.166814261524,
617.250375005591,617.333872867547,617.41733536811,617.500780503602,617.584226338445,
617.667690933683,617.751244119105,617.834841952678,617.918573515539,617.998407354005,
618.081085159299,618.163660733751,618.246155174823,618.328588911261,618.41099027326,
618.493378189876,618.575771576746,618.658233567548,618.740730253467,618.823341934791,
618.893752757054),.UNSPECIFIED.);
#512=B_SPLINE_CURVE_WITH_KNOTS('',3,(#67534,#67535,#67536,#67537,#67538,
#67539,#67540,#67541,#67542,#67543,#67544,#67545,#67546,#67547,#67548,#67549,
#67550,#67551,#67552,#67553,#67554,#67555,#67556,#67557,#67558,#67559,#67560,
#67561,#67562,#67563,#67564,#67565,#67566,#67567,#67568,#67569,#67570,#67571,
#67572,#67573,#67574,#67575,#67576,#67577,#67578,#67579,#67580,#67581,#67582,
#67583,#67584,#67585,#67586,#67587,#67588,#67589,#67590,#67591,#67592,#67593,
#67594,#67595,#67596,#67597,#67598,#67599,#67600,#67601,#67602,#67603,#67604,
#67605,#67606,#67607,#67608,#67609,#67610,#67611,#67612,#67613,#67614,#67615,
#67616,#67617,#67618,#67619,#67620,#67621,#67622,#67623,#67624,#67625,#67626,
#67627,#67628,#67629,#67630,#67631,#67632,#67633,#67634,#67635,#67636,#67637,
#67638,#67639,#67640,#67641,#67642,#67643,#67644,#67645,#67646,#67647,#67648,
#67649,#67650,#67651,#67652,#67653,#67654,#67655,#67656,#67657,#67658,#67659,
#67660,#67661,#67662,#67663,#67664,#67665,#67666,#67667,#67668,#67669,#67670,
#67671,#67672,#67673,#67674,#67675,#67676,#67677,#67678,#67679,#67680,#67681,
#67682,#67683,#67684,#67685,#67686,#67687,#67688,#67689,#67690,#67691,#67692,
#67693,#67694,#67695,#67696,#67697,#67698,#67699,#67700,#67701,#67702,#67703,
#67704,#67705,#67706,#67707,#67708,#67709,#67710,#67711,#67712,#67713,#67714,
#67715,#67716,#67717,#67718,#67719,#67720,#67721,#67722,#67723,#67724,#67725,
#67726,#67727,#67728,#67729,#67730,#67731,#67732,#67733,#67734,#67735,#67736,
#67737,#67738,#67739,#67740,#67741,#67742,#67743,#67744,#67745,#67746,#67747,
#67748,#67749,#67750,#67751,#67752,#67753,#67754,#67755,#67756,#67757,#67758,
#67759),.UNSPECIFIED.,.F.,.F.,(4,3,3,3,3,3,3,3,3,3,3,3,3,3,3,3,3,3,3,3,
3,3,3,3,3,3,3,3,3,3,3,3,3,3,3,3,3,3,3,3,3,3,3,3,3,3,3,3,3,3,3,3,3,3,3,3,
3,3,3,3,3,3,3,3,3,3,3,3,3,3,3,3,3,3,3,4),(618.893752757189,618.997390856205,
619.081137588906,619.164781265921,619.248342009987,619.331839871943,619.415302372504,
619.498747507996,619.582193342838,619.665657938075,619.749211123496,619.832808957068,
619.916540519929,619.996374358404,620.080121091106,620.163764768122,620.247325512189,
620.330823374146,620.414285874708,620.497731010201,620.581176845044,620.664641440282,
620.748194625704,620.831792459277,620.915524022139,620.995357860603,621.079104593305,
621.162748270321,621.246309014388,621.329806876344,621.413269376907,621.496714512399,
621.580160347242,621.66362494248,621.747178127902,621.830775961475,621.914507524337,
621.994341362802,622.078088095504,622.161731772519,622.245292516586,622.328790378542,
622.412252879105,622.495698014597,622.579143849439,622.662608444677,622.746161630099,
622.829759463671,622.913491026533,622.993324865001,623.077071597703,623.160715274719,
623.244276018786,623.327773880743,623.411236381306,623.494681516799,623.578127351642,
623.66159194688,623.745145132302,623.828742965875,623.912474528737,623.9923083672,
624.076055099902,624.159698776917,624.243259520983,624.326757382939,624.410219883502,
624.493665018994,624.577110853836,624.660575449074,624.744128634495,624.827726468068,
624.911458030929,624.991291869399,625.116148226334,625.176938064369),
 .UNSPECIFIED.);
#513=B_SPLINE_CURVE_WITH_KNOTS('',3,(#67761,#67762,#67763,#67764,#67765,
#67766,#67767,#67768,#67769,#67770,#67771,#67772,#67773,#67774,#67775,#67776,
#67777,#67778,#67779,#67780,#67781,#67782,#67783,#67784,#67785,#67786,#67787,
#67788,#67789,#67790,#67791,#67792,#67793,#67794,#67795,#67796,#67797,#67798,
#67799,#67800,#67801,#67802,#67803,#67804,#67805,#67806,#67807,#67808,#67809,
#67810,#67811,#67812,#67813,#67814,#67815,#67816,#67817,#67818,#67819,#67820,
#67821,#67822,#67823,#67824,#67825,#67826,#67827,#67828,#67829,#67830,#67831,
#67832,#67833,#67834,#67835,#67836,#67837,#67838,#67839,#67840,#67841,#67842,
#67843,#67844,#67845,#67846,#67847,#67848,#67849,#67850,#67851,#67852,#67853,
#67854,#67855,#67856,#67857,#67858,#67859,#67860,#67861,#67862,#67863,#67864,
#67865,#67866,#67867,#67868,#67869,#67870,#67871,#67872,#67873,#67874,#67875,
#67876,#67877,#67878,#67879,#67880,#67881,#67882,#67883,#67884,#67885,#67886,
#67887,#67888,#67889,#67890,#67891,#67892,#67893,#67894,#67895,#67896,#67897,
#67898,#67899,#67900,#67901,#67902,#67903,#67904,#67905,#67906,#67907,#67908,
#67909,#67910,#67911,#67912,#67913,#67914,#67915,#67916,#67917,#67918,#67919,
#67920,#67921,#67922,#67923,#67924,#67925,#67926,#67927,#67928,#67929,#67930,
#67931,#67932,#67933,#67934,#67935,#67936,#67937,#67938,#67939,#67940,#67941,
#67942,#67943,#67944,#67945,#67946,#67947,#67948,#67949,#67950,#67951,#67952,
#67953,#67954,#67955,#67956,#67957,#67958,#67959,#67960,#67961,#67962,#67963,
#67964,#67965,#67966,#67967,#67968,#67969,#67970,#67971,#67972,#67973,#67974,
#67975,#67976,#67977,#67978,#67979,#67980,#67981,#67982,#67983,#67984,#67985,
#67986,#67987,#67988,#67989),.UNSPECIFIED.,.F.,.F.,(4,3,3,3,3,3,3,3,3,3,
3,3,3,3,3,3,3,3,3,3,3,3,3,3,3,3,3,3,3,3,3,3,3,3,3,3,3,3,3,3,3,3,3,3,3,3,
3,3,3,3,3,3,3,3,3,3,3,3,3,3,3,3,3,3,3,3,3,3,3,3,3,3,3,3,3,3,4),(625.176938064508,
625.259311614705,625.34161229195,625.42386527977,625.50609381087,625.588316912524,
625.670553605361,625.752872415273,625.835233050282,625.917722023103,625.990275371599,
626.074022104303,626.15766578132,626.241226525389,626.324724387348,626.408186887912,
626.491632023406,626.575077858251,626.658542453491,626.742095638914,626.825693472489,
626.909425035352,626.989258873798,627.073005606499,627.156649283513,627.240210027579,
627.323707889534,627.407170390096,627.490615525587,627.574061360429,627.657525955666,
627.741079141087,627.824676974658,627.908408537519,627.988242375997,628.071989108695,
628.155632785706,628.239193529768,628.32269139172,628.406153892279,628.489599027766,
628.573044862605,628.656509457839,628.740062643256,628.823660476825,628.907392039682,
628.987225878196,629.070972610911,629.15461628794,629.238177032019,629.321674893989,
629.405137394565,629.48858253007,629.572028364926,629.655492960177,629.739046145611,
629.822643979196,629.90637554207,629.986209380395,630.069956113086,630.153599790091,
630.237160534146,630.320658396091,630.404120896643,630.487566032125,630.571011866957,
630.654476462184,630.738029647596,630.821627481159,630.905359044011,630.985192882594,
631.074280882029,631.163199898981,631.251887095224,631.340431909341,631.428786118239,
631.460123371444),.UNSPECIFIED.);
#514=B_SPLINE_CURVE_WITH_KNOTS('',3,(#67991,#67992,#67993,#67994,#67995,
#67996,#67997,#67998,#67999,#68000,#68001,#68002,#68003,#68004,#68005,#68006,
#68007,#68008,#68009,#68010,#68011,#68012,#68013,#68014,#68015,#68016,#68017,
#68018,#68019,#68020,#68021,#68022,#68023,#68024,#68025,#68026,#68027,#68028,
#68029,#68030,#68031,#68032,#68033,#68034,#68035,#68036,#68037,#68038,#68039,
#68040,#68041,#68042,#68043,#68044,#68045,#68046,#68047,#68048,#68049,#68050,
#68051,#68052,#68053,#68054,#68055,#68056,#68057,#68058,#68059,#68060,#68061,
#68062,#68063,#68064,#68065,#68066,#68067,#68068,#68069,#68070,#68071,#68072,
#68073,#68074,#68075,#68076,#68077,#68078,#68079,#68080,#68081,#68082,#68083,
#68084,#68085,#68086,#68087,#68088,#68089,#68090,#68091,#68092,#68093,#68094,
#68095,#68096,#68097,#68098,#68099,#68100,#68101,#68102,#68103,#68104,#68105,
#68106,#68107,#68108,#68109,#68110,#68111,#68112,#68113,#68114,#68115,#68116,
#68117,#68118,#68119,#68120,#68121,#68122,#68123,#68124,#68125,#68126,#68127,
#68128,#68129,#68130,#68131,#68132,#68133,#68134,#68135,#68136,#68137,#68138,
#68139,#68140,#68141,#68142,#68143,#68144,#68145,#68146,#68147,#68148,#68149,
#68150,#68151,#68152,#68153,#68154,#68155,#68156,#68157,#68158,#68159,#68160,
#68161,#68162,#68163,#68164,#68165,#68166,#68167,#68168,#68169,#68170,#68171,
#68172,#68173,#68174,#68175,#68176,#68177,#68178,#68179,#68180,#68181,#68182,
#68183,#68184,#68185,#68186,#68187,#68188,#68189,#68190,#68191,#68192,#68193,
#68194,#68195,#68196,#68197,#68198,#68199,#68200,#68201,#68202,#68203,#68204,
#68205,#68206,#68207,#68208,#68209,#68210,#68211,#68212,#68213,#68214,#68215,
#68216,#68217,#68218,#68219),.UNSPECIFIED.,.F.,.F.,(4,3,3,3,3,3,3,3,3,3,
3,3,3,3,3,3,3,3,3,3,3,3,3,3,3,3,3,3,3,3,3,3,3,3,3,3,3,3,3,3,3,3,3,3,3,3,
3,3,3,3,3,3,3,3,3,3,3,3,3,3,3,3,3,3,3,3,3,3,3,3,3,3,3,3,3,3,4),(631.460123371548,
631.546693513228,631.633348853353,631.721055736213,631.80797793898,631.896077161887,
631.984176384793,632.067923117583,632.151566794687,632.235127538841,632.318625400886,
632.402087901536,632.485533037116,632.568978872045,632.65244346737,632.735996652878,
632.819594486535,632.90332604948,632.983159886993,633.066906619599,633.150550296519,
633.234111040491,633.317608902353,633.401071402822,633.484516538222,633.567962372973,
633.65142696812,633.734980153453,633.818577986937,633.902309549713,633.982143389192,
634.065890121777,634.149533798674,634.233094542622,634.316592404458,634.4000549049,
634.48350004027,634.56694587499,634.650410470106,634.733963655405,634.817561488855,
634.901293051595,634.981126891391,635.064873624674,635.148517302272,635.232078046922,
635.315575909461,635.399038410605,635.482483546677,635.565929382098,635.649393977911,
635.732947163902,635.81654499804,635.900276561457,635.98011039359,636.063857125522,
636.147500801769,636.231061545069,636.314559406263,636.398021906071,636.481467040813,
636.564912874911,636.648377469411,636.731930654108,636.815528486962,636.899260049123,
636.979093895789,637.061786402032,637.146976686619,637.229466102182,637.311901894868,
637.394303020694,637.476688404206,637.55910075618,637.641530032067,637.724022169906,
637.743308678728),.UNSPECIFIED.);
#515=B_SPLINE_CURVE_WITH_KNOTS('',3,(#68221,#68222,#68223,#68224,#68225,
#68226,#68227,#68228,#68229,#68230,#68231,#68232,#68233,#68234,#68235,#68236,
#68237,#68238,#68239,#68240,#68241,#68242,#68243,#68244,#68245,#68246,#68247,
#68248,#68249,#68250,#68251,#68252,#68253,#68254,#68255,#68256,#68257,#68258,
#68259,#68260,#68261,#68262,#68263,#68264,#68265,#68266,#68267,#68268,#68269,
#68270,#68271,#68272,#68273,#68274,#68275,#68276,#68277,#68278,#68279,#68280,
#68281,#68282,#68283,#68284,#68285,#68286,#68287,#68288,#68289,#68290,#68291,
#68292,#68293,#68294,#68295,#68296,#68297,#68298,#68299,#68300,#68301,#68302,
#68303,#68304,#68305,#68306,#68307,#68308,#68309,#68310,#68311,#68312,#68313,
#68314,#68315,#68316,#68317,#68318,#68319,#68320,#68321,#68322,#68323,#68324,
#68325,#68326,#68327,#68328,#68329,#68330,#68331,#68332,#68333,#68334,#68335,
#68336,#68337,#68338,#68339,#68340,#68341,#68342,#68343,#68344,#68345,#68346,
#68347,#68348,#68349,#68350,#68351,#68352,#68353,#68354,#68355,#68356,#68357,
#68358,#68359,#68360,#68361,#68362,#68363,#68364,#68365,#68366,#68367,#68368,
#68369,#68370,#68371,#68372,#68373,#68374,#68375,#68376,#68377,#68378,#68379,
#68380,#68381,#68382,#68383,#68384,#68385,#68386,#68387,#68388,#68389,#68390,
#68391,#68392,#68393,#68394,#68395,#68396,#68397,#68398,#68399,#68400,#68401,
#68402,#68403,#68404,#68405,#68406,#68407,#68408,#68409,#68410,#68411,#68412,
#68413,#68414,#68415,#68416,#68417,#68418,#68419,#68420,#68421,#68422,#68423,
#68424,#68425,#68426,#68427,#68428,#68429,#68430,#68431,#68432,#68433,#68434,
#68435,#68436,#68437,#68438,#68439,#68440,#68441,#68442,#68443,#68444,#68445,
#68446,#68447,#68448,#68449),.UNSPECIFIED.,.F.,.F.,(4,3,3,3,3,3,3,3,3,3,
3,3,3,3,3,3,3,3,3,3,3,3,3,3,3,3,3,3,3,3,3,3,3,3,3,3,3,3,3,3,3,3,3,3,3,3,
3,3,3,3,3,3,3,3,3,3,3,3,3,3,3,3,3,3,3,3,3,3,3,3,3,3,3,3,3,3,4),(637.743308678919,
637.853102143197,637.965883558142,637.978077397988,638.061824134453,638.145467815241,
638.229028563087,638.312526428825,638.39598893316,638.479434072418,638.562879911016,
638.646344509996,638.729897699117,638.813495536373,638.89722710285,638.977060900188,
639.060807626974,639.144451298083,639.228012036256,639.311509892338,639.394972387078,
639.478417516778,639.561863345865,639.64532793539,639.728881115197,639.812478943199,
639.896210500623,639.976044402387,640.059791133763,640.143434809401,640.226995552038,
640.310493412517,640.393955911532,640.477401045437,640.560846878652,640.644311472225,
640.727864655931,640.811462487759,640.895194048843,640.975027904586,641.058774661087,
641.142418361982,641.225979129983,641.309477015903,641.392939540389,641.476384699777,
641.559830558465,641.643295177476,641.726848386422,641.810446243421,641.894177829305,
641.974011406785,642.057758095575,642.141401728705,642.224962428956,642.308460247211,
642.391922704397,642.475367796717,642.558813588631,642.642278141223,642.725831284686,
642.809429076606,642.893160598758,642.972994908984,643.056741646573,643.140385328139,
643.223946076417,643.307443942247,643.390906446161,643.474351584687,643.557797422244,
643.641262019876,643.724815207176,643.80841304235,643.892144606327,643.971978411183,
644.026493985907),.UNSPECIFIED.);
#516=B_SPLINE_CURVE_WITH_KNOTS('',3,(#68451,#68452,#68453,#68454,#68455,
#68456,#68457,#68458,#68459,#68460,#68461,#68462,#68463,#68464,#68465,#68466,
#68467,#68468,#68469,#68470,#68471,#68472,#68473,#68474,#68475,#68476,#68477,
#68478,#68479,#68480,#68481,#68482,#68483,#68484,#68485,#68486,#68487,#68488,
#68489,#68490,#68491,#68492,#68493,#68494,#68495,#68496,#68497,#68498,#68499,
#68500,#68501,#68502,#68503,#68504,#68505,#68506,#68507,#68508,#68509,#68510,
#68511,#68512,#68513,#68514,#68515,#68516,#68517,#68518,#68519,#68520,#68521,
#68522,#68523,#68524,#68525,#68526,#68527,#68528,#68529,#68530,#68531,#68532,
#68533,#68534,#68535,#68536,#68537,#68538,#68539,#68540,#68541,#68542,#68543,
#68544,#68545,#68546,#68547,#68548,#68549,#68550,#68551,#68552,#68553,#68554,
#68555,#68556,#68557,#68558,#68559,#68560,#68561,#68562,#68563,#68564,#68565,
#68566,#68567,#68568,#68569,#68570,#68571,#68572,#68573,#68574,#68575,#68576,
#68577,#68578,#68579,#68580,#68581,#68582,#68583,#68584,#68585,#68586,#68587,
#68588,#68589,#68590,#68591,#68592,#68593,#68594,#68595,#68596,#68597,#68598,
#68599,#68600,#68601,#68602,#68603,#68604,#68605,#68606,#68607,#68608,#68609,
#68610,#68611,#68612,#68613,#68614,#68615,#68616,#68617,#68618,#68619,#68620,
#68621,#68622,#68623,#68624,#68625,#68626,#68627,#68628,#68629,#68630,#68631,
#68632,#68633,#68634,#68635,#68636,#68637,#68638,#68639,#68640,#68641,#68642,
#68643,#68644,#68645,#68646,#68647,#68648,#68649,#68650,#68651,#68652,#68653,
#68654,#68655,#68656,#68657,#68658,#68659,#68660,#68661,#68662,#68663,#68664,
#68665,#68666,#68667,#68668,#68669,#68670,#68671,#68672,#68673,#68674,#68675,
#68676,#68677,#68678,#68679),.UNSPECIFIED.,.F.,.F.,(4,3,3,3,3,3,3,3,3,3,
3,3,3,3,3,3,3,3,3,3,3,3,3,3,3,3,3,3,3,3,3,3,3,3,3,3,3,3,3,3,3,3,3,3,3,3,
3,3,3,3,3,3,3,3,3,3,3,3,3,3,3,3,3,3,3,3,3,3,3,3,3,3,3,3,3,3,4),(644.026493986012,
644.109537955112,644.192482538858,644.275348512794,644.362300187868,644.44507887594,
644.527846816126,644.610622659315,644.693425058872,644.776317805284,644.859263325024,
644.942326964429,644.970961913383,645.054708329126,645.138351689163,645.221912116555,
645.305409662465,645.388871849031,645.472316671817,645.555762195533,645.639226481512,
645.722779362358,645.806376893423,645.890108160352,645.969945415582,646.053692273466,
646.137336073569,646.22089693853,646.304394919091,646.387857534394,646.471302782264,
646.554748727028,646.638213429636,646.721766717822,646.805364651814,646.889096310106,
646.968928917781,647.052676524747,647.136321080378,647.219882706454,647.303381452869,
647.386844838472,647.470290859233,647.553737578735,647.637203057182,647.720757118529,
647.804355825444,647.8880882484,647.96791241998,648.05165691988,648.135298362673,
648.218856873399,648.302352505182,648.385812788147,648.469255713997,648.552699349197,
648.636161756846,648.719712785976,648.803308476886,648.887037941935,648.966895922179,
649.050644101301,649.134289212132,649.217851376111,649.30135064278,649.38481452026,
649.468261015592,649.551708192002,649.635174109323,649.718728578814,649.80232767779,
649.886060461603,649.965879424379,650.063250642433,650.160218070957,650.256427406118,
650.309679292896),.UNSPECIFIED.);
#517=B_SPLINE_CURVE_WITH_KNOTS('',3,(#68680,#68681,#68682,#68683,#68684,
#68685,#68686,#68687,#68688,#68689,#68690,#68691,#68692,#68693,#68694,#68695,
#68696,#68697,#68698,#68699,#68700,#68701,#68702,#68703,#68704,#68705,#68706,
#68707,#68708,#68709,#68710,#68711,#68712,#68713,#68714,#68715,#68716,#68717,
#68718,#68719,#68720,#68721,#68722,#68723,#68724,#68725,#68726,#68727,#68728,
#68729,#68730,#68731,#68732,#68733,#68734,#68735,#68736,#68737,#68738,#68739,
#68740,#68741,#68742,#68743,#68744,#68745,#68746,#68747,#68748,#68749,#68750,
#68751,#68752,#68753,#68754,#68755,#68756,#68757,#68758,#68759,#68760,#68761,
#68762,#68763,#68764,#68765,#68766,#68767,#68768,#68769,#68770,#68771,#68772,
#68773,#68774,#68775,#68776,#68777,#68778,#68779,#68780,#68781,#68782,#68783,
#68784,#68785,#68786,#68787,#68788,#68789,#68790,#68791,#68792,#68793,#68794,
#68795,#68796,#68797,#68798,#68799,#68800,#68801,#68802,#68803,#68804,#68805,
#68806,#68807,#68808,#68809,#68810,#68811,#68812,#68813,#68814,#68815,#68816,
#68817,#68818,#68819,#68820,#68821,#68822,#68823,#68824,#68825,#68826,#68827,
#68828,#68829,#68830,#68831,#68832,#68833,#68834,#68835,#68836,#68837,#68838,
#68839,#68840,#68841,#68842,#68843,#68844,#68845,#68846,#68847,#68848,#68849,
#68850,#68851,#68852,#68853,#68854,#68855,#68856,#68857,#68858,#68859,#68860,
#68861,#68862,#68863,#68864,#68865,#68866,#68867,#68868,#68869,#68870,#68871,
#68872,#68873,#68874,#68875,#68876,#68877,#68878,#68879,#68880,#68881,#68882,
#68883,#68884,#68885,#68886,#68887,#68888,#68889,#68890,#68891,#68892,#68893,
#68894,#68895,#68896,#68897,#68898,#68899,#68900,#68901,#68902,#68903,#68904,
#68905,#68906,#68907,#68908),.UNSPECIFIED.,.F.,.F.,(4,3,3,3,3,3,3,3,3,3,
3,3,3,3,3,3,3,3,3,3,3,3,3,3,3,3,3,3,3,3,3,3,3,3,3,3,3,3,3,3,3,3,3,3,3,3,
3,3,3,3,3,3,3,3,3,3,3,3,3,3,3,3,3,3,3,3,3,3,3,3,3,3,3,3,3,3,4),(650.309679293087,
650.393240888994,650.476794100226,650.560356785155,650.64394680446,650.727635725486,
650.811376412273,650.895255518796,650.964862926578,651.048594280005,651.132222559778,
651.215767904574,651.299250381044,651.382697570685,651.466127442671,651.549558075561,
651.633007544585,651.716545808257,651.800128807747,651.883845835778,651.963846428777,
652.047606764442,652.131263971344,652.214838159334,652.298349366392,652.381825016557,
652.465283180996,652.548741912418,652.63221926006,652.715784899703,652.799395044793,
652.883138552625,652.962829930976,653.046603759892,653.130274747674,653.21386298612,
653.29738849552,653.380878776592,653.464351769309,653.547825511206,653.631318036458,
653.71489902901,653.798524646585,653.882283671955,653.961813433175,654.045456562427,
654.12899646569,654.21245337217,654.295847438193,654.379206565333,654.462548596396,
654.545891689939,654.629254001462,654.712706198894,654.796203587478,654.879836649319,
654.960796935374,655.044659957653,655.128419513097,655.212095608986,655.295708181083,
655.379284019893,655.462841641018,655.546399004614,655.629974066765,655.713635427877,
655.797340356763,655.881176104609,655.959780437573,656.043939027961,656.127994732299,
656.211965259881,656.295868258194,656.379720658669,656.46354316079,656.547365129084,
656.592864600267),.UNSPECIFIED.);
#518=B_SPLINE_CURVE_WITH_KNOTS('',3,(#68944,#68945,#68946,#68947,#68948,
#68949,#68950,#68951,#68952,#68953,#68954,#68955,#68956,#68957),
 .UNSPECIFIED.,.F.,.F.,(4,2,2,2,2,2,4),(9.99999997530754E-7,0.14182095517119,
0.287631757675626,0.503086521065188,0.729440907199506,0.877555757740989,
1.02857701706101),.UNSPECIFIED.);
#519=B_SPLINE_CURVE_WITH_KNOTS('',3,(#68959,#68960,#68961,#68962,#68963,
#68964,#68965,#68966,#68967,#68968,#68969,#68970,#68971,#68972,#68973,#68974,
#68975,#68976,#68977,#68978,#68979,#68980,#68981,#68982,#68983,#68984,#68985,
#68986,#68987,#68988,#68989,#68990,#68991,#68992,#68993,#68994,#68995,#68996,
#68997,#68998),.UNSPECIFIED.,.F.,.F.,(4,3,3,3,3,3,3,3,3,3,3,3,3,4),(4.93160007214672E-5,
0.0427649574919466,0.0897675869051093,0.136885129702485,0.183792086508501,
0.226860990507049,0.271471569794514,0.316625657925887,0.36158817713321,
0.405632700818853,0.446562496691295,0.493853126657646,0.540253376387635,
0.570947559363461),.UNSPECIFIED.);
#520=B_SPLINE_CURVE_WITH_KNOTS('',3,(#69000,#69001,#69002,#69003,#69004,
#69005,#69006,#69007,#69008,#69009,#69010,#69011,#69012,#69013,#69014,#69015),
 .UNSPECIFIED.,.F.,.F.,(4,3,3,3,3,4),(0.570947559371518,0.610709772227026,
0.657923274718644,0.663253192970537,0.709071515790179,0.741547465068122),
 .UNSPECIFIED.);
#521=B_SPLINE_CURVE_WITH_KNOTS('',3,(#69016,#69017,#69018,#69019,#69020,
#69021,#69022,#69023),.UNSPECIFIED.,.F.,.F.,(4,2,2,4),(9.9999998720568E-7,
0.131584807698003,0.260004416323543,0.387888081590916),.UNSPECIFIED.);
#522=B_SPLINE_CURVE_WITH_KNOTS('',3,(#69024,#69025,#69026,#69027,#69028,
#69029,#69030,#69031,#69032,#69033,#69034,#69035,#69036),.UNSPECIFIED.,
 .F.,.F.,(4,3,3,3,4),(0.,0.035677492973614,0.0785154168662275,0.121353340758841,
0.141322436288203),.UNSPECIFIED.);
#523=B_SPLINE_CURVE_WITH_KNOTS('',3,(#71664,#71665,#71666,#71667,#71668,
#71669,#71670,#71671,#71672,#71673,#71674,#71675,#71676,#71677,#71678,#71679,
#71680,#71681,#71682,#71683,#71684,#71685,#71686,#71687,#71688,#71689,#71690,
#71691,#71692,#71693,#71694,#71695,#71696,#71697,#71698,#71699,#71700,#71701,
#71702,#71703,#71704,#71705,#71706,#71707,#71708,#71709,#71710,#71711,#71712,
#71713,#71714,#71715,#71716,#71717,#71718,#71719,#71720,#71721,#71722,#71723,
#71724,#71725,#71726,#71727,#71728,#71729,#71730,#71731,#71732,#71733,#71734,
#71735,#71736,#71737,#71738,#71739,#71740,#71741,#71742,#71743,#71744,#71745,
#71746,#71747,#71748,#71749,#71750,#71751,#71752,#71753,#71754,#71755,#71756,
#71757,#71758,#71759,#71760,#71761,#71762,#71763,#71764,#71765,#71766,#71767,
#71768,#71769,#71770,#71771,#71772),.UNSPECIFIED.,.F.,.F.,(4,3,3,3,3,3,
3,3,3,3,3,3,3,3,3,3,3,3,3,3,3,3,3,3,3,3,3,3,3,3,3,3,3,3,3,3,4),(0.,0.0425921116508081,
0.091851351018792,0.141964108158449,0.191921079243666,0.218095752617461,
0.225856603980169,0.23160484665435,0.280505726837147,0.329371060234496,
0.377847157263669,0.425414716551405,0.439775785479548,0.446420638306663,
0.452418457109636,0.499737342125707,0.546051644014923,0.591938747193708,
0.610715853224386,0.643992397049059,0.655720876057318,0.663290984417249,
0.709181628316052,0.755355716299187,0.801114214970311,0.838962703861931,
0.858401290391878,0.865203582172363,0.876928203821775,0.922101076309233,
0.967129201685174,0.987605688361699,0.997059820269138,1.00412746240269,
1.04824287918054,1.09162239942997,1.13094109509738),.UNSPECIFIED.);
#524=B_SPLINE_CURVE_WITH_KNOTS('',3,(#74389,#74390,#74391,#74392,#74393,
#74394,#74395,#74396,#74397,#74398,#74399,#74400,#74401,#74402,#74403,#74404,
#74405,#74406,#74407,#74408,#74409,#74410,#74411,#74412,#74413,#74414,#74415,
#74416,#74417,#74418,#74419,#74420,#74421,#74422,#74423,#74424,#74425,#74426,
#74427,#74428,#74429,#74430,#74431,#74432,#74433,#74434,#74435,#74436,#74437,
#74438,#74439,#74440,#74441,#74442,#74443,#74444,#74445,#74446,#74447,#74448,
#74449,#74450,#74451,#74452,#74453,#74454,#74455,#74456,#74457,#74458,#74459,
#74460,#74461,#74462,#74463,#74464,#74465,#74466,#74467,#74468,#74469,#74470,
#74471,#74472,#74473,#74474,#74475,#74476,#74477,#74478,#74479,#74480,#74481,
#74482,#74483,#74484,#74485,#74486,#74487,#74488,#74489,#74490,#74491),
 .UNSPECIFIED.,.F.,.F.,(4,3,3,3,3,3,3,3,3,3,3,3,3,3,3,3,3,3,3,3,3,3,3,3,
3,3,3,3,3,3,3,3,3,3,4),(0.,0.0356758182649354,0.0785730265952882,0.121470234925641,
0.165563949885192,0.190087645004234,0.198856444779804,0.243742273156061,
0.289203976462101,0.335107841320739,0.380915801839053,0.394295401400751,
0.400490449519785,0.447465268323391,0.494416412115105,0.541058829760706,
0.557943071789862,0.602254762481671,0.609820269595172,0.65601947932705,
0.703024739023473,0.750889917889998,0.79353081291717,0.815029168382123,
0.821776719603583,0.828059272245824,0.836527523847076,0.885339424328542,
0.934151324810009,0.958199867374806,0.969807589082792,0.977523525467601,
1.02733960679315,1.07700026305144,1.12653966532838),.UNSPECIFIED.);
#525=SHAPE_REPRESENTATION_RELATIONSHIP('SRR','None',#74558,#534);
#526=SHAPE_REPRESENTATION_RELATIONSHIP('SRR','None',#74559,#535);
#527=SHAPE_REPRESENTATION_RELATIONSHIP('SRR','None',#74560,#536);
#528=SHAPE_REPRESENTATION_RELATIONSHIP('SRR','None',#74561,#537);
#529=SHAPE_REPRESENTATION_RELATIONSHIP('SRR','None',#74562,#538);
#530=SHAPE_REPRESENTATION_RELATIONSHIP('SRR','None',#74563,#539);
#531=SHAPE_REPRESENTATION_RELATIONSHIP('SRR','None',#74564,#540);
#532=SHAPE_REPRESENTATION_RELATIONSHIP('SRR','None',#74565,#541);
#533=SHAPE_REPRESENTATION_RELATIONSHIP('SRR','None',#74566,#542);
#534=ADVANCED_BREP_SHAPE_REPRESENTATION('',(#552),#74514);
#535=ADVANCED_BREP_SHAPE_REPRESENTATION('',(#553),#74515);
#536=ADVANCED_BREP_SHAPE_REPRESENTATION('',(#554),#74516);
#537=ADVANCED_BREP_SHAPE_REPRESENTATION('',(#555),#74517);
#538=ADVANCED_BREP_SHAPE_REPRESENTATION('',(#556),#74518);
#539=ADVANCED_BREP_SHAPE_REPRESENTATION('',(#557),#74519);
#540=ADVANCED_BREP_SHAPE_REPRESENTATION('',(#558),#74520);
#541=ADVANCED_BREP_SHAPE_REPRESENTATION('',(#559),#74521);
#542=ADVANCED_BREP_SHAPE_REPRESENTATION('',(#560),#74522);
#543=STYLED_ITEM('',(#74612),#552);
#544=STYLED_ITEM('',(#74612),#553);
#545=STYLED_ITEM('',(#74612),#554);
#546=STYLED_ITEM('',(#74612),#555);
#547=STYLED_ITEM('',(#74612),#556);
#548=STYLED_ITEM('',(#74612),#557);
#549=STYLED_ITEM('',(#74612),#558);
#550=STYLED_ITEM('',(#74612),#559);
#551=STYLED_ITEM('',(#74613),#560);
#552=MANIFOLD_SOLID_BREP('Body1',#4722);
#553=MANIFOLD_SOLID_BREP('Body1',#4723);
#554=MANIFOLD_SOLID_BREP('Body1',#4724);
#555=MANIFOLD_SOLID_BREP('Body1',#4725);
#556=MANIFOLD_SOLID_BREP('Body1',#4726);
#557=MANIFOLD_SOLID_BREP('Body1',#4727);
#558=MANIFOLD_SOLID_BREP('Body1',#4728);
#559=MANIFOLD_SOLID_BREP('Body1',#4729);
#560=MANIFOLD_SOLID_BREP('Body1',#4730);
#561=FACE_BOUND('',#834,.T.);
#562=FACE_BOUND('',#835,.T.);
#563=FACE_BOUND('',#839,.T.);
#564=FACE_BOUND('',#840,.T.);
#565=FACE_BOUND('',#848,.T.);
#566=FACE_BOUND('',#849,.T.);
#567=FACE_BOUND('',#855,.T.);
#568=FACE_BOUND('',#856,.T.);
#569=FACE_BOUND('',#869,.T.);
#570=FACE_BOUND('',#870,.T.);
#571=FACE_BOUND('',#871,.T.);
#572=FACE_BOUND('',#873,.T.);
#573=FACE_BOUND('',#874,.T.);
#574=FACE_BOUND('',#875,.T.);
#575=FACE_BOUND('',#888,.T.);
#576=FACE_BOUND('',#889,.T.);
#577=FACE_BOUND('',#890,.T.);
#578=FACE_BOUND('',#892,.T.);
#579=FACE_BOUND('',#893,.T.);
#580=FACE_BOUND('',#894,.T.);
#581=FACE_BOUND('',#905,.T.);
#582=FACE_BOUND('',#906,.T.);
#583=FACE_BOUND('',#907,.T.);
#584=FACE_BOUND('',#909,.T.);
#585=FACE_BOUND('',#910,.T.);
#586=FACE_BOUND('',#911,.T.);
#587=FACE_BOUND('',#924,.T.);
#588=FACE_BOUND('',#925,.T.);
#589=FACE_BOUND('',#926,.T.);
#590=FACE_BOUND('',#928,.T.);
#591=FACE_BOUND('',#929,.T.);
#592=FACE_BOUND('',#930,.T.);
#593=FACE_BOUND('',#934,.T.);
#594=FACE_BOUND('',#944,.T.);
#595=FACE_BOUND('',#945,.T.);
#596=FACE_BOUND('',#949,.T.);
#597=FACE_BOUND('',#950,.T.);
#598=FACE_BOUND('',#958,.T.);
#599=FACE_BOUND('',#959,.T.);
#600=FACE_BOUND('',#965,.T.);
#601=FACE_BOUND('',#966,.T.);
#602=FACE_BOUND('',#984,.T.);
#603=FACE_BOUND('',#989,.T.);
#604=FACE_BOUND('',#991,.T.);
#605=FACE_BOUND('',#994,.T.);
#606=FACE_BOUND('',#997,.T.);
#607=FACE_BOUND('',#1004,.T.);
#608=FACE_BOUND('',#1010,.T.);
#609=PLANE('',#4845);
#610=PLANE('',#4846);
#611=PLANE('',#4850);
#612=PLANE('',#4857);
#613=PLANE('',#4861);
#614=PLANE('',#4862);
#615=PLANE('',#4867);
#616=PLANE('',#4868);
#617=PLANE('',#4871);
#618=PLANE('',#4874);
#619=PLANE('',#4875);
#620=PLANE('',#4878);
#621=PLANE('',#4881);
#622=PLANE('',#4882);
#623=PLANE('',#4902);
#624=PLANE('',#4906);
#625=PLANE('',#4907);
#626=PLANE('',#4911);
#627=PLANE('',#4912);
#628=PLANE('',#4913);
#629=PLANE('',#4914);
#630=PLANE('',#4915);
#631=PLANE('',#4919);
#632=PLANE('',#4923);
#633=PLANE('',#4927);
#634=PLANE('',#4928);
#635=PLANE('',#4930);
#636=PLANE('',#4934);
#637=PLANE('',#4942);
#638=PLANE('',#4946);
#639=PLANE('',#4950);
#640=PLANE('',#4952);
#641=PLANE('',#4956);
#642=PLANE('',#4959);
#643=PLANE('',#4968);
#644=PLANE('',#4972);
#645=PLANE('',#4976);
#646=PLANE('',#4978);
#647=PLANE('',#4982);
#648=PLANE('',#4985);
#649=PLANE('',#4999);
#650=PLANE('',#5000);
#651=PLANE('',#5004);
#652=PLANE('',#5011);
#653=PLANE('',#5015);
#654=PLANE('',#5016);
#655=PLANE('',#5021);
#656=PLANE('',#5022);
#657=PLANE('',#5025);
#658=PLANE('',#5028);
#659=PLANE('',#5029);
#660=PLANE('',#5032);
#661=PLANE('',#5035);
#662=PLANE('',#5036);
#663=PLANE('',#5045);
#664=PLANE('',#5057);
#665=PLANE('',#5058);
#666=PLANE('',#5059);
#667=PLANE('',#5060);
#668=PLANE('',#5061);
#669=PLANE('',#5062);
#670=PLANE('',#5064);
#671=PLANE('',#5068);
#672=PLANE('',#5076);
#673=PLANE('',#5080);
#674=PLANE('',#5081);
#675=PLANE('',#5082);
#676=PLANE('',#5083);
#677=PLANE('',#5084);
#678=PLANE('',#5085);
#679=PLANE('',#5086);
#680=PLANE('',#5087);
#681=PLANE('',#5088);
#682=FACE_OUTER_BOUND('',#826,.T.);
#683=FACE_OUTER_BOUND('',#827,.T.);
#684=FACE_OUTER_BOUND('',#828,.T.);
#685=FACE_OUTER_BOUND('',#829,.T.);
#686=FACE_OUTER_BOUND('',#830,.T.);
#687=FACE_OUTER_BOUND('',#831,.T.);
#688=FACE_OUTER_BOUND('',#832,.T.);
#689=FACE_OUTER_BOUND('',#833,.T.);
#690=FACE_OUTER_BOUND('',#836,.T.);
#691=FACE_OUTER_BOUND('',#837,.T.);
#692=FACE_OUTER_BOUND('',#838,.T.);
#693=FACE_OUTER_BOUND('',#841,.T.);
#694=FACE_OUTER_BOUND('',#842,.T.);
#695=FACE_OUTER_BOUND('',#843,.T.);
#696=FACE_OUTER_BOUND('',#844,.T.);
#697=FACE_OUTER_BOUND('',#845,.T.);
#698=FACE_OUTER_BOUND('',#846,.T.);
#699=FACE_OUTER_BOUND('',#847,.T.);
#700=FACE_OUTER_BOUND('',#850,.T.);
#701=FACE_OUTER_BOUND('',#851,.T.);
#702=FACE_OUTER_BOUND('',#852,.T.);
#703=FACE_OUTER_BOUND('',#853,.T.);
#704=FACE_OUTER_BOUND('',#854,.T.);
#705=FACE_OUTER_BOUND('',#857,.T.);
#706=FACE_OUTER_BOUND('',#858,.T.);
#707=FACE_OUTER_BOUND('',#859,.T.);
#708=FACE_OUTER_BOUND('',#860,.T.);
#709=FACE_OUTER_BOUND('',#861,.T.);
#710=FACE_OUTER_BOUND('',#862,.T.);
#711=FACE_OUTER_BOUND('',#863,.T.);
#712=FACE_OUTER_BOUND('',#864,.T.);
#713=FACE_OUTER_BOUND('',#865,.T.);
#714=FACE_OUTER_BOUND('',#866,.T.);
#715=FACE_OUTER_BOUND('',#867,.T.);
#716=FACE_OUTER_BOUND('',#868,.T.);
#717=FACE_OUTER_BOUND('',#872,.T.);
#718=FACE_OUTER_BOUND('',#876,.T.);
#719=FACE_OUTER_BOUND('',#877,.T.);
#720=FACE_OUTER_BOUND('',#878,.T.);
#721=FACE_OUTER_BOUND('',#879,.T.);
#722=FACE_OUTER_BOUND('',#880,.T.);
#723=FACE_OUTER_BOUND('',#881,.T.);
#724=FACE_OUTER_BOUND('',#882,.T.);
#725=FACE_OUTER_BOUND('',#883,.T.);
#726=FACE_OUTER_BOUND('',#884,.T.);
#727=FACE_OUTER_BOUND('',#885,.T.);
#728=FACE_OUTER_BOUND('',#886,.T.);
#729=FACE_OUTER_BOUND('',#887,.T.);
#730=FACE_OUTER_BOUND('',#891,.T.);
#731=FACE_OUTER_BOUND('',#895,.T.);
#732=FACE_OUTER_BOUND('',#896,.T.);
#733=FACE_OUTER_BOUND('',#897,.T.);
#734=FACE_OUTER_BOUND('',#898,.T.);
#735=FACE_OUTER_BOUND('',#899,.T.);
#736=FACE_OUTER_BOUND('',#900,.T.);
#737=FACE_OUTER_BOUND('',#901,.T.);
#738=FACE_OUTER_BOUND('',#902,.T.);
#739=FACE_OUTER_BOUND('',#903,.T.);
#740=FACE_OUTER_BOUND('',#904,.T.);
#741=FACE_OUTER_BOUND('',#908,.T.);
#742=FACE_OUTER_BOUND('',#912,.T.);
#743=FACE_OUTER_BOUND('',#913,.T.);
#744=FACE_OUTER_BOUND('',#914,.T.);
#745=FACE_OUTER_BOUND('',#915,.T.);
#746=FACE_OUTER_BOUND('',#916,.T.);
#747=FACE_OUTER_BOUND('',#917,.T.);
#748=FACE_OUTER_BOUND('',#918,.T.);
#749=FACE_OUTER_BOUND('',#919,.T.);
#750=FACE_OUTER_BOUND('',#920,.T.);
#751=FACE_OUTER_BOUND('',#921,.T.);
#752=FACE_OUTER_BOUND('',#922,.T.);
#753=FACE_OUTER_BOUND('',#923,.T.);
#754=FACE_OUTER_BOUND('',#927,.T.);
#755=FACE_OUTER_BOUND('',#931,.T.);
#756=FACE_OUTER_BOUND('',#932,.T.);
#757=FACE_OUTER_BOUND('',#933,.T.);
#758=FACE_OUTER_BOUND('',#935,.T.);
#759=FACE_OUTER_BOUND('',#936,.T.);
#760=FACE_OUTER_BOUND('',#937,.T.);
#761=FACE_OUTER_BOUND('',#938,.T.);
#762=FACE_OUTER_BOUND('',#939,.T.);
#763=FACE_OUTER_BOUND('',#940,.T.);
#764=FACE_OUTER_BOUND('',#941,.T.);
#765=FACE_OUTER_BOUND('',#942,.T.);
#766=FACE_OUTER_BOUND('',#943,.T.);
#767=FACE_OUTER_BOUND('',#946,.T.);
#768=FACE_OUTER_BOUND('',#947,.T.);
#769=FACE_OUTER_BOUND('',#948,.T.);
#770=FACE_OUTER_BOUND('',#951,.T.);
#771=FACE_OUTER_BOUND('',#952,.T.);
#772=FACE_OUTER_BOUND('',#953,.T.);
#773=FACE_OUTER_BOUND('',#954,.T.);
#774=FACE_OUTER_BOUND('',#955,.T.);
#775=FACE_OUTER_BOUND('',#956,.T.);
#776=FACE_OUTER_BOUND('',#957,.T.);
#777=FACE_OUTER_BOUND('',#960,.T.);
#778=FACE_OUTER_BOUND('',#961,.T.);
#779=FACE_OUTER_BOUND('',#962,.T.);
#780=FACE_OUTER_BOUND('',#963,.T.);
#781=FACE_OUTER_BOUND('',#964,.T.);
#782=FACE_OUTER_BOUND('',#967,.T.);
#783=FACE_OUTER_BOUND('',#968,.T.);
#784=FACE_OUTER_BOUND('',#969,.T.);
#785=FACE_OUTER_BOUND('',#970,.T.);
#786=FACE_OUTER_BOUND('',#971,.T.);
#787=FACE_OUTER_BOUND('',#972,.T.);
#788=FACE_OUTER_BOUND('',#973,.T.);
#789=FACE_OUTER_BOUND('',#974,.T.);
#790=FACE_OUTER_BOUND('',#975,.T.);
#791=FACE_OUTER_BOUND('',#976,.T.);
#792=FACE_OUTER_BOUND('',#977,.T.);
#793=FACE_OUTER_BOUND('',#978,.T.);
#794=FACE_OUTER_BOUND('',#979,.T.);
#795=FACE_OUTER_BOUND('',#980,.T.);
#796=FACE_OUTER_BOUND('',#981,.T.);
#797=FACE_OUTER_BOUND('',#982,.T.);
#798=FACE_OUTER_BOUND('',#983,.T.);
#799=FACE_OUTER_BOUND('',#985,.T.);
#800=FACE_OUTER_BOUND('',#986,.T.);
#801=FACE_OUTER_BOUND('',#987,.T.);
#802=FACE_OUTER_BOUND('',#988,.T.);
#803=FACE_OUTER_BOUND('',#990,.T.);
#804=FACE_OUTER_BOUND('',#992,.T.);
#805=FACE_OUTER_BOUND('',#993,.T.);
#806=FACE_OUTER_BOUND('',#995,.T.);
#807=FACE_OUTER_BOUND('',#996,.T.);
#808=FACE_OUTER_BOUND('',#998,.T.);
#809=FACE_OUTER_BOUND('',#999,.T.);
#810=FACE_OUTER_BOUND('',#1000,.T.);
#811=FACE_OUTER_BOUND('',#1001,.T.);
#812=FACE_OUTER_BOUND('',#1002,.T.);
#813=FACE_OUTER_BOUND('',#1003,.T.);
#814=FACE_OUTER_BOUND('',#1005,.T.);
#815=FACE_OUTER_BOUND('',#1006,.T.);
#816=FACE_OUTER_BOUND('',#1007,.T.);
#817=FACE_OUTER_BOUND('',#1008,.T.);
#818=FACE_OUTER_BOUND('',#1009,.T.);
#819=FACE_OUTER_BOUND('',#1011,.T.);
#820=FACE_OUTER_BOUND('',#1012,.T.);
#821=FACE_OUTER_BOUND('',#1013,.T.);
#822=FACE_OUTER_BOUND('',#1014,.T.);
#823=FACE_OUTER_BOUND('',#1015,.T.);
#824=FACE_OUTER_BOUND('',#1016,.T.);
#825=FACE_OUTER_BOUND('',#1017,.T.);
#826=EDGE_LOOP('',(#2958,#2959,#2960,#2961));
#827=EDGE_LOOP('',(#2962,#2963,#2964,#2965));
#828=EDGE_LOOP('',(#2966,#2967,#2968,#2969));
#829=EDGE_LOOP('',(#2970,#2971,#2972,#2973));
#830=EDGE_LOOP('',(#2974,#2975,#2976,#2977));
#831=EDGE_LOOP('',(#2978,#2979,#2980,#2981));
#832=EDGE_LOOP('',(#2982,#2983,#2984,#2985));
#833=EDGE_LOOP('',(#2986,#2987,#2988,#2989));
#834=EDGE_LOOP('',(#2990));
#835=EDGE_LOOP('',(#2991));
#836=EDGE_LOOP('',(#2992,#2993,#2994,#2995));
#837=EDGE_LOOP('',(#2996,#2997,#2998,#2999));
#838=EDGE_LOOP('',(#3000,#3001,#3002,#3003));
#839=EDGE_LOOP('',(#3004));
#840=EDGE_LOOP('',(#3005));
#841=EDGE_LOOP('',(#3006,#3007,#3008,#3009));
#842=EDGE_LOOP('',(#3010,#3011,#3012,#3013));
#843=EDGE_LOOP('',(#3014,#3015,#3016,#3017,#3018,#3019,#3020,#3021,#3022,
#3023,#3024,#3025,#3026,#3027,#3028,#3029,#3030,#3031,#3032,#3033));
#844=EDGE_LOOP('',(#3034,#3035,#3036,#3037));
#845=EDGE_LOOP('',(#3038,#3039,#3040,#3041));
#846=EDGE_LOOP('',(#3042,#3043,#3044,#3045));
#847=EDGE_LOOP('',(#3046,#3047,#3048,#3049));
#848=EDGE_LOOP('',(#3050));
#849=EDGE_LOOP('',(#3051));
#850=EDGE_LOOP('',(#3052,#3053,#3054,#3055));
#851=EDGE_LOOP('',(#3056,#3057,#3058,#3059));
#852=EDGE_LOOP('',(#3060,#3061,#3062,#3063));
#853=EDGE_LOOP('',(#3064,#3065,#3066,#3067));
#854=EDGE_LOOP('',(#3068,#3069,#3070,#3071));
#855=EDGE_LOOP('',(#3072));
#856=EDGE_LOOP('',(#3073));
#857=EDGE_LOOP('',(#3074,#3075,#3076,#3077));
#858=EDGE_LOOP('',(#3078,#3079,#3080,#3081));
#859=EDGE_LOOP('',(#3082,#3083,#3084,#3085,#3086,#3087,#3088,#3089,#3090,
#3091,#3092,#3093,#3094,#3095,#3096,#3097,#3098,#3099,#3100,#3101));
#860=EDGE_LOOP('',(#3102,#3103,#3104,#3105));
#861=EDGE_LOOP('',(#3106,#3107,#3108,#3109));
#862=EDGE_LOOP('',(#3110,#3111,#3112,#3113));
#863=EDGE_LOOP('',(#3114,#3115,#3116,#3117));
#864=EDGE_LOOP('',(#3118,#3119,#3120,#3121));
#865=EDGE_LOOP('',(#3122,#3123,#3124,#3125));
#866=EDGE_LOOP('',(#3126,#3127,#3128,#3129));
#867=EDGE_LOOP('',(#3130,#3131,#3132,#3133));
#868=EDGE_LOOP('',(#3134,#3135,#3136,#3137,#3138,#3139,#3140,#3141));
#869=EDGE_LOOP('',(#3142));
#870=EDGE_LOOP('',(#3143));
#871=EDGE_LOOP('',(#3144));
#872=EDGE_LOOP('',(#3145,#3146,#3147,#3148));
#873=EDGE_LOOP('',(#3149));
#874=EDGE_LOOP('',(#3150));
#875=EDGE_LOOP('',(#3151));
#876=EDGE_LOOP('',(#3152,#3153,#3154,#3155));
#877=EDGE_LOOP('',(#3156));
#878=EDGE_LOOP('',(#3157));
#879=EDGE_LOOP('',(#3158,#3159,#3160,#3161));
#880=EDGE_LOOP('',(#3162,#3163,#3164,#3165));
#881=EDGE_LOOP('',(#3166,#3167,#3168,#3169));
#882=EDGE_LOOP('',(#3170,#3171,#3172,#3173));
#883=EDGE_LOOP('',(#3174,#3175,#3176,#3177,#3178,#3179,#3180,#3181,#3182,
#3183,#3184,#3185));
#884=EDGE_LOOP('',(#3186,#3187,#3188,#3189));
#885=EDGE_LOOP('',(#3190,#3191,#3192,#3193));
#886=EDGE_LOOP('',(#3194,#3195,#3196,#3197));
#887=EDGE_LOOP('',(#3198,#3199,#3200,#3201,#3202,#3203,#3204,#3205));
#888=EDGE_LOOP('',(#3206));
#889=EDGE_LOOP('',(#3207));
#890=EDGE_LOOP('',(#3208));
#891=EDGE_LOOP('',(#3209,#3210,#3211,#3212));
#892=EDGE_LOOP('',(#3213));
#893=EDGE_LOOP('',(#3214));
#894=EDGE_LOOP('',(#3215));
#895=EDGE_LOOP('',(#3216));
#896=EDGE_LOOP('',(#3217,#3218,#3219,#3220));
#897=EDGE_LOOP('',(#3221));
#898=EDGE_LOOP('',(#3222,#3223,#3224,#3225));
#899=EDGE_LOOP('',(#3226,#3227,#3228,#3229));
#900=EDGE_LOOP('',(#3230,#3231,#3232,#3233));
#901=EDGE_LOOP('',(#3234,#3235,#3236,#3237));
#902=EDGE_LOOP('',(#3238,#3239,#3240,#3241));
#903=EDGE_LOOP('',(#3242,#3243,#3244,#3245));
#904=EDGE_LOOP('',(#3246,#3247,#3248,#3249));
#905=EDGE_LOOP('',(#3250));
#906=EDGE_LOOP('',(#3251));
#907=EDGE_LOOP('',(#3252));
#908=EDGE_LOOP('',(#3253,#3254,#3255,#3256));
#909=EDGE_LOOP('',(#3257));
#910=EDGE_LOOP('',(#3258));
#911=EDGE_LOOP('',(#3259));
#912=EDGE_LOOP('',(#3260,#3261,#3262,#3263));
#913=EDGE_LOOP('',(#3264));
#914=EDGE_LOOP('',(#3265,#3266,#3267,#3268));
#915=EDGE_LOOP('',(#3269));
#916=EDGE_LOOP('',(#3270,#3271,#3272,#3273));
#917=EDGE_LOOP('',(#3274,#3275,#3276,#3277,#3278,#3279,#3280));
#918=EDGE_LOOP('',(#3281,#3282,#3283,#3284));
#919=EDGE_LOOP('',(#3285,#3286,#3287,#3288));
#920=EDGE_LOOP('',(#3289,#3290,#3291,#3292));
#921=EDGE_LOOP('',(#3293,#3294,#3295,#3296));
#922=EDGE_LOOP('',(#3297,#3298,#3299,#3300));
#923=EDGE_LOOP('',(#3301,#3302,#3303,#3304));
#924=EDGE_LOOP('',(#3305));
#925=EDGE_LOOP('',(#3306));
#926=EDGE_LOOP('',(#3307));
#927=EDGE_LOOP('',(#3308,#3309,#3310,#3311));
#928=EDGE_LOOP('',(#3312));
#929=EDGE_LOOP('',(#3313));
#930=EDGE_LOOP('',(#3314));
#931=EDGE_LOOP('',(#3315,#3316,#3317,#3318));
#932=EDGE_LOOP('',(#3319));
#933=EDGE_LOOP('',(#3320,#3321,#3322,#3323,#3324,#3325,#3326,#3327,#3328));
#934=EDGE_LOOP('',(#3329,#3330));
#935=EDGE_LOOP('',(#3331));
#936=EDGE_LOOP('',(#3332,#3333,#3334,#3335));
#937=EDGE_LOOP('',(#3336,#3337,#3338,#3339));
#938=EDGE_LOOP('',(#3340,#3341,#3342,#3343));
#939=EDGE_LOOP('',(#3344,#3345,#3346,#3347));
#940=EDGE_LOOP('',(#3348,#3349,#3350,#3351));
#941=EDGE_LOOP('',(#3352,#3353,#3354,#3355));
#942=EDGE_LOOP('',(#3356,#3357,#3358,#3359));
#943=EDGE_LOOP('',(#3360,#3361,#3362,#3363));
#944=EDGE_LOOP('',(#3364));
#945=EDGE_LOOP('',(#3365));
#946=EDGE_LOOP('',(#3366,#3367,#3368,#3369));
#947=EDGE_LOOP('',(#3370,#3371,#3372,#3373));
#948=EDGE_LOOP('',(#3374,#3375,#3376,#3377));
#949=EDGE_LOOP('',(#3378));
#950=EDGE_LOOP('',(#3379));
#951=EDGE_LOOP('',(#3380,#3381,#3382,#3383));
#952=EDGE_LOOP('',(#3384,#3385,#3386,#3387));
#953=EDGE_LOOP('',(#3388,#3389,#3390,#3391,#3392,#3393,#3394,#3395,#3396,
#3397,#3398,#3399,#3400,#3401,#3402,#3403,#3404,#3405,#3406,#3407));
#954=EDGE_LOOP('',(#3408,#3409,#3410,#3411));
#955=EDGE_LOOP('',(#3412,#3413,#3414,#3415));
#956=EDGE_LOOP('',(#3416,#3417,#3418,#3419));
#957=EDGE_LOOP('',(#3420,#3421,#3422,#3423));
#958=EDGE_LOOP('',(#3424));
#959=EDGE_LOOP('',(#3425));
#960=EDGE_LOOP('',(#3426,#3427,#3428,#3429));
#961=EDGE_LOOP('',(#3430,#3431,#3432,#3433));
#962=EDGE_LOOP('',(#3434,#3435,#3436,#3437));
#963=EDGE_LOOP('',(#3438,#3439,#3440,#3441));
#964=EDGE_LOOP('',(#3442,#3443,#3444,#3445));
#965=EDGE_LOOP('',(#3446));
#966=EDGE_LOOP('',(#3447));
#967=EDGE_LOOP('',(#3448,#3449,#3450,#3451));
#968=EDGE_LOOP('',(#3452,#3453,#3454,#3455));
#969=EDGE_LOOP('',(#3456,#3457,#3458,#3459,#3460,#3461,#3462,#3463,#3464,
#3465,#3466,#3467,#3468,#3469,#3470,#3471,#3472,#3473,#3474,#3475));
#970=EDGE_LOOP('',(#3476,#3477,#3478,#3479));
#971=EDGE_LOOP('',(#3480,#3481,#3482,#3483,#3484));
#972=EDGE_LOOP('',(#3485,#3486,#3487,#3488));
#973=EDGE_LOOP('',(#3489,#3490,#3491,#3492));
#974=EDGE_LOOP('',(#3493,#3494,#3495,#3496,#3497));
#975=EDGE_LOOP('',(#3498,#3499,#3500));
#976=EDGE_LOOP('',(#3501,#3502,#3503,#3504,#3505,#3506,#3507,#3508,#3509,
#3510));
#977=EDGE_LOOP('',(#3511,#3512,#3513,#3514));
#978=EDGE_LOOP('',(#3515,#3516,#3517,#3518,#3519));
#979=EDGE_LOOP('',(#3520,#3521,#3522,#3523,#3524,#3525,#3526,#3527,#3528,
#3529));
#980=EDGE_LOOP('',(#3530,#3531,#3532,#3533));
#981=EDGE_LOOP('',(#3534,#3535,#3536));
#982=EDGE_LOOP('',(#3537,#3538,#3539,#3540));
#983=EDGE_LOOP('',(#3541,#3542,#3543,#3544,#3545,#3546,#3547,#3548,#3549));
#984=EDGE_LOOP('',(#3550,#3551,#3552,#3553,#3554,#3555,#3556,#3557,#3558,
#3559,#3560,#3561,#3562,#3563,#3564,#3565,#3566,#3567,#3568));
#985=EDGE_LOOP('',(#3569,#3570));
#986=EDGE_LOOP('',(#3571,#3572,#3573,#3574));
#987=EDGE_LOOP('',(#3575,#3576,#3577,#3578,#3579,#3580));
#988=EDGE_LOOP('',(#3581,#3582,#3583,#3584));
#989=EDGE_LOOP('',(#3585));
#990=EDGE_LOOP('',(#3586,#3587,#3588,#3589));
#991=EDGE_LOOP('',(#3590));
#992=EDGE_LOOP('',(#3591,#3592,#3593,#3594));
#993=EDGE_LOOP('',(#3595,#3596,#3597,#3598));
#994=EDGE_LOOP('',(#3599,#3600,#3601,#3602));
#995=EDGE_LOOP('',(#3603,#3604,#3605,#3606));
#996=EDGE_LOOP('',(#3607,#3608,#3609,#3610));
#997=EDGE_LOOP('',(#3611));
#998=EDGE_LOOP('',(#3612));
#999=EDGE_LOOP('',(#3613,#3614,#3615,#3616));
#1000=EDGE_LOOP('',(#3617));
#1001=EDGE_LOOP('',(#3618,#3619,#3620,#3621,#3622,#3623,#3624,#3625,#3626,
#3627,#3628,#3629,#3630,#3631,#3632,#3633,#3634,#3635,#3636,#3637,#3638,
#3639,#3640,#3641,#3642,#3643,#3644,#3645,#3646,#3647,#3648,#3649,#3650,
#3651,#3652,#3653,#3654,#3655,#3656,#3657,#3658,#3659,#3660,#3661,#3662,
#3663,#3664,#3665,#3666,#3667,#3668,#3669,#3670,#3671,#3672,#3673,#3674,
#3675,#3676,#3677,#3678,#3679,#3680,#3681,#3682,#3683,#3684,#3685,#3686,
#3687,#3688,#3689,#3690,#3691,#3692,#3693,#3694,#3695,#3696,#3697,#3698,
#3699,#3700,#3701,#3702,#3703,#3704,#3705,#3706,#3707,#3708,#3709,#3710,
#3711,#3712,#3713,#3714,#3715,#3716,#3717,#3718,#3719,#3720,#3721,#3722,
#3723,#3724,#3725,#3726,#3727,#3728,#3729,#3730,#3731,#3732,#3733,#3734,
#3735,#3736,#3737,#3738,#3739,#3740,#3741,#3742,#3743,#3744,#3745,#3746,
#3747,#3748,#3749,#3750,#3751,#3752,#3753,#3754,#3755,#3756,#3757,#3758,
#3759,#3760,#3761,#3762,#3763,#3764,#3765,#3766,#3767,#3768,#3769,#3770,
#3771,#3772,#3773,#3774,#3775,#3776,#3777,#3778,#3779,#3780,#3781,#3782,
#3783,#3784,#3785,#3786,#3787,#3788,#3789,#3790,#3791,#3792,#3793,#3794,
#3795,#3796,#3797,#3798,#3799,#3800,#3801,#3802,#3803,#3804,#3805,#3806,
#3807,#3808,#3809,#3810,#3811,#3812,#3813,#3814,#3815,#3816,#3817,#3818,
#3819,#3820,#3821,#3822,#3823,#3824,#3825,#3826,#3827));
#1002=EDGE_LOOP('',(#3828,#3829,#3830,#3831,#3832,#3833,#3834,#3835,#3836,
#3837,#3838,#3839,#3840,#3841,#3842,#3843,#3844,#3845,#3846,#3847,#3848,
#3849,#3850,#3851,#3852,#3853,#3854,#3855,#3856,#3857,#3858,#3859,#3860,
#3861,#3862,#3863,#3864,#3865,#3866,#3867,#3868,#3869,#3870,#3871,#3872,
#3873,#3874,#3875,#3876,#3877,#3878,#3879,#3880,#3881,#3882,#3883,#3884,
#3885,#3886,#3887,#3888,#3889,#3890,#3891,#3892,#3893,#3894,#3895,#3896,
#3897,#3898,#3899,#3900,#3901,#3902,#3903,#3904,#3905,#3906,#3907,#3908,
#3909,#3910,#3911,#3912,#3913,#3914,#3915,#3916,#3917,#3918,#3919,#3920,
#3921,#3922,#3923,#3924,#3925,#3926,#3927,#3928,#3929,#3930,#3931,#3932,
#3933,#3934,#3935,#3936,#3937,#3938,#3939,#3940,#3941,#3942,#3943,#3944,
#3945,#3946,#3947,#3948,#3949,#3950,#3951,#3952,#3953,#3954,#3955,#3956,
#3957,#3958,#3959,#3960,#3961,#3962,#3963,#3964,#3965,#3966,#3967,#3968,
#3969,#3970,#3971,#3972,#3973,#3974,#3975,#3976,#3977,#3978,#3979,#3980,
#3981,#3982,#3983,#3984,#3985,#3986,#3987,#3988,#3989,#3990,#3991,#3992,
#3993,#3994,#3995,#3996,#3997,#3998,#3999,#4000,#4001,#4002,#4003,#4004,
#4005,#4006,#4007,#4008,#4009,#4010,#4011,#4012,#4013,#4014,#4015,#4016,
#4017,#4018,#4019,#4020,#4021,#4022,#4023,#4024,#4025,#4026,#4027,#4028,
#4029,#4030,#4031,#4032,#4033,#4034,#4035,#4036,#4037));
#1003=EDGE_LOOP('',(#4038));
#1004=EDGE_LOOP('',(#4039,#4040,#4041,#4042,#4043,#4044));
#1005=EDGE_LOOP('',(#4045,#4046,#4047,#4048));
#1006=EDGE_LOOP('',(#4049,#4050,#4051,#4052));
#1007=EDGE_LOOP('',(#4053,#4054,#4055,#4056));
#1008=EDGE_LOOP('',(#4057,#4058,#4059,#4060));
#1009=EDGE_LOOP('',(#4061));
#1010=EDGE_LOOP('',(#4062,#4063,#4064,#4065,#4066,#4067,#4068));
#1011=EDGE_LOOP('',(#4069,#4070,#4071,#4072));
#1012=EDGE_LOOP('',(#4073,#4074,#4075,#4076));
#1013=EDGE_LOOP('',(#4077,#4078,#4079,#4080));
#1014=EDGE_LOOP('',(#4081,#4082,#4083,#4084,#4085,#4086));
#1015=EDGE_LOOP('',(#4087,#4088,#4089,#4090,#4091,#4092,#4093,#4094,#4095,
#4096,#4097,#4098,#4099,#4100,#4101,#4102,#4103,#4104,#4105,#4106,#4107,
#4108,#4109,#4110,#4111,#4112,#4113,#4114,#4115,#4116,#4117,#4118,#4119,
#4120,#4121,#4122,#4123,#4124,#4125,#4126,#4127,#4128,#4129,#4130,#4131,
#4132,#4133,#4134,#4135,#4136,#4137,#4138,#4139,#4140,#4141,#4142,#4143,
#4144,#4145,#4146,#4147,#4148,#4149,#4150,#4151,#4152,#4153,#4154,#4155,
#4156,#4157,#4158,#4159,#4160,#4161,#4162,#4163,#4164,#4165,#4166,#4167,
#4168,#4169,#4170,#4171,#4172,#4173,#4174,#4175,#4176,#4177,#4178,#4179,
#4180,#4181,#4182,#4183,#4184,#4185,#4186,#4187,#4188,#4189,#4190,#4191,
#4192,#4193,#4194,#4195,#4196,#4197,#4198,#4199,#4200,#4201,#4202,#4203,
#4204,#4205,#4206,#4207,#4208,#4209,#4210,#4211,#4212,#4213,#4214,#4215,
#4216,#4217,#4218,#4219,#4220,#4221,#4222,#4223,#4224,#4225,#4226,#4227,
#4228,#4229,#4230,#4231,#4232,#4233,#4234,#4235,#4236,#4237,#4238,#4239,
#4240,#4241,#4242,#4243,#4244,#4245,#4246,#4247,#4248,#4249,#4250,#4251,
#4252,#4253,#4254,#4255,#4256,#4257,#4258,#4259,#4260,#4261,#4262,#4263,
#4264,#4265,#4266,#4267,#4268,#4269,#4270,#4271,#4272,#4273,#4274,#4275,
#4276,#4277,#4278,#4279,#4280,#4281,#4282,#4283,#4284,#4285,#4286,#4287,
#4288,#4289,#4290,#4291,#4292,#4293,#4294,#4295,#4296,#4297));
#1016=EDGE_LOOP('',(#4298,#4299,#4300,#4301,#4302,#4303,#4304,#4305,#4306,
#4307,#4308,#4309,#4310,#4311,#4312,#4313,#4314,#4315,#4316,#4317,#4318,
#4319,#4320,#4321,#4322,#4323,#4324,#4325,#4326,#4327,#4328,#4329,#4330,
#4331,#4332,#4333,#4334,#4335,#4336,#4337,#4338,#4339,#4340,#4341,#4342,
#4343,#4344,#4345,#4346,#4347,#4348,#4349,#4350,#4351,#4352,#4353,#4354,
#4355,#4356,#4357,#4358,#4359,#4360,#4361,#4362,#4363,#4364,#4365,#4366,
#4367,#4368,#4369,#4370,#4371,#4372,#4373,#4374,#4375,#4376,#4377,#4378,
#4379,#4380,#4381,#4382,#4383,#4384,#4385,#4386,#4387,#4388,#4389,#4390,
#4391,#4392,#4393,#4394,#4395,#4396,#4397,#4398,#4399,#4400,#4401,#4402,
#4403,#4404,#4405,#4406,#4407,#4408,#4409,#4410,#4411,#4412,#4413,#4414,
#4415,#4416,#4417,#4418,#4419,#4420,#4421,#4422,#4423,#4424,#4425,#4426,
#4427,#4428,#4429,#4430,#4431,#4432,#4433,#4434,#4435,#4436,#4437,#4438,
#4439,#4440,#4441,#4442,#4443,#4444,#4445,#4446,#4447,#4448,#4449,#4450,
#4451,#4452,#4453,#4454,#4455,#4456,#4457,#4458,#4459,#4460,#4461,#4462,
#4463,#4464,#4465,#4466,#4467,#4468,#4469,#4470,#4471,#4472,#4473,#4474,
#4475,#4476,#4477,#4478,#4479,#4480,#4481,#4482,#4483,#4484,#4485,#4486,
#4487,#4488,#4489,#4490,#4491,#4492,#4493,#4494,#4495,#4496,#4497,#4498,
#4499,#4500,#4501,#4502,#4503,#4504,#4505,#4506,#4507,#4508,#4509));
#1017=EDGE_LOOP('',(#4510,#4511,#4512,#4513));
#1018=LINE('',#5835,#1215);
#1019=LINE('',#5841,#1216);
#1020=LINE('',#5847,#1217);
#1021=LINE('',#5853,#1218);
#1022=LINE('',#5858,#1219);
#1023=LINE('',#5860,#1220);
#1024=LINE('',#5862,#1221);
#1025=LINE('',#5863,#1222);
#1026=LINE('',#5866,#1223);
#1027=LINE('',#5868,#1224);
#1028=LINE('',#5869,#1225);
#1029=LINE('',#5874,#1226);
#1030=LINE('',#5878,#1227);
#1031=LINE('',#5880,#1228);
#1032=LINE('',#5881,#1229);
#1033=LINE('',#5886,#1230);
#1034=LINE('',#5891,#1231);
#1035=LINE('',#5895,#1232);
#1036=LINE('',#5899,#1233);
#1037=LINE('',#5901,#1234);
#1038=LINE('',#5902,#1235);
#1039=LINE('',#5907,#1236);
#1040=LINE('',#5910,#1237);
#1041=LINE('',#5911,#1238);
#1042=LINE('',#5915,#1239);
#1043=LINE('',#5917,#1240);
#1044=LINE('',#5919,#1241);
#1045=LINE('',#5923,#1242);
#1046=LINE('',#5926,#1243);
#1047=LINE('',#5928,#1244);
#1048=LINE('',#5932,#1245);
#1049=LINE('',#5936,#1246);
#1050=LINE('',#5938,#1247);
#1051=LINE('',#5939,#1248);
#1052=LINE('',#5942,#1249);
#1053=LINE('',#5943,#1250);
#1054=LINE('',#5947,#1251);
#1055=LINE('',#5950,#1252);
#1056=LINE('',#5951,#1253);
#1057=LINE('',#5955,#1254);
#1058=LINE('',#5957,#1255);
#1059=LINE('',#5960,#1256);
#1060=LINE('',#5961,#1257);
#1061=LINE('',#5965,#1258);
#1062=LINE('',#5968,#1259);
#1063=LINE('',#5969,#1260);
#1064=LINE('',#5973,#1261);
#1065=LINE('',#5975,#1262);
#1066=LINE('',#5982,#1263);
#1067=LINE('',#5988,#1264);
#1068=LINE('',#5994,#1265);
#1069=LINE('',#6000,#1266);
#1070=LINE('',#6006,#1267);
#1071=LINE('',#6013,#1268);
#1072=LINE('',#6016,#1269);
#1073=LINE('',#6019,#1270);
#1074=LINE('',#6021,#1271);
#1075=LINE('',#6022,#1272);
#1076=LINE('',#6028,#1273);
#1077=LINE('',#6032,#1274);
#1078=LINE('',#6033,#1275);
#1079=LINE('',#6035,#1276);
#1080=LINE('',#6037,#1277);
#1081=LINE('',#6038,#1278);
#1082=LINE('',#6040,#1279);
#1083=LINE('',#6046,#1280);
#1084=LINE('',#6052,#1281);
#1085=LINE('',#6053,#1282);
#1086=LINE('',#6054,#1283);
#1087=LINE('',#6057,#1284);
#1088=LINE('',#6058,#1285);
#1089=LINE('',#6061,#1286);
#1090=LINE('',#6062,#1287);
#1091=LINE('',#6067,#1288);
#1092=LINE('',#6072,#1289);
#1093=LINE('',#6074,#1290);
#1094=LINE('',#6075,#1291);
#1095=LINE('',#6077,#1292);
#1096=LINE('',#6078,#1293);
#1097=LINE('',#6083,#1294);
#1098=LINE('',#6087,#1295);
#1099=LINE('',#6089,#1296);
#1100=LINE('',#6090,#1297);
#1101=LINE('',#6103,#1298);
#1102=LINE('',#6110,#1299);
#1103=LINE('',#6116,#1300);
#1104=LINE('',#6121,#1301);
#1105=LINE('',#6123,#1302);
#1106=LINE('',#6125,#1303);
#1107=LINE('',#6126,#1304);
#1108=LINE('',#6131,#1305);
#1109=LINE('',#6135,#1306);
#1110=LINE('',#6137,#1307);
#1111=LINE('',#6138,#1308);
#1112=LINE('',#6151,#1309);
#1113=LINE('',#6156,#1310);
#1114=LINE('',#6163,#1311);
#1115=LINE('',#6213,#1312);
#1116=LINE('',#6266,#1313);
#1117=LINE('',#6271,#1314);
#1118=LINE('',#6273,#1315);
#1119=LINE('',#6275,#1316);
#1120=LINE('',#6276,#1317);
#1121=LINE('',#6282,#1318);
#1122=LINE('',#6285,#1319);
#1123=LINE('',#6287,#1320);
#1124=LINE('',#6288,#1321);
#1125=LINE('',#6301,#1322);
#1126=LINE('',#6304,#1323);
#1127=LINE('',#6306,#1324);
#1128=LINE('',#6314,#1325);
#1129=LINE('',#6320,#1326);
#1130=LINE('',#6326,#1327);
#1131=LINE('',#6332,#1328);
#1132=LINE('',#6337,#1329);
#1133=LINE('',#6339,#1330);
#1134=LINE('',#6341,#1331);
#1135=LINE('',#6342,#1332);
#1136=LINE('',#6345,#1333);
#1137=LINE('',#6347,#1334);
#1138=LINE('',#6348,#1335);
#1139=LINE('',#6353,#1336);
#1140=LINE('',#6357,#1337);
#1141=LINE('',#6359,#1338);
#1142=LINE('',#6360,#1339);
#1143=LINE('',#6365,#1340);
#1144=LINE('',#6370,#1341);
#1145=LINE('',#6374,#1342);
#1146=LINE('',#6378,#1343);
#1147=LINE('',#6380,#1344);
#1148=LINE('',#6381,#1345);
#1149=LINE('',#6386,#1346);
#1150=LINE('',#6389,#1347);
#1151=LINE('',#6390,#1348);
#1152=LINE('',#6394,#1349);
#1153=LINE('',#6396,#1350);
#1154=LINE('',#6398,#1351);
#1155=LINE('',#6402,#1352);
#1156=LINE('',#6405,#1353);
#1157=LINE('',#6407,#1354);
#1158=LINE('',#6411,#1355);
#1159=LINE('',#6415,#1356);
#1160=LINE('',#6417,#1357);
#1161=LINE('',#6418,#1358);
#1162=LINE('',#6421,#1359);
#1163=LINE('',#6422,#1360);
#1164=LINE('',#6426,#1361);
#1165=LINE('',#6429,#1362);
#1166=LINE('',#6430,#1363);
#1167=LINE('',#6434,#1364);
#1168=LINE('',#6436,#1365);
#1169=LINE('',#6439,#1366);
#1170=LINE('',#6440,#1367);
#1171=LINE('',#6444,#1368);
#1172=LINE('',#6447,#1369);
#1173=LINE('',#6448,#1370);
#1174=LINE('',#6452,#1371);
#1175=LINE('',#6454,#1372);
#1176=LINE('',#6460,#1373);
#1177=LINE('',#6484,#1374);
#1178=LINE('',#6558,#1375);
#1179=LINE('',#6853,#1376);
#1180=LINE('',#7870,#1377);
#1181=LINE('',#7898,#1378);
#1182=LINE('',#7944,#1379);
#1183=LINE('',#7949,#1380);
#1184=LINE('',#7951,#1381);
#1185=LINE('',#7953,#1382);
#1186=LINE('',#7954,#1383);
#1187=LINE('',#7957,#1384);
#1188=LINE('',#7959,#1385);
#1189=LINE('',#7960,#1386);
#1190=LINE('',#7963,#1387);
#1191=LINE('',#7964,#1388);
#1192=LINE('',#7967,#1389);
#1193=LINE('',#7968,#1390);
#1194=LINE('',#7970,#1391);
#1195=LINE('',#7979,#1392);
#1196=LINE('',#68914,#1393);
#1197=LINE('',#68916,#1394);
#1198=LINE('',#68918,#1395);
#1199=LINE('',#68920,#1396);
#1200=LINE('',#68922,#1397);
#1201=LINE('',#68923,#1398);
#1202=LINE('',#68926,#1399);
#1203=LINE('',#68930,#1400);
#1204=LINE('',#68932,#1401);
#1205=LINE('',#68933,#1402);
#1206=LINE('',#68936,#1403);
#1207=LINE('',#68937,#1404);
#1208=LINE('',#68940,#1405);
#1209=LINE('',#68941,#1406);
#1210=LINE('',#69039,#1407);
#1211=LINE('',#69040,#1408);
#1212=LINE('',#69043,#1409);
#1213=LINE('',#69044,#1410);
#1214=LINE('',#69046,#1411);
#1215=VECTOR('',#5106,7.5);
#1216=VECTOR('',#5113,7.5);
#1217=VECTOR('',#5120,7.5);
#1218=VECTOR('',#5127,7.5);
#1219=VECTOR('',#5132,10.);
#1220=VECTOR('',#5133,10.);
#1221=VECTOR('',#5134,10.);
#1222=VECTOR('',#5135,10.);
#1223=VECTOR('',#5138,10.);
#1224=VECTOR('',#5139,10.);
#1225=VECTOR('',#5140,10.);
#1226=VECTOR('',#5145,10.);
#1227=VECTOR('',#5150,10.);
#1228=VECTOR('',#5151,10.);
#1229=VECTOR('',#5152,10.);
#1230=VECTOR('',#5157,10.);
#1231=VECTOR('',#5162,10.);
#1232=VECTOR('',#5165,10.);
#1233=VECTOR('',#5170,10.);
#1234=VECTOR('',#5171,10.);
#1235=VECTOR('',#5172,10.);
#1236=VECTOR('',#5177,10.);
#1237=VECTOR('',#5182,10.);
#1238=VECTOR('',#5183,10.);
#1239=VECTOR('',#5186,10.);
#1240=VECTOR('',#5187,10.);
#1241=VECTOR('',#5188,10.);
#1242=VECTOR('',#5191,10.);
#1243=VECTOR('',#5194,10.);
#1244=VECTOR('',#5195,10.);
#1245=VECTOR('',#5198,10.);
#1246=VECTOR('',#5203,10.);
#1247=VECTOR('',#5204,10.);
#1248=VECTOR('',#5205,10.);
#1249=VECTOR('',#5208,10.);
#1250=VECTOR('',#5209,10.);
#1251=VECTOR('',#5214,10.);
#1252=VECTOR('',#5217,10.);
#1253=VECTOR('',#5218,10.);
#1254=VECTOR('',#5223,10.);
#1255=VECTOR('',#5226,10.);
#1256=VECTOR('',#5229,10.);
#1257=VECTOR('',#5230,10.);
#1258=VECTOR('',#5235,10.);
#1259=VECTOR('',#5238,10.);
#1260=VECTOR('',#5239,10.);
#1261=VECTOR('',#5244,10.);
#1262=VECTOR('',#5247,10.);
#1263=VECTOR('',#5256,6.00000000000001);
#1264=VECTOR('',#5263,6.00000000000001);
#1265=VECTOR('',#5270,7.5);
#1266=VECTOR('',#5277,7.5);
#1267=VECTOR('',#5284,7.5);
#1268=VECTOR('',#5291,10.);
#1269=VECTOR('',#5294,10.);
#1270=VECTOR('',#5297,9.99999999999999);
#1271=VECTOR('',#5298,9.99999999999999);
#1272=VECTOR('',#5299,10.);
#1273=VECTOR('',#5306,10.);
#1274=VECTOR('',#5309,10.);
#1275=VECTOR('',#5310,9.99999999999999);
#1276=VECTOR('',#5311,9.99999999999999);
#1277=VECTOR('',#5312,10.);
#1278=VECTOR('',#5313,9.99999999999999);
#1279=VECTOR('',#5316,9.99999999999999);
#1280=VECTOR('',#5323,7.5);
#1281=VECTOR('',#5330,10.);
#1282=VECTOR('',#5331,10.);
#1283=VECTOR('',#5332,10.);
#1284=VECTOR('',#5335,9.99999999999999);
#1285=VECTOR('',#5336,10.);
#1286=VECTOR('',#5339,10.);
#1287=VECTOR('',#5340,10.);
#1288=VECTOR('',#5345,7.5);
#1289=VECTOR('',#5350,9.99999999999999);
#1290=VECTOR('',#5351,10.);
#1291=VECTOR('',#5352,9.99999999999999);
#1292=VECTOR('',#5353,9.99999999999999);
#1293=VECTOR('',#5354,10.);
#1294=VECTOR('',#5359,10.);
#1295=VECTOR('',#5364,9.99999999999999);
#1296=VECTOR('',#5365,10.);
#1297=VECTOR('',#5366,9.99999999999999);
#1298=VECTOR('',#5387,6.00000000000001);
#1299=VECTOR('',#5396,6.00000000000001);
#1300=VECTOR('',#5403,7.5);
#1301=VECTOR('',#5408,10.);
#1302=VECTOR('',#5409,10.);
#1303=VECTOR('',#5410,10.);
#1304=VECTOR('',#5411,10.);
#1305=VECTOR('',#5416,10.);
#1306=VECTOR('',#5421,10.);
#1307=VECTOR('',#5422,10.);
#1308=VECTOR('',#5423,10.);
#1309=VECTOR('',#5442,7.5);
#1310=VECTOR('',#5449,7.5);
#1311=VECTOR('',#5458,6.00000000000001);
#1312=VECTOR('',#5463,6.);
#1313=VECTOR('',#5468,7.5);
#1314=VECTOR('',#5473,10.);
#1315=VECTOR('',#5474,10.);
#1316=VECTOR('',#5475,10.);
#1317=VECTOR('',#5476,10.);
#1318=VECTOR('',#5483,10.);
#1319=VECTOR('',#5486,10.);
#1320=VECTOR('',#5487,10.);
#1321=VECTOR('',#5488,10.);
#1322=VECTOR('',#5507,7.5);
#1323=VECTOR('',#5512,7.5);
#1324=VECTOR('',#5513,7.5);
#1325=VECTOR('',#5524,7.5);
#1326=VECTOR('',#5531,7.5);
#1327=VECTOR('',#5538,7.5);
#1328=VECTOR('',#5545,7.5);
#1329=VECTOR('',#5550,10.);
#1330=VECTOR('',#5551,10.);
#1331=VECTOR('',#5552,10.);
#1332=VECTOR('',#5553,10.);
#1333=VECTOR('',#5556,10.);
#1334=VECTOR('',#5557,10.);
#1335=VECTOR('',#5558,10.);
#1336=VECTOR('',#5563,10.);
#1337=VECTOR('',#5568,10.);
#1338=VECTOR('',#5569,10.);
#1339=VECTOR('',#5570,10.);
#1340=VECTOR('',#5575,10.);
#1341=VECTOR('',#5580,10.);
#1342=VECTOR('',#5583,10.);
#1343=VECTOR('',#5588,10.);
#1344=VECTOR('',#5589,10.);
#1345=VECTOR('',#5590,10.);
#1346=VECTOR('',#5595,10.);
#1347=VECTOR('',#5600,10.);
#1348=VECTOR('',#5601,10.);
#1349=VECTOR('',#5604,10.);
#1350=VECTOR('',#5605,10.);
#1351=VECTOR('',#5606,10.);
#1352=VECTOR('',#5609,10.);
#1353=VECTOR('',#5612,10.);
#1354=VECTOR('',#5613,10.);
#1355=VECTOR('',#5616,10.);
#1356=VECTOR('',#5621,10.);
#1357=VECTOR('',#5622,10.);
#1358=VECTOR('',#5623,10.);
#1359=VECTOR('',#5626,10.);
#1360=VECTOR('',#5627,10.);
#1361=VECTOR('',#5632,10.);
#1362=VECTOR('',#5635,10.);
#1363=VECTOR('',#5636,10.);
#1364=VECTOR('',#5641,10.);
#1365=VECTOR('',#5644,10.);
#1366=VECTOR('',#5647,10.);
#1367=VECTOR('',#5648,10.);
#1368=VECTOR('',#5653,10.);
#1369=VECTOR('',#5656,10.);
#1370=VECTOR('',#5657,10.);
#1371=VECTOR('',#5662,10.);
#1372=VECTOR('',#5665,10.);
#1373=VECTOR('',#5672,6.11325);
#1374=VECTOR('',#5675,6.11325);
#1375=VECTOR('',#5680,5.13675);
#1376=VECTOR('',#5689,10.);
#1377=VECTOR('',#5702,7.5);
#1378=VECTOR('',#5703,7.5);
#1379=VECTOR('',#5712,6.);
#1380=VECTOR('',#5717,10.);
#1381=VECTOR('',#5718,10.);
#1382=VECTOR('',#5719,10.);
#1383=VECTOR('',#5720,10.);
#1384=VECTOR('',#5723,10.);
#1385=VECTOR('',#5724,10.);
#1386=VECTOR('',#5725,10.);
#1387=VECTOR('',#5728,10.);
#1388=VECTOR('',#5729,10.);
#1389=VECTOR('',#5732,10.);
#1390=VECTOR('',#5733,10.);
#1391=VECTOR('',#5736,10.);
#1392=VECTOR('',#5749,7.5);
#1393=VECTOR('',#5770,10.);
#1394=VECTOR('',#5771,10.);
#1395=VECTOR('',#5772,10.);
#1396=VECTOR('',#5773,10.);
#1397=VECTOR('',#5774,10.);
#1398=VECTOR('',#5775,10.);
#1399=VECTOR('',#5778,7.);
#1400=VECTOR('',#5783,10.);
#1401=VECTOR('',#5784,10.);
#1402=VECTOR('',#5785,10.);
#1403=VECTOR('',#5788,10.);
#1404=VECTOR('',#5789,10.);
#1405=VECTOR('',#5792,10.);
#1406=VECTOR('',#5793,10.);
#1407=VECTOR('',#5798,10.);
#1408=VECTOR('',#5799,10.);
#1409=VECTOR('',#5802,10.);
#1410=VECTOR('',#5803,10.);
#1411=VECTOR('',#5806,10.);
#1412=CIRCLE('',#4834,7.5);
#1413=CIRCLE('',#4835,7.5);
#1414=CIRCLE('',#4837,7.5);
#1415=CIRCLE('',#4838,7.5);
#1416=CIRCLE('',#4840,7.5);
#1417=CIRCLE('',#4841,7.5);
#1418=CIRCLE('',#4843,7.5);
#1419=CIRCLE('',#4844,7.5);
#1420=CIRCLE('',#4848,3.00000000000002);
#1421=CIRCLE('',#4849,3.00000000000002);
#1422=CIRCLE('',#4852,3.00000000000002);
#1423=CIRCLE('',#4853,3.00000000000002);
#1424=CIRCLE('',#4855,3.00000000000002);
#1425=CIRCLE('',#4856,3.00000000000002);
#1426=CIRCLE('',#4859,3.00000000000002);
#1427=CIRCLE('',#4860,3.00000000000002);
#1428=CIRCLE('',#4863,3.00000000000002);
#1429=CIRCLE('',#4864,3.00000000000002);
#1430=CIRCLE('',#4865,3.00000000000002);
#1431=CIRCLE('',#4866,3.00000000000002);
#1432=CIRCLE('',#4870,3.00000000000002);
#1433=CIRCLE('',#4873,3.00000000000002);
#1434=CIRCLE('',#4877,3.00000000000002);
#1435=CIRCLE('',#4880,3.00000000000002);
#1436=CIRCLE('',#4885,6.00000000000001);
#1437=CIRCLE('',#4886,6.00000000000001);
#1438=CIRCLE('',#4888,6.00000000000001);
#1439=CIRCLE('',#4889,6.00000000000001);
#1440=CIRCLE('',#4891,7.5);
#1441=CIRCLE('',#4892,7.5);
#1442=CIRCLE('',#4894,7.5);
#1443=CIRCLE('',#4895,7.5);
#1444=CIRCLE('',#4897,7.5);
#1445=CIRCLE('',#4898,7.5);
#1446=CIRCLE('',#4900,12.);
#1447=CIRCLE('',#4901,12.);
#1448=CIRCLE('',#4904,12.);
#1449=CIRCLE('',#4905,12.);
#1450=CIRCLE('',#4908,7.5);
#1451=CIRCLE('',#4910,7.5);
#1452=CIRCLE('',#4917,7.5);
#1453=CIRCLE('',#4918,7.5);
#1454=CIRCLE('',#4921,12.);
#1455=CIRCLE('',#4922,12.);
#1456=CIRCLE('',#4925,12.);
#1457=CIRCLE('',#4926,12.);
#1458=CIRCLE('',#4931,6.00000000000001);
#1459=CIRCLE('',#4933,6.00000000000001);
#1460=CIRCLE('',#4937,6.00000000000001);
#1461=CIRCLE('',#4938,6.00000000000001);
#1462=CIRCLE('',#4940,7.5);
#1463=CIRCLE('',#4941,7.5);
#1464=CIRCLE('',#4944,12.);
#1465=CIRCLE('',#4945,12.);
#1466=CIRCLE('',#4948,12.);
#1467=CIRCLE('',#4949,12.);
#1468=CIRCLE('',#4951,7.5);
#1469=CIRCLE('',#4953,7.5);
#1470=CIRCLE('',#4955,7.5);
#1471=CIRCLE('',#4957,7.5);
#1472=CIRCLE('',#4962,6.00000000000001);
#1473=CIRCLE('',#4963,6.00000000000001);
#1474=CIRCLE('',#4966,7.5);
#1475=CIRCLE('',#4967,7.5);
#1476=CIRCLE('',#4970,12.);
#1477=CIRCLE('',#4971,12.);
#1478=CIRCLE('',#4974,12.);
#1479=CIRCLE('',#4975,12.);
#1480=CIRCLE('',#4977,7.5);
#1481=CIRCLE('',#4979,7.5);
#1482=CIRCLE('',#4981,7.5);
#1483=CIRCLE('',#4984,7.5);
#1484=CIRCLE('',#4988,7.5);
#1485=CIRCLE('',#4989,7.5);
#1486=CIRCLE('',#4991,7.5);
#1487=CIRCLE('',#4992,7.5);
#1488=CIRCLE('',#4994,7.5);
#1489=CIRCLE('',#4995,7.5);
#1490=CIRCLE('',#4997,7.5);
#1491=CIRCLE('',#4998,7.5);
#1492=CIRCLE('',#5002,3.00000000000002);
#1493=CIRCLE('',#5003,3.00000000000002);
#1494=CIRCLE('',#5006,3.00000000000002);
#1495=CIRCLE('',#5007,3.00000000000002);
#1496=CIRCLE('',#5009,3.00000000000002);
#1497=CIRCLE('',#5010,3.00000000000002);
#1498=CIRCLE('',#5013,3.00000000000002);
#1499=CIRCLE('',#5014,3.00000000000002);
#1500=CIRCLE('',#5017,3.00000000000002);
#1501=CIRCLE('',#5018,3.00000000000002);
#1502=CIRCLE('',#5019,3.00000000000002);
#1503=CIRCLE('',#5020,3.00000000000002);
#1504=CIRCLE('',#5024,3.00000000000002);
#1505=CIRCLE('',#5027,3.00000000000002);
#1506=CIRCLE('',#5031,3.00000000000002);
#1507=CIRCLE('',#5034,3.00000000000002);
#1508=CIRCLE('',#5040,6.11325);
#1509=CIRCLE('',#5042,5.13675);
#1510=CIRCLE('',#5046,6.11325);
#1511=CIRCLE('',#5051,7.5);
#1512=CIRCLE('',#5052,7.5);
#1513=CIRCLE('',#5056,6.);
#1514=CIRCLE('',#5065,7.5);
#1515=CIRCLE('',#5067,7.5);
#1516=CIRCLE('',#5071,5.91675);
#1517=CIRCLE('',#5072,5.91675);
#1518=CIRCLE('',#5074,4.91825);
#1519=CIRCLE('',#5075,4.91825);
#1520=CIRCLE('',#5077,7.);
#1521=CIRCLE('',#5079,7.);
#1522=VERTEX_POINT('',#5832);
#1523=VERTEX_POINT('',#5834);
#1524=VERTEX_POINT('',#5838);
#1525=VERTEX_POINT('',#5840);
#1526=VERTEX_POINT('',#5844);
#1527=VERTEX_POINT('',#5846);
#1528=VERTEX_POINT('',#5850);
#1529=VERTEX_POINT('',#5852);
#1530=VERTEX_POINT('',#5856);
#1531=VERTEX_POINT('',#5857);
#1532=VERTEX_POINT('',#5859);
#1533=VERTEX_POINT('',#5861);
#1534=VERTEX_POINT('',#5865);
#1535=VERTEX_POINT('',#5867);
#1536=VERTEX_POINT('',#5871);
#1537=VERTEX_POINT('',#5873);
#1538=VERTEX_POINT('',#5877);
#1539=VERTEX_POINT('',#5879);
#1540=VERTEX_POINT('',#5883);
#1541=VERTEX_POINT('',#5885);
#1542=VERTEX_POINT('',#5889);
#1543=VERTEX_POINT('',#5890);
#1544=VERTEX_POINT('',#5892);
#1545=VERTEX_POINT('',#5894);
#1546=VERTEX_POINT('',#5898);
#1547=VERTEX_POINT('',#5900);
#1548=VERTEX_POINT('',#5904);
#1549=VERTEX_POINT('',#5906);
#1550=VERTEX_POINT('',#5913);
#1551=VERTEX_POINT('',#5914);
#1552=VERTEX_POINT('',#5916);
#1553=VERTEX_POINT('',#5918);
#1554=VERTEX_POINT('',#5920);
#1555=VERTEX_POINT('',#5922);
#1556=VERTEX_POINT('',#5924);
#1557=VERTEX_POINT('',#5927);
#1558=VERTEX_POINT('',#5929);
#1559=VERTEX_POINT('',#5931);
#1560=VERTEX_POINT('',#5935);
#1561=VERTEX_POINT('',#5937);
#1562=VERTEX_POINT('',#5941);
#1563=VERTEX_POINT('',#5945);
#1564=VERTEX_POINT('',#5949);
#1565=VERTEX_POINT('',#5953);
#1566=VERTEX_POINT('',#5959);
#1567=VERTEX_POINT('',#5963);
#1568=VERTEX_POINT('',#5967);
#1569=VERTEX_POINT('',#5971);
#1570=VERTEX_POINT('',#5979);
#1571=VERTEX_POINT('',#5981);
#1572=VERTEX_POINT('',#5985);
#1573=VERTEX_POINT('',#5987);
#1574=VERTEX_POINT('',#5991);
#1575=VERTEX_POINT('',#5993);
#1576=VERTEX_POINT('',#5997);
#1577=VERTEX_POINT('',#5999);
#1578=VERTEX_POINT('',#6003);
#1579=VERTEX_POINT('',#6005);
#1580=VERTEX_POINT('',#6009);
#1581=VERTEX_POINT('',#6010);
#1582=VERTEX_POINT('',#6012);
#1583=VERTEX_POINT('',#6014);
#1584=VERTEX_POINT('',#6018);
#1585=VERTEX_POINT('',#6020);
#1586=VERTEX_POINT('',#6024);
#1587=VERTEX_POINT('',#6026);
#1588=VERTEX_POINT('',#6030);
#1589=VERTEX_POINT('',#6031);
#1590=VERTEX_POINT('',#6034);
#1591=VERTEX_POINT('',#6036);
#1592=VERTEX_POINT('',#6041);
#1593=VERTEX_POINT('',#6044);
#1594=VERTEX_POINT('',#6050);
#1595=VERTEX_POINT('',#6051);
#1596=VERTEX_POINT('',#6056);
#1597=VERTEX_POINT('',#6060);
#1598=VERTEX_POINT('',#6064);
#1599=VERTEX_POINT('',#6066);
#1600=VERTEX_POINT('',#6070);
#1601=VERTEX_POINT('',#6071);
#1602=VERTEX_POINT('',#6073);
#1603=VERTEX_POINT('',#6076);
#1604=VERTEX_POINT('',#6080);
#1605=VERTEX_POINT('',#6082);
#1606=VERTEX_POINT('',#6086);
#1607=VERTEX_POINT('',#6088);
#1608=VERTEX_POINT('',#6098);
#1609=VERTEX_POINT('',#6101);
#1610=VERTEX_POINT('',#6107);
#1611=VERTEX_POINT('',#6109);
#1612=VERTEX_POINT('',#6113);
#1613=VERTEX_POINT('',#6115);
#1614=VERTEX_POINT('',#6119);
#1615=VERTEX_POINT('',#6120);
#1616=VERTEX_POINT('',#6122);
#1617=VERTEX_POINT('',#6124);
#1618=VERTEX_POINT('',#6128);
#1619=VERTEX_POINT('',#6130);
#1620=VERTEX_POINT('',#6134);
#1621=VERTEX_POINT('',#6136);
#1622=VERTEX_POINT('',#6143);
#1623=VERTEX_POINT('',#6146);
#1624=VERTEX_POINT('',#6149);
#1625=VERTEX_POINT('',#6153);
#1626=VERTEX_POINT('',#6160);
#1627=VERTEX_POINT('',#6162);
#1628=VERTEX_POINT('',#6166);
#1629=VERTEX_POINT('',#6167);
#1630=VERTEX_POINT('',#6212);
#1631=VERTEX_POINT('',#6214);
#1632=VERTEX_POINT('',#6237);
#1633=VERTEX_POINT('',#6263);
#1634=VERTEX_POINT('',#6265);
#1635=VERTEX_POINT('',#6269);
#1636=VERTEX_POINT('',#6270);
#1637=VERTEX_POINT('',#6272);
#1638=VERTEX_POINT('',#6274);
#1639=VERTEX_POINT('',#6278);
#1640=VERTEX_POINT('',#6280);
#1641=VERTEX_POINT('',#6284);
#1642=VERTEX_POINT('',#6286);
#1643=VERTEX_POINT('',#6293);
#1644=VERTEX_POINT('',#6296);
#1645=VERTEX_POINT('',#6299);
#1646=VERTEX_POINT('',#6305);
#1647=VERTEX_POINT('',#6311);
#1648=VERTEX_POINT('',#6313);
#1649=VERTEX_POINT('',#6317);
#1650=VERTEX_POINT('',#6319);
#1651=VERTEX_POINT('',#6323);
#1652=VERTEX_POINT('',#6325);
#1653=VERTEX_POINT('',#6329);
#1654=VERTEX_POINT('',#6331);
#1655=VERTEX_POINT('',#6335);
#1656=VERTEX_POINT('',#6336);
#1657=VERTEX_POINT('',#6338);
#1658=VERTEX_POINT('',#6340);
#1659=VERTEX_POINT('',#6344);
#1660=VERTEX_POINT('',#6346);
#1661=VERTEX_POINT('',#6350);
#1662=VERTEX_POINT('',#6352);
#1663=VERTEX_POINT('',#6356);
#1664=VERTEX_POINT('',#6358);
#1665=VERTEX_POINT('',#6362);
#1666=VERTEX_POINT('',#6364);
#1667=VERTEX_POINT('',#6368);
#1668=VERTEX_POINT('',#6369);
#1669=VERTEX_POINT('',#6371);
#1670=VERTEX_POINT('',#6373);
#1671=VERTEX_POINT('',#6377);
#1672=VERTEX_POINT('',#6379);
#1673=VERTEX_POINT('',#6383);
#1674=VERTEX_POINT('',#6385);
#1675=VERTEX_POINT('',#6392);
#1676=VERTEX_POINT('',#6393);
#1677=VERTEX_POINT('',#6395);
#1678=VERTEX_POINT('',#6397);
#1679=VERTEX_POINT('',#6399);
#1680=VERTEX_POINT('',#6401);
#1681=VERTEX_POINT('',#6403);
#1682=VERTEX_POINT('',#6406);
#1683=VERTEX_POINT('',#6408);
#1684=VERTEX_POINT('',#6410);
#1685=VERTEX_POINT('',#6414);
#1686=VERTEX_POINT('',#6416);
#1687=VERTEX_POINT('',#6420);
#1688=VERTEX_POINT('',#6424);
#1689=VERTEX_POINT('',#6428);
#1690=VERTEX_POINT('',#6432);
#1691=VERTEX_POINT('',#6438);
#1692=VERTEX_POINT('',#6442);
#1693=VERTEX_POINT('',#6446);
#1694=VERTEX_POINT('',#6450);
#1695=VERTEX_POINT('',#6458);
#1696=VERTEX_POINT('',#6459);
#1697=VERTEX_POINT('',#6461);
#1698=VERTEX_POINT('',#6466);
#1699=VERTEX_POINT('',#6482);
#1700=VERTEX_POINT('',#6483);
#1701=VERTEX_POINT('',#6485);
#1702=VERTEX_POINT('',#6508);
#1703=VERTEX_POINT('',#6515);
#1704=VERTEX_POINT('',#6556);
#1705=VERTEX_POINT('',#6557);
#1706=VERTEX_POINT('',#6559);
#1707=VERTEX_POINT('',#6598);
#1708=VERTEX_POINT('',#6653);
#1709=VERTEX_POINT('',#6700);
#1710=VERTEX_POINT('',#6752);
#1711=VERTEX_POINT('',#6851);
#1712=VERTEX_POINT('',#6852);
#1713=VERTEX_POINT('',#6854);
#1714=VERTEX_POINT('',#7023);
#1715=VERTEX_POINT('',#7050);
#1716=VERTEX_POINT('',#7240);
#1717=VERTEX_POINT('',#7245);
#1718=VERTEX_POINT('',#7324);
#1719=VERTEX_POINT('',#7326);
#1720=VERTEX_POINT('',#7332);
#1721=VERTEX_POINT('',#7458);
#1722=VERTEX_POINT('',#7580);
#1723=VERTEX_POINT('',#7706);
#1724=VERTEX_POINT('',#7713);
#1725=VERTEX_POINT('',#7803);
#1726=VERTEX_POINT('',#7810);
#1727=VERTEX_POINT('',#7867);
#1728=VERTEX_POINT('',#7869);
#1729=VERTEX_POINT('',#7871);
#1730=VERTEX_POINT('',#7884);
#1731=VERTEX_POINT('',#7897);
#1732=VERTEX_POINT('',#7943);
#1733=VERTEX_POINT('',#7947);
#1734=VERTEX_POINT('',#7948);
#1735=VERTEX_POINT('',#7950);
#1736=VERTEX_POINT('',#7952);
#1737=VERTEX_POINT('',#7956);
#1738=VERTEX_POINT('',#7958);
#1739=VERTEX_POINT('',#7962);
#1740=VERTEX_POINT('',#7966);
#1741=VERTEX_POINT('',#7974);
#1742=VERTEX_POINT('',#7977);
#1743=VERTEX_POINT('',#7983);
#1744=VERTEX_POINT('',#7984);
#1745=VERTEX_POINT('',#8064);
#1746=VERTEX_POINT('',#8066);
#1747=VERTEX_POINT('',#8110);
#1748=VERTEX_POINT('',#8355);
#1749=VERTEX_POINT('',#8366);
#1750=VERTEX_POINT('',#8614);
#1751=VERTEX_POINT('',#8627);
#1752=VERTEX_POINT('',#8872);
#1753=VERTEX_POINT('',#8883);
#1754=VERTEX_POINT('',#8895);
#1755=VERTEX_POINT('',#8906);
#1756=VERTEX_POINT('',#9154);
#1757=VERTEX_POINT('',#9166);
#1758=VERTEX_POINT('',#9414);
#1759=VERTEX_POINT('',#9425);
#1760=VERTEX_POINT('',#9673);
#1761=VERTEX_POINT('',#9685);
#1762=VERTEX_POINT('',#9933);
#1763=VERTEX_POINT('',#9944);
#1764=VERTEX_POINT('',#10192);
#1765=VERTEX_POINT('',#10203);
#1766=VERTEX_POINT('',#10451);
#1767=VERTEX_POINT('',#10462);
#1768=VERTEX_POINT('',#10707);
#1769=VERTEX_POINT('',#10952);
#1770=VERTEX_POINT('',#11197);
#1771=VERTEX_POINT('',#11209);
#1772=VERTEX_POINT('',#11454);
#1773=VERTEX_POINT('',#11465);
#1774=VERTEX_POINT('',#11710);
#1775=VERTEX_POINT('',#11723);
#1776=VERTEX_POINT('',#11734);
#1777=VERTEX_POINT('',#11745);
#1778=VERTEX_POINT('',#11990);
#1779=VERTEX_POINT('',#12001);
#1780=VERTEX_POINT('',#12249);
#1781=VERTEX_POINT('',#12260);
#1782=VERTEX_POINT('',#12508);
#1783=VERTEX_POINT('',#12519);
#1784=VERTEX_POINT('',#12530);
#1785=VERTEX_POINT('',#12542);
#1786=VERTEX_POINT('',#12787);
#1787=VERTEX_POINT('',#12798);
#1788=VERTEX_POINT('',#13043);
#1789=VERTEX_POINT('',#13057);
#1790=VERTEX_POINT('',#13302);
#1791=VERTEX_POINT('',#13313);
#1792=VERTEX_POINT('',#13325);
#1793=VERTEX_POINT('',#13336);
#1794=VERTEX_POINT('',#13584);
#1795=VERTEX_POINT('',#13596);
#1796=VERTEX_POINT('',#13844);
#1797=VERTEX_POINT('',#13855);
#1798=VERTEX_POINT('',#13866);
#1799=VERTEX_POINT('',#13878);
#1800=VERTEX_POINT('',#14126);
#1801=VERTEX_POINT('',#14137);
#1802=VERTEX_POINT('',#14385);
#1803=VERTEX_POINT('',#14396);
#1804=VERTEX_POINT('',#14644);
#1805=VERTEX_POINT('',#14655);
#1806=VERTEX_POINT('',#14668);
#1807=VERTEX_POINT('',#14913);
#1808=VERTEX_POINT('',#15158);
#1809=VERTEX_POINT('',#15170);
#1810=VERTEX_POINT('',#15181);
#1811=VERTEX_POINT('',#15192);
#1812=VERTEX_POINT('',#15437);
#1813=VERTEX_POINT('',#15450);
#1814=VERTEX_POINT('',#15461);
#1815=VERTEX_POINT('',#15472);
#1816=VERTEX_POINT('',#15717);
#1817=VERTEX_POINT('',#15728);
#1818=VERTEX_POINT('',#15739);
#1819=VERTEX_POINT('',#15750);
#1820=VERTEX_POINT('',#15998);
#1821=VERTEX_POINT('',#16009);
#1822=VERTEX_POINT('',#16020);
#1823=VERTEX_POINT('',#16032);
#1824=VERTEX_POINT('',#16277);
#1825=VERTEX_POINT('',#16288);
#1826=VERTEX_POINT('',#16533);
#1827=VERTEX_POINT('',#16546);
#1828=VERTEX_POINT('',#16557);
#1829=VERTEX_POINT('',#16568);
#1830=VERTEX_POINT('',#16580);
#1831=VERTEX_POINT('',#16591);
#1832=VERTEX_POINT('',#16602);
#1833=VERTEX_POINT('',#16614);
#1834=VERTEX_POINT('',#16862);
#1835=VERTEX_POINT('',#16873);
#1836=VERTEX_POINT('',#16884);
#1837=VERTEX_POINT('',#16896);
#1838=VERTEX_POINT('',#16907);
#1839=VERTEX_POINT('',#16918);
#1840=VERTEX_POINT('',#16930);
#1841=VERTEX_POINT('',#16941);
#1842=VERTEX_POINT('',#17189);
#1843=VERTEX_POINT('',#17200);
#1844=VERTEX_POINT('',#17213);
#1845=VERTEX_POINT('',#17224);
#1846=VERTEX_POINT('',#17235);
#1847=VERTEX_POINT('',#17247);
#1848=VERTEX_POINT('',#17258);
#1849=VERTEX_POINT('',#17506);
#1850=VERTEX_POINT('',#17515);
#1851=VERTEX_POINT('',#17517);
#1852=VERTEX_POINT('',#17526);
#1853=VERTEX_POINT('',#17537);
#1854=VERTEX_POINT('',#17782);
#1855=VERTEX_POINT('',#17795);
#1856=VERTEX_POINT('',#17806);
#1857=VERTEX_POINT('',#17817);
#1858=VERTEX_POINT('',#18062);
#1859=VERTEX_POINT('',#18073);
#1860=VERTEX_POINT('',#18084);
#1861=VERTEX_POINT('',#18095);
#1862=VERTEX_POINT('',#18108);
#1863=VERTEX_POINT('',#18119);
#1864=VERTEX_POINT('',#18130);
#1865=VERTEX_POINT('',#18142);
#1866=VERTEX_POINT('',#18153);
#1867=VERTEX_POINT('',#18164);
#1868=VERTEX_POINT('',#18409);
#1869=VERTEX_POINT('',#18654);
#1870=VERTEX_POINT('',#18665);
#1871=VERTEX_POINT('',#18676);
#1872=VERTEX_POINT('',#18688);
#1873=VERTEX_POINT('',#18699);
#1874=VERTEX_POINT('',#18710);
#1875=VERTEX_POINT('',#18722);
#1876=VERTEX_POINT('',#18733);
#1877=VERTEX_POINT('',#18744);
#1878=VERTEX_POINT('',#18755);
#1879=VERTEX_POINT('',#18767);
#1880=VERTEX_POINT('',#18778);
#1881=VERTEX_POINT('',#18789);
#1882=VERTEX_POINT('',#18801);
#1883=VERTEX_POINT('',#18812);
#1884=VERTEX_POINT('',#18823);
#1885=VERTEX_POINT('',#18834);
#1886=VERTEX_POINT('',#18847);
#1887=VERTEX_POINT('',#18858);
#1888=VERTEX_POINT('',#18869);
#1889=VERTEX_POINT('',#18881);
#1890=VERTEX_POINT('',#18892);
#1891=VERTEX_POINT('',#19140);
#1892=VERTEX_POINT('',#19151);
#1893=VERTEX_POINT('',#19163);
#1894=VERTEX_POINT('',#19174);
#1895=VERTEX_POINT('',#19185);
#1896=VERTEX_POINT('',#19197);
#1897=VERTEX_POINT('',#19208);
#1898=VERTEX_POINT('',#19219);
#1899=VERTEX_POINT('',#19467);
#1900=VERTEX_POINT('',#19480);
#1901=VERTEX_POINT('',#19491);
#1902=VERTEX_POINT('',#19502);
#1903=VERTEX_POINT('',#19514);
#1904=VERTEX_POINT('',#19525);
#1905=VERTEX_POINT('',#19536);
#1906=VERTEX_POINT('',#19548);
#1907=VERTEX_POINT('',#19793);
#1908=VERTEX_POINT('',#19804);
#1909=VERTEX_POINT('',#20049);
#1910=VERTEX_POINT('',#20061);
#1911=VERTEX_POINT('',#20072);
#1912=VERTEX_POINT('',#20083);
#1913=VERTEX_POINT('',#20331);
#1914=VERTEX_POINT('',#20342);
#1915=VERTEX_POINT('',#20353);
#1916=VERTEX_POINT('',#20364);
#1917=VERTEX_POINT('',#20609);
#1918=VERTEX_POINT('',#20620);
#1919=VERTEX_POINT('',#20631);
#1920=VERTEX_POINT('',#20643);
#1921=VERTEX_POINT('',#20888);
#1922=VERTEX_POINT('',#20899);
#1923=VERTEX_POINT('',#20910);
#1924=VERTEX_POINT('',#20923);
#1925=VERTEX_POINT('',#21168);
#1926=VERTEX_POINT('',#21413);
#1927=VERTEX_POINT('',#21425);
#1928=VERTEX_POINT('',#21436);
#1929=VERTEX_POINT('',#21684);
#1930=VERTEX_POINT('',#21695);
#1931=VERTEX_POINT('',#21943);
#1932=VERTEX_POINT('',#21954);
#1933=VERTEX_POINT('',#22202);
#1934=VERTEX_POINT('',#22214);
#1935=VERTEX_POINT('',#22462);
#1936=VERTEX_POINT('',#22473);
#1937=VERTEX_POINT('',#22721);
#1938=VERTEX_POINT('',#22734);
#1939=VERTEX_POINT('',#22982);
#1940=VERTEX_POINT('',#22993);
#1941=VERTEX_POINT('',#23005);
#1942=VERTEX_POINT('',#23016);
#1943=VERTEX_POINT('',#23261);
#1944=VERTEX_POINT('',#23273);
#1945=VERTEX_POINT('',#23518);
#1946=VERTEX_POINT('',#23529);
#1947=VERTEX_POINT('',#23774);
#1948=VERTEX_POINT('',#23786);
#1949=VERTEX_POINT('',#23797);
#1950=VERTEX_POINT('',#23808);
#1951=VERTEX_POINT('',#24056);
#1952=VERTEX_POINT('',#24067);
#1953=VERTEX_POINT('',#24563);
#1954=VERTEX_POINT('',#24564);
#1955=VERTEX_POINT('',#24614);
#1956=VERTEX_POINT('',#24616);
#1957=VERTEX_POINT('',#24629);
#1958=VERTEX_POINT('',#24856);
#1959=VERTEX_POINT('',#25086);
#1960=VERTEX_POINT('',#25313);
#1961=VERTEX_POINT('',#25540);
#1962=VERTEX_POINT('',#25770);
#1963=VERTEX_POINT('',#26000);
#1964=VERTEX_POINT('',#26227);
#1965=VERTEX_POINT('',#26454);
#1966=VERTEX_POINT('',#26465);
#1967=VERTEX_POINT('',#26695);
#1968=VERTEX_POINT('',#26925);
#1969=VERTEX_POINT('',#27155);
#1970=VERTEX_POINT('',#27385);
#1971=VERTEX_POINT('',#27612);
#1972=VERTEX_POINT('',#27842);
#1973=VERTEX_POINT('',#28072);
#1974=VERTEX_POINT('',#28083);
#1975=VERTEX_POINT('',#28313);
#1976=VERTEX_POINT('',#28543);
#1977=VERTEX_POINT('',#28773);
#1978=VERTEX_POINT('',#29000);
#1979=VERTEX_POINT('',#29230);
#1980=VERTEX_POINT('',#29460);
#1981=VERTEX_POINT('',#29690);
#1982=VERTEX_POINT('',#29917);
#1983=VERTEX_POINT('',#30147);
#1984=VERTEX_POINT('',#30377);
#1985=VERTEX_POINT('',#30604);
#1986=VERTEX_POINT('',#30834);
#1987=VERTEX_POINT('',#31064);
#1988=VERTEX_POINT('',#31076);
#1989=VERTEX_POINT('',#31306);
#1990=VERTEX_POINT('',#31539);
#1991=VERTEX_POINT('',#31769);
#1992=VERTEX_POINT('',#31996);
#1993=VERTEX_POINT('',#32226);
#1994=VERTEX_POINT('',#32456);
#1995=VERTEX_POINT('',#32683);
#1996=VERTEX_POINT('',#32694);
#1997=VERTEX_POINT('',#32924);
#1998=VERTEX_POINT('',#33154);
#1999=VERTEX_POINT('',#33381);
#2000=VERTEX_POINT('',#33611);
#2001=VERTEX_POINT('',#33841);
#2002=VERTEX_POINT('',#34068);
#2003=VERTEX_POINT('',#34295);
#2004=VERTEX_POINT('',#34525);
#2005=VERTEX_POINT('',#34755);
#2006=VERTEX_POINT('',#34985);
#2007=VERTEX_POINT('',#35218);
#2008=VERTEX_POINT('',#35448);
#2009=VERTEX_POINT('',#35675);
#2010=VERTEX_POINT('',#35905);
#2011=VERTEX_POINT('',#36135);
#2012=VERTEX_POINT('',#36362);
#2013=VERTEX_POINT('',#36592);
#2014=VERTEX_POINT('',#36822);
#2015=VERTEX_POINT('',#37052);
#2016=VERTEX_POINT('',#37279);
#2017=VERTEX_POINT('',#37509);
#2018=VERTEX_POINT('',#37520);
#2019=VERTEX_POINT('',#37750);
#2020=VERTEX_POINT('',#37977);
#2021=VERTEX_POINT('',#38207);
#2022=VERTEX_POINT('',#38437);
#2023=VERTEX_POINT('',#38664);
#2024=VERTEX_POINT('',#38891);
#2025=VERTEX_POINT('',#39121);
#2026=VERTEX_POINT('',#39351);
#2027=VERTEX_POINT('',#39581);
#2028=VERTEX_POINT('',#39811);
#2029=VERTEX_POINT('',#40041);
#2030=VERTEX_POINT('',#40268);
#2031=VERTEX_POINT('',#40498);
#2032=VERTEX_POINT('',#40728);
#2033=VERTEX_POINT('',#40955);
#2034=VERTEX_POINT('',#41185);
#2035=VERTEX_POINT('',#41415);
#2036=VERTEX_POINT('',#41645);
#2037=VERTEX_POINT('',#41872);
#2038=VERTEX_POINT('',#42102);
#2039=VERTEX_POINT('',#42332);
#2040=VERTEX_POINT('',#42344);
#2041=VERTEX_POINT('',#42571);
#2042=VERTEX_POINT('',#42801);
#2043=VERTEX_POINT('',#43031);
#2044=VERTEX_POINT('',#43261);
#2045=VERTEX_POINT('',#43491);
#2046=VERTEX_POINT('',#43721);
#2047=VERTEX_POINT('',#43948);
#2048=VERTEX_POINT('',#44178);
#2049=VERTEX_POINT('',#44408);
#2050=VERTEX_POINT('',#44635);
#2051=VERTEX_POINT('',#44865);
#2052=VERTEX_POINT('',#45095);
#2053=VERTEX_POINT('',#45325);
#2054=VERTEX_POINT('',#45549);
#2055=VERTEX_POINT('',#45779);
#2056=VERTEX_POINT('',#46009);
#2057=VERTEX_POINT('',#46239);
#2058=VERTEX_POINT('',#46466);
#2059=VERTEX_POINT('',#46696);
#2060=VERTEX_POINT('',#46893);
#2061=VERTEX_POINT('',#46895);
#2062=VERTEX_POINT('',#47041);
#2063=VERTEX_POINT('',#47271);
#2064=VERTEX_POINT('',#47501);
#2065=VERTEX_POINT('',#47731);
#2066=VERTEX_POINT('',#47961);
#2067=VERTEX_POINT('',#48191);
#2068=VERTEX_POINT('',#48418);
#2069=VERTEX_POINT('',#48645);
#2070=VERTEX_POINT('',#48875);
#2071=VERTEX_POINT('',#49105);
#2072=VERTEX_POINT('',#49332);
#2073=VERTEX_POINT('',#49562);
#2074=VERTEX_POINT('',#49573);
#2075=VERTEX_POINT('',#49803);
#2076=VERTEX_POINT('',#50030);
#2077=VERTEX_POINT('',#50260);
#2078=VERTEX_POINT('',#50490);
#2079=VERTEX_POINT('',#50720);
#2080=VERTEX_POINT('',#50947);
#2081=VERTEX_POINT('',#51177);
#2082=VERTEX_POINT('',#51407);
#2083=VERTEX_POINT('',#51634);
#2084=VERTEX_POINT('',#51864);
#2085=VERTEX_POINT('',#52097);
#2086=VERTEX_POINT('',#52327);
#2087=VERTEX_POINT('',#52557);
#2088=VERTEX_POINT('',#52787);
#2089=VERTEX_POINT('',#53014);
#2090=VERTEX_POINT('',#53241);
#2091=VERTEX_POINT('',#53471);
#2092=VERTEX_POINT('',#53701);
#2093=VERTEX_POINT('',#53928);
#2094=VERTEX_POINT('',#54158);
#2095=VERTEX_POINT('',#54388);
#2096=VERTEX_POINT('',#54399);
#2097=VERTEX_POINT('',#54626);
#2098=VERTEX_POINT('',#54856);
#2099=VERTEX_POINT('',#55086);
#2100=VERTEX_POINT('',#55313);
#2101=VERTEX_POINT('',#55543);
#2102=VERTEX_POINT('',#55773);
#2103=VERTEX_POINT('',#56003);
#2104=VERTEX_POINT('',#56015);
#2105=VERTEX_POINT('',#56245);
#2106=VERTEX_POINT('',#56475);
#2107=VERTEX_POINT('',#56702);
#2108=VERTEX_POINT('',#56932);
#2109=VERTEX_POINT('',#57162);
#2110=VERTEX_POINT('',#57389);
#2111=VERTEX_POINT('',#57619);
#2112=VERTEX_POINT('',#57849);
#2113=VERTEX_POINT('',#58079);
#2114=VERTEX_POINT('',#58306);
#2115=VERTEX_POINT('',#58536);
#2116=VERTEX_POINT('',#58766);
#2117=VERTEX_POINT('',#58996);
#2118=VERTEX_POINT('',#59007);
#2119=VERTEX_POINT('',#59237);
#2120=VERTEX_POINT('',#59467);
#2121=VERTEX_POINT('',#59694);
#2122=VERTEX_POINT('',#59924);
#2123=VERTEX_POINT('',#60154);
#2124=VERTEX_POINT('',#60384);
#2125=VERTEX_POINT('',#60614);
#2126=VERTEX_POINT('',#60625);
#2127=VERTEX_POINT('',#60852);
#2128=VERTEX_POINT('',#61079);
#2129=VERTEX_POINT('',#61309);
#2130=VERTEX_POINT('',#61539);
#2131=VERTEX_POINT('',#61766);
#2132=VERTEX_POINT('',#61993);
#2133=VERTEX_POINT('',#62223);
#2134=VERTEX_POINT('',#62453);
#2135=VERTEX_POINT('',#62683);
#2136=VERTEX_POINT('',#62913);
#2137=VERTEX_POINT('',#63143);
#2138=VERTEX_POINT('',#63370);
#2139=VERTEX_POINT('',#63600);
#2140=VERTEX_POINT('',#63833);
#2141=VERTEX_POINT('',#64063);
#2142=VERTEX_POINT('',#64293);
#2143=VERTEX_POINT('',#64523);
#2144=VERTEX_POINT('',#64753);
#2145=VERTEX_POINT('',#64980);
#2146=VERTEX_POINT('',#65210);
#2147=VERTEX_POINT('',#65440);
#2148=VERTEX_POINT('',#65452);
#2149=VERTEX_POINT('',#65463);
#2150=VERTEX_POINT('',#65693);
#2151=VERTEX_POINT('',#65923);
#2152=VERTEX_POINT('',#66150);
#2153=VERTEX_POINT('',#66380);
#2154=VERTEX_POINT('',#66610);
#2155=VERTEX_POINT('',#66840);
#2156=VERTEX_POINT('',#67070);
#2157=VERTEX_POINT('',#67303);
#2158=VERTEX_POINT('',#67533);
#2159=VERTEX_POINT('',#67760);
#2160=VERTEX_POINT('',#67990);
#2161=VERTEX_POINT('',#68220);
#2162=VERTEX_POINT('',#68450);
#2163=VERTEX_POINT('',#68910);
#2164=VERTEX_POINT('',#68912);
#2165=VERTEX_POINT('',#68913);
#2166=VERTEX_POINT('',#68915);
#2167=VERTEX_POINT('',#68917);
#2168=VERTEX_POINT('',#68919);
#2169=VERTEX_POINT('',#68921);
#2170=VERTEX_POINT('',#68925);
#2171=VERTEX_POINT('',#68929);
#2172=VERTEX_POINT('',#68931);
#2173=VERTEX_POINT('',#68935);
#2174=VERTEX_POINT('',#68939);
#2175=VERTEX_POINT('',#68943);
#2176=VERTEX_POINT('',#68958);
#2177=VERTEX_POINT('',#68999);
#2178=VERTEX_POINT('',#69038);
#2179=VERTEX_POINT('',#69042);
#2180=EDGE_CURVE('',#1522,#1522,#1412,.T.);
#2181=EDGE_CURVE('',#1522,#1523,#1018,.T.);
#2182=EDGE_CURVE('',#1523,#1523,#1413,.T.);
#2183=EDGE_CURVE('',#1524,#1524,#1414,.T.);
#2184=EDGE_CURVE('',#1524,#1525,#1019,.T.);
#2185=EDGE_CURVE('',#1525,#1525,#1415,.T.);
#2186=EDGE_CURVE('',#1526,#1526,#1416,.T.);
#2187=EDGE_CURVE('',#1526,#1527,#1020,.T.);
#2188=EDGE_CURVE('',#1527,#1527,#1417,.T.);
#2189=EDGE_CURVE('',#1528,#1528,#1418,.T.);
#2190=EDGE_CURVE('',#1528,#1529,#1021,.T.);
#2191=EDGE_CURVE('',#1529,#1529,#1419,.T.);
#2192=EDGE_CURVE('',#1530,#1531,#1022,.T.);
#2193=EDGE_CURVE('',#1531,#1532,#1023,.T.);
#2194=EDGE_CURVE('',#1532,#1533,#1024,.T.);
#2195=EDGE_CURVE('',#1533,#1530,#1025,.T.);
#2196=EDGE_CURVE('',#1532,#1534,#1026,.T.);
#2197=EDGE_CURVE('',#1534,#1535,#1027,.T.);
#2198=EDGE_CURVE('',#1535,#1533,#1028,.T.);
#2199=EDGE_CURVE('',#1534,#1536,#1420,.T.);
#2200=EDGE_CURVE('',#1536,#1537,#1029,.T.);
#2201=EDGE_CURVE('',#1537,#1535,#1421,.T.);
#2202=EDGE_CURVE('',#1536,#1538,#1030,.T.);
#2203=EDGE_CURVE('',#1538,#1539,#1031,.T.);
#2204=EDGE_CURVE('',#1539,#1537,#1032,.T.);
#2205=EDGE_CURVE('',#1538,#1540,#1422,.T.);
#2206=EDGE_CURVE('',#1540,#1541,#1033,.T.);
#2207=EDGE_CURVE('',#1541,#1539,#1423,.T.);
#2208=EDGE_CURVE('',#1542,#1543,#1034,.T.);
#2209=EDGE_CURVE('',#1542,#1544,#1424,.T.);
#2210=EDGE_CURVE('',#1544,#1545,#1035,.T.);
#2211=EDGE_CURVE('',#1545,#1543,#1425,.T.);
#2212=EDGE_CURVE('',#1544,#1546,#1036,.T.);
#2213=EDGE_CURVE('',#1546,#1547,#1037,.T.);
#2214=EDGE_CURVE('',#1547,#1545,#1038,.T.);
#2215=EDGE_CURVE('',#1546,#1548,#1426,.T.);
#2216=EDGE_CURVE('',#1548,#1549,#1039,.T.);
#2217=EDGE_CURVE('',#1549,#1547,#1427,.T.);
#2218=EDGE_CURVE('',#1548,#1531,#1040,.T.);
#2219=EDGE_CURVE('',#1530,#1549,#1041,.T.);
#2220=EDGE_CURVE('',#1550,#1551,#1042,.T.);
#2221=EDGE_CURVE('',#1551,#1552,#1043,.T.);
#2222=EDGE_CURVE('',#1552,#1553,#1044,.T.);
#2223=EDGE_CURVE('',#1553,#1554,#1428,.T.);
#2224=EDGE_CURVE('',#1554,#1555,#1045,.T.);
#2225=EDGE_CURVE('',#1555,#1556,#1429,.T.);
#2226=EDGE_CURVE('',#1556,#1540,#1046,.T.);
#2227=EDGE_CURVE('',#1557,#1542,#1047,.T.);
#2228=EDGE_CURVE('',#1557,#1558,#1430,.T.);
#2229=EDGE_CURVE('',#1558,#1559,#1048,.T.);
#2230=EDGE_CURVE('',#1559,#1550,#1431,.T.);
#2231=EDGE_CURVE('',#1560,#1551,#1049,.T.);
#2232=EDGE_CURVE('',#1561,#1560,#1050,.T.);
#2233=EDGE_CURVE('',#1552,#1561,#1051,.T.);
#2234=EDGE_CURVE('',#1562,#1561,#1052,.T.);
#2235=EDGE_CURVE('',#1553,#1562,#1053,.T.);
#2236=EDGE_CURVE('',#1563,#1562,#1432,.T.);
#2237=EDGE_CURVE('',#1554,#1563,#1054,.T.);
#2238=EDGE_CURVE('',#1564,#1563,#1055,.T.);
#2239=EDGE_CURVE('',#1555,#1564,#1056,.T.);
#2240=EDGE_CURVE('',#1565,#1564,#1433,.T.);
#2241=EDGE_CURVE('',#1556,#1565,#1057,.T.);
#2242=EDGE_CURVE('',#1565,#1541,#1058,.T.);
#2243=EDGE_CURVE('',#1566,#1543,#1059,.T.);
#2244=EDGE_CURVE('',#1557,#1566,#1060,.T.);
#2245=EDGE_CURVE('',#1567,#1566,#1434,.T.);
#2246=EDGE_CURVE('',#1558,#1567,#1061,.T.);
#2247=EDGE_CURVE('',#1568,#1567,#1062,.T.);
#2248=EDGE_CURVE('',#1559,#1568,#1063,.T.);
#2249=EDGE_CURVE('',#1569,#1568,#1435,.T.);
#2250=EDGE_CURVE('',#1550,#1569,#1064,.T.);
#2251=EDGE_CURVE('',#1560,#1569,#1065,.T.);
#2252=EDGE_CURVE('',#1570,#1570,#1436,.T.);
#2253=EDGE_CURVE('',#1570,#1571,#1066,.T.);
#2254=EDGE_CURVE('',#1571,#1571,#1437,.T.);
#2255=EDGE_CURVE('',#1572,#1572,#1438,.T.);
#2256=EDGE_CURVE('',#1572,#1573,#1067,.T.);
#2257=EDGE_CURVE('',#1573,#1573,#1439,.T.);
#2258=EDGE_CURVE('',#1574,#1574,#1440,.T.);
#2259=EDGE_CURVE('',#1574,#1575,#1068,.T.);
#2260=EDGE_CURVE('',#1575,#1575,#1441,.T.);
#2261=EDGE_CURVE('',#1576,#1576,#1442,.T.);
#2262=EDGE_CURVE('',#1576,#1577,#1069,.T.);
#2263=EDGE_CURVE('',#1577,#1577,#1443,.T.);
#2264=EDGE_CURVE('',#1578,#1578,#1444,.T.);
#2265=EDGE_CURVE('',#1578,#1579,#1070,.T.);
#2266=EDGE_CURVE('',#1579,#1579,#1445,.T.);
#2267=EDGE_CURVE('',#1580,#1581,#1446,.T.);
#2268=EDGE_CURVE('',#1581,#1582,#1071,.T.);
#2269=EDGE_CURVE('',#1583,#1582,#1447,.T.);
#2270=EDGE_CURVE('',#1580,#1583,#1072,.T.);
#2271=EDGE_CURVE('',#1584,#1580,#1073,.T.);
#2272=EDGE_CURVE('',#1585,#1583,#1074,.T.);
#2273=EDGE_CURVE('',#1584,#1585,#1075,.T.);
#2274=EDGE_CURVE('',#1586,#1584,#1448,.T.);
#2275=EDGE_CURVE('',#1587,#1585,#1449,.T.);
#2276=EDGE_CURVE('',#1586,#1587,#1076,.T.);
#2277=EDGE_CURVE('',#1588,#1589,#1077,.T.);
#2278=EDGE_CURVE('',#1589,#1587,#1078,.T.);
#2279=EDGE_CURVE('',#1582,#1590,#1079,.T.);
#2280=EDGE_CURVE('',#1590,#1591,#1080,.T.);
#2281=EDGE_CURVE('',#1591,#1588,#1081,.T.);
#2282=EDGE_CURVE('',#1581,#1586,#1082,.T.);
#2283=EDGE_CURVE('',#1592,#1592,#1450,.T.);
#2284=EDGE_CURVE('',#1593,#1593,#1451,.T.);
#2285=EDGE_CURVE('',#1593,#1592,#1083,.T.);
#2286=EDGE_CURVE('',#1594,#1595,#1084,.T.);
#2287=EDGE_CURVE('',#1594,#1589,#1085,.T.);
#2288=EDGE_CURVE('',#1595,#1588,#1086,.T.);
#2289=EDGE_CURVE('',#1595,#1596,#1087,.T.);
#2290=EDGE_CURVE('',#1596,#1591,#1088,.T.);
#2291=EDGE_CURVE('',#1596,#1597,#1089,.T.);
#2292=EDGE_CURVE('',#1597,#1590,#1090,.T.);
#2293=EDGE_CURVE('',#1598,#1598,#1452,.T.);
#2294=EDGE_CURVE('',#1598,#1599,#1091,.T.);
#2295=EDGE_CURVE('',#1599,#1599,#1453,.T.);
#2296=EDGE_CURVE('',#1600,#1601,#1092,.T.);
#2297=EDGE_CURVE('',#1600,#1602,#1093,.T.);
#2298=EDGE_CURVE('',#1602,#1597,#1094,.T.);
#2299=EDGE_CURVE('',#1594,#1603,#1095,.T.);
#2300=EDGE_CURVE('',#1601,#1603,#1096,.T.);
#2301=EDGE_CURVE('',#1604,#1600,#1454,.T.);
#2302=EDGE_CURVE('',#1604,#1605,#1097,.T.);
#2303=EDGE_CURVE('',#1605,#1602,#1455,.T.);
#2304=EDGE_CURVE('',#1606,#1604,#1098,.T.);
#2305=EDGE_CURVE('',#1606,#1607,#1099,.T.);
#2306=EDGE_CURVE('',#1607,#1605,#1100,.T.);
#2307=EDGE_CURVE('',#1601,#1606,#1456,.T.);
#2308=EDGE_CURVE('',#1603,#1607,#1457,.T.);
#2309=EDGE_CURVE('',#1608,#1608,#1458,.T.);
#2310=EDGE_CURVE('',#1609,#1609,#1459,.T.);
#2311=EDGE_CURVE('',#1609,#1608,#1101,.T.);
#2312=EDGE_CURVE('',#1610,#1610,#1460,.T.);
#2313=EDGE_CURVE('',#1610,#1611,#1102,.T.);
#2314=EDGE_CURVE('',#1611,#1611,#1461,.T.);
#2315=EDGE_CURVE('',#1612,#1612,#1462,.T.);
#2316=EDGE_CURVE('',#1612,#1613,#1103,.T.);
#2317=EDGE_CURVE('',#1613,#1613,#1463,.T.);
#2318=EDGE_CURVE('',#1614,#1615,#1104,.T.);
#2319=EDGE_CURVE('',#1614,#1616,#1105,.T.);
#2320=EDGE_CURVE('',#1616,#1617,#1106,.T.);
#2321=EDGE_CURVE('',#1615,#1617,#1107,.T.);
#2322=EDGE_CURVE('',#1618,#1614,#1464,.T.);
#2323=EDGE_CURVE('',#1618,#1619,#1108,.T.);
#2324=EDGE_CURVE('',#1619,#1616,#1465,.T.);
#2325=EDGE_CURVE('',#1620,#1618,#1109,.T.);
#2326=EDGE_CURVE('',#1620,#1621,#1110,.T.);
#2327=EDGE_CURVE('',#1621,#1619,#1111,.T.);
#2328=EDGE_CURVE('',#1615,#1620,#1466,.T.);
#2329=EDGE_CURVE('',#1617,#1621,#1467,.T.);
#2330=EDGE_CURVE('',#1622,#1622,#1468,.T.);
#2331=EDGE_CURVE('',#1623,#1623,#1469,.T.);
#2332=EDGE_CURVE('',#1624,#1624,#1470,.T.);
#2333=EDGE_CURVE('',#1624,#1623,#1112,.T.);
#2334=EDGE_CURVE('',#1625,#1625,#1471,.T.);
#2335=EDGE_CURVE('',#1622,#1625,#1113,.T.);
#2336=EDGE_CURVE('',#1626,#1626,#1472,.T.);
#2337=EDGE_CURVE('',#1626,#1627,#1114,.T.);
#2338=EDGE_CURVE('',#1627,#1627,#1473,.T.);
#2339=EDGE_CURVE('',#1628,#1629,#55,.T.);
#2340=EDGE_CURVE('',#1629,#1628,#56,.T.);
#2341=EDGE_CURVE('',#1629,#1630,#1115,.T.);
#2342=EDGE_CURVE('',#1631,#1630,#57,.T.);
#2343=EDGE_CURVE('',#1632,#1631,#58,.T.);
#2344=EDGE_CURVE('',#1630,#1632,#59,.T.);
#2345=EDGE_CURVE('',#1633,#1633,#1474,.T.);
#2346=EDGE_CURVE('',#1633,#1634,#1116,.T.);
#2347=EDGE_CURVE('',#1634,#1634,#1475,.T.);
#2348=EDGE_CURVE('',#1635,#1636,#1117,.T.);
#2349=EDGE_CURVE('',#1636,#1637,#1118,.T.);
#2350=EDGE_CURVE('',#1638,#1637,#1119,.T.);
#2351=EDGE_CURVE('',#1635,#1638,#1120,.T.);
#2352=EDGE_CURVE('',#1639,#1635,#1476,.T.);
#2353=EDGE_CURVE('',#1640,#1638,#1477,.T.);
#2354=EDGE_CURVE('',#1639,#1640,#1121,.T.);
#2355=EDGE_CURVE('',#1641,#1639,#1122,.T.);
#2356=EDGE_CURVE('',#1642,#1640,#1123,.T.);
#2357=EDGE_CURVE('',#1641,#1642,#1124,.T.);
#2358=EDGE_CURVE('',#1636,#1641,#1478,.T.);
#2359=EDGE_CURVE('',#1637,#1642,#1479,.T.);
#2360=EDGE_CURVE('',#1643,#1643,#1480,.T.);
#2361=EDGE_CURVE('',#1644,#1644,#1481,.T.);
#2362=EDGE_CURVE('',#1645,#1645,#1482,.T.);
#2363=EDGE_CURVE('',#1645,#1644,#1125,.T.);
#2364=EDGE_CURVE('',#1643,#1630,#1126,.T.);
#2365=EDGE_CURVE('',#1631,#1646,#1127,.T.);
#2366=EDGE_CURVE('',#1646,#1646,#1483,.T.);
#2367=EDGE_CURVE('',#1647,#1647,#1484,.T.);
#2368=EDGE_CURVE('',#1647,#1648,#1128,.T.);
#2369=EDGE_CURVE('',#1648,#1648,#1485,.T.);
#2370=EDGE_CURVE('',#1649,#1649,#1486,.T.);
#2371=EDGE_CURVE('',#1649,#1650,#1129,.T.);
#2372=EDGE_CURVE('',#1650,#1650,#1487,.T.);
#2373=EDGE_CURVE('',#1651,#1651,#1488,.T.);
#2374=EDGE_CURVE('',#1651,#1652,#1130,.T.);
#2375=EDGE_CURVE('',#1652,#1652,#1489,.T.);
#2376=EDGE_CURVE('',#1653,#1653,#1490,.T.);
#2377=EDGE_CURVE('',#1653,#1654,#1131,.T.);
#2378=EDGE_CURVE('',#1654,#1654,#1491,.T.);
#2379=EDGE_CURVE('',#1655,#1656,#1132,.T.);
#2380=EDGE_CURVE('',#1656,#1657,#1133,.T.);
#2381=EDGE_CURVE('',#1657,#1658,#1134,.T.);
#2382=EDGE_CURVE('',#1658,#1655,#1135,.T.);
#2383=EDGE_CURVE('',#1657,#1659,#1136,.T.);
#2384=EDGE_CURVE('',#1659,#1660,#1137,.T.);
#2385=EDGE_CURVE('',#1660,#1658,#1138,.T.);
#2386=EDGE_CURVE('',#1659,#1661,#1492,.T.);
#2387=EDGE_CURVE('',#1661,#1662,#1139,.T.);
#2388=EDGE_CURVE('',#1662,#1660,#1493,.T.);
#2389=EDGE_CURVE('',#1661,#1663,#1140,.T.);
#2390=EDGE_CURVE('',#1663,#1664,#1141,.T.);
#2391=EDGE_CURVE('',#1664,#1662,#1142,.T.);
#2392=EDGE_CURVE('',#1663,#1665,#1494,.T.);
#2393=EDGE_CURVE('',#1665,#1666,#1143,.T.);
#2394=EDGE_CURVE('',#1666,#1664,#1495,.T.);
#2395=EDGE_CURVE('',#1667,#1668,#1144,.T.);
#2396=EDGE_CURVE('',#1667,#1669,#1496,.T.);
#2397=EDGE_CURVE('',#1669,#1670,#1145,.T.);
#2398=EDGE_CURVE('',#1670,#1668,#1497,.T.);
#2399=EDGE_CURVE('',#1669,#1671,#1146,.T.);
#2400=EDGE_CURVE('',#1671,#1672,#1147,.T.);
#2401=EDGE_CURVE('',#1672,#1670,#1148,.T.);
#2402=EDGE_CURVE('',#1671,#1673,#1498,.T.);
#2403=EDGE_CURVE('',#1673,#1674,#1149,.T.);
#2404=EDGE_CURVE('',#1674,#1672,#1499,.T.);
#2405=EDGE_CURVE('',#1673,#1656,#1150,.T.);
#2406=EDGE_CURVE('',#1655,#1674,#1151,.T.);
#2407=EDGE_CURVE('',#1675,#1676,#1152,.T.);
#2408=EDGE_CURVE('',#1676,#1677,#1153,.T.);
#2409=EDGE_CURVE('',#1677,#1678,#1154,.T.);
#2410=EDGE_CURVE('',#1678,#1679,#1500,.T.);
#2411=EDGE_CURVE('',#1679,#1680,#1155,.T.);
#2412=EDGE_CURVE('',#1680,#1681,#1501,.T.);
#2413=EDGE_CURVE('',#1681,#1665,#1156,.T.);
#2414=EDGE_CURVE('',#1682,#1667,#1157,.T.);
#2415=EDGE_CURVE('',#1682,#1683,#1502,.T.);
#2416=EDGE_CURVE('',#1683,#1684,#1158,.T.);
#2417=EDGE_CURVE('',#1684,#1675,#1503,.T.);
#2418=EDGE_CURVE('',#1685,#1676,#1159,.T.);
#2419=EDGE_CURVE('',#1686,#1685,#1160,.T.);
#2420=EDGE_CURVE('',#1677,#1686,#1161,.T.);
#2421=EDGE_CURVE('',#1687,#1686,#1162,.T.);
#2422=EDGE_CURVE('',#1678,#1687,#1163,.T.);
#2423=EDGE_CURVE('',#1688,#1687,#1504,.T.);
#2424=EDGE_CURVE('',#1679,#1688,#1164,.T.);
#2425=EDGE_CURVE('',#1689,#1688,#1165,.T.);
#2426=EDGE_CURVE('',#1680,#1689,#1166,.T.);
#2427=EDGE_CURVE('',#1690,#1689,#1505,.T.);
#2428=EDGE_CURVE('',#1681,#1690,#1167,.T.);
#2429=EDGE_CURVE('',#1690,#1666,#1168,.T.);
#2430=EDGE_CURVE('',#1691,#1668,#1169,.T.);
#2431=EDGE_CURVE('',#1682,#1691,#1170,.T.);
#2432=EDGE_CURVE('',#1692,#1691,#1506,.T.);
#2433=EDGE_CURVE('',#1683,#1692,#1171,.T.);
#2434=EDGE_CURVE('',#1693,#1692,#1172,.T.);
#2435=EDGE_CURVE('',#1684,#1693,#1173,.T.);
#2436=EDGE_CURVE('',#1694,#1693,#1507,.T.);
#2437=EDGE_CURVE('',#1675,#1694,#1174,.T.);
#2438=EDGE_CURVE('',#1685,#1694,#1175,.T.);
#2439=EDGE_CURVE('',#1695,#1696,#1176,.T.);
#2440=EDGE_CURVE('',#1696,#1697,#60,.T.);
#2441=EDGE_CURVE('',#1698,#1697,#61,.T.);
#2442=EDGE_CURVE('',#1695,#1698,#62,.F.);
#2443=EDGE_CURVE('',#1699,#1700,#1177,.T.);
#2444=EDGE_CURVE('',#1701,#1699,#63,.F.);
#2445=EDGE_CURVE('',#1702,#1701,#64,.T.);
#2446=EDGE_CURVE('',#1703,#1702,#1508,.T.);
#2447=EDGE_CURVE('',#1703,#1700,#65,.T.);
#2448=EDGE_CURVE('',#1704,#1705,#1178,.T.);
#2449=EDGE_CURVE('',#1704,#1706,#66,.F.);
#2450=EDGE_CURVE('',#1707,#1706,#1509,.T.);
#2451=EDGE_CURVE('',#1707,#1705,#67,.T.);
#2452=EDGE_CURVE('',#1705,#1708,#68,.T.);
#2453=EDGE_CURVE('',#1709,#1708,#69,.T.);
#2454=EDGE_CURVE('',#1709,#1704,#70,.F.);
#2455=EDGE_CURVE('',#1700,#1710,#71,.T.);
#2456=EDGE_CURVE('',#1710,#1696,#72,.T.);
#2457=EDGE_CURVE('',#1699,#1695,#73,.F.);
#2458=EDGE_CURVE('',#1711,#1712,#1179,.T.);
#2459=EDGE_CURVE('',#1711,#1713,#1510,.T.);
#2460=EDGE_CURVE('',#1713,#1712,#74,.T.);
#2461=EDGE_CURVE('',#1714,#1698,#75,.T.);
#2462=EDGE_CURVE('',#1714,#1715,#76,.T.);
#2463=EDGE_CURVE('',#1708,#1715,#77,.T.);
#2464=EDGE_CURVE('',#1702,#1707,#78,.T.);
#2465=EDGE_CURVE('',#1715,#1716,#79,.T.);
#2466=EDGE_CURVE('',#1717,#1714,#80,.T.);
#2467=EDGE_CURVE('',#1717,#1716,#81,.T.);
#2468=EDGE_CURVE('',#1718,#1711,#47,.T.);
#2469=EDGE_CURVE('',#1719,#1718,#82,.T.);
#2470=EDGE_CURVE('',#1720,#1719,#83,.T.);
#2471=EDGE_CURVE('',#1720,#1713,#84,.T.);
#2472=EDGE_CURVE('',#1697,#1721,#85,.T.);
#2473=EDGE_CURVE('',#1706,#1703,#86,.T.);
#2474=EDGE_CURVE('',#1722,#1709,#87,.T.);
#2475=EDGE_CURVE('',#1721,#1722,#88,.T.);
#2476=EDGE_CURVE('',#1716,#1723,#89,.T.);
#2477=EDGE_CURVE('',#1724,#1717,#90,.T.);
#2478=EDGE_CURVE('',#1723,#1724,#91,.T.);
#2479=EDGE_CURVE('',#1712,#1720,#92,.T.);
#2480=EDGE_CURVE('',#1725,#1718,#93,.T.);
#2481=EDGE_CURVE('',#1726,#1725,#94,.T.);
#2482=EDGE_CURVE('',#1719,#1726,#95,.T.);
#2483=EDGE_CURVE('',#1727,#1727,#1511,.T.);
#2484=EDGE_CURVE('',#1727,#1728,#1180,.T.);
#2485=EDGE_CURVE('',#1728,#1729,#96,.T.);
#2486=EDGE_CURVE('',#1729,#1730,#97,.T.);
#2487=EDGE_CURVE('',#1730,#1731,#1181,.T.);
#2488=EDGE_CURVE('',#1731,#1731,#1512,.T.);
#2489=EDGE_CURVE('',#1730,#1728,#98,.T.);
#2490=EDGE_CURVE('',#1726,#1722,#99,.T.);
#2491=EDGE_CURVE('',#1723,#1724,#100,.T.);
#2492=EDGE_CURVE('',#1721,#1725,#101,.T.);
#2493=EDGE_CURVE('',#1728,#1732,#1182,.T.);
#2494=EDGE_CURVE('',#1732,#1732,#1513,.T.);
#2495=EDGE_CURVE('',#1733,#1734,#1183,.T.);
#2496=EDGE_CURVE('',#1734,#1735,#1184,.T.);
#2497=EDGE_CURVE('',#1735,#1736,#1185,.T.);
#2498=EDGE_CURVE('',#1736,#1733,#1186,.T.);
#2499=EDGE_CURVE('',#1737,#1734,#1187,.T.);
#2500=EDGE_CURVE('',#1738,#1737,#1188,.T.);
#2501=EDGE_CURVE('',#1735,#1738,#1189,.T.);
#2502=EDGE_CURVE('',#1739,#1738,#1190,.T.);
#2503=EDGE_CURVE('',#1736,#1739,#1191,.T.);
#2504=EDGE_CURVE('',#1740,#1739,#1192,.T.);
#2505=EDGE_CURVE('',#1733,#1740,#1193,.T.);
#2506=EDGE_CURVE('',#1737,#1740,#1194,.T.);
#2507=EDGE_CURVE('',#1741,#1741,#1514,.T.);
#2508=EDGE_CURVE('',#1742,#1742,#1515,.T.);
#2509=EDGE_CURVE('',#1742,#1741,#1195,.T.);
#2510=EDGE_CURVE('',#1743,#1744,#102,.T.);
#2511=EDGE_CURVE('',#1745,#1744,#1516,.F.);
#2512=EDGE_CURVE('',#1745,#1746,#103,.T.);
#2513=EDGE_CURVE('',#1746,#1747,#104,.T.);
#2514=EDGE_CURVE('',#1747,#1748,#105,.T.);
#2515=EDGE_CURVE('',#1748,#1749,#106,.T.);
#2516=EDGE_CURVE('',#1749,#1750,#107,.T.);
#2517=EDGE_CURVE('',#1750,#1751,#108,.T.);
#2518=EDGE_CURVE('',#1751,#1752,#109,.T.);
#2519=EDGE_CURVE('',#1752,#1753,#110,.T.);
#2520=EDGE_CURVE('',#1753,#1754,#111,.T.);
#2521=EDGE_CURVE('',#1754,#1755,#112,.T.);
#2522=EDGE_CURVE('',#1755,#1756,#113,.T.);
#2523=EDGE_CURVE('',#1756,#1757,#114,.T.);
#2524=EDGE_CURVE('',#1757,#1758,#115,.T.);
#2525=EDGE_CURVE('',#1758,#1759,#116,.T.);
#2526=EDGE_CURVE('',#1759,#1760,#117,.T.);
#2527=EDGE_CURVE('',#1760,#1761,#118,.T.);
#2528=EDGE_CURVE('',#1761,#1762,#119,.T.);
#2529=EDGE_CURVE('',#1762,#1763,#120,.T.);
#2530=EDGE_CURVE('',#1763,#1764,#121,.T.);
#2531=EDGE_CURVE('',#1764,#1765,#122,.T.);
#2532=EDGE_CURVE('',#1765,#1766,#123,.T.);
#2533=EDGE_CURVE('',#1766,#1767,#124,.T.);
#2534=EDGE_CURVE('',#1767,#1768,#125,.T.);
#2535=EDGE_CURVE('',#1768,#1769,#126,.T.);
#2536=EDGE_CURVE('',#1769,#1770,#127,.T.);
#2537=EDGE_CURVE('',#1770,#1771,#128,.T.);
#2538=EDGE_CURVE('',#1771,#1772,#129,.T.);
#2539=EDGE_CURVE('',#1772,#1773,#130,.T.);
#2540=EDGE_CURVE('',#1773,#1774,#131,.T.);
#2541=EDGE_CURVE('',#1774,#1775,#132,.T.);
#2542=EDGE_CURVE('',#1775,#1776,#133,.T.);
#2543=EDGE_CURVE('',#1776,#1777,#134,.T.);
#2544=EDGE_CURVE('',#1777,#1778,#135,.T.);
#2545=EDGE_CURVE('',#1778,#1779,#136,.T.);
#2546=EDGE_CURVE('',#1779,#1780,#137,.T.);
#2547=EDGE_CURVE('',#1780,#1781,#138,.T.);
#2548=EDGE_CURVE('',#1781,#1782,#139,.T.);
#2549=EDGE_CURVE('',#1782,#1783,#140,.T.);
#2550=EDGE_CURVE('',#1783,#1784,#141,.T.);
#2551=EDGE_CURVE('',#1784,#1785,#142,.T.);
#2552=EDGE_CURVE('',#1785,#1786,#143,.T.);
#2553=EDGE_CURVE('',#1786,#1787,#144,.T.);
#2554=EDGE_CURVE('',#1787,#1788,#145,.T.);
#2555=EDGE_CURVE('',#1788,#1789,#146,.T.);
#2556=EDGE_CURVE('',#1789,#1790,#147,.T.);
#2557=EDGE_CURVE('',#1790,#1791,#148,.T.);
#2558=EDGE_CURVE('',#1791,#1792,#149,.T.);
#2559=EDGE_CURVE('',#1792,#1793,#150,.T.);
#2560=EDGE_CURVE('',#1793,#1794,#151,.T.);
#2561=EDGE_CURVE('',#1794,#1795,#152,.T.);
#2562=EDGE_CURVE('',#1795,#1796,#153,.T.);
#2563=EDGE_CURVE('',#1796,#1797,#154,.T.);
#2564=EDGE_CURVE('',#1797,#1798,#155,.T.);
#2565=EDGE_CURVE('',#1798,#1799,#156,.T.);
#2566=EDGE_CURVE('',#1799,#1800,#157,.T.);
#2567=EDGE_CURVE('',#1800,#1801,#158,.T.);
#2568=EDGE_CURVE('',#1801,#1802,#159,.T.);
#2569=EDGE_CURVE('',#1802,#1803,#160,.T.);
#2570=EDGE_CURVE('',#1803,#1804,#161,.T.);
#2571=EDGE_CURVE('',#1804,#1805,#162,.T.);
#2572=EDGE_CURVE('',#1805,#1806,#163,.T.);
#2573=EDGE_CURVE('',#1806,#1807,#164,.T.);
#2574=EDGE_CURVE('',#1807,#1808,#165,.T.);
#2575=EDGE_CURVE('',#1808,#1809,#166,.T.);
#2576=EDGE_CURVE('',#1809,#1810,#167,.T.);
#2577=EDGE_CURVE('',#1810,#1811,#168,.T.);
#2578=EDGE_CURVE('',#1811,#1812,#169,.T.);
#2579=EDGE_CURVE('',#1812,#1813,#170,.T.);
#2580=EDGE_CURVE('',#1813,#1814,#171,.T.);
#2581=EDGE_CURVE('',#1814,#1815,#172,.T.);
#2582=EDGE_CURVE('',#1815,#1816,#173,.T.);
#2583=EDGE_CURVE('',#1816,#1817,#174,.T.);
#2584=EDGE_CURVE('',#1817,#1818,#175,.T.);
#2585=EDGE_CURVE('',#1818,#1819,#176,.T.);
#2586=EDGE_CURVE('',#1819,#1820,#177,.T.);
#2587=EDGE_CURVE('',#1820,#1821,#178,.T.);
#2588=EDGE_CURVE('',#1821,#1822,#179,.T.);
#2589=EDGE_CURVE('',#1822,#1823,#180,.T.);
#2590=EDGE_CURVE('',#1823,#1824,#181,.T.);
#2591=EDGE_CURVE('',#1824,#1825,#182,.T.);
#2592=EDGE_CURVE('',#1825,#1826,#183,.T.);
#2593=EDGE_CURVE('',#1826,#1827,#184,.T.);
#2594=EDGE_CURVE('',#1827,#1828,#185,.T.);
#2595=EDGE_CURVE('',#1828,#1829,#186,.T.);
#2596=EDGE_CURVE('',#1829,#1830,#187,.T.);
#2597=EDGE_CURVE('',#1830,#1831,#188,.T.);
#2598=EDGE_CURVE('',#1831,#1832,#189,.T.);
#2599=EDGE_CURVE('',#1832,#1833,#190,.T.);
#2600=EDGE_CURVE('',#1833,#1834,#191,.T.);
#2601=EDGE_CURVE('',#1834,#1835,#192,.T.);
#2602=EDGE_CURVE('',#1835,#1836,#193,.T.);
#2603=EDGE_CURVE('',#1836,#1837,#194,.T.);
#2604=EDGE_CURVE('',#1837,#1838,#195,.T.);
#2605=EDGE_CURVE('',#1838,#1839,#196,.T.);
#2606=EDGE_CURVE('',#1839,#1840,#197,.T.);
#2607=EDGE_CURVE('',#1840,#1841,#198,.T.);
#2608=EDGE_CURVE('',#1841,#1842,#199,.T.);
#2609=EDGE_CURVE('',#1842,#1843,#200,.T.);
#2610=EDGE_CURVE('',#1843,#1844,#201,.T.);
#2611=EDGE_CURVE('',#1844,#1845,#202,.T.);
#2612=EDGE_CURVE('',#1845,#1846,#203,.T.);
#2613=EDGE_CURVE('',#1846,#1847,#204,.T.);
#2614=EDGE_CURVE('',#1847,#1848,#205,.T.);
#2615=EDGE_CURVE('',#1848,#1849,#206,.T.);
#2616=EDGE_CURVE('',#1850,#1849,#1517,.T.);
#2617=EDGE_CURVE('',#1850,#1851,#207,.T.);
#2618=EDGE_CURVE('',#1851,#1852,#208,.T.);
#2619=EDGE_CURVE('',#1852,#1853,#209,.T.);
#2620=EDGE_CURVE('',#1853,#1854,#210,.T.);
#2621=EDGE_CURVE('',#1854,#1855,#211,.T.);
#2622=EDGE_CURVE('',#1855,#1856,#212,.T.);
#2623=EDGE_CURVE('',#1856,#1857,#213,.T.);
#2624=EDGE_CURVE('',#1857,#1858,#214,.T.);
#2625=EDGE_CURVE('',#1858,#1859,#215,.T.);
#2626=EDGE_CURVE('',#1859,#1860,#216,.T.);
#2627=EDGE_CURVE('',#1860,#1861,#217,.T.);
#2628=EDGE_CURVE('',#1861,#1862,#218,.T.);
#2629=EDGE_CURVE('',#1862,#1863,#219,.T.);
#2630=EDGE_CURVE('',#1863,#1864,#220,.T.);
#2631=EDGE_CURVE('',#1864,#1865,#221,.T.);
#2632=EDGE_CURVE('',#1865,#1866,#222,.T.);
#2633=EDGE_CURVE('',#1866,#1867,#223,.T.);
#2634=EDGE_CURVE('',#1867,#1868,#224,.T.);
#2635=EDGE_CURVE('',#1868,#1869,#225,.T.);
#2636=EDGE_CURVE('',#1869,#1870,#226,.T.);
#2637=EDGE_CURVE('',#1870,#1871,#227,.T.);
#2638=EDGE_CURVE('',#1871,#1872,#228,.T.);
#2639=EDGE_CURVE('',#1872,#1873,#229,.T.);
#2640=EDGE_CURVE('',#1873,#1874,#230,.T.);
#2641=EDGE_CURVE('',#1874,#1875,#231,.T.);
#2642=EDGE_CURVE('',#1875,#1876,#232,.T.);
#2643=EDGE_CURVE('',#1876,#1877,#233,.T.);
#2644=EDGE_CURVE('',#1877,#1878,#234,.T.);
#2645=EDGE_CURVE('',#1878,#1879,#235,.T.);
#2646=EDGE_CURVE('',#1879,#1880,#236,.T.);
#2647=EDGE_CURVE('',#1880,#1881,#237,.T.);
#2648=EDGE_CURVE('',#1881,#1882,#238,.T.);
#2649=EDGE_CURVE('',#1882,#1883,#239,.T.);
#2650=EDGE_CURVE('',#1883,#1884,#240,.T.);
#2651=EDGE_CURVE('',#1884,#1885,#241,.T.);
#2652=EDGE_CURVE('',#1885,#1886,#242,.T.);
#2653=EDGE_CURVE('',#1886,#1887,#243,.T.);
#2654=EDGE_CURVE('',#1887,#1888,#244,.T.);
#2655=EDGE_CURVE('',#1888,#1889,#245,.T.);
#2656=EDGE_CURVE('',#1889,#1890,#246,.T.);
#2657=EDGE_CURVE('',#1890,#1891,#247,.T.);
#2658=EDGE_CURVE('',#1891,#1892,#248,.T.);
#2659=EDGE_CURVE('',#1892,#1893,#249,.T.);
#2660=EDGE_CURVE('',#1893,#1894,#250,.T.);
#2661=EDGE_CURVE('',#1894,#1895,#251,.T.);
#2662=EDGE_CURVE('',#1895,#1896,#252,.T.);
#2663=EDGE_CURVE('',#1896,#1897,#253,.T.);
#2664=EDGE_CURVE('',#1897,#1898,#254,.T.);
#2665=EDGE_CURVE('',#1898,#1899,#255,.T.);
#2666=EDGE_CURVE('',#1899,#1900,#256,.T.);
#2667=EDGE_CURVE('',#1900,#1901,#257,.T.);
#2668=EDGE_CURVE('',#1901,#1902,#258,.T.);
#2669=EDGE_CURVE('',#1902,#1903,#259,.T.);
#2670=EDGE_CURVE('',#1903,#1904,#260,.T.);
#2671=EDGE_CURVE('',#1904,#1905,#261,.T.);
#2672=EDGE_CURVE('',#1905,#1906,#262,.T.);
#2673=EDGE_CURVE('',#1906,#1907,#263,.T.);
#2674=EDGE_CURVE('',#1907,#1908,#264,.T.);
#2675=EDGE_CURVE('',#1908,#1909,#265,.T.);
#2676=EDGE_CURVE('',#1909,#1910,#266,.T.);
#2677=EDGE_CURVE('',#1910,#1911,#267,.T.);
#2678=EDGE_CURVE('',#1911,#1912,#268,.T.);
#2679=EDGE_CURVE('',#1912,#1913,#269,.T.);
#2680=EDGE_CURVE('',#1913,#1914,#270,.T.);
#2681=EDGE_CURVE('',#1914,#1915,#271,.T.);
#2682=EDGE_CURVE('',#1915,#1916,#272,.T.);
#2683=EDGE_CURVE('',#1916,#1917,#273,.T.);
#2684=EDGE_CURVE('',#1917,#1918,#274,.T.);
#2685=EDGE_CURVE('',#1918,#1919,#275,.T.);
#2686=EDGE_CURVE('',#1919,#1920,#276,.T.);
#2687=EDGE_CURVE('',#1920,#1921,#277,.T.);
#2688=EDGE_CURVE('',#1921,#1922,#278,.T.);
#2689=EDGE_CURVE('',#1922,#1923,#279,.T.);
#2690=EDGE_CURVE('',#1923,#1924,#280,.T.);
#2691=EDGE_CURVE('',#1924,#1925,#281,.T.);
#2692=EDGE_CURVE('',#1925,#1926,#282,.T.);
#2693=EDGE_CURVE('',#1926,#1927,#283,.T.);
#2694=EDGE_CURVE('',#1927,#1928,#284,.T.);
#2695=EDGE_CURVE('',#1928,#1929,#285,.T.);
#2696=EDGE_CURVE('',#1929,#1930,#286,.T.);
#2697=EDGE_CURVE('',#1930,#1931,#287,.T.);
#2698=EDGE_CURVE('',#1931,#1932,#288,.T.);
#2699=EDGE_CURVE('',#1932,#1933,#289,.T.);
#2700=EDGE_CURVE('',#1933,#1934,#290,.T.);
#2701=EDGE_CURVE('',#1934,#1935,#291,.T.);
#2702=EDGE_CURVE('',#1935,#1936,#292,.T.);
#2703=EDGE_CURVE('',#1936,#1937,#293,.T.);
#2704=EDGE_CURVE('',#1937,#1938,#294,.T.);
#2705=EDGE_CURVE('',#1938,#1939,#295,.T.);
#2706=EDGE_CURVE('',#1939,#1940,#296,.T.);
#2707=EDGE_CURVE('',#1940,#1941,#297,.T.);
#2708=EDGE_CURVE('',#1941,#1942,#298,.T.);
#2709=EDGE_CURVE('',#1942,#1943,#299,.T.);
#2710=EDGE_CURVE('',#1943,#1944,#300,.T.);
#2711=EDGE_CURVE('',#1944,#1945,#301,.T.);
#2712=EDGE_CURVE('',#1945,#1946,#302,.T.);
#2713=EDGE_CURVE('',#1946,#1947,#303,.T.);
#2714=EDGE_CURVE('',#1947,#1948,#304,.T.);
#2715=EDGE_CURVE('',#1948,#1949,#305,.T.);
#2716=EDGE_CURVE('',#1949,#1950,#306,.T.);
#2717=EDGE_CURVE('',#1950,#1951,#307,.T.);
#2718=EDGE_CURVE('',#1951,#1952,#308,.T.);
#2719=EDGE_CURVE('',#1952,#1743,#309,.T.);
#2720=EDGE_CURVE('',#1953,#1954,#310,.T.);
#2721=EDGE_CURVE('',#1955,#1954,#1518,.T.);
#2722=EDGE_CURVE('',#1956,#1955,#311,.T.);
#2723=EDGE_CURVE('',#1957,#1956,#312,.T.);
#2724=EDGE_CURVE('',#1958,#1957,#313,.T.);
#2725=EDGE_CURVE('',#1959,#1958,#314,.T.);
#2726=EDGE_CURVE('',#1960,#1959,#315,.T.);
#2727=EDGE_CURVE('',#1961,#1960,#316,.T.);
#2728=EDGE_CURVE('',#1962,#1961,#317,.T.);
#2729=EDGE_CURVE('',#1963,#1962,#318,.T.);
#2730=EDGE_CURVE('',#1964,#1963,#319,.T.);
#2731=EDGE_CURVE('',#1965,#1964,#320,.T.);
#2732=EDGE_CURVE('',#1966,#1965,#321,.T.);
#2733=EDGE_CURVE('',#1967,#1966,#322,.T.);
#2734=EDGE_CURVE('',#1968,#1967,#323,.T.);
#2735=EDGE_CURVE('',#1969,#1968,#324,.T.);
#2736=EDGE_CURVE('',#1970,#1969,#325,.T.);
#2737=EDGE_CURVE('',#1971,#1970,#326,.T.);
#2738=EDGE_CURVE('',#1972,#1971,#327,.T.);
#2739=EDGE_CURVE('',#1973,#1972,#328,.T.);
#2740=EDGE_CURVE('',#1974,#1973,#329,.T.);
#2741=EDGE_CURVE('',#1975,#1974,#330,.T.);
#2742=EDGE_CURVE('',#1976,#1975,#331,.T.);
#2743=EDGE_CURVE('',#1977,#1976,#332,.T.);
#2744=EDGE_CURVE('',#1978,#1977,#333,.T.);
#2745=EDGE_CURVE('',#1979,#1978,#334,.T.);
#2746=EDGE_CURVE('',#1980,#1979,#335,.T.);
#2747=EDGE_CURVE('',#1981,#1980,#336,.T.);
#2748=EDGE_CURVE('',#1982,#1981,#337,.T.);
#2749=EDGE_CURVE('',#1983,#1982,#338,.T.);
#2750=EDGE_CURVE('',#1984,#1983,#339,.T.);
#2751=EDGE_CURVE('',#1985,#1984,#340,.T.);
#2752=EDGE_CURVE('',#1986,#1985,#341,.T.);
#2753=EDGE_CURVE('',#1987,#1986,#342,.T.);
#2754=EDGE_CURVE('',#1988,#1987,#343,.T.);
#2755=EDGE_CURVE('',#1989,#1988,#344,.T.);
#2756=EDGE_CURVE('',#1990,#1989,#345,.T.);
#2757=EDGE_CURVE('',#1991,#1990,#346,.T.);
#2758=EDGE_CURVE('',#1992,#1991,#347,.T.);
#2759=EDGE_CURVE('',#1993,#1992,#348,.T.);
#2760=EDGE_CURVE('',#1994,#1993,#349,.T.);
#2761=EDGE_CURVE('',#1995,#1994,#350,.T.);
#2762=EDGE_CURVE('',#1996,#1995,#351,.T.);
#2763=EDGE_CURVE('',#1997,#1996,#352,.T.);
#2764=EDGE_CURVE('',#1998,#1997,#353,.T.);
#2765=EDGE_CURVE('',#1999,#1998,#354,.T.);
#2766=EDGE_CURVE('',#2000,#1999,#355,.T.);
#2767=EDGE_CURVE('',#2001,#2000,#356,.T.);
#2768=EDGE_CURVE('',#2002,#2001,#357,.T.);
#2769=EDGE_CURVE('',#2003,#2002,#358,.T.);
#2770=EDGE_CURVE('',#2004,#2003,#359,.T.);
#2771=EDGE_CURVE('',#2005,#2004,#360,.T.);
#2772=EDGE_CURVE('',#2006,#2005,#361,.T.);
#2773=EDGE_CURVE('',#2007,#2006,#362,.T.);
#2774=EDGE_CURVE('',#2008,#2007,#363,.T.);
#2775=EDGE_CURVE('',#2009,#2008,#364,.T.);
#2776=EDGE_CURVE('',#2010,#2009,#365,.T.);
#2777=EDGE_CURVE('',#2011,#2010,#366,.T.);
#2778=EDGE_CURVE('',#2012,#2011,#367,.T.);
#2779=EDGE_CURVE('',#2013,#2012,#368,.T.);
#2780=EDGE_CURVE('',#2014,#2013,#369,.T.);
#2781=EDGE_CURVE('',#2015,#2014,#370,.T.);
#2782=EDGE_CURVE('',#2016,#2015,#371,.T.);
#2783=EDGE_CURVE('',#2017,#2016,#372,.T.);
#2784=EDGE_CURVE('',#2018,#2017,#373,.T.);
#2785=EDGE_CURVE('',#2019,#2018,#374,.T.);
#2786=EDGE_CURVE('',#2020,#2019,#375,.T.);
#2787=EDGE_CURVE('',#2021,#2020,#376,.T.);
#2788=EDGE_CURVE('',#2022,#2021,#377,.T.);
#2789=EDGE_CURVE('',#2023,#2022,#378,.T.);
#2790=EDGE_CURVE('',#2024,#2023,#379,.T.);
#2791=EDGE_CURVE('',#2025,#2024,#380,.T.);
#2792=EDGE_CURVE('',#2026,#2025,#381,.T.);
#2793=EDGE_CURVE('',#2027,#2026,#382,.T.);
#2794=EDGE_CURVE('',#2028,#2027,#383,.T.);
#2795=EDGE_CURVE('',#2029,#2028,#384,.T.);
#2796=EDGE_CURVE('',#2030,#2029,#385,.T.);
#2797=EDGE_CURVE('',#2031,#2030,#386,.T.);
#2798=EDGE_CURVE('',#2032,#2031,#387,.T.);
#2799=EDGE_CURVE('',#2033,#2032,#388,.T.);
#2800=EDGE_CURVE('',#2034,#2033,#389,.T.);
#2801=EDGE_CURVE('',#2035,#2034,#390,.T.);
#2802=EDGE_CURVE('',#2036,#2035,#391,.T.);
#2803=EDGE_CURVE('',#2037,#2036,#392,.T.);
#2804=EDGE_CURVE('',#2038,#2037,#393,.T.);
#2805=EDGE_CURVE('',#2039,#2038,#394,.T.);
#2806=EDGE_CURVE('',#2040,#2039,#395,.T.);
#2807=EDGE_CURVE('',#2041,#2040,#396,.T.);
#2808=EDGE_CURVE('',#2042,#2041,#397,.T.);
#2809=EDGE_CURVE('',#2043,#2042,#398,.T.);
#2810=EDGE_CURVE('',#2044,#2043,#399,.T.);
#2811=EDGE_CURVE('',#2045,#2044,#400,.T.);
#2812=EDGE_CURVE('',#2046,#2045,#401,.T.);
#2813=EDGE_CURVE('',#2047,#2046,#402,.T.);
#2814=EDGE_CURVE('',#2048,#2047,#403,.T.);
#2815=EDGE_CURVE('',#2049,#2048,#404,.T.);
#2816=EDGE_CURVE('',#2050,#2049,#405,.T.);
#2817=EDGE_CURVE('',#2051,#2050,#406,.T.);
#2818=EDGE_CURVE('',#2052,#2051,#407,.T.);
#2819=EDGE_CURVE('',#2053,#2052,#408,.T.);
#2820=EDGE_CURVE('',#2054,#2053,#409,.T.);
#2821=EDGE_CURVE('',#2055,#2054,#410,.T.);
#2822=EDGE_CURVE('',#2056,#2055,#411,.T.);
#2823=EDGE_CURVE('',#2057,#2056,#412,.T.);
#2824=EDGE_CURVE('',#2058,#2057,#413,.T.);
#2825=EDGE_CURVE('',#2059,#2058,#414,.T.);
#2826=EDGE_CURVE('',#2060,#2059,#1519,.T.);
#2827=EDGE_CURVE('',#2060,#2061,#415,.T.);
#2828=EDGE_CURVE('',#2061,#2062,#416,.T.);
#2829=EDGE_CURVE('',#2062,#2063,#417,.T.);
#2830=EDGE_CURVE('',#2063,#2064,#418,.T.);
#2831=EDGE_CURVE('',#2064,#2065,#419,.T.);
#2832=EDGE_CURVE('',#2065,#2066,#420,.T.);
#2833=EDGE_CURVE('',#2066,#2067,#421,.T.);
#2834=EDGE_CURVE('',#2067,#2068,#422,.T.);
#2835=EDGE_CURVE('',#2068,#2069,#423,.T.);
#2836=EDGE_CURVE('',#2069,#2070,#424,.T.);
#2837=EDGE_CURVE('',#2070,#2071,#425,.T.);
#2838=EDGE_CURVE('',#2071,#2072,#426,.T.);
#2839=EDGE_CURVE('',#2072,#2073,#427,.T.);
#2840=EDGE_CURVE('',#2073,#2074,#428,.T.);
#2841=EDGE_CURVE('',#2074,#2075,#429,.T.);
#2842=EDGE_CURVE('',#2075,#2076,#430,.T.);
#2843=EDGE_CURVE('',#2076,#2077,#431,.T.);
#2844=EDGE_CURVE('',#2077,#2078,#432,.T.);
#2845=EDGE_CURVE('',#2078,#2079,#433,.T.);
#2846=EDGE_CURVE('',#2079,#2080,#434,.T.);
#2847=EDGE_CURVE('',#2080,#2081,#435,.T.);
#2848=EDGE_CURVE('',#2081,#2082,#436,.T.);
#2849=EDGE_CURVE('',#2082,#2083,#437,.T.);
#2850=EDGE_CURVE('',#2083,#2084,#438,.T.);
#2851=EDGE_CURVE('',#2084,#2085,#439,.T.);
#2852=EDGE_CURVE('',#2085,#2086,#440,.T.);
#2853=EDGE_CURVE('',#2086,#2087,#441,.T.);
#2854=EDGE_CURVE('',#2087,#2088,#442,.T.);
#2855=EDGE_CURVE('',#2088,#2089,#443,.T.);
#2856=EDGE_CURVE('',#2089,#2090,#444,.T.);
#2857=EDGE_CURVE('',#2090,#2091,#445,.T.);
#2858=EDGE_CURVE('',#2091,#2092,#446,.T.);
#2859=EDGE_CURVE('',#2092,#2093,#447,.T.);
#2860=EDGE_CURVE('',#2093,#2094,#448,.T.);
#2861=EDGE_CURVE('',#2094,#2095,#449,.T.);
#2862=EDGE_CURVE('',#2095,#2096,#450,.T.);
#2863=EDGE_CURVE('',#2096,#2097,#451,.T.);
#2864=EDGE_CURVE('',#2097,#2098,#452,.T.);
#2865=EDGE_CURVE('',#2098,#2099,#453,.T.);
#2866=EDGE_CURVE('',#2099,#2100,#454,.T.);
#2867=EDGE_CURVE('',#2100,#2101,#455,.T.);
#2868=EDGE_CURVE('',#2101,#2102,#456,.T.);
#2869=EDGE_CURVE('',#2102,#2103,#457,.T.);
#2870=EDGE_CURVE('',#2103,#2104,#458,.T.);
#2871=EDGE_CURVE('',#2104,#2105,#459,.T.);
#2872=EDGE_CURVE('',#2105,#2106,#460,.T.);
#2873=EDGE_CURVE('',#2106,#2107,#461,.T.);
#2874=EDGE_CURVE('',#2107,#2108,#462,.T.);
#2875=EDGE_CURVE('',#2108,#2109,#463,.T.);
#2876=EDGE_CURVE('',#2109,#2110,#464,.T.);
#2877=EDGE_CURVE('',#2110,#2111,#465,.T.);
#2878=EDGE_CURVE('',#2111,#2112,#466,.T.);
#2879=EDGE_CURVE('',#2112,#2113,#467,.T.);
#2880=EDGE_CURVE('',#2113,#2114,#468,.T.);
#2881=EDGE_CURVE('',#2114,#2115,#469,.T.);
#2882=EDGE_CURVE('',#2115,#2116,#470,.T.);
#2883=EDGE_CURVE('',#2116,#2117,#471,.T.);
#2884=EDGE_CURVE('',#2117,#2118,#472,.T.);
#2885=EDGE_CURVE('',#2118,#2119,#473,.T.);
#2886=EDGE_CURVE('',#2119,#2120,#474,.T.);
#2887=EDGE_CURVE('',#2120,#2121,#475,.T.);
#2888=EDGE_CURVE('',#2121,#2122,#476,.T.);
#2889=EDGE_CURVE('',#2122,#2123,#477,.T.);
#2890=EDGE_CURVE('',#2123,#2124,#478,.T.);
#2891=EDGE_CURVE('',#2124,#2125,#479,.T.);
#2892=EDGE_CURVE('',#2125,#2126,#480,.T.);
#2893=EDGE_CURVE('',#2126,#2127,#481,.T.);
#2894=EDGE_CURVE('',#2127,#2128,#482,.T.);
#2895=EDGE_CURVE('',#2128,#2129,#483,.T.);
#2896=EDGE_CURVE('',#2129,#2130,#484,.T.);
#2897=EDGE_CURVE('',#2130,#2131,#485,.T.);
#2898=EDGE_CURVE('',#2131,#2132,#486,.T.);
#2899=EDGE_CURVE('',#2132,#2133,#487,.T.);
#2900=EDGE_CURVE('',#2133,#2134,#488,.T.);
#2901=EDGE_CURVE('',#2134,#2135,#489,.T.);
#2902=EDGE_CURVE('',#2135,#2136,#490,.T.);
#2903=EDGE_CURVE('',#2136,#2137,#491,.T.);
#2904=EDGE_CURVE('',#2137,#2138,#492,.T.);
#2905=EDGE_CURVE('',#2138,#2139,#493,.T.);
#2906=EDGE_CURVE('',#2139,#2140,#494,.T.);
#2907=EDGE_CURVE('',#2140,#2141,#495,.T.);
#2908=EDGE_CURVE('',#2141,#2142,#496,.T.);
#2909=EDGE_CURVE('',#2142,#2143,#497,.T.);
#2910=EDGE_CURVE('',#2143,#2144,#498,.T.);
#2911=EDGE_CURVE('',#2144,#2145,#499,.T.);
#2912=EDGE_CURVE('',#2145,#2146,#500,.T.);
#2913=EDGE_CURVE('',#2146,#2147,#501,.T.);
#2914=EDGE_CURVE('',#2147,#2148,#502,.T.);
#2915=EDGE_CURVE('',#2148,#2149,#503,.T.);
#2916=EDGE_CURVE('',#2149,#2150,#504,.T.);
#2917=EDGE_CURVE('',#2150,#2151,#505,.T.);
#2918=EDGE_CURVE('',#2151,#2152,#506,.T.);
#2919=EDGE_CURVE('',#2152,#2153,#507,.T.);
#2920=EDGE_CURVE('',#2153,#2154,#508,.T.);
#2921=EDGE_CURVE('',#2154,#2155,#509,.T.);
#2922=EDGE_CURVE('',#2155,#2156,#510,.T.);
#2923=EDGE_CURVE('',#2156,#2157,#511,.T.);
#2924=EDGE_CURVE('',#2157,#2158,#512,.T.);
#2925=EDGE_CURVE('',#2158,#2159,#513,.T.);
#2926=EDGE_CURVE('',#2159,#2160,#514,.T.);
#2927=EDGE_CURVE('',#2160,#2161,#515,.T.);
#2928=EDGE_CURVE('',#2161,#2162,#516,.T.);
#2929=EDGE_CURVE('',#2162,#1953,#517,.T.);
#2930=EDGE_CURVE('',#2163,#2163,#1520,.T.);
#2931=EDGE_CURVE('',#2164,#2165,#1196,.T.);
#2932=EDGE_CURVE('',#2166,#2164,#1197,.T.);
#2933=EDGE_CURVE('',#2167,#2166,#1198,.T.);
#2934=EDGE_CURVE('',#2168,#2167,#1199,.T.);
#2935=EDGE_CURVE('',#2169,#2168,#1200,.T.);
#2936=EDGE_CURVE('',#2165,#2169,#1201,.T.);
#2937=EDGE_CURVE('',#2163,#2170,#1202,.T.);
#2938=EDGE_CURVE('',#2170,#2170,#1521,.T.);
#2939=EDGE_CURVE('',#2167,#2171,#1203,.T.);
#2940=EDGE_CURVE('',#2172,#2171,#1204,.T.);
#2941=EDGE_CURVE('',#2168,#2172,#1205,.T.);
#2942=EDGE_CURVE('',#2166,#2173,#1206,.T.);
#2943=EDGE_CURVE('',#2171,#2173,#1207,.T.);
#2944=EDGE_CURVE('',#2164,#2174,#1208,.T.);
#2945=EDGE_CURVE('',#2173,#2174,#1209,.T.);
#2946=EDGE_CURVE('',#2175,#1745,#518,.T.);
#2947=EDGE_CURVE('',#1744,#2176,#519,.T.);
#2948=EDGE_CURVE('',#2176,#2177,#520,.T.);
#2949=EDGE_CURVE('',#2177,#2060,#521,.T.);
#2950=EDGE_CURVE('',#2059,#2175,#522,.T.);
#2951=EDGE_CURVE('',#2165,#2178,#1210,.T.);
#2952=EDGE_CURVE('',#2174,#2178,#1211,.T.);
#2953=EDGE_CURVE('',#2179,#2172,#1212,.T.);
#2954=EDGE_CURVE('',#2169,#2179,#1213,.T.);
#2955=EDGE_CURVE('',#2178,#2179,#1214,.T.);
#2956=EDGE_CURVE('',#1849,#1955,#523,.T.);
#2957=EDGE_CURVE('',#1954,#1850,#524,.T.);
#2958=ORIENTED_EDGE('',*,*,#2180,.F.);
#2959=ORIENTED_EDGE('',*,*,#2181,.T.);
#2960=ORIENTED_EDGE('',*,*,#2182,.F.);
#2961=ORIENTED_EDGE('',*,*,#2181,.F.);
#2962=ORIENTED_EDGE('',*,*,#2183,.F.);
#2963=ORIENTED_EDGE('',*,*,#2184,.T.);
#2964=ORIENTED_EDGE('',*,*,#2185,.F.);
#2965=ORIENTED_EDGE('',*,*,#2184,.F.);
#2966=ORIENTED_EDGE('',*,*,#2186,.F.);
#2967=ORIENTED_EDGE('',*,*,#2187,.T.);
#2968=ORIENTED_EDGE('',*,*,#2188,.F.);
#2969=ORIENTED_EDGE('',*,*,#2187,.F.);
#2970=ORIENTED_EDGE('',*,*,#2189,.F.);
#2971=ORIENTED_EDGE('',*,*,#2190,.T.);
#2972=ORIENTED_EDGE('',*,*,#2191,.F.);
#2973=ORIENTED_EDGE('',*,*,#2190,.F.);
#2974=ORIENTED_EDGE('',*,*,#2192,.T.);
#2975=ORIENTED_EDGE('',*,*,#2193,.T.);
#2976=ORIENTED_EDGE('',*,*,#2194,.T.);
#2977=ORIENTED_EDGE('',*,*,#2195,.T.);
#2978=ORIENTED_EDGE('',*,*,#2194,.F.);
#2979=ORIENTED_EDGE('',*,*,#2196,.T.);
#2980=ORIENTED_EDGE('',*,*,#2197,.T.);
#2981=ORIENTED_EDGE('',*,*,#2198,.T.);
#2982=ORIENTED_EDGE('',*,*,#2197,.F.);
#2983=ORIENTED_EDGE('',*,*,#2199,.T.);
#2984=ORIENTED_EDGE('',*,*,#2200,.T.);
#2985=ORIENTED_EDGE('',*,*,#2201,.T.);
#2986=ORIENTED_EDGE('',*,*,#2200,.F.);
#2987=ORIENTED_EDGE('',*,*,#2202,.T.);
#2988=ORIENTED_EDGE('',*,*,#2203,.T.);
#2989=ORIENTED_EDGE('',*,*,#2204,.T.);
#2990=ORIENTED_EDGE('',*,*,#2183,.T.);
#2991=ORIENTED_EDGE('',*,*,#2189,.T.);
#2992=ORIENTED_EDGE('',*,*,#2203,.F.);
#2993=ORIENTED_EDGE('',*,*,#2205,.T.);
#2994=ORIENTED_EDGE('',*,*,#2206,.T.);
#2995=ORIENTED_EDGE('',*,*,#2207,.T.);
#2996=ORIENTED_EDGE('',*,*,#2208,.F.);
#2997=ORIENTED_EDGE('',*,*,#2209,.T.);
#2998=ORIENTED_EDGE('',*,*,#2210,.T.);
#2999=ORIENTED_EDGE('',*,*,#2211,.T.);
#3000=ORIENTED_EDGE('',*,*,#2210,.F.);
#3001=ORIENTED_EDGE('',*,*,#2212,.T.);
#3002=ORIENTED_EDGE('',*,*,#2213,.T.);
#3003=ORIENTED_EDGE('',*,*,#2214,.T.);
#3004=ORIENTED_EDGE('',*,*,#2185,.T.);
#3005=ORIENTED_EDGE('',*,*,#2191,.T.);
#3006=ORIENTED_EDGE('',*,*,#2213,.F.);
#3007=ORIENTED_EDGE('',*,*,#2215,.T.);
#3008=ORIENTED_EDGE('',*,*,#2216,.T.);
#3009=ORIENTED_EDGE('',*,*,#2217,.T.);
#3010=ORIENTED_EDGE('',*,*,#2216,.F.);
#3011=ORIENTED_EDGE('',*,*,#2218,.T.);
#3012=ORIENTED_EDGE('',*,*,#2192,.F.);
#3013=ORIENTED_EDGE('',*,*,#2219,.T.);
#3014=ORIENTED_EDGE('',*,*,#2220,.T.);
#3015=ORIENTED_EDGE('',*,*,#2221,.T.);
#3016=ORIENTED_EDGE('',*,*,#2222,.T.);
#3017=ORIENTED_EDGE('',*,*,#2223,.T.);
#3018=ORIENTED_EDGE('',*,*,#2224,.T.);
#3019=ORIENTED_EDGE('',*,*,#2225,.T.);
#3020=ORIENTED_EDGE('',*,*,#2226,.T.);
#3021=ORIENTED_EDGE('',*,*,#2205,.F.);
#3022=ORIENTED_EDGE('',*,*,#2202,.F.);
#3023=ORIENTED_EDGE('',*,*,#2199,.F.);
#3024=ORIENTED_EDGE('',*,*,#2196,.F.);
#3025=ORIENTED_EDGE('',*,*,#2193,.F.);
#3026=ORIENTED_EDGE('',*,*,#2218,.F.);
#3027=ORIENTED_EDGE('',*,*,#2215,.F.);
#3028=ORIENTED_EDGE('',*,*,#2212,.F.);
#3029=ORIENTED_EDGE('',*,*,#2209,.F.);
#3030=ORIENTED_EDGE('',*,*,#2227,.F.);
#3031=ORIENTED_EDGE('',*,*,#2228,.T.);
#3032=ORIENTED_EDGE('',*,*,#2229,.T.);
#3033=ORIENTED_EDGE('',*,*,#2230,.T.);
#3034=ORIENTED_EDGE('',*,*,#2231,.F.);
#3035=ORIENTED_EDGE('',*,*,#2232,.F.);
#3036=ORIENTED_EDGE('',*,*,#2233,.F.);
#3037=ORIENTED_EDGE('',*,*,#2221,.F.);
#3038=ORIENTED_EDGE('',*,*,#2233,.T.);
#3039=ORIENTED_EDGE('',*,*,#2234,.F.);
#3040=ORIENTED_EDGE('',*,*,#2235,.F.);
#3041=ORIENTED_EDGE('',*,*,#2222,.F.);
#3042=ORIENTED_EDGE('',*,*,#2235,.T.);
#3043=ORIENTED_EDGE('',*,*,#2236,.F.);
#3044=ORIENTED_EDGE('',*,*,#2237,.F.);
#3045=ORIENTED_EDGE('',*,*,#2223,.F.);
#3046=ORIENTED_EDGE('',*,*,#2237,.T.);
#3047=ORIENTED_EDGE('',*,*,#2238,.F.);
#3048=ORIENTED_EDGE('',*,*,#2239,.F.);
#3049=ORIENTED_EDGE('',*,*,#2224,.F.);
#3050=ORIENTED_EDGE('',*,*,#2182,.T.);
#3051=ORIENTED_EDGE('',*,*,#2188,.T.);
#3052=ORIENTED_EDGE('',*,*,#2239,.T.);
#3053=ORIENTED_EDGE('',*,*,#2240,.F.);
#3054=ORIENTED_EDGE('',*,*,#2241,.F.);
#3055=ORIENTED_EDGE('',*,*,#2225,.F.);
#3056=ORIENTED_EDGE('',*,*,#2241,.T.);
#3057=ORIENTED_EDGE('',*,*,#2242,.T.);
#3058=ORIENTED_EDGE('',*,*,#2206,.F.);
#3059=ORIENTED_EDGE('',*,*,#2226,.F.);
#3060=ORIENTED_EDGE('',*,*,#2243,.F.);
#3061=ORIENTED_EDGE('',*,*,#2244,.F.);
#3062=ORIENTED_EDGE('',*,*,#2227,.T.);
#3063=ORIENTED_EDGE('',*,*,#2208,.T.);
#3064=ORIENTED_EDGE('',*,*,#2244,.T.);
#3065=ORIENTED_EDGE('',*,*,#2245,.F.);
#3066=ORIENTED_EDGE('',*,*,#2246,.F.);
#3067=ORIENTED_EDGE('',*,*,#2228,.F.);
#3068=ORIENTED_EDGE('',*,*,#2246,.T.);
#3069=ORIENTED_EDGE('',*,*,#2247,.F.);
#3070=ORIENTED_EDGE('',*,*,#2248,.F.);
#3071=ORIENTED_EDGE('',*,*,#2229,.F.);
#3072=ORIENTED_EDGE('',*,*,#2180,.T.);
#3073=ORIENTED_EDGE('',*,*,#2186,.T.);
#3074=ORIENTED_EDGE('',*,*,#2248,.T.);
#3075=ORIENTED_EDGE('',*,*,#2249,.F.);
#3076=ORIENTED_EDGE('',*,*,#2250,.F.);
#3077=ORIENTED_EDGE('',*,*,#2230,.F.);
#3078=ORIENTED_EDGE('',*,*,#2250,.T.);
#3079=ORIENTED_EDGE('',*,*,#2251,.F.);
#3080=ORIENTED_EDGE('',*,*,#2231,.T.);
#3081=ORIENTED_EDGE('',*,*,#2220,.F.);
#3082=ORIENTED_EDGE('',*,*,#2251,.T.);
#3083=ORIENTED_EDGE('',*,*,#2249,.T.);
#3084=ORIENTED_EDGE('',*,*,#2247,.T.);
#3085=ORIENTED_EDGE('',*,*,#2245,.T.);
#3086=ORIENTED_EDGE('',*,*,#2243,.T.);
#3087=ORIENTED_EDGE('',*,*,#2211,.F.);
#3088=ORIENTED_EDGE('',*,*,#2214,.F.);
#3089=ORIENTED_EDGE('',*,*,#2217,.F.);
#3090=ORIENTED_EDGE('',*,*,#2219,.F.);
#3091=ORIENTED_EDGE('',*,*,#2195,.F.);
#3092=ORIENTED_EDGE('',*,*,#2198,.F.);
#3093=ORIENTED_EDGE('',*,*,#2201,.F.);
#3094=ORIENTED_EDGE('',*,*,#2204,.F.);
#3095=ORIENTED_EDGE('',*,*,#2207,.F.);
#3096=ORIENTED_EDGE('',*,*,#2242,.F.);
#3097=ORIENTED_EDGE('',*,*,#2240,.T.);
#3098=ORIENTED_EDGE('',*,*,#2238,.T.);
#3099=ORIENTED_EDGE('',*,*,#2236,.T.);
#3100=ORIENTED_EDGE('',*,*,#2234,.T.);
#3101=ORIENTED_EDGE('',*,*,#2232,.T.);
#3102=ORIENTED_EDGE('',*,*,#2252,.F.);
#3103=ORIENTED_EDGE('',*,*,#2253,.T.);
#3104=ORIENTED_EDGE('',*,*,#2254,.F.);
#3105=ORIENTED_EDGE('',*,*,#2253,.F.);
#3106=ORIENTED_EDGE('',*,*,#2255,.F.);
#3107=ORIENTED_EDGE('',*,*,#2256,.T.);
#3108=ORIENTED_EDGE('',*,*,#2257,.F.);
#3109=ORIENTED_EDGE('',*,*,#2256,.F.);
#3110=ORIENTED_EDGE('',*,*,#2258,.F.);
#3111=ORIENTED_EDGE('',*,*,#2259,.T.);
#3112=ORIENTED_EDGE('',*,*,#2260,.T.);
#3113=ORIENTED_EDGE('',*,*,#2259,.F.);
#3114=ORIENTED_EDGE('',*,*,#2261,.T.);
#3115=ORIENTED_EDGE('',*,*,#2262,.T.);
#3116=ORIENTED_EDGE('',*,*,#2263,.T.);
#3117=ORIENTED_EDGE('',*,*,#2262,.F.);
#3118=ORIENTED_EDGE('',*,*,#2264,.T.);
#3119=ORIENTED_EDGE('',*,*,#2265,.T.);
#3120=ORIENTED_EDGE('',*,*,#2266,.F.);
#3121=ORIENTED_EDGE('',*,*,#2265,.F.);
#3122=ORIENTED_EDGE('',*,*,#2267,.T.);
#3123=ORIENTED_EDGE('',*,*,#2268,.T.);
#3124=ORIENTED_EDGE('',*,*,#2269,.F.);
#3125=ORIENTED_EDGE('',*,*,#2270,.F.);
#3126=ORIENTED_EDGE('',*,*,#2271,.T.);
#3127=ORIENTED_EDGE('',*,*,#2270,.T.);
#3128=ORIENTED_EDGE('',*,*,#2272,.F.);
#3129=ORIENTED_EDGE('',*,*,#2273,.F.);
#3130=ORIENTED_EDGE('',*,*,#2274,.T.);
#3131=ORIENTED_EDGE('',*,*,#2273,.T.);
#3132=ORIENTED_EDGE('',*,*,#2275,.F.);
#3133=ORIENTED_EDGE('',*,*,#2276,.F.);
#3134=ORIENTED_EDGE('',*,*,#2277,.T.);
#3135=ORIENTED_EDGE('',*,*,#2278,.T.);
#3136=ORIENTED_EDGE('',*,*,#2275,.T.);
#3137=ORIENTED_EDGE('',*,*,#2272,.T.);
#3138=ORIENTED_EDGE('',*,*,#2269,.T.);
#3139=ORIENTED_EDGE('',*,*,#2279,.T.);
#3140=ORIENTED_EDGE('',*,*,#2280,.T.);
#3141=ORIENTED_EDGE('',*,*,#2281,.T.);
#3142=ORIENTED_EDGE('',*,*,#2252,.T.);
#3143=ORIENTED_EDGE('',*,*,#2261,.F.);
#3144=ORIENTED_EDGE('',*,*,#2266,.T.);
#3145=ORIENTED_EDGE('',*,*,#2274,.F.);
#3146=ORIENTED_EDGE('',*,*,#2282,.F.);
#3147=ORIENTED_EDGE('',*,*,#2267,.F.);
#3148=ORIENTED_EDGE('',*,*,#2271,.F.);
#3149=ORIENTED_EDGE('',*,*,#2254,.T.);
#3150=ORIENTED_EDGE('',*,*,#2283,.F.);
#3151=ORIENTED_EDGE('',*,*,#2264,.F.);
#3152=ORIENTED_EDGE('',*,*,#2284,.T.);
#3153=ORIENTED_EDGE('',*,*,#2285,.T.);
#3154=ORIENTED_EDGE('',*,*,#2283,.T.);
#3155=ORIENTED_EDGE('',*,*,#2285,.F.);
#3156=ORIENTED_EDGE('',*,*,#2284,.F.);
#3157=ORIENTED_EDGE('',*,*,#2260,.F.);
#3158=ORIENTED_EDGE('',*,*,#2286,.F.);
#3159=ORIENTED_EDGE('',*,*,#2287,.T.);
#3160=ORIENTED_EDGE('',*,*,#2277,.F.);
#3161=ORIENTED_EDGE('',*,*,#2288,.F.);
#3162=ORIENTED_EDGE('',*,*,#2289,.F.);
#3163=ORIENTED_EDGE('',*,*,#2288,.T.);
#3164=ORIENTED_EDGE('',*,*,#2281,.F.);
#3165=ORIENTED_EDGE('',*,*,#2290,.F.);
#3166=ORIENTED_EDGE('',*,*,#2291,.F.);
#3167=ORIENTED_EDGE('',*,*,#2290,.T.);
#3168=ORIENTED_EDGE('',*,*,#2280,.F.);
#3169=ORIENTED_EDGE('',*,*,#2292,.F.);
#3170=ORIENTED_EDGE('',*,*,#2293,.T.);
#3171=ORIENTED_EDGE('',*,*,#2294,.T.);
#3172=ORIENTED_EDGE('',*,*,#2295,.F.);
#3173=ORIENTED_EDGE('',*,*,#2294,.F.);
#3174=ORIENTED_EDGE('',*,*,#2296,.F.);
#3175=ORIENTED_EDGE('',*,*,#2297,.T.);
#3176=ORIENTED_EDGE('',*,*,#2298,.T.);
#3177=ORIENTED_EDGE('',*,*,#2292,.T.);
#3178=ORIENTED_EDGE('',*,*,#2279,.F.);
#3179=ORIENTED_EDGE('',*,*,#2268,.F.);
#3180=ORIENTED_EDGE('',*,*,#2282,.T.);
#3181=ORIENTED_EDGE('',*,*,#2276,.T.);
#3182=ORIENTED_EDGE('',*,*,#2278,.F.);
#3183=ORIENTED_EDGE('',*,*,#2287,.F.);
#3184=ORIENTED_EDGE('',*,*,#2299,.T.);
#3185=ORIENTED_EDGE('',*,*,#2300,.F.);
#3186=ORIENTED_EDGE('',*,*,#2301,.F.);
#3187=ORIENTED_EDGE('',*,*,#2302,.T.);
#3188=ORIENTED_EDGE('',*,*,#2303,.T.);
#3189=ORIENTED_EDGE('',*,*,#2297,.F.);
#3190=ORIENTED_EDGE('',*,*,#2304,.F.);
#3191=ORIENTED_EDGE('',*,*,#2305,.T.);
#3192=ORIENTED_EDGE('',*,*,#2306,.T.);
#3193=ORIENTED_EDGE('',*,*,#2302,.F.);
#3194=ORIENTED_EDGE('',*,*,#2307,.F.);
#3195=ORIENTED_EDGE('',*,*,#2300,.T.);
#3196=ORIENTED_EDGE('',*,*,#2308,.T.);
#3197=ORIENTED_EDGE('',*,*,#2305,.F.);
#3198=ORIENTED_EDGE('',*,*,#2291,.T.);
#3199=ORIENTED_EDGE('',*,*,#2298,.F.);
#3200=ORIENTED_EDGE('',*,*,#2303,.F.);
#3201=ORIENTED_EDGE('',*,*,#2306,.F.);
#3202=ORIENTED_EDGE('',*,*,#2308,.F.);
#3203=ORIENTED_EDGE('',*,*,#2299,.F.);
#3204=ORIENTED_EDGE('',*,*,#2286,.T.);
#3205=ORIENTED_EDGE('',*,*,#2289,.T.);
#3206=ORIENTED_EDGE('',*,*,#2255,.T.);
#3207=ORIENTED_EDGE('',*,*,#2263,.F.);
#3208=ORIENTED_EDGE('',*,*,#2293,.F.);
#3209=ORIENTED_EDGE('',*,*,#2307,.T.);
#3210=ORIENTED_EDGE('',*,*,#2304,.T.);
#3211=ORIENTED_EDGE('',*,*,#2301,.T.);
#3212=ORIENTED_EDGE('',*,*,#2296,.T.);
#3213=ORIENTED_EDGE('',*,*,#2257,.T.);
#3214=ORIENTED_EDGE('',*,*,#2258,.T.);
#3215=ORIENTED_EDGE('',*,*,#2295,.T.);
#3216=ORIENTED_EDGE('',*,*,#2309,.T.);
#3217=ORIENTED_EDGE('',*,*,#2310,.F.);
#3218=ORIENTED_EDGE('',*,*,#2311,.T.);
#3219=ORIENTED_EDGE('',*,*,#2309,.F.);
#3220=ORIENTED_EDGE('',*,*,#2311,.F.);
#3221=ORIENTED_EDGE('',*,*,#2310,.T.);
#3222=ORIENTED_EDGE('',*,*,#2312,.F.);
#3223=ORIENTED_EDGE('',*,*,#2313,.T.);
#3224=ORIENTED_EDGE('',*,*,#2314,.F.);
#3225=ORIENTED_EDGE('',*,*,#2313,.F.);
#3226=ORIENTED_EDGE('',*,*,#2315,.T.);
#3227=ORIENTED_EDGE('',*,*,#2316,.T.);
#3228=ORIENTED_EDGE('',*,*,#2317,.F.);
#3229=ORIENTED_EDGE('',*,*,#2316,.F.);
#3230=ORIENTED_EDGE('',*,*,#2318,.F.);
#3231=ORIENTED_EDGE('',*,*,#2319,.T.);
#3232=ORIENTED_EDGE('',*,*,#2320,.T.);
#3233=ORIENTED_EDGE('',*,*,#2321,.F.);
#3234=ORIENTED_EDGE('',*,*,#2322,.F.);
#3235=ORIENTED_EDGE('',*,*,#2323,.T.);
#3236=ORIENTED_EDGE('',*,*,#2324,.T.);
#3237=ORIENTED_EDGE('',*,*,#2319,.F.);
#3238=ORIENTED_EDGE('',*,*,#2325,.F.);
#3239=ORIENTED_EDGE('',*,*,#2326,.T.);
#3240=ORIENTED_EDGE('',*,*,#2327,.T.);
#3241=ORIENTED_EDGE('',*,*,#2323,.F.);
#3242=ORIENTED_EDGE('',*,*,#2328,.F.);
#3243=ORIENTED_EDGE('',*,*,#2321,.T.);
#3244=ORIENTED_EDGE('',*,*,#2329,.T.);
#3245=ORIENTED_EDGE('',*,*,#2326,.F.);
#3246=ORIENTED_EDGE('',*,*,#2329,.F.);
#3247=ORIENTED_EDGE('',*,*,#2320,.F.);
#3248=ORIENTED_EDGE('',*,*,#2324,.F.);
#3249=ORIENTED_EDGE('',*,*,#2327,.F.);
#3250=ORIENTED_EDGE('',*,*,#2312,.T.);
#3251=ORIENTED_EDGE('',*,*,#2315,.F.);
#3252=ORIENTED_EDGE('',*,*,#2330,.F.);
#3253=ORIENTED_EDGE('',*,*,#2328,.T.);
#3254=ORIENTED_EDGE('',*,*,#2325,.T.);
#3255=ORIENTED_EDGE('',*,*,#2322,.T.);
#3256=ORIENTED_EDGE('',*,*,#2318,.T.);
#3257=ORIENTED_EDGE('',*,*,#2314,.T.);
#3258=ORIENTED_EDGE('',*,*,#2317,.T.);
#3259=ORIENTED_EDGE('',*,*,#2331,.F.);
#3260=ORIENTED_EDGE('',*,*,#2332,.F.);
#3261=ORIENTED_EDGE('',*,*,#2333,.T.);
#3262=ORIENTED_EDGE('',*,*,#2331,.T.);
#3263=ORIENTED_EDGE('',*,*,#2333,.F.);
#3264=ORIENTED_EDGE('',*,*,#2334,.T.);
#3265=ORIENTED_EDGE('',*,*,#2330,.T.);
#3266=ORIENTED_EDGE('',*,*,#2335,.T.);
#3267=ORIENTED_EDGE('',*,*,#2334,.F.);
#3268=ORIENTED_EDGE('',*,*,#2335,.F.);
#3269=ORIENTED_EDGE('',*,*,#2332,.T.);
#3270=ORIENTED_EDGE('',*,*,#2336,.F.);
#3271=ORIENTED_EDGE('',*,*,#2337,.T.);
#3272=ORIENTED_EDGE('',*,*,#2338,.F.);
#3273=ORIENTED_EDGE('',*,*,#2337,.F.);
#3274=ORIENTED_EDGE('',*,*,#2339,.F.);
#3275=ORIENTED_EDGE('',*,*,#2340,.F.);
#3276=ORIENTED_EDGE('',*,*,#2341,.T.);
#3277=ORIENTED_EDGE('',*,*,#2342,.F.);
#3278=ORIENTED_EDGE('',*,*,#2343,.F.);
#3279=ORIENTED_EDGE('',*,*,#2344,.F.);
#3280=ORIENTED_EDGE('',*,*,#2341,.F.);
#3281=ORIENTED_EDGE('',*,*,#2345,.T.);
#3282=ORIENTED_EDGE('',*,*,#2346,.T.);
#3283=ORIENTED_EDGE('',*,*,#2347,.F.);
#3284=ORIENTED_EDGE('',*,*,#2346,.F.);
#3285=ORIENTED_EDGE('',*,*,#2348,.T.);
#3286=ORIENTED_EDGE('',*,*,#2349,.T.);
#3287=ORIENTED_EDGE('',*,*,#2350,.F.);
#3288=ORIENTED_EDGE('',*,*,#2351,.F.);
#3289=ORIENTED_EDGE('',*,*,#2352,.T.);
#3290=ORIENTED_EDGE('',*,*,#2351,.T.);
#3291=ORIENTED_EDGE('',*,*,#2353,.F.);
#3292=ORIENTED_EDGE('',*,*,#2354,.F.);
#3293=ORIENTED_EDGE('',*,*,#2355,.T.);
#3294=ORIENTED_EDGE('',*,*,#2354,.T.);
#3295=ORIENTED_EDGE('',*,*,#2356,.F.);
#3296=ORIENTED_EDGE('',*,*,#2357,.F.);
#3297=ORIENTED_EDGE('',*,*,#2358,.T.);
#3298=ORIENTED_EDGE('',*,*,#2357,.T.);
#3299=ORIENTED_EDGE('',*,*,#2359,.F.);
#3300=ORIENTED_EDGE('',*,*,#2349,.F.);
#3301=ORIENTED_EDGE('',*,*,#2359,.T.);
#3302=ORIENTED_EDGE('',*,*,#2356,.T.);
#3303=ORIENTED_EDGE('',*,*,#2353,.T.);
#3304=ORIENTED_EDGE('',*,*,#2350,.T.);
#3305=ORIENTED_EDGE('',*,*,#2336,.T.);
#3306=ORIENTED_EDGE('',*,*,#2360,.F.);
#3307=ORIENTED_EDGE('',*,*,#2347,.T.);
#3308=ORIENTED_EDGE('',*,*,#2358,.F.);
#3309=ORIENTED_EDGE('',*,*,#2348,.F.);
#3310=ORIENTED_EDGE('',*,*,#2352,.F.);
#3311=ORIENTED_EDGE('',*,*,#2355,.F.);
#3312=ORIENTED_EDGE('',*,*,#2338,.T.);
#3313=ORIENTED_EDGE('',*,*,#2361,.F.);
#3314=ORIENTED_EDGE('',*,*,#2345,.F.);
#3315=ORIENTED_EDGE('',*,*,#2362,.T.);
#3316=ORIENTED_EDGE('',*,*,#2363,.T.);
#3317=ORIENTED_EDGE('',*,*,#2361,.T.);
#3318=ORIENTED_EDGE('',*,*,#2363,.F.);
#3319=ORIENTED_EDGE('',*,*,#2362,.F.);
#3320=ORIENTED_EDGE('',*,*,#2360,.T.);
#3321=ORIENTED_EDGE('',*,*,#2364,.T.);
#3322=ORIENTED_EDGE('',*,*,#2344,.T.);
#3323=ORIENTED_EDGE('',*,*,#2343,.T.);
#3324=ORIENTED_EDGE('',*,*,#2365,.T.);
#3325=ORIENTED_EDGE('',*,*,#2366,.T.);
#3326=ORIENTED_EDGE('',*,*,#2365,.F.);
#3327=ORIENTED_EDGE('',*,*,#2342,.T.);
#3328=ORIENTED_EDGE('',*,*,#2364,.F.);
#3329=ORIENTED_EDGE('',*,*,#2339,.T.);
#3330=ORIENTED_EDGE('',*,*,#2340,.T.);
#3331=ORIENTED_EDGE('',*,*,#2366,.F.);
#3332=ORIENTED_EDGE('',*,*,#2367,.F.);
#3333=ORIENTED_EDGE('',*,*,#2368,.T.);
#3334=ORIENTED_EDGE('',*,*,#2369,.F.);
#3335=ORIENTED_EDGE('',*,*,#2368,.F.);
#3336=ORIENTED_EDGE('',*,*,#2370,.F.);
#3337=ORIENTED_EDGE('',*,*,#2371,.T.);
#3338=ORIENTED_EDGE('',*,*,#2372,.F.);
#3339=ORIENTED_EDGE('',*,*,#2371,.F.);
#3340=ORIENTED_EDGE('',*,*,#2373,.F.);
#3341=ORIENTED_EDGE('',*,*,#2374,.T.);
#3342=ORIENTED_EDGE('',*,*,#2375,.F.);
#3343=ORIENTED_EDGE('',*,*,#2374,.F.);
#3344=ORIENTED_EDGE('',*,*,#2376,.F.);
#3345=ORIENTED_EDGE('',*,*,#2377,.T.);
#3346=ORIENTED_EDGE('',*,*,#2378,.F.);
#3347=ORIENTED_EDGE('',*,*,#2377,.F.);
#3348=ORIENTED_EDGE('',*,*,#2379,.T.);
#3349=ORIENTED_EDGE('',*,*,#2380,.T.);
#3350=ORIENTED_EDGE('',*,*,#2381,.T.);
#3351=ORIENTED_EDGE('',*,*,#2382,.T.);
#3352=ORIENTED_EDGE('',*,*,#2381,.F.);
#3353=ORIENTED_EDGE('',*,*,#2383,.T.);
#3354=ORIENTED_EDGE('',*,*,#2384,.T.);
#3355=ORIENTED_EDGE('',*,*,#2385,.T.);
#3356=ORIENTED_EDGE('',*,*,#2384,.F.);
#3357=ORIENTED_EDGE('',*,*,#2386,.T.);
#3358=ORIENTED_EDGE('',*,*,#2387,.T.);
#3359=ORIENTED_EDGE('',*,*,#2388,.T.);
#3360=ORIENTED_EDGE('',*,*,#2387,.F.);
#3361=ORIENTED_EDGE('',*,*,#2389,.T.);
#3362=ORIENTED_EDGE('',*,*,#2390,.T.);
#3363=ORIENTED_EDGE('',*,*,#2391,.T.);
#3364=ORIENTED_EDGE('',*,*,#2370,.T.);
#3365=ORIENTED_EDGE('',*,*,#2376,.T.);
#3366=ORIENTED_EDGE('',*,*,#2390,.F.);
#3367=ORIENTED_EDGE('',*,*,#2392,.T.);
#3368=ORIENTED_EDGE('',*,*,#2393,.T.);
#3369=ORIENTED_EDGE('',*,*,#2394,.T.);
#3370=ORIENTED_EDGE('',*,*,#2395,.F.);
#3371=ORIENTED_EDGE('',*,*,#2396,.T.);
#3372=ORIENTED_EDGE('',*,*,#2397,.T.);
#3373=ORIENTED_EDGE('',*,*,#2398,.T.);
#3374=ORIENTED_EDGE('',*,*,#2397,.F.);
#3375=ORIENTED_EDGE('',*,*,#2399,.T.);
#3376=ORIENTED_EDGE('',*,*,#2400,.T.);
#3377=ORIENTED_EDGE('',*,*,#2401,.T.);
#3378=ORIENTED_EDGE('',*,*,#2372,.T.);
#3379=ORIENTED_EDGE('',*,*,#2378,.T.);
#3380=ORIENTED_EDGE('',*,*,#2400,.F.);
#3381=ORIENTED_EDGE('',*,*,#2402,.T.);
#3382=ORIENTED_EDGE('',*,*,#2403,.T.);
#3383=ORIENTED_EDGE('',*,*,#2404,.T.);
#3384=ORIENTED_EDGE('',*,*,#2403,.F.);
#3385=ORIENTED_EDGE('',*,*,#2405,.T.);
#3386=ORIENTED_EDGE('',*,*,#2379,.F.);
#3387=ORIENTED_EDGE('',*,*,#2406,.T.);
#3388=ORIENTED_EDGE('',*,*,#2407,.T.);
#3389=ORIENTED_EDGE('',*,*,#2408,.T.);
#3390=ORIENTED_EDGE('',*,*,#2409,.T.);
#3391=ORIENTED_EDGE('',*,*,#2410,.T.);
#3392=ORIENTED_EDGE('',*,*,#2411,.T.);
#3393=ORIENTED_EDGE('',*,*,#2412,.T.);
#3394=ORIENTED_EDGE('',*,*,#2413,.T.);
#3395=ORIENTED_EDGE('',*,*,#2392,.F.);
#3396=ORIENTED_EDGE('',*,*,#2389,.F.);
#3397=ORIENTED_EDGE('',*,*,#2386,.F.);
#3398=ORIENTED_EDGE('',*,*,#2383,.F.);
#3399=ORIENTED_EDGE('',*,*,#2380,.F.);
#3400=ORIENTED_EDGE('',*,*,#2405,.F.);
#3401=ORIENTED_EDGE('',*,*,#2402,.F.);
#3402=ORIENTED_EDGE('',*,*,#2399,.F.);
#3403=ORIENTED_EDGE('',*,*,#2396,.F.);
#3404=ORIENTED_EDGE('',*,*,#2414,.F.);
#3405=ORIENTED_EDGE('',*,*,#2415,.T.);
#3406=ORIENTED_EDGE('',*,*,#2416,.T.);
#3407=ORIENTED_EDGE('',*,*,#2417,.T.);
#3408=ORIENTED_EDGE('',*,*,#2418,.F.);
#3409=ORIENTED_EDGE('',*,*,#2419,.F.);
#3410=ORIENTED_EDGE('',*,*,#2420,.F.);
#3411=ORIENTED_EDGE('',*,*,#2408,.F.);
#3412=ORIENTED_EDGE('',*,*,#2420,.T.);
#3413=ORIENTED_EDGE('',*,*,#2421,.F.);
#3414=ORIENTED_EDGE('',*,*,#2422,.F.);
#3415=ORIENTED_EDGE('',*,*,#2409,.F.);
#3416=ORIENTED_EDGE('',*,*,#2422,.T.);
#3417=ORIENTED_EDGE('',*,*,#2423,.F.);
#3418=ORIENTED_EDGE('',*,*,#2424,.F.);
#3419=ORIENTED_EDGE('',*,*,#2410,.F.);
#3420=ORIENTED_EDGE('',*,*,#2424,.T.);
#3421=ORIENTED_EDGE('',*,*,#2425,.F.);
#3422=ORIENTED_EDGE('',*,*,#2426,.F.);
#3423=ORIENTED_EDGE('',*,*,#2411,.F.);
#3424=ORIENTED_EDGE('',*,*,#2369,.T.);
#3425=ORIENTED_EDGE('',*,*,#2375,.T.);
#3426=ORIENTED_EDGE('',*,*,#2426,.T.);
#3427=ORIENTED_EDGE('',*,*,#2427,.F.);
#3428=ORIENTED_EDGE('',*,*,#2428,.F.);
#3429=ORIENTED_EDGE('',*,*,#2412,.F.);
#3430=ORIENTED_EDGE('',*,*,#2428,.T.);
#3431=ORIENTED_EDGE('',*,*,#2429,.T.);
#3432=ORIENTED_EDGE('',*,*,#2393,.F.);
#3433=ORIENTED_EDGE('',*,*,#2413,.F.);
#3434=ORIENTED_EDGE('',*,*,#2430,.F.);
#3435=ORIENTED_EDGE('',*,*,#2431,.F.);
#3436=ORIENTED_EDGE('',*,*,#2414,.T.);
#3437=ORIENTED_EDGE('',*,*,#2395,.T.);
#3438=ORIENTED_EDGE('',*,*,#2431,.T.);
#3439=ORIENTED_EDGE('',*,*,#2432,.F.);
#3440=ORIENTED_EDGE('',*,*,#2433,.F.);
#3441=ORIENTED_EDGE('',*,*,#2415,.F.);
#3442=ORIENTED_EDGE('',*,*,#2433,.T.);
#3443=ORIENTED_EDGE('',*,*,#2434,.F.);
#3444=ORIENTED_EDGE('',*,*,#2435,.F.);
#3445=ORIENTED_EDGE('',*,*,#2416,.F.);
#3446=ORIENTED_EDGE('',*,*,#2367,.T.);
#3447=ORIENTED_EDGE('',*,*,#2373,.T.);
#3448=ORIENTED_EDGE('',*,*,#2435,.T.);
#3449=ORIENTED_EDGE('',*,*,#2436,.F.);
#3450=ORIENTED_EDGE('',*,*,#2437,.F.);
#3451=ORIENTED_EDGE('',*,*,#2417,.F.);
#3452=ORIENTED_EDGE('',*,*,#2437,.T.);
#3453=ORIENTED_EDGE('',*,*,#2438,.F.);
#3454=ORIENTED_EDGE('',*,*,#2418,.T.);
#3455=ORIENTED_EDGE('',*,*,#2407,.F.);
#3456=ORIENTED_EDGE('',*,*,#2438,.T.);
#3457=ORIENTED_EDGE('',*,*,#2436,.T.);
#3458=ORIENTED_EDGE('',*,*,#2434,.T.);
#3459=ORIENTED_EDGE('',*,*,#2432,.T.);
#3460=ORIENTED_EDGE('',*,*,#2430,.T.);
#3461=ORIENTED_EDGE('',*,*,#2398,.F.);
#3462=ORIENTED_EDGE('',*,*,#2401,.F.);
#3463=ORIENTED_EDGE('',*,*,#2404,.F.);
#3464=ORIENTED_EDGE('',*,*,#2406,.F.);
#3465=ORIENTED_EDGE('',*,*,#2382,.F.);
#3466=ORIENTED_EDGE('',*,*,#2385,.F.);
#3467=ORIENTED_EDGE('',*,*,#2388,.F.);
#3468=ORIENTED_EDGE('',*,*,#2391,.F.);
#3469=ORIENTED_EDGE('',*,*,#2394,.F.);
#3470=ORIENTED_EDGE('',*,*,#2429,.F.);
#3471=ORIENTED_EDGE('',*,*,#2427,.T.);
#3472=ORIENTED_EDGE('',*,*,#2425,.T.);
#3473=ORIENTED_EDGE('',*,*,#2423,.T.);
#3474=ORIENTED_EDGE('',*,*,#2421,.T.);
#3475=ORIENTED_EDGE('',*,*,#2419,.T.);
#3476=ORIENTED_EDGE('',*,*,#2439,.T.);
#3477=ORIENTED_EDGE('',*,*,#2440,.T.);
#3478=ORIENTED_EDGE('',*,*,#2441,.F.);
#3479=ORIENTED_EDGE('',*,*,#2442,.F.);
#3480=ORIENTED_EDGE('',*,*,#2443,.F.);
#3481=ORIENTED_EDGE('',*,*,#2444,.F.);
#3482=ORIENTED_EDGE('',*,*,#2445,.F.);
#3483=ORIENTED_EDGE('',*,*,#2446,.F.);
#3484=ORIENTED_EDGE('',*,*,#2447,.T.);
#3485=ORIENTED_EDGE('',*,*,#2448,.F.);
#3486=ORIENTED_EDGE('',*,*,#2449,.T.);
#3487=ORIENTED_EDGE('',*,*,#2450,.F.);
#3488=ORIENTED_EDGE('',*,*,#2451,.T.);
#3489=ORIENTED_EDGE('',*,*,#2448,.T.);
#3490=ORIENTED_EDGE('',*,*,#2452,.T.);
#3491=ORIENTED_EDGE('',*,*,#2453,.F.);
#3492=ORIENTED_EDGE('',*,*,#2454,.T.);
#3493=ORIENTED_EDGE('',*,*,#2443,.T.);
#3494=ORIENTED_EDGE('',*,*,#2455,.T.);
#3495=ORIENTED_EDGE('',*,*,#2456,.T.);
#3496=ORIENTED_EDGE('',*,*,#2439,.F.);
#3497=ORIENTED_EDGE('',*,*,#2457,.F.);
#3498=ORIENTED_EDGE('',*,*,#2458,.F.);
#3499=ORIENTED_EDGE('',*,*,#2459,.T.);
#3500=ORIENTED_EDGE('',*,*,#2460,.T.);
#3501=ORIENTED_EDGE('',*,*,#2461,.F.);
#3502=ORIENTED_EDGE('',*,*,#2462,.T.);
#3503=ORIENTED_EDGE('',*,*,#2463,.F.);
#3504=ORIENTED_EDGE('',*,*,#2452,.F.);
#3505=ORIENTED_EDGE('',*,*,#2451,.F.);
#3506=ORIENTED_EDGE('',*,*,#2464,.F.);
#3507=ORIENTED_EDGE('',*,*,#2445,.T.);
#3508=ORIENTED_EDGE('',*,*,#2444,.T.);
#3509=ORIENTED_EDGE('',*,*,#2457,.T.);
#3510=ORIENTED_EDGE('',*,*,#2442,.T.);
#3511=ORIENTED_EDGE('',*,*,#2465,.F.);
#3512=ORIENTED_EDGE('',*,*,#2462,.F.);
#3513=ORIENTED_EDGE('',*,*,#2466,.F.);
#3514=ORIENTED_EDGE('',*,*,#2467,.T.);
#3515=ORIENTED_EDGE('',*,*,#2468,.F.);
#3516=ORIENTED_EDGE('',*,*,#2469,.F.);
#3517=ORIENTED_EDGE('',*,*,#2470,.F.);
#3518=ORIENTED_EDGE('',*,*,#2471,.T.);
#3519=ORIENTED_EDGE('',*,*,#2459,.F.);
#3520=ORIENTED_EDGE('',*,*,#2472,.F.);
#3521=ORIENTED_EDGE('',*,*,#2440,.F.);
#3522=ORIENTED_EDGE('',*,*,#2456,.F.);
#3523=ORIENTED_EDGE('',*,*,#2455,.F.);
#3524=ORIENTED_EDGE('',*,*,#2447,.F.);
#3525=ORIENTED_EDGE('',*,*,#2473,.F.);
#3526=ORIENTED_EDGE('',*,*,#2449,.F.);
#3527=ORIENTED_EDGE('',*,*,#2454,.F.);
#3528=ORIENTED_EDGE('',*,*,#2474,.F.);
#3529=ORIENTED_EDGE('',*,*,#2475,.F.);
#3530=ORIENTED_EDGE('',*,*,#2476,.F.);
#3531=ORIENTED_EDGE('',*,*,#2467,.F.);
#3532=ORIENTED_EDGE('',*,*,#2477,.F.);
#3533=ORIENTED_EDGE('',*,*,#2478,.F.);
#3534=ORIENTED_EDGE('',*,*,#2479,.F.);
#3535=ORIENTED_EDGE('',*,*,#2460,.F.);
#3536=ORIENTED_EDGE('',*,*,#2471,.F.);
#3537=ORIENTED_EDGE('',*,*,#2480,.F.);
#3538=ORIENTED_EDGE('',*,*,#2481,.F.);
#3539=ORIENTED_EDGE('',*,*,#2482,.F.);
#3540=ORIENTED_EDGE('',*,*,#2469,.T.);
#3541=ORIENTED_EDGE('',*,*,#2483,.F.);
#3542=ORIENTED_EDGE('',*,*,#2484,.T.);
#3543=ORIENTED_EDGE('',*,*,#2485,.T.);
#3544=ORIENTED_EDGE('',*,*,#2486,.T.);
#3545=ORIENTED_EDGE('',*,*,#2487,.T.);
#3546=ORIENTED_EDGE('',*,*,#2488,.F.);
#3547=ORIENTED_EDGE('',*,*,#2487,.F.);
#3548=ORIENTED_EDGE('',*,*,#2489,.T.);
#3549=ORIENTED_EDGE('',*,*,#2484,.F.);
#3550=ORIENTED_EDGE('',*,*,#2480,.T.);
#3551=ORIENTED_EDGE('',*,*,#2468,.T.);
#3552=ORIENTED_EDGE('',*,*,#2458,.T.);
#3553=ORIENTED_EDGE('',*,*,#2479,.T.);
#3554=ORIENTED_EDGE('',*,*,#2470,.T.);
#3555=ORIENTED_EDGE('',*,*,#2482,.T.);
#3556=ORIENTED_EDGE('',*,*,#2490,.T.);
#3557=ORIENTED_EDGE('',*,*,#2474,.T.);
#3558=ORIENTED_EDGE('',*,*,#2453,.T.);
#3559=ORIENTED_EDGE('',*,*,#2463,.T.);
#3560=ORIENTED_EDGE('',*,*,#2465,.T.);
#3561=ORIENTED_EDGE('',*,*,#2476,.T.);
#3562=ORIENTED_EDGE('',*,*,#2491,.T.);
#3563=ORIENTED_EDGE('',*,*,#2477,.T.);
#3564=ORIENTED_EDGE('',*,*,#2466,.T.);
#3565=ORIENTED_EDGE('',*,*,#2461,.T.);
#3566=ORIENTED_EDGE('',*,*,#2441,.T.);
#3567=ORIENTED_EDGE('',*,*,#2472,.T.);
#3568=ORIENTED_EDGE('',*,*,#2492,.T.);
#3569=ORIENTED_EDGE('',*,*,#2478,.T.);
#3570=ORIENTED_EDGE('',*,*,#2491,.F.);
#3571=ORIENTED_EDGE('',*,*,#2481,.T.);
#3572=ORIENTED_EDGE('',*,*,#2492,.F.);
#3573=ORIENTED_EDGE('',*,*,#2475,.T.);
#3574=ORIENTED_EDGE('',*,*,#2490,.F.);
#3575=ORIENTED_EDGE('',*,*,#2486,.F.);
#3576=ORIENTED_EDGE('',*,*,#2485,.F.);
#3577=ORIENTED_EDGE('',*,*,#2493,.T.);
#3578=ORIENTED_EDGE('',*,*,#2494,.F.);
#3579=ORIENTED_EDGE('',*,*,#2493,.F.);
#3580=ORIENTED_EDGE('',*,*,#2489,.F.);
#3581=ORIENTED_EDGE('',*,*,#2495,.T.);
#3582=ORIENTED_EDGE('',*,*,#2496,.T.);
#3583=ORIENTED_EDGE('',*,*,#2497,.T.);
#3584=ORIENTED_EDGE('',*,*,#2498,.T.);
#3585=ORIENTED_EDGE('',*,*,#2483,.T.);
#3586=ORIENTED_EDGE('',*,*,#2499,.F.);
#3587=ORIENTED_EDGE('',*,*,#2500,.F.);
#3588=ORIENTED_EDGE('',*,*,#2501,.F.);
#3589=ORIENTED_EDGE('',*,*,#2496,.F.);
#3590=ORIENTED_EDGE('',*,*,#2494,.T.);
#3591=ORIENTED_EDGE('',*,*,#2501,.T.);
#3592=ORIENTED_EDGE('',*,*,#2502,.F.);
#3593=ORIENTED_EDGE('',*,*,#2503,.F.);
#3594=ORIENTED_EDGE('',*,*,#2497,.F.);
#3595=ORIENTED_EDGE('',*,*,#2503,.T.);
#3596=ORIENTED_EDGE('',*,*,#2504,.F.);
#3597=ORIENTED_EDGE('',*,*,#2505,.F.);
#3598=ORIENTED_EDGE('',*,*,#2498,.F.);
#3599=ORIENTED_EDGE('',*,*,#2464,.T.);
#3600=ORIENTED_EDGE('',*,*,#2450,.T.);
#3601=ORIENTED_EDGE('',*,*,#2473,.T.);
#3602=ORIENTED_EDGE('',*,*,#2446,.T.);
#3603=ORIENTED_EDGE('',*,*,#2505,.T.);
#3604=ORIENTED_EDGE('',*,*,#2506,.F.);
#3605=ORIENTED_EDGE('',*,*,#2499,.T.);
#3606=ORIENTED_EDGE('',*,*,#2495,.F.);
#3607=ORIENTED_EDGE('',*,*,#2506,.T.);
#3608=ORIENTED_EDGE('',*,*,#2504,.T.);
#3609=ORIENTED_EDGE('',*,*,#2502,.T.);
#3610=ORIENTED_EDGE('',*,*,#2500,.T.);
#3611=ORIENTED_EDGE('',*,*,#2488,.T.);
#3612=ORIENTED_EDGE('',*,*,#2507,.T.);
#3613=ORIENTED_EDGE('',*,*,#2508,.F.);
#3614=ORIENTED_EDGE('',*,*,#2509,.T.);
#3615=ORIENTED_EDGE('',*,*,#2507,.F.);
#3616=ORIENTED_EDGE('',*,*,#2509,.F.);
#3617=ORIENTED_EDGE('',*,*,#2508,.T.);
#3618=ORIENTED_EDGE('',*,*,#2510,.T.);
#3619=ORIENTED_EDGE('',*,*,#2511,.F.);
#3620=ORIENTED_EDGE('',*,*,#2512,.T.);
#3621=ORIENTED_EDGE('',*,*,#2513,.T.);
#3622=ORIENTED_EDGE('',*,*,#2514,.T.);
#3623=ORIENTED_EDGE('',*,*,#2515,.T.);
#3624=ORIENTED_EDGE('',*,*,#2516,.T.);
#3625=ORIENTED_EDGE('',*,*,#2517,.T.);
#3626=ORIENTED_EDGE('',*,*,#2518,.T.);
#3627=ORIENTED_EDGE('',*,*,#2519,.T.);
#3628=ORIENTED_EDGE('',*,*,#2520,.T.);
#3629=ORIENTED_EDGE('',*,*,#2521,.T.);
#3630=ORIENTED_EDGE('',*,*,#2522,.T.);
#3631=ORIENTED_EDGE('',*,*,#2523,.T.);
#3632=ORIENTED_EDGE('',*,*,#2524,.T.);
#3633=ORIENTED_EDGE('',*,*,#2525,.T.);
#3634=ORIENTED_EDGE('',*,*,#2526,.T.);
#3635=ORIENTED_EDGE('',*,*,#2527,.T.);
#3636=ORIENTED_EDGE('',*,*,#2528,.T.);
#3637=ORIENTED_EDGE('',*,*,#2529,.T.);
#3638=ORIENTED_EDGE('',*,*,#2530,.T.);
#3639=ORIENTED_EDGE('',*,*,#2531,.T.);
#3640=ORIENTED_EDGE('',*,*,#2532,.T.);
#3641=ORIENTED_EDGE('',*,*,#2533,.T.);
#3642=ORIENTED_EDGE('',*,*,#2534,.T.);
#3643=ORIENTED_EDGE('',*,*,#2535,.T.);
#3644=ORIENTED_EDGE('',*,*,#2536,.T.);
#3645=ORIENTED_EDGE('',*,*,#2537,.T.);
#3646=ORIENTED_EDGE('',*,*,#2538,.T.);
#3647=ORIENTED_EDGE('',*,*,#2539,.T.);
#3648=ORIENTED_EDGE('',*,*,#2540,.T.);
#3649=ORIENTED_EDGE('',*,*,#2541,.T.);
#3650=ORIENTED_EDGE('',*,*,#2542,.T.);
#3651=ORIENTED_EDGE('',*,*,#2543,.T.);
#3652=ORIENTED_EDGE('',*,*,#2544,.T.);
#3653=ORIENTED_EDGE('',*,*,#2545,.T.);
#3654=ORIENTED_EDGE('',*,*,#2546,.T.);
#3655=ORIENTED_EDGE('',*,*,#2547,.T.);
#3656=ORIENTED_EDGE('',*,*,#2548,.T.);
#3657=ORIENTED_EDGE('',*,*,#2549,.T.);
#3658=ORIENTED_EDGE('',*,*,#2550,.T.);
#3659=ORIENTED_EDGE('',*,*,#2551,.T.);
#3660=ORIENTED_EDGE('',*,*,#2552,.T.);
#3661=ORIENTED_EDGE('',*,*,#2553,.T.);
#3662=ORIENTED_EDGE('',*,*,#2554,.T.);
#3663=ORIENTED_EDGE('',*,*,#2555,.T.);
#3664=ORIENTED_EDGE('',*,*,#2556,.T.);
#3665=ORIENTED_EDGE('',*,*,#2557,.T.);
#3666=ORIENTED_EDGE('',*,*,#2558,.T.);
#3667=ORIENTED_EDGE('',*,*,#2559,.T.);
#3668=ORIENTED_EDGE('',*,*,#2560,.T.);
#3669=ORIENTED_EDGE('',*,*,#2561,.T.);
#3670=ORIENTED_EDGE('',*,*,#2562,.T.);
#3671=ORIENTED_EDGE('',*,*,#2563,.T.);
#3672=ORIENTED_EDGE('',*,*,#2564,.T.);
#3673=ORIENTED_EDGE('',*,*,#2565,.T.);
#3674=ORIENTED_EDGE('',*,*,#2566,.T.);
#3675=ORIENTED_EDGE('',*,*,#2567,.T.);
#3676=ORIENTED_EDGE('',*,*,#2568,.T.);
#3677=ORIENTED_EDGE('',*,*,#2569,.T.);
#3678=ORIENTED_EDGE('',*,*,#2570,.T.);
#3679=ORIENTED_EDGE('',*,*,#2571,.T.);
#3680=ORIENTED_EDGE('',*,*,#2572,.T.);
#3681=ORIENTED_EDGE('',*,*,#2573,.T.);
#3682=ORIENTED_EDGE('',*,*,#2574,.T.);
#3683=ORIENTED_EDGE('',*,*,#2575,.T.);
#3684=ORIENTED_EDGE('',*,*,#2576,.T.);
#3685=ORIENTED_EDGE('',*,*,#2577,.T.);
#3686=ORIENTED_EDGE('',*,*,#2578,.T.);
#3687=ORIENTED_EDGE('',*,*,#2579,.T.);
#3688=ORIENTED_EDGE('',*,*,#2580,.T.);
#3689=ORIENTED_EDGE('',*,*,#2581,.T.);
#3690=ORIENTED_EDGE('',*,*,#2582,.T.);
#3691=ORIENTED_EDGE('',*,*,#2583,.T.);
#3692=ORIENTED_EDGE('',*,*,#2584,.T.);
#3693=ORIENTED_EDGE('',*,*,#2585,.T.);
#3694=ORIENTED_EDGE('',*,*,#2586,.T.);
#3695=ORIENTED_EDGE('',*,*,#2587,.T.);
#3696=ORIENTED_EDGE('',*,*,#2588,.T.);
#3697=ORIENTED_EDGE('',*,*,#2589,.T.);
#3698=ORIENTED_EDGE('',*,*,#2590,.T.);
#3699=ORIENTED_EDGE('',*,*,#2591,.T.);
#3700=ORIENTED_EDGE('',*,*,#2592,.T.);
#3701=ORIENTED_EDGE('',*,*,#2593,.T.);
#3702=ORIENTED_EDGE('',*,*,#2594,.T.);
#3703=ORIENTED_EDGE('',*,*,#2595,.T.);
#3704=ORIENTED_EDGE('',*,*,#2596,.T.);
#3705=ORIENTED_EDGE('',*,*,#2597,.T.);
#3706=ORIENTED_EDGE('',*,*,#2598,.T.);
#3707=ORIENTED_EDGE('',*,*,#2599,.T.);
#3708=ORIENTED_EDGE('',*,*,#2600,.T.);
#3709=ORIENTED_EDGE('',*,*,#2601,.T.);
#3710=ORIENTED_EDGE('',*,*,#2602,.T.);
#3711=ORIENTED_EDGE('',*,*,#2603,.T.);
#3712=ORIENTED_EDGE('',*,*,#2604,.T.);
#3713=ORIENTED_EDGE('',*,*,#2605,.T.);
#3714=ORIENTED_EDGE('',*,*,#2606,.T.);
#3715=ORIENTED_EDGE('',*,*,#2607,.T.);
#3716=ORIENTED_EDGE('',*,*,#2608,.T.);
#3717=ORIENTED_EDGE('',*,*,#2609,.T.);
#3718=ORIENTED_EDGE('',*,*,#2610,.T.);
#3719=ORIENTED_EDGE('',*,*,#2611,.T.);
#3720=ORIENTED_EDGE('',*,*,#2612,.T.);
#3721=ORIENTED_EDGE('',*,*,#2613,.T.);
#3722=ORIENTED_EDGE('',*,*,#2614,.T.);
#3723=ORIENTED_EDGE('',*,*,#2615,.T.);
#3724=ORIENTED_EDGE('',*,*,#2616,.F.);
#3725=ORIENTED_EDGE('',*,*,#2617,.T.);
#3726=ORIENTED_EDGE('',*,*,#2618,.T.);
#3727=ORIENTED_EDGE('',*,*,#2619,.T.);
#3728=ORIENTED_EDGE('',*,*,#2620,.T.);
#3729=ORIENTED_EDGE('',*,*,#2621,.T.);
#3730=ORIENTED_EDGE('',*,*,#2622,.T.);
#3731=ORIENTED_EDGE('',*,*,#2623,.T.);
#3732=ORIENTED_EDGE('',*,*,#2624,.T.);
#3733=ORIENTED_EDGE('',*,*,#2625,.T.);
#3734=ORIENTED_EDGE('',*,*,#2626,.T.);
#3735=ORIENTED_EDGE('',*,*,#2627,.T.);
#3736=ORIENTED_EDGE('',*,*,#2628,.T.);
#3737=ORIENTED_EDGE('',*,*,#2629,.T.);
#3738=ORIENTED_EDGE('',*,*,#2630,.T.);
#3739=ORIENTED_EDGE('',*,*,#2631,.T.);
#3740=ORIENTED_EDGE('',*,*,#2632,.T.);
#3741=ORIENTED_EDGE('',*,*,#2633,.T.);
#3742=ORIENTED_EDGE('',*,*,#2634,.T.);
#3743=ORIENTED_EDGE('',*,*,#2635,.T.);
#3744=ORIENTED_EDGE('',*,*,#2636,.T.);
#3745=ORIENTED_EDGE('',*,*,#2637,.T.);
#3746=ORIENTED_EDGE('',*,*,#2638,.T.);
#3747=ORIENTED_EDGE('',*,*,#2639,.T.);
#3748=ORIENTED_EDGE('',*,*,#2640,.T.);
#3749=ORIENTED_EDGE('',*,*,#2641,.T.);
#3750=ORIENTED_EDGE('',*,*,#2642,.T.);
#3751=ORIENTED_EDGE('',*,*,#2643,.T.);
#3752=ORIENTED_EDGE('',*,*,#2644,.T.);
#3753=ORIENTED_EDGE('',*,*,#2645,.T.);
#3754=ORIENTED_EDGE('',*,*,#2646,.T.);
#3755=ORIENTED_EDGE('',*,*,#2647,.T.);
#3756=ORIENTED_EDGE('',*,*,#2648,.T.);
#3757=ORIENTED_EDGE('',*,*,#2649,.T.);
#3758=ORIENTED_EDGE('',*,*,#2650,.T.);
#3759=ORIENTED_EDGE('',*,*,#2651,.T.);
#3760=ORIENTED_EDGE('',*,*,#2652,.T.);
#3761=ORIENTED_EDGE('',*,*,#2653,.T.);
#3762=ORIENTED_EDGE('',*,*,#2654,.T.);
#3763=ORIENTED_EDGE('',*,*,#2655,.T.);
#3764=ORIENTED_EDGE('',*,*,#2656,.T.);
#3765=ORIENTED_EDGE('',*,*,#2657,.T.);
#3766=ORIENTED_EDGE('',*,*,#2658,.T.);
#3767=ORIENTED_EDGE('',*,*,#2659,.T.);
#3768=ORIENTED_EDGE('',*,*,#2660,.T.);
#3769=ORIENTED_EDGE('',*,*,#2661,.T.);
#3770=ORIENTED_EDGE('',*,*,#2662,.T.);
#3771=ORIENTED_EDGE('',*,*,#2663,.T.);
#3772=ORIENTED_EDGE('',*,*,#2664,.T.);
#3773=ORIENTED_EDGE('',*,*,#2665,.T.);
#3774=ORIENTED_EDGE('',*,*,#2666,.T.);
#3775=ORIENTED_EDGE('',*,*,#2667,.T.);
#3776=ORIENTED_EDGE('',*,*,#2668,.T.);
#3777=ORIENTED_EDGE('',*,*,#2669,.T.);
#3778=ORIENTED_EDGE('',*,*,#2670,.T.);
#3779=ORIENTED_EDGE('',*,*,#2671,.T.);
#3780=ORIENTED_EDGE('',*,*,#2672,.T.);
#3781=ORIENTED_EDGE('',*,*,#2673,.T.);
#3782=ORIENTED_EDGE('',*,*,#2674,.T.);
#3783=ORIENTED_EDGE('',*,*,#2675,.T.);
#3784=ORIENTED_EDGE('',*,*,#2676,.T.);
#3785=ORIENTED_EDGE('',*,*,#2677,.T.);
#3786=ORIENTED_EDGE('',*,*,#2678,.T.);
#3787=ORIENTED_EDGE('',*,*,#2679,.T.);
#3788=ORIENTED_EDGE('',*,*,#2680,.T.);
#3789=ORIENTED_EDGE('',*,*,#2681,.T.);
#3790=ORIENTED_EDGE('',*,*,#2682,.T.);
#3791=ORIENTED_EDGE('',*,*,#2683,.T.);
#3792=ORIENTED_EDGE('',*,*,#2684,.T.);
#3793=ORIENTED_EDGE('',*,*,#2685,.T.);
#3794=ORIENTED_EDGE('',*,*,#2686,.T.);
#3795=ORIENTED_EDGE('',*,*,#2687,.T.);
#3796=ORIENTED_EDGE('',*,*,#2688,.T.);
#3797=ORIENTED_EDGE('',*,*,#2689,.T.);
#3798=ORIENTED_EDGE('',*,*,#2690,.T.);
#3799=ORIENTED_EDGE('',*,*,#2691,.T.);
#3800=ORIENTED_EDGE('',*,*,#2692,.T.);
#3801=ORIENTED_EDGE('',*,*,#2693,.T.);
#3802=ORIENTED_EDGE('',*,*,#2694,.T.);
#3803=ORIENTED_EDGE('',*,*,#2695,.T.);
#3804=ORIENTED_EDGE('',*,*,#2696,.T.);
#3805=ORIENTED_EDGE('',*,*,#2697,.T.);
#3806=ORIENTED_EDGE('',*,*,#2698,.T.);
#3807=ORIENTED_EDGE('',*,*,#2699,.T.);
#3808=ORIENTED_EDGE('',*,*,#2700,.T.);
#3809=ORIENTED_EDGE('',*,*,#2701,.T.);
#3810=ORIENTED_EDGE('',*,*,#2702,.T.);
#3811=ORIENTED_EDGE('',*,*,#2703,.T.);
#3812=ORIENTED_EDGE('',*,*,#2704,.T.);
#3813=ORIENTED_EDGE('',*,*,#2705,.T.);
#3814=ORIENTED_EDGE('',*,*,#2706,.T.);
#3815=ORIENTED_EDGE('',*,*,#2707,.T.);
#3816=ORIENTED_EDGE('',*,*,#2708,.T.);
#3817=ORIENTED_EDGE('',*,*,#2709,.T.);
#3818=ORIENTED_EDGE('',*,*,#2710,.T.);
#3819=ORIENTED_EDGE('',*,*,#2711,.T.);
#3820=ORIENTED_EDGE('',*,*,#2712,.T.);
#3821=ORIENTED_EDGE('',*,*,#2713,.T.);
#3822=ORIENTED_EDGE('',*,*,#2714,.T.);
#3823=ORIENTED_EDGE('',*,*,#2715,.T.);
#3824=ORIENTED_EDGE('',*,*,#2716,.T.);
#3825=ORIENTED_EDGE('',*,*,#2717,.T.);
#3826=ORIENTED_EDGE('',*,*,#2718,.T.);
#3827=ORIENTED_EDGE('',*,*,#2719,.T.);
#3828=ORIENTED_EDGE('',*,*,#2720,.T.);
#3829=ORIENTED_EDGE('',*,*,#2721,.F.);
#3830=ORIENTED_EDGE('',*,*,#2722,.F.);
#3831=ORIENTED_EDGE('',*,*,#2723,.F.);
#3832=ORIENTED_EDGE('',*,*,#2724,.F.);
#3833=ORIENTED_EDGE('',*,*,#2725,.F.);
#3834=ORIENTED_EDGE('',*,*,#2726,.F.);
#3835=ORIENTED_EDGE('',*,*,#2727,.F.);
#3836=ORIENTED_EDGE('',*,*,#2728,.F.);
#3837=ORIENTED_EDGE('',*,*,#2729,.F.);
#3838=ORIENTED_EDGE('',*,*,#2730,.F.);
#3839=ORIENTED_EDGE('',*,*,#2731,.F.);
#3840=ORIENTED_EDGE('',*,*,#2732,.F.);
#3841=ORIENTED_EDGE('',*,*,#2733,.F.);
#3842=ORIENTED_EDGE('',*,*,#2734,.F.);
#3843=ORIENTED_EDGE('',*,*,#2735,.F.);
#3844=ORIENTED_EDGE('',*,*,#2736,.F.);
#3845=ORIENTED_EDGE('',*,*,#2737,.F.);
#3846=ORIENTED_EDGE('',*,*,#2738,.F.);
#3847=ORIENTED_EDGE('',*,*,#2739,.F.);
#3848=ORIENTED_EDGE('',*,*,#2740,.F.);
#3849=ORIENTED_EDGE('',*,*,#2741,.F.);
#3850=ORIENTED_EDGE('',*,*,#2742,.F.);
#3851=ORIENTED_EDGE('',*,*,#2743,.F.);
#3852=ORIENTED_EDGE('',*,*,#2744,.F.);
#3853=ORIENTED_EDGE('',*,*,#2745,.F.);
#3854=ORIENTED_EDGE('',*,*,#2746,.F.);
#3855=ORIENTED_EDGE('',*,*,#2747,.F.);
#3856=ORIENTED_EDGE('',*,*,#2748,.F.);
#3857=ORIENTED_EDGE('',*,*,#2749,.F.);
#3858=ORIENTED_EDGE('',*,*,#2750,.F.);
#3859=ORIENTED_EDGE('',*,*,#2751,.F.);
#3860=ORIENTED_EDGE('',*,*,#2752,.F.);
#3861=ORIENTED_EDGE('',*,*,#2753,.F.);
#3862=ORIENTED_EDGE('',*,*,#2754,.F.);
#3863=ORIENTED_EDGE('',*,*,#2755,.F.);
#3864=ORIENTED_EDGE('',*,*,#2756,.F.);
#3865=ORIENTED_EDGE('',*,*,#2757,.F.);
#3866=ORIENTED_EDGE('',*,*,#2758,.F.);
#3867=ORIENTED_EDGE('',*,*,#2759,.F.);
#3868=ORIENTED_EDGE('',*,*,#2760,.F.);
#3869=ORIENTED_EDGE('',*,*,#2761,.F.);
#3870=ORIENTED_EDGE('',*,*,#2762,.F.);
#3871=ORIENTED_EDGE('',*,*,#2763,.F.);
#3872=ORIENTED_EDGE('',*,*,#2764,.F.);
#3873=ORIENTED_EDGE('',*,*,#2765,.F.);
#3874=ORIENTED_EDGE('',*,*,#2766,.F.);
#3875=ORIENTED_EDGE('',*,*,#2767,.F.);
#3876=ORIENTED_EDGE('',*,*,#2768,.F.);
#3877=ORIENTED_EDGE('',*,*,#2769,.F.);
#3878=ORIENTED_EDGE('',*,*,#2770,.F.);
#3879=ORIENTED_EDGE('',*,*,#2771,.F.);
#3880=ORIENTED_EDGE('',*,*,#2772,.F.);
#3881=ORIENTED_EDGE('',*,*,#2773,.F.);
#3882=ORIENTED_EDGE('',*,*,#2774,.F.);
#3883=ORIENTED_EDGE('',*,*,#2775,.F.);
#3884=ORIENTED_EDGE('',*,*,#2776,.F.);
#3885=ORIENTED_EDGE('',*,*,#2777,.F.);
#3886=ORIENTED_EDGE('',*,*,#2778,.F.);
#3887=ORIENTED_EDGE('',*,*,#2779,.F.);
#3888=ORIENTED_EDGE('',*,*,#2780,.F.);
#3889=ORIENTED_EDGE('',*,*,#2781,.F.);
#3890=ORIENTED_EDGE('',*,*,#2782,.F.);
#3891=ORIENTED_EDGE('',*,*,#2783,.F.);
#3892=ORIENTED_EDGE('',*,*,#2784,.F.);
#3893=ORIENTED_EDGE('',*,*,#2785,.F.);
#3894=ORIENTED_EDGE('',*,*,#2786,.F.);
#3895=ORIENTED_EDGE('',*,*,#2787,.F.);
#3896=ORIENTED_EDGE('',*,*,#2788,.F.);
#3897=ORIENTED_EDGE('',*,*,#2789,.F.);
#3898=ORIENTED_EDGE('',*,*,#2790,.F.);
#3899=ORIENTED_EDGE('',*,*,#2791,.F.);
#3900=ORIENTED_EDGE('',*,*,#2792,.F.);
#3901=ORIENTED_EDGE('',*,*,#2793,.F.);
#3902=ORIENTED_EDGE('',*,*,#2794,.F.);
#3903=ORIENTED_EDGE('',*,*,#2795,.F.);
#3904=ORIENTED_EDGE('',*,*,#2796,.F.);
#3905=ORIENTED_EDGE('',*,*,#2797,.F.);
#3906=ORIENTED_EDGE('',*,*,#2798,.F.);
#3907=ORIENTED_EDGE('',*,*,#2799,.F.);
#3908=ORIENTED_EDGE('',*,*,#2800,.F.);
#3909=ORIENTED_EDGE('',*,*,#2801,.F.);
#3910=ORIENTED_EDGE('',*,*,#2802,.F.);
#3911=ORIENTED_EDGE('',*,*,#2803,.F.);
#3912=ORIENTED_EDGE('',*,*,#2804,.F.);
#3913=ORIENTED_EDGE('',*,*,#2805,.F.);
#3914=ORIENTED_EDGE('',*,*,#2806,.F.);
#3915=ORIENTED_EDGE('',*,*,#2807,.F.);
#3916=ORIENTED_EDGE('',*,*,#2808,.F.);
#3917=ORIENTED_EDGE('',*,*,#2809,.F.);
#3918=ORIENTED_EDGE('',*,*,#2810,.F.);
#3919=ORIENTED_EDGE('',*,*,#2811,.F.);
#3920=ORIENTED_EDGE('',*,*,#2812,.F.);
#3921=ORIENTED_EDGE('',*,*,#2813,.F.);
#3922=ORIENTED_EDGE('',*,*,#2814,.F.);
#3923=ORIENTED_EDGE('',*,*,#2815,.F.);
#3924=ORIENTED_EDGE('',*,*,#2816,.F.);
#3925=ORIENTED_EDGE('',*,*,#2817,.F.);
#3926=ORIENTED_EDGE('',*,*,#2818,.F.);
#3927=ORIENTED_EDGE('',*,*,#2819,.F.);
#3928=ORIENTED_EDGE('',*,*,#2820,.F.);
#3929=ORIENTED_EDGE('',*,*,#2821,.F.);
#3930=ORIENTED_EDGE('',*,*,#2822,.F.);
#3931=ORIENTED_EDGE('',*,*,#2823,.F.);
#3932=ORIENTED_EDGE('',*,*,#2824,.F.);
#3933=ORIENTED_EDGE('',*,*,#2825,.F.);
#3934=ORIENTED_EDGE('',*,*,#2826,.F.);
#3935=ORIENTED_EDGE('',*,*,#2827,.T.);
#3936=ORIENTED_EDGE('',*,*,#2828,.T.);
#3937=ORIENTED_EDGE('',*,*,#2829,.T.);
#3938=ORIENTED_EDGE('',*,*,#2830,.T.);
#3939=ORIENTED_EDGE('',*,*,#2831,.T.);
#3940=ORIENTED_EDGE('',*,*,#2832,.T.);
#3941=ORIENTED_EDGE('',*,*,#2833,.T.);
#3942=ORIENTED_EDGE('',*,*,#2834,.T.);
#3943=ORIENTED_EDGE('',*,*,#2835,.T.);
#3944=ORIENTED_EDGE('',*,*,#2836,.T.);
#3945=ORIENTED_EDGE('',*,*,#2837,.T.);
#3946=ORIENTED_EDGE('',*,*,#2838,.T.);
#3947=ORIENTED_EDGE('',*,*,#2839,.T.);
#3948=ORIENTED_EDGE('',*,*,#2840,.T.);
#3949=ORIENTED_EDGE('',*,*,#2841,.T.);
#3950=ORIENTED_EDGE('',*,*,#2842,.T.);
#3951=ORIENTED_EDGE('',*,*,#2843,.T.);
#3952=ORIENTED_EDGE('',*,*,#2844,.T.);
#3953=ORIENTED_EDGE('',*,*,#2845,.T.);
#3954=ORIENTED_EDGE('',*,*,#2846,.T.);
#3955=ORIENTED_EDGE('',*,*,#2847,.T.);
#3956=ORIENTED_EDGE('',*,*,#2848,.T.);
#3957=ORIENTED_EDGE('',*,*,#2849,.T.);
#3958=ORIENTED_EDGE('',*,*,#2850,.T.);
#3959=ORIENTED_EDGE('',*,*,#2851,.T.);
#3960=ORIENTED_EDGE('',*,*,#2852,.T.);
#3961=ORIENTED_EDGE('',*,*,#2853,.T.);
#3962=ORIENTED_EDGE('',*,*,#2854,.T.);
#3963=ORIENTED_EDGE('',*,*,#2855,.T.);
#3964=ORIENTED_EDGE('',*,*,#2856,.T.);
#3965=ORIENTED_EDGE('',*,*,#2857,.T.);
#3966=ORIENTED_EDGE('',*,*,#2858,.T.);
#3967=ORIENTED_EDGE('',*,*,#2859,.T.);
#3968=ORIENTED_EDGE('',*,*,#2860,.T.);
#3969=ORIENTED_EDGE('',*,*,#2861,.T.);
#3970=ORIENTED_EDGE('',*,*,#2862,.T.);
#3971=ORIENTED_EDGE('',*,*,#2863,.T.);
#3972=ORIENTED_EDGE('',*,*,#2864,.T.);
#3973=ORIENTED_EDGE('',*,*,#2865,.T.);
#3974=ORIENTED_EDGE('',*,*,#2866,.T.);
#3975=ORIENTED_EDGE('',*,*,#2867,.T.);
#3976=ORIENTED_EDGE('',*,*,#2868,.T.);
#3977=ORIENTED_EDGE('',*,*,#2869,.T.);
#3978=ORIENTED_EDGE('',*,*,#2870,.T.);
#3979=ORIENTED_EDGE('',*,*,#2871,.T.);
#3980=ORIENTED_EDGE('',*,*,#2872,.T.);
#3981=ORIENTED_EDGE('',*,*,#2873,.T.);
#3982=ORIENTED_EDGE('',*,*,#2874,.T.);
#3983=ORIENTED_EDGE('',*,*,#2875,.T.);
#3984=ORIENTED_EDGE('',*,*,#2876,.T.);
#3985=ORIENTED_EDGE('',*,*,#2877,.T.);
#3986=ORIENTED_EDGE('',*,*,#2878,.T.);
#3987=ORIENTED_EDGE('',*,*,#2879,.T.);
#3988=ORIENTED_EDGE('',*,*,#2880,.T.);
#3989=ORIENTED_EDGE('',*,*,#2881,.T.);
#3990=ORIENTED_EDGE('',*,*,#2882,.T.);
#3991=ORIENTED_EDGE('',*,*,#2883,.T.);
#3992=ORIENTED_EDGE('',*,*,#2884,.T.);
#3993=ORIENTED_EDGE('',*,*,#2885,.T.);
#3994=ORIENTED_EDGE('',*,*,#2886,.T.);
#3995=ORIENTED_EDGE('',*,*,#2887,.T.);
#3996=ORIENTED_EDGE('',*,*,#2888,.T.);
#3997=ORIENTED_EDGE('',*,*,#2889,.T.);
#3998=ORIENTED_EDGE('',*,*,#2890,.T.);
#3999=ORIENTED_EDGE('',*,*,#2891,.T.);
#4000=ORIENTED_EDGE('',*,*,#2892,.T.);
#4001=ORIENTED_EDGE('',*,*,#2893,.T.);
#4002=ORIENTED_EDGE('',*,*,#2894,.T.);
#4003=ORIENTED_EDGE('',*,*,#2895,.T.);
#4004=ORIENTED_EDGE('',*,*,#2896,.T.);
#4005=ORIENTED_EDGE('',*,*,#2897,.T.);
#4006=ORIENTED_EDGE('',*,*,#2898,.T.);
#4007=ORIENTED_EDGE('',*,*,#2899,.T.);
#4008=ORIENTED_EDGE('',*,*,#2900,.T.);
#4009=ORIENTED_EDGE('',*,*,#2901,.T.);
#4010=ORIENTED_EDGE('',*,*,#2902,.T.);
#4011=ORIENTED_EDGE('',*,*,#2903,.T.);
#4012=ORIENTED_EDGE('',*,*,#2904,.T.);
#4013=ORIENTED_EDGE('',*,*,#2905,.T.);
#4014=ORIENTED_EDGE('',*,*,#2906,.T.);
#4015=ORIENTED_EDGE('',*,*,#2907,.T.);
#4016=ORIENTED_EDGE('',*,*,#2908,.T.);
#4017=ORIENTED_EDGE('',*,*,#2909,.T.);
#4018=ORIENTED_EDGE('',*,*,#2910,.T.);
#4019=ORIENTED_EDGE('',*,*,#2911,.T.);
#4020=ORIENTED_EDGE('',*,*,#2912,.T.);
#4021=ORIENTED_EDGE('',*,*,#2913,.T.);
#4022=ORIENTED_EDGE('',*,*,#2914,.T.);
#4023=ORIENTED_EDGE('',*,*,#2915,.T.);
#4024=ORIENTED_EDGE('',*,*,#2916,.T.);
#4025=ORIENTED_EDGE('',*,*,#2917,.T.);
#4026=ORIENTED_EDGE('',*,*,#2918,.T.);
#4027=ORIENTED_EDGE('',*,*,#2919,.T.);
#4028=ORIENTED_EDGE('',*,*,#2920,.T.);
#4029=ORIENTED_EDGE('',*,*,#2921,.T.);
#4030=ORIENTED_EDGE('',*,*,#2922,.T.);
#4031=ORIENTED_EDGE('',*,*,#2923,.T.);
#4032=ORIENTED_EDGE('',*,*,#2924,.T.);
#4033=ORIENTED_EDGE('',*,*,#2925,.T.);
#4034=ORIENTED_EDGE('',*,*,#2926,.T.);
#4035=ORIENTED_EDGE('',*,*,#2927,.T.);
#4036=ORIENTED_EDGE('',*,*,#2928,.T.);
#4037=ORIENTED_EDGE('',*,*,#2929,.T.);
#4038=ORIENTED_EDGE('',*,*,#2930,.T.);
#4039=ORIENTED_EDGE('',*,*,#2931,.F.);
#4040=ORIENTED_EDGE('',*,*,#2932,.F.);
#4041=ORIENTED_EDGE('',*,*,#2933,.F.);
#4042=ORIENTED_EDGE('',*,*,#2934,.F.);
#4043=ORIENTED_EDGE('',*,*,#2935,.F.);
#4044=ORIENTED_EDGE('',*,*,#2936,.F.);
#4045=ORIENTED_EDGE('',*,*,#2930,.F.);
#4046=ORIENTED_EDGE('',*,*,#2937,.T.);
#4047=ORIENTED_EDGE('',*,*,#2938,.T.);
#4048=ORIENTED_EDGE('',*,*,#2937,.F.);
#4049=ORIENTED_EDGE('',*,*,#2934,.T.);
#4050=ORIENTED_EDGE('',*,*,#2939,.T.);
#4051=ORIENTED_EDGE('',*,*,#2940,.F.);
#4052=ORIENTED_EDGE('',*,*,#2941,.F.);
#4053=ORIENTED_EDGE('',*,*,#2933,.T.);
#4054=ORIENTED_EDGE('',*,*,#2942,.T.);
#4055=ORIENTED_EDGE('',*,*,#2943,.F.);
#4056=ORIENTED_EDGE('',*,*,#2939,.F.);
#4057=ORIENTED_EDGE('',*,*,#2932,.T.);
#4058=ORIENTED_EDGE('',*,*,#2944,.T.);
#4059=ORIENTED_EDGE('',*,*,#2945,.F.);
#4060=ORIENTED_EDGE('',*,*,#2942,.F.);
#4061=ORIENTED_EDGE('',*,*,#2938,.F.);
#4062=ORIENTED_EDGE('',*,*,#2946,.T.);
#4063=ORIENTED_EDGE('',*,*,#2511,.T.);
#4064=ORIENTED_EDGE('',*,*,#2947,.T.);
#4065=ORIENTED_EDGE('',*,*,#2948,.T.);
#4066=ORIENTED_EDGE('',*,*,#2949,.T.);
#4067=ORIENTED_EDGE('',*,*,#2826,.T.);
#4068=ORIENTED_EDGE('',*,*,#2950,.T.);
#4069=ORIENTED_EDGE('',*,*,#2931,.T.);
#4070=ORIENTED_EDGE('',*,*,#2951,.T.);
#4071=ORIENTED_EDGE('',*,*,#2952,.F.);
#4072=ORIENTED_EDGE('',*,*,#2944,.F.);
#4073=ORIENTED_EDGE('',*,*,#2935,.T.);
#4074=ORIENTED_EDGE('',*,*,#2941,.T.);
#4075=ORIENTED_EDGE('',*,*,#2953,.F.);
#4076=ORIENTED_EDGE('',*,*,#2954,.F.);
#4077=ORIENTED_EDGE('',*,*,#2936,.T.);
#4078=ORIENTED_EDGE('',*,*,#2954,.T.);
#4079=ORIENTED_EDGE('',*,*,#2955,.F.);
#4080=ORIENTED_EDGE('',*,*,#2951,.F.);
#4081=ORIENTED_EDGE('',*,*,#2955,.T.);
#4082=ORIENTED_EDGE('',*,*,#2953,.T.);
#4083=ORIENTED_EDGE('',*,*,#2940,.T.);
#4084=ORIENTED_EDGE('',*,*,#2943,.T.);
#4085=ORIENTED_EDGE('',*,*,#2945,.T.);
#4086=ORIENTED_EDGE('',*,*,#2952,.T.);
#4087=ORIENTED_EDGE('',*,*,#2956,.F.);
#4088=ORIENTED_EDGE('',*,*,#2615,.F.);
#4089=ORIENTED_EDGE('',*,*,#2614,.F.);
#4090=ORIENTED_EDGE('',*,*,#2613,.F.);
#4091=ORIENTED_EDGE('',*,*,#2612,.F.);
#4092=ORIENTED_EDGE('',*,*,#2611,.F.);
#4093=ORIENTED_EDGE('',*,*,#2610,.F.);
#4094=ORIENTED_EDGE('',*,*,#2609,.F.);
#4095=ORIENTED_EDGE('',*,*,#2608,.F.);
#4096=ORIENTED_EDGE('',*,*,#2607,.F.);
#4097=ORIENTED_EDGE('',*,*,#2606,.F.);
#4098=ORIENTED_EDGE('',*,*,#2605,.F.);
#4099=ORIENTED_EDGE('',*,*,#2604,.F.);
#4100=ORIENTED_EDGE('',*,*,#2603,.F.);
#4101=ORIENTED_EDGE('',*,*,#2602,.F.);
#4102=ORIENTED_EDGE('',*,*,#2601,.F.);
#4103=ORIENTED_EDGE('',*,*,#2600,.F.);
#4104=ORIENTED_EDGE('',*,*,#2599,.F.);
#4105=ORIENTED_EDGE('',*,*,#2598,.F.);
#4106=ORIENTED_EDGE('',*,*,#2597,.F.);
#4107=ORIENTED_EDGE('',*,*,#2596,.F.);
#4108=ORIENTED_EDGE('',*,*,#2595,.F.);
#4109=ORIENTED_EDGE('',*,*,#2594,.F.);
#4110=ORIENTED_EDGE('',*,*,#2593,.F.);
#4111=ORIENTED_EDGE('',*,*,#2592,.F.);
#4112=ORIENTED_EDGE('',*,*,#2591,.F.);
#4113=ORIENTED_EDGE('',*,*,#2590,.F.);
#4114=ORIENTED_EDGE('',*,*,#2589,.F.);
#4115=ORIENTED_EDGE('',*,*,#2588,.F.);
#4116=ORIENTED_EDGE('',*,*,#2587,.F.);
#4117=ORIENTED_EDGE('',*,*,#2586,.F.);
#4118=ORIENTED_EDGE('',*,*,#2585,.F.);
#4119=ORIENTED_EDGE('',*,*,#2584,.F.);
#4120=ORIENTED_EDGE('',*,*,#2583,.F.);
#4121=ORIENTED_EDGE('',*,*,#2582,.F.);
#4122=ORIENTED_EDGE('',*,*,#2581,.F.);
#4123=ORIENTED_EDGE('',*,*,#2580,.F.);
#4124=ORIENTED_EDGE('',*,*,#2579,.F.);
#4125=ORIENTED_EDGE('',*,*,#2578,.F.);
#4126=ORIENTED_EDGE('',*,*,#2577,.F.);
#4127=ORIENTED_EDGE('',*,*,#2576,.F.);
#4128=ORIENTED_EDGE('',*,*,#2575,.F.);
#4129=ORIENTED_EDGE('',*,*,#2574,.F.);
#4130=ORIENTED_EDGE('',*,*,#2573,.F.);
#4131=ORIENTED_EDGE('',*,*,#2572,.F.);
#4132=ORIENTED_EDGE('',*,*,#2571,.F.);
#4133=ORIENTED_EDGE('',*,*,#2570,.F.);
#4134=ORIENTED_EDGE('',*,*,#2569,.F.);
#4135=ORIENTED_EDGE('',*,*,#2568,.F.);
#4136=ORIENTED_EDGE('',*,*,#2567,.F.);
#4137=ORIENTED_EDGE('',*,*,#2566,.F.);
#4138=ORIENTED_EDGE('',*,*,#2565,.F.);
#4139=ORIENTED_EDGE('',*,*,#2564,.F.);
#4140=ORIENTED_EDGE('',*,*,#2563,.F.);
#4141=ORIENTED_EDGE('',*,*,#2562,.F.);
#4142=ORIENTED_EDGE('',*,*,#2561,.F.);
#4143=ORIENTED_EDGE('',*,*,#2560,.F.);
#4144=ORIENTED_EDGE('',*,*,#2559,.F.);
#4145=ORIENTED_EDGE('',*,*,#2558,.F.);
#4146=ORIENTED_EDGE('',*,*,#2557,.F.);
#4147=ORIENTED_EDGE('',*,*,#2556,.F.);
#4148=ORIENTED_EDGE('',*,*,#2555,.F.);
#4149=ORIENTED_EDGE('',*,*,#2554,.F.);
#4150=ORIENTED_EDGE('',*,*,#2553,.F.);
#4151=ORIENTED_EDGE('',*,*,#2552,.F.);
#4152=ORIENTED_EDGE('',*,*,#2551,.F.);
#4153=ORIENTED_EDGE('',*,*,#2550,.F.);
#4154=ORIENTED_EDGE('',*,*,#2549,.F.);
#4155=ORIENTED_EDGE('',*,*,#2548,.F.);
#4156=ORIENTED_EDGE('',*,*,#2547,.F.);
#4157=ORIENTED_EDGE('',*,*,#2546,.F.);
#4158=ORIENTED_EDGE('',*,*,#2545,.F.);
#4159=ORIENTED_EDGE('',*,*,#2544,.F.);
#4160=ORIENTED_EDGE('',*,*,#2543,.F.);
#4161=ORIENTED_EDGE('',*,*,#2542,.F.);
#4162=ORIENTED_EDGE('',*,*,#2541,.F.);
#4163=ORIENTED_EDGE('',*,*,#2540,.F.);
#4164=ORIENTED_EDGE('',*,*,#2539,.F.);
#4165=ORIENTED_EDGE('',*,*,#2538,.F.);
#4166=ORIENTED_EDGE('',*,*,#2537,.F.);
#4167=ORIENTED_EDGE('',*,*,#2536,.F.);
#4168=ORIENTED_EDGE('',*,*,#2535,.F.);
#4169=ORIENTED_EDGE('',*,*,#2534,.F.);
#4170=ORIENTED_EDGE('',*,*,#2533,.F.);
#4171=ORIENTED_EDGE('',*,*,#2532,.F.);
#4172=ORIENTED_EDGE('',*,*,#2531,.F.);
#4173=ORIENTED_EDGE('',*,*,#2530,.F.);
#4174=ORIENTED_EDGE('',*,*,#2529,.F.);
#4175=ORIENTED_EDGE('',*,*,#2528,.F.);
#4176=ORIENTED_EDGE('',*,*,#2527,.F.);
#4177=ORIENTED_EDGE('',*,*,#2526,.F.);
#4178=ORIENTED_EDGE('',*,*,#2525,.F.);
#4179=ORIENTED_EDGE('',*,*,#2524,.F.);
#4180=ORIENTED_EDGE('',*,*,#2523,.F.);
#4181=ORIENTED_EDGE('',*,*,#2522,.F.);
#4182=ORIENTED_EDGE('',*,*,#2521,.F.);
#4183=ORIENTED_EDGE('',*,*,#2520,.F.);
#4184=ORIENTED_EDGE('',*,*,#2519,.F.);
#4185=ORIENTED_EDGE('',*,*,#2518,.F.);
#4186=ORIENTED_EDGE('',*,*,#2517,.F.);
#4187=ORIENTED_EDGE('',*,*,#2516,.F.);
#4188=ORIENTED_EDGE('',*,*,#2515,.F.);
#4189=ORIENTED_EDGE('',*,*,#2514,.F.);
#4190=ORIENTED_EDGE('',*,*,#2513,.F.);
#4191=ORIENTED_EDGE('',*,*,#2512,.F.);
#4192=ORIENTED_EDGE('',*,*,#2946,.F.);
#4193=ORIENTED_EDGE('',*,*,#2950,.F.);
#4194=ORIENTED_EDGE('',*,*,#2825,.T.);
#4195=ORIENTED_EDGE('',*,*,#2824,.T.);
#4196=ORIENTED_EDGE('',*,*,#2823,.T.);
#4197=ORIENTED_EDGE('',*,*,#2822,.T.);
#4198=ORIENTED_EDGE('',*,*,#2821,.T.);
#4199=ORIENTED_EDGE('',*,*,#2820,.T.);
#4200=ORIENTED_EDGE('',*,*,#2819,.T.);
#4201=ORIENTED_EDGE('',*,*,#2818,.T.);
#4202=ORIENTED_EDGE('',*,*,#2817,.T.);
#4203=ORIENTED_EDGE('',*,*,#2816,.T.);
#4204=ORIENTED_EDGE('',*,*,#2815,.T.);
#4205=ORIENTED_EDGE('',*,*,#2814,.T.);
#4206=ORIENTED_EDGE('',*,*,#2813,.T.);
#4207=ORIENTED_EDGE('',*,*,#2812,.T.);
#4208=ORIENTED_EDGE('',*,*,#2811,.T.);
#4209=ORIENTED_EDGE('',*,*,#2810,.T.);
#4210=ORIENTED_EDGE('',*,*,#2809,.T.);
#4211=ORIENTED_EDGE('',*,*,#2808,.T.);
#4212=ORIENTED_EDGE('',*,*,#2807,.T.);
#4213=ORIENTED_EDGE('',*,*,#2806,.T.);
#4214=ORIENTED_EDGE('',*,*,#2805,.T.);
#4215=ORIENTED_EDGE('',*,*,#2804,.T.);
#4216=ORIENTED_EDGE('',*,*,#2803,.T.);
#4217=ORIENTED_EDGE('',*,*,#2802,.T.);
#4218=ORIENTED_EDGE('',*,*,#2801,.T.);
#4219=ORIENTED_EDGE('',*,*,#2800,.T.);
#4220=ORIENTED_EDGE('',*,*,#2799,.T.);
#4221=ORIENTED_EDGE('',*,*,#2798,.T.);
#4222=ORIENTED_EDGE('',*,*,#2797,.T.);
#4223=ORIENTED_EDGE('',*,*,#2796,.T.);
#4224=ORIENTED_EDGE('',*,*,#2795,.T.);
#4225=ORIENTED_EDGE('',*,*,#2794,.T.);
#4226=ORIENTED_EDGE('',*,*,#2793,.T.);
#4227=ORIENTED_EDGE('',*,*,#2792,.T.);
#4228=ORIENTED_EDGE('',*,*,#2791,.T.);
#4229=ORIENTED_EDGE('',*,*,#2790,.T.);
#4230=ORIENTED_EDGE('',*,*,#2789,.T.);
#4231=ORIENTED_EDGE('',*,*,#2788,.T.);
#4232=ORIENTED_EDGE('',*,*,#2787,.T.);
#4233=ORIENTED_EDGE('',*,*,#2786,.T.);
#4234=ORIENTED_EDGE('',*,*,#2785,.T.);
#4235=ORIENTED_EDGE('',*,*,#2784,.T.);
#4236=ORIENTED_EDGE('',*,*,#2783,.T.);
#4237=ORIENTED_EDGE('',*,*,#2782,.T.);
#4238=ORIENTED_EDGE('',*,*,#2781,.T.);
#4239=ORIENTED_EDGE('',*,*,#2780,.T.);
#4240=ORIENTED_EDGE('',*,*,#2779,.T.);
#4241=ORIENTED_EDGE('',*,*,#2778,.T.);
#4242=ORIENTED_EDGE('',*,*,#2777,.T.);
#4243=ORIENTED_EDGE('',*,*,#2776,.T.);
#4244=ORIENTED_EDGE('',*,*,#2775,.T.);
#4245=ORIENTED_EDGE('',*,*,#2774,.T.);
#4246=ORIENTED_EDGE('',*,*,#2773,.T.);
#4247=ORIENTED_EDGE('',*,*,#2772,.T.);
#4248=ORIENTED_EDGE('',*,*,#2771,.T.);
#4249=ORIENTED_EDGE('',*,*,#2770,.T.);
#4250=ORIENTED_EDGE('',*,*,#2769,.T.);
#4251=ORIENTED_EDGE('',*,*,#2768,.T.);
#4252=ORIENTED_EDGE('',*,*,#2767,.T.);
#4253=ORIENTED_EDGE('',*,*,#2766,.T.);
#4254=ORIENTED_EDGE('',*,*,#2765,.T.);
#4255=ORIENTED_EDGE('',*,*,#2764,.T.);
#4256=ORIENTED_EDGE('',*,*,#2763,.T.);
#4257=ORIENTED_EDGE('',*,*,#2762,.T.);
#4258=ORIENTED_EDGE('',*,*,#2761,.T.);
#4259=ORIENTED_EDGE('',*,*,#2760,.T.);
#4260=ORIENTED_EDGE('',*,*,#2759,.T.);
#4261=ORIENTED_EDGE('',*,*,#2758,.T.);
#4262=ORIENTED_EDGE('',*,*,#2757,.T.);
#4263=ORIENTED_EDGE('',*,*,#2756,.T.);
#4264=ORIENTED_EDGE('',*,*,#2755,.T.);
#4265=ORIENTED_EDGE('',*,*,#2754,.T.);
#4266=ORIENTED_EDGE('',*,*,#2753,.T.);
#4267=ORIENTED_EDGE('',*,*,#2752,.T.);
#4268=ORIENTED_EDGE('',*,*,#2751,.T.);
#4269=ORIENTED_EDGE('',*,*,#2750,.T.);
#4270=ORIENTED_EDGE('',*,*,#2749,.T.);
#4271=ORIENTED_EDGE('',*,*,#2748,.T.);
#4272=ORIENTED_EDGE('',*,*,#2747,.T.);
#4273=ORIENTED_EDGE('',*,*,#2746,.T.);
#4274=ORIENTED_EDGE('',*,*,#2745,.T.);
#4275=ORIENTED_EDGE('',*,*,#2744,.T.);
#4276=ORIENTED_EDGE('',*,*,#2743,.T.);
#4277=ORIENTED_EDGE('',*,*,#2742,.T.);
#4278=ORIENTED_EDGE('',*,*,#2741,.T.);
#4279=ORIENTED_EDGE('',*,*,#2740,.T.);
#4280=ORIENTED_EDGE('',*,*,#2739,.T.);
#4281=ORIENTED_EDGE('',*,*,#2738,.T.);
#4282=ORIENTED_EDGE('',*,*,#2737,.T.);
#4283=ORIENTED_EDGE('',*,*,#2736,.T.);
#4284=ORIENTED_EDGE('',*,*,#2735,.T.);
#4285=ORIENTED_EDGE('',*,*,#2734,.T.);
#4286=ORIENTED_EDGE('',*,*,#2733,.T.);
#4287=ORIENTED_EDGE('',*,*,#2732,.T.);
#4288=ORIENTED_EDGE('',*,*,#2731,.T.);
#4289=ORIENTED_EDGE('',*,*,#2730,.T.);
#4290=ORIENTED_EDGE('',*,*,#2729,.T.);
#4291=ORIENTED_EDGE('',*,*,#2728,.T.);
#4292=ORIENTED_EDGE('',*,*,#2727,.T.);
#4293=ORIENTED_EDGE('',*,*,#2726,.T.);
#4294=ORIENTED_EDGE('',*,*,#2725,.T.);
#4295=ORIENTED_EDGE('',*,*,#2724,.T.);
#4296=ORIENTED_EDGE('',*,*,#2723,.T.);
#4297=ORIENTED_EDGE('',*,*,#2722,.T.);
#4298=ORIENTED_EDGE('',*,*,#2957,.F.);
#4299=ORIENTED_EDGE('',*,*,#2720,.F.);
#4300=ORIENTED_EDGE('',*,*,#2929,.F.);
#4301=ORIENTED_EDGE('',*,*,#2928,.F.);
#4302=ORIENTED_EDGE('',*,*,#2927,.F.);
#4303=ORIENTED_EDGE('',*,*,#2926,.F.);
#4304=ORIENTED_EDGE('',*,*,#2925,.F.);
#4305=ORIENTED_EDGE('',*,*,#2924,.F.);
#4306=ORIENTED_EDGE('',*,*,#2923,.F.);
#4307=ORIENTED_EDGE('',*,*,#2922,.F.);
#4308=ORIENTED_EDGE('',*,*,#2921,.F.);
#4309=ORIENTED_EDGE('',*,*,#2920,.F.);
#4310=ORIENTED_EDGE('',*,*,#2919,.F.);
#4311=ORIENTED_EDGE('',*,*,#2918,.F.);
#4312=ORIENTED_EDGE('',*,*,#2917,.F.);
#4313=ORIENTED_EDGE('',*,*,#2916,.F.);
#4314=ORIENTED_EDGE('',*,*,#2915,.F.);
#4315=ORIENTED_EDGE('',*,*,#2914,.F.);
#4316=ORIENTED_EDGE('',*,*,#2913,.F.);
#4317=ORIENTED_EDGE('',*,*,#2912,.F.);
#4318=ORIENTED_EDGE('',*,*,#2911,.F.);
#4319=ORIENTED_EDGE('',*,*,#2910,.F.);
#4320=ORIENTED_EDGE('',*,*,#2909,.F.);
#4321=ORIENTED_EDGE('',*,*,#2908,.F.);
#4322=ORIENTED_EDGE('',*,*,#2907,.F.);
#4323=ORIENTED_EDGE('',*,*,#2906,.F.);
#4324=ORIENTED_EDGE('',*,*,#2905,.F.);
#4325=ORIENTED_EDGE('',*,*,#2904,.F.);
#4326=ORIENTED_EDGE('',*,*,#2903,.F.);
#4327=ORIENTED_EDGE('',*,*,#2902,.F.);
#4328=ORIENTED_EDGE('',*,*,#2901,.F.);
#4329=ORIENTED_EDGE('',*,*,#2900,.F.);
#4330=ORIENTED_EDGE('',*,*,#2899,.F.);
#4331=ORIENTED_EDGE('',*,*,#2898,.F.);
#4332=ORIENTED_EDGE('',*,*,#2897,.F.);
#4333=ORIENTED_EDGE('',*,*,#2896,.F.);
#4334=ORIENTED_EDGE('',*,*,#2895,.F.);
#4335=ORIENTED_EDGE('',*,*,#2894,.F.);
#4336=ORIENTED_EDGE('',*,*,#2893,.F.);
#4337=ORIENTED_EDGE('',*,*,#2892,.F.);
#4338=ORIENTED_EDGE('',*,*,#2891,.F.);
#4339=ORIENTED_EDGE('',*,*,#2890,.F.);
#4340=ORIENTED_EDGE('',*,*,#2889,.F.);
#4341=ORIENTED_EDGE('',*,*,#2888,.F.);
#4342=ORIENTED_EDGE('',*,*,#2887,.F.);
#4343=ORIENTED_EDGE('',*,*,#2886,.F.);
#4344=ORIENTED_EDGE('',*,*,#2885,.F.);
#4345=ORIENTED_EDGE('',*,*,#2884,.F.);
#4346=ORIENTED_EDGE('',*,*,#2883,.F.);
#4347=ORIENTED_EDGE('',*,*,#2882,.F.);
#4348=ORIENTED_EDGE('',*,*,#2881,.F.);
#4349=ORIENTED_EDGE('',*,*,#2880,.F.);
#4350=ORIENTED_EDGE('',*,*,#2879,.F.);
#4351=ORIENTED_EDGE('',*,*,#2878,.F.);
#4352=ORIENTED_EDGE('',*,*,#2877,.F.);
#4353=ORIENTED_EDGE('',*,*,#2876,.F.);
#4354=ORIENTED_EDGE('',*,*,#2875,.F.);
#4355=ORIENTED_EDGE('',*,*,#2874,.F.);
#4356=ORIENTED_EDGE('',*,*,#2873,.F.);
#4357=ORIENTED_EDGE('',*,*,#2872,.F.);
#4358=ORIENTED_EDGE('',*,*,#2871,.F.);
#4359=ORIENTED_EDGE('',*,*,#2870,.F.);
#4360=ORIENTED_EDGE('',*,*,#2869,.F.);
#4361=ORIENTED_EDGE('',*,*,#2868,.F.);
#4362=ORIENTED_EDGE('',*,*,#2867,.F.);
#4363=ORIENTED_EDGE('',*,*,#2866,.F.);
#4364=ORIENTED_EDGE('',*,*,#2865,.F.);
#4365=ORIENTED_EDGE('',*,*,#2864,.F.);
#4366=ORIENTED_EDGE('',*,*,#2863,.F.);
#4367=ORIENTED_EDGE('',*,*,#2862,.F.);
#4368=ORIENTED_EDGE('',*,*,#2861,.F.);
#4369=ORIENTED_EDGE('',*,*,#2860,.F.);
#4370=ORIENTED_EDGE('',*,*,#2859,.F.);
#4371=ORIENTED_EDGE('',*,*,#2858,.F.);
#4372=ORIENTED_EDGE('',*,*,#2857,.F.);
#4373=ORIENTED_EDGE('',*,*,#2856,.F.);
#4374=ORIENTED_EDGE('',*,*,#2855,.F.);
#4375=ORIENTED_EDGE('',*,*,#2854,.F.);
#4376=ORIENTED_EDGE('',*,*,#2853,.F.);
#4377=ORIENTED_EDGE('',*,*,#2852,.F.);
#4378=ORIENTED_EDGE('',*,*,#2851,.F.);
#4379=ORIENTED_EDGE('',*,*,#2850,.F.);
#4380=ORIENTED_EDGE('',*,*,#2849,.F.);
#4381=ORIENTED_EDGE('',*,*,#2848,.F.);
#4382=ORIENTED_EDGE('',*,*,#2847,.F.);
#4383=ORIENTED_EDGE('',*,*,#2846,.F.);
#4384=ORIENTED_EDGE('',*,*,#2845,.F.);
#4385=ORIENTED_EDGE('',*,*,#2844,.F.);
#4386=ORIENTED_EDGE('',*,*,#2843,.F.);
#4387=ORIENTED_EDGE('',*,*,#2842,.F.);
#4388=ORIENTED_EDGE('',*,*,#2841,.F.);
#4389=ORIENTED_EDGE('',*,*,#2840,.F.);
#4390=ORIENTED_EDGE('',*,*,#2839,.F.);
#4391=ORIENTED_EDGE('',*,*,#2838,.F.);
#4392=ORIENTED_EDGE('',*,*,#2837,.F.);
#4393=ORIENTED_EDGE('',*,*,#2836,.F.);
#4394=ORIENTED_EDGE('',*,*,#2835,.F.);
#4395=ORIENTED_EDGE('',*,*,#2834,.F.);
#4396=ORIENTED_EDGE('',*,*,#2833,.F.);
#4397=ORIENTED_EDGE('',*,*,#2832,.F.);
#4398=ORIENTED_EDGE('',*,*,#2831,.F.);
#4399=ORIENTED_EDGE('',*,*,#2830,.F.);
#4400=ORIENTED_EDGE('',*,*,#2829,.F.);
#4401=ORIENTED_EDGE('',*,*,#2828,.F.);
#4402=ORIENTED_EDGE('',*,*,#2827,.F.);
#4403=ORIENTED_EDGE('',*,*,#2949,.F.);
#4404=ORIENTED_EDGE('',*,*,#2948,.F.);
#4405=ORIENTED_EDGE('',*,*,#2947,.F.);
#4406=ORIENTED_EDGE('',*,*,#2510,.F.);
#4407=ORIENTED_EDGE('',*,*,#2719,.F.);
#4408=ORIENTED_EDGE('',*,*,#2718,.F.);
#4409=ORIENTED_EDGE('',*,*,#2717,.F.);
#4410=ORIENTED_EDGE('',*,*,#2716,.F.);
#4411=ORIENTED_EDGE('',*,*,#2715,.F.);
#4412=ORIENTED_EDGE('',*,*,#2714,.F.);
#4413=ORIENTED_EDGE('',*,*,#2713,.F.);
#4414=ORIENTED_EDGE('',*,*,#2712,.F.);
#4415=ORIENTED_EDGE('',*,*,#2711,.F.);
#4416=ORIENTED_EDGE('',*,*,#2710,.F.);
#4417=ORIENTED_EDGE('',*,*,#2709,.F.);
#4418=ORIENTED_EDGE('',*,*,#2708,.F.);
#4419=ORIENTED_EDGE('',*,*,#2707,.F.);
#4420=ORIENTED_EDGE('',*,*,#2706,.F.);
#4421=ORIENTED_EDGE('',*,*,#2705,.F.);
#4422=ORIENTED_EDGE('',*,*,#2704,.F.);
#4423=ORIENTED_EDGE('',*,*,#2703,.F.);
#4424=ORIENTED_EDGE('',*,*,#2702,.F.);
#4425=ORIENTED_EDGE('',*,*,#2701,.F.);
#4426=ORIENTED_EDGE('',*,*,#2700,.F.);
#4427=ORIENTED_EDGE('',*,*,#2699,.F.);
#4428=ORIENTED_EDGE('',*,*,#2698,.F.);
#4429=ORIENTED_EDGE('',*,*,#2697,.F.);
#4430=ORIENTED_EDGE('',*,*,#2696,.F.);
#4431=ORIENTED_EDGE('',*,*,#2695,.F.);
#4432=ORIENTED_EDGE('',*,*,#2694,.F.);
#4433=ORIENTED_EDGE('',*,*,#2693,.F.);
#4434=ORIENTED_EDGE('',*,*,#2692,.F.);
#4435=ORIENTED_EDGE('',*,*,#2691,.F.);
#4436=ORIENTED_EDGE('',*,*,#2690,.F.);
#4437=ORIENTED_EDGE('',*,*,#2689,.F.);
#4438=ORIENTED_EDGE('',*,*,#2688,.F.);
#4439=ORIENTED_EDGE('',*,*,#2687,.F.);
#4440=ORIENTED_EDGE('',*,*,#2686,.F.);
#4441=ORIENTED_EDGE('',*,*,#2685,.F.);
#4442=ORIENTED_EDGE('',*,*,#2684,.F.);
#4443=ORIENTED_EDGE('',*,*,#2683,.F.);
#4444=ORIENTED_EDGE('',*,*,#2682,.F.);
#4445=ORIENTED_EDGE('',*,*,#2681,.F.);
#4446=ORIENTED_EDGE('',*,*,#2680,.F.);
#4447=ORIENTED_EDGE('',*,*,#2679,.F.);
#4448=ORIENTED_EDGE('',*,*,#2678,.F.);
#4449=ORIENTED_EDGE('',*,*,#2677,.F.);
#4450=ORIENTED_EDGE('',*,*,#2676,.F.);
#4451=ORIENTED_EDGE('',*,*,#2675,.F.);
#4452=ORIENTED_EDGE('',*,*,#2674,.F.);
#4453=ORIENTED_EDGE('',*,*,#2673,.F.);
#4454=ORIENTED_EDGE('',*,*,#2672,.F.);
#4455=ORIENTED_EDGE('',*,*,#2671,.F.);
#4456=ORIENTED_EDGE('',*,*,#2670,.F.);
#4457=ORIENTED_EDGE('',*,*,#2669,.F.);
#4458=ORIENTED_EDGE('',*,*,#2668,.F.);
#4459=ORIENTED_EDGE('',*,*,#2667,.F.);
#4460=ORIENTED_EDGE('',*,*,#2666,.F.);
#4461=ORIENTED_EDGE('',*,*,#2665,.F.);
#4462=ORIENTED_EDGE('',*,*,#2664,.F.);
#4463=ORIENTED_EDGE('',*,*,#2663,.F.);
#4464=ORIENTED_EDGE('',*,*,#2662,.F.);
#4465=ORIENTED_EDGE('',*,*,#2661,.F.);
#4466=ORIENTED_EDGE('',*,*,#2660,.F.);
#4467=ORIENTED_EDGE('',*,*,#2659,.F.);
#4468=ORIENTED_EDGE('',*,*,#2658,.F.);
#4469=ORIENTED_EDGE('',*,*,#2657,.F.);
#4470=ORIENTED_EDGE('',*,*,#2656,.F.);
#4471=ORIENTED_EDGE('',*,*,#2655,.F.);
#4472=ORIENTED_EDGE('',*,*,#2654,.F.);
#4473=ORIENTED_EDGE('',*,*,#2653,.F.);
#4474=ORIENTED_EDGE('',*,*,#2652,.F.);
#4475=ORIENTED_EDGE('',*,*,#2651,.F.);
#4476=ORIENTED_EDGE('',*,*,#2650,.F.);
#4477=ORIENTED_EDGE('',*,*,#2649,.F.);
#4478=ORIENTED_EDGE('',*,*,#2648,.F.);
#4479=ORIENTED_EDGE('',*,*,#2647,.F.);
#4480=ORIENTED_EDGE('',*,*,#2646,.F.);
#4481=ORIENTED_EDGE('',*,*,#2645,.F.);
#4482=ORIENTED_EDGE('',*,*,#2644,.F.);
#4483=ORIENTED_EDGE('',*,*,#2643,.F.);
#4484=ORIENTED_EDGE('',*,*,#2642,.F.);
#4485=ORIENTED_EDGE('',*,*,#2641,.F.);
#4486=ORIENTED_EDGE('',*,*,#2640,.F.);
#4487=ORIENTED_EDGE('',*,*,#2639,.F.);
#4488=ORIENTED_EDGE('',*,*,#2638,.F.);
#4489=ORIENTED_EDGE('',*,*,#2637,.F.);
#4490=ORIENTED_EDGE('',*,*,#2636,.F.);
#4491=ORIENTED_EDGE('',*,*,#2635,.F.);
#4492=ORIENTED_EDGE('',*,*,#2634,.F.);
#4493=ORIENTED_EDGE('',*,*,#2633,.F.);
#4494=ORIENTED_EDGE('',*,*,#2632,.F.);
#4495=ORIENTED_EDGE('',*,*,#2631,.F.);
#4496=ORIENTED_EDGE('',*,*,#2630,.F.);
#4497=ORIENTED_EDGE('',*,*,#2629,.F.);
#4498=ORIENTED_EDGE('',*,*,#2628,.F.);
#4499=ORIENTED_EDGE('',*,*,#2627,.F.);
#4500=ORIENTED_EDGE('',*,*,#2626,.F.);
#4501=ORIENTED_EDGE('',*,*,#2625,.F.);
#4502=ORIENTED_EDGE('',*,*,#2624,.F.);
#4503=ORIENTED_EDGE('',*,*,#2623,.F.);
#4504=ORIENTED_EDGE('',*,*,#2622,.F.);
#4505=ORIENTED_EDGE('',*,*,#2621,.F.);
#4506=ORIENTED_EDGE('',*,*,#2620,.F.);
#4507=ORIENTED_EDGE('',*,*,#2619,.F.);
#4508=ORIENTED_EDGE('',*,*,#2618,.F.);
#4509=ORIENTED_EDGE('',*,*,#2617,.F.);
#4510=ORIENTED_EDGE('',*,*,#2956,.T.);
#4511=ORIENTED_EDGE('',*,*,#2721,.T.);
#4512=ORIENTED_EDGE('',*,*,#2957,.T.);
#4513=ORIENTED_EDGE('',*,*,#2616,.T.);
#4514=CYLINDRICAL_SURFACE('',#4833,7.5);
#4515=CYLINDRICAL_SURFACE('',#4836,7.5);
#4516=CYLINDRICAL_SURFACE('',#4839,7.5);
#4517=CYLINDRICAL_SURFACE('',#4842,7.5);
#4518=CYLINDRICAL_SURFACE('',#4847,3.00000000000002);
#4519=CYLINDRICAL_SURFACE('',#4851,3.00000000000002);
#4520=CYLINDRICAL_SURFACE('',#4854,3.00000000000002);
#4521=CYLINDRICAL_SURFACE('',#4858,3.00000000000002);
#4522=CYLINDRICAL_SURFACE('',#4869,3.00000000000002);
#4523=CYLINDRICAL_SURFACE('',#4872,3.00000000000002);
#4524=CYLINDRICAL_SURFACE('',#4876,3.00000000000002);
#4525=CYLINDRICAL_SURFACE('',#4879,3.00000000000002);
#4526=CYLINDRICAL_SURFACE('',#4884,6.00000000000001);
#4527=CYLINDRICAL_SURFACE('',#4887,6.00000000000001);
#4528=CYLINDRICAL_SURFACE('',#4890,7.5);
#4529=CYLINDRICAL_SURFACE('',#4893,7.5);
#4530=CYLINDRICAL_SURFACE('',#4896,7.5);
#4531=CYLINDRICAL_SURFACE('',#4899,12.);
#4532=CYLINDRICAL_SURFACE('',#4903,12.);
#4533=CYLINDRICAL_SURFACE('',#4909,7.5);
#4534=CYLINDRICAL_SURFACE('',#4916,7.5);
#4535=CYLINDRICAL_SURFACE('',#4920,12.);
#4536=CYLINDRICAL_SURFACE('',#4924,12.);
#4537=CYLINDRICAL_SURFACE('',#4932,6.00000000000001);
#4538=CYLINDRICAL_SURFACE('',#4936,6.00000000000001);
#4539=CYLINDRICAL_SURFACE('',#4939,7.5);
#4540=CYLINDRICAL_SURFACE('',#4943,12.);
#4541=CYLINDRICAL_SURFACE('',#4947,12.);
#4542=CYLINDRICAL_SURFACE('',#4954,7.5);
#4543=CYLINDRICAL_SURFACE('',#4958,7.5);
#4544=CYLINDRICAL_SURFACE('',#4961,6.00000000000001);
#4545=CYLINDRICAL_SURFACE('',#4964,6.);
#4546=CYLINDRICAL_SURFACE('',#4965,7.5);
#4547=CYLINDRICAL_SURFACE('',#4969,12.);
#4548=CYLINDRICAL_SURFACE('',#4973,12.);
#4549=CYLINDRICAL_SURFACE('',#4980,7.5);
#4550=CYLINDRICAL_SURFACE('',#4983,7.5);
#4551=CYLINDRICAL_SURFACE('',#4987,7.5);
#4552=CYLINDRICAL_SURFACE('',#4990,7.5);
#4553=CYLINDRICAL_SURFACE('',#4993,7.5);
#4554=CYLINDRICAL_SURFACE('',#4996,7.5);
#4555=CYLINDRICAL_SURFACE('',#5001,3.00000000000002);
#4556=CYLINDRICAL_SURFACE('',#5005,3.00000000000002);
#4557=CYLINDRICAL_SURFACE('',#5008,3.00000000000002);
#4558=CYLINDRICAL_SURFACE('',#5012,3.00000000000002);
#4559=CYLINDRICAL_SURFACE('',#5023,3.00000000000002);
#4560=CYLINDRICAL_SURFACE('',#5026,3.00000000000002);
#4561=CYLINDRICAL_SURFACE('',#5030,3.00000000000002);
#4562=CYLINDRICAL_SURFACE('',#5033,3.00000000000002);
#4563=CYLINDRICAL_SURFACE('',#5038,6.11325);
#4564=CYLINDRICAL_SURFACE('',#5039,6.11325);
#4565=CYLINDRICAL_SURFACE('',#5041,5.13675);
#4566=CYLINDRICAL_SURFACE('',#5043,5.13675);
#4567=CYLINDRICAL_SURFACE('',#5044,6.11325);
#4568=CYLINDRICAL_SURFACE('',#5047,6.11325);
#4569=CYLINDRICAL_SURFACE('',#5048,6.11325);
#4570=CYLINDRICAL_SURFACE('',#5050,7.5);
#4571=CYLINDRICAL_SURFACE('',#5053,5.13675);
#4572=CYLINDRICAL_SURFACE('',#5054,5.13675);
#4573=CYLINDRICAL_SURFACE('',#5055,6.);
#4574=CYLINDRICAL_SURFACE('',#5066,7.5);
#4575=CYLINDRICAL_SURFACE('',#5070,5.91675);
#4576=CYLINDRICAL_SURFACE('',#5073,4.91825);
#4577=CYLINDRICAL_SURFACE('',#5078,7.);
#4578=ADVANCED_FACE('',(#682),#4514,.F.);
#4579=ADVANCED_FACE('',(#683),#4515,.F.);
#4580=ADVANCED_FACE('',(#684),#4516,.F.);
#4581=ADVANCED_FACE('',(#685),#4517,.F.);
#4582=ADVANCED_FACE('',(#686),#609,.F.);
#4583=ADVANCED_FACE('',(#687),#610,.F.);
#4584=ADVANCED_FACE('',(#688),#4518,.F.);
#4585=ADVANCED_FACE('',(#689,#561,#562),#611,.F.);
#4586=ADVANCED_FACE('',(#690),#4519,.F.);
#4587=ADVANCED_FACE('',(#691),#4520,.T.);
#4588=ADVANCED_FACE('',(#692,#563,#564),#612,.F.);
#4589=ADVANCED_FACE('',(#693),#4521,.T.);
#4590=ADVANCED_FACE('',(#694),#613,.F.);
#4591=ADVANCED_FACE('',(#695),#614,.F.);
#4592=ADVANCED_FACE('',(#696),#615,.T.);
#4593=ADVANCED_FACE('',(#697),#616,.T.);
#4594=ADVANCED_FACE('',(#698),#4522,.F.);
#4595=ADVANCED_FACE('',(#699,#565,#566),#617,.T.);
#4596=ADVANCED_FACE('',(#700),#4523,.F.);
#4597=ADVANCED_FACE('',(#701),#618,.T.);
#4598=ADVANCED_FACE('',(#702),#619,.T.);
#4599=ADVANCED_FACE('',(#703),#4524,.T.);
#4600=ADVANCED_FACE('',(#704,#567,#568),#620,.T.);
#4601=ADVANCED_FACE('',(#705),#4525,.T.);
#4602=ADVANCED_FACE('',(#706),#621,.T.);
#4603=ADVANCED_FACE('',(#707),#622,.T.);
#4604=ADVANCED_FACE('',(#708),#4526,.F.);
#4605=ADVANCED_FACE('',(#709),#4527,.F.);
#4606=ADVANCED_FACE('',(#710),#4528,.T.);
#4607=ADVANCED_FACE('',(#711),#4529,.T.);
#4608=ADVANCED_FACE('',(#712),#4530,.F.);
#4609=ADVANCED_FACE('',(#713),#4531,.T.);
#4610=ADVANCED_FACE('',(#714),#623,.T.);
#4611=ADVANCED_FACE('',(#715),#4532,.T.);
#4612=ADVANCED_FACE('',(#716,#569,#570,#571),#624,.T.);
#4613=ADVANCED_FACE('',(#717,#572,#573,#574),#625,.F.);
#4614=ADVANCED_FACE('',(#718),#4533,.T.);
#4615=ADVANCED_FACE('',(#719),#626,.T.);
#4616=ADVANCED_FACE('',(#720),#627,.F.);
#4617=ADVANCED_FACE('',(#721),#628,.T.);
#4618=ADVANCED_FACE('',(#722),#629,.T.);
#4619=ADVANCED_FACE('',(#723),#630,.T.);
#4620=ADVANCED_FACE('',(#724),#4534,.F.);
#4621=ADVANCED_FACE('',(#725),#631,.F.);
#4622=ADVANCED_FACE('',(#726),#4535,.T.);
#4623=ADVANCED_FACE('',(#727),#632,.F.);
#4624=ADVANCED_FACE('',(#728),#4536,.T.);
#4625=ADVANCED_FACE('',(#729,#575,#576,#577),#633,.F.);
#4626=ADVANCED_FACE('',(#730,#578,#579,#580),#634,.T.);
#4627=ADVANCED_FACE('',(#731),#635,.T.);
#4628=ADVANCED_FACE('',(#732),#4537,.T.);
#4629=ADVANCED_FACE('',(#733),#636,.F.);
#4630=ADVANCED_FACE('',(#734),#4538,.F.);
#4631=ADVANCED_FACE('',(#735),#4539,.F.);
#4632=ADVANCED_FACE('',(#736),#637,.F.);
#4633=ADVANCED_FACE('',(#737),#4540,.T.);
#4634=ADVANCED_FACE('',(#738),#638,.F.);
#4635=ADVANCED_FACE('',(#739),#4541,.T.);
#4636=ADVANCED_FACE('',(#740,#581,#582,#583),#639,.F.);
#4637=ADVANCED_FACE('',(#741,#584,#585,#586),#640,.T.);
#4638=ADVANCED_FACE('',(#742),#4542,.T.);
#4639=ADVANCED_FACE('',(#743),#641,.F.);
#4640=ADVANCED_FACE('',(#744),#4543,.T.);
#4641=ADVANCED_FACE('',(#745),#642,.T.);
#4642=ADVANCED_FACE('',(#746),#4544,.F.);
#4643=ADVANCED_FACE('',(#747),#4545,.F.);
#4644=ADVANCED_FACE('',(#748),#4546,.F.);
#4645=ADVANCED_FACE('',(#749),#643,.T.);
#4646=ADVANCED_FACE('',(#750),#4547,.T.);
#4647=ADVANCED_FACE('',(#751),#644,.T.);
#4648=ADVANCED_FACE('',(#752),#4548,.T.);
#4649=ADVANCED_FACE('',(#753,#587,#588,#589),#645,.T.);
#4650=ADVANCED_FACE('',(#754,#590,#591,#592),#646,.F.);
#4651=ADVANCED_FACE('',(#755),#4549,.T.);
#4652=ADVANCED_FACE('',(#756),#647,.T.);
#4653=ADVANCED_FACE('',(#757,#593),#4550,.T.);
#4654=ADVANCED_FACE('',(#758),#648,.F.);
#4655=ADVANCED_FACE('',(#759),#4551,.F.);
#4656=ADVANCED_FACE('',(#760),#4552,.F.);
#4657=ADVANCED_FACE('',(#761),#4553,.F.);
#4658=ADVANCED_FACE('',(#762),#4554,.F.);
#4659=ADVANCED_FACE('',(#763),#649,.F.);
#4660=ADVANCED_FACE('',(#764),#650,.F.);
#4661=ADVANCED_FACE('',(#765),#4555,.F.);
#4662=ADVANCED_FACE('',(#766,#594,#595),#651,.F.);
#4663=ADVANCED_FACE('',(#767),#4556,.F.);
#4664=ADVANCED_FACE('',(#768),#4557,.T.);
#4665=ADVANCED_FACE('',(#769,#596,#597),#652,.F.);
#4666=ADVANCED_FACE('',(#770),#4558,.T.);
#4667=ADVANCED_FACE('',(#771),#653,.F.);
#4668=ADVANCED_FACE('',(#772),#654,.F.);
#4669=ADVANCED_FACE('',(#773),#655,.T.);
#4670=ADVANCED_FACE('',(#774),#656,.T.);
#4671=ADVANCED_FACE('',(#775),#4559,.F.);
#4672=ADVANCED_FACE('',(#776,#598,#599),#657,.T.);
#4673=ADVANCED_FACE('',(#777),#4560,.F.);
#4674=ADVANCED_FACE('',(#778),#658,.T.);
#4675=ADVANCED_FACE('',(#779),#659,.T.);
#4676=ADVANCED_FACE('',(#780),#4561,.T.);
#4677=ADVANCED_FACE('',(#781,#600,#601),#660,.T.);
#4678=ADVANCED_FACE('',(#782),#4562,.T.);
#4679=ADVANCED_FACE('',(#783),#661,.T.);
#4680=ADVANCED_FACE('',(#784),#662,.T.);
#4681=ADVANCED_FACE('',(#785),#4563,.F.);
#4682=ADVANCED_FACE('',(#786),#4564,.F.);
#4683=ADVANCED_FACE('',(#787),#4565,.F.);
#4684=ADVANCED_FACE('',(#788),#4566,.F.);
#4685=ADVANCED_FACE('',(#789),#4567,.F.);
#4686=ADVANCED_FACE('',(#790),#663,.T.);
#4687=ADVANCED_FACE('',(#791),#48,.F.);
#4688=ADVANCED_FACE('',(#792),#4568,.F.);
#4689=ADVANCED_FACE('',(#793),#4569,.F.);
#4690=ADVANCED_FACE('',(#794),#49,.F.);
#4691=ADVANCED_FACE('',(#795),#50,.F.);
#4692=ADVANCED_FACE('',(#796),#51,.F.);
#4693=ADVANCED_FACE('',(#797),#52,.F.);
#4694=ADVANCED_FACE('',(#798,#602),#4570,.F.);
#4695=ADVANCED_FACE('',(#799),#4571,.F.);
#4696=ADVANCED_FACE('',(#800),#4572,.F.);
#4697=ADVANCED_FACE('',(#801),#4573,.F.);
#4698=ADVANCED_FACE('',(#802,#603),#664,.F.);
#4699=ADVANCED_FACE('',(#803,#604),#665,.T.);
#4700=ADVANCED_FACE('',(#804),#666,.T.);
#4701=ADVANCED_FACE('',(#805,#605),#667,.T.);
#4702=ADVANCED_FACE('',(#806),#668,.T.);
#4703=ADVANCED_FACE('',(#807,#606),#669,.T.);
#4704=ADVANCED_FACE('',(#808),#670,.F.);
#4705=ADVANCED_FACE('',(#809),#4574,.T.);
#4706=ADVANCED_FACE('',(#810),#671,.T.);
#4707=ADVANCED_FACE('',(#811),#4575,.T.);
#4708=ADVANCED_FACE('',(#812),#4576,.T.);
#4709=ADVANCED_FACE('',(#813,#607),#672,.T.);
#4710=ADVANCED_FACE('',(#814),#4577,.T.);
#4711=ADVANCED_FACE('',(#815),#673,.T.);
#4712=ADVANCED_FACE('',(#816),#674,.T.);
#4713=ADVANCED_FACE('',(#817),#675,.T.);
#4714=ADVANCED_FACE('',(#818,#608),#676,.F.);
#4715=ADVANCED_FACE('',(#819),#677,.T.);
#4716=ADVANCED_FACE('',(#820),#678,.T.);
#4717=ADVANCED_FACE('',(#821),#679,.T.);
#4718=ADVANCED_FACE('',(#822),#680,.T.);
#4719=ADVANCED_FACE('',(#823),#53,.F.);
#4720=ADVANCED_FACE('',(#824),#54,.F.);
#4721=ADVANCED_FACE('',(#825),#681,.F.);
#4722=CLOSED_SHELL('',(#4578,#4579,#4580,#4581,#4582,#4583,#4584,#4585,
#4586,#4587,#4588,#4589,#4590,#4591,#4592,#4593,#4594,#4595,#4596,#4597,
#4598,#4599,#4600,#4601,#4602,#4603));
#4723=CLOSED_SHELL('',(#4604,#4605,#4606,#4607,#4608,#4609,#4610,#4611,
#4612,#4613,#4614,#4615,#4616,#4617,#4618,#4619,#4620,#4621,#4622,#4623,
#4624,#4625,#4626));
#4724=CLOSED_SHELL('',(#4627,#4628,#4629));
#4725=CLOSED_SHELL('',(#4630,#4631,#4632,#4633,#4634,#4635,#4636,#4637,
#4638,#4639,#4640,#4641));
#4726=CLOSED_SHELL('',(#4642,#4643,#4644,#4645,#4646,#4647,#4648,#4649,
#4650,#4651,#4652,#4653,#4654));
#4727=CLOSED_SHELL('',(#4655,#4656,#4657,#4658,#4659,#4660,#4661,#4662,
#4663,#4664,#4665,#4666,#4667,#4668,#4669,#4670,#4671,#4672,#4673,#4674,
#4675,#4676,#4677,#4678,#4679,#4680));
#4728=CLOSED_SHELL('',(#4681,#4682,#4683,#4684,#4685,#4686,#4687,#4688,
#4689,#4690,#4691,#4692,#4693,#4694,#4695,#4696,#4697,#4698,#4699,#4700,
#4701,#4702,#4703));
#4729=CLOSED_SHELL('',(#4704,#4705,#4706));
#4730=CLOSED_SHELL('',(#4707,#4708,#4709,#4710,#4711,#4712,#4713,#4714,
#4715,#4716,#4717,#4718,#4719,#4720,#4721));
#4731=DERIVED_UNIT_ELEMENT(#4749,1.);
#4732=DERIVED_UNIT_ELEMENT(#74525,-3.);
#4733=DERIVED_UNIT_ELEMENT(#4749,1.);
#4734=DERIVED_UNIT_ELEMENT(#74525,-3.);
#4735=DERIVED_UNIT_ELEMENT(#4749,1.);
#4736=DERIVED_UNIT_ELEMENT(#74525,-3.);
#4737=DERIVED_UNIT_ELEMENT(#4749,1.);
#4738=DERIVED_UNIT_ELEMENT(#74525,-3.);
#4739=DERIVED_UNIT_ELEMENT(#4749,1.);
#4740=DERIVED_UNIT_ELEMENT(#74525,-3.);
#4741=DERIVED_UNIT_ELEMENT(#4749,1.);
#4742=DERIVED_UNIT_ELEMENT(#74525,-3.);
#4743=DERIVED_UNIT_ELEMENT(#4749,1.);
#4744=DERIVED_UNIT_ELEMENT(#74525,-3.);
#4745=DERIVED_UNIT_ELEMENT(#4749,1.);
#4746=DERIVED_UNIT_ELEMENT(#74525,-3.);
#4747=DERIVED_UNIT_ELEMENT(#4749,1.);
#4748=DERIVED_UNIT_ELEMENT(#74525,-3.);
#4749=(
MASS_UNIT()
NAMED_UNIT(*)
SI_UNIT(.KILO.,.GRAM.)
);
#4750=DERIVED_UNIT((#4731,#4732));
#4751=DERIVED_UNIT((#4733,#4734));
#4752=DERIVED_UNIT((#4735,#4736));
#4753=DERIVED_UNIT((#4737,#4738));
#4754=DERIVED_UNIT((#4739,#4740));
#4755=DERIVED_UNIT((#4741,#4742));
#4756=DERIVED_UNIT((#4743,#4744));
#4757=DERIVED_UNIT((#4745,#4746));
#4758=DERIVED_UNIT((#4747,#4748));
#4759=MEASURE_REPRESENTATION_ITEM('density measure',
POSITIVE_RATIO_MEASURE(7850.),#4750);
#4760=MEASURE_REPRESENTATION_ITEM('density measure',
POSITIVE_RATIO_MEASURE(7850.),#4751);
#4761=MEASURE_REPRESENTATION_ITEM('density measure',
POSITIVE_RATIO_MEASURE(7850.),#4752);
#4762=MEASURE_REPRESENTATION_ITEM('density measure',
POSITIVE_RATIO_MEASURE(7850.),#4753);
#4763=MEASURE_REPRESENTATION_ITEM('density measure',
POSITIVE_RATIO_MEASURE(7850.),#4754);
#4764=MEASURE_REPRESENTATION_ITEM('density measure',
POSITIVE_RATIO_MEASURE(7850.),#4755);
#4765=MEASURE_REPRESENTATION_ITEM('density measure',
POSITIVE_RATIO_MEASURE(7850.),#4756);
#4766=MEASURE_REPRESENTATION_ITEM('density measure',
POSITIVE_RATIO_MEASURE(7850.),#4757);
#4767=MEASURE_REPRESENTATION_ITEM('density measure',
POSITIVE_RATIO_MEASURE(7850.),#4758);
#4768=PROPERTY_DEFINITION_REPRESENTATION(#4813,#4786);
#4769=PROPERTY_DEFINITION_REPRESENTATION(#4814,#4787);
#4770=PROPERTY_DEFINITION_REPRESENTATION(#4815,#4788);
#4771=PROPERTY_DEFINITION_REPRESENTATION(#4816,#4789);
#4772=PROPERTY_DEFINITION_REPRESENTATION(#4817,#4790);
#4773=PROPERTY_DEFINITION_REPRESENTATION(#4818,#4791);
#4774=PROPERTY_DEFINITION_REPRESENTATION(#4819,#4792);
#4775=PROPERTY_DEFINITION_REPRESENTATION(#4820,#4793);
#4776=PROPERTY_DEFINITION_REPRESENTATION(#4821,#4794);
#4777=PROPERTY_DEFINITION_REPRESENTATION(#4822,#4795);
#4778=PROPERTY_DEFINITION_REPRESENTATION(#4823,#4796);
#4779=PROPERTY_DEFINITION_REPRESENTATION(#4824,#4797);
#4780=PROPERTY_DEFINITION_REPRESENTATION(#4825,#4798);
#4781=PROPERTY_DEFINITION_REPRESENTATION(#4826,#4799);
#4782=PROPERTY_DEFINITION_REPRESENTATION(#4827,#4800);
#4783=PROPERTY_DEFINITION_REPRESENTATION(#4828,#4801);
#4784=PROPERTY_DEFINITION_REPRESENTATION(#4829,#4802);
#4785=PROPERTY_DEFINITION_REPRESENTATION(#4830,#4803);
#4786=REPRESENTATION('material name',(#4804),#74514);
#4787=REPRESENTATION('density',(#4759),#74514);
#4788=REPRESENTATION('material name',(#4805),#74515);
#4789=REPRESENTATION('density',(#4760),#74515);
#4790=REPRESENTATION('material name',(#4806),#74516);
#4791=REPRESENTATION('density',(#4761),#74516);
#4792=REPRESENTATION('material name',(#4807),#74517);
#4793=REPRESENTATION('density',(#4762),#74517);
#4794=REPRESENTATION('material name',(#4808),#74518);
#4795=REPRESENTATION('density',(#4763),#74518);
#4796=REPRESENTATION('material name',(#4809),#74519);
#4797=REPRESENTATION('density',(#4764),#74519);
#4798=REPRESENTATION('material name',(#4810),#74520);
#4799=REPRESENTATION('density',(#4765),#74520);
#4800=REPRESENTATION('material name',(#4811),#74521);
#4801=REPRESENTATION('density',(#4766),#74521);
#4802=REPRESENTATION('material name',(#4812),#74522);
#4803=REPRESENTATION('density',(#4767),#74522);
#4804=DESCRIPTIVE_REPRESENTATION_ITEM('Steel (1)','Steel (1)');
#4805=DESCRIPTIVE_REPRESENTATION_ITEM('Steel (1)','Steel (1)');
#4806=DESCRIPTIVE_REPRESENTATION_ITEM('Steel (1)','Steel (1)');
#4807=DESCRIPTIVE_REPRESENTATION_ITEM('Steel (1)','Steel (1)');
#4808=DESCRIPTIVE_REPRESENTATION_ITEM('Steel (1)','Steel (1)');
#4809=DESCRIPTIVE_REPRESENTATION_ITEM('Steel (1)','Steel (1)');
#4810=DESCRIPTIVE_REPRESENTATION_ITEM('Steel (1)','Steel (1)');
#4811=DESCRIPTIVE_REPRESENTATION_ITEM('Steel (1)','Steel (1)');
#4812=DESCRIPTIVE_REPRESENTATION_ITEM('Steel (1)','Steel (1)');
#4813=PROPERTY_DEFINITION('material property','material name',#74569);
#4814=PROPERTY_DEFINITION('material property','density of part',#74569);
#4815=PROPERTY_DEFINITION('material property','material name',#74570);
#4816=PROPERTY_DEFINITION('material property','density of part',#74570);
#4817=PROPERTY_DEFINITION('material property','material name',#74571);
#4818=PROPERTY_DEFINITION('material property','density of part',#74571);
#4819=PROPERTY_DEFINITION('material property','material name',#74572);
#4820=PROPERTY_DEFINITION('material property','density of part',#74572);
#4821=PROPERTY_DEFINITION('material property','material name',#74573);
#4822=PROPERTY_DEFINITION('material property','density of part',#74573);
#4823=PROPERTY_DEFINITION('material property','material name',#74574);
#4824=PROPERTY_DEFINITION('material property','density of part',#74574);
#4825=PROPERTY_DEFINITION('material property','material name',#74575);
#4826=PROPERTY_DEFINITION('material property','density of part',#74575);
#4827=PROPERTY_DEFINITION('material property','material name',#74576);
#4828=PROPERTY_DEFINITION('material property','density of part',#74576);
#4829=PROPERTY_DEFINITION('material property','material name',#74577);
#4830=PROPERTY_DEFINITION('material property','density of part',#74577);
#4831=AXIS2_PLACEMENT_3D('',#5829,#5098,#5099);
#4832=AXIS2_PLACEMENT_3D('',#5830,#5100,#5101);
#4833=AXIS2_PLACEMENT_3D('',#5831,#5102,#5103);
#4834=AXIS2_PLACEMENT_3D('',#5833,#5104,#5105);
#4835=AXIS2_PLACEMENT_3D('',#5836,#5107,#5108);
#4836=AXIS2_PLACEMENT_3D('',#5837,#5109,#5110);
#4837=AXIS2_PLACEMENT_3D('',#5839,#5111,#5112);
#4838=AXIS2_PLACEMENT_3D('',#5842,#5114,#5115);
#4839=AXIS2_PLACEMENT_3D('',#5843,#5116,#5117);
#4840=AXIS2_PLACEMENT_3D('',#5845,#5118,#5119);
#4841=AXIS2_PLACEMENT_3D('',#5848,#5121,#5122);
#4842=AXIS2_PLACEMENT_3D('',#5849,#5123,#5124);
#4843=AXIS2_PLACEMENT_3D('',#5851,#5125,#5126);
#4844=AXIS2_PLACEMENT_3D('',#5854,#5128,#5129);
#4845=AXIS2_PLACEMENT_3D('',#5855,#5130,#5131);
#4846=AXIS2_PLACEMENT_3D('',#5864,#5136,#5137);
#4847=AXIS2_PLACEMENT_3D('',#5870,#5141,#5142);
#4848=AXIS2_PLACEMENT_3D('',#5872,#5143,#5144);
#4849=AXIS2_PLACEMENT_3D('',#5875,#5146,#5147);
#4850=AXIS2_PLACEMENT_3D('',#5876,#5148,#5149);
#4851=AXIS2_PLACEMENT_3D('',#5882,#5153,#5154);
#4852=AXIS2_PLACEMENT_3D('',#5884,#5155,#5156);
#4853=AXIS2_PLACEMENT_3D('',#5887,#5158,#5159);
#4854=AXIS2_PLACEMENT_3D('',#5888,#5160,#5161);
#4855=AXIS2_PLACEMENT_3D('',#5893,#5163,#5164);
#4856=AXIS2_PLACEMENT_3D('',#5896,#5166,#5167);
#4857=AXIS2_PLACEMENT_3D('',#5897,#5168,#5169);
#4858=AXIS2_PLACEMENT_3D('',#5903,#5173,#5174);
#4859=AXIS2_PLACEMENT_3D('',#5905,#5175,#5176);
#4860=AXIS2_PLACEMENT_3D('',#5908,#5178,#5179);
#4861=AXIS2_PLACEMENT_3D('',#5909,#5180,#5181);
#4862=AXIS2_PLACEMENT_3D('',#5912,#5184,#5185);
#4863=AXIS2_PLACEMENT_3D('',#5921,#5189,#5190);
#4864=AXIS2_PLACEMENT_3D('',#5925,#5192,#5193);
#4865=AXIS2_PLACEMENT_3D('',#5930,#5196,#5197);
#4866=AXIS2_PLACEMENT_3D('',#5933,#5199,#5200);
#4867=AXIS2_PLACEMENT_3D('',#5934,#5201,#5202);
#4868=AXIS2_PLACEMENT_3D('',#5940,#5206,#5207);
#4869=AXIS2_PLACEMENT_3D('',#5944,#5210,#5211);
#4870=AXIS2_PLACEMENT_3D('',#5946,#5212,#5213);
#4871=AXIS2_PLACEMENT_3D('',#5948,#5215,#5216);
#4872=AXIS2_PLACEMENT_3D('',#5952,#5219,#5220);
#4873=AXIS2_PLACEMENT_3D('',#5954,#5221,#5222);
#4874=AXIS2_PLACEMENT_3D('',#5956,#5224,#5225);
#4875=AXIS2_PLACEMENT_3D('',#5958,#5227,#5228);
#4876=AXIS2_PLACEMENT_3D('',#5962,#5231,#5232);
#4877=AXIS2_PLACEMENT_3D('',#5964,#5233,#5234);
#4878=AXIS2_PLACEMENT_3D('',#5966,#5236,#5237);
#4879=AXIS2_PLACEMENT_3D('',#5970,#5240,#5241);
#4880=AXIS2_PLACEMENT_3D('',#5972,#5242,#5243);
#4881=AXIS2_PLACEMENT_3D('',#5974,#5245,#5246);
#4882=AXIS2_PLACEMENT_3D('',#5976,#5248,#5249);
#4883=AXIS2_PLACEMENT_3D('',#5977,#5250,#5251);
#4884=AXIS2_PLACEMENT_3D('',#5978,#5252,#5253);
#4885=AXIS2_PLACEMENT_3D('',#5980,#5254,#5255);
#4886=AXIS2_PLACEMENT_3D('',#5983,#5257,#5258);
#4887=AXIS2_PLACEMENT_3D('',#5984,#5259,#5260);
#4888=AXIS2_PLACEMENT_3D('',#5986,#5261,#5262);
#4889=AXIS2_PLACEMENT_3D('',#5989,#5264,#5265);
#4890=AXIS2_PLACEMENT_3D('',#5990,#5266,#5267);
#4891=AXIS2_PLACEMENT_3D('',#5992,#5268,#5269);
#4892=AXIS2_PLACEMENT_3D('',#5995,#5271,#5272);
#4893=AXIS2_PLACEMENT_3D('',#5996,#5273,#5274);
#4894=AXIS2_PLACEMENT_3D('',#5998,#5275,#5276);
#4895=AXIS2_PLACEMENT_3D('',#6001,#5278,#5279);
#4896=AXIS2_PLACEMENT_3D('',#6002,#5280,#5281);
#4897=AXIS2_PLACEMENT_3D('',#6004,#5282,#5283);
#4898=AXIS2_PLACEMENT_3D('',#6007,#5285,#5286);
#4899=AXIS2_PLACEMENT_3D('',#6008,#5287,#5288);
#4900=AXIS2_PLACEMENT_3D('',#6011,#5289,#5290);
#4901=AXIS2_PLACEMENT_3D('',#6015,#5292,#5293);
#4902=AXIS2_PLACEMENT_3D('',#6017,#5295,#5296);
#4903=AXIS2_PLACEMENT_3D('',#6023,#5300,#5301);
#4904=AXIS2_PLACEMENT_3D('',#6025,#5302,#5303);
#4905=AXIS2_PLACEMENT_3D('',#6027,#5304,#5305);
#4906=AXIS2_PLACEMENT_3D('',#6029,#5307,#5308);
#4907=AXIS2_PLACEMENT_3D('',#6039,#5314,#5315);
#4908=AXIS2_PLACEMENT_3D('',#6042,#5317,#5318);
#4909=AXIS2_PLACEMENT_3D('',#6043,#5319,#5320);
#4910=AXIS2_PLACEMENT_3D('',#6045,#5321,#5322);
#4911=AXIS2_PLACEMENT_3D('',#6047,#5324,#5325);
#4912=AXIS2_PLACEMENT_3D('',#6048,#5326,#5327);
#4913=AXIS2_PLACEMENT_3D('',#6049,#5328,#5329);
#4914=AXIS2_PLACEMENT_3D('',#6055,#5333,#5334);
#4915=AXIS2_PLACEMENT_3D('',#6059,#5337,#5338);
#4916=AXIS2_PLACEMENT_3D('',#6063,#5341,#5342);
#4917=AXIS2_PLACEMENT_3D('',#6065,#5343,#5344);
#4918=AXIS2_PLACEMENT_3D('',#6068,#5346,#5347);
#4919=AXIS2_PLACEMENT_3D('',#6069,#5348,#5349);
#4920=AXIS2_PLACEMENT_3D('',#6079,#5355,#5356);
#4921=AXIS2_PLACEMENT_3D('',#6081,#5357,#5358);
#4922=AXIS2_PLACEMENT_3D('',#6084,#5360,#5361);
#4923=AXIS2_PLACEMENT_3D('',#6085,#5362,#5363);
#4924=AXIS2_PLACEMENT_3D('',#6091,#5367,#5368);
#4925=AXIS2_PLACEMENT_3D('',#6092,#5369,#5370);
#4926=AXIS2_PLACEMENT_3D('',#6093,#5371,#5372);
#4927=AXIS2_PLACEMENT_3D('',#6094,#5373,#5374);
#4928=AXIS2_PLACEMENT_3D('',#6095,#5375,#5376);
#4929=AXIS2_PLACEMENT_3D('',#6096,#5377,#5378);
#4930=AXIS2_PLACEMENT_3D('',#6097,#5379,#5380);
#4931=AXIS2_PLACEMENT_3D('',#6099,#5381,#5382);
#4932=AXIS2_PLACEMENT_3D('',#6100,#5383,#5384);
#4933=AXIS2_PLACEMENT_3D('',#6102,#5385,#5386);
#4934=AXIS2_PLACEMENT_3D('',#6104,#5388,#5389);
#4935=AXIS2_PLACEMENT_3D('',#6105,#5390,#5391);
#4936=AXIS2_PLACEMENT_3D('',#6106,#5392,#5393);
#4937=AXIS2_PLACEMENT_3D('',#6108,#5394,#5395);
#4938=AXIS2_PLACEMENT_3D('',#6111,#5397,#5398);
#4939=AXIS2_PLACEMENT_3D('',#6112,#5399,#5400);
#4940=AXIS2_PLACEMENT_3D('',#6114,#5401,#5402);
#4941=AXIS2_PLACEMENT_3D('',#6117,#5404,#5405);
#4942=AXIS2_PLACEMENT_3D('',#6118,#5406,#5407);
#4943=AXIS2_PLACEMENT_3D('',#6127,#5412,#5413);
#4944=AXIS2_PLACEMENT_3D('',#6129,#5414,#5415);
#4945=AXIS2_PLACEMENT_3D('',#6132,#5417,#5418);
#4946=AXIS2_PLACEMENT_3D('',#6133,#5419,#5420);
#4947=AXIS2_PLACEMENT_3D('',#6139,#5424,#5425);
#4948=AXIS2_PLACEMENT_3D('',#6140,#5426,#5427);
#4949=AXIS2_PLACEMENT_3D('',#6141,#5428,#5429);
#4950=AXIS2_PLACEMENT_3D('',#6142,#5430,#5431);
#4951=AXIS2_PLACEMENT_3D('',#6144,#5432,#5433);
#4952=AXIS2_PLACEMENT_3D('',#6145,#5434,#5435);
#4953=AXIS2_PLACEMENT_3D('',#6147,#5436,#5437);
#4954=AXIS2_PLACEMENT_3D('',#6148,#5438,#5439);
#4955=AXIS2_PLACEMENT_3D('',#6150,#5440,#5441);
#4956=AXIS2_PLACEMENT_3D('',#6152,#5443,#5444);
#4957=AXIS2_PLACEMENT_3D('',#6154,#5445,#5446);
#4958=AXIS2_PLACEMENT_3D('',#6155,#5447,#5448);
#4959=AXIS2_PLACEMENT_3D('',#6157,#5450,#5451);
#4960=AXIS2_PLACEMENT_3D('',#6158,#5452,#5453);
#4961=AXIS2_PLACEMENT_3D('',#6159,#5454,#5455);
#4962=AXIS2_PLACEMENT_3D('',#6161,#5456,#5457);
#4963=AXIS2_PLACEMENT_3D('',#6164,#5459,#5460);
#4964=AXIS2_PLACEMENT_3D('',#6165,#5461,#5462);
#4965=AXIS2_PLACEMENT_3D('',#6262,#5464,#5465);
#4966=AXIS2_PLACEMENT_3D('',#6264,#5466,#5467);
#4967=AXIS2_PLACEMENT_3D('',#6267,#5469,#5470);
#4968=AXIS2_PLACEMENT_3D('',#6268,#5471,#5472);
#4969=AXIS2_PLACEMENT_3D('',#6277,#5477,#5478);
#4970=AXIS2_PLACEMENT_3D('',#6279,#5479,#5480);
#4971=AXIS2_PLACEMENT_3D('',#6281,#5481,#5482);
#4972=AXIS2_PLACEMENT_3D('',#6283,#5484,#5485);
#4973=AXIS2_PLACEMENT_3D('',#6289,#5489,#5490);
#4974=AXIS2_PLACEMENT_3D('',#6290,#5491,#5492);
#4975=AXIS2_PLACEMENT_3D('',#6291,#5493,#5494);
#4976=AXIS2_PLACEMENT_3D('',#6292,#5495,#5496);
#4977=AXIS2_PLACEMENT_3D('',#6294,#5497,#5498);
#4978=AXIS2_PLACEMENT_3D('',#6295,#5499,#5500);
#4979=AXIS2_PLACEMENT_3D('',#6297,#5501,#5502);
#4980=AXIS2_PLACEMENT_3D('',#6298,#5503,#5504);
#4981=AXIS2_PLACEMENT_3D('',#6300,#5505,#5506);
#4982=AXIS2_PLACEMENT_3D('',#6302,#5508,#5509);
#4983=AXIS2_PLACEMENT_3D('',#6303,#5510,#5511);
#4984=AXIS2_PLACEMENT_3D('',#6307,#5514,#5515);
#4985=AXIS2_PLACEMENT_3D('',#6308,#5516,#5517);
#4986=AXIS2_PLACEMENT_3D('',#6309,#5518,#5519);
#4987=AXIS2_PLACEMENT_3D('',#6310,#5520,#5521);
#4988=AXIS2_PLACEMENT_3D('',#6312,#5522,#5523);
#4989=AXIS2_PLACEMENT_3D('',#6315,#5525,#5526);
#4990=AXIS2_PLACEMENT_3D('',#6316,#5527,#5528);
#4991=AXIS2_PLACEMENT_3D('',#6318,#5529,#5530);
#4992=AXIS2_PLACEMENT_3D('',#6321,#5532,#5533);
#4993=AXIS2_PLACEMENT_3D('',#6322,#5534,#5535);
#4994=AXIS2_PLACEMENT_3D('',#6324,#5536,#5537);
#4995=AXIS2_PLACEMENT_3D('',#6327,#5539,#5540);
#4996=AXIS2_PLACEMENT_3D('',#6328,#5541,#5542);
#4997=AXIS2_PLACEMENT_3D('',#6330,#5543,#5544);
#4998=AXIS2_PLACEMENT_3D('',#6333,#5546,#5547);
#4999=AXIS2_PLACEMENT_3D('',#6334,#5548,#5549);
#5000=AXIS2_PLACEMENT_3D('',#6343,#5554,#5555);
#5001=AXIS2_PLACEMENT_3D('',#6349,#5559,#5560);
#5002=AXIS2_PLACEMENT_3D('',#6351,#5561,#5562);
#5003=AXIS2_PLACEMENT_3D('',#6354,#5564,#5565);
#5004=AXIS2_PLACEMENT_3D('',#6355,#5566,#5567);
#5005=AXIS2_PLACEMENT_3D('',#6361,#5571,#5572);
#5006=AXIS2_PLACEMENT_3D('',#6363,#5573,#5574);
#5007=AXIS2_PLACEMENT_3D('',#6366,#5576,#5577);
#5008=AXIS2_PLACEMENT_3D('',#6367,#5578,#5579);
#5009=AXIS2_PLACEMENT_3D('',#6372,#5581,#5582);
#5010=AXIS2_PLACEMENT_3D('',#6375,#5584,#5585);
#5011=AXIS2_PLACEMENT_3D('',#6376,#5586,#5587);
#5012=AXIS2_PLACEMENT_3D('',#6382,#5591,#5592);
#5013=AXIS2_PLACEMENT_3D('',#6384,#5593,#5594);
#5014=AXIS2_PLACEMENT_3D('',#6387,#5596,#5597);
#5015=AXIS2_PLACEMENT_3D('',#6388,#5598,#5599);
#5016=AXIS2_PLACEMENT_3D('',#6391,#5602,#5603);
#5017=AXIS2_PLACEMENT_3D('',#6400,#5607,#5608);
#5018=AXIS2_PLACEMENT_3D('',#6404,#5610,#5611);
#5019=AXIS2_PLACEMENT_3D('',#6409,#5614,#5615);
#5020=AXIS2_PLACEMENT_3D('',#6412,#5617,#5618);
#5021=AXIS2_PLACEMENT_3D('',#6413,#5619,#5620);
#5022=AXIS2_PLACEMENT_3D('',#6419,#5624,#5625);
#5023=AXIS2_PLACEMENT_3D('',#6423,#5628,#5629);
#5024=AXIS2_PLACEMENT_3D('',#6425,#5630,#5631);
#5025=AXIS2_PLACEMENT_3D('',#6427,#5633,#5634);
#5026=AXIS2_PLACEMENT_3D('',#6431,#5637,#5638);
#5027=AXIS2_PLACEMENT_3D('',#6433,#5639,#5640);
#5028=AXIS2_PLACEMENT_3D('',#6435,#5642,#5643);
#5029=AXIS2_PLACEMENT_3D('',#6437,#5645,#5646);
#5030=AXIS2_PLACEMENT_3D('',#6441,#5649,#5650);
#5031=AXIS2_PLACEMENT_3D('',#6443,#5651,#5652);
#5032=AXIS2_PLACEMENT_3D('',#6445,#5654,#5655);
#5033=AXIS2_PLACEMENT_3D('',#6449,#5658,#5659);
#5034=AXIS2_PLACEMENT_3D('',#6451,#5660,#5661);
#5035=AXIS2_PLACEMENT_3D('',#6453,#5663,#5664);
#5036=AXIS2_PLACEMENT_3D('',#6455,#5666,#5667);
#5037=AXIS2_PLACEMENT_3D('',#6456,#5668,#5669);
#5038=AXIS2_PLACEMENT_3D('',#6457,#5670,#5671);
#5039=AXIS2_PLACEMENT_3D('',#6481,#5673,#5674);
#5040=AXIS2_PLACEMENT_3D('',#6516,#5676,#5677);
#5041=AXIS2_PLACEMENT_3D('',#6555,#5678,#5679);
#5042=AXIS2_PLACEMENT_3D('',#6599,#5681,#5682);
#5043=AXIS2_PLACEMENT_3D('',#6652,#5683,#5684);
#5044=AXIS2_PLACEMENT_3D('',#6751,#5685,#5686);
#5045=AXIS2_PLACEMENT_3D('',#6850,#5687,#5688);
#5046=AXIS2_PLACEMENT_3D('',#6855,#5690,#5691);
#5047=AXIS2_PLACEMENT_3D('',#7239,#5692,#5693);
#5048=AXIS2_PLACEMENT_3D('',#7323,#5694,#5695);
#5049=AXIS2_PLACEMENT_3D('',#7325,#5696,#5697);
#5050=AXIS2_PLACEMENT_3D('',#7866,#5698,#5699);
#5051=AXIS2_PLACEMENT_3D('',#7868,#5700,#5701);
#5052=AXIS2_PLACEMENT_3D('',#7899,#5704,#5705);
#5053=AXIS2_PLACEMENT_3D('',#7940,#5706,#5707);
#5054=AXIS2_PLACEMENT_3D('',#7941,#5708,#5709);
#5055=AXIS2_PLACEMENT_3D('',#7942,#5710,#5711);
#5056=AXIS2_PLACEMENT_3D('',#7945,#5713,#5714);
#5057=AXIS2_PLACEMENT_3D('',#7946,#5715,#5716);
#5058=AXIS2_PLACEMENT_3D('',#7955,#5721,#5722);
#5059=AXIS2_PLACEMENT_3D('',#7961,#5726,#5727);
#5060=AXIS2_PLACEMENT_3D('',#7965,#5730,#5731);
#5061=AXIS2_PLACEMENT_3D('',#7969,#5734,#5735);
#5062=AXIS2_PLACEMENT_3D('',#7971,#5737,#5738);
#5063=AXIS2_PLACEMENT_3D('',#7972,#5739,#5740);
#5064=AXIS2_PLACEMENT_3D('',#7973,#5741,#5742);
#5065=AXIS2_PLACEMENT_3D('',#7975,#5743,#5744);
#5066=AXIS2_PLACEMENT_3D('',#7976,#5745,#5746);
#5067=AXIS2_PLACEMENT_3D('',#7978,#5747,#5748);
#5068=AXIS2_PLACEMENT_3D('',#7980,#5750,#5751);
#5069=AXIS2_PLACEMENT_3D('',#7981,#5752,#5753);
#5070=AXIS2_PLACEMENT_3D('',#7982,#5754,#5755);
#5071=AXIS2_PLACEMENT_3D('',#8065,#5756,#5757);
#5072=AXIS2_PLACEMENT_3D('',#17516,#5758,#5759);
#5073=AXIS2_PLACEMENT_3D('',#24562,#5760,#5761);
#5074=AXIS2_PLACEMENT_3D('',#24615,#5762,#5763);
#5075=AXIS2_PLACEMENT_3D('',#46894,#5764,#5765);
#5076=AXIS2_PLACEMENT_3D('',#68909,#5766,#5767);
#5077=AXIS2_PLACEMENT_3D('',#68911,#5768,#5769);
#5078=AXIS2_PLACEMENT_3D('',#68924,#5776,#5777);
#5079=AXIS2_PLACEMENT_3D('',#68927,#5779,#5780);
#5080=AXIS2_PLACEMENT_3D('',#68928,#5781,#5782);
#5081=AXIS2_PLACEMENT_3D('',#68934,#5786,#5787);
#5082=AXIS2_PLACEMENT_3D('',#68938,#5790,#5791);
#5083=AXIS2_PLACEMENT_3D('',#68942,#5794,#5795);
#5084=AXIS2_PLACEMENT_3D('',#69037,#5796,#5797);
#5085=AXIS2_PLACEMENT_3D('',#69041,#5800,#5801);
#5086=AXIS2_PLACEMENT_3D('',#69045,#5804,#5805);
#5087=AXIS2_PLACEMENT_3D('',#69047,#5807,#5808);
#5088=AXIS2_PLACEMENT_3D('',#74492,#5809,#5810);
#5089=AXIS2_PLACEMENT_3D('',#74493,#5811,#5812);
#5090=AXIS2_PLACEMENT_3D('',#74494,#5813,#5814);
#5091=AXIS2_PLACEMENT_3D('',#74495,#5815,#5816);
#5092=AXIS2_PLACEMENT_3D('',#74496,#5817,#5818);
#5093=AXIS2_PLACEMENT_3D('',#74497,#5819,#5820);
#5094=AXIS2_PLACEMENT_3D('',#74498,#5821,#5822);
#5095=AXIS2_PLACEMENT_3D('',#74499,#5823,#5824);
#5096=AXIS2_PLACEMENT_3D('',#74500,#5825,#5826);
#5097=AXIS2_PLACEMENT_3D('',#74501,#5827,#5828);
#5098=DIRECTION('axis',(0.,0.,1.));
#5099=DIRECTION('refdir',(1.,0.,0.));
#5100=DIRECTION('axis',(0.,0.,1.));
#5101=DIRECTION('refdir',(1.,0.,0.));
#5102=DIRECTION('center_axis',(0.,1.,0.));
#5103=DIRECTION('ref_axis',(1.,0.,0.));
#5104=DIRECTION('center_axis',(0.,1.,0.));
#5105=DIRECTION('ref_axis',(1.,0.,0.));
#5106=DIRECTION('',(0.,1.,0.));
#5107=DIRECTION('center_axis',(0.,-1.,-8.88178419700126E-16));
#5108=DIRECTION('ref_axis',(1.,0.,0.));
#5109=DIRECTION('center_axis',(0.,1.,0.));
#5110=DIRECTION('ref_axis',(1.,0.,0.));
#5111=DIRECTION('center_axis',(0.,1.,-8.88178419700126E-16));
#5112=DIRECTION('ref_axis',(1.,0.,0.));
#5113=DIRECTION('',(0.,1.,0.));
#5114=DIRECTION('center_axis',(0.,-1.,0.));
#5115=DIRECTION('ref_axis',(1.,0.,0.));
#5116=DIRECTION('center_axis',(0.,1.,0.));
#5117=DIRECTION('ref_axis',(1.,0.,0.));
#5118=DIRECTION('center_axis',(0.,1.,0.));
#5119=DIRECTION('ref_axis',(1.,0.,0.));
#5120=DIRECTION('',(0.,1.,0.));
#5121=DIRECTION('center_axis',(0.,-1.,-8.88178419700126E-16));
#5122=DIRECTION('ref_axis',(1.,0.,0.));
#5123=DIRECTION('center_axis',(0.,1.,0.));
#5124=DIRECTION('ref_axis',(1.,0.,0.));
#5125=DIRECTION('center_axis',(0.,1.,-8.88178419700126E-16));
#5126=DIRECTION('ref_axis',(1.,0.,0.));
#5127=DIRECTION('',(0.,1.,0.));
#5128=DIRECTION('center_axis',(0.,-1.,0.));
#5129=DIRECTION('ref_axis',(1.,0.,0.));
#5130=DIRECTION('center_axis',(0.,1.,0.));
#5131=DIRECTION('ref_axis',(0.,0.,1.));
#5132=DIRECTION('',(-1.,0.,0.));
#5133=DIRECTION('',(0.,0.,-1.));
#5134=DIRECTION('',(1.,0.,0.));
#5135=DIRECTION('',(0.,0.,1.));
#5136=DIRECTION('center_axis',(0.,0.,1.));
#5137=DIRECTION('ref_axis',(0.,-1.,0.));
#5138=DIRECTION('',(0.,1.,0.));
#5139=DIRECTION('',(1.,0.,0.));
#5140=DIRECTION('',(0.,-1.,0.));
#5141=DIRECTION('center_axis',(-1.,0.,0.));
#5142=DIRECTION('ref_axis',(0.,5.92118946466746E-15,1.));
#5143=DIRECTION('center_axis',(-1.,0.,0.));
#5144=DIRECTION('ref_axis',(0.,5.92118946466746E-15,1.));
#5145=DIRECTION('',(1.,0.,0.));
#5146=DIRECTION('center_axis',(1.,0.,0.));
#5147=DIRECTION('ref_axis',(0.,5.92118946466746E-15,1.));
#5148=DIRECTION('center_axis',(0.,1.,-8.88178419700126E-16));
#5149=DIRECTION('ref_axis',(0.,8.88178419700126E-16,1.));
#5150=DIRECTION('',(0.,-8.88178419700126E-16,-1.));
#5151=DIRECTION('',(1.,0.,0.));
#5152=DIRECTION('',(0.,8.88178419700126E-16,1.));
#5153=DIRECTION('center_axis',(-1.,0.,0.));
#5154=DIRECTION('ref_axis',(0.,1.,-8.88178419700118E-15));
#5155=DIRECTION('center_axis',(-1.,0.,0.));
#5156=DIRECTION('ref_axis',(0.,1.,-8.88178419700118E-15));
#5157=DIRECTION('',(1.,0.,0.));
#5158=DIRECTION('center_axis',(1.,0.,0.));
#5159=DIRECTION('ref_axis',(0.,1.,-8.88178419700118E-15));
#5160=DIRECTION('center_axis',(-1.,0.,0.));
#5161=DIRECTION('ref_axis',(0.,1.,-7.58652400160517E-15));
#5162=DIRECTION('',(1.,0.,0.));
#5163=DIRECTION('center_axis',(1.,0.,0.));
#5164=DIRECTION('ref_axis',(0.,1.,-7.58652400160517E-15));
#5165=DIRECTION('',(1.,0.,0.));
#5166=DIRECTION('center_axis',(-1.,0.,0.));
#5167=DIRECTION('ref_axis',(0.,1.,-7.58652400160517E-15));
#5168=DIRECTION('center_axis',(0.,-1.,0.));
#5169=DIRECTION('ref_axis',(0.,0.,-1.));
#5170=DIRECTION('',(0.,0.,1.));
#5171=DIRECTION('',(1.,0.,0.));
#5172=DIRECTION('',(0.,0.,-1.));
#5173=DIRECTION('center_axis',(-1.,0.,0.));
#5174=DIRECTION('ref_axis',(0.,5.92118946466745E-15,1.));
#5175=DIRECTION('center_axis',(1.,0.,0.));
#5176=DIRECTION('ref_axis',(0.,5.92118946466745E-15,1.));
#5177=DIRECTION('',(1.,0.,0.));
#5178=DIRECTION('center_axis',(-1.,0.,0.));
#5179=DIRECTION('ref_axis',(0.,5.92118946466745E-15,1.));
#5180=DIRECTION('center_axis',(0.,0.,-1.));
#5181=DIRECTION('ref_axis',(0.,1.,0.));
#5182=DIRECTION('',(0.,-1.,0.));
#5183=DIRECTION('',(0.,1.,0.));
#5184=DIRECTION('center_axis',(1.,0.,0.));
#5185=DIRECTION('ref_axis',(0.,1.,0.));
#5186=DIRECTION('',(0.,1.,0.));
#5187=DIRECTION('',(0.,0.,-1.));
#5188=DIRECTION('',(0.,-1.,0.));
#5189=DIRECTION('center_axis',(1.,0.,0.));
#5190=DIRECTION('ref_axis',(0.,-5.92118946466746E-15,1.));
#5191=DIRECTION('',(0.,8.88178419700126E-16,-1.));
#5192=DIRECTION('center_axis',(1.,0.,0.));
#5193=DIRECTION('ref_axis',(0.,-1.,-8.88178419700118E-15));
#5194=DIRECTION('',(0.,1.,-7.61818177922111E-18));
#5195=DIRECTION('',(0.,1.,-1.49625744558646E-17));
#5196=DIRECTION('center_axis',(-1.,0.,0.));
#5197=DIRECTION('ref_axis',(0.,-1.,-7.58652400160517E-15));
#5198=DIRECTION('',(0.,0.,1.));
#5199=DIRECTION('center_axis',(-1.,0.,0.));
#5200=DIRECTION('ref_axis',(0.,-5.92118946466745E-15,1.));
#5201=DIRECTION('center_axis',(0.,1.,0.));
#5202=DIRECTION('ref_axis',(0.,0.,1.));
#5203=DIRECTION('',(-1.,0.,0.));
#5204=DIRECTION('',(0.,0.,1.));
#5205=DIRECTION('',(1.,0.,0.));
#5206=DIRECTION('center_axis',(0.,0.,-1.));
#5207=DIRECTION('ref_axis',(0.,1.,0.));
#5208=DIRECTION('',(0.,1.,0.));
#5209=DIRECTION('',(1.,0.,0.));
#5210=DIRECTION('center_axis',(1.,0.,0.));
#5211=DIRECTION('ref_axis',(0.,-5.92118946466746E-15,1.));
#5212=DIRECTION('center_axis',(-1.,0.,0.));
#5213=DIRECTION('ref_axis',(0.,-5.92118946466746E-15,1.));
#5214=DIRECTION('',(1.,0.,0.));
#5215=DIRECTION('center_axis',(0.,1.,8.88178419700126E-16));
#5216=DIRECTION('ref_axis',(0.,-8.88178419700126E-16,1.));
#5217=DIRECTION('',(0.,-8.88178419700126E-16,1.));
#5218=DIRECTION('',(1.,0.,0.));
#5219=DIRECTION('center_axis',(1.,0.,0.));
#5220=DIRECTION('ref_axis',(0.,-1.,-8.88178419700118E-15));
#5221=DIRECTION('center_axis',(-1.,0.,0.));
#5222=DIRECTION('ref_axis',(0.,-1.,-8.88178419700118E-15));
#5223=DIRECTION('',(1.,0.,0.));
#5224=DIRECTION('center_axis',(0.,7.61818177922111E-18,1.));
#5225=DIRECTION('ref_axis',(0.,-1.,7.61818177922111E-18));
#5226=DIRECTION('',(0.,1.,7.61818177922111E-18));
#5227=DIRECTION('center_axis',(0.,1.49625744558646E-17,-1.));
#5228=DIRECTION('ref_axis',(0.,1.,1.49625744558646E-17));
#5229=DIRECTION('',(0.,1.,1.49625744558646E-17));
#5230=DIRECTION('',(1.,0.,0.));
#5231=DIRECTION('center_axis',(1.,0.,0.));
#5232=DIRECTION('ref_axis',(0.,-1.,-7.58652400160517E-15));
#5233=DIRECTION('center_axis',(1.,0.,0.));
#5234=DIRECTION('ref_axis',(0.,-1.,-7.58652400160517E-15));
#5235=DIRECTION('',(1.,0.,0.));
#5236=DIRECTION('center_axis',(0.,-1.,0.));
#5237=DIRECTION('ref_axis',(0.,0.,-1.));
#5238=DIRECTION('',(0.,0.,-1.));
#5239=DIRECTION('',(1.,0.,0.));
#5240=DIRECTION('center_axis',(1.,0.,0.));
#5241=DIRECTION('ref_axis',(0.,-5.92118946466745E-15,1.));
#5242=DIRECTION('center_axis',(1.,0.,0.));
#5243=DIRECTION('ref_axis',(0.,-5.92118946466745E-15,1.));
#5244=DIRECTION('',(1.,0.,0.));
#5245=DIRECTION('center_axis',(0.,0.,1.));
#5246=DIRECTION('ref_axis',(0.,-1.,0.));
#5247=DIRECTION('',(0.,-1.,0.));
#5248=DIRECTION('center_axis',(1.,0.,0.));
#5249=DIRECTION('ref_axis',(0.,1.,0.));
#5250=DIRECTION('axis',(0.,0.,1.));
#5251=DIRECTION('refdir',(1.,0.,0.));
#5252=DIRECTION('center_axis',(0.,-1.,0.));
#5253=DIRECTION('ref_axis',(1.,0.,0.));
#5254=DIRECTION('center_axis',(0.,-1.,0.));
#5255=DIRECTION('ref_axis',(1.,0.,0.));
#5256=DIRECTION('',(0.,-1.,0.));
#5257=DIRECTION('center_axis',(0.,1.,0.));
#5258=DIRECTION('ref_axis',(1.,0.,0.));
#5259=DIRECTION('center_axis',(0.,1.,0.));
#5260=DIRECTION('ref_axis',(1.,0.,0.));
#5261=DIRECTION('center_axis',(0.,1.,0.));
#5262=DIRECTION('ref_axis',(1.,0.,0.));
#5263=DIRECTION('',(0.,1.,0.));
#5264=DIRECTION('center_axis',(0.,-1.,0.));
#5265=DIRECTION('ref_axis',(1.,0.,0.));
#5266=DIRECTION('center_axis',(-3.66477378287572E-33,-1.,2.99251489117293E-17));
#5267=DIRECTION('ref_axis',(1.,3.66477378287573E-33,2.44929359829471E-16));
#5268=DIRECTION('center_axis',(0.,-1.,0.));
#5269=DIRECTION('ref_axis',(1.,0.,0.));
#5270=DIRECTION('',(3.66477378287572E-33,1.,-2.99251489117293E-17));
#5271=DIRECTION('center_axis',(-3.66477378287572E-33,-1.,2.99251489117293E-17));
#5272=DIRECTION('ref_axis',(1.,3.66477378287573E-33,2.44929359829471E-16));
#5273=DIRECTION('center_axis',(-3.66477378287572E-33,-1.,2.99251489117293E-17));
#5274=DIRECTION('ref_axis',(1.,3.66477378287573E-33,2.44929359829471E-16));
#5275=DIRECTION('center_axis',(0.,1.,0.));
#5276=DIRECTION('ref_axis',(1.,0.,2.44929359829471E-16));
#5277=DIRECTION('',(3.66477378287572E-33,1.,-2.99251489117293E-17));
#5278=DIRECTION('center_axis',(0.,-1.,0.));
#5279=DIRECTION('ref_axis',(1.,0.,0.));
#5280=DIRECTION('center_axis',(0.,1.,0.));
#5281=DIRECTION('ref_axis',(1.,0.,0.));
#5282=DIRECTION('center_axis',(0.,-1.,0.));
#5283=DIRECTION('ref_axis',(1.,0.,0.));
#5284=DIRECTION('',(0.,1.,0.));
#5285=DIRECTION('center_axis',(0.,-1.,0.));
#5286=DIRECTION('ref_axis',(1.,0.,0.));
#5287=DIRECTION('center_axis',(0.,1.,0.));
#5288=DIRECTION('ref_axis',(0.812015371342714,0.,0.583636048152574));
#5289=DIRECTION('center_axis',(0.,1.,0.));
#5290=DIRECTION('ref_axis',(0.812015371342714,0.,0.583636048152574));
#5291=DIRECTION('',(0.,1.,0.));
#5292=DIRECTION('center_axis',(0.,1.,0.));
#5293=DIRECTION('ref_axis',(0.812015371342714,0.,0.583636048152574));
#5294=DIRECTION('',(0.,1.,0.));
#5295=DIRECTION('center_axis',(0.812015371342714,0.,0.583636048152575));
#5296=DIRECTION('ref_axis',(0.583636048152575,0.,-0.812015371342714));
#5297=DIRECTION('',(0.583636048152575,0.,-0.812015371342714));
#5298=DIRECTION('',(0.583636048152575,0.,-0.812015371342714));
#5299=DIRECTION('',(0.,1.,0.));
#5300=DIRECTION('center_axis',(0.,1.,0.));
#5301=DIRECTION('ref_axis',(-0.812015371342714,0.,-0.583636048152575));
#5302=DIRECTION('center_axis',(0.,1.,0.));
#5303=DIRECTION('ref_axis',(-0.812015371342714,0.,-0.583636048152575));
#5304=DIRECTION('center_axis',(0.,1.,0.));
#5305=DIRECTION('ref_axis',(-0.812015371342714,0.,-0.583636048152575));
#5306=DIRECTION('',(0.,1.,0.));
#5307=DIRECTION('center_axis',(0.,1.,0.));
#5308=DIRECTION('ref_axis',(1.,0.,0.));
#5309=DIRECTION('',(-0.812015371342711,0.,-0.583636048152579));
#5310=DIRECTION('',(-0.583636048152575,0.,0.812015371342714));
#5311=DIRECTION('',(-0.583636048152575,0.,0.812015371342714));
#5312=DIRECTION('',(0.812015371342709,0.,0.583636048152581));
#5313=DIRECTION('',(-0.583636048152575,0.,0.812015371342714));
#5314=DIRECTION('center_axis',(0.,1.,0.));
#5315=DIRECTION('ref_axis',(1.,0.,0.));
#5316=DIRECTION('',(-0.583636048152575,0.,0.812015371342714));
#5317=DIRECTION('center_axis',(0.,-1.,0.));
#5318=DIRECTION('ref_axis',(1.,0.,2.44929359829471E-16));
#5319=DIRECTION('center_axis',(-3.66477378287572E-33,-1.,2.99251489117293E-17));
#5320=DIRECTION('ref_axis',(1.,3.66477378287573E-33,2.44929359829471E-16));
#5321=DIRECTION('center_axis',(3.66477378287572E-33,1.,-2.99251489117293E-17));
#5322=DIRECTION('ref_axis',(1.,3.66477378287573E-33,2.44929359829471E-16));
#5323=DIRECTION('',(3.66477378287572E-33,1.,-2.99251489117293E-17));
#5324=DIRECTION('center_axis',(-3.66477378287572E-33,-1.,2.99251489117293E-17));
#5325=DIRECTION('ref_axis',(1.,3.66477378287573E-33,2.44929359829471E-16));
#5326=DIRECTION('center_axis',(-3.66477378287572E-33,-1.,2.99251489117293E-17));
#5327=DIRECTION('ref_axis',(1.,3.66477378287573E-33,2.44929359829471E-16));
#5328=DIRECTION('center_axis',(-0.583636048152579,0.,0.812015371342711));
#5329=DIRECTION('ref_axis',(-0.812015371342711,0.,-0.583636048152579));
#5330=DIRECTION('',(0.812015371342711,0.,0.583636048152579));
#5331=DIRECTION('',(0.,-1.,0.));
#5332=DIRECTION('',(0.,-1.,0.));
#5333=DIRECTION('center_axis',(0.812015371342714,0.,0.583636048152575));
#5334=DIRECTION('ref_axis',(-0.583636048152575,0.,0.812015371342714));
#5335=DIRECTION('',(0.583636048152575,0.,-0.812015371342714));
#5336=DIRECTION('',(0.,-1.,0.));
#5337=DIRECTION('center_axis',(0.583636048152581,0.,-0.812015371342709));
#5338=DIRECTION('ref_axis',(0.812015371342709,0.,0.583636048152581));
#5339=DIRECTION('',(-0.812015371342709,0.,-0.583636048152581));
#5340=DIRECTION('',(0.,-1.,0.));
#5341=DIRECTION('center_axis',(0.,1.,0.));
#5342=DIRECTION('ref_axis',(1.,0.,0.));
#5343=DIRECTION('center_axis',(0.,-1.,0.));
#5344=DIRECTION('ref_axis',(1.,0.,0.));
#5345=DIRECTION('',(0.,1.,0.));
#5346=DIRECTION('center_axis',(0.,-1.,0.));
#5347=DIRECTION('ref_axis',(1.,0.,0.));
#5348=DIRECTION('center_axis',(0.812015371342714,0.,0.583636048152575));
#5349=DIRECTION('ref_axis',(-0.583636048152575,0.,0.812015371342714));
#5350=DIRECTION('',(-0.583636048152575,0.,0.812015371342714));
#5351=DIRECTION('',(0.,-1.,0.));
#5352=DIRECTION('',(-0.583636048152575,0.,0.812015371342714));
#5353=DIRECTION('',(-0.583636048152575,0.,0.812015371342714));
#5354=DIRECTION('',(0.,-1.,0.));
#5355=DIRECTION('center_axis',(0.,1.,0.));
#5356=DIRECTION('ref_axis',(0.812015371342714,0.,0.583636048152574));
#5357=DIRECTION('center_axis',(0.,1.,0.));
#5358=DIRECTION('ref_axis',(0.812015371342714,0.,0.583636048152574));
#5359=DIRECTION('',(0.,-1.,0.));
#5360=DIRECTION('center_axis',(0.,1.,0.));
#5361=DIRECTION('ref_axis',(0.812015371342714,0.,0.583636048152574));
#5362=DIRECTION('center_axis',(-0.812015371342714,0.,-0.583636048152575));
#5363=DIRECTION('ref_axis',(0.583636048152575,0.,-0.812015371342714));
#5364=DIRECTION('',(0.583636048152575,0.,-0.812015371342714));
#5365=DIRECTION('',(0.,-1.,0.));
#5366=DIRECTION('',(0.583636048152575,0.,-0.812015371342714));
#5367=DIRECTION('center_axis',(0.,1.,0.));
#5368=DIRECTION('ref_axis',(-0.812015371342714,0.,-0.583636048152575));
#5369=DIRECTION('center_axis',(0.,1.,0.));
#5370=DIRECTION('ref_axis',(-0.812015371342714,0.,-0.583636048152575));
#5371=DIRECTION('center_axis',(0.,1.,0.));
#5372=DIRECTION('ref_axis',(-0.812015371342714,0.,-0.583636048152575));
#5373=DIRECTION('center_axis',(0.,1.,0.));
#5374=DIRECTION('ref_axis',(1.,0.,0.));
#5375=DIRECTION('center_axis',(0.,1.,0.));
#5376=DIRECTION('ref_axis',(1.,0.,0.));
#5377=DIRECTION('axis',(0.,0.,1.));
#5378=DIRECTION('refdir',(1.,0.,0.));
#5379=DIRECTION('center_axis',(0.,-1.,0.));
#5380=DIRECTION('ref_axis',(1.,0.,0.));
#5381=DIRECTION('center_axis',(0.,-1.,0.));
#5382=DIRECTION('ref_axis',(1.,0.,0.));
#5383=DIRECTION('center_axis',(0.,1.,0.));
#5384=DIRECTION('ref_axis',(1.,0.,0.));
#5385=DIRECTION('center_axis',(0.,1.,0.));
#5386=DIRECTION('ref_axis',(1.,0.,0.));
#5387=DIRECTION('',(0.,-1.,0.));
#5388=DIRECTION('center_axis',(0.,-1.,0.));
#5389=DIRECTION('ref_axis',(1.,0.,0.));
#5390=DIRECTION('axis',(0.,0.,1.));
#5391=DIRECTION('refdir',(1.,0.,0.));
#5392=DIRECTION('center_axis',(0.,1.,0.));
#5393=DIRECTION('ref_axis',(1.,0.,0.));
#5394=DIRECTION('center_axis',(0.,1.,0.));
#5395=DIRECTION('ref_axis',(1.,0.,0.));
#5396=DIRECTION('',(0.,1.,0.));
#5397=DIRECTION('center_axis',(0.,-1.,0.));
#5398=DIRECTION('ref_axis',(1.,0.,0.));
#5399=DIRECTION('center_axis',(0.,1.,0.));
#5400=DIRECTION('ref_axis',(1.,0.,0.));
#5401=DIRECTION('center_axis',(0.,-1.,0.));
#5402=DIRECTION('ref_axis',(1.,0.,0.));
#5403=DIRECTION('',(0.,1.,0.));
#5404=DIRECTION('center_axis',(0.,-1.,0.));
#5405=DIRECTION('ref_axis',(1.,0.,0.));
#5406=DIRECTION('center_axis',(0.812015371342714,0.,-0.583636048152575));
#5407=DIRECTION('ref_axis',(0.583636048152575,0.,0.812015371342714));
#5408=DIRECTION('',(0.583636048152575,0.,0.812015371342714));
#5409=DIRECTION('',(0.,-1.,0.));
#5410=DIRECTION('',(0.583636048152575,0.,0.812015371342714));
#5411=DIRECTION('',(0.,-1.,0.));
#5412=DIRECTION('center_axis',(0.,1.,0.));
#5413=DIRECTION('ref_axis',(0.812015371342714,0.,-0.583636048152574));
#5414=DIRECTION('center_axis',(0.,1.,0.));
#5415=DIRECTION('ref_axis',(0.812015371342714,0.,-0.583636048152574));
#5416=DIRECTION('',(0.,-1.,0.));
#5417=DIRECTION('center_axis',(0.,1.,0.));
#5418=DIRECTION('ref_axis',(0.812015371342714,0.,-0.583636048152574));
#5419=DIRECTION('center_axis',(-0.812015371342714,0.,0.583636048152575));
#5420=DIRECTION('ref_axis',(-0.583636048152575,0.,-0.812015371342714));
#5421=DIRECTION('',(-0.583636048152575,0.,-0.812015371342714));
#5422=DIRECTION('',(0.,-1.,0.));
#5423=DIRECTION('',(-0.583636048152575,0.,-0.812015371342714));
#5424=DIRECTION('center_axis',(0.,1.,0.));
#5425=DIRECTION('ref_axis',(-0.812015371342714,0.,0.583636048152574));
#5426=DIRECTION('center_axis',(0.,1.,0.));
#5427=DIRECTION('ref_axis',(-0.812015371342714,0.,0.583636048152574));
#5428=DIRECTION('center_axis',(0.,1.,0.));
#5429=DIRECTION('ref_axis',(-0.812015371342714,0.,0.583636048152574));
#5430=DIRECTION('center_axis',(0.,1.,0.));
#5431=DIRECTION('ref_axis',(1.,0.,0.));
#5432=DIRECTION('center_axis',(0.,-1.,0.));
#5433=DIRECTION('ref_axis',(1.,0.,0.));
#5434=DIRECTION('center_axis',(0.,1.,0.));
#5435=DIRECTION('ref_axis',(1.,0.,0.));
#5436=DIRECTION('center_axis',(0.,1.,0.));
#5437=DIRECTION('ref_axis',(1.,0.,0.));
#5438=DIRECTION('center_axis',(0.,1.,0.));
#5439=DIRECTION('ref_axis',(1.,0.,0.));
#5440=DIRECTION('center_axis',(0.,1.,0.));
#5441=DIRECTION('ref_axis',(1.,0.,0.));
#5442=DIRECTION('',(0.,-1.,0.));
#5443=DIRECTION('center_axis',(0.,1.,0.));
#5444=DIRECTION('ref_axis',(1.,0.,0.));
#5445=DIRECTION('center_axis',(0.,-1.,0.));
#5446=DIRECTION('ref_axis',(1.,0.,0.));
#5447=DIRECTION('center_axis',(0.,1.,0.));
#5448=DIRECTION('ref_axis',(1.,0.,0.));
#5449=DIRECTION('',(0.,-1.,0.));
#5450=DIRECTION('center_axis',(0.,1.,0.));
#5451=DIRECTION('ref_axis',(1.,0.,0.));
#5452=DIRECTION('axis',(0.,0.,1.));
#5453=DIRECTION('refdir',(1.,0.,0.));
#5454=DIRECTION('center_axis',(0.,-1.,0.));
#5455=DIRECTION('ref_axis',(1.,0.,0.));
#5456=DIRECTION('center_axis',(0.,-1.,0.));
#5457=DIRECTION('ref_axis',(1.,0.,0.));
#5458=DIRECTION('',(0.,-1.,0.));
#5459=DIRECTION('center_axis',(0.,1.,0.));
#5460=DIRECTION('ref_axis',(1.,0.,0.));
#5461=DIRECTION('center_axis',(-1.,0.,0.));
#5462=DIRECTION('ref_axis',(0.,1.,0.));
#5463=DIRECTION('',(-1.,0.,0.));
#5464=DIRECTION('center_axis',(0.,1.,0.));
#5465=DIRECTION('ref_axis',(1.,0.,0.));
#5466=DIRECTION('center_axis',(0.,-1.,0.));
#5467=DIRECTION('ref_axis',(1.,0.,0.));
#5468=DIRECTION('',(0.,1.,0.));
#5469=DIRECTION('center_axis',(0.,-1.,0.));
#5470=DIRECTION('ref_axis',(1.,0.,0.));
#5471=DIRECTION('center_axis',(-0.812015371342714,0.,0.583636048152575));
#5472=DIRECTION('ref_axis',(0.583636048152575,0.,0.812015371342714));
#5473=DIRECTION('',(0.583636048152575,0.,0.812015371342714));
#5474=DIRECTION('',(0.,1.,0.));
#5475=DIRECTION('',(0.583636048152575,0.,0.812015371342714));
#5476=DIRECTION('',(0.,1.,0.));
#5477=DIRECTION('center_axis',(0.,1.,0.));
#5478=DIRECTION('ref_axis',(0.812015371342714,0.,-0.583636048152574));
#5479=DIRECTION('center_axis',(0.,1.,0.));
#5480=DIRECTION('ref_axis',(0.812015371342714,0.,-0.583636048152574));
#5481=DIRECTION('center_axis',(0.,1.,0.));
#5482=DIRECTION('ref_axis',(0.812015371342714,0.,-0.583636048152574));
#5483=DIRECTION('',(0.,1.,0.));
#5484=DIRECTION('center_axis',(0.812015371342714,0.,-0.583636048152575));
#5485=DIRECTION('ref_axis',(-0.583636048152575,0.,-0.812015371342714));
#5486=DIRECTION('',(-0.583636048152575,0.,-0.812015371342714));
#5487=DIRECTION('',(-0.583636048152575,0.,-0.812015371342714));
#5488=DIRECTION('',(0.,1.,0.));
#5489=DIRECTION('center_axis',(0.,1.,0.));
#5490=DIRECTION('ref_axis',(-0.812015371342714,0.,0.583636048152574));
#5491=DIRECTION('center_axis',(0.,1.,0.));
#5492=DIRECTION('ref_axis',(-0.812015371342714,0.,0.583636048152574));
#5493=DIRECTION('center_axis',(0.,1.,0.));
#5494=DIRECTION('ref_axis',(-0.812015371342714,0.,0.583636048152574));
#5495=DIRECTION('center_axis',(0.,1.,0.));
#5496=DIRECTION('ref_axis',(1.,0.,0.));
#5497=DIRECTION('center_axis',(0.,1.,0.));
#5498=DIRECTION('ref_axis',(1.,0.,2.44929359829471E-16));
#5499=DIRECTION('center_axis',(0.,1.,0.));
#5500=DIRECTION('ref_axis',(1.,0.,0.));
#5501=DIRECTION('center_axis',(0.,-1.,0.));
#5502=DIRECTION('ref_axis',(1.,0.,2.44929359829471E-16));
#5503=DIRECTION('center_axis',(-3.66477378287572E-33,-1.,2.99251489117293E-17));
#5504=DIRECTION('ref_axis',(1.,3.66477378287573E-33,2.44929359829471E-16));
#5505=DIRECTION('center_axis',(3.66477378287572E-33,1.,-2.99251489117293E-17));
#5506=DIRECTION('ref_axis',(1.,3.66477378287573E-33,2.44929359829471E-16));
#5507=DIRECTION('',(3.66477378287572E-33,1.,-2.99251489117293E-17));
#5508=DIRECTION('center_axis',(-3.66477378287572E-33,-1.,2.99251489117293E-17));
#5509=DIRECTION('ref_axis',(1.,3.66477378287573E-33,2.44929359829471E-16));
#5510=DIRECTION('center_axis',(-3.66477378287572E-33,-1.,2.99251489117293E-17));
#5511=DIRECTION('ref_axis',(1.,3.66477378287573E-33,2.44929359829471E-16));
#5512=DIRECTION('',(3.66477378287572E-33,1.,-2.99251489117293E-17));
#5513=DIRECTION('',(3.66477378287572E-33,1.,-2.99251489117293E-17));
#5514=DIRECTION('center_axis',(-3.66477378287572E-33,-1.,2.99251489117293E-17));
#5515=DIRECTION('ref_axis',(1.,3.66477378287573E-33,2.44929359829471E-16));
#5516=DIRECTION('center_axis',(-3.66477378287572E-33,-1.,2.99251489117293E-17));
#5517=DIRECTION('ref_axis',(1.,3.66477378287573E-33,2.44929359829471E-16));
#5518=DIRECTION('axis',(0.,0.,1.));
#5519=DIRECTION('refdir',(1.,0.,0.));
#5520=DIRECTION('center_axis',(0.,1.,0.));
#5521=DIRECTION('ref_axis',(1.,0.,0.));
#5522=DIRECTION('center_axis',(0.,1.,0.));
#5523=DIRECTION('ref_axis',(1.,0.,0.));
#5524=DIRECTION('',(0.,1.,0.));
#5525=DIRECTION('center_axis',(-1.08770485875751E-31,-1.,8.88178419700126E-16));
#5526=DIRECTION('ref_axis',(1.,-1.08770485875751E-31,9.66075982551394E-47));
#5527=DIRECTION('center_axis',(0.,1.,0.));
#5528=DIRECTION('ref_axis',(1.,0.,0.));
#5529=DIRECTION('center_axis',(-1.08770485875751E-31,1.,8.88178419700126E-16));
#5530=DIRECTION('ref_axis',(1.,1.08770485875751E-31,9.66075982551394E-47));
#5531=DIRECTION('',(0.,1.,0.));
#5532=DIRECTION('center_axis',(0.,-1.,0.));
#5533=DIRECTION('ref_axis',(1.,0.,0.));
#5534=DIRECTION('center_axis',(0.,1.,0.));
#5535=DIRECTION('ref_axis',(1.,0.,0.));
#5536=DIRECTION('center_axis',(0.,1.,0.));
#5537=DIRECTION('ref_axis',(1.,0.,0.));
#5538=DIRECTION('',(0.,1.,0.));
#5539=DIRECTION('center_axis',(-1.08770485875751E-31,-1.,8.88178419700126E-16));
#5540=DIRECTION('ref_axis',(1.,-1.08770485875751E-31,9.66075982551394E-47));
#5541=DIRECTION('center_axis',(0.,1.,0.));
#5542=DIRECTION('ref_axis',(1.,0.,0.));
#5543=DIRECTION('center_axis',(-1.08770485875751E-31,1.,8.88178419700126E-16));
#5544=DIRECTION('ref_axis',(1.,1.08770485875751E-31,9.66075982551394E-47));
#5545=DIRECTION('',(0.,1.,0.));
#5546=DIRECTION('center_axis',(0.,-1.,0.));
#5547=DIRECTION('ref_axis',(1.,0.,0.));
#5548=DIRECTION('center_axis',(0.,1.,0.));
#5549=DIRECTION('ref_axis',(1.22464679914735E-16,0.,-1.));
#5550=DIRECTION('',(1.,0.,1.22464679914735E-16));
#5551=DIRECTION('',(-1.22464679914735E-16,0.,1.));
#5552=DIRECTION('',(-1.,0.,-1.22464679914735E-16));
#5553=DIRECTION('',(1.22464679914735E-16,0.,-1.));
#5554=DIRECTION('center_axis',(1.22464679914735E-16,0.,-1.));
#5555=DIRECTION('ref_axis',(0.,-1.,0.));
#5556=DIRECTION('',(0.,1.,0.));
#5557=DIRECTION('',(-1.,0.,-1.22464679914735E-16));
#5558=DIRECTION('',(0.,-1.,0.));
#5559=DIRECTION('center_axis',(1.,0.,1.22464679914735E-16));
#5560=DIRECTION('ref_axis',(1.22464679914735E-16,5.92118946466746E-15,-1.));
#5561=DIRECTION('center_axis',(1.,0.,1.22464679914735E-16));
#5562=DIRECTION('ref_axis',(1.22464679914735E-16,5.92118946466746E-15,-1.));
#5563=DIRECTION('',(-1.,0.,-1.22464679914735E-16));
#5564=DIRECTION('center_axis',(-1.,0.,-1.22464679914735E-16));
#5565=DIRECTION('ref_axis',(1.22464679914735E-16,5.92118946466746E-15,-1.));
#5566=DIRECTION('center_axis',(-1.08770485875751E-31,1.,8.88178419700126E-16));
#5567=DIRECTION('ref_axis',(1.22464679914735E-16,8.88178419700126E-16,-1.));
#5568=DIRECTION('',(-1.22464679914735E-16,-8.88178419700126E-16,1.));
#5569=DIRECTION('',(-1.,0.,-1.22464679914735E-16));
#5570=DIRECTION('',(1.22464679914735E-16,8.88178419700126E-16,-1.));
#5571=DIRECTION('center_axis',(1.,0.,1.22464679914735E-16));
#5572=DIRECTION('ref_axis',(-1.0877048587575E-30,1.,8.88178419700118E-15));
#5573=DIRECTION('center_axis',(1.,0.,1.22464679914735E-16));
#5574=DIRECTION('ref_axis',(-1.0877048587575E-30,1.,8.88178419700118E-15));
#5575=DIRECTION('',(-1.,0.,-1.22464679914735E-16));
#5576=DIRECTION('center_axis',(-1.,0.,-1.22464679914735E-16));
#5577=DIRECTION('ref_axis',(-1.0877048587575E-30,1.,8.88178419700118E-15));
#5578=DIRECTION('center_axis',(1.,0.,1.22464679914735E-16));
#5579=DIRECTION('ref_axis',(-9.29081233522032E-31,1.,7.58652400160517E-15));
#5580=DIRECTION('',(-1.,0.,-1.22464679914735E-16));
#5581=DIRECTION('center_axis',(-1.,0.,-1.22464679914735E-16));
#5582=DIRECTION('ref_axis',(-9.29081233522032E-31,1.,7.58652400160517E-15));
#5583=DIRECTION('',(-1.,0.,-1.22464679914735E-16));
#5584=DIRECTION('center_axis',(1.,0.,1.22464679914735E-16));
#5585=DIRECTION('ref_axis',(-9.29081233522032E-31,1.,7.58652400160517E-15));
#5586=DIRECTION('center_axis',(0.,-1.,0.));
#5587=DIRECTION('ref_axis',(-1.22464679914735E-16,0.,1.));
#5588=DIRECTION('',(1.22464679914735E-16,0.,-1.));
#5589=DIRECTION('',(-1.,0.,-1.22464679914735E-16));
#5590=DIRECTION('',(-1.22464679914735E-16,0.,1.));
#5591=DIRECTION('center_axis',(1.,0.,1.22464679914735E-16));
#5592=DIRECTION('ref_axis',(1.22464679914735E-16,5.92118946466745E-15,-1.));
#5593=DIRECTION('center_axis',(-1.,0.,-1.22464679914735E-16));
#5594=DIRECTION('ref_axis',(1.22464679914735E-16,5.92118946466745E-15,-1.));
#5595=DIRECTION('',(-1.,0.,-1.22464679914735E-16));
#5596=DIRECTION('center_axis',(1.,0.,1.22464679914735E-16));
#5597=DIRECTION('ref_axis',(1.22464679914735E-16,5.92118946466745E-15,-1.));
#5598=DIRECTION('center_axis',(-1.22464679914735E-16,0.,1.));
#5599=DIRECTION('ref_axis',(0.,1.,0.));
#5600=DIRECTION('',(0.,-1.,0.));
#5601=DIRECTION('',(0.,1.,0.));
#5602=DIRECTION('center_axis',(-1.,0.,-1.22464679914735E-16));
#5603=DIRECTION('ref_axis',(0.,1.,0.));
#5604=DIRECTION('',(0.,1.,0.));
#5605=DIRECTION('',(-1.22464679914735E-16,0.,1.));
#5606=DIRECTION('',(0.,-1.,0.));
#5607=DIRECTION('center_axis',(-1.,0.,-1.22464679914735E-16));
#5608=DIRECTION('ref_axis',(1.22464679914735E-16,-5.92118946466746E-15,
-1.));
#5609=DIRECTION('',(-1.22464679914735E-16,8.88178419700126E-16,1.));
#5610=DIRECTION('center_axis',(-1.,0.,-1.22464679914735E-16));
#5611=DIRECTION('ref_axis',(-1.0877048587575E-30,-1.,8.88178419700118E-15));
#5612=DIRECTION('',(-9.32958193124582E-34,1.,7.61818177922111E-18));
#5613=DIRECTION('',(-1.83238689143786E-33,1.,1.49625744558646E-17));
#5614=DIRECTION('center_axis',(1.,0.,1.22464679914735E-16));
#5615=DIRECTION('ref_axis',(-9.29081233522032E-31,-1.,7.58652400160517E-15));
#5616=DIRECTION('',(1.22464679914735E-16,0.,-1.));
#5617=DIRECTION('center_axis',(1.,0.,1.22464679914735E-16));
#5618=DIRECTION('ref_axis',(1.22464679914735E-16,-5.92118946466745E-15,
-1.));
#5619=DIRECTION('center_axis',(0.,1.,0.));
#5620=DIRECTION('ref_axis',(1.22464679914735E-16,0.,-1.));
#5621=DIRECTION('',(1.,0.,1.22464679914735E-16));
#5622=DIRECTION('',(1.22464679914735E-16,0.,-1.));
#5623=DIRECTION('',(-1.,0.,-1.22464679914735E-16));
#5624=DIRECTION('center_axis',(-1.22464679914735E-16,0.,1.));
#5625=DIRECTION('ref_axis',(0.,1.,0.));
#5626=DIRECTION('',(0.,1.,0.));
#5627=DIRECTION('',(-1.,0.,-1.22464679914735E-16));
#5628=DIRECTION('center_axis',(-1.,0.,-1.22464679914735E-16));
#5629=DIRECTION('ref_axis',(1.22464679914735E-16,-5.92118946466746E-15,
-1.));
#5630=DIRECTION('center_axis',(1.,0.,1.22464679914735E-16));
#5631=DIRECTION('ref_axis',(1.22464679914735E-16,-5.92118946466746E-15,
-1.));
#5632=DIRECTION('',(-1.,0.,-1.22464679914735E-16));
#5633=DIRECTION('center_axis',(1.08770485875751E-31,1.,-8.88178419700126E-16));
#5634=DIRECTION('ref_axis',(1.22464679914735E-16,-8.88178419700126E-16,
-1.));
#5635=DIRECTION('',(1.22464679914735E-16,-8.88178419700126E-16,-1.));
#5636=DIRECTION('',(-1.,0.,-1.22464679914735E-16));
#5637=DIRECTION('center_axis',(-1.,0.,-1.22464679914735E-16));
#5638=DIRECTION('ref_axis',(-1.0877048587575E-30,-1.,8.88178419700118E-15));
#5639=DIRECTION('center_axis',(1.,0.,1.22464679914735E-16));
#5640=DIRECTION('ref_axis',(-1.0877048587575E-30,-1.,8.88178419700118E-15));
#5641=DIRECTION('',(-1.,0.,-1.22464679914735E-16));
#5642=DIRECTION('center_axis',(1.22464679914735E-16,7.61818177922111E-18,
-1.));
#5643=DIRECTION('ref_axis',(9.32958193124582E-34,-1.,-7.61818177922111E-18));
#5644=DIRECTION('',(9.32958193124582E-34,1.,-7.61818177922111E-18));
#5645=DIRECTION('center_axis',(-1.22464679914735E-16,1.49625744558646E-17,
1.));
#5646=DIRECTION('ref_axis',(1.83238689143786E-33,1.,-1.49625744558646E-17));
#5647=DIRECTION('',(1.83238689143786E-33,1.,-1.49625744558646E-17));
#5648=DIRECTION('',(-1.,0.,-1.22464679914735E-16));
#5649=DIRECTION('center_axis',(-1.,0.,-1.22464679914735E-16));
#5650=DIRECTION('ref_axis',(-9.29081233522032E-31,-1.,7.58652400160517E-15));
#5651=DIRECTION('center_axis',(-1.,0.,-1.22464679914735E-16));
#5652=DIRECTION('ref_axis',(-9.29081233522032E-31,-1.,7.58652400160517E-15));
#5653=DIRECTION('',(-1.,0.,-1.22464679914735E-16));
#5654=DIRECTION('center_axis',(0.,-1.,0.));
#5655=DIRECTION('ref_axis',(-1.22464679914735E-16,0.,1.));
#5656=DIRECTION('',(-1.22464679914735E-16,0.,1.));
#5657=DIRECTION('',(-1.,0.,-1.22464679914735E-16));
#5658=DIRECTION('center_axis',(-1.,0.,-1.22464679914735E-16));
#5659=DIRECTION('ref_axis',(1.22464679914735E-16,-5.92118946466745E-15,
-1.));
#5660=DIRECTION('center_axis',(-1.,0.,-1.22464679914735E-16));
#5661=DIRECTION('ref_axis',(1.22464679914735E-16,-5.92118946466745E-15,
-1.));
#5662=DIRECTION('',(-1.,0.,-1.22464679914735E-16));
#5663=DIRECTION('center_axis',(1.22464679914735E-16,0.,-1.));
#5664=DIRECTION('ref_axis',(0.,-1.,0.));
#5665=DIRECTION('',(0.,-1.,0.));
#5666=DIRECTION('center_axis',(-1.,0.,-1.22464679914735E-16));
#5667=DIRECTION('ref_axis',(0.,1.,0.));
#5668=DIRECTION('axis',(0.,0.,1.));
#5669=DIRECTION('refdir',(1.,0.,0.));
#5670=DIRECTION('center_axis',(-1.,0.,0.));
#5671=DIRECTION('ref_axis',(0.,-0.609000462850127,-0.793169865948229));
#5672=DIRECTION('',(-1.,0.,0.));
#5673=DIRECTION('center_axis',(-1.,0.,0.));
#5674=DIRECTION('ref_axis',(0.,-0.609000462850127,-0.793169865948229));
#5675=DIRECTION('',(-1.,0.,0.));
#5676=DIRECTION('center_axis',(-1.,0.,0.));
#5677=DIRECTION('ref_axis',(0.,1.,0.));
#5678=DIRECTION('center_axis',(-1.,0.,0.));
#5679=DIRECTION('ref_axis',(0.,0.859771171146174,-0.51067948193161));
#5680=DIRECTION('',(-1.,0.,0.));
#5681=DIRECTION('center_axis',(-1.,0.,0.));
#5682=DIRECTION('ref_axis',(0.,1.,0.));
#5683=DIRECTION('center_axis',(-1.,0.,0.));
#5684=DIRECTION('ref_axis',(0.,0.936836199765117,-0.3497684016741));
#5685=DIRECTION('center_axis',(-1.,0.,0.));
#5686=DIRECTION('ref_axis',(0.,-0.609000462850127,-0.793169865948229));
#5687=DIRECTION('center_axis',(1.,0.,0.));
#5688=DIRECTION('ref_axis',(0.,0.,-1.));
#5689=DIRECTION('',(0.,-1.,0.));
#5690=DIRECTION('center_axis',(1.,0.,0.));
#5691=DIRECTION('ref_axis',(0.,1.,0.));
#5692=DIRECTION('center_axis',(-1.,0.,0.));
#5693=DIRECTION('ref_axis',(0.,1.,0.));
#5694=DIRECTION('center_axis',(-1.,0.,0.));
#5695=DIRECTION('ref_axis',(0.,1.,0.));
#5696=DIRECTION('center_axis',(0.882978451059903,-0.305829609536471,0.356114173959174));
#5697=DIRECTION('ref_axis',(0.46437508102478,0.679952147198259,-0.5674688199749));
#5698=DIRECTION('center_axis',(0.,1.,0.));
#5699=DIRECTION('ref_axis',(1.,0.,0.));
#5700=DIRECTION('center_axis',(0.,1.,0.));
#5701=DIRECTION('ref_axis',(1.,0.,0.));
#5702=DIRECTION('',(0.,1.,0.));
#5703=DIRECTION('',(0.,1.,0.));
#5704=DIRECTION('center_axis',(0.,-1.,0.));
#5705=DIRECTION('ref_axis',(1.,0.,0.));
#5706=DIRECTION('center_axis',(-1.,0.,0.));
#5707=DIRECTION('ref_axis',(0.,1.,0.));
#5708=DIRECTION('center_axis',(-1.,0.,0.));
#5709=DIRECTION('ref_axis',(0.,1.,0.));
#5710=DIRECTION('center_axis',(-1.,0.,0.));
#5711=DIRECTION('ref_axis',(0.,1.,0.));
#5712=DIRECTION('',(-1.,0.,0.));
#5713=DIRECTION('center_axis',(1.,0.,0.));
#5714=DIRECTION('ref_axis',(0.,1.,0.));
#5715=DIRECTION('center_axis',(0.,1.,0.));
#5716=DIRECTION('ref_axis',(1.,0.,0.));
#5717=DIRECTION('',(-1.,0.,0.));
#5718=DIRECTION('',(0.,0.,-1.));
#5719=DIRECTION('',(1.,0.,0.));
#5720=DIRECTION('',(0.,0.,1.));
#5721=DIRECTION('center_axis',(-1.,0.,0.));
#5722=DIRECTION('ref_axis',(0.,0.,1.));
#5723=DIRECTION('',(0.,-1.,0.));
#5724=DIRECTION('',(0.,0.,1.));
#5725=DIRECTION('',(0.,1.,0.));
#5726=DIRECTION('center_axis',(0.,0.,-1.));
#5727=DIRECTION('ref_axis',(-1.,0.,0.));
#5728=DIRECTION('',(-1.,0.,0.));
#5729=DIRECTION('',(0.,1.,0.));
#5730=DIRECTION('center_axis',(1.,0.,0.));
#5731=DIRECTION('ref_axis',(0.,0.,-1.));
#5732=DIRECTION('',(0.,0.,-1.));
#5733=DIRECTION('',(0.,1.,0.));
#5734=DIRECTION('center_axis',(0.,0.,1.));
#5735=DIRECTION('ref_axis',(1.,0.,0.));
#5736=DIRECTION('',(1.,0.,0.));
#5737=DIRECTION('center_axis',(0.,1.,0.));
#5738=DIRECTION('ref_axis',(1.,0.,0.));
#5739=DIRECTION('axis',(0.,0.,1.));
#5740=DIRECTION('refdir',(1.,0.,0.));
#5741=DIRECTION('center_axis',(0.,1.,0.));
#5742=DIRECTION('ref_axis',(1.,0.,0.));
#5743=DIRECTION('center_axis',(0.,-1.,0.));
#5744=DIRECTION('ref_axis',(1.,0.,0.));
#5745=DIRECTION('center_axis',(0.,1.,0.));
#5746=DIRECTION('ref_axis',(1.,0.,0.));
#5747=DIRECTION('center_axis',(0.,1.,0.));
#5748=DIRECTION('ref_axis',(1.,0.,0.));
#5749=DIRECTION('',(0.,-1.,0.));
#5750=DIRECTION('center_axis',(0.,1.,0.));
#5751=DIRECTION('ref_axis',(1.,0.,0.));
#5752=DIRECTION('axis',(0.,0.,1.));
#5753=DIRECTION('refdir',(1.,0.,0.));
#5754=DIRECTION('center_axis',(-1.,0.,0.));
#5755=DIRECTION('ref_axis',(0.,1.,0.));
#5756=DIRECTION('center_axis',(-1.,0.,0.));
#5757=DIRECTION('ref_axis',(0.,1.,0.));
#5758=DIRECTION('center_axis',(-1.,0.,0.));
#5759=DIRECTION('ref_axis',(0.,1.,0.));
#5760=DIRECTION('center_axis',(-1.,0.,0.));
#5761=DIRECTION('ref_axis',(0.,1.,2.00814192590157E-12));
#5762=DIRECTION('center_axis',(-1.,0.,0.));
#5763=DIRECTION('ref_axis',(0.,1.,2.00814192590157E-12));
#5764=DIRECTION('center_axis',(1.,0.,0.));
#5765=DIRECTION('ref_axis',(0.,1.,2.00814192590157E-12));
#5766=DIRECTION('center_axis',(1.,0.,0.));
#5767=DIRECTION('ref_axis',(0.,1.,0.));
#5768=DIRECTION('center_axis',(1.,0.,0.));
#5769=DIRECTION('ref_axis',(0.,1.,0.));
#5770=DIRECTION('',(0.,-0.5,0.866025403784439));
#5771=DIRECTION('',(0.,0.5,0.866025403784439));
#5772=DIRECTION('',(0.,1.,0.));
#5773=DIRECTION('',(0.,0.499999999999999,-0.866025403784439));
#5774=DIRECTION('',(0.,-0.500000000000001,-0.866025403784438));
#5775=DIRECTION('',(0.,-1.,0.));
#5776=DIRECTION('center_axis',(1.,0.,0.));
#5777=DIRECTION('ref_axis',(0.,1.,0.));
#5778=DIRECTION('',(-1.,0.,0.));
#5779=DIRECTION('center_axis',(1.,0.,0.));
#5780=DIRECTION('ref_axis',(0.,1.,0.));
#5781=DIRECTION('center_axis',(0.,-0.866025403784439,-0.499999999999999));
#5782=DIRECTION('ref_axis',(0.,0.499999999999999,-0.866025403784439));
#5783=DIRECTION('',(1.,0.,0.));
#5784=DIRECTION('',(0.,0.499999999999999,-0.866025403784439));
#5785=DIRECTION('',(1.,0.,0.));
#5786=DIRECTION('center_axis',(0.,0.,-1.));
#5787=DIRECTION('ref_axis',(0.,1.,0.));
#5788=DIRECTION('',(1.,0.,0.));
#5789=DIRECTION('',(0.,1.,0.));
#5790=DIRECTION('center_axis',(0.,0.866025403784439,-0.5));
#5791=DIRECTION('ref_axis',(0.,0.5,0.866025403784439));
#5792=DIRECTION('',(1.,0.,0.));
#5793=DIRECTION('',(0.,0.5,0.866025403784439));
#5794=DIRECTION('center_axis',(1.,0.,0.));
#5795=DIRECTION('ref_axis',(0.,1.,0.));
#5796=DIRECTION('center_axis',(0.,0.866025403784439,0.5));
#5797=DIRECTION('ref_axis',(0.,-0.5,0.866025403784439));
#5798=DIRECTION('',(1.,0.,0.));
#5799=DIRECTION('',(0.,-0.5,0.866025403784439));
#5800=DIRECTION('center_axis',(0.,-0.866025403784438,0.500000000000001));
#5801=DIRECTION('ref_axis',(0.,-0.500000000000001,-0.866025403784438));
#5802=DIRECTION('',(0.,-0.500000000000001,-0.866025403784438));
#5803=DIRECTION('',(1.,0.,0.));
#5804=DIRECTION('center_axis',(0.,0.,1.));
#5805=DIRECTION('ref_axis',(0.,-1.,0.));
#5806=DIRECTION('',(0.,-1.,0.));
#5807=DIRECTION('center_axis',(1.,0.,0.));
#5808=DIRECTION('ref_axis',(0.,0.,-1.));
#5809=DIRECTION('center_axis',(1.,0.,0.));
#5810=DIRECTION('ref_axis',(0.,1.,0.));
#5811=DIRECTION('',(0.,0.,1.));
#5812=DIRECTION('',(1.,0.,0.));
#5813=DIRECTION('',(0.,0.,1.));
#5814=DIRECTION('',(1.,0.,0.));
#5815=DIRECTION('',(0.,0.,1.));
#5816=DIRECTION('',(1.,0.,0.));
#5817=DIRECTION('',(0.,0.,1.));
#5818=DIRECTION('',(1.,0.,0.));
#5819=DIRECTION('',(0.,0.,1.));
#5820=DIRECTION('',(1.,0.,0.));
#5821=DIRECTION('',(0.,0.,1.));
#5822=DIRECTION('',(1.,0.,0.));
#5823=DIRECTION('',(0.,0.,1.));
#5824=DIRECTION('',(1.,0.,0.));
#5825=DIRECTION('',(0.,0.,1.));
#5826=DIRECTION('',(1.,0.,0.));
#5827=DIRECTION('',(0.,0.,1.));
#5828=DIRECTION('',(1.,0.,0.));
#5829=CARTESIAN_POINT('',(0.,0.,0.));
#5830=CARTESIAN_POINT('',(0.,0.,0.));
#5831=CARTESIAN_POINT('Origin',(-54.7683231875009,0.,15.));
#5832=CARTESIAN_POINT('',(-62.2683231875009,-114.3,15.));
#5833=CARTESIAN_POINT('Origin',(-54.7683231875009,-114.3,15.));
#5834=CARTESIAN_POINT('',(-62.2683231875009,-112.3,15.));
#5835=CARTESIAN_POINT('',(-62.2683231875009,0.,15.));
#5836=CARTESIAN_POINT('Origin',(-54.7683231875009,-112.3,15.));
#5837=CARTESIAN_POINT('Origin',(-54.7683231875009,0.,15.));
#5838=CARTESIAN_POINT('',(-62.2683231875009,112.3,15.));
#5839=CARTESIAN_POINT('Origin',(-54.7683231875009,112.3,15.));
#5840=CARTESIAN_POINT('',(-62.2683231875009,114.3,15.));
#5841=CARTESIAN_POINT('',(-62.2683231875009,0.,15.));
#5842=CARTESIAN_POINT('Origin',(-54.7683231875009,114.3,15.));
#5843=CARTESIAN_POINT('Origin',(175.231676812499,0.,15.));
#5844=CARTESIAN_POINT('',(167.731676812499,-114.3,15.));
#5845=CARTESIAN_POINT('Origin',(175.231676812499,-114.3,15.));
#5846=CARTESIAN_POINT('',(167.731676812499,-112.3,15.));
#5847=CARTESIAN_POINT('',(167.731676812499,0.,15.));
#5848=CARTESIAN_POINT('Origin',(175.231676812499,-112.3,15.));
#5849=CARTESIAN_POINT('Origin',(175.231676812499,0.,15.));
#5850=CARTESIAN_POINT('',(167.731676812499,112.3,15.));
#5851=CARTESIAN_POINT('Origin',(175.231676812499,112.3,15.));
#5852=CARTESIAN_POINT('',(167.731676812499,114.3,15.));
#5853=CARTESIAN_POINT('',(167.731676812499,0.,15.));
#5854=CARTESIAN_POINT('Origin',(175.231676812499,114.3,15.));
#5855=CARTESIAN_POINT('Origin',(0.,99.3,28.));
#5856=CARTESIAN_POINT('',(198.,99.3,30.));
#5857=CARTESIAN_POINT('',(-198.,99.3,30.));
#5858=CARTESIAN_POINT('',(0.,99.3,30.));
#5859=CARTESIAN_POINT('',(-198.,99.3,28.));
#5860=CARTESIAN_POINT('',(-198.,99.3,30.));
#5861=CARTESIAN_POINT('',(198.,99.3,28.));
#5862=CARTESIAN_POINT('',(0.,99.3,28.));
#5863=CARTESIAN_POINT('',(198.,99.3,30.));
#5864=CARTESIAN_POINT('Origin',(0.,109.3,28.));
#5865=CARTESIAN_POINT('',(-198.,109.3,28.));
#5866=CARTESIAN_POINT('',(-198.,112.3,28.));
#5867=CARTESIAN_POINT('',(198.,109.3,28.));
#5868=CARTESIAN_POINT('',(0.,109.3,28.));
#5869=CARTESIAN_POINT('',(198.,112.3,28.));
#5870=CARTESIAN_POINT('Origin',(0.,109.3,25.));
#5871=CARTESIAN_POINT('',(-198.,112.3,25.));
#5872=CARTESIAN_POINT('Origin',(-198.,109.3,25.));
#5873=CARTESIAN_POINT('',(198.,112.3,25.));
#5874=CARTESIAN_POINT('',(0.,112.3,25.));
#5875=CARTESIAN_POINT('Origin',(198.,109.3,25.));
#5876=CARTESIAN_POINT('Origin',(0.,112.3,5.));
#5877=CARTESIAN_POINT('',(-198.,112.3,5.));
#5878=CARTESIAN_POINT('',(-198.,112.3,5.));
#5879=CARTESIAN_POINT('',(198.,112.3,5.));
#5880=CARTESIAN_POINT('',(0.,112.3,5.));
#5881=CARTESIAN_POINT('',(198.,112.3,5.));
#5882=CARTESIAN_POINT('Origin',(0.,109.3,5.00000000000003));
#5883=CARTESIAN_POINT('',(-198.,109.3,2.));
#5884=CARTESIAN_POINT('Origin',(-198.,109.3,5.00000000000003));
#5885=CARTESIAN_POINT('',(198.,109.3,2.));
#5886=CARTESIAN_POINT('',(0.,109.3,2.));
#5887=CARTESIAN_POINT('Origin',(198.,109.3,5.00000000000003));
#5888=CARTESIAN_POINT('Origin',(0.,111.3,3.00000000000002));
#5889=CARTESIAN_POINT('',(-198.,111.3,0.));
#5890=CARTESIAN_POINT('',(198.,111.3,0.));
#5891=CARTESIAN_POINT('',(0.,111.3,-2.22044604925031E-15));
#5892=CARTESIAN_POINT('',(-198.,114.3,3.));
#5893=CARTESIAN_POINT('Origin',(-198.,111.3,3.00000000000002));
#5894=CARTESIAN_POINT('',(198.,114.3,3.));
#5895=CARTESIAN_POINT('',(0.,114.3,3.));
#5896=CARTESIAN_POINT('Origin',(198.,111.3,3.00000000000002));
#5897=CARTESIAN_POINT('Origin',(0.,114.3,27.));
#5898=CARTESIAN_POINT('',(-198.,114.3,27.));
#5899=CARTESIAN_POINT('',(-198.,114.3,3.));
#5900=CARTESIAN_POINT('',(198.,114.3,27.));
#5901=CARTESIAN_POINT('',(0.,114.3,27.));
#5902=CARTESIAN_POINT('',(198.,114.3,3.));
#5903=CARTESIAN_POINT('Origin',(0.,111.3,27.));
#5904=CARTESIAN_POINT('',(-198.,111.3,30.));
#5905=CARTESIAN_POINT('Origin',(-198.,111.3,27.));
#5906=CARTESIAN_POINT('',(198.,111.3,30.));
#5907=CARTESIAN_POINT('',(0.,111.3,30.));
#5908=CARTESIAN_POINT('Origin',(198.,111.3,27.));
#5909=CARTESIAN_POINT('Origin',(0.,99.3,30.));
#5910=CARTESIAN_POINT('',(-198.,111.3,30.));
#5911=CARTESIAN_POINT('',(198.,111.3,30.));
#5912=CARTESIAN_POINT('Origin',(-198.,-57.15,15.));
#5913=CARTESIAN_POINT('',(-198.,-111.3,30.));
#5914=CARTESIAN_POINT('',(-198.,-99.3,30.));
#5915=CARTESIAN_POINT('',(-198.,-111.3,30.));
#5916=CARTESIAN_POINT('',(-198.,-99.3,28.));
#5917=CARTESIAN_POINT('',(-198.,-99.3,30.));
#5918=CARTESIAN_POINT('',(-198.,-109.3,28.));
#5919=CARTESIAN_POINT('',(-198.,-112.3,28.));
#5920=CARTESIAN_POINT('',(-198.,-112.3,25.));
#5921=CARTESIAN_POINT('Origin',(-198.,-109.3,25.));
#5922=CARTESIAN_POINT('',(-198.,-112.3,5.));
#5923=CARTESIAN_POINT('',(-198.,-112.3,5.));
#5924=CARTESIAN_POINT('',(-198.,-109.3,2.));
#5925=CARTESIAN_POINT('Origin',(-198.,-109.3,5.00000000000003));
#5926=CARTESIAN_POINT('',(-198.,0.,2.));
#5927=CARTESIAN_POINT('',(-198.,-111.3,0.));
#5928=CARTESIAN_POINT('',(-198.,0.,0.));
#5929=CARTESIAN_POINT('',(-198.,-114.3,3.));
#5930=CARTESIAN_POINT('Origin',(-198.,-111.3,3.00000000000002));
#5931=CARTESIAN_POINT('',(-198.,-114.3,27.));
#5932=CARTESIAN_POINT('',(-198.,-114.3,3.));
#5933=CARTESIAN_POINT('Origin',(-198.,-111.3,27.));
#5934=CARTESIAN_POINT('Origin',(0.,-99.3,28.));
#5935=CARTESIAN_POINT('',(198.,-99.3,30.));
#5936=CARTESIAN_POINT('',(0.,-99.3,30.));
#5937=CARTESIAN_POINT('',(198.,-99.3,28.));
#5938=CARTESIAN_POINT('',(198.,-99.3,30.));
#5939=CARTESIAN_POINT('',(0.,-99.3,28.));
#5940=CARTESIAN_POINT('Origin',(0.,-109.3,28.));
#5941=CARTESIAN_POINT('',(198.,-109.3,28.));
#5942=CARTESIAN_POINT('',(198.,-112.3,28.));
#5943=CARTESIAN_POINT('',(0.,-109.3,28.));
#5944=CARTESIAN_POINT('Origin',(0.,-109.3,25.));
#5945=CARTESIAN_POINT('',(198.,-112.3,25.));
#5946=CARTESIAN_POINT('Origin',(198.,-109.3,25.));
#5947=CARTESIAN_POINT('',(0.,-112.3,25.));
#5948=CARTESIAN_POINT('Origin',(0.,-112.3,5.));
#5949=CARTESIAN_POINT('',(198.,-112.3,5.));
#5950=CARTESIAN_POINT('',(198.,-112.3,5.));
#5951=CARTESIAN_POINT('',(0.,-112.3,5.));
#5952=CARTESIAN_POINT('Origin',(0.,-109.3,5.00000000000003));
#5953=CARTESIAN_POINT('',(198.,-109.3,2.));
#5954=CARTESIAN_POINT('Origin',(198.,-109.3,5.00000000000003));
#5955=CARTESIAN_POINT('',(0.,-109.3,2.));
#5956=CARTESIAN_POINT('Origin',(0.,0.,2.));
#5957=CARTESIAN_POINT('',(198.,0.,2.));
#5958=CARTESIAN_POINT('Origin',(0.,-111.3,-1.66533453693773E-15));
#5959=CARTESIAN_POINT('',(198.,-111.3,0.));
#5960=CARTESIAN_POINT('',(198.,0.,0.));
#5961=CARTESIAN_POINT('',(0.,-111.3,-2.22044604925031E-15));
#5962=CARTESIAN_POINT('Origin',(0.,-111.3,3.00000000000002));
#5963=CARTESIAN_POINT('',(198.,-114.3,3.));
#5964=CARTESIAN_POINT('Origin',(198.,-111.3,3.00000000000002));
#5965=CARTESIAN_POINT('',(0.,-114.3,3.));
#5966=CARTESIAN_POINT('Origin',(0.,-114.3,27.));
#5967=CARTESIAN_POINT('',(198.,-114.3,27.));
#5968=CARTESIAN_POINT('',(198.,-114.3,3.));
#5969=CARTESIAN_POINT('',(0.,-114.3,27.));
#5970=CARTESIAN_POINT('Origin',(0.,-111.3,27.));
#5971=CARTESIAN_POINT('',(198.,-111.3,30.));
#5972=CARTESIAN_POINT('Origin',(198.,-111.3,27.));
#5973=CARTESIAN_POINT('',(0.,-111.3,30.));
#5974=CARTESIAN_POINT('Origin',(0.,-99.3,30.));
#5975=CARTESIAN_POINT('',(198.,-111.3,30.));
#5976=CARTESIAN_POINT('Origin',(198.,-57.15,15.));
#5977=CARTESIAN_POINT('',(0.,0.,0.));
#5978=CARTESIAN_POINT('Origin',(60.231676812499,-90.,175.));
#5979=CARTESIAN_POINT('',(54.231676812499,-82.,175.));
#5980=CARTESIAN_POINT('Origin',(60.231676812499,-82.,175.));
#5981=CARTESIAN_POINT('',(54.231676812499,-90.,175.));
#5982=CARTESIAN_POINT('',(54.231676812499,-90.,175.));
#5983=CARTESIAN_POINT('Origin',(60.231676812499,-90.,175.));
#5984=CARTESIAN_POINT('Origin',(60.231676812499,-90.,175.));
#5985=CARTESIAN_POINT('',(54.231676812499,82.,175.));
#5986=CARTESIAN_POINT('Origin',(60.231676812499,82.,175.));
#5987=CARTESIAN_POINT('',(54.231676812499,90.,175.));
#5988=CARTESIAN_POINT('',(54.231676812499,-90.,175.));
#5989=CARTESIAN_POINT('Origin',(60.231676812499,90.,175.));
#5990=CARTESIAN_POINT('Origin',(-54.768323187501,4.78802382587669E-15,335.));
#5991=CARTESIAN_POINT('',(-62.268323187501,90.,335.));
#5992=CARTESIAN_POINT('Origin',(-54.768323187501,90.,335.));
#5993=CARTESIAN_POINT('',(-62.268323187501,118.,335.));
#5994=CARTESIAN_POINT('',(-62.268323187501,4.78802382587669E-15,335.));
#5995=CARTESIAN_POINT('Origin',(-54.768323187501,118.,335.));
#5996=CARTESIAN_POINT('Origin',(-54.768323187501,4.78802382587669E-15,335.));
#5997=CARTESIAN_POINT('',(-62.268323187501,-82.,335.));
#5998=CARTESIAN_POINT('Origin',(-54.768323187501,-82.,335.));
#5999=CARTESIAN_POINT('',(-62.268323187501,82.,335.));
#6000=CARTESIAN_POINT('',(-62.268323187501,4.78802382587669E-15,335.));
#6001=CARTESIAN_POINT('Origin',(-54.768323187501,82.,335.));
#6002=CARTESIAN_POINT('Origin',(175.231676812499,-90.,15.));
#6003=CARTESIAN_POINT('',(167.731676812499,-90.,15.));
#6004=CARTESIAN_POINT('Origin',(175.231676812499,-90.,15.));
#6005=CARTESIAN_POINT('',(167.731676812499,-82.,15.));
#6006=CARTESIAN_POINT('',(167.731676812499,-90.,15.));
#6007=CARTESIAN_POINT('Origin',(175.231676812499,-82.,15.));
#6008=CARTESIAN_POINT('Origin',(175.231676812499,-90.,15.));
#6009=CARTESIAN_POINT('',(184.975861268612,-90.,22.0036325778309));
#6010=CARTESIAN_POINT('',(165.487492356386,-90.,7.99636742216909));
#6011=CARTESIAN_POINT('Origin',(175.231676812499,-90.,15.));
#6012=CARTESIAN_POINT('',(165.487492356386,-82.,7.99636742216912));
#6013=CARTESIAN_POINT('',(165.487492356386,-90.,7.99636742216909));
#6014=CARTESIAN_POINT('',(184.975861268612,-82.,22.0036325778309));
#6015=CARTESIAN_POINT('Origin',(175.231676812499,-82.,15.));
#6016=CARTESIAN_POINT('',(184.975861268612,-90.,22.0036325778309));
#6017=CARTESIAN_POINT('Origin',(-45.0241387313884,-90.,342.003632577831));
#6018=CARTESIAN_POINT('',(-45.0241387313884,-90.,342.003632577831));
#6019=CARTESIAN_POINT('',(-45.0241387313884,-90.,342.003632577831));
#6020=CARTESIAN_POINT('',(-45.0241387313884,-82.,342.003632577831));
#6021=CARTESIAN_POINT('',(-45.0241387313884,-82.,342.003632577831));
#6022=CARTESIAN_POINT('',(-45.0241387313884,-90.,342.003632577831));
#6023=CARTESIAN_POINT('Origin',(-54.768323187501,-90.,335.));
#6024=CARTESIAN_POINT('',(-64.5125076436135,-90.,327.996367422169));
#6025=CARTESIAN_POINT('Origin',(-54.768323187501,-90.,335.));
#6026=CARTESIAN_POINT('',(-64.5125076436135,-82.,327.996367422169));
#6027=CARTESIAN_POINT('Origin',(-54.768323187501,-82.,335.));
#6028=CARTESIAN_POINT('',(-64.5125076436135,-90.,327.996367422169));
#6029=CARTESIAN_POINT('Origin',(60.231676812499,-82.,175.));
#6030=CARTESIAN_POINT('',(-39.60939337502,-82.,298.488745960275));
#6031=CARTESIAN_POINT('',(-42.0454394890482,-82.,296.737837815817));
#6032=CARTESIAN_POINT('',(-42.0454394890482,-82.,296.737837815817));
#6033=CARTESIAN_POINT('',(165.487492356386,-82.,7.99636742216909));
#6034=CARTESIAN_POINT('',(-22.280326233118,-82.,269.238549807567));
#6035=CARTESIAN_POINT('',(165.487492356386,-82.,7.99636742216909));
#6036=CARTESIAN_POINT('',(-19.8442801190899,-82.,270.989457952024));
#6037=CARTESIAN_POINT('',(-22.280326233118,-82.,269.238549807567));
#6038=CARTESIAN_POINT('',(167.923538470415,-82.,9.74727556662682));
#6039=CARTESIAN_POINT('Origin',(60.231676812499,-90.,175.));
#6040=CARTESIAN_POINT('',(165.487492356386,-90.,7.99636742216909));
#6041=CARTESIAN_POINT('',(-62.268323187501,-90.,335.));
#6042=CARTESIAN_POINT('Origin',(-54.768323187501,-90.,335.));
#6043=CARTESIAN_POINT('Origin',(-54.768323187501,4.78802382587669E-15,335.));
#6044=CARTESIAN_POINT('',(-62.268323187501,-118.,335.));
#6045=CARTESIAN_POINT('Origin',(-54.768323187501,-118.,335.));
#6046=CARTESIAN_POINT('',(-62.268323187501,4.78802382587669E-15,335.));
#6047=CARTESIAN_POINT('Origin',(-54.768323187501,-118.,335.));
#6048=CARTESIAN_POINT('Origin',(-54.768323187501,118.,335.));
#6049=CARTESIAN_POINT('Origin',(-39.60939337502,82.,298.488745960275));
#6050=CARTESIAN_POINT('',(-42.0454394890482,82.,296.737837815817));
#6051=CARTESIAN_POINT('',(-39.60939337502,82.,298.488745960275));
#6052=CARTESIAN_POINT('',(-35.9553242039781,82.,301.115108176961));
#6053=CARTESIAN_POINT('',(-42.0454394890482,82.,296.737837815817));
#6054=CARTESIAN_POINT('',(-39.60939337502,82.,298.488745960275));
#6055=CARTESIAN_POINT('Origin',(-19.84428011909,82.,270.989457952024));
#6056=CARTESIAN_POINT('',(-19.8442801190899,82.,270.989457952024));
#6057=CARTESIAN_POINT('',(16.5396291756623,82.,220.368366759326));
#6058=CARTESIAN_POINT('',(-19.8442801190899,82.,270.989457952024));
#6059=CARTESIAN_POINT('Origin',(-22.280326233118,82.,269.238549807567));
#6060=CARTESIAN_POINT('',(-22.280326233118,82.,269.238549807567));
#6061=CARTESIAN_POINT('',(-17.4082340050621,82.,272.740366096482));
#6062=CARTESIAN_POINT('',(-22.280326233118,82.,269.238549807567));
#6063=CARTESIAN_POINT('Origin',(175.231676812499,90.,15.));
#6064=CARTESIAN_POINT('',(167.731676812499,82.,15.));
#6065=CARTESIAN_POINT('Origin',(175.231676812499,82.,15.));
#6066=CARTESIAN_POINT('',(167.731676812499,90.,15.));
#6067=CARTESIAN_POINT('',(167.731676812499,90.,15.));
#6068=CARTESIAN_POINT('Origin',(175.231676812499,90.,15.));
#6069=CARTESIAN_POINT('Origin',(165.487492356386,90.,7.99636742216909));
#6070=CARTESIAN_POINT('',(165.487492356386,90.,7.99636742216909));
#6071=CARTESIAN_POINT('',(-64.5125076436135,90.,327.996367422169));
#6072=CARTESIAN_POINT('',(165.487492356386,90.,7.99636742216909));
#6073=CARTESIAN_POINT('',(165.487492356386,82.,7.99636742216912));
#6074=CARTESIAN_POINT('',(165.487492356386,90.,7.99636742216909));
#6075=CARTESIAN_POINT('',(165.487492356386,82.,7.99636742216909));
#6076=CARTESIAN_POINT('',(-64.5125076436135,82.,327.996367422169));
#6077=CARTESIAN_POINT('',(165.487492356386,82.,7.99636742216909));
#6078=CARTESIAN_POINT('',(-64.5125076436135,90.,327.996367422169));
#6079=CARTESIAN_POINT('Origin',(175.231676812499,90.,15.));
#6080=CARTESIAN_POINT('',(184.975861268612,90.,22.0036325778309));
#6081=CARTESIAN_POINT('Origin',(175.231676812499,90.,15.));
#6082=CARTESIAN_POINT('',(184.975861268612,82.,22.0036325778309));
#6083=CARTESIAN_POINT('',(184.975861268612,90.,22.0036325778309));
#6084=CARTESIAN_POINT('Origin',(175.231676812499,82.,15.));
#6085=CARTESIAN_POINT('Origin',(-45.0241387313884,90.,342.003632577831));
#6086=CARTESIAN_POINT('',(-45.0241387313884,90.,342.003632577831));
#6087=CARTESIAN_POINT('',(-45.0241387313884,90.,342.003632577831));
#6088=CARTESIAN_POINT('',(-45.0241387313884,82.,342.003632577831));
#6089=CARTESIAN_POINT('',(-45.0241387313884,90.,342.003632577831));
#6090=CARTESIAN_POINT('',(-45.0241387313884,82.,342.003632577831));
#6091=CARTESIAN_POINT('Origin',(-54.768323187501,90.,335.));
#6092=CARTESIAN_POINT('Origin',(-54.768323187501,90.,335.));
#6093=CARTESIAN_POINT('Origin',(-54.768323187501,82.,335.));
#6094=CARTESIAN_POINT('Origin',(60.231676812499,82.,175.));
#6095=CARTESIAN_POINT('Origin',(60.231676812499,90.,175.));
#6096=CARTESIAN_POINT('',(0.,0.,0.));
#6097=CARTESIAN_POINT('Origin',(60.231676812499,-95.,175.));
#6098=CARTESIAN_POINT('',(54.231676812499,-95.,175.));
#6099=CARTESIAN_POINT('Origin',(60.231676812499,-95.,175.));
#6100=CARTESIAN_POINT('Origin',(60.231676812499,-90.,175.));
#6101=CARTESIAN_POINT('',(54.231676812499,95.,175.));
#6102=CARTESIAN_POINT('Origin',(60.231676812499,95.,175.));
#6103=CARTESIAN_POINT('',(54.231676812499,-90.,175.));
#6104=CARTESIAN_POINT('Origin',(60.231676812499,95.,175.));
#6105=CARTESIAN_POINT('',(0.,0.,0.));
#6106=CARTESIAN_POINT('Origin',(60.231676812499,95.,175.));
#6107=CARTESIAN_POINT('',(54.231676812499,72.,175.));
#6108=CARTESIAN_POINT('Origin',(60.231676812499,72.,175.));
#6109=CARTESIAN_POINT('',(54.231676812499,80.,175.));
#6110=CARTESIAN_POINT('',(54.231676812499,95.,175.));
#6111=CARTESIAN_POINT('Origin',(60.231676812499,80.,175.));
#6112=CARTESIAN_POINT('Origin',(175.231676812499,80.,335.));
#6113=CARTESIAN_POINT('',(167.731676812499,72.,335.));
#6114=CARTESIAN_POINT('Origin',(175.231676812499,72.,335.));
#6115=CARTESIAN_POINT('',(167.731676812499,80.,335.));
#6116=CARTESIAN_POINT('',(167.731676812499,80.,335.));
#6117=CARTESIAN_POINT('Origin',(175.231676812499,80.,335.));
#6118=CARTESIAN_POINT('Origin',(-64.5125076436135,80.,22.0036325778309));
#6119=CARTESIAN_POINT('',(-64.5125076436135,80.,22.0036325778309));
#6120=CARTESIAN_POINT('',(165.487492356386,80.,342.003632577831));
#6121=CARTESIAN_POINT('',(-64.5125076436135,80.,22.0036325778309));
#6122=CARTESIAN_POINT('',(-64.5125076436135,72.,22.0036325778309));
#6123=CARTESIAN_POINT('',(-64.5125076436135,80.,22.0036325778309));
#6124=CARTESIAN_POINT('',(165.487492356386,72.,342.003632577831));
#6125=CARTESIAN_POINT('',(-64.5125076436135,72.,22.0036325778309));
#6126=CARTESIAN_POINT('',(165.487492356386,80.,342.003632577831));
#6127=CARTESIAN_POINT('Origin',(-54.7683231875009,80.,15.));
#6128=CARTESIAN_POINT('',(-45.0241387313884,80.,7.99636742216912));
#6129=CARTESIAN_POINT('Origin',(-54.7683231875009,80.,15.));
#6130=CARTESIAN_POINT('',(-45.0241387313884,72.,7.99636742216912));
#6131=CARTESIAN_POINT('',(-45.0241387313884,80.,7.99636742216912));
#6132=CARTESIAN_POINT('Origin',(-54.7683231875009,72.,15.));
#6133=CARTESIAN_POINT('Origin',(184.975861268612,80.,327.996367422169));
#6134=CARTESIAN_POINT('',(184.975861268612,80.,327.996367422169));
#6135=CARTESIAN_POINT('',(184.975861268612,80.,327.996367422169));
#6136=CARTESIAN_POINT('',(184.975861268612,72.,327.996367422169));
#6137=CARTESIAN_POINT('',(184.975861268612,80.,327.996367422169));
#6138=CARTESIAN_POINT('',(184.975861268612,72.,327.996367422169));
#6139=CARTESIAN_POINT('Origin',(175.231676812499,80.,335.));
#6140=CARTESIAN_POINT('Origin',(175.231676812499,80.,335.));
#6141=CARTESIAN_POINT('Origin',(175.231676812499,72.,335.));
#6142=CARTESIAN_POINT('Origin',(60.231676812499,72.,175.));
#6143=CARTESIAN_POINT('',(-62.2683231875009,72.,15.));
#6144=CARTESIAN_POINT('Origin',(-54.7683231875009,72.,15.));
#6145=CARTESIAN_POINT('Origin',(60.231676812499,80.,175.));
#6146=CARTESIAN_POINT('',(-62.2683231875009,80.,15.));
#6147=CARTESIAN_POINT('Origin',(-54.7683231875009,80.,15.));
#6148=CARTESIAN_POINT('Origin',(-54.7683231875009,0.,15.));
#6149=CARTESIAN_POINT('',(-62.2683231875009,118.,15.));
#6150=CARTESIAN_POINT('Origin',(-54.7683231875009,118.,15.));
#6151=CARTESIAN_POINT('',(-62.2683231875009,0.,15.));
#6152=CARTESIAN_POINT('Origin',(-54.7683231875009,-118.,15.));
#6153=CARTESIAN_POINT('',(-62.2683231875009,-118.,15.));
#6154=CARTESIAN_POINT('Origin',(-54.7683231875009,-118.,15.));
#6155=CARTESIAN_POINT('Origin',(-54.7683231875009,0.,15.));
#6156=CARTESIAN_POINT('',(-62.2683231875009,0.,15.));
#6157=CARTESIAN_POINT('Origin',(-54.7683231875009,118.,15.));
#6158=CARTESIAN_POINT('',(0.,0.,0.));
#6159=CARTESIAN_POINT('Origin',(60.231676812499,-95.,175.));
#6160=CARTESIAN_POINT('',(54.231676812499,-72.,175.));
#6161=CARTESIAN_POINT('Origin',(60.231676812499,-72.,175.));
#6162=CARTESIAN_POINT('',(54.231676812499,-80.,175.));
#6163=CARTESIAN_POINT('',(54.231676812499,-95.,175.));
#6164=CARTESIAN_POINT('Origin',(60.231676812499,-80.,175.));
#6165=CARTESIAN_POINT('Origin',(185.231676812499,0.,335.));
#6166=CARTESIAN_POINT('',(179.731676812499,2.46330733588707E-15,329.));
#6167=CARTESIAN_POINT('',(182.731676812499,-6.,335.));
#6168=CARTESIAN_POINT('Ctrl Pts',(179.731676812499,-1.38777878078145E-16,
329.));
#6169=CARTESIAN_POINT('Ctrl Pts',(179.731676812499,-0.410146780646358,329.));
#6170=CARTESIAN_POINT('Ctrl Pts',(179.789372806578,-0.816861849349989,329.042276815307));
#6171=CARTESIAN_POINT('Ctrl Pts',(179.994045571984,-1.60462674459781,329.204579222783));
#6172=CARTESIAN_POINT('Ctrl Pts',(180.139940991557,-1.98596758305952,329.324554046353));
#6173=CARTESIAN_POINT('Ctrl Pts',(180.642335947217,-3.07201535485507,329.786388864399));
#6174=CARTESIAN_POINT('Ctrl Pts',(181.058329790287,-3.7207625323499,330.235481158111));
#6175=CARTESIAN_POINT('Ctrl Pts',(181.763206112437,-4.74828751391861,331.26300613968));
#6176=CARTESIAN_POINT('Ctrl Pts',(182.110324034524,-5.20624497170395,331.912343858094));
#6177=CARTESIAN_POINT('Ctrl Pts',(182.596018078742,-5.8328999714949,333.382629157599));
#6178=CARTESIAN_POINT('Ctrl Pts',(182.731676812499,-6.00000000000001,334.205219010374));
#6179=CARTESIAN_POINT('Ctrl Pts',(182.731676812499,-6.00000000000001,335.));
#6180=CARTESIAN_POINT('Ctrl Pts',(182.731676812499,-6.,335.));
#6181=CARTESIAN_POINT('Ctrl Pts',(182.731676812499,-6.,335.794780989626));
#6182=CARTESIAN_POINT('Ctrl Pts',(182.596018078742,-5.8328999714949,336.617370842401));
#6183=CARTESIAN_POINT('Ctrl Pts',(182.110324034524,-5.20624497170395,338.087656141906));
#6184=CARTESIAN_POINT('Ctrl Pts',(181.763206112437,-4.74828751391861,338.73699386032));
#6185=CARTESIAN_POINT('Ctrl Pts',(181.058329790287,-3.7207625323499,339.764518841889));
#6186=CARTESIAN_POINT('Ctrl Pts',(180.642335947217,-3.07201535485507,340.213611135601));
#6187=CARTESIAN_POINT('Ctrl Pts',(180.139940991557,-1.98596758305952,340.675445953647));
#6188=CARTESIAN_POINT('Ctrl Pts',(179.994045571984,-1.60462674459781,340.795420777217));
#6189=CARTESIAN_POINT('Ctrl Pts',(179.789372806578,-0.816861849349989,340.957723184693));
#6190=CARTESIAN_POINT('Ctrl Pts',(179.731676812499,-0.410146780646358,341.));
#6191=CARTESIAN_POINT('Ctrl Pts',(179.731676812499,0.410146780646357,341.));
#6192=CARTESIAN_POINT('Ctrl Pts',(179.789372806578,0.816861849350014,340.957723184693));
#6193=CARTESIAN_POINT('Ctrl Pts',(179.994045571984,1.60462674459784,340.795420777217));
#6194=CARTESIAN_POINT('Ctrl Pts',(180.139940991557,1.9859675830595,340.675445953647));
#6195=CARTESIAN_POINT('Ctrl Pts',(180.642335947218,3.07201535485506,340.213611135601));
#6196=CARTESIAN_POINT('Ctrl Pts',(181.058329790287,3.7207625323499,339.764518841889));
#6197=CARTESIAN_POINT('Ctrl Pts',(181.763206112437,4.74828751391861,338.73699386032));
#6198=CARTESIAN_POINT('Ctrl Pts',(182.110324034524,5.20624497170395,338.087656141906));
#6199=CARTESIAN_POINT('Ctrl Pts',(182.596018078742,5.8328999714949,336.617370842401));
#6200=CARTESIAN_POINT('Ctrl Pts',(182.731676812499,6.,335.794780989626));
#6201=CARTESIAN_POINT('Ctrl Pts',(182.731676812499,6.,334.205219010374));
#6202=CARTESIAN_POINT('Ctrl Pts',(182.596018078742,5.8328999714949,333.382629157599));
#6203=CARTESIAN_POINT('Ctrl Pts',(182.110324034524,5.20624497170395,331.912343858094));
#6204=CARTESIAN_POINT('Ctrl Pts',(181.763206112437,4.74828751391861,331.26300613968));
#6205=CARTESIAN_POINT('Ctrl Pts',(181.058329790287,3.7207625323499,330.235481158111));
#6206=CARTESIAN_POINT('Ctrl Pts',(180.642335947218,3.07201535485506,329.786388864399));
#6207=CARTESIAN_POINT('Ctrl Pts',(180.139940991557,1.9859675830595,329.324554046353));
#6208=CARTESIAN_POINT('Ctrl Pts',(179.994045571984,1.60462674459784,329.204579222783));
#6209=CARTESIAN_POINT('Ctrl Pts',(179.789372806578,0.816861849350014,329.042276815307));
#6210=CARTESIAN_POINT('Ctrl Pts',(179.731676812499,0.410146780646354,329.));
#6211=CARTESIAN_POINT('Ctrl Pts',(179.731676812499,-2.67147415300428E-15,
329.));
#6212=CARTESIAN_POINT('',(167.731676812499,-6.,335.));
#6213=CARTESIAN_POINT('',(185.231676812499,-6.,335.));
#6214=CARTESIAN_POINT('',(167.731676812499,6.,335.));
#6215=CARTESIAN_POINT('Ctrl Pts',(167.731676812499,6.,335.));
#6216=CARTESIAN_POINT('Ctrl Pts',(167.731676812499,6.,335.794780989625));
#6217=CARTESIAN_POINT('Ctrl Pts',(167.867335546256,5.8328999714949,336.617370842401));
#6218=CARTESIAN_POINT('Ctrl Pts',(168.353029590474,5.20624497170395,338.087656141906));
#6219=CARTESIAN_POINT('Ctrl Pts',(168.700147512561,4.74828751391861,338.73699386032));
#6220=CARTESIAN_POINT('Ctrl Pts',(169.405023834711,3.7207625323499,339.764518841889));
#6221=CARTESIAN_POINT('Ctrl Pts',(169.821017677781,3.07201535485507,340.213611135601));
#6222=CARTESIAN_POINT('Ctrl Pts',(170.323412633441,1.98596758305952,340.675445953647));
#6223=CARTESIAN_POINT('Ctrl Pts',(170.469308053014,1.60462674459781,340.795420777217));
#6224=CARTESIAN_POINT('Ctrl Pts',(170.67398081842,0.81686184934999,340.957723184693));
#6225=CARTESIAN_POINT('Ctrl Pts',(170.731676812499,0.410146780646358,341.));
#6226=CARTESIAN_POINT('Ctrl Pts',(170.731676812499,-0.410146780646357,341.));
#6227=CARTESIAN_POINT('Ctrl Pts',(170.67398081842,-0.816861849349986,340.957723184693));
#6228=CARTESIAN_POINT('Ctrl Pts',(170.469308053014,-1.60462674459781,340.795420777217));
#6229=CARTESIAN_POINT('Ctrl Pts',(170.323412633441,-1.98596758305952,340.675445953647));
#6230=CARTESIAN_POINT('Ctrl Pts',(169.821017677781,-3.07201535485507,340.213611135601));
#6231=CARTESIAN_POINT('Ctrl Pts',(169.405023834711,-3.7207625323499,339.764518841889));
#6232=CARTESIAN_POINT('Ctrl Pts',(168.700147512561,-4.74828751391861,338.73699386032));
#6233=CARTESIAN_POINT('Ctrl Pts',(168.353029590474,-5.20624497170395,338.087656141906));
#6234=CARTESIAN_POINT('Ctrl Pts',(167.867335546256,-5.8328999714949,336.617370842401));
#6235=CARTESIAN_POINT('Ctrl Pts',(167.731676812499,-6.,335.794780989626));
#6236=CARTESIAN_POINT('Ctrl Pts',(167.731676812499,-6.,335.));
#6237=CARTESIAN_POINT('',(170.731676812499,5.89805981832114E-16,329.));
#6238=CARTESIAN_POINT('Ctrl Pts',(170.731676812499,1.2490009027033E-15,
329.));
#6239=CARTESIAN_POINT('Ctrl Pts',(170.731676812499,0.410146780646359,329.));
#6240=CARTESIAN_POINT('Ctrl Pts',(170.67398081842,0.816861849349989,329.042276815307));
#6241=CARTESIAN_POINT('Ctrl Pts',(170.469308053014,1.60462674459781,329.204579222783));
#6242=CARTESIAN_POINT('Ctrl Pts',(170.323412633441,1.98596758305952,329.324554046353));
#6243=CARTESIAN_POINT('Ctrl Pts',(169.821017677781,3.07201535485507,329.786388864399));
#6244=CARTESIAN_POINT('Ctrl Pts',(169.405023834711,3.7207625323499,330.235481158111));
#6245=CARTESIAN_POINT('Ctrl Pts',(168.700147512561,4.74828751391861,331.26300613968));
#6246=CARTESIAN_POINT('Ctrl Pts',(168.353029590474,5.20624497170395,331.912343858094));
#6247=CARTESIAN_POINT('Ctrl Pts',(167.867335546256,5.8328999714949,333.382629157599));
#6248=CARTESIAN_POINT('Ctrl Pts',(167.731676812499,6.,334.205219010374));
#6249=CARTESIAN_POINT('Ctrl Pts',(167.731676812499,6.,335.));
#6250=CARTESIAN_POINT('Ctrl Pts',(167.731676812499,-6.,335.));
#6251=CARTESIAN_POINT('Ctrl Pts',(167.731676812499,-6.,334.205219010374));
#6252=CARTESIAN_POINT('Ctrl Pts',(167.867335546256,-5.8328999714949,333.382629157599));
#6253=CARTESIAN_POINT('Ctrl Pts',(168.353029590474,-5.20624497170395,331.912343858094));
#6254=CARTESIAN_POINT('Ctrl Pts',(168.700147512561,-4.74828751391861,331.26300613968));
#6255=CARTESIAN_POINT('Ctrl Pts',(169.405023834711,-3.7207625323499,330.235481158111));
#6256=CARTESIAN_POINT('Ctrl Pts',(169.821017677781,-3.07201535485506,329.786388864399));
#6257=CARTESIAN_POINT('Ctrl Pts',(170.323412633441,-1.98596758305952,329.324554046353));
#6258=CARTESIAN_POINT('Ctrl Pts',(170.469308053014,-1.60462674459781,329.204579222783));
#6259=CARTESIAN_POINT('Ctrl Pts',(170.67398081842,-0.816861849349986,329.042276815307));
#6260=CARTESIAN_POINT('Ctrl Pts',(170.731676812499,-0.410146780646357,329.));
#6261=CARTESIAN_POINT('Ctrl Pts',(170.731676812499,-1.79550893470375E-16,
329.));
#6262=CARTESIAN_POINT('Origin',(-54.7683231875009,-80.,15.));
#6263=CARTESIAN_POINT('',(-62.2683231875009,-80.,15.));
#6264=CARTESIAN_POINT('Origin',(-54.7683231875009,-80.,15.));
#6265=CARTESIAN_POINT('',(-62.2683231875009,-72.,15.));
#6266=CARTESIAN_POINT('',(-62.2683231875009,-80.,15.));
#6267=CARTESIAN_POINT('Origin',(-54.7683231875009,-72.,15.));
#6268=CARTESIAN_POINT('Origin',(-64.5125076436135,-80.,22.0036325778309));
#6269=CARTESIAN_POINT('',(-64.5125076436135,-80.,22.0036325778309));
#6270=CARTESIAN_POINT('',(165.487492356386,-80.,342.003632577831));
#6271=CARTESIAN_POINT('',(-64.5125076436135,-80.,22.0036325778309));
#6272=CARTESIAN_POINT('',(165.487492356386,-72.,342.003632577831));
#6273=CARTESIAN_POINT('',(165.487492356386,-80.,342.003632577831));
#6274=CARTESIAN_POINT('',(-64.5125076436135,-72.,22.0036325778309));
#6275=CARTESIAN_POINT('',(-64.5125076436135,-72.,22.0036325778309));
#6276=CARTESIAN_POINT('',(-64.5125076436135,-80.,22.0036325778309));
#6277=CARTESIAN_POINT('Origin',(-54.7683231875009,-80.,15.));
#6278=CARTESIAN_POINT('',(-45.0241387313884,-80.,7.99636742216912));
#6279=CARTESIAN_POINT('Origin',(-54.7683231875009,-80.,15.));
#6280=CARTESIAN_POINT('',(-45.0241387313884,-72.,7.99636742216912));
#6281=CARTESIAN_POINT('Origin',(-54.7683231875009,-72.,15.));
#6282=CARTESIAN_POINT('',(-45.0241387313884,-80.,7.99636742216912));
#6283=CARTESIAN_POINT('Origin',(184.975861268612,-80.,327.996367422169));
#6284=CARTESIAN_POINT('',(184.975861268612,-80.,327.996367422169));
#6285=CARTESIAN_POINT('',(184.975861268612,-80.,327.996367422169));
#6286=CARTESIAN_POINT('',(184.975861268612,-72.,327.996367422169));
#6287=CARTESIAN_POINT('',(184.975861268612,-72.,327.996367422169));
#6288=CARTESIAN_POINT('',(184.975861268612,-80.,327.996367422169));
#6289=CARTESIAN_POINT('Origin',(175.231676812499,-80.,335.));
#6290=CARTESIAN_POINT('Origin',(175.231676812499,-80.,335.));
#6291=CARTESIAN_POINT('Origin',(175.231676812499,-72.,335.));
#6292=CARTESIAN_POINT('Origin',(60.231676812499,-72.,175.));
#6293=CARTESIAN_POINT('',(167.731676812499,-72.,335.));
#6294=CARTESIAN_POINT('Origin',(175.231676812499,-72.,335.));
#6295=CARTESIAN_POINT('Origin',(60.231676812499,-80.,175.));
#6296=CARTESIAN_POINT('',(167.731676812499,-80.,335.));
#6297=CARTESIAN_POINT('Origin',(175.231676812499,-80.,335.));
#6298=CARTESIAN_POINT('Origin',(175.231676812499,4.78802382587669E-15,335.));
#6299=CARTESIAN_POINT('',(167.731676812499,-118.,335.));
#6300=CARTESIAN_POINT('Origin',(175.231676812499,-118.,335.));
#6301=CARTESIAN_POINT('',(167.731676812499,4.78802382587669E-15,335.));
#6302=CARTESIAN_POINT('Origin',(175.231676812499,-118.,335.));
#6303=CARTESIAN_POINT('Origin',(175.231676812499,4.78802382587669E-15,335.));
#6304=CARTESIAN_POINT('',(167.731676812499,4.78802382587669E-15,335.));
#6305=CARTESIAN_POINT('',(167.731676812499,118.,335.));
#6306=CARTESIAN_POINT('',(167.731676812499,4.78802382587669E-15,335.));
#6307=CARTESIAN_POINT('Origin',(175.231676812499,118.,335.));
#6308=CARTESIAN_POINT('Origin',(175.231676812499,118.,335.));
#6309=CARTESIAN_POINT('',(0.,0.,0.));
#6310=CARTESIAN_POINT('Origin',(-54.768323187501,-118.,335.));
#6311=CARTESIAN_POINT('',(-62.268323187501,-114.3,335.));
#6312=CARTESIAN_POINT('Origin',(-54.768323187501,-114.3,335.));
#6313=CARTESIAN_POINT('',(-62.268323187501,-112.3,335.));
#6314=CARTESIAN_POINT('',(-62.268323187501,-118.,335.));
#6315=CARTESIAN_POINT('Origin',(-54.768323187501,-112.3,335.));
#6316=CARTESIAN_POINT('Origin',(-54.768323187501,-118.,335.));
#6317=CARTESIAN_POINT('',(-62.268323187501,112.3,335.));
#6318=CARTESIAN_POINT('Origin',(-54.768323187501,112.3,335.));
#6319=CARTESIAN_POINT('',(-62.268323187501,114.3,335.));
#6320=CARTESIAN_POINT('',(-62.268323187501,-118.,335.));
#6321=CARTESIAN_POINT('Origin',(-54.768323187501,114.3,335.));
#6322=CARTESIAN_POINT('Origin',(175.231676812499,-118.,335.));
#6323=CARTESIAN_POINT('',(167.731676812499,-114.3,335.));
#6324=CARTESIAN_POINT('Origin',(175.231676812499,-114.3,335.));
#6325=CARTESIAN_POINT('',(167.731676812499,-112.3,335.));
#6326=CARTESIAN_POINT('',(167.731676812499,-118.,335.));
#6327=CARTESIAN_POINT('Origin',(175.231676812499,-112.3,335.));
#6328=CARTESIAN_POINT('Origin',(175.231676812499,-118.,335.));
#6329=CARTESIAN_POINT('',(167.731676812499,112.3,335.));
#6330=CARTESIAN_POINT('Origin',(175.231676812499,112.3,335.));
#6331=CARTESIAN_POINT('',(167.731676812499,114.3,335.));
#6332=CARTESIAN_POINT('',(167.731676812499,-118.,335.));
#6333=CARTESIAN_POINT('Origin',(175.231676812499,114.3,335.));
#6334=CARTESIAN_POINT('Origin',(-3.94336269325448E-14,99.3,322.));
#6335=CARTESIAN_POINT('',(-198.,99.3,320.));
#6336=CARTESIAN_POINT('',(198.,99.3,320.));
#6337=CARTESIAN_POINT('',(-3.91886975727153E-14,99.3,320.));
#6338=CARTESIAN_POINT('',(198.,99.3,322.));
#6339=CARTESIAN_POINT('',(198.,99.3,320.));
#6340=CARTESIAN_POINT('',(-198.,99.3,322.));
#6341=CARTESIAN_POINT('',(-3.94336269325448E-14,99.3,322.));
#6342=CARTESIAN_POINT('',(-198.,99.3,320.));
#6343=CARTESIAN_POINT('Origin',(-3.94336269325448E-14,109.3,322.));
#6344=CARTESIAN_POINT('',(198.,109.3,322.));
#6345=CARTESIAN_POINT('',(198.,112.3,322.));
#6346=CARTESIAN_POINT('',(-198.,109.3,322.));
#6347=CARTESIAN_POINT('',(-3.94336269325448E-14,109.3,322.));
#6348=CARTESIAN_POINT('',(-198.,112.3,322.));
#6349=CARTESIAN_POINT('Origin',(-3.9801020972289E-14,109.3,325.));
#6350=CARTESIAN_POINT('',(198.,112.3,325.));
#6351=CARTESIAN_POINT('Origin',(198.,109.3,325.));
#6352=CARTESIAN_POINT('',(-198.,112.3,325.));
#6353=CARTESIAN_POINT('',(-3.9801020972289E-14,112.3,325.));
#6354=CARTESIAN_POINT('Origin',(-198.,109.3,325.));
#6355=CARTESIAN_POINT('Origin',(-4.22503145705837E-14,112.3,345.));
#6356=CARTESIAN_POINT('',(198.,112.3,345.));
#6357=CARTESIAN_POINT('',(198.,112.3,345.));
#6358=CARTESIAN_POINT('',(-198.,112.3,345.));
#6359=CARTESIAN_POINT('',(-4.22503145705837E-14,112.3,345.));
#6360=CARTESIAN_POINT('',(-198.,112.3,345.));
#6361=CARTESIAN_POINT('Origin',(-4.22503145705837E-14,109.3,345.));
#6362=CARTESIAN_POINT('',(198.,109.3,348.));
#6363=CARTESIAN_POINT('Origin',(198.,109.3,345.));
#6364=CARTESIAN_POINT('',(-198.,109.3,348.));
#6365=CARTESIAN_POINT('',(-4.26177086103279E-14,109.3,348.));
#6366=CARTESIAN_POINT('Origin',(-198.,109.3,345.));
#6367=CARTESIAN_POINT('Origin',(-4.24952439304132E-14,111.3,347.));
#6368=CARTESIAN_POINT('',(198.,111.3,350.));
#6369=CARTESIAN_POINT('',(-198.,111.3,350.));
#6370=CARTESIAN_POINT('',(-4.28626379701574E-14,111.3,350.));
#6371=CARTESIAN_POINT('',(198.,114.3,347.));
#6372=CARTESIAN_POINT('Origin',(198.,111.3,347.));
#6373=CARTESIAN_POINT('',(-198.,114.3,347.));
#6374=CARTESIAN_POINT('',(-4.24952439304132E-14,114.3,347.));
#6375=CARTESIAN_POINT('Origin',(-198.,111.3,347.));
#6376=CARTESIAN_POINT('Origin',(-3.95560916124595E-14,114.3,323.));
#6377=CARTESIAN_POINT('',(198.,114.3,323.));
#6378=CARTESIAN_POINT('',(198.,114.3,347.));
#6379=CARTESIAN_POINT('',(-198.,114.3,323.));
#6380=CARTESIAN_POINT('',(-3.95560916124595E-14,114.3,323.));
#6381=CARTESIAN_POINT('',(-198.,114.3,347.));
#6382=CARTESIAN_POINT('Origin',(-3.95560916124595E-14,111.3,323.));
#6383=CARTESIAN_POINT('',(198.,111.3,320.));
#6384=CARTESIAN_POINT('Origin',(198.,111.3,323.));
#6385=CARTESIAN_POINT('',(-198.,111.3,320.));
#6386=CARTESIAN_POINT('',(-3.91886975727153E-14,111.3,320.));
#6387=CARTESIAN_POINT('Origin',(-198.,111.3,323.));
#6388=CARTESIAN_POINT('Origin',(-3.91886975727153E-14,99.3,320.));
#6389=CARTESIAN_POINT('',(198.,111.3,320.));
#6390=CARTESIAN_POINT('',(-198.,111.3,320.));
#6391=CARTESIAN_POINT('Origin',(198.,-57.15,335.));
#6392=CARTESIAN_POINT('',(198.,-111.3,320.));
#6393=CARTESIAN_POINT('',(198.,-99.3,320.));
#6394=CARTESIAN_POINT('',(198.,-111.3,320.));
#6395=CARTESIAN_POINT('',(198.,-99.3,322.));
#6396=CARTESIAN_POINT('',(198.,-99.3,320.));
#6397=CARTESIAN_POINT('',(198.,-109.3,322.));
#6398=CARTESIAN_POINT('',(198.,-112.3,322.));
#6399=CARTESIAN_POINT('',(198.,-112.3,325.));
#6400=CARTESIAN_POINT('Origin',(198.,-109.3,325.));
#6401=CARTESIAN_POINT('',(198.,-112.3,345.));
#6402=CARTESIAN_POINT('',(198.,-112.3,345.));
#6403=CARTESIAN_POINT('',(198.,-109.3,348.));
#6404=CARTESIAN_POINT('Origin',(198.,-109.3,345.));
#6405=CARTESIAN_POINT('',(198.,0.,348.));
#6406=CARTESIAN_POINT('',(198.,-111.3,350.));
#6407=CARTESIAN_POINT('',(198.,0.,350.));
#6408=CARTESIAN_POINT('',(198.,-114.3,347.));
#6409=CARTESIAN_POINT('Origin',(198.,-111.3,347.));
#6410=CARTESIAN_POINT('',(198.,-114.3,323.));
#6411=CARTESIAN_POINT('',(198.,-114.3,347.));
#6412=CARTESIAN_POINT('Origin',(198.,-111.3,323.));
#6413=CARTESIAN_POINT('Origin',(-3.94336269325448E-14,-99.3,322.));
#6414=CARTESIAN_POINT('',(-198.,-99.3,320.));
#6415=CARTESIAN_POINT('',(-3.91886975727153E-14,-99.3,320.));
#6416=CARTESIAN_POINT('',(-198.,-99.3,322.));
#6417=CARTESIAN_POINT('',(-198.,-99.3,320.));
#6418=CARTESIAN_POINT('',(-3.94336269325448E-14,-99.3,322.));
#6419=CARTESIAN_POINT('Origin',(-3.94336269325448E-14,-109.3,322.));
#6420=CARTESIAN_POINT('',(-198.,-109.3,322.));
#6421=CARTESIAN_POINT('',(-198.,-112.3,322.));
#6422=CARTESIAN_POINT('',(-3.94336269325448E-14,-109.3,322.));
#6423=CARTESIAN_POINT('Origin',(-3.9801020972289E-14,-109.3,325.));
#6424=CARTESIAN_POINT('',(-198.,-112.3,325.));
#6425=CARTESIAN_POINT('Origin',(-198.,-109.3,325.));
#6426=CARTESIAN_POINT('',(-3.9801020972289E-14,-112.3,325.));
#6427=CARTESIAN_POINT('Origin',(-4.22503145705837E-14,-112.3,345.));
#6428=CARTESIAN_POINT('',(-198.,-112.3,345.));
#6429=CARTESIAN_POINT('',(-198.,-112.3,345.));
#6430=CARTESIAN_POINT('',(-4.22503145705837E-14,-112.3,345.));
#6431=CARTESIAN_POINT('Origin',(-4.22503145705837E-14,-109.3,345.));
#6432=CARTESIAN_POINT('',(-198.,-109.3,348.));
#6433=CARTESIAN_POINT('Origin',(-198.,-109.3,345.));
#6434=CARTESIAN_POINT('',(-4.26177086103279E-14,-109.3,348.));
#6435=CARTESIAN_POINT('Origin',(-4.26177086103279E-14,0.,348.));
#6436=CARTESIAN_POINT('',(-198.,0.,348.));
#6437=CARTESIAN_POINT('Origin',(-4.28626379701574E-14,-111.3,350.));
#6438=CARTESIAN_POINT('',(-198.,-111.3,350.));
#6439=CARTESIAN_POINT('',(-198.,0.,350.));
#6440=CARTESIAN_POINT('',(-4.28626379701574E-14,-111.3,350.));
#6441=CARTESIAN_POINT('Origin',(-4.24952439304132E-14,-111.3,347.));
#6442=CARTESIAN_POINT('',(-198.,-114.3,347.));
#6443=CARTESIAN_POINT('Origin',(-198.,-111.3,347.));
#6444=CARTESIAN_POINT('',(-4.24952439304132E-14,-114.3,347.));
#6445=CARTESIAN_POINT('Origin',(-3.95560916124595E-14,-114.3,323.));
#6446=CARTESIAN_POINT('',(-198.,-114.3,323.));
#6447=CARTESIAN_POINT('',(-198.,-114.3,347.));
#6448=CARTESIAN_POINT('',(-3.95560916124595E-14,-114.3,323.));
#6449=CARTESIAN_POINT('Origin',(-3.95560916124595E-14,-111.3,323.));
#6450=CARTESIAN_POINT('',(-198.,-111.3,320.));
#6451=CARTESIAN_POINT('Origin',(-198.,-111.3,323.));
#6452=CARTESIAN_POINT('',(-3.91886975727153E-14,-111.3,320.));
#6453=CARTESIAN_POINT('Origin',(-3.91886975727153E-14,-99.3,320.));
#6454=CARTESIAN_POINT('',(-198.,-111.3,320.));
#6455=CARTESIAN_POINT('Origin',(-198.,-57.15,335.));
#6456=CARTESIAN_POINT('',(0.,0.,0.));
#6457=CARTESIAN_POINT('Origin',(189.09641784506,0.,335.));
#6458=CARTESIAN_POINT('',(182.497067674234,3.72297189708675,339.84884582308));
#6459=CARTESIAN_POINT('',(182.351531742639,3.7230579181248,339.848957366357));
#6460=CARTESIAN_POINT('',(189.09641784506,3.72297207951854,339.848845683008));
#6461=CARTESIAN_POINT('',(182.22440740295,5.47906074734768,337.711405334762));
#6462=CARTESIAN_POINT('Ctrl Pts',(182.351531742639,3.72305791812513,339.848957366357));
#6463=CARTESIAN_POINT('Ctrl Pts',(182.309156962742,4.46015191372697,339.282216531334));
#6464=CARTESIAN_POINT('Ctrl Pts',(182.266782182846,5.0665419705826,338.545000890668));
#6465=CARTESIAN_POINT('Ctrl Pts',(182.22440740295,5.47906074734771,337.711405334762));
#6466=CARTESIAN_POINT('',(182.352165757496,5.64138616135816,337.35555453857));
#6467=CARTESIAN_POINT('Ctrl Pts',(182.352160408299,5.64119776293606,337.355570708331));
#6468=CARTESIAN_POINT('Ctrl Pts',(182.347280418627,5.63503809829326,337.370322074647));
#6469=CARTESIAN_POINT('Ctrl Pts',(182.342360083051,5.62882375230088,337.385041670668));
#6470=CARTESIAN_POINT('Ctrl Pts',(182.301724441946,5.57746887366511,337.505365888699));
#6471=CARTESIAN_POINT('Ctrl Pts',(182.263984346319,5.52957139421465,337.609336160882));
#6472=CARTESIAN_POINT('Ctrl Pts',(182.22440740295,5.47906074734761,337.711405334762));
#6473=CARTESIAN_POINT('Ctrl Pts',(182.352270629205,5.64116224684411,337.355655761626));
#6474=CARTESIAN_POINT('Ctrl Pts',(182.367004937392,5.5152148489162,337.65726591955));
#6475=CARTESIAN_POINT('Ctrl Pts',(182.38167825968,5.36528272706277,337.94828699133));
#6476=CARTESIAN_POINT('Ctrl Pts',(182.411323504127,5.02168948100245,338.501373249097));
#6477=CARTESIAN_POINT('Ctrl Pts',(182.426246036053,4.82892822965015,338.762768314849));
#6478=CARTESIAN_POINT('Ctrl Pts',(182.460098215889,4.3471640672988,339.317707503377));
#6479=CARTESIAN_POINT('Ctrl Pts',(182.47861721716,4.04778944020427,339.599449032827));
#6480=CARTESIAN_POINT('Ctrl Pts',(182.497067674234,3.72297189708706,339.84884582308));
#6481=CARTESIAN_POINT('Origin',(189.09641784506,0.,335.));
#6482=CARTESIAN_POINT('',(184.246855413009,3.72297205899879,339.848845698763));
#6483=CARTESIAN_POINT('',(184.10166737808,3.72297207951882,339.848845683008));
#6484=CARTESIAN_POINT('',(189.09641784506,3.72297207951854,339.848845683008));
#6485=CARTESIAN_POINT('',(184.866944866212,-6.11325015325735,335.00025044505));
#6486=CARTESIAN_POINT('Ctrl Pts',(184.246855413009,3.72297205899967,339.848845698763));
#6487=CARTESIAN_POINT('Ctrl Pts',(184.268934436031,3.33920697021122,340.143502776249));
#6488=CARTESIAN_POINT('Ctrl Pts',(184.291464041663,2.92094987252177,340.392223513158));
#6489=CARTESIAN_POINT('Ctrl Pts',(184.340221220368,1.93946808592249,340.827132353816));
#6490=CARTESIAN_POINT('Ctrl Pts',(184.366324208566,1.37080299567188,340.986478115408));
#6491=CARTESIAN_POINT('Ctrl Pts',(184.411226219626,0.40085064572472,341.112585291422));
#6492=CARTESIAN_POINT('Ctrl Pts',(184.429328483896,0.0095859947715813,341.125708129067));
#6493=CARTESIAN_POINT('Ctrl Pts',(184.476014395384,-1.0175552976218,341.061694134485));
#6494=CARTESIAN_POINT('Ctrl Pts',(184.504435437676,-1.64471261302678,340.922371502746));
#6495=CARTESIAN_POINT('Ctrl Pts',(184.551841454068,-2.60324007796866,340.545113175205));
#6496=CARTESIAN_POINT('Ctrl Pts',(184.569886367204,-2.95298225246032,340.367034005226));
#6497=CARTESIAN_POINT('Ctrl Pts',(184.605223128158,-3.61305626692964,339.94676455908));
#6498=CARTESIAN_POINT('Ctrl Pts',(184.622723901052,-3.92191967308958,339.705656125618));
#6499=CARTESIAN_POINT('Ctrl Pts',(184.658511598607,-4.49155593275061,339.165687607535));
#6500=CARTESIAN_POINT('Ctrl Pts',(184.676723696593,-4.75060287248685,338.867659608251));
#6501=CARTESIAN_POINT('Ctrl Pts',(184.723589464835,-5.34323436716115,338.035695073479));
#6502=CARTESIAN_POINT('Ctrl Pts',(184.751252957232,-5.62644634462081,337.471579081712));
#6503=CARTESIAN_POINT('Ctrl Pts',(184.794456244581,-5.91605090024649,336.572482643603));
#6504=CARTESIAN_POINT('Ctrl Pts',(184.809100767287,-5.98963528962925,336.263576346589));
#6505=CARTESIAN_POINT('Ctrl Pts',(184.83828269457,-6.08838679889893,335.636077797764));
#6506=CARTESIAN_POINT('Ctrl Pts',(184.852615078266,-6.11323696023334,335.318411729172));
#6507=CARTESIAN_POINT('Ctrl Pts',(184.866945140388,-6.11324999486967,335.000250451567));
#6508=CARTESIAN_POINT('',(185.231676812499,-1.57888188187692,329.094159029776));
#6509=CARTESIAN_POINT('Ctrl Pts',(185.231676812499,-1.57888188187676,329.094159029776));
#6510=CARTESIAN_POINT('Ctrl Pts',(185.187737705833,-2.51057908317658,329.343241224495));
#6511=CARTESIAN_POINT('Ctrl Pts',(185.099859492502,-4.2531939892229,330.290287295343));
#6512=CARTESIAN_POINT('Ctrl Pts',(184.978279148315,-5.80226434466389,332.555945898845));
#6513=CARTESIAN_POINT('Ctrl Pts',(184.900637910794,-6.11262810662625,334.260548714089));
#6514=CARTESIAN_POINT('Ctrl Pts',(184.866935779939,-6.11326624072883,335.000250028895));
#6515=CARTESIAN_POINT('',(185.231464663099,1.57895204657858,329.094077731008));
#6516=CARTESIAN_POINT('Origin',(185.231676812499,0.,335.));
#6517=CARTESIAN_POINT('Ctrl Pts',(185.231408519459,1.57891980348589,329.094169167961));
#6518=CARTESIAN_POINT('Ctrl Pts',(185.210757145151,1.13681385221908,328.975972446527));
#6519=CARTESIAN_POINT('Ctrl Pts',(185.190336444102,0.68283589441395,328.907792814077));
#6520=CARTESIAN_POINT('Ctrl Pts',(185.149007405165,-0.22033833777906,328.874452483892));
#6521=CARTESIAN_POINT('Ctrl Pts',(185.128252990665,-0.666646880717682,328.906851779263));
#6522=CARTESIAN_POINT('Ctrl Pts',(185.094374985324,-1.39805812041619,329.041327412546));
#6523=CARTESIAN_POINT('Ctrl Pts',(185.081079478582,-1.68636324840246,329.116418570456));
#6524=CARTESIAN_POINT('Ctrl Pts',(185.032407357034,-2.70956750800716,329.464344394618));
#6525=CARTESIAN_POINT('Ctrl Pts',(184.996011299734,-3.39575068278064,329.856645196845));
#6526=CARTESIAN_POINT('Ctrl Pts',(184.942820817711,-4.28726067841481,330.624393229993));
#6527=CARTESIAN_POINT('Ctrl Pts',(184.925290369686,-4.55984109234911,330.909231098686));
#6528=CARTESIAN_POINT('Ctrl Pts',(184.883954763866,-5.12252800957322,331.623899404652));
#6529=CARTESIAN_POINT('Ctrl Pts',(184.859969757072,-5.38921493978292,332.068330999931));
#6530=CARTESIAN_POINT('Ctrl Pts',(184.818554092538,-5.75387511572488,332.89831036936));
#6531=CARTESIAN_POINT('Ctrl Pts',(184.801200855331,-5.87629802858345,333.269882635371));
#6532=CARTESIAN_POINT('Ctrl Pts',(184.756766777966,-6.09343376380386,334.229308936403));
#6533=CARTESIAN_POINT('Ctrl Pts',(184.729309773233,-6.13945282222875,334.824024973921));
#6534=CARTESIAN_POINT('Ctrl Pts',(184.684270483466,-6.07253416191094,335.805219443325));
#6535=CARTESIAN_POINT('Ctrl Pts',(184.666907708606,-6.0087844673568,336.191034156922));
#6536=CARTESIAN_POINT('Ctrl Pts',(184.621708365516,-5.75182080730419,337.159263264515));
#6537=CARTESIAN_POINT('Ctrl Pts',(184.593444189998,-5.50711706799555,337.723502312827));
#6538=CARTESIAN_POINT('Ctrl Pts',(184.547548627562,-4.97589630068615,338.572745620514));
#6539=CARTESIAN_POINT('Ctrl Pts',(184.53018003246,-4.73779610431471,338.882955921816));
#6540=CARTESIAN_POINT('Ctrl Pts',(184.476580942928,-3.92765088339003,339.752067851529));
#6541=CARTESIAN_POINT('Ctrl Pts',(184.439464154545,-3.27449478949327,340.22362693388));
#6542=CARTESIAN_POINT('Ctrl Pts',(184.385690918484,-2.1896798842563,340.721328010574));
#6543=CARTESIAN_POINT('Ctrl Pts',(184.367997331634,-1.8149967898242,340.850989257694));
#6544=CARTESIAN_POINT('Ctrl Pts',(184.332218877124,-1.05262541283211,341.034467978713));
#6545=CARTESIAN_POINT('Ctrl Pts',(184.314227942815,-0.667020259991067,341.089162340613));
#6546=CARTESIAN_POINT('Ctrl Pts',(184.278398981821,0.111536129765465,341.124712743585));
#6547=CARTESIAN_POINT('Ctrl Pts',(184.260932970875,0.502727641306943,341.105064727192));
#6548=CARTESIAN_POINT('Ctrl Pts',(184.214136410801,1.53067764544669,340.953907940929));
#6549=CARTESIAN_POINT('Ctrl Pts',(184.1842683051,2.15291708630206,340.758200620928));
#6550=CARTESIAN_POINT('Ctrl Pts',(184.136654629982,3.0817633410511,340.2940369392));
#6551=CARTESIAN_POINT('Ctrl Pts',(184.119272559744,3.41331187873858,340.086589962314));
#6552=CARTESIAN_POINT('Ctrl Pts',(184.101672843366,3.72287595009632,339.848919490427));
#6553=CARTESIAN_POINT('Ctrl Pts',(184.101670110764,3.72292401514821,339.848882587113));
#6554=CARTESIAN_POINT('Ctrl Pts',(184.101667378079,3.72297207952784,339.848845683001));
#6555=CARTESIAN_POINT('Origin',(185.231676812499,0.,335.));
#6556=CARTESIAN_POINT('',(184.058316793539,-4.81229327647336,336.796673031942));
#6557=CARTESIAN_POINT('',(183.581261447482,-4.81229344167014,336.796672589472));
#6558=CARTESIAN_POINT('',(185.231676812499,-4.81229334914346,336.796672837299));
#6559=CARTESIAN_POINT('',(185.231676812499,3.87994761181556,338.366334370211));
#6560=CARTESIAN_POINT('Ctrl Pts',(185.231676812499,3.87994761181582,338.366334370211));
#6561=CARTESIAN_POINT('Ctrl Pts',(185.20996580513,4.14235680482802,338.063888501864));
#6562=CARTESIAN_POINT('Ctrl Pts',(185.188753847695,4.36850674913513,337.731793007431));
#6563=CARTESIAN_POINT('Ctrl Pts',(185.145841871396,4.73497299547714,337.029670755389));
#6564=CARTESIAN_POINT('Ctrl Pts',(185.124297691399,4.87586902127356,336.662954808833));
#6565=CARTESIAN_POINT('Ctrl Pts',(185.088641172671,5.03911669330309,336.030508488665));
#6566=CARTESIAN_POINT('Ctrl Pts',(185.074632630748,5.08505461986033,335.772571767282));
#6567=CARTESIAN_POINT('Ctrl Pts',(185.024001495001,5.17911272059516,334.834079504077));
#6568=CARTESIAN_POINT('Ctrl Pts',(184.986563269637,5.1114288291029,334.149117473459));
#6569=CARTESIAN_POINT('Ctrl Pts',(184.931866564113,4.81520318126492,333.180754559098));
#6570=CARTESIAN_POINT('Ctrl Pts',(184.91425665323,4.6879575595803,332.874231121232));
#6571=CARTESIAN_POINT('Ctrl Pts',(184.878406205672,4.37574190234418,332.289018376107));
#6572=CARTESIAN_POINT('Ctrl Pts',(184.860242387235,4.19133006282589,332.011810013501));
#6573=CARTESIAN_POINT('Ctrl Pts',(184.823844294599,3.77165501678537,331.49699049157));
#6574=CARTESIAN_POINT('Ctrl Pts',(184.805957392279,3.53738598463557,331.260565721072));
#6575=CARTESIAN_POINT('Ctrl Pts',(184.75156741732,2.75745710874045,330.612808226125));
#6576=CARTESIAN_POINT('Ctrl Pts',(184.714210704466,2.15146534302681,330.285960234983));
#6577=CARTESIAN_POINT('Ctrl Pts',(184.659475360251,1.18310823591439,329.990426889));
#6578=CARTESIAN_POINT('Ctrl Pts',(184.641904078175,0.85821770171409,329.924663998108));
#6579=CARTESIAN_POINT('Ctrl Pts',(184.606089385025,0.198282503839793,329.856304065841));
#6580=CARTESIAN_POINT('Ctrl Pts',(184.587920312546,-0.13523862490782,329.854261738142));
#6581=CARTESIAN_POINT('Ctrl Pts',(184.533279894219,-1.12812501165542,329.944824830453));
#6582=CARTESIAN_POINT('Ctrl Pts',(184.498451887637,-1.7717130728769,330.132915585397));
#6583=CARTESIAN_POINT('Ctrl Pts',(184.443749858932,-2.66284907206899,330.594266702118));
#6584=CARTESIAN_POINT('Ctrl Pts',(184.425051832764,-2.94787866512476,330.779660956538));
#6585=CARTESIAN_POINT('Ctrl Pts',(184.388767227444,-3.47015821111336,331.198264076558));
#6586=CARTESIAN_POINT('Ctrl Pts',(184.371238350057,-3.70726722602787,331.429093672636));
#6587=CARTESIAN_POINT('Ctrl Pts',(184.335462940532,-4.13614372007297,331.935718384815));
#6588=CARTESIAN_POINT('Ctrl Pts',(184.317287363418,-4.32637787769082,332.210744097465));
#6589=CARTESIAN_POINT('Ctrl Pts',(184.262735370472,-4.8103228805498,333.080422073587));
#6590=CARTESIAN_POINT('Ctrl Pts',(184.22796605832,-5.01733792261535,333.715348928986));
#6591=CARTESIAN_POINT('Ctrl Pts',(184.174569905377,-5.13728177955315,334.689163986469));
#6592=CARTESIAN_POINT('Ctrl Pts',(184.1569893391,-5.14666817789588,335.009218592103));
#6593=CARTESIAN_POINT('Ctrl Pts',(184.121609678241,-5.10520666186254,335.657091153077));
#6594=CARTESIAN_POINT('Ctrl Pts',(184.104081307411,-5.05252221416993,335.983324333829));
#6595=CARTESIAN_POINT('Ctrl Pts',(184.077035990567,-4.92499983736479,336.469901749377));
#6596=CARTESIAN_POINT('Ctrl Pts',(184.067700098037,-4.8726894053407,336.634905209024));
#6597=CARTESIAN_POINT('Ctrl Pts',(184.058316793539,-4.81229327647345,336.796673031942));
#6598=CARTESIAN_POINT('',(185.231660786429,-3.87998480257461,338.366291504652));
#6599=CARTESIAN_POINT('Origin',(185.231676812499,0.,335.));
#6600=CARTESIAN_POINT('Ctrl Pts',(185.231660786429,-3.87998480257461,338.366291504652));
#6601=CARTESIAN_POINT('Ctrl Pts',(185.198841754409,-3.48679804038719,338.819478241377));
#6602=CARTESIAN_POINT('Ctrl Pts',(185.16716547498,-3.01724325598196,339.200286613357));
#6603=CARTESIAN_POINT('Ctrl Pts',(185.12378319743,-2.31888914664931,339.587858377999));
#6604=CARTESIAN_POINT('Ctrl Pts',(185.112888660786,-2.13968347867559,339.674125022322));
#6605=CARTESIAN_POINT('Ctrl Pts',(185.065810758349,-1.34414494710687,340.001722621249));
#6606=CARTESIAN_POINT('Ctrl Pts',(185.031025840614,-0.689409600570319,340.133095870716));
#6607=CARTESIAN_POINT('Ctrl Pts',(184.985849981913,0.138732706103458,340.137575612723));
#6608=CARTESIAN_POINT('Ctrl Pts',(184.976722348467,0.305196459457193,340.130378620157));
#6609=CARTESIAN_POINT('Ctrl Pts',(184.93117040401,1.13444531613264,340.054018755214));
#6610=CARTESIAN_POINT('Ctrl Pts',(184.896179138579,1.77969160026001,339.864439680823));
#6611=CARTESIAN_POINT('Ctrl Pts',(184.841625647083,2.6657547103338,339.403470072734));
#6612=CARTESIAN_POINT('Ctrl Pts',(184.823400079311,2.9451848259215,339.221693010019));
#6613=CARTESIAN_POINT('Ctrl Pts',(184.787552880288,3.46219644347254,338.808891037211));
#6614=CARTESIAN_POINT('Ctrl Pts',(184.770004716252,3.69899443635314,338.579370792128));
#6615=CARTESIAN_POINT('Ctrl Pts',(184.734481342641,4.12615259863405,338.07734591993));
#6616=CARTESIAN_POINT('Ctrl Pts',(184.716368530761,4.31535007448866,337.805874728676));
#6617=CARTESIAN_POINT('Ctrl Pts',(184.669070759649,4.73972687988867,337.0513458403));
#6618=CARTESIAN_POINT('Ctrl Pts',(184.64070517982,4.92765582124248,336.546358950252));
#6619=CARTESIAN_POINT('Ctrl Pts',(184.593828157937,5.09981772532086,335.697912186798));
#6620=CARTESIAN_POINT('Ctrl Pts',(184.575660754802,5.1341253925422,335.368748612603));
#6621=CARTESIAN_POINT('Ctrl Pts',(184.539500817174,5.13910858994622,334.705249812477));
#6622=CARTESIAN_POINT('Ctrl Pts',(184.521602036035,5.10916052483512,334.372464308965));
#6623=CARTESIAN_POINT('Ctrl Pts',(184.467945480004,4.92340967754059,333.390844320072));
#6624=CARTESIAN_POINT('Ctrl Pts',(184.431436715369,4.67366577046203,332.767022387495));
#6625=CARTESIAN_POINT('Ctrl Pts',(184.377255848456,4.12740600091846,331.923326514062));
#6626=CARTESIAN_POINT('Ctrl Pts',(184.359207055715,3.91516063337641,331.657409171325));
#6627=CARTESIAN_POINT('Ctrl Pts',(184.331665015962,3.56184547559044,331.294967774504));
#6628=CARTESIAN_POINT('Ctrl Pts',(184.322529305878,3.43970202932531,331.181301770471));
#6629=CARTESIAN_POINT('Ctrl Pts',(184.27753117341,2.81129293142445,330.651161764138));
#6630=CARTESIAN_POINT('Ctrl Pts',(184.243018370146,2.23405572599016,330.328302552668));
#6631=CARTESIAN_POINT('Ctrl Pts',(184.198246245456,1.45348912444086,330.070360091181));
#6632=CARTESIAN_POINT('Ctrl Pts',(184.189113003422,1.29278305477879,330.025797386536));
#6633=CARTESIAN_POINT('Ctrl Pts',(184.143877899258,0.486418116876675,329.843922724558));
#6634=CARTESIAN_POINT('Ctrl Pts',(184.109167450003,-0.179347486611541,329.824135504527));
#6635=CARTESIAN_POINT('Ctrl Pts',(184.064102325035,-0.994987552158871,329.957783832522));
#6636=CARTESIAN_POINT('Ctrl Pts',(184.054973186473,-1.15795156059106,329.992696142295));
#6637=CARTESIAN_POINT('Ctrl Pts',(184.009497659063,-1.96135003293104,330.206135307985));
#6638=CARTESIAN_POINT('Ctrl Pts',(183.974577203188,-2.56457202387815,330.49988808083));
#6639=CARTESIAN_POINT('Ctrl Pts',(183.920143775137,-3.36032431538043,331.100655938906));
#6640=CARTESIAN_POINT('Ctrl Pts',(183.901920970343,-3.60552434750443,331.326191891106));
#6641=CARTESIAN_POINT('Ctrl Pts',(183.866047047229,-4.04693461136795,331.819270717901));
#6642=CARTESIAN_POINT('Ctrl Pts',(183.848470886864,-4.24253554603068,332.08527680355));
#6643=CARTESIAN_POINT('Ctrl Pts',(183.812937838096,-4.58051914075442,332.651785905477));
#6644=CARTESIAN_POINT('Ctrl Pts',(183.794832750312,-4.72197314197139,332.951044125878));
#6645=CARTESIAN_POINT('Ctrl Pts',(183.740138191902,-5.06063518098444,333.892815761633));
#6646=CARTESIAN_POINT('Ctrl Pts',(183.704937726923,-5.16180369180752,334.562203161041));
#6647=CARTESIAN_POINT('Ctrl Pts',(183.65014115901,-5.11653344930504,335.563074239064));
#6648=CARTESIAN_POINT('Ctrl Pts',(183.632024523124,-5.06957717985736,335.891832003873));
#6649=CARTESIAN_POINT('Ctrl Pts',(183.603097831844,-4.94319086685525,336.411558018397));
#6650=CARTESIAN_POINT('Ctrl Pts',(183.592181128069,-4.88340826534985,336.606195258429));
#6651=CARTESIAN_POINT('Ctrl Pts',(183.581261447482,-4.81229344167016,336.796672589472));
#6652=CARTESIAN_POINT('Origin',(185.231676812499,0.,335.));
#6653=CARTESIAN_POINT('',(182.104574390455,-4.16808369392632,331.997787668581));
#6654=CARTESIAN_POINT('Ctrl Pts',(183.581261447482,-4.81229344167014,336.796672589472));
#6655=CARTESIAN_POINT('Ctrl Pts',(183.574404858247,-4.76763965069489,336.916275430142));
#6656=CARTESIAN_POINT('Ctrl Pts',(183.567545028061,-4.71851788329508,337.03423801728));
#6657=CARTESIAN_POINT('Ctrl Pts',(183.525857405484,-4.39553174791915,337.734944741595));
#6658=CARTESIAN_POINT('Ctrl Pts',(183.490590408521,-4.01852059594133,338.263762155306));
#6659=CARTESIAN_POINT('Ctrl Pts',(183.447056524281,-3.43330383098911,338.824448809187));
#6660=CARTESIAN_POINT('Ctrl Pts',(183.438122189421,-3.30740520662722,338.93383446743));
#6661=CARTESIAN_POINT('Ctrl Pts',(183.393766963293,-2.66213201654426,339.441563714041));
#6662=CARTESIAN_POINT('Ctrl Pts',(183.35793605831,-2.07521296953646,339.744254881504));
#6663=CARTESIAN_POINT('Ctrl Pts',(183.313831604382,-1.28730799481885,339.975625212872));
#6664=CARTESIAN_POINT('Ctrl Pts',(183.304891260124,-1.12511665638188,340.014790067098));
#6665=CARTESIAN_POINT('Ctrl Pts',(183.277525250885,-0.627891302656741,340.109516229218));
#6666=CARTESIAN_POINT('Ctrl Pts',(183.258850647331,-0.289003227088744,340.139832050651));
#6667=CARTESIAN_POINT('Ctrl Pts',(183.204067553403,0.715942364873389,340.129974231577));
#6668=CARTESIAN_POINT('Ctrl Pts',(183.169051486757,1.37392207659993,339.994149660602));
#6669=CARTESIAN_POINT('Ctrl Pts',(183.095925320236,2.60572135352441,339.477242136658));
#6670=CARTESIAN_POINT('Ctrl Pts',(183.060540187497,3.16708981082988,339.099392149873));
#6671=CARTESIAN_POINT('Ctrl Pts',(182.993542234995,4.03667924256993,338.226056893305));
#6672=CARTESIAN_POINT('Ctrl Pts',(182.962816006145,4.36528727345767,337.765237843109));
#6673=CARTESIAN_POINT('Ctrl Pts',(182.914826762285,4.75825638268382,336.963323415389));
#6674=CARTESIAN_POINT('Ctrl Pts',(182.897101413311,4.8747897302867,336.652894821662));
#6675=CARTESIAN_POINT('Ctrl Pts',(182.860929234834,5.04653726178304,336.013952186779));
#6676=CARTESIAN_POINT('Ctrl Pts',(182.842826325575,5.10135136518025,335.686921483203));
#6677=CARTESIAN_POINT('Ctrl Pts',(182.806976985386,5.14737805903147,335.026063851458));
#6678=CARTESIAN_POINT('Ctrl Pts',(182.78931135407,5.13832742675459,334.693782453588));
#6679=CARTESIAN_POINT('Ctrl Pts',(182.735918922984,5.01599852377635,333.71227950727));
#6680=CARTESIAN_POINT('Ctrl Pts',(182.69989861597,4.81017518725431,333.081484549774));
#6681=CARTESIAN_POINT('Ctrl Pts',(182.655625882176,4.41011242773355,332.360889697057));
#6682=CARTESIAN_POINT('Ctrl Pts',(182.646688201559,4.32214210106214,332.219158160999));
#6683=CARTESIAN_POINT('Ctrl Pts',(182.603520128176,3.86839407895673,331.561802727404));
#6684=CARTESIAN_POINT('Ctrl Pts',(182.56886565616,3.41640076617818,331.112338958661));
#6685=CARTESIAN_POINT('Ctrl Pts',(182.5259497374,2.75657752653948,330.662346682603));
#6686=CARTESIAN_POINT('Ctrl Pts',(182.51702011832,2.6144554422385,330.575231327291));
#6687=CARTESIAN_POINT('Ctrl Pts',(182.472496265327,1.89114024363531,330.178901099645));
#6688=CARTESIAN_POINT('Ctrl Pts',(182.436429323386,1.25847279790753,329.976488090054));
#6689=CARTESIAN_POINT('Ctrl Pts',(182.392100773262,0.439292854233025,329.879353750766));
#6690=CARTESIAN_POINT('Ctrl Pts',(182.383159214547,0.272876512558731,329.867794481007));
#6691=CARTESIAN_POINT('Ctrl Pts',(182.339954928001,-0.526060850280547,329.851274015462));
#6692=CARTESIAN_POINT('Ctrl Pts',(182.305258652713,-1.15534826314823,329.955070004742));
#6693=CARTESIAN_POINT('Ctrl Pts',(182.257553533066,-1.98967609420732,330.257383379467));
#6694=CARTESIAN_POINT('Ctrl Pts',(182.243900241156,-2.22261065129362,330.361980708259));
#6695=CARTESIAN_POINT('Ctrl Pts',(182.209193930791,-2.78260135923999,330.665351934514));
#6696=CARTESIAN_POINT('Ctrl Pts',(182.188206356022,-3.09706803350275,330.884149441227));
#6697=CARTESIAN_POINT('Ctrl Pts',(182.146387628146,-3.67745595577699,331.392464891957));
#6698=CARTESIAN_POINT('Ctrl Pts',(182.125698569782,-3.94038367340356,331.681663211721));
#6699=CARTESIAN_POINT('Ctrl Pts',(182.104574390455,-4.16808369392644,331.997787668581));
#6700=CARTESIAN_POINT('',(182.508202138845,-4.80479214222282,333.183309963564));
#6701=CARTESIAN_POINT('Ctrl Pts',(182.508329008463,-4.80477551437407,333.183318184444));
#6702=CARTESIAN_POINT('Ctrl Pts',(182.493038547972,-4.78161868580243,333.122072807318));
#6703=CARTESIAN_POINT('Ctrl Pts',(182.47705683224,-4.75732077296609,333.061350830662));
#6704=CARTESIAN_POINT('Ctrl Pts',(182.361001743482,-4.58002834629899,332.641628114898));
#6705=CARTESIAN_POINT('Ctrl Pts',(182.237933532832,-4.38798420311668,332.303083772074));
#6706=CARTESIAN_POINT('Ctrl Pts',(182.104574390455,-4.16808369392643,331.997787668581));
#6707=CARTESIAN_POINT('Ctrl Pts',(184.058316793539,-4.81229327647343,336.796673031942));
#6708=CARTESIAN_POINT('Ctrl Pts',(184.031402794846,-4.63905991995926,337.260669375179));
#6709=CARTESIAN_POINT('Ctrl Pts',(184.004066240865,-4.39930198500671,337.698042940383));
#6710=CARTESIAN_POINT('Ctrl Pts',(183.959477777831,-3.89923347510022,338.360509443272));
#6711=CARTESIAN_POINT('Ctrl Pts',(183.941711744794,-3.67329168398738,338.606101798829));
#6712=CARTESIAN_POINT('Ctrl Pts',(183.90579520563,-3.18019378259923,339.04729984871));
#6713=CARTESIAN_POINT('Ctrl Pts',(183.887734091215,-2.91473116938132,339.242476026157));
#6714=CARTESIAN_POINT('Ctrl Pts',(183.833511158755,-2.06243404651175,339.751128071117));
#6715=CARTESIAN_POINT('Ctrl Pts',(183.798761180772,-1.43184871781604,339.977615845926));
#6716=CARTESIAN_POINT('Ctrl Pts',(183.744366530398,-0.449350383568896,340.127693201517));
#6717=CARTESIAN_POINT('Ctrl Pts',(183.726244974851,-0.118996400989805,340.145970270493));
#6718=CARTESIAN_POINT('Ctrl Pts',(183.690771909644,0.539390933238602,340.118924872461));
#6719=CARTESIAN_POINT('Ctrl Pts',(183.673263779812,0.865894535513429,340.073909855269));
#6720=CARTESIAN_POINT('Ctrl Pts',(183.637441117833,1.5097350692145,339.921149051693));
#6721=CARTESIAN_POINT('Ctrl Pts',(183.619198339197,1.8253794029355,339.813001922891));
#6722=CARTESIAN_POINT('Ctrl Pts',(183.564292305223,2.738274016909,339.397408168506));
#6723=CARTESIAN_POINT('Ctrl Pts',(183.529231270503,3.28801853298999,339.00303388018));
#6724=CARTESIAN_POINT('Ctrl Pts',(183.474576098567,3.97208456320005,338.2737527464));
#6725=CARTESIAN_POINT('Ctrl Pts',(183.456424617832,4.17398380994281,338.012106368056));
#6726=CARTESIAN_POINT('Ctrl Pts',(183.421100160243,4.52222629171864,337.457880496178));
#6727=CARTESIAN_POINT('Ctrl Pts',(183.403828819226,4.6685639219126,337.167076686023));
#6728=CARTESIAN_POINT('Ctrl Pts',(183.350579746682,5.02636832228254,336.248490411596));
#6729=CARTESIAN_POINT('Ctrl Pts',(183.314295360742,5.14515622988651,335.592019100404));
#6730=CARTESIAN_POINT('Ctrl Pts',(183.242884447268,5.12729226920193,334.260694268346));
#6731=CARTESIAN_POINT('Ctrl Pts',(183.206240992382,4.98712623354329,333.598502470096));
#6732=CARTESIAN_POINT('Ctrl Pts',(183.15153263591,4.59048297762633,332.670029592873));
#6733=CARTESIAN_POINT('Ctrl Pts',(183.133525660923,4.42662346468804,332.372014283161));
#6734=CARTESIAN_POINT('Ctrl Pts',(183.079457857919,3.85923300195422,331.545696032195));
#6735=CARTESIAN_POINT('Ctrl Pts',(183.042995844251,3.38156985082007,331.076877369247));
#6736=CARTESIAN_POINT('Ctrl Pts',(182.989556769326,2.54990709080552,330.528406180653));
#6737=CARTESIAN_POINT('Ctrl Pts',(182.971703859499,2.25463090722395,330.372494268806));
#6738=CARTESIAN_POINT('Ctrl Pts',(182.935557501039,1.64052021887021,330.121054922684));
#6739=CARTESIAN_POINT('Ctrl Pts',(182.917353750986,1.32332475086542,330.025643806206));
#6740=CARTESIAN_POINT('Ctrl Pts',(182.862335274629,0.330533052436667,329.828771292242));
#6741=CARTESIAN_POINT('Ctrl Pts',(182.826457095763,-0.357862786546009,329.830589265057));
#6742=CARTESIAN_POINT('Ctrl Pts',(182.752296089695,-1.68354853246715,330.100768808326));
#6743=CARTESIAN_POINT('Ctrl Pts',(182.717021322299,-2.30869609605098,330.362463116437));
#6744=CARTESIAN_POINT('Ctrl Pts',(182.652106720335,-3.29831072274798,331.02772756185));
#6745=CARTESIAN_POINT('Ctrl Pts',(182.623532676823,-3.68407824459055,331.382625374769));
#6746=CARTESIAN_POINT('Ctrl Pts',(182.581198022466,-4.17732424866067,331.998669568381));
#6747=CARTESIAN_POINT('Ctrl Pts',(182.566842787961,-4.32819357168361,332.220654920079));
#6748=CARTESIAN_POINT('Ctrl Pts',(182.537698961815,-4.5945884635041,332.687315536805));
#6749=CARTESIAN_POINT('Ctrl Pts',(182.522952343314,-4.70951594817475,332.9313757916));
#6750=CARTESIAN_POINT('Ctrl Pts',(182.508191721177,-4.8047733248247,333.183312393516));
#6751=CARTESIAN_POINT('Origin',(189.09641784506,0.,335.));
#6752=CARTESIAN_POINT('',(182.971417840485,-6.11287942610948,335.000034739551));
#6753=CARTESIAN_POINT('Ctrl Pts',(184.101667378079,3.72297207952785,339.848845683001));
#6754=CARTESIAN_POINT('Ctrl Pts',(184.06577619351,4.35425146681177,339.364145676672));
#6755=CARTESIAN_POINT('Ctrl Pts',(184.028753388829,4.88483466193755,338.760806757196));
#6756=CARTESIAN_POINT('Ctrl Pts',(183.975242140408,5.48153190724963,337.73453769235));
#6757=CARTESIAN_POINT('Ctrl Pts',(183.957754505071,5.64525739647646,337.37822516427));
#6758=CARTESIAN_POINT('Ctrl Pts',(183.921955243047,5.90331852565447,336.636460988997));
#6759=CARTESIAN_POINT('Ctrl Pts',(183.90371825822,5.99652186406069,336.252552776751));
#6760=CARTESIAN_POINT('Ctrl Pts',(183.849244162369,6.16357588372059,335.080159955476));
#6761=CARTESIAN_POINT('Ctrl Pts',(183.814673825568,6.12233986624375,334.283727463203));
#6762=CARTESIAN_POINT('Ctrl Pts',(183.76030572938,5.83597727670729,333.138361590064));
#6763=CARTESIAN_POINT('Ctrl Pts',(183.742219507261,5.70516911181519,332.769440905078));
#6764=CARTESIAN_POINT('Ctrl Pts',(183.707033966877,5.37616921254842,332.064201434522));
#6765=CARTESIAN_POINT('Ctrl Pts',(183.689753551581,5.17923231673713,331.72927171304));
#6766=CARTESIAN_POINT('Ctrl Pts',(183.654152583233,4.71968857120385,331.094466222427));
#6767=CARTESIAN_POINT('Ctrl Pts',(183.635893744349,4.45685056697839,330.797010174992));
#6768=CARTESIAN_POINT('Ctrl Pts',(183.580774235543,3.58212912876583,329.982093757339));
#6769=CARTESIAN_POINT('Ctrl Pts',(183.545795551112,2.89589044099009,329.557127752101));
#6770=CARTESIAN_POINT('Ctrl Pts',(183.49110700814,1.78201204891041,329.139240876818));
#6771=CARTESIAN_POINT('Ctrl Pts',(183.472983860139,1.40440778926222,329.037474092261));
#6772=CARTESIAN_POINT('Ctrl Pts',(183.429381363174,0.457065736262491,328.877213822844));
#6773=CARTESIAN_POINT('Ctrl Pts',(183.404099041264,-0.116111425258274,328.861274384291));
#6774=CARTESIAN_POINT('Ctrl Pts',(183.3600040241,-1.0717100492714,328.968736056802));
#6775=CARTESIAN_POINT('Ctrl Pts',(183.341838260232,-1.45516963137122,329.04960635248));
#6776=CARTESIAN_POINT('Ctrl Pts',(183.301857700579,-2.29133659393769,329.311670256026));
#6777=CARTESIAN_POINT('Ctrl Pts',(183.280383262249,-2.73548133766137,329.511423189919));
#6778=CARTESIAN_POINT('Ctrl Pts',(183.240332694653,-3.49026222444738,329.965484366751));
#6779=CARTESIAN_POINT('Ctrl Pts',(183.22207706571,-3.80860591688538,330.201793487443));
#6780=CARTESIAN_POINT('Ctrl Pts',(183.167072252517,-4.69356128800703,331.002615052679));
#6781=CARTESIAN_POINT('Ctrl Pts',(183.132167029559,-5.17471703029592,331.648744745133));
#6782=CARTESIAN_POINT('Ctrl Pts',(183.074871172973,-5.71081509644631,332.773154926883));
#6783=CARTESIAN_POINT('Ctrl Pts',(183.054135616454,-5.8585197077799,333.197218323336));
#6784=CARTESIAN_POINT('Ctrl Pts',(183.013181414721,-6.06137256395018,334.081822709202));
#6785=CARTESIAN_POINT('Ctrl Pts',(182.992662680761,-6.11325334319966,334.540200001429));
#6786=CARTESIAN_POINT('Ctrl Pts',(182.971631360442,-6.11324999983842,335.000044447211));
#6787=CARTESIAN_POINT('Ctrl Pts',(182.971417840484,-6.11287942610948,335.000034739551));
#6788=CARTESIAN_POINT('Ctrl Pts',(182.951327947679,-6.1130202861597,335.441078492841));
#6789=CARTESIAN_POINT('Ctrl Pts',(182.885455337599,-5.95859552868657,336.887118858306));
#6790=CARTESIAN_POINT('Ctrl Pts',(182.773800010244,-4.83029117599585,339.147696732808));
#6791=CARTESIAN_POINT('Ctrl Pts',(182.63645185842,-2.29132112187004,340.94001112084));
#6792=CARTESIAN_POINT('Ctrl Pts',(182.499103706597,0.793490165733074,341.316971685497));
#6793=CARTESIAN_POINT('Ctrl Pts',(182.40413033467,2.79592192577249,340.536520946628));
#6794=CARTESIAN_POINT('Ctrl Pts',(182.354939680017,3.66377807797318,339.894536771844));
#6795=CARTESIAN_POINT('Ctrl Pts',(182.351531742639,3.72305791812513,339.848957366357));
#6796=CARTESIAN_POINT('Ctrl Pts',(182.497067674234,3.72297189708705,339.84884582308));
#6797=CARTESIAN_POINT('Ctrl Pts',(182.506942057296,3.54913485701041,339.982318908943));
#6798=CARTESIAN_POINT('Ctrl Pts',(182.51684541491,3.36801225584443,340.106526560382));
#6799=CARTESIAN_POINT('Ctrl Pts',(182.544634213801,2.84640571252878,340.424268096816));
#6800=CARTESIAN_POINT('Ctrl Pts',(182.56266887492,2.49373645185283,340.595174463556));
#6801=CARTESIAN_POINT('Ctrl Pts',(182.598653591292,1.76007502943536,340.867477519029));
#6802=CARTESIAN_POINT('Ctrl Pts',(182.61622231947,1.38073110582571,340.968144057333));
#6803=CARTESIAN_POINT('Ctrl Pts',(182.669676867992,0.211030556525817,341.160972236312));
#6804=CARTESIAN_POINT('Ctrl Pts',(182.70645653674,-0.589998681150672,341.136286509658));
#6805=CARTESIAN_POINT('Ctrl Pts',(182.760155597291,-1.74930998512255,340.870951182526));
#6806=CARTESIAN_POINT('Ctrl Pts',(182.77785545865,-2.12525767241027,340.745557508671));
#6807=CARTESIAN_POINT('Ctrl Pts',(182.813596937793,-2.84112731345366,340.426835855446));
#6808=CARTESIAN_POINT('Ctrl Pts',(182.831545415987,-3.17994840794276,340.235501035293));
#6809=CARTESIAN_POINT('Ctrl Pts',(182.867286529096,-3.81873547811517,339.789753689841));
#6810=CARTESIAN_POINT('Ctrl Pts',(182.884744271952,-4.11697244107476,339.535969791996));
#6811=CARTESIAN_POINT('Ctrl Pts',(182.938488550358,-4.94564300042357,338.681304238242));
#6812=CARTESIAN_POINT('Ctrl Pts',(182.975538596472,-5.38429373502866,338.003459523774));
#6813=CARTESIAN_POINT('Ctrl Pts',(183.029479066173,-5.8267361261942,336.891682844458));
#6814=CARTESIAN_POINT('Ctrl Pts',(183.047298692267,-5.93721977410194,336.509547483994));
#6815=CARTESIAN_POINT('Ctrl Pts',(183.083905818102,-6.08379936212537,335.72259216024));
#6816=CARTESIAN_POINT('Ctrl Pts',(183.102617773177,-6.11822770455929,335.319433322501));
#6817=CARTESIAN_POINT('Ctrl Pts',(183.13888783016,-6.10728751354646,334.524875739508));
#6818=CARTESIAN_POINT('Ctrl Pts',(183.156305159263,-6.06440909376596,334.135330725164));
#6819=CARTESIAN_POINT('Ctrl Pts',(183.21019802125,-5.82148314915544,332.969894819936));
#6820=CARTESIAN_POINT('Ctrl Pts',(183.247141359612,-5.5063884631937,332.226792200719));
#6821=CARTESIAN_POINT('Ctrl Pts',(183.319668521704,-4.6017562250993,330.894774932291));
#6822=CARTESIAN_POINT('Ctrl Pts',(183.357053550118,-4.01740774154997,330.321384832669));
#6823=CARTESIAN_POINT('Ctrl Pts',(183.411619846854,-3.00884645031306,329.663961180505));
#6824=CARTESIAN_POINT('Ctrl Pts',(183.429169468911,-2.65945790878523,329.48150794177));
#6825=CARTESIAN_POINT('Ctrl Pts',(183.464868374054,-1.93143117386542,329.186632514181));
#6826=CARTESIAN_POINT('Ctrl Pts',(183.482937768214,-1.55456821070283,329.074717421328));
#6827=CARTESIAN_POINT('Ctrl Pts',(183.537703942053,-0.386455172397558,328.847025209151));
#6828=CARTESIAN_POINT('Ctrl Pts',(183.572741573386,0.419044494804354,328.849158734953));
#6829=CARTESIAN_POINT('Ctrl Pts',(183.627441193638,1.5849296429038,329.082834237044));
#6830=CARTESIAN_POINT('Ctrl Pts',(183.645494368152,1.96023768523414,329.196351183364));
#6831=CARTESIAN_POINT('Ctrl Pts',(183.68079565119,2.68291193061905,329.49310217574));
#6832=CARTESIAN_POINT('Ctrl Pts',(183.698241466175,3.02869057786356,329.675436834926));
#6833=CARTESIAN_POINT('Ctrl Pts',(183.733980331057,3.6844885044124,330.105925853116));
#6834=CARTESIAN_POINT('Ctrl Pts',(183.752201849441,3.99251437679522,330.353793380723));
#6835=CARTESIAN_POINT('Ctrl Pts',(183.806480331159,4.83747867651192,331.180215283661));
#6836=CARTESIAN_POINT('Ctrl Pts',(183.84109938916,5.28879016709082,331.83445910563));
#6837=CARTESIAN_POINT('Ctrl Pts',(183.886472648189,5.68270280946381,332.737723543505));
#6838=CARTESIAN_POINT('Ctrl Pts',(183.895608100515,5.75296897842462,332.922897617365));
#6839=CARTESIAN_POINT('Ctrl Pts',(183.941859290831,6.06453728829434,333.881947657604));
#6840=CARTESIAN_POINT('Ctrl Pts',(183.977540424845,6.15918472154949,334.694892606177));
#6841=CARTESIAN_POINT('Ctrl Pts',(184.024025798513,6.07624292445715,335.700330900127));
#6842=CARTESIAN_POINT('Ctrl Pts',(184.033175274057,6.05031410281653,335.897157616979));
#6843=CARTESIAN_POINT('Ctrl Pts',(184.060675687534,5.94278233206975,336.489251283774));
#6844=CARTESIAN_POINT('Ctrl Pts',(184.078635082676,5.83160136248364,336.878020796191));
#6845=CARTESIAN_POINT('Ctrl Pts',(184.132599901332,5.39230653803588,337.98609184279));
#6846=CARTESIAN_POINT('Ctrl Pts',(184.169066451217,4.96255223853182,338.656062637848));
#6847=CARTESIAN_POINT('Ctrl Pts',(184.218649363363,4.2016545045412,339.451443104235));
#6848=CARTESIAN_POINT('Ctrl Pts',(184.232676234344,3.96942652186749,339.659616522155));
#6849=CARTESIAN_POINT('Ctrl Pts',(184.246855413009,3.72297205899967,339.848845698762));
#6850=CARTESIAN_POINT('Origin',(180.696454890107,-1.2379162167118E-15,335.));
#6851=CARTESIAN_POINT('',(180.696454890107,3.31445696909756,340.13675));
#6852=CARTESIAN_POINT('',(180.696492164137,-2.55835334313229,340.136710345109));
#6853=CARTESIAN_POINT('',(180.696454890107,0.,340.13675));
#6854=CARTESIAN_POINT('',(180.696454890107,1.88832481980914,340.814297458627));
#6855=CARTESIAN_POINT('Origin',(180.696454890107,0.,335.));
#6856=CARTESIAN_POINT('Ctrl Pts',(180.696454890107,1.88832481980918,340.814297458627));
#6857=CARTESIAN_POINT('Ctrl Pts',(180.696454890107,1.72234987206334,340.854084373528));
#6858=CARTESIAN_POINT('Ctrl Pts',(180.696454890107,1.55490266737403,340.886650186877));
#6859=CARTESIAN_POINT('Ctrl Pts',(180.696454890107,1.38643951722482,340.912046446392));
#6860=CARTESIAN_POINT('Ctrl Pts',(180.696454890107,1.21798855966071,340.937440867843));
#6861=CARTESIAN_POINT('Ctrl Pts',(180.696454890107,1.04852103763536,340.955666657136));
#6862=CARTESIAN_POINT('Ctrl Pts',(180.696454890107,0.878495083065094,340.966723276416));
#6863=CARTESIAN_POINT('Ctrl Pts',(180.696454890106,0.782313019899616,340.972977900639));
#6864=CARTESIAN_POINT('Ctrl Pts',(180.696454890107,0.685952353875762,340.976937415162));
#6865=CARTESIAN_POINT('Ctrl Pts',(180.696454890106,0.589497696366717,340.97859454858));
#6866=CARTESIAN_POINT('Ctrl Pts',(180.696454890106,0.545379466010032,340.979352519172));
#6867=CARTESIAN_POINT('Ctrl Pts',(180.696454890107,0.501241594199461,340.979628729878));
#6868=CARTESIAN_POINT('Ctrl Pts',(180.696454890106,0.457092311071317,340.979422130108));
#6869=CARTESIAN_POINT('Ctrl Pts',(180.696454890106,0.428525290762674,340.979288448665));
#6870=CARTESIAN_POINT('Ctrl Pts',(180.696454890107,0.399960654754582,340.978952617827));
#6871=CARTESIAN_POINT('Ctrl Pts',(180.696454890107,0.371408088900426,340.978414853351));
#6872=CARTESIAN_POINT('Ctrl Pts',(180.696454890107,0.203593320499692,340.975254197965));
#6873=CARTESIAN_POINT('Ctrl Pts',(180.696454890106,0.0361136110770114,340.965121784186));
#6874=CARTESIAN_POINT('Ctrl Pts',(180.696454890106,-0.130589187275098,340.948025867259));
#6875=CARTESIAN_POINT('Ctrl Pts',(180.696454890106,-0.296170731460119,340.931044938613));
#6876=CARTESIAN_POINT('Ctrl Pts',(180.696454890106,-0.460986474971263,340.907193694938));
#6877=CARTESIAN_POINT('Ctrl Pts',(180.696454890106,-0.624587627822799,340.876431826722));
#6878=CARTESIAN_POINT('Ctrl Pts',(180.696454890106,-0.690380933313477,340.864060734235));
#6879=CARTESIAN_POINT('Ctrl Pts',(180.696454890107,-0.755977566272227,340.850571450757));
#6880=CARTESIAN_POINT('Ctrl Pts',(180.696454890107,-0.821347224492345,340.835959217821));
#6881=CARTESIAN_POINT('Ctrl Pts',(180.696454890107,-0.857644271323373,340.827845653858));
#6882=CARTESIAN_POINT('Ctrl Pts',(180.696454890107,-0.893871326317157,340.819385849771));
#6883=CARTESIAN_POINT('Ctrl Pts',(180.696454890107,-0.930023097778579,340.810578830702));
#6884=CARTESIAN_POINT('Ctrl Pts',(180.696454890107,-0.957697296363754,340.803837053334));
#6885=CARTESIAN_POINT('Ctrl Pts',(180.696454890107,-0.985330455584287,340.796890932872));
#6886=CARTESIAN_POINT('Ctrl Pts',(180.696454890106,-1.01289593960887,340.789746501884));
#6887=CARTESIAN_POINT('Ctrl Pts',(180.696454890106,-1.14387746377719,340.755798668453));
#6888=CARTESIAN_POINT('Ctrl Pts',(180.696454890106,-1.27344265908636,340.71734924744));
#6889=CARTESIAN_POINT('Ctrl Pts',(180.696454890106,-1.40136267565137,340.674406381647));
#6890=CARTESIAN_POINT('Ctrl Pts',(180.696454890106,-1.55702980066537,340.622148786336));
#6891=CARTESIAN_POINT('Ctrl Pts',(180.696454890106,-1.71026170156066,340.563238091871));
#6892=CARTESIAN_POINT('Ctrl Pts',(180.696454890106,-1.86067649098094,340.497921756323));
#6893=CARTESIAN_POINT('Ctrl Pts',(180.696454890106,-2.01048424259179,340.43286902175));
#6894=CARTESIAN_POINT('Ctrl Pts',(180.696454890106,-2.15749817695002,340.361461748611));
#6895=CARTESIAN_POINT('Ctrl Pts',(180.696454890106,-2.30131165414403,340.283902230785));
#6896=CARTESIAN_POINT('Ctrl Pts',(180.696454890106,-2.38812811128342,340.237081566363));
#6897=CARTESIAN_POINT('Ctrl Pts',(180.696454890106,-2.47377764295648,340.18801810646));
#6898=CARTESIAN_POINT('Ctrl Pts',(180.696454890107,-2.55816418736645,340.13675));
#6899=CARTESIAN_POINT('Ctrl Pts',(185.231465761173,-1.57897629365943,329.093805880512));
#6900=CARTESIAN_POINT('Ctrl Pts',(185.187526654506,-2.51072920729258,329.342902969502));
#6901=CARTESIAN_POINT('Ctrl Pts',(185.099648441175,-4.25344831580121,330.290005670493));
#6902=CARTESIAN_POINT('Ctrl Pts',(184.96783112118,-5.93304968749718,332.746577952619));
#6903=CARTESIAN_POINT('Ctrl Pts',(184.836013801182,-6.30803335278088,335.698484020827));
#6904=CARTESIAN_POINT('Ctrl Pts',(184.704196481186,-5.29636932799949,338.49694942919));
#6905=CARTESIAN_POINT('Ctrl Pts',(184.572379161188,-3.12028812894157,340.526647782566));
#6906=CARTESIAN_POINT('Ctrl Pts',(184.440561841193,-0.258262683773776,341.341399014455));
#6907=CARTESIAN_POINT('Ctrl Pts',(184.308744521195,2.66055317911897,340.762062281473));
#6908=CARTESIAN_POINT('Ctrl Pts',(184.176927201199,4.99446944125117,338.916002801078));
#6909=CARTESIAN_POINT('Ctrl Pts',(184.045109881202,6.23040426257297,336.209052024929));
#6910=CARTESIAN_POINT('Ctrl Pts',(183.913292561205,6.09664594605466,333.236306302429));
#6911=CARTESIAN_POINT('Ctrl Pts',(183.781475241208,4.62260115430969,330.651292619679));
#6912=CARTESIAN_POINT('Ctrl Pts',(183.649657921213,2.13232327726643,329.022300393848));
#6913=CARTESIAN_POINT('Ctrl Pts',(183.517840601215,-0.826724487129161,328.707446948171));
#6914=CARTESIAN_POINT('Ctrl Pts',(183.386023281219,-3.60402487195393,329.775949553599));
#6915=CARTESIAN_POINT('Ctrl Pts',(183.254205961221,-5.58901576521575,331.992908371219));
#6916=CARTESIAN_POINT('Ctrl Pts',(183.122388641226,-6.34531641714774,334.870946885228));
#6917=CARTESIAN_POINT('Ctrl Pts',(182.990571321228,-5.70666151580543,337.777356955005));
#6918=CARTESIAN_POINT('Ctrl Pts',(182.858754001232,-3.81345246746879,340.073193030899));
#6919=CARTESIAN_POINT('Ctrl Pts',(182.726936681235,-1.081892576986,341.253739083616));
#6920=CARTESIAN_POINT('Ctrl Pts',(182.595119361239,1.88751380770297,341.05946322403));
#6921=CARTESIAN_POINT('Ctrl Pts',(182.463302041241,4.4419707709344,339.533078493106));
#6922=CARTESIAN_POINT('Ctrl Pts',(182.331484721246,6.01991459103887,337.010141634552));
#6923=CARTESIAN_POINT('Ctrl Pts',(182.199667401248,6.27444029061672,334.045310123841));
#6924=CARTESIAN_POINT('Ctrl Pts',(182.067850081252,5.14962919993828,331.290350087674));
#6925=CARTESIAN_POINT('Ctrl Pts',(181.936032761254,2.89270329319507,329.350979521661));
#6926=CARTESIAN_POINT('Ctrl Pts',(181.804215441259,-8.68525194521966E-6,
328.653426946938));
#6927=CARTESIAN_POINT('Ctrl Pts',(181.672392861162,-2.89299401697966,329.351388838593));
#6928=CARTESIAN_POINT('Ctrl Pts',(181.584509387731,-4.39722124418262,330.644407214387));
#6929=CARTESIAN_POINT('Ctrl Pts',(181.540565020965,-4.96093856271488,331.427132287955));
#6930=CARTESIAN_POINT('Ctrl Pts',(185.419558053325,-1.49483501435035,329.408538109904));
#6931=CARTESIAN_POINT('Ctrl Pts',(185.37561894666,-2.37693621220545,329.644361188497));
#6932=CARTESIAN_POINT('Ctrl Pts',(185.287740733328,-4.02678843230346,330.540994206556));
#6933=CARTESIAN_POINT('Ctrl Pts',(185.155923413332,-5.61688636515029,332.866659434938));
#6934=CARTESIAN_POINT('Ctrl Pts',(185.024106093335,-5.971887713129,335.661262854603));
#6935=CARTESIAN_POINT('Ctrl Pts',(184.892288773338,-5.01413374742697,338.310602237131));
#6936=CARTESIAN_POINT('Ctrl Pts',(184.760471453342,-2.95401265283952,340.232141008409));
#6937=CARTESIAN_POINT('Ctrl Pts',(184.628654133345,-0.244500252572128,341.003475368718));
#6938=CARTESIAN_POINT('Ctrl Pts',(184.496836813348,2.51877628920628,340.45501062163));
#6939=CARTESIAN_POINT('Ctrl Pts',(184.365019493352,4.72832165300097,338.707324883124));
#6940=CARTESIAN_POINT('Ctrl Pts',(184.233202173355,5.89839536074794,336.144623455269));
#6941=CARTESIAN_POINT('Ctrl Pts',(184.101384853358,5.77176482437128,333.330290895243));
#6942=CARTESIAN_POINT('Ctrl Pts',(183.969567533362,4.37626966952355,330.883028715902));
#6943=CARTESIAN_POINT('Ctrl Pts',(183.837750213365,2.01869496684138,329.340843043416));
#6944=CARTESIAN_POINT('Ctrl Pts',(183.705932893368,-0.782669578729003,329.042767665794));
#6945=CARTESIAN_POINT('Ctrl Pts',(183.574115573371,-3.41197179008965,330.0543313694));
#6946=CARTESIAN_POINT('Ctrl Pts',(183.442298253375,-5.29118549477264,332.153151775544));
#6947=CARTESIAN_POINT('Ctrl Pts',(183.310480933378,-6.00718401889474,334.877823932224));
#6948=CARTESIAN_POINT('Ctrl Pts',(183.178663613381,-5.40256207970122,337.629355767001));
#6949=CARTESIAN_POINT('Ctrl Pts',(183.046846293385,-3.61023930303708,339.802850180587));
#6950=CARTESIAN_POINT('Ctrl Pts',(182.915028973388,-1.02424014365426,340.920486704163));
#6951=CARTESIAN_POINT('Ctrl Pts',(182.783211653391,1.78693102686489,340.736563513855));
#6952=CARTESIAN_POINT('Ctrl Pts',(182.651394333395,4.20526480845682,339.291517536713));
#6953=CARTESIAN_POINT('Ctrl Pts',(182.519577013398,5.69912236821994,336.903024200679));
#6954=CARTESIAN_POINT('Ctrl Pts',(182.387759693401,5.94008477488104,334.096184115962));
#6955=CARTESIAN_POINT('Ctrl Pts',(182.255942373404,4.87521318078071,331.488031769574));
#6956=CARTESIAN_POINT('Ctrl Pts',(182.124125053408,2.738555471769,329.652007353302));
#6957=CARTESIAN_POINT('Ctrl Pts',(181.992307733411,-8.22242789026327E-6,
328.991626309435));
#6958=CARTESIAN_POINT('Ctrl Pts',(181.860485153315,-2.73883070331901,329.652394858347));
#6959=CARTESIAN_POINT('Ctrl Pts',(181.772601679884,-4.16289991689208,330.876510223535));
#6960=CARTESIAN_POINT('Ctrl Pts',(181.728657313119,-4.69657758470859,331.617525051482));
#6961=CARTESIAN_POINT('Ctrl Pts',(185.607650345478,-1.41069373504128,329.723270339297));
#6962=CARTESIAN_POINT('Ctrl Pts',(185.563711238813,-2.24314321711833,329.945819407492));
#6963=CARTESIAN_POINT('Ctrl Pts',(185.475833025482,-3.80012854880572,330.791982742619));
#6964=CARTESIAN_POINT('Ctrl Pts',(185.344015705485,-5.30072304280342,332.986740917257));
#6965=CARTESIAN_POINT('Ctrl Pts',(185.212198385488,-5.63574207347713,335.62404168838));
#6966=CARTESIAN_POINT('Ctrl Pts',(185.080381065492,-4.73189816685444,338.124255045072));
#6967=CARTESIAN_POINT('Ctrl Pts',(184.948563745495,-2.78773717673747,339.937634234253));
#6968=CARTESIAN_POINT('Ctrl Pts',(184.816746425498,-0.230737821370482,340.665551722981));
#6969=CARTESIAN_POINT('Ctrl Pts',(184.684929105501,2.37699939929359,340.147958961786));
#6970=CARTESIAN_POINT('Ctrl Pts',(184.553111785505,4.46217386475077,338.49864696517));
#6971=CARTESIAN_POINT('Ctrl Pts',(184.421294465508,5.56638645892292,336.080194885608));
#6972=CARTESIAN_POINT('Ctrl Pts',(184.289477145511,5.44688370268791,333.424275488058));
#6973=CARTESIAN_POINT('Ctrl Pts',(184.157659825515,4.12993818473742,331.114764812125));
#6974=CARTESIAN_POINT('Ctrl Pts',(184.025842505518,1.90506665641634,329.659385692984));
#6975=CARTESIAN_POINT('Ctrl Pts',(183.894025185521,-0.738614670328843,329.378088383418));
#6976=CARTESIAN_POINT('Ctrl Pts',(183.762207865525,-3.21991870822537,330.332713185201));
#6977=CARTESIAN_POINT('Ctrl Pts',(183.630390545528,-4.99335522432953,332.313395179871));
#6978=CARTESIAN_POINT('Ctrl Pts',(183.498573225531,-5.66905162064175,334.884700979218));
#6979=CARTESIAN_POINT('Ctrl Pts',(183.366755905535,-5.09846264359701,337.481354578996));
#6980=CARTESIAN_POINT('Ctrl Pts',(183.234938585538,-3.40702613860538,339.532507330276));
#6981=CARTESIAN_POINT('Ctrl Pts',(183.103121265541,-0.966587710322523,340.587234324711));
#6982=CARTESIAN_POINT('Ctrl Pts',(182.971303945544,1.68634824602681,340.41366380368));
#6983=CARTESIAN_POINT('Ctrl Pts',(182.839486625548,3.96855884597923,339.04995658032));
#6984=CARTESIAN_POINT('Ctrl Pts',(182.707669305551,5.37833014540103,336.795906766805));
#6985=CARTESIAN_POINT('Ctrl Pts',(182.575851985554,5.60572925914536,334.147058108084));
#6986=CARTESIAN_POINT('Ctrl Pts',(182.444034665558,4.60079716162315,331.685713451475));
#6987=CARTESIAN_POINT('Ctrl Pts',(182.312217345561,2.58440765034293,329.953035184941));
#6988=CARTESIAN_POINT('Ctrl Pts',(182.180400025564,-7.75960383703391E-6,
329.329825671931));
#6989=CARTESIAN_POINT('Ctrl Pts',(182.048577445467,-2.58466738965833,329.953400878101));
#6990=CARTESIAN_POINT('Ctrl Pts',(181.960693972037,-3.92857858960154,331.108613232682));
#6991=CARTESIAN_POINT('Ctrl Pts',(181.916749605272,-4.4322166067023,331.807917815009));
#6992=CARTESIAN_POINT('Ctrl Pts',(185.795742637632,-1.3265524557322,330.03800256869));
#6993=CARTESIAN_POINT('Ctrl Pts',(185.751803530966,-2.1093502220312,330.247277626486));
#6994=CARTESIAN_POINT('Ctrl Pts',(185.663925317635,-3.57346866530796,331.042971278682));
#6995=CARTESIAN_POINT('Ctrl Pts',(185.532107997638,-4.98455972045654,333.106822399577));
#6996=CARTESIAN_POINT('Ctrl Pts',(185.400290677642,-5.29959643382524,335.586820522156));
#6997=CARTESIAN_POINT('Ctrl Pts',(185.268473357645,-4.44966258628191,337.937907853013));
#6998=CARTESIAN_POINT('Ctrl Pts',(185.136656037648,-2.62146170063543,339.643127460095));
#6999=CARTESIAN_POINT('Ctrl Pts',(185.004838717651,-0.216975390168832,340.327628077244));
#7000=CARTESIAN_POINT('Ctrl Pts',(184.873021397655,2.23522250938089,339.840907301943));
#7001=CARTESIAN_POINT('Ctrl Pts',(184.741204077658,4.19602607650056,338.289969047214));
#7002=CARTESIAN_POINT('Ctrl Pts',(184.609386757661,5.2343775570979,336.015766315947));
#7003=CARTESIAN_POINT('Ctrl Pts',(184.477569437665,5.12200258100453,333.518260080872));
#7004=CARTESIAN_POINT('Ctrl Pts',(184.345752117668,3.88360669995128,331.346500908347));
#7005=CARTESIAN_POINT('Ctrl Pts',(184.213934797671,1.79143834599129,329.977928342551));
#7006=CARTESIAN_POINT('Ctrl Pts',(184.082117477675,-0.694559761928685,329.713409101043));
#7007=CARTESIAN_POINT('Ctrl Pts',(183.950300157678,-3.02786562636109,330.611095001001));
#7008=CARTESIAN_POINT('Ctrl Pts',(183.818482837681,-4.69552495388641,332.473638584196));
#7009=CARTESIAN_POINT('Ctrl Pts',(183.686665517684,-5.33091922238874,334.891578026213));
#7010=CARTESIAN_POINT('Ctrl Pts',(183.554848197688,-4.79436320749281,337.333353390992));
#7011=CARTESIAN_POINT('Ctrl Pts',(183.423030877691,-3.20381297417367,339.262164479964));
#7012=CARTESIAN_POINT('Ctrl Pts',(183.291213557694,-0.908935276990783,340.253981945258));
#7013=CARTESIAN_POINT('Ctrl Pts',(183.159396237698,1.58576546518872,340.090764093505));
#7014=CARTESIAN_POINT('Ctrl Pts',(183.027578917701,3.73185288350165,338.808395623926));
#7015=CARTESIAN_POINT('Ctrl Pts',(182.895761597704,5.05753792258211,336.688789332932));
#7016=CARTESIAN_POINT('Ctrl Pts',(182.763944277708,5.27137374340969,334.197932100204));
#7017=CARTESIAN_POINT('Ctrl Pts',(182.632126957711,4.32638114246559,331.883395133376));
#7018=CARTESIAN_POINT('Ctrl Pts',(182.500309637714,2.43025982891686,330.25406301658));
#7019=CARTESIAN_POINT('Ctrl Pts',(182.368492317717,-7.2967797819764E-6,
329.668025034428));
#7020=CARTESIAN_POINT('Ctrl Pts',(182.236669737621,-2.43050407599766,330.254406897855));
#7021=CARTESIAN_POINT('Ctrl Pts',(182.148786264191,-3.694257262311,331.340716241829));
#7022=CARTESIAN_POINT('Ctrl Pts',(182.104841897425,-4.16785562869599,331.998310578537));
#7023=CARTESIAN_POINT('',(182.098201455916,5.31714584066979,331.98324026125));
#7024=CARTESIAN_POINT('Ctrl Pts',(182.098201455916,5.31714584066979,331.98324026125));
#7025=CARTESIAN_POINT('Ctrl Pts',(182.36457224063,5.17153456945061,332.589533674022));
#7026=CARTESIAN_POINT('Ctrl Pts',(182.554272439508,5.16167093112009,333.243177234899));
#7027=CARTESIAN_POINT('Ctrl Pts',(182.670936690558,5.19563211857749,334.03882223056));
#7028=CARTESIAN_POINT('Ctrl Pts',(182.68630128761,5.2025413294724,334.166354142561));
#7029=CARTESIAN_POINT('Ctrl Pts',(182.703702995273,5.21403594167573,334.350346852869));
#7030=CARTESIAN_POINT('Ctrl Pts',(182.708406884636,5.21778458694108,334.406932672582));
#7031=CARTESIAN_POINT('Ctrl Pts',(182.714388202159,5.22360384695214,334.490341292768));
#7032=CARTESIAN_POINT('Ctrl Pts',(182.716165632488,5.22551862931197,334.517145465015));
#7033=CARTESIAN_POINT('Ctrl Pts',(182.718501948241,5.22832067126957,334.555496791075));
#7034=CARTESIAN_POINT('Ctrl Pts',(182.719178355383,5.2291721325378,334.567040032337));
#7035=CARTESIAN_POINT('Ctrl Pts',(182.720301290642,5.23065780095879,334.586993502636));
#7036=CARTESIAN_POINT('Ctrl Pts',(182.720760367791,5.23128822200705,334.595403370524));
#7037=CARTESIAN_POINT('Ctrl Pts',(182.721612623099,5.23250403548237,334.611514451517));
#7038=CARTESIAN_POINT('Ctrl Pts',(182.722008094904,5.23308874225913,334.619215625598));
#7039=CARTESIAN_POINT('Ctrl Pts',(182.722906943869,5.2344672066849,334.637262610451));
#7040=CARTESIAN_POINT('Ctrl Pts',(182.723400757176,5.23526382239148,334.647608723816));
#7041=CARTESIAN_POINT('Ctrl Pts',(182.725084299949,5.23812572066465,334.684485286556));
#7042=CARTESIAN_POINT('Ctrl Pts',(182.726154441246,5.24022647461265,334.711018977282));
#7043=CARTESIAN_POINT('Ctrl Pts',(182.729082371591,5.2469763856141,334.794640030317));
#7044=CARTESIAN_POINT('Ctrl Pts',(182.730428556705,5.25177509506523,334.85173840005));
#7045=CARTESIAN_POINT('Ctrl Pts',(182.732688615482,5.2680118439349,335.037633251014));
#7046=CARTESIAN_POINT('Ctrl Pts',(182.730932937796,5.28021507889153,335.166443779557));
#7047=CARTESIAN_POINT('Ctrl Pts',(182.696705720863,5.36952673614242,336.03602657289));
#7048=CARTESIAN_POINT('Ctrl Pts',(182.558201552268,5.47160557667786,336.732739156913));
#7049=CARTESIAN_POINT('Ctrl Pts',(182.352165757496,5.64138616135816,337.35555453857));
#7050=CARTESIAN_POINT('',(181.566511620574,-4.60983126052084,330.984868456448));
#7051=CARTESIAN_POINT('Ctrl Pts',(182.098194326107,5.31700541326403,331.983167389824));
#7052=CARTESIAN_POINT('Ctrl Pts',(182.090071372961,5.22902379605754,331.82810451581));
#7053=CARTESIAN_POINT('Ctrl Pts',(182.081948419816,5.13427134210817,331.676921153739));
#7054=CARTESIAN_POINT('Ctrl Pts',(182.073825466671,5.03310363410748,331.53017387023));
#7055=CARTESIAN_POINT('Ctrl Pts',(182.071904021973,5.00917290933089,331.49546152058));
#7056=CARTESIAN_POINT('Ctrl Pts',(182.069982577276,4.98488341958961,331.460997258886));
#7057=CARTESIAN_POINT('Ctrl Pts',(182.068061132578,4.96024022379589,331.426788211603));
#7058=CARTESIAN_POINT('Ctrl Pts',(182.060324476436,4.86101492090906,331.28904621148));
#7059=CARTESIAN_POINT('Ctrl Pts',(182.052587820295,4.75603357271204,331.155418986902));
#7060=CARTESIAN_POINT('Ctrl Pts',(182.044851164153,4.64566163367922,331.026380296523));
#7061=CARTESIAN_POINT('Ctrl Pts',(182.037115822775,4.5353084512093,330.897363534927));
#7062=CARTESIAN_POINT('Ctrl Pts',(182.029380481398,4.41956671061087,330.772933990555));
#7063=CARTESIAN_POINT('Ctrl Pts',(182.02164514002,4.29884172136742,330.65353184561));
#7064=CARTESIAN_POINT('Ctrl Pts',(182.013909513125,4.17811227606205,330.534125293429));
#7065=CARTESIAN_POINT('Ctrl Pts',(182.00617388623,4.0523994357841,330.419746735568));
#7066=CARTESIAN_POINT('Ctrl Pts',(181.998438259334,3.92214543589988,330.310799562596));
#7067=CARTESIAN_POINT('Ctrl Pts',(181.990703046904,3.79189841486783,330.201858226882));
#7068=CARTESIAN_POINT('Ctrl Pts',(181.982967834474,3.65711096304351,330.098347895273));
#7069=CARTESIAN_POINT('Ctrl Pts',(181.975232622044,3.51825864005062,330.000631869505));
#7070=CARTESIAN_POINT('Ctrl Pts',(181.967495806112,3.37937753310672,329.902895587301));
#7071=CARTESIAN_POINT('Ctrl Pts',(181.959758990181,3.23643012848004,329.810956192851));
#7072=CARTESIAN_POINT('Ctrl Pts',(181.952022174249,3.08992193242528,329.725134313178));
#7073=CARTESIAN_POINT('Ctrl Pts',(181.946762720359,2.99032629665983,329.666792971882));
#7074=CARTESIAN_POINT('Ctrl Pts',(181.94150326647,2.88908575465452,329.61127777646));
#7075=CARTESIAN_POINT('Ctrl Pts',(181.936243812581,2.78636597990251,329.558677533123));
#7076=CARTESIAN_POINT('Ctrl Pts',(181.92850168363,2.63515831487129,329.481247846441));
#7077=CARTESIAN_POINT('Ctrl Pts',(181.92075955468,2.48069895433928,329.410113469557));
#7078=CARTESIAN_POINT('Ctrl Pts',(181.913017425729,2.32352993282106,329.34552971413));
#7079=CARTESIAN_POINT('Ctrl Pts',(181.905276596609,2.16638729849708,329.280956801706));
#7080=CARTESIAN_POINT('Ctrl Pts',(181.897535767488,2.00653620131673,329.22293243518));
#7081=CARTESIAN_POINT('Ctrl Pts',(181.889794938368,1.84453883308438,329.171663869015));
#7082=CARTESIAN_POINT('Ctrl Pts',(181.882053852307,1.68253608769299,329.120393601099));
#7083=CARTESIAN_POINT('Ctrl Pts',(181.874312766246,1.51838722708001,329.075879679895));
#7084=CARTESIAN_POINT('Ctrl Pts',(181.866571680185,1.3526705309753,329.038279778694));
#7085=CARTESIAN_POINT('Ctrl Pts',(181.858831037032,1.18696331637532,329.000682028776));
#7086=CARTESIAN_POINT('Ctrl Pts',(181.851090393878,1.01968875205604,328.969997576298));
#7087=CARTESIAN_POINT('Ctrl Pts',(181.843349750725,0.851436510272571,328.946333224278));
#7088=CARTESIAN_POINT('Ctrl Pts',(181.835607595032,0.683151391608317,328.922664248189));
#7089=CARTESIAN_POINT('Ctrl Pts',(181.827865439339,0.513888524648997,328.906018157963));
#7090=CARTESIAN_POINT('Ctrl Pts',(181.820123283645,0.344244788922837,328.896450124084));
#7091=CARTESIAN_POINT('Ctrl Pts',(181.814891019959,0.229597035336734,328.889983904828));
#7092=CARTESIAN_POINT('Ctrl Pts',(181.809658756272,0.114775467815156,328.886749342777));
#7093=CARTESIAN_POINT('Ctrl Pts',(181.804426492585,-3.50001460560987E-5,
328.8867500001));
#7094=CARTESIAN_POINT('Ctrl Pts',(181.796700703164,-0.169560381862912,328.886750970683));
#7095=CARTESIAN_POINT('Ctrl Pts',(181.788974913744,-0.339113346876187,328.893807899507));
#7096=CARTESIAN_POINT('Ctrl Pts',(181.781249124323,-0.508097471414815,328.907901632275));
#7097=CARTESIAN_POINT('Ctrl Pts',(181.773524701802,-0.677051698117159,328.921992871482));
#7098=CARTESIAN_POINT('Ctrl Pts',(181.765800279281,-0.845436969768592,328.943118403924));
#7099=CARTESIAN_POINT('Ctrl Pts',(181.758075856761,-1.01266077447828,328.971207109352));
#7100=CARTESIAN_POINT('Ctrl Pts',(181.750351129555,-1.17989117521914,328.999296922719));
#7101=CARTESIAN_POINT('Ctrl Pts',(181.74262640235,-1.34595970453457,329.0343504093));
#7102=CARTESIAN_POINT('Ctrl Pts',(181.734901675144,-1.51028209450224,329.076244978265));
#7103=CARTESIAN_POINT('Ctrl Pts',(181.727177328386,-1.67459639149987,329.1181374839));
#7104=CARTESIAN_POINT('Ctrl Pts',(181.719452981628,-1.83716441457824,329.166870318647));
#7105=CARTESIAN_POINT('Ctrl Pts',(181.71172863487,-1.99741494345117,329.222270419431));
#7106=CARTESIAN_POINT('Ctrl Pts',(181.704002541135,-2.1577017153836,329.277683049779));
#7107=CARTESIAN_POINT('Ctrl Pts',(181.696276447399,-2.31566964619419,329.339765856229));
#7108=CARTESIAN_POINT('Ctrl Pts',(181.688550353664,-2.47076463802303,329.40829653272));
#7109=CARTESIAN_POINT('Ctrl Pts',(181.683236626639,-2.57743334770278,329.455429446223));
#7110=CARTESIAN_POINT('Ctrl Pts',(181.677922899614,-2.68274346761574,329.505611299942));
#7111=CARTESIAN_POINT('Ctrl Pts',(181.672609172588,-2.7865206371216,329.558756732015));
#7112=CARTESIAN_POINT('Ctrl Pts',(181.664863530544,-2.93779314386834,329.636225049662));
#7113=CARTESIAN_POINT('Ctrl Pts',(181.657117888501,-3.08585657722454,329.720017559832));
#7114=CARTESIAN_POINT('Ctrl Pts',(181.649372246457,-3.23018632527504,329.80984375317));
#7115=CARTESIAN_POINT('Ctrl Pts',(181.641627509334,-3.3744992113262,329.899659452142));
#7116=CARTESIAN_POINT('Ctrl Pts',(181.633882772212,-3.51507901533247,329.995507264189));
#7117=CARTESIAN_POINT('Ctrl Pts',(181.626138035089,-3.65142820285723,330.09705214775));
#7118=CARTESIAN_POINT('Ctrl Pts',(181.618394362755,-3.78775864433969,330.198583070358));
#7119=CARTESIAN_POINT('Ctrl Pts',(181.610650690422,-3.91985937979659,330.305809313032));
#7120=CARTESIAN_POINT('Ctrl Pts',(181.602907018089,-4.04726388326374,330.418353939715));
#7121=CARTESIAN_POINT('Ctrl Pts',(181.595162963828,-4.17467467047373,330.530904117233));
#7122=CARTESIAN_POINT('Ctrl Pts',(181.587418909567,-4.29738852701738,330.648772996642));
#7123=CARTESIAN_POINT('Ctrl Pts',(181.579674855307,-4.41497333122138,330.771544484436));
#7124=CARTESIAN_POINT('Ctrl Pts',(181.575287110396,-4.48159633112227,330.841106234991));
#7125=CARTESIAN_POINT('Ctrl Pts',(181.570899365485,-4.54657339642634,330.912241177313));
#7126=CARTESIAN_POINT('Ctrl Pts',(181.566511620574,-4.60983126052084,330.984868456448));
#7127=CARTESIAN_POINT('Ctrl Pts',(182.104574390455,-4.16808369392609,331.997787668581));
#7128=CARTESIAN_POINT('Ctrl Pts',(182.024840110229,-4.22040928104604,331.815253763263));
#7129=CARTESIAN_POINT('Ctrl Pts',(181.939623298558,-4.28217880461786,331.639873365627));
#7130=CARTESIAN_POINT('Ctrl Pts',(181.758511384681,-4.42957189444357,331.300341201909));
#7131=CARTESIAN_POINT('Ctrl Pts',(181.66421667762,-4.51390798575797,331.139204559319));
#7132=CARTESIAN_POINT('Ctrl Pts',(181.566513177962,-4.60957431560398,330.985046921468));
#7133=CARTESIAN_POINT('Ctrl Pts',(185.231676812499,-1.57888188187688,329.094159029776));
#7134=CARTESIAN_POINT('Ctrl Pts',(185.231676812499,-1.73835198187131,329.150566371651));
#7135=CARTESIAN_POINT('Ctrl Pts',(185.231676812499,-1.89508205965106,329.213606388089));
#7136=CARTESIAN_POINT('Ctrl Pts',(185.231676812499,-2.04872667936675,329.282990086686));
#7137=CARTESIAN_POINT('Ctrl Pts',(185.231676812499,-2.20308815783609,329.352697508377));
#7138=CARTESIAN_POINT('Ctrl Pts',(185.231676812499,-2.35433594020408,329.42880840094));
#7139=CARTESIAN_POINT('Ctrl Pts',(185.231676812499,-2.5020949046273,329.511076494482));
#7140=CARTESIAN_POINT('Ctrl Pts',(185.231676812499,-2.64871564282186,329.592710855226));
#7141=CARTESIAN_POINT('Ctrl Pts',(185.231676812499,-2.79190164442619,329.680408433974));
#7142=CARTESIAN_POINT('Ctrl Pts',(185.231676812499,-2.93125343180188,329.773967200279));
#7143=CARTESIAN_POINT('Ctrl Pts',(185.231676812499,-3.06871479501524,329.866256763256));
#7144=CARTESIAN_POINT('Ctrl Pts',(185.231676812499,-3.20244572065316,329.964250061903));
#7145=CARTESIAN_POINT('Ctrl Pts',(185.231676812499,-3.33202330707788,330.067783390882));
#7146=CARTESIAN_POINT('Ctrl Pts',(185.231676812499,-3.38627701191309,330.111132451673));
#7147=CARTESIAN_POINT('Ctrl Pts',(185.231676812499,-3.43980208895837,330.155453043346));
#7148=CARTESIAN_POINT('Ctrl Pts',(185.231676812499,-3.4925651108654,330.200734444903));
#7149=CARTESIAN_POINT('Ctrl Pts',(185.231676812499,-3.5182625935215,330.222788110313));
#7150=CARTESIAN_POINT('Ctrl Pts',(185.231676812499,-3.54377929119041,330.245069694118));
#7151=CARTESIAN_POINT('Ctrl Pts',(185.231676812499,-3.56911120994015,330.26757801486));
#7152=CARTESIAN_POINT('Ctrl Pts',(185.231676812499,-3.58437253362646,330.281138249751));
#7153=CARTESIAN_POINT('Ctrl Pts',(185.231676812499,-3.59956441158646,330.294778713852));
#7154=CARTESIAN_POINT('Ctrl Pts',(185.231676812499,-3.61467856278962,330.308492172096));
#7155=CARTESIAN_POINT('Ctrl Pts',(185.231676812499,-3.72900933401943,330.41222742234));
#7156=CARTESIAN_POINT('Ctrl Pts',(185.231676812499,-3.83902172849591,330.520249660355));
#7157=CARTESIAN_POINT('Ctrl Pts',(185.231676812499,-3.94442751503383,330.632378002573));
#7158=CARTESIAN_POINT('Ctrl Pts',(185.231676812499,-4.05752303973181,330.752686518009));
#7159=CARTESIAN_POINT('Ctrl Pts',(185.231676812499,-4.16531615956235,330.877722271505));
#7160=CARTESIAN_POINT('Ctrl Pts',(185.231676812499,-4.26759160960737,331.007088100841));
#7161=CARTESIAN_POINT('Ctrl Pts',(185.231676812499,-4.36956160869967,331.136067572397));
#7162=CARTESIAN_POINT('Ctrl Pts',(185.231676812499,-4.46604714172357,331.269352010455));
#7163=CARTESIAN_POINT('Ctrl Pts',(185.231676812499,-4.55678877768288,331.406570494987));
#7164=CARTESIAN_POINT('Ctrl Pts',(185.231676812499,-4.63744662151081,331.528540382115));
#7165=CARTESIAN_POINT('Ctrl Pts',(185.231676812499,-4.71356574636673,331.653619176505));
#7166=CARTESIAN_POINT('Ctrl Pts',(185.231676812499,-4.78493037128097,331.78155472816));
#7167=CARTESIAN_POINT('Ctrl Pts',(185.231676812499,-4.81541526497096,331.83620507763));
#7168=CARTESIAN_POINT('Ctrl Pts',(185.231676812499,-4.8450321714567,331.891376775287));
#7169=CARTESIAN_POINT('Ctrl Pts',(185.231676812499,-4.87376238450164,331.947050328813));
#7170=CARTESIAN_POINT('Ctrl Pts',(185.231676812499,-4.88925064968163,331.977063568157));
#7171=CARTESIAN_POINT('Ctrl Pts',(185.231676812499,-4.90448120272001,332.007222658275));
#7172=CARTESIAN_POINT('Ctrl Pts',(185.231676812499,-4.91945097087971,332.037524544675));
#7173=CARTESIAN_POINT('Ctrl Pts',(185.231676812499,-4.9311703709993,332.061247018351));
#7174=CARTESIAN_POINT('Ctrl Pts',(185.231676812499,-4.94273150315958,332.085060457977));
#7175=CARTESIAN_POINT('Ctrl Pts',(185.231676812499,-4.95412148534072,332.108939074973));
#7176=CARTESIAN_POINT('Ctrl Pts',(185.231676812499,-5.02353469935308,332.254460948973));
#7177=CARTESIAN_POINT('Ctrl Pts',(185.231676812499,-5.08668092357429,332.402570634041));
#7178=CARTESIAN_POINT('Ctrl Pts',(185.231676812499,-5.14335414057236,332.55290189119));
#7179=CARTESIAN_POINT('Ctrl Pts',(185.231676812499,-5.19772593705412,332.697128405079));
#7180=CARTESIAN_POINT('Ctrl Pts',(185.231676812499,-5.24613970701393,332.843400400837));
#7181=CARTESIAN_POINT('Ctrl Pts',(185.231676812499,-5.2883700108282,332.991406338361));
#7182=CARTESIAN_POINT('Ctrl Pts',(185.231676812499,-5.33253917815909,333.14620747475));
#7183=CARTESIAN_POINT('Ctrl Pts',(185.231676812499,-5.36994432102688,333.302906181851));
#7184=CARTESIAN_POINT('Ctrl Pts',(185.231676812499,-5.4005338396348,333.46105196999));
#7185=CARTESIAN_POINT('Ctrl Pts',(185.231676812499,-5.43080057094012,333.617528969122));
#7186=CARTESIAN_POINT('Ctrl Pts',(185.231676812499,-5.45439463767241,333.775423415486));
#7187=CARTESIAN_POINT('Ctrl Pts',(185.231676812499,-5.47121620981323,333.934290241842));
#7188=CARTESIAN_POINT('Ctrl Pts',(185.231676812499,-5.47970963242515,334.014504093672));
#7189=CARTESIAN_POINT('Ctrl Pts',(185.231676812499,-5.48647571610912,334.094965633454));
#7190=CARTESIAN_POINT('Ctrl Pts',(185.231676812499,-5.49149684516094,334.175615808331));
#7191=CARTESIAN_POINT('Ctrl Pts',(185.231676812499,-5.49271232726811,334.195139075606));
#7192=CARTESIAN_POINT('Ctrl Pts',(185.231676812499,-5.49382492256659,334.214663472413));
#7193=CARTESIAN_POINT('Ctrl Pts',(185.231676812499,-5.49483465321806,334.234187817882));
#7194=CARTESIAN_POINT('Ctrl Pts',(185.231676812499,-5.5029708203841,334.391510306122));
#7195=CARTESIAN_POINT('Ctrl Pts',(185.231676812499,-5.50443303249865,334.548837541304));
#7196=CARTESIAN_POINT('Ctrl Pts',(185.231676812499,-5.4992155195584,334.705746654721));
#7197=CARTESIAN_POINT('Ctrl Pts',(185.231676812499,-5.49404352625385,334.861286831297));
#7198=CARTESIAN_POINT('Ctrl Pts',(185.231676812499,-5.48230771340722,335.016416879734));
#7199=CARTESIAN_POINT('Ctrl Pts',(185.231676812499,-5.46395236187144,335.170717561847));
#7200=CARTESIAN_POINT('Ctrl Pts',(185.231676812499,-5.44693143715193,335.313800645235));
#7201=CARTESIAN_POINT('Ctrl Pts',(185.231676812499,-5.42421792833861,335.456170938082));
#7202=CARTESIAN_POINT('Ctrl Pts',(185.231676812499,-5.39572976443111,335.597480368818));
#7203=CARTESIAN_POINT('Ctrl Pts',(185.231676812499,-5.36488434807988,335.750482445033));
#7204=CARTESIAN_POINT('Ctrl Pts',(185.231676812499,-5.32726895980449,335.902241751547));
#7205=CARTESIAN_POINT('Ctrl Pts',(185.231676812499,-5.28300576036397,336.052318876615));
#7206=CARTESIAN_POINT('Ctrl Pts',(185.231676812499,-5.26896492839455,336.099925188905));
#7207=CARTESIAN_POINT('Ctrl Pts',(185.231676812499,-5.25425487034703,336.14736198236));
#7208=CARTESIAN_POINT('Ctrl Pts',(185.231676812499,-5.2388786826432,336.194614475456));
#7209=CARTESIAN_POINT('Ctrl Pts',(185.231676812499,-5.23167458064542,336.216753368819));
#7210=CARTESIAN_POINT('Ctrl Pts',(185.231676812499,-5.22432424857934,336.238851799957));
#7211=CARTESIAN_POINT('Ctrl Pts',(185.231676812499,-5.21682797777118,336.260908217447));
#7212=CARTESIAN_POINT('Ctrl Pts',(185.231676812499,-5.2096173598859,336.282124153012));
#7213=CARTESIAN_POINT('Ctrl Pts',(185.231676812499,-5.20227473994666,336.303292285562));
#7214=CARTESIAN_POINT('Ctrl Pts',(185.231676812499,-5.1948013758209,336.324409488964));
#7215=CARTESIAN_POINT('Ctrl Pts',(185.231676812499,-5.14337557704968,336.469721430745));
#7216=CARTESIAN_POINT('Ctrl Pts',(185.231676812499,-5.08575233256317,336.612653986095));
#7217=CARTESIAN_POINT('Ctrl Pts',(185.231676812499,-5.02210170694438,336.752803828727));
#7218=CARTESIAN_POINT('Ctrl Pts',(185.231676812499,-4.95893748112331,336.891882686519));
#7219=CARTESIAN_POINT('Ctrl Pts',(185.231676812499,-4.88983719424972,337.028221804996));
#7220=CARTESIAN_POINT('Ctrl Pts',(185.231676812499,-4.81492740369595,337.161395345287));
#7221=CARTESIAN_POINT('Ctrl Pts',(185.231676812499,-4.77883982411297,337.225551321403));
#7222=CARTESIAN_POINT('Ctrl Pts',(185.231676812499,-4.74140342345992,337.288972099951));
#7223=CARTESIAN_POINT('Ctrl Pts',(185.231676812499,-4.70262948771864,337.351606785902));
#7224=CARTESIAN_POINT('Ctrl Pts',(185.231676812499,-4.68910049919007,337.373461259313));
#7225=CARTESIAN_POINT('Ctrl Pts',(185.231676812499,-4.675407234967,337.395222225542));
#7226=CARTESIAN_POINT('Ctrl Pts',(185.231676812499,-4.66155480165754,337.416880163837));
#7227=CARTESIAN_POINT('Ctrl Pts',(185.231676812499,-4.58035938880544,337.543827191992));
#7228=CARTESIAN_POINT('Ctrl Pts',(185.231676812499,-4.4937984836642,337.667083797264));
#7229=CARTESIAN_POINT('Ctrl Pts',(185.231676812499,-4.40201176383362,337.786251222207));
#7230=CARTESIAN_POINT('Ctrl Pts',(185.231676812499,-4.38153716639785,337.812833554136));
#7231=CARTESIAN_POINT('Ctrl Pts',(185.231676812499,-4.36080239410286,337.839212266764));
#7232=CARTESIAN_POINT('Ctrl Pts',(185.231676812499,-4.33980875715192,337.86538267042));
#7233=CARTESIAN_POINT('Ctrl Pts',(185.231676812499,-4.24507766023181,337.983473263819));
#7234=CARTESIAN_POINT('Ctrl Pts',(185.231676812499,-4.1450777393752,338.097325920217));
#7235=CARTESIAN_POINT('Ctrl Pts',(185.231676812499,-4.04013750288101,338.206631798415));
#7236=CARTESIAN_POINT('Ctrl Pts',(185.231676812499,-3.98795564423823,338.260984485958));
#7237=CARTESIAN_POINT('Ctrl Pts',(185.231676812499,-3.93455183338055,338.314212240782));
#7238=CARTESIAN_POINT('Ctrl Pts',(185.231676812499,-3.87996446941807,338.366272709916));
#7239=CARTESIAN_POINT('Origin',(189.09641784506,0.,335.));
#7240=CARTESIAN_POINT('',(181.433471471437,-4.42539066683714,330.782448221021));
#7241=CARTESIAN_POINT('Ctrl Pts',(181.56641430909,-4.60985083416171,330.984890929342));
#7242=CARTESIAN_POINT('Ctrl Pts',(181.522338792745,-4.54928340234734,330.915351890387));
#7243=CARTESIAN_POINT('Ctrl Pts',(181.477947892443,-4.48772044764387,330.847849582925));
#7244=CARTESIAN_POINT('Ctrl Pts',(181.433471471437,-4.4253906668373,330.782448221021));
#7245=CARTESIAN_POINT('',(181.93402621666,5.10326494491037,331.634214435745));
#7246=CARTESIAN_POINT('Ctrl Pts',(181.93402621666,5.10326494491053,331.634214435745));
#7247=CARTESIAN_POINT('Ctrl Pts',(181.990740853293,5.17775085053129,331.747151312973));
#7248=CARTESIAN_POINT('Ctrl Pts',(182.045657125741,5.2491901014954,331.863643016254));
#7249=CARTESIAN_POINT('Ctrl Pts',(182.09819904041,5.31704363992713,331.983234763259));
#7250=CARTESIAN_POINT('Ctrl Pts',(181.93402621666,5.10326494491048,331.634214435745));
#7251=CARTESIAN_POINT('Ctrl Pts',(181.926218208781,5.00890916558778,331.491150496651));
#7252=CARTESIAN_POINT('Ctrl Pts',(181.918410200902,4.90853007055727,331.352050989582));
#7253=CARTESIAN_POINT('Ctrl Pts',(181.910602193022,4.8024832581551,331.217410924031));
#7254=CARTESIAN_POINT('Ctrl Pts',(181.902794646657,4.69644271394199,331.082778816752));
#7255=CARTESIAN_POINT('Ctrl Pts',(181.894987100292,4.58473530854143,330.952605861636));
#7256=CARTESIAN_POINT('Ctrl Pts',(181.887179553927,4.4677576066271,330.827354852024));
#7257=CARTESIAN_POINT('Ctrl Pts',(181.879371329259,4.35076974194103,330.702092960874));
#7258=CARTESIAN_POINT('Ctrl Pts',(181.87156310459,4.22851087061426,330.581754091798));
#7259=CARTESIAN_POINT('Ctrl Pts',(181.863754879922,4.10141575942253,330.466765577332));
#7260=CARTESIAN_POINT('Ctrl Pts',(181.855946921021,3.97432497414003,330.351780976706));
#7261=CARTESIAN_POINT('Ctrl Pts',(181.84813896212,3.84239850333922,330.242146567915));
#7262=CARTESIAN_POINT('Ctrl Pts',(181.840331003219,3.70610593010505,330.138250891157));
#7263=CARTESIAN_POINT('Ctrl Pts',(181.832522197085,3.56979856793164,330.034343940806));
#7264=CARTESIAN_POINT('Ctrl Pts',(181.824713390952,3.42912439710866,329.936177149669));
#7265=CARTESIAN_POINT('Ctrl Pts',(181.816904584819,3.28458452298962,329.844097550008));
#7266=CARTESIAN_POINT('Ctrl Pts',(181.814232233331,3.23511968276336,329.81258581172));
#7267=CARTESIAN_POINT('Ctrl Pts',(181.811559881842,3.18520235873944,329.781786612718));
#7268=CARTESIAN_POINT('Ctrl Pts',(181.808887530354,3.13485339884983,329.751712686007));
#7269=CARTESIAN_POINT('Ctrl Pts',(181.801150672344,2.98908561519292,329.66464416161));
#7270=CARTESIAN_POINT('Ctrl Pts',(181.793413814334,2.83967110941098,329.583642068593));
#7271=CARTESIAN_POINT('Ctrl Pts',(181.785676956324,2.68713419412161,329.508995047782));
#7272=CARTESIAN_POINT('Ctrl Pts',(181.777941031189,2.53461567104635,329.434357027573));
#7273=CARTESIAN_POINT('Ctrl Pts',(181.770205106055,2.37897577251338,329.366072688317));
#7274=CARTESIAN_POINT('Ctrl Pts',(181.76246918092,2.22076193399246,329.30438396703));
#7275=CARTESIAN_POINT('Ctrl Pts',(181.754732579435,2.06253426287033,329.242689852311));
#7276=CARTESIAN_POINT('Ctrl Pts',(181.746995977951,1.90173249432713,329.18759262466));
#7277=CARTESIAN_POINT('Ctrl Pts',(181.739259376466,1.73892322056481,329.139285743574));
#7278=CARTESIAN_POINT('Ctrl Pts',(181.731522841827,1.57611535350781,329.090979279868));
#7279=CARTESIAN_POINT('Ctrl Pts',(181.723786307188,1.4113003184333,329.049463132175));
#7280=CARTESIAN_POINT('Ctrl Pts',(181.716049772549,1.24505923772503,329.014880698177));
#7281=CARTESIAN_POINT('Ctrl Pts',(181.708311535401,1.07878157385147,328.980290653937));
#7282=CARTESIAN_POINT('Ctrl Pts',(181.700573298253,0.911077545689822,328.952637435205));
#7283=CARTESIAN_POINT('Ctrl Pts',(181.692835061105,0.742538621281503,328.932013352157));
#7284=CARTESIAN_POINT('Ctrl Pts',(181.689806322086,0.676572638743626,328.92394110471));
#7285=CARTESIAN_POINT('Ctrl Pts',(181.686777583067,0.610478838334116,328.91694511559));
#7286=CARTESIAN_POINT('Ctrl Pts',(181.683748844048,0.544292940753909,328.911028760361));
#7287=CARTESIAN_POINT('Ctrl Pts',(181.676010618166,0.375192393463351,328.895912867948));
#7288=CARTESIAN_POINT('Ctrl Pts',(181.668272392283,0.205433266660727,328.887843045992));
#7289=CARTESIAN_POINT('Ctrl Pts',(181.660534166401,0.0356130198117278,328.886853733525));
#7290=CARTESIAN_POINT('Ctrl Pts',(181.652797465714,-0.134173755661763,328.88586461605));
#7291=CARTESIAN_POINT('Ctrl Pts',(181.645060765027,-0.3040213126236,328.891953225026));
#7292=CARTESIAN_POINT('Ctrl Pts',(181.63732406434,-0.473331423985043,328.90510189375));
#7293=CARTESIAN_POINT('Ctrl Pts',(181.62958756594,-0.64263710848922,328.918250218683));
#7294=CARTESIAN_POINT('Ctrl Pts',(181.62185106754,-0.811405061496992,328.938458213732));
#7295=CARTESIAN_POINT('Ctrl Pts',(181.61411456914,-0.979040697736622,328.965656218388));
#7296=CARTESIAN_POINT('Ctrl Pts',(181.606378644741,-1.14666389644456,328.99285220512));
#7297=CARTESIAN_POINT('Ctrl Pts',(181.598642720342,-1.31315463580628,329.027037113852));
#7298=CARTESIAN_POINT('Ctrl Pts',(181.590906795942,-1.47792674418541,329.068089843792));
#7299=CARTESIAN_POINT('Ctrl Pts',(181.583169911958,-1.64271929133618,329.109147666022));
#7300=CARTESIAN_POINT('Ctrl Pts',(181.575433027974,-1.80579247617785,329.157074935507));
#7301=CARTESIAN_POINT('Ctrl Pts',(181.56769614399,-1.96657281252487,329.211699996066));
#7302=CARTESIAN_POINT('Ctrl Pts',(181.564667481908,-2.02951149808858,329.233083391502));
#7303=CARTESIAN_POINT('Ctrl Pts',(181.561638819825,-2.09209899386936,329.25549261054));
#7304=CARTESIAN_POINT('Ctrl Pts',(181.558610157743,-2.15430159130236,329.278915293739));
#7305=CARTESIAN_POINT('Ctrl Pts',(181.550801355749,-2.31467860055276,329.339306017522));
#7306=CARTESIAN_POINT('Ctrl Pts',(181.542992553756,-2.47252542602931,329.40644852171));
#7307=CARTESIAN_POINT('Ctrl Pts',(181.535183751763,-2.62728026094965,329.480106523408));
#7308=CARTESIAN_POINT('Ctrl Pts',(181.527375758222,-2.78201907395733,329.553756899224));
#7309=CARTESIAN_POINT('Ctrl Pts',(181.519567764681,-2.93366626292296,329.633921295823));
#7310=CARTESIAN_POINT('Ctrl Pts',(181.51175977114,-3.08168227924436,329.720316307553));
#7311=CARTESIAN_POINT('Ctrl Pts',(181.503951611735,-3.22970143984743,329.806713154559));
#7312=CARTESIAN_POINT('Ctrl Pts',(181.496143452331,-3.37408901161883,329.899340730889));
#7313=CARTESIAN_POINT('Ctrl Pts',(181.488335292926,-3.51433151700546,329.997870498369));
#7314=CARTESIAN_POINT('Ctrl Pts',(181.480527696507,-3.65456391059011,330.096393161631));
#7315=CARTESIAN_POINT('Ctrl Pts',(181.472720100088,-3.79065158843474,330.200816991173));
#7316=CARTESIAN_POINT('Ctrl Pts',(181.464912503669,-3.92211110399618,330.310770846886));
#7317=CARTESIAN_POINT('Ctrl Pts',(181.45710449039,-4.05357763839256,330.420730573213));
#7318=CARTESIAN_POINT('Ctrl Pts',(181.449296477111,-4.18041528485859,330.53622072209));
#7319=CARTESIAN_POINT('Ctrl Pts',(181.441488463832,-4.30217403518314,330.656830174458));
#7320=CARTESIAN_POINT('Ctrl Pts',(181.438816133034,-4.34384656401224,330.698109350431));
#7321=CARTESIAN_POINT('Ctrl Pts',(181.436143802235,-4.38492446347651,330.73998786296));
#7322=CARTESIAN_POINT('Ctrl Pts',(181.433471471437,-4.42539066683728,330.782448221021));
#7323=CARTESIAN_POINT('Origin',(189.09641784506,0.,335.));
#7324=CARTESIAN_POINT('',(180.763832419144,3.42440815596402,340.064114369154));
#7325=CARTESIAN_POINT('Origin',(181.305293072034,1.78859679747709,337.316743696534));
#7326=CARTESIAN_POINT('',(181.127182464992,-3.98471776201124,339.636029163189));
#7327=CARTESIAN_POINT('Ctrl Pts',(181.127182464992,-3.98471776201124,339.636029163189));
#7328=CARTESIAN_POINT('Ctrl Pts',(181.067955450267,-2.99815593998204,340.482329942323));
#7329=CARTESIAN_POINT('Ctrl Pts',(180.946838768317,-0.4141468295078,341.549221172133));
#7330=CARTESIAN_POINT('Ctrl Pts',(180.825722086368,2.29912071323036,340.825045741512));
#7331=CARTESIAN_POINT('Ctrl Pts',(180.763832419144,3.42440815596409,340.064114369154));
#7332=CARTESIAN_POINT('',(180.967537046477,-3.74458518213069,339.832174187285));
#7333=CARTESIAN_POINT('Ctrl Pts',(180.967537046477,-3.74458518213077,339.832174187285));
#7334=CARTESIAN_POINT('Ctrl Pts',(181.021129560953,-3.82667683118351,339.768559102086));
#7335=CARTESIAN_POINT('Ctrl Pts',(181.074441913781,-3.9067932259694,339.703123245957));
#7336=CARTESIAN_POINT('Ctrl Pts',(181.127155953893,-3.98478354106129,339.636089482893));
#7337=CARTESIAN_POINT('Ctrl Pts',(180.967537046477,-3.74458518213076,339.832174187285));
#7338=CARTESIAN_POINT('Ctrl Pts',(180.928811024139,-3.07271202188714,340.352827247918));
#7339=CARTESIAN_POINT('Ctrl Pts',(180.838450305348,-1.24788233890097,341.236855210088));
#7340=CARTESIAN_POINT('Ctrl Pts',(180.748089586558,0.810419303791811,341.164371694386));
#7341=CARTESIAN_POINT('Ctrl Pts',(180.696454890107,1.88832481980924,340.814297458627));
#7342=CARTESIAN_POINT('Ctrl Pts',(185.231361012054,3.8792849430986,338.366214240201));
#7343=CARTESIAN_POINT('Ctrl Pts',(185.185572085065,4.43269208993578,337.728459763145));
#7344=CARTESIAN_POINT('Ctrl Pts',(185.094000440801,5.21810240427798,336.175231791177));
#7345=CARTESIAN_POINT('Ctrl Pts',(184.956646079264,5.15285959308729,333.5646422366));
#7346=CARTESIAN_POINT('Ctrl Pts',(184.81929792744,3.85951183190938,331.296424465933));
#7347=CARTESIAN_POINT('Ctrl Pts',(184.681949775617,1.64650067071449,329.910579844264));
#7348=CARTESIAN_POINT('Ctrl Pts',(184.544601623793,-0.958914747099921,329.737539388153));
#7349=CARTESIAN_POINT('Ctrl Pts',(184.40725347197,-3.33582893453105,330.818465109628));
#7350=CARTESIAN_POINT('Ctrl Pts',(184.269905320146,-4.91785548454191,332.895822139143));
#7351=CARTESIAN_POINT('Ctrl Pts',(184.132557168322,-5.32799673609857,335.474578828195));
#7352=CARTESIAN_POINT('Ctrl Pts',(183.995209016499,-4.46852102288055,337.9402460905));
#7353=CARTESIAN_POINT('Ctrl Pts',(183.857860864675,-2.54423183283122,339.705271838468));
#7354=CARTESIAN_POINT('Ctrl Pts',(183.720512712852,-0.013672882354056,340.349065869959));
#7355=CARTESIAN_POINT('Ctrl Pts',(183.583164561028,2.52014341764217,339.718216674611));
#7356=CARTESIAN_POINT('Ctrl Pts',(183.445816409204,4.45342772461749,337.963051390792));
#7357=CARTESIAN_POINT('Ctrl Pts',(183.308468257381,5.32549297122311,335.501812761407));
#7358=CARTESIAN_POINT('Ctrl Pts',(183.171120105557,4.928532499482,332.920995423183));
#7359=CARTESIAN_POINT('Ctrl Pts',(183.033771953734,3.3571385152569,330.83558891529));
#7360=CARTESIAN_POINT('Ctrl Pts',(182.89642380191,0.98576231142187,329.742529137502));
#7361=CARTESIAN_POINT('Ctrl Pts',(182.759075650087,-1.62051696004763,329.902284917117));
#7362=CARTESIAN_POINT('Ctrl Pts',(182.621727498263,-3.8406417937291,331.276783964202));
#7363=CARTESIAN_POINT('Ctrl Pts',(182.48437934644,-5.14558092249528,333.53849882316));
#7364=CARTESIAN_POINT('Ctrl Pts',(182.347031194616,-5.22436997067687,336.148463143921));
#7365=CARTESIAN_POINT('Ctrl Pts',(182.209683042792,-4.0582669213237,338.484771380675));
#7366=CARTESIAN_POINT('Ctrl Pts',(182.072334890969,-1.92509982860368,339.990620599394));
#7367=CARTESIAN_POINT('Ctrl Pts',(181.934986739145,0.666666827042015,340.307331649402));
#7368=CARTESIAN_POINT('Ctrl Pts',(181.797638587322,3.09968853668966,339.359057841091));
#7369=CARTESIAN_POINT('Ctrl Pts',(181.706073152773,4.22888407421017,338.034729998404));
#7370=CARTESIAN_POINT('Ctrl Pts',(181.660290435498,4.60334381111095,337.278042084719));
#7371=CARTESIAN_POINT('Ctrl Pts',(185.419486611316,4.12539012104192,338.579769770854));
#7372=CARTESIAN_POINT('Ctrl Pts',(185.373697684327,4.71390589391333,337.901555600488));
#7373=CARTESIAN_POINT('Ctrl Pts',(185.282126040064,5.54914331505611,336.249789508214));
#7374=CARTESIAN_POINT('Ctrl Pts',(185.144771678526,5.47976144373112,333.473581903844));
#7375=CARTESIAN_POINT('Ctrl Pts',(185.007423526703,4.10436258664865,331.061466444233));
#7376=CARTESIAN_POINT('Ctrl Pts',(184.870075374879,1.75095609136382,329.587702646164));
#7377=CARTESIAN_POINT('Ctrl Pts',(184.732727223055,-1.01974912455067,329.403684354482));
#7378=CARTESIAN_POINT('Ctrl Pts',(184.595379071232,-3.54745679522268,330.553184934708));
#7379=CARTESIAN_POINT('Ctrl Pts',(184.458030919408,-5.22984847213511,332.762331283362));
#7380=CARTESIAN_POINT('Ctrl Pts',(184.320682767585,-5.66600943793726,335.504686517802));
#7381=CARTESIAN_POINT('Ctrl Pts',(184.183334615761,-4.75200784522287,338.126777834859));
#7382=CARTESIAN_POINT('Ctrl Pts',(184.045986463938,-2.70564009160373,340.003778336461));
#7383=CARTESIAN_POINT('Ctrl Pts',(183.908638312114,-0.0145403017867841,
340.688415215796));
#7384=CARTESIAN_POINT('Ctrl Pts',(183.77129016029,2.68002348660821,340.017544404157));
#7385=CARTESIAN_POINT('Ctrl Pts',(183.633942008467,4.73595701511844,338.151029923043));
#7386=CARTESIAN_POINT('Ctrl Pts',(183.496593856643,5.66334683206167,335.533648195191));
#7387=CARTESIAN_POINT('Ctrl Pts',(183.35924570482,5.24120284609892,332.789101582224));
#7388=CARTESIAN_POINT('Ctrl Pts',(183.221897552996,3.57011827410332,330.571395089348));
#7389=CARTESIAN_POINT('Ctrl Pts',(183.084549401172,1.0482999214765,329.408990657828));
#7390=CARTESIAN_POINT('Ctrl Pts',(182.947201249349,-1.72332395171299,329.578881481696));
#7391=CARTESIAN_POINT('Ctrl Pts',(182.809853097525,-4.08429541699382,331.040579932157));
#7392=CARTESIAN_POINT('Ctrl Pts',(182.672504945702,-5.47202100800777,333.445779929738));
#7393=CARTESIAN_POINT('Ctrl Pts',(182.535156793878,-5.55580850126549,336.221322634921));
#7394=CARTESIAN_POINT('Ctrl Pts',(182.397808642055,-4.31572687011933,338.705848278432));
#7395=CARTESIAN_POINT('Ctrl Pts',(182.260460490231,-2.04722981978158,340.307229868545));
#7396=CARTESIAN_POINT('Ctrl Pts',(182.123112338408,0.708960744736812,340.644033340343));
#7397=CARTESIAN_POINT('Ctrl Pts',(181.985764186584,3.29633544715907,339.635600224901));
#7398=CARTESIAN_POINT('Ctrl Pts',(181.894198752035,4.49716812213418,338.227255883257));
#7399=CARTESIAN_POINT('Ctrl Pts',(181.84841603476,4.89538390725887,337.422563036606));
#7400=CARTESIAN_POINT('Ctrl Pts',(185.607612210577,4.37149529898523,338.793325301507));
#7401=CARTESIAN_POINT('Ctrl Pts',(185.561823283589,4.99511969789087,338.074651437831));
#7402=CARTESIAN_POINT('Ctrl Pts',(185.470251639326,5.88018422583424,336.32434722525));
#7403=CARTESIAN_POINT('Ctrl Pts',(185.332897277787,5.80666329437495,333.382521571088));
#7404=CARTESIAN_POINT('Ctrl Pts',(185.195549125964,4.34921334138792,330.826508422535));
#7405=CARTESIAN_POINT('Ctrl Pts',(185.05820097414,1.85541151201316,329.264825448066));
#7406=CARTESIAN_POINT('Ctrl Pts',(184.920852822317,-1.08058350200144,329.06982932081));
#7407=CARTESIAN_POINT('Ctrl Pts',(184.783504670493,-3.75908465591431,330.287904759788));
#7408=CARTESIAN_POINT('Ctrl Pts',(184.646156518669,-5.54184145972833,332.628840427582));
#7409=CARTESIAN_POINT('Ctrl Pts',(184.508808366846,-6.00402213977596,335.534794207408));
#7410=CARTESIAN_POINT('Ctrl Pts',(184.371460215022,-5.0354946675652,338.313309579218));
#7411=CARTESIAN_POINT('Ctrl Pts',(184.234112063199,-2.86704835037625,340.302284834453));
#7412=CARTESIAN_POINT('Ctrl Pts',(184.096763911375,-0.015407721219518,341.027764561634));
#7413=CARTESIAN_POINT('Ctrl Pts',(183.959415759552,2.83990355557424,340.316872133703));
#7414=CARTESIAN_POINT('Ctrl Pts',(183.822067607728,5.0184863056194,338.339008455293));
#7415=CARTESIAN_POINT('Ctrl Pts',(183.684719455904,6.00120069290021,335.565483628977));
#7416=CARTESIAN_POINT('Ctrl Pts',(183.547371304081,5.55387319271584,332.657207741263));
#7417=CARTESIAN_POINT('Ctrl Pts',(183.410023152257,3.78309803294972,330.307201263408));
#7418=CARTESIAN_POINT('Ctrl Pts',(183.272675000434,1.11083753153113,329.075452178153));
#7419=CARTESIAN_POINT('Ctrl Pts',(183.13532684861,-1.82613094337834,329.255478046274));
#7420=CARTESIAN_POINT('Ctrl Pts',(182.997978696786,-4.32794904025854,330.804375900113));
#7421=CARTESIAN_POINT('Ctrl Pts',(182.860630544963,-5.79846109352026,333.353061036317));
#7422=CARTESIAN_POINT('Ctrl Pts',(182.723282393139,-5.88724703185409,336.29418212592));
#7423=CARTESIAN_POINT('Ctrl Pts',(182.585934241316,-4.57318681891496,338.926925176187));
#7424=CARTESIAN_POINT('Ctrl Pts',(182.448586089492,-2.16935981095946,340.623839137696));
#7425=CARTESIAN_POINT('Ctrl Pts',(182.311237937669,0.751254662431609,340.980735031283));
#7426=CARTESIAN_POINT('Ctrl Pts',(182.173889785845,3.49298235762849,339.912142608713));
#7427=CARTESIAN_POINT('Ctrl Pts',(182.082324351296,4.76545217005818,338.419781768109));
#7428=CARTESIAN_POINT('Ctrl Pts',(182.036541634022,5.18742400340681,337.567083988495));
#7429=CARTESIAN_POINT('Ctrl Pts',(185.79573780984,4.61760047692855,339.006880832161));
#7430=CARTESIAN_POINT('Ctrl Pts',(185.74994888285,5.27633350186842,338.247747275175));
#7431=CARTESIAN_POINT('Ctrl Pts',(185.658377238587,6.21122513661239,336.398904942287));
#7432=CARTESIAN_POINT('Ctrl Pts',(185.52102287705,6.13356514501877,333.291461238332));
#7433=CARTESIAN_POINT('Ctrl Pts',(185.383674725226,4.59406409612719,330.591550400835));
#7434=CARTESIAN_POINT('Ctrl Pts',(185.246326573402,1.95986693266248,328.941948249966));
#7435=CARTESIAN_POINT('Ctrl Pts',(185.108978421579,-1.14141787945219,328.735974287139));
#7436=CARTESIAN_POINT('Ctrl Pts',(184.971630269755,-3.97071251660595,330.022624584868));
#7437=CARTESIAN_POINT('Ctrl Pts',(184.834282117932,-5.85383444732154,332.495349571801));
#7438=CARTESIAN_POINT('Ctrl Pts',(184.696933966108,-6.34203484161467,335.564901897015));
#7439=CARTESIAN_POINT('Ctrl Pts',(184.559585814284,-5.31898148990753,338.499841323576));
#7440=CARTESIAN_POINT('Ctrl Pts',(184.422237662461,-3.02845660914876,340.600791332446));
#7441=CARTESIAN_POINT('Ctrl Pts',(184.284889510637,-0.0162751406522468,
341.367113907471));
#7442=CARTESIAN_POINT('Ctrl Pts',(184.147541358814,2.99978362454027,340.616199863249));
#7443=CARTESIAN_POINT('Ctrl Pts',(184.01019320699,5.30101559612035,338.526986987545));
#7444=CARTESIAN_POINT('Ctrl Pts',(183.872845055167,6.33905455373877,335.597319062762));
#7445=CARTESIAN_POINT('Ctrl Pts',(183.735496903343,5.86654353933276,332.525313900304));
#7446=CARTESIAN_POINT('Ctrl Pts',(183.598148751519,3.99607779179613,330.043007437467));
#7447=CARTESIAN_POINT('Ctrl Pts',(183.460800599696,1.17337514158575,328.741913698478));
#7448=CARTESIAN_POINT('Ctrl Pts',(183.323452447872,-1.92893793504369,328.932074610852));
#7449=CARTESIAN_POINT('Ctrl Pts',(183.186104296049,-4.57160266352325,330.568171868067));
#7450=CARTESIAN_POINT('Ctrl Pts',(183.048756144225,-6.12490117903275,333.260342142895));
#7451=CARTESIAN_POINT('Ctrl Pts',(182.911407992402,-6.21868556244271,336.367041616919));
#7452=CARTESIAN_POINT('Ctrl Pts',(182.774059840578,-4.8306467677106,339.148002073944));
#7453=CARTESIAN_POINT('Ctrl Pts',(182.636711688754,-2.29148980213735,340.940448406847));
#7454=CARTESIAN_POINT('Ctrl Pts',(182.499363536931,0.793548580126407,341.317436722223));
#7455=CARTESIAN_POINT('Ctrl Pts',(182.362015385107,3.6896292680979,340.188684992523));
#7456=CARTESIAN_POINT('Ctrl Pts',(182.270449950558,5.03373621798219,338.612307652963));
#7457=CARTESIAN_POINT('Ctrl Pts',(182.224667233284,5.47946409955473,337.711604940384));
#7458=CARTESIAN_POINT('',(181.756492029768,3.56482183513016,338.698411259755));
#7459=CARTESIAN_POINT('Ctrl Pts',(182.22440740295,5.4790607473474,337.711405334762));
#7460=CARTESIAN_POINT('Ctrl Pts',(182.142804741226,5.18929109068282,337.921859087869));
#7461=CARTESIAN_POINT('Ctrl Pts',(182.059571383508,4.87878498043077,338.108495568584));
#7462=CARTESIAN_POINT('Ctrl Pts',(181.901355642956,4.23927546969376,338.434860777857));
#7463=CARTESIAN_POINT('Ctrl Pts',(181.825122559984,3.9053528405947,338.577120586524));
#7464=CARTESIAN_POINT('Ctrl Pts',(181.756589936366,3.56482809562168,338.69804120123));
#7465=CARTESIAN_POINT('Ctrl Pts',(185.231676812499,3.87994761181598,338.366334370211));
#7466=CARTESIAN_POINT('Ctrl Pts',(185.231676812499,3.98887908888609,338.26227654353));
#7467=CARTESIAN_POINT('Ctrl Pts',(185.231676812499,4.09289145755542,338.153540045282));
#7468=CARTESIAN_POINT('Ctrl Pts',(185.231676812499,4.19185479778346,338.040592391316));
#7469=CARTESIAN_POINT('Ctrl Pts',(185.231676812499,4.29083907028961,337.927620847173));
#7470=CARTESIAN_POINT('Ctrl Pts',(185.231676812499,4.3847726230792,337.810435804385));
#7471=CARTESIAN_POINT('Ctrl Pts',(185.231676812499,4.47350176833772,337.689455228141));
#7472=CARTESIAN_POINT('Ctrl Pts',(185.231676812499,4.56329988235493,337.567017132431));
#7473=CARTESIAN_POINT('Ctrl Pts',(185.231676812499,4.64776796769129,337.440690993295));
#7474=CARTESIAN_POINT('Ctrl Pts',(185.231676812499,4.72671497984256,337.31086694092));
#7475=CARTESIAN_POINT('Ctrl Pts',(185.231676812499,4.80373291167902,337.184215155829));
#7476=CARTESIAN_POINT('Ctrl Pts',(185.231676812499,4.87549659502638,337.054233621307));
#7477=CARTESIAN_POINT('Ctrl Pts',(185.231676812499,4.94179273439114,336.921253015162));
#7478=CARTESIAN_POINT('Ctrl Pts',(185.231676812499,4.95944215239198,336.885850798286));
#7479=CARTESIAN_POINT('Ctrl Pts',(185.231676812499,4.9767038507218,336.850235880878));
#7480=CARTESIAN_POINT('Ctrl Pts',(185.231676812499,4.9935733184925,336.814414206659));
#7481=CARTESIAN_POINT('Ctrl Pts',(185.231676812499,5.00746136130366,336.784923475127));
#7482=CARTESIAN_POINT('Ctrl Pts',(185.231676812499,5.02108356015116,336.755292608717));
#7483=CARTESIAN_POINT('Ctrl Pts',(185.231676812499,5.03443728573539,336.725524870692));
#7484=CARTESIAN_POINT('Ctrl Pts',(185.231676812499,5.04217089902195,336.708285324106));
#7485=CARTESIAN_POINT('Ctrl Pts',(185.231676812499,5.04981262271537,336.691003908423));
#7486=CARTESIAN_POINT('Ctrl Pts',(185.231676812499,5.05735898264887,336.673688581363));
#7487=CARTESIAN_POINT('Ctrl Pts',(185.231676812499,5.11956259584394,336.530960707751));
#7488=CARTESIAN_POINT('Ctrl Pts',(185.231676812499,5.17535555766318,336.385785177069));
#7489=CARTESIAN_POINT('Ctrl Pts',(185.231676812499,5.22457476715685,336.238591709152));
#7490=CARTESIAN_POINT('Ctrl Pts',(185.231676812499,5.23101520818529,336.21933112249));
#7491=CARTESIAN_POINT('Ctrl Pts',(185.231676812499,5.23734304307221,336.200035929469));
#7492=CARTESIAN_POINT('Ctrl Pts',(185.231676812499,5.24355786134782,336.180707045276));
#7493=CARTESIAN_POINT('Ctrl Pts',(185.231676812499,5.29059944982507,336.03440165458));
#7494=CARTESIAN_POINT('Ctrl Pts',(185.231676812499,5.33116954348734,335.886168433814));
#7495=CARTESIAN_POINT('Ctrl Pts',(185.231676812499,5.36533293185482,335.73645063595));
#7496=CARTESIAN_POINT('Ctrl Pts',(185.231676812499,5.39984925438767,335.585186137699));
#7497=CARTESIAN_POINT('Ctrl Pts',(185.231676812499,5.42782602535396,335.432405558752));
#7498=CARTESIAN_POINT('Ctrl Pts',(185.231676812499,5.44928286384492,335.278541235197));
#7499=CARTESIAN_POINT('Ctrl Pts',(185.231676812499,5.47082747880391,335.124047477493));
#7500=CARTESIAN_POINT('Ctrl Pts',(185.231676812499,5.48579888563856,334.96846034964));
#7501=CARTESIAN_POINT('Ctrl Pts',(185.231676812499,5.49416675161173,334.812203344854));
#7502=CARTESIAN_POINT('Ctrl Pts',(185.231676812499,5.49544915618552,334.788256415222));
#7503=CARTESIAN_POINT('Ctrl Pts',(185.231676812499,5.49657636724469,334.764293738091));
#7504=CARTESIAN_POINT('Ctrl Pts',(185.231676812499,5.49754816778483,334.740316825971));
#7505=CARTESIAN_POINT('Ctrl Pts',(185.231676812499,5.4984004910039,334.719287738131));
#7506=CARTESIAN_POINT('Ctrl Pts',(185.231676812499,5.49913331564855,334.698246030343));
#7507=CARTESIAN_POINT('Ctrl Pts',(185.231676812499,5.49974632691056,334.677197959552));
#7508=CARTESIAN_POINT('Ctrl Pts',(185.231676812499,5.50439948919236,334.517429134441));
#7509=CARTESIAN_POINT('Ctrl Pts',(185.231676812499,5.50214028330716,334.357775528399));
#7510=CARTESIAN_POINT('Ctrl Pts',(185.231676812499,5.49304585829882,334.198707600937));
#7511=CARTESIAN_POINT('Ctrl Pts',(185.231676812499,5.48395143329048,334.039639673475));
#7512=CARTESIAN_POINT('Ctrl Pts',(185.231676812499,5.46802189731941,333.881156663705));
#7513=CARTESIAN_POINT('Ctrl Pts',(185.231676812499,5.44528583335869,333.723709915607));
#7514=CARTESIAN_POINT('Ctrl Pts',(185.231676812499,5.43418336044101,333.646825532287));
#7515=CARTESIAN_POINT('Ctrl Pts',(185.231676812499,5.42145708271963,333.570188034188));
#7516=CARTESIAN_POINT('Ctrl Pts',(185.231676812499,5.40710599800657,333.493849160467));
#7517=CARTESIAN_POINT('Ctrl Pts',(185.231676812499,5.37769011372305,333.337374892452));
#7518=CARTESIAN_POINT('Ctrl Pts',(185.231676812499,5.34145116456449,333.182154935493));
#7519=CARTESIAN_POINT('Ctrl Pts',(185.231676812499,5.29861321794033,333.028558091743));
#7520=CARTESIAN_POINT('Ctrl Pts',(185.231676812499,5.27225910298788,332.934064559828));
#7521=CARTESIAN_POINT('Ctrl Pts',(185.231676812499,5.24340636780778,332.840185356584));
#7522=CARTESIAN_POINT('Ctrl Pts',(185.231676812499,5.21209752347118,332.747007855073));
#7523=CARTESIAN_POINT('Ctrl Pts',(185.231676812499,5.19774869360684,332.704304646293));
#7524=CARTESIAN_POINT('Ctrl Pts',(185.231676812499,5.18288388705462,332.661748845767));
#7525=CARTESIAN_POINT('Ctrl Pts',(185.231676812499,5.16750670028485,332.619349011203));
#7526=CARTESIAN_POINT('Ctrl Pts',(185.231676812499,5.16013741342817,332.599029524404));
#7527=CARTESIAN_POINT('Ctrl Pts',(185.231676812499,5.15265044561141,332.578745859302));
#7528=CARTESIAN_POINT('Ctrl Pts',(185.231676812499,5.14504616788639,332.558498967188));
#7529=CARTESIAN_POINT('Ctrl Pts',(185.231676812499,5.13740571884857,332.538155766562));
#7530=CARTESIAN_POINT('Ctrl Pts',(185.231676812499,5.12964958327893,332.517857060067));
#7531=CARTESIAN_POINT('Ctrl Pts',(185.231676812499,5.12178078536785,332.497609729186));
#7532=CARTESIAN_POINT('Ctrl Pts',(185.231676812499,5.06280079278511,332.34584735853));
#7533=CARTESIAN_POINT('Ctrl Pts',(185.231676812499,4.99745588381262,332.196865405903));
#7534=CARTESIAN_POINT('Ctrl Pts',(185.231676812499,4.92604289876815,332.051036300688));
#7535=CARTESIAN_POINT('Ctrl Pts',(185.231676812499,4.85395352364228,331.903825971033));
#7536=CARTESIAN_POINT('Ctrl Pts',(185.231676812499,4.77568040330955,331.759827788406));
#7537=CARTESIAN_POINT('Ctrl Pts',(185.231676812499,4.69147536577344,331.619427723857));
#7538=CARTESIAN_POINT('Ctrl Pts',(185.231676812499,4.60716592630847,331.478853583766));
#7539=CARTESIAN_POINT('Ctrl Pts',(185.231676812499,4.5169096000525,331.341885760191));
#7540=CARTESIAN_POINT('Ctrl Pts',(185.231676812499,4.4209090797894,331.208925334346));
#7541=CARTESIAN_POINT('Ctrl Pts',(185.231676812499,4.35701600287431,331.120433618968));
#7542=CARTESIAN_POINT('Ctrl Pts',(185.231676812499,4.29057747731511,331.033717298733));
#7543=CARTESIAN_POINT('Ctrl Pts',(185.231676812499,4.22164182107164,330.948900409606));
#7544=CARTESIAN_POINT('Ctrl Pts',(185.231676812499,4.18078803288743,330.898634822657));
#7545=CARTESIAN_POINT('Ctrl Pts',(185.231676812499,4.13905703477076,330.849036452026));
#7546=CARTESIAN_POINT('Ctrl Pts',(185.231676812499,4.09647004598961,330.80012006803));
#7547=CARTESIAN_POINT('Ctrl Pts',(185.231676812499,4.06686009781426,330.766109408049));
#7548=CARTESIAN_POINT('Ctrl Pts',(185.231676812499,4.03683632805114,330.732428447414));
#7549=CARTESIAN_POINT('Ctrl Pts',(185.231676812499,4.00640559299697,330.69908238668));
#7550=CARTESIAN_POINT('Ctrl Pts',(185.231676812499,3.99119933337399,330.682419336773));
#7551=CARTESIAN_POINT('Ctrl Pts',(185.231676812499,3.97588993501583,330.665838295175));
#7552=CARTESIAN_POINT('Ctrl Pts',(185.231676812499,3.96048314632903,330.649345180255));
#7553=CARTESIAN_POINT('Ctrl Pts',(185.231676812499,3.84539202131251,330.526139028103));
#7554=CARTESIAN_POINT('Ctrl Pts',(185.231676812499,3.72508679254122,330.408066830259));
#7555=CARTESIAN_POINT('Ctrl Pts',(185.231676812499,3.60001757347812,330.295335573318));
#7556=CARTESIAN_POINT('Ctrl Pts',(185.231676812499,3.47494835441503,330.182604316378));
#7557=CARTESIAN_POINT('Ctrl Pts',(185.231676812499,3.34511458049823,330.075213491582));
#7558=CARTESIAN_POINT('Ctrl Pts',(185.231676812499,3.21091932475301,329.973398455747));
#7559=CARTESIAN_POINT('Ctrl Pts',(185.231676812499,3.15167027138406,329.928445715366));
#7560=CARTESIAN_POINT('Ctrl Pts',(185.231676812499,3.09157045089737,329.884580305075));
#7561=CARTESIAN_POINT('Ctrl Pts',(185.231676812499,3.03065207423348,329.841824638955));
#7562=CARTESIAN_POINT('Ctrl Pts',(185.231676812499,2.98416479193989,329.809197460928));
#7563=CARTESIAN_POINT('Ctrl Pts',(185.231676812499,2.93720080625702,329.777216550693));
#7564=CARTESIAN_POINT('Ctrl Pts',(185.231676812499,2.8897739093974,329.745892454179));
#7565=CARTESIAN_POINT('Ctrl Pts',(185.231676812499,2.86904115537433,329.732199068547));
#7566=CARTESIAN_POINT('Ctrl Pts',(185.231676812499,2.84822276624274,329.718633121031));
#7567=CARTESIAN_POINT('Ctrl Pts',(185.231676812499,2.82732709096244,329.705199893148));
#7568=CARTESIAN_POINT('Ctrl Pts',(185.231676812499,2.68375632121808,329.612902379839));
#7569=CARTESIAN_POINT('Ctrl Pts',(185.231676812499,2.53644282832064,329.526803017701));
#7570=CARTESIAN_POINT('Ctrl Pts',(185.231676812499,2.38580446285762,329.447132130605));
#7571=CARTESIAN_POINT('Ctrl Pts',(185.231676812499,2.23563497383018,329.367709226826));
#7572=CARTESIAN_POINT('Ctrl Pts',(185.231676812499,2.08216068135469,329.294674353791));
#7573=CARTESIAN_POINT('Ctrl Pts',(185.231676812499,1.92575956440724,329.228292618111));
#7574=CARTESIAN_POINT('Ctrl Pts',(185.231676812499,1.90861073917047,329.221014097303));
#7575=CARTESIAN_POINT('Ctrl Pts',(185.231676812499,1.89142669618393,329.213815603767));
#7576=CARTESIAN_POINT('Ctrl Pts',(185.231676812499,1.87420791206738,329.206697518036));
#7577=CARTESIAN_POINT('Ctrl Pts',(185.231676812499,1.77690397932603,329.166472974276));
#7578=CARTESIAN_POINT('Ctrl Pts',(185.231676812499,1.67849090257524,329.128815625578));
#7579=CARTESIAN_POINT('Ctrl Pts',(185.231676812499,1.57907388322304,329.093732219127));
#7580=CARTESIAN_POINT('',(182.258435337963,-4.41716094758247,337.622001091848));
#7581=CARTESIAN_POINT('Ctrl Pts',(182.258477686866,-4.41710803447555,337.621844669693));
#7582=CARTESIAN_POINT('Ctrl Pts',(182.349960492498,-4.70739653859804,337.376661777648));
#7583=CARTESIAN_POINT('Ctrl Pts',(182.440441383438,-4.97446109536007,337.095107460796));
#7584=CARTESIAN_POINT('Ctrl Pts',(182.568982327825,-5.33380935274516,336.568720006854));
#7585=CARTESIAN_POINT('Ctrl Pts',(182.614744225292,-5.45551217225447,336.341694783932));
#7586=CARTESIAN_POINT('Ctrl Pts',(182.670714469732,-5.59449636699666,335.964114480957));
#7587=CARTESIAN_POINT('Ctrl Pts',(182.687574387585,-5.63385575200452,335.824697776433));
#7588=CARTESIAN_POINT('Ctrl Pts',(182.706239595221,-5.6731353981708,335.620282861155));
#7589=CARTESIAN_POINT('Ctrl Pts',(182.711142624749,-5.68272605401884,335.558138683474));
#7590=CARTESIAN_POINT('Ctrl Pts',(182.716919714594,-5.69283968382394,335.470904937064));
#7591=CARTESIAN_POINT('Ctrl Pts',(182.718435698403,-5.69533642365568,335.446158968727));
#7592=CARTESIAN_POINT('Ctrl Pts',(182.720459401172,-5.69842158081797,335.41019580278));
#7593=CARTESIAN_POINT('Ctrl Pts',(182.721063514815,-5.69930484271052,335.399014218728));
#7594=CARTESIAN_POINT('Ctrl Pts',(182.722057144062,-5.70069009110022,335.379824532242));
#7595=CARTESIAN_POINT('Ctrl Pts',(182.722458743629,-5.70122898255233,335.371820293223));
#7596=CARTESIAN_POINT('Ctrl Pts',(182.723251756172,-5.70224885894303,335.355491589503));
#7597=CARTESIAN_POINT('Ctrl Pts',(182.723642136471,-5.70272672527546,335.347167209565));
#7598=CARTESIAN_POINT('Ctrl Pts',(182.724577978155,-5.70380994661762,335.326474111663));
#7599=CARTESIAN_POINT('Ctrl Pts',(182.725106794512,-5.70436469462718,335.314102744529));
#7600=CARTESIAN_POINT('Ctrl Pts',(182.726971316045,-5.70609320273036,335.26779388918));
#7601=CARTESIAN_POINT('Ctrl Pts',(182.728107592672,-5.70666173958303,335.233838419053));
#7602=CARTESIAN_POINT('Ctrl Pts',(182.731015334075,-5.7062376554595,335.124764542842));
#7603=CARTESIAN_POINT('Ctrl Pts',(182.731884562569,-5.70252219120966,335.049775454453));
#7604=CARTESIAN_POINT('Ctrl Pts',(182.731029638564,-5.67813275898276,334.793468251929));
#7605=CARTESIAN_POINT('Ctrl Pts',(182.723830789714,-5.64105770048092,334.615488743082));
#7606=CARTESIAN_POINT('Ctrl Pts',(182.692813006775,-5.50897328499186,334.199640387766));
#7607=CARTESIAN_POINT('Ctrl Pts',(182.663869070168,-5.39824504733339,333.970817760501));
#7608=CARTESIAN_POINT('Ctrl Pts',(182.593220142657,-5.13036614653951,333.550186573158));
#7609=CARTESIAN_POINT('Ctrl Pts',(182.552104916986,-4.97514574927775,333.358657311859));
#7610=CARTESIAN_POINT('Ctrl Pts',(182.508320087374,-4.80500519224339,333.183282451721));
#7611=CARTESIAN_POINT('Ctrl Pts',(181.756492029768,3.56482183513016,338.698411259755));
#7612=CARTESIAN_POINT('Ctrl Pts',(181.764934144517,3.45271479600097,338.806468907455));
#7613=CARTESIAN_POINT('Ctrl Pts',(181.773376259266,3.33571674076433,338.909401826378));
#7614=CARTESIAN_POINT('Ctrl Pts',(181.781818374015,3.2143022604258,339.006801909394));
#7615=CARTESIAN_POINT('Ctrl Pts',(181.78720325498,3.13685691130715,339.068929453096));
#7616=CARTESIAN_POINT('Ctrl Pts',(181.792588135945,3.05761537103361,339.128806670922));
#7617=CARTESIAN_POINT('Ctrl Pts',(181.79797301691,2.97670766664917,339.186336349341));
#7618=CARTESIAN_POINT('Ctrl Pts',(181.806031590385,2.85562779789292,339.272430571956));
#7619=CARTESIAN_POINT('Ctrl Pts',(181.81409016386,2.73078611467066,339.353285532255));
#7620=CARTESIAN_POINT('Ctrl Pts',(181.822148737336,2.60265733937138,339.428586155458));
#7621=CARTESIAN_POINT('Ctrl Pts',(181.830205583936,2.474556020847,339.503870642456));
#7622=CARTESIAN_POINT('Ctrl Pts',(181.838262430535,2.34316930203407,339.573602998336));
#7623=CARTESIAN_POINT('Ctrl Pts',(181.846319277135,2.20899874841433,339.637512813136));
#7624=CARTESIAN_POINT('Ctrl Pts',(181.854376313082,2.07482504159838,339.701424129907));
#7625=CARTESIAN_POINT('Ctrl Pts',(181.862433349029,1.93786766757888,339.759512485029));
#7626=CARTESIAN_POINT('Ctrl Pts',(181.870490384976,1.79865101653544,339.811554331317));
#7627=CARTESIAN_POINT('Ctrl Pts',(181.878546931079,1.65944282945296,339.863593013615));
#7628=CARTESIAN_POINT('Ctrl Pts',(181.886603477182,1.51797595199898,339.909585806759));
#7629=CARTESIAN_POINT('Ctrl Pts',(181.894660023285,1.37479288358573,339.949358048246));
#7630=CARTESIAN_POINT('Ctrl Pts',(181.90271854851,1.2315746416961,339.98914005994));
#7631=CARTESIAN_POINT('Ctrl Pts',(181.910777073734,1.08663968699248,340.022698377151));
#7632=CARTESIAN_POINT('Ctrl Pts',(181.918835598959,0.940544380227419,340.049908596333));
#7633=CARTESIAN_POINT('Ctrl Pts',(181.924330788884,0.840920511667451,340.068463520234));
#7634=CARTESIAN_POINT('Ctrl Pts',(181.929825978809,0.740757356148767,340.084067618826));
#7635=CARTESIAN_POINT('Ctrl Pts',(181.935321168733,0.640233743136665,340.096695136718));
#7636=CARTESIAN_POINT('Ctrl Pts',(181.9433976224,0.492491023764222,340.115254197386));
#7637=CARTESIAN_POINT('Ctrl Pts',(181.951474076068,0.343915819091288,340.127387947124));
#7638=CARTESIAN_POINT('Ctrl Pts',(181.959550529735,0.195078012643335,340.133044431084));
#7639=CARTESIAN_POINT('Ctrl Pts',(181.967625476531,0.0462679757346483,340.13869985968));
#7640=CARTESIAN_POINT('Ctrl Pts',(181.975700423327,-0.102804235986503,340.137880421174));
#7641=CARTESIAN_POINT('Ctrl Pts',(181.983775370123,-0.251566345801858,340.130586217593));
#7642=CARTESIAN_POINT('Ctrl Pts',(181.991850664336,-0.400334855969035,340.123291700186));
#7643=CARTESIAN_POINT('Ctrl Pts',(181.999925958549,-0.548792908144701,340.109521873129));
#7644=CARTESIAN_POINT('Ctrl Pts',(182.008001252762,-0.696370379884273,340.089328920056));
#7645=CARTESIAN_POINT('Ctrl Pts',(182.016076104672,-0.84393976846008,340.069137072998));
#7646=CARTESIAN_POINT('Ctrl Pts',(182.024150956582,-0.990628346638582,340.042522849499));
#7647=CARTESIAN_POINT('Ctrl Pts',(182.032225808493,-1.13587323525567,340.00959005867));
#7648=CARTESIAN_POINT('Ctrl Pts',(182.040302551253,-1.28115213519398,339.976649556123));
#7649=CARTESIAN_POINT('Ctrl Pts',(182.048379294014,-1.42498634838971,339.937387602384));
#7650=CARTESIAN_POINT('Ctrl Pts',(182.056456036775,-1.56682461334312,339.891958829909));
#7651=CARTESIAN_POINT('Ctrl Pts',(182.061860464702,-1.66173350210462,339.861560867026));
#7652=CARTESIAN_POINT('Ctrl Pts',(182.06726489263,-1.75574897728243,339.828402813942));
#7653=CARTESIAN_POINT('Ctrl Pts',(182.072669320557,-1.84870995570134,339.792543381357));
#7654=CARTESIAN_POINT('Ctrl Pts',(182.080740085132,-1.98753430151757,339.73899228546));
#7655=CARTESIAN_POINT('Ctrl Pts',(182.088810849707,-2.12405523137392,339.679395580914));
#7656=CARTESIAN_POINT('Ctrl Pts',(182.096881614282,-2.25774675738525,339.613976608308));
#7657=CARTESIAN_POINT('Ctrl Pts',(182.104950790195,-2.39141196734384,339.548570512877));
#7658=CARTESIAN_POINT('Ctrl Pts',(182.113019966108,-2.52224858781886,339.477344581109));
#7659=CARTESIAN_POINT('Ctrl Pts',(182.121089142021,-2.64975313097116,339.400569157212));
#7660=CARTESIAN_POINT('Ctrl Pts',(182.129158598995,-2.77726211529379,339.323791059115));
#7661=CARTESIAN_POINT('Ctrl Pts',(182.13722805597,-2.90143850497578,339.241463249543));
#7662=CARTESIAN_POINT('Ctrl Pts',(182.145297512944,-3.02180534132847,339.153900942683));
#7663=CARTESIAN_POINT('Ctrl Pts',(182.153366504103,-3.14216522941335,339.066343690424));
#7664=CARTESIAN_POINT('Ctrl Pts',(182.161435495261,-3.25871573730262,338.973552740628));
#7665=CARTESIAN_POINT('Ctrl Pts',(182.16950448642,-3.37101070813753,338.87588536571));
#7666=CARTESIAN_POINT('Ctrl Pts',(182.177575384854,-3.48333222224721,338.778194905056));
#7667=CARTESIAN_POINT('Ctrl Pts',(182.185646283288,-3.59139593957822,338.67562593289));
#7668=CARTESIAN_POINT('Ctrl Pts',(182.193717181722,-3.6947899848816,338.568574999929));
#7669=CARTESIAN_POINT('Ctrl Pts',(182.199150611942,-3.76439615510316,338.496506966996));
#7670=CARTESIAN_POINT('Ctrl Pts',(182.204584042161,-3.83188667994544,338.422408447104));
#7671=CARTESIAN_POINT('Ctrl Pts',(182.21001747238,-3.89714554158373,338.346409596898));
#7672=CARTESIAN_POINT('Ctrl Pts',(182.218340811104,-3.99711399396613,338.229988818981));
#7673=CARTESIAN_POINT('Ctrl Pts',(182.226664149828,-4.09187050337891,338.109076110878));
#7674=CARTESIAN_POINT('Ctrl Pts',(182.234987488552,-4.18103669417411,337.984146900618));
#7675=CARTESIAN_POINT('Ctrl Pts',(182.242803438356,-4.26476733334942,337.866833347875));
#7676=CARTESIAN_POINT('Ctrl Pts',(182.250619388159,-4.34356867268145,337.745978508847));
#7677=CARTESIAN_POINT('Ctrl Pts',(182.258435337963,-4.41716094758247,337.622001091848));
#7678=CARTESIAN_POINT('Ctrl Pts',(181.37007030626,4.28788785758327,332.172095440742));
#7679=CARTESIAN_POINT('Ctrl Pts',(181.328355740759,3.86434819387074,331.529891326477));
#7680=CARTESIAN_POINT('Ctrl Pts',(181.244928279822,2.72375436716049,330.440274865794));
#7681=CARTESIAN_POINT('Ctrl Pts',(181.119787923451,0.473039962656459,329.708131390012));
#7682=CARTESIAN_POINT('Ctrl Pts',(180.99464756708,-1.87184555895904,330.029474338107));
#7683=CARTESIAN_POINT('Ctrl Pts',(180.911220106143,-3.18761322620324,330.899516724865));
#7684=CARTESIAN_POINT('Ctrl Pts',(180.869505540642,-3.7183409627162,331.456418907311));
#7685=CARTESIAN_POINT('Ctrl Pts',(181.558087260742,4.55974375143968,331.992803783117));
#7686=CARTESIAN_POINT('Ctrl Pts',(181.516372695242,4.10935129733558,331.309883358323));
#7687=CARTESIAN_POINT('Ctrl Pts',(181.432945234305,2.89644281021763,330.151184247459));
#7688=CARTESIAN_POINT('Ctrl Pts',(181.307804877934,0.503031115911629,329.372622225845));
#7689=CARTESIAN_POINT('Ctrl Pts',(181.182664521562,-1.99052222786772,329.714338601904));
#7690=CARTESIAN_POINT('Ctrl Pts',(181.099237060626,-3.38971073240211,330.639542447777));
#7691=CARTESIAN_POINT('Ctrl Pts',(181.057522495125,-3.95408707820623,331.231752722606));
#7692=CARTESIAN_POINT('Ctrl Pts',(181.746104215225,4.83159964529608,331.813512125491));
#7693=CARTESIAN_POINT('Ctrl Pts',(181.704389649724,4.35435440080044,331.089875390168));
#7694=CARTESIAN_POINT('Ctrl Pts',(181.620962188788,3.06913125327478,329.862093629124));
#7695=CARTESIAN_POINT('Ctrl Pts',(181.495821832417,0.533022269166806,329.037113061678));
#7696=CARTESIAN_POINT('Ctrl Pts',(181.370681476045,-2.1091988967764,329.399202865703));
#7697=CARTESIAN_POINT('Ctrl Pts',(181.287254015109,-3.59180823860098,330.37956817069));
#7698=CARTESIAN_POINT('Ctrl Pts',(181.245539449608,-4.18983319369624,331.007086537901));
#7699=CARTESIAN_POINT('Ctrl Pts',(181.934121169709,5.1034555391525,331.634220467866));
#7700=CARTESIAN_POINT('Ctrl Pts',(181.892406604207,4.59935750426528,330.869867422015));
#7701=CARTESIAN_POINT('Ctrl Pts',(181.808979143271,3.24181969633193,329.573003010789));
#7702=CARTESIAN_POINT('Ctrl Pts',(181.6838387869,0.563013422421977,328.70160389751));
#7703=CARTESIAN_POINT('Ctrl Pts',(181.558698430529,-2.22787556568508,329.084067129501));
#7704=CARTESIAN_POINT('Ctrl Pts',(181.475270969592,-3.79390574479985,330.119593893603));
#7705=CARTESIAN_POINT('Ctrl Pts',(181.433556404091,-4.42557930918627,330.782420353195));
#7706=CARTESIAN_POINT('',(180.993849537574,-1.82724795145699,330.199232823142));
#7707=CARTESIAN_POINT('Ctrl Pts',(181.433471471437,-4.42539066683718,330.782448221021));
#7708=CARTESIAN_POINT('Ctrl Pts',(181.335375473532,-4.01063179047883,330.638200736283));
#7709=CARTESIAN_POINT('Ctrl Pts',(181.245907584842,-3.58266997347834,330.517361513033));
#7710=CARTESIAN_POINT('Ctrl Pts',(181.096214561382,-2.71608572687693,330.323224835212));
#7711=CARTESIAN_POINT('Ctrl Pts',(181.03528545648,-2.27326928320113,330.248969261106));
#7712=CARTESIAN_POINT('Ctrl Pts',(180.993969721933,-1.82720031248029,330.19937707939));
#7713=CARTESIAN_POINT('',(181.235953224802,2.48747578839151,330.505707534587));
#7714=CARTESIAN_POINT('Ctrl Pts',(181.236066270803,2.48739342482026,330.505858565532));
#7715=CARTESIAN_POINT('Ctrl Pts',(181.329278473347,2.95503192785205,330.630394558558));
#7716=CARTESIAN_POINT('Ctrl Pts',(181.439439013854,3.40978123839685,330.785458718465));
#7717=CARTESIAN_POINT('Ctrl Pts',(181.676346524597,4.28251791449889,331.157496738812));
#7718=CARTESIAN_POINT('Ctrl Pts',(181.805383790547,4.70817800168015,331.378046456073));
#7719=CARTESIAN_POINT('Ctrl Pts',(181.93402621666,5.10326494491035,331.634214435745));
#7720=CARTESIAN_POINT('Ctrl Pts',(180.993842605595,-1.82717158359009,330.199203757019));
#7721=CARTESIAN_POINT('Ctrl Pts',(180.99417094369,-1.82151293100644,330.197050087361));
#7722=CARTESIAN_POINT('Ctrl Pts',(180.994499281784,-1.81585046631374,330.194906420758));
#7723=CARTESIAN_POINT('Ctrl Pts',(180.994827619879,-1.81018422265156,330.192772769822));
#7724=CARTESIAN_POINT('Ctrl Pts',(181.002908535245,-1.67072908100198,330.140260274553));
#7725=CARTESIAN_POINT('Ctrl Pts',(181.010989450612,-1.52897030831888,330.093813700451));
#7726=CARTESIAN_POINT('Ctrl Pts',(181.019070365978,-1.38545129924182,330.05361493008));
#7727=CARTESIAN_POINT('Ctrl Pts',(181.027478360995,-1.23612327655373,330.011789091589));
#7728=CARTESIAN_POINT('Ctrl Pts',(181.035886356013,-1.08488989577882,329.97672753868));
#7729=CARTESIAN_POINT('Ctrl Pts',(181.04429435103,-0.932379817120784,329.948577582589));
#7730=CARTESIAN_POINT('Ctrl Pts',(181.052374953363,-0.785808215333428,329.921523736765));
#7731=CARTESIAN_POINT('Ctrl Pts',(181.060455555697,-0.638057813713283,329.900853427042));
#7732=CARTESIAN_POINT('Ctrl Pts',(181.06853615803,-0.489696403519162,329.886645133097));
#7733=CARTESIAN_POINT('Ctrl Pts',(181.076616788472,-0.341334477244848,329.872436789728));
#7734=CARTESIAN_POINT('Ctrl Pts',(181.084697418914,-0.192361865645472,329.864690534929));
#7735=CARTESIAN_POINT('Ctrl Pts',(181.092778049357,-0.0433509756674483,
329.863432930895));
#7736=CARTESIAN_POINT('Ctrl Pts',(181.10086036639,0.105691015909345,329.862175064374));
#7737=CARTESIAN_POINT('Ctrl Pts',(181.108942683424,0.254770973150995,329.867408554713));
#7738=CARTESIAN_POINT('Ctrl Pts',(181.117025000458,0.403316444216384,329.879107850352));
#7739=CARTESIAN_POINT('Ctrl Pts',(181.1180054357,0.421335932225548,329.880527047558));
#7740=CARTESIAN_POINT('Ctrl Pts',(181.118985870942,0.439347559076759,329.882041327492));
#7741=CARTESIAN_POINT('Ctrl Pts',(181.119966306184,0.457350306861083,329.88365059253));
#7742=CARTESIAN_POINT('Ctrl Pts',(181.128037500542,0.605553543663938,329.89689847504));
#7743=CARTESIAN_POINT('Ctrl Pts',(181.1361086949,0.753208183541544,329.91659254913));
#7744=CARTESIAN_POINT('Ctrl Pts',(181.144179889258,0.899747050476711,329.942663170437));
#7745=CARTESIAN_POINT('Ctrl Pts',(181.152250191989,1.0462697292173,329.968730911714));
#7746=CARTESIAN_POINT('Ctrl Pts',(181.160320494719,1.19167655492713,330.001173740569));
#7747=CARTESIAN_POINT('Ctrl Pts',(181.16839079745,1.3354088573094,330.039870591777));
#7748=CARTESIAN_POINT('Ctrl Pts',(181.176459923976,1.47912021145519,330.07856180312));
#7749=CARTESIAN_POINT('Ctrl Pts',(181.184529050502,1.62115721050249,330.123505130563));
#7750=CARTESIAN_POINT('Ctrl Pts',(181.192598177028,1.76097459482369,330.174529138117));
#7751=CARTESIAN_POINT('Ctrl Pts',(181.200668287031,1.90080902029365,330.225559364551));
#7752=CARTESIAN_POINT('Ctrl Pts',(181.208738397034,2.038422979052,330.282671640769));
#7753=CARTESIAN_POINT('Ctrl Pts',(181.216808507037,2.17328891739442,330.345645496524));
#7754=CARTESIAN_POINT('Ctrl Pts',(181.223180833583,2.27978186467651,330.395370961556));
#7755=CARTESIAN_POINT('Ctrl Pts',(181.22955316013,2.38456171924082,330.448750140761));
#7756=CARTESIAN_POINT('Ctrl Pts',(181.235925486676,2.48737852733284,330.505653704457));
#7757=CARTESIAN_POINT('Ctrl Pts',(180.751352012451,-3.51522511306203,339.536198064046));
#7758=CARTESIAN_POINT('Ctrl Pts',(180.712625990112,-2.88450494225346,340.024960537033));
#7759=CARTESIAN_POINT('Ctrl Pts',(180.622265271322,-1.17144813710853,340.854840788682));
#7760=CARTESIAN_POINT('Ctrl Pts',(180.531904552531,0.760780206681846,340.786796970132));
#7761=CARTESIAN_POINT('Ctrl Pts',(180.48026985608,1.77266279316809,340.458165176456));
#7762=CARTESIAN_POINT('Ctrl Pts',(180.82341369046,-3.59167846941827,339.634856771792));
#7763=CARTESIAN_POINT('Ctrl Pts',(180.784687668121,-2.94724063546469,340.134249440661));
#7764=CARTESIAN_POINT('Ctrl Pts',(180.694326949331,-1.19692620437268,340.98217892915));
#7765=CARTESIAN_POINT('Ctrl Pts',(180.60396623054,0.777326572385168,340.91265521155));
#7766=CARTESIAN_POINT('Ctrl Pts',(180.552331534089,1.81121680204847,340.576875937179));
#7767=CARTESIAN_POINT('Ctrl Pts',(180.895475368468,-3.66813182577451,339.733515479539));
#7768=CARTESIAN_POINT('Ctrl Pts',(180.85674934613,-3.00997632867591,340.24353834429));
#7769=CARTESIAN_POINT('Ctrl Pts',(180.766388627339,-1.22240427163682,341.109517069619));
#7770=CARTESIAN_POINT('Ctrl Pts',(180.676027908549,0.79387293808849,341.038513452968));
#7771=CARTESIAN_POINT('Ctrl Pts',(180.624393212098,1.84977081092886,340.695586697903));
#7772=CARTESIAN_POINT('Ctrl Pts',(180.967537046477,-3.74458518213076,339.832174187285));
#7773=CARTESIAN_POINT('Ctrl Pts',(180.928811024139,-3.07271202188714,340.352827247918));
#7774=CARTESIAN_POINT('Ctrl Pts',(180.838450305348,-1.24788233890097,341.236855210088));
#7775=CARTESIAN_POINT('Ctrl Pts',(180.748089586558,0.810419303791811,341.164371694386));
#7776=CARTESIAN_POINT('Ctrl Pts',(180.696454890107,1.88832481980924,340.814297458627));
#7777=CARTESIAN_POINT('Ctrl Pts',(180.696529438166,-2.55854249889813,340.136670690217));
#7778=CARTESIAN_POINT('Ctrl Pts',(180.73617790029,-2.7597370763773,340.0944890875));
#7779=CARTESIAN_POINT('Ctrl Pts',(180.778964893207,-2.95961823467644,340.047992945047));
#7780=CARTESIAN_POINT('Ctrl Pts',(180.869583792205,-3.35496090197214,339.94657615533));
#7781=CARTESIAN_POINT('Ctrl Pts',(180.917495527076,-3.55084795862925,339.891574190277));
#7782=CARTESIAN_POINT('Ctrl Pts',(180.967537046477,-3.74458518213073,339.832174187285));
#7783=CARTESIAN_POINT('Ctrl Pts',(181.135238634734,-4.11718022388969,339.518921605947));
#7784=CARTESIAN_POINT('Ctrl Pts',(181.073326230095,-3.11267730650807,340.434139400932));
#7785=CARTESIAN_POINT('Ctrl Pts',(180.949524158232,-0.47430519230716,341.565277535024));
#7786=CARTESIAN_POINT('Ctrl Pts',(180.825722086368,2.29912071323036,340.825045741512));
#7787=CARTESIAN_POINT('Ctrl Pts',(180.763832419144,3.42440815596409,340.064114369154));
#7788=CARTESIAN_POINT('Ctrl Pts',(181.323574328469,-3.89748481312009,339.277789014107));
#7789=CARTESIAN_POINT('Ctrl Pts',(181.261661923831,-2.94658282381369,340.144170193138));
#7790=CARTESIAN_POINT('Ctrl Pts',(181.137859851967,-0.448995959194304,341.214950061744));
#7791=CARTESIAN_POINT('Ctrl Pts',(181.014057780104,2.17643813874135,340.514217517499));
#7792=CARTESIAN_POINT('Ctrl Pts',(180.952168112879,3.24167951268005,339.793889937379));
#7793=CARTESIAN_POINT('Ctrl Pts',(181.511910022206,-3.6777894023505,339.036656422269));
#7794=CARTESIAN_POINT('Ctrl Pts',(181.449997617566,-2.78048834111931,339.854200985343));
#7795=CARTESIAN_POINT('Ctrl Pts',(181.326195545702,-0.423686726081443,340.864622588464));
#7796=CARTESIAN_POINT('Ctrl Pts',(181.202393473839,2.05375556425234,340.203389293486));
#7797=CARTESIAN_POINT('Ctrl Pts',(181.140503806615,3.05895086939599,339.523665505604));
#7798=CARTESIAN_POINT('Ctrl Pts',(181.700245715941,-3.45809399158091,338.795523830431));
#7799=CARTESIAN_POINT('Ctrl Pts',(181.638333311301,-2.61439385842493,339.564231777549));
#7800=CARTESIAN_POINT('Ctrl Pts',(181.514531239438,-0.398377492968587,340.514295115184));
#7801=CARTESIAN_POINT('Ctrl Pts',(181.390729167575,1.93107298976333,339.892561069473));
#7802=CARTESIAN_POINT('Ctrl Pts',(181.328839500351,2.87622222611195,339.253441073828));
#7803=CARTESIAN_POINT('',(181.337571198602,2.72350574788935,339.355309059494));
#7804=CARTESIAN_POINT('Ctrl Pts',(181.337515959362,2.723475111057,339.355310357786));
#7805=CARTESIAN_POINT('Ctrl Pts',(181.241203275559,2.82033438186087,339.490333974197));
#7806=CARTESIAN_POINT('Ctrl Pts',(181.144706554227,2.92995105049118,339.616169622604));
#7807=CARTESIAN_POINT('Ctrl Pts',(180.953497167844,3.16562337980582,339.851156463483));
#7808=CARTESIAN_POINT('Ctrl Pts',(180.85798168447,3.2926517407027,339.961263535214));
#7809=CARTESIAN_POINT('Ctrl Pts',(180.763832419144,3.4244081559647,340.064114369153));
#7810=CARTESIAN_POINT('',(181.698952960354,-3.45859239216069,338.797938813013));
#7811=CARTESIAN_POINT('Ctrl Pts',(181.698952960354,-3.45859239215945,338.797938813014));
#7812=CARTESIAN_POINT('Ctrl Pts',(181.690923324486,-3.349099573853,338.897648431055));
#7813=CARTESIAN_POINT('Ctrl Pts',(181.682893688618,-3.23526892443982,338.99264087084));
#7814=CARTESIAN_POINT('Ctrl Pts',(181.674864052751,-3.11753099767851,339.082548351338));
#7815=CARTESIAN_POINT('Ctrl Pts',(181.666835946353,-2.99981549741501,339.172438706429));
#7816=CARTESIAN_POINT('Ctrl Pts',(181.658807839955,-2.87819447181031,339.257245829385));
#7817=CARTESIAN_POINT('Ctrl Pts',(181.650779733557,-2.75313052873629,339.336643039753));
#7818=CARTESIAN_POINT('Ctrl Pts',(181.642752285051,-2.62807683447564,339.416033743633));
#7819=CARTESIAN_POINT('Ctrl Pts',(181.634724836545,-2.49958107022608,339.49001523899));
#7820=CARTESIAN_POINT('Ctrl Pts',(181.626697388039,-2.3681339250979,339.558304758932));
#7821=CARTESIAN_POINT('Ctrl Pts',(181.618669726312,-2.23668328853949,339.626596092744));
#7822=CARTESIAN_POINT('Ctrl Pts',(181.610642064586,-2.10228141428578,339.689194995255));
#7823=CARTESIAN_POINT('Ctrl Pts',(181.602614402859,-1.96544285195621,339.745865037924));
#7824=CARTESIAN_POINT('Ctrl Pts',(181.594583330202,-1.82854614732993,339.802559159526));
#7825=CARTESIAN_POINT('Ctrl Pts',(181.586552257546,-1.68921099663222,339.853319256526));
#7826=CARTESIAN_POINT('Ctrl Pts',(181.57852118489,-1.54797184628561,339.897957097159));
#7827=CARTESIAN_POINT('Ctrl Pts',(181.570488744678,-1.40670864529598,339.942602538862));
#7828=CARTESIAN_POINT('Ctrl Pts',(181.562456304465,-1.26354112110727,339.981123548396));
#7829=CARTESIAN_POINT('Ctrl Pts',(181.554423864253,-1.11901844459552,340.013381920735));
#7830=CARTESIAN_POINT('Ctrl Pts',(181.54638628216,-0.974403253435857,340.045660942927));
#7831=CARTESIAN_POINT('Ctrl Pts',(181.538348700066,-0.828431506451216,340.071669246487));
#7832=CARTESIAN_POINT('Ctrl Pts',(181.530311117973,-0.681662966543317,340.091319687718));
#7833=CARTESIAN_POINT('Ctrl Pts',(181.524635398209,-0.578022705946049,340.105195800754));
#7834=CARTESIAN_POINT('Ctrl Pts',(181.518959678445,-0.473985336372291,340.115902674231));
#7835=CARTESIAN_POINT('Ctrl Pts',(181.513283958681,-0.369749448980302,340.123425212441));
#7836=CARTESIAN_POINT('Ctrl Pts',(181.505278951843,-0.22273567346082,340.134034962801));
#7837=CARTESIAN_POINT('Ctrl Pts',(181.497273945005,-0.0751969877806426,
340.138317571497));
#7838=CARTESIAN_POINT('Ctrl Pts',(181.489268938167,0.072306158600289,340.136241075137));
#7839=CARTESIAN_POINT('Ctrl Pts',(181.481267916047,0.219735881144422,340.134165612412));
#7840=CARTESIAN_POINT('Ctrl Pts',(181.473266893926,0.367129758108576,340.125737359625));
#7841=CARTESIAN_POINT('Ctrl Pts',(181.465265871806,0.513926528021877,340.110976431788));
#7842=CARTESIAN_POINT('Ctrl Pts',(181.45726784588,0.660668325990168,340.096221031572));
#7843=CARTESIAN_POINT('Ctrl Pts',(181.449269819954,0.806813122657021,340.075137718697));
#7844=CARTESIAN_POINT('Ctrl Pts',(181.441271794028,0.951803762915764,340.047798545841));
#7845=CARTESIAN_POINT('Ctrl Pts',(181.433275778068,1.0967579659101,340.02046624353));
#7846=CARTESIAN_POINT('Ctrl Pts',(181.425279762108,1.2405582549564,339.986881280004));
#7847=CARTESIAN_POINT('Ctrl Pts',(181.417283746148,1.38265646389062,339.94716703431));
#7848=CARTESIAN_POINT('Ctrl Pts',(181.409287738572,1.52475452381916,339.907452830261));
#7849=CARTESIAN_POINT('Ctrl Pts',(181.401291730997,1.66515017650093,339.861609444636));
#7850=CARTESIAN_POINT('Ctrl Pts',(181.393295723421,1.8033088432631,339.809810576136));
#7851=CARTESIAN_POINT('Ctrl Pts',(181.385300004087,1.94146252965741,339.75801357489));
#7852=CARTESIAN_POINT('Ctrl Pts',(181.377304284753,2.07737907176908,339.700261642185));
#7853=CARTESIAN_POINT('Ctrl Pts',(181.369308565419,2.21054241446942,339.636777199341));
#7854=CARTESIAN_POINT('Ctrl Pts',(181.361310820325,2.34373949485135,339.573276672357));
#7855=CARTESIAN_POINT('Ctrl Pts',(181.35331307523,2.4741816741913,339.504040882687));
#7856=CARTESIAN_POINT('Ctrl Pts',(181.345315330136,2.60137568129605,339.429339129855));
#7857=CARTESIAN_POINT('Ctrl Pts',(181.342733952958,2.64242921616399,339.405228158871));
#7858=CARTESIAN_POINT('Ctrl Pts',(181.34015257578,2.68314456862808,339.380548118814));
#7859=CARTESIAN_POINT('Ctrl Pts',(181.337571198602,2.72350574788935,339.355309059494));
#7860=CARTESIAN_POINT('Ctrl Pts',(181.127180420915,-3.98468371561092,339.636058369257));
#7861=CARTESIAN_POINT('Ctrl Pts',(181.229310902963,-3.86352131576755,339.506182820355));
#7862=CARTESIAN_POINT('Ctrl Pts',(181.332333550813,-3.75334228949432,339.366387183163));
#7863=CARTESIAN_POINT('Ctrl Pts',(181.524375317495,-3.5785839673492,339.083778531583));
#7864=CARTESIAN_POINT('Ctrl Pts',(181.612373862498,-3.51097495739658,338.945369027672));
#7865=CARTESIAN_POINT('Ctrl Pts',(181.698952960354,-3.45859239216168,338.797938813012));
#7866=CARTESIAN_POINT('Origin',(175.231676812499,0.,335.));
#7867=CARTESIAN_POINT('',(167.731676812499,-45.,335.));
#7868=CARTESIAN_POINT('Origin',(175.231676812499,-45.,335.));
#7869=CARTESIAN_POINT('',(167.731676812499,-6.,335.));
#7870=CARTESIAN_POINT('',(167.731676812499,0.,335.));
#7871=CARTESIAN_POINT('',(170.731676812499,-4.5102810375397E-15,341.));
#7872=CARTESIAN_POINT('Ctrl Pts',(167.731676812499,-6.,335.));
#7873=CARTESIAN_POINT('Ctrl Pts',(167.731676812499,-6.,335.794780989626));
#7874=CARTESIAN_POINT('Ctrl Pts',(167.867335546256,-5.8328999714949,336.617370842401));
#7875=CARTESIAN_POINT('Ctrl Pts',(168.353029590474,-5.20624497170395,338.087656141906));
#7876=CARTESIAN_POINT('Ctrl Pts',(168.700147512561,-4.74828751391861,338.73699386032));
#7877=CARTESIAN_POINT('Ctrl Pts',(169.405023834711,-3.7207625323499,339.764518841889));
#7878=CARTESIAN_POINT('Ctrl Pts',(169.821017677781,-3.07201535485506,340.213611135601));
#7879=CARTESIAN_POINT('Ctrl Pts',(170.323412633441,-1.98596758305952,340.675445953647));
#7880=CARTESIAN_POINT('Ctrl Pts',(170.469308053014,-1.60462674459781,340.795420777217));
#7881=CARTESIAN_POINT('Ctrl Pts',(170.67398081842,-0.816861849349986,340.957723184693));
#7882=CARTESIAN_POINT('Ctrl Pts',(170.731676812499,-0.410146780646359,341.));
#7883=CARTESIAN_POINT('Ctrl Pts',(170.731676812499,-2.63677968348475E-15,
341.));
#7884=CARTESIAN_POINT('',(167.731676812499,6.,335.));
#7885=CARTESIAN_POINT('Ctrl Pts',(170.731676812499,4.02455846426619E-15,
341.));
#7886=CARTESIAN_POINT('Ctrl Pts',(170.731676812499,0.410146780646362,341.));
#7887=CARTESIAN_POINT('Ctrl Pts',(170.67398081842,0.816861849349989,340.957723184693));
#7888=CARTESIAN_POINT('Ctrl Pts',(170.469308053014,1.60462674459781,340.795420777217));
#7889=CARTESIAN_POINT('Ctrl Pts',(170.323412633441,1.98596758305952,340.675445953647));
#7890=CARTESIAN_POINT('Ctrl Pts',(169.821017677781,3.07201535485507,340.213611135601));
#7891=CARTESIAN_POINT('Ctrl Pts',(169.405023834711,3.7207625323499,339.764518841889));
#7892=CARTESIAN_POINT('Ctrl Pts',(168.700147512561,4.74828751391861,338.73699386032));
#7893=CARTESIAN_POINT('Ctrl Pts',(168.353029590474,5.20624497170395,338.087656141906));
#7894=CARTESIAN_POINT('Ctrl Pts',(167.867335546256,5.8328999714949,336.617370842401));
#7895=CARTESIAN_POINT('Ctrl Pts',(167.731676812499,6.,335.794780989626));
#7896=CARTESIAN_POINT('Ctrl Pts',(167.731676812499,6.,335.));
#7897=CARTESIAN_POINT('',(167.731676812499,45.,335.));
#7898=CARTESIAN_POINT('',(167.731676812499,0.,335.));
#7899=CARTESIAN_POINT('Origin',(175.231676812499,45.,335.));
#7900=CARTESIAN_POINT('Ctrl Pts',(167.731676812499,6.00000000000001,335.));
#7901=CARTESIAN_POINT('Ctrl Pts',(167.731676812499,6.00000000000001,334.205219010374));
#7902=CARTESIAN_POINT('Ctrl Pts',(167.867335546256,5.8328999714949,333.382629157599));
#7903=CARTESIAN_POINT('Ctrl Pts',(168.353029590474,5.20624497170395,331.912343858094));
#7904=CARTESIAN_POINT('Ctrl Pts',(168.700147512561,4.74828751391861,331.26300613968));
#7905=CARTESIAN_POINT('Ctrl Pts',(169.405023834711,3.7207625323499,330.235481158111));
#7906=CARTESIAN_POINT('Ctrl Pts',(169.821017677781,3.07201535485507,329.786388864399));
#7907=CARTESIAN_POINT('Ctrl Pts',(170.323412633441,1.98596758305952,329.324554046353));
#7908=CARTESIAN_POINT('Ctrl Pts',(170.469308053014,1.60462674459781,329.204579222783));
#7909=CARTESIAN_POINT('Ctrl Pts',(170.67398081842,0.816861849349989,329.042276815307));
#7910=CARTESIAN_POINT('Ctrl Pts',(170.731676812499,0.410146780646358,329.));
#7911=CARTESIAN_POINT('Ctrl Pts',(170.731676812499,-0.410146780646357,329.));
#7912=CARTESIAN_POINT('Ctrl Pts',(170.67398081842,-0.816861849349986,329.042276815307));
#7913=CARTESIAN_POINT('Ctrl Pts',(170.469308053014,-1.60462674459781,329.204579222783));
#7914=CARTESIAN_POINT('Ctrl Pts',(170.323412633441,-1.98596758305952,329.324554046353));
#7915=CARTESIAN_POINT('Ctrl Pts',(169.821017677781,-3.07201535485506,329.786388864399));
#7916=CARTESIAN_POINT('Ctrl Pts',(169.405023834711,-3.7207625323499,330.235481158111));
#7917=CARTESIAN_POINT('Ctrl Pts',(168.700147512561,-4.74828751391861,331.26300613968));
#7918=CARTESIAN_POINT('Ctrl Pts',(168.353029590474,-5.20624497170395,331.912343858094));
#7919=CARTESIAN_POINT('Ctrl Pts',(167.867335546256,-5.8328999714949,333.382629157599));
#7920=CARTESIAN_POINT('Ctrl Pts',(167.731676812499,-6.,334.205219010374));
#7921=CARTESIAN_POINT('Ctrl Pts',(167.731676812499,-6.,335.));
#7922=CARTESIAN_POINT('Ctrl Pts',(181.698952960354,-3.45859239216063,338.797938813013));
#7923=CARTESIAN_POINT('Ctrl Pts',(181.730827803918,-3.51819566196673,338.74366110459));
#7924=CARTESIAN_POINT('Ctrl Pts',(181.762380948322,-3.57609877279402,338.688362743726));
#7925=CARTESIAN_POINT('Ctrl Pts',(181.953767151073,-3.92184589325217,338.342615623268));
#7926=CARTESIAN_POINT('Ctrl Pts',(182.11679605996,-4.1918704925973,338.001551728627));
#7927=CARTESIAN_POINT('Ctrl Pts',(182.258446931496,-4.41720487047243,337.621927095625));
#7928=CARTESIAN_POINT('Ctrl Pts',(180.993849537574,-1.82724795145699,330.199232823142));
#7929=CARTESIAN_POINT('Ctrl Pts',(180.810080956896,-1.24773913194053,329.978662596696));
#7930=CARTESIAN_POINT('Ctrl Pts',(180.696454890107,-0.616939978405845,329.86325));
#7931=CARTESIAN_POINT('Ctrl Pts',(180.696454890107,0.678169718332449,329.86325));
#7932=CARTESIAN_POINT('Ctrl Pts',(180.835357252731,1.37227470332214,330.003511731902));
#7933=CARTESIAN_POINT('Ctrl Pts',(181.108046445603,2.16628886234032,330.338816012577));
#7934=CARTESIAN_POINT('Ctrl Pts',(181.170594782469,2.32971338705471,330.418390085475));
#7935=CARTESIAN_POINT('Ctrl Pts',(181.235953224802,2.48747578839151,330.505707534587));
#7936=CARTESIAN_POINT('Ctrl Pts',(181.756465142864,3.56497732371045,338.698261381234));
#7937=CARTESIAN_POINT('Ctrl Pts',(181.620014599316,3.31523915334618,338.938999074555));
#7938=CARTESIAN_POINT('Ctrl Pts',(181.475233027865,3.03225184044892,339.162240449674));
#7939=CARTESIAN_POINT('Ctrl Pts',(181.337518659071,2.72350972420708,339.355306572981));
#7940=CARTESIAN_POINT('Origin',(185.231676812499,0.,335.));
#7941=CARTESIAN_POINT('Origin',(185.231676812499,0.,335.));
#7942=CARTESIAN_POINT('Origin',(185.231676812499,0.,335.));
#7943=CARTESIAN_POINT('',(165.231676812499,-6.,335.));
#7944=CARTESIAN_POINT('',(185.231676812499,-6.,335.));
#7945=CARTESIAN_POINT('Origin',(165.231676812499,0.,335.));
#7946=CARTESIAN_POINT('Origin',(175.231676812499,-45.,335.));
#7947=CARTESIAN_POINT('',(185.231676812499,-45.,345.));
#7948=CARTESIAN_POINT('',(165.231676812499,-45.,345.));
#7949=CARTESIAN_POINT('',(185.231676812499,-45.,345.));
#7950=CARTESIAN_POINT('',(165.231676812499,-45.,325.));
#7951=CARTESIAN_POINT('',(165.231676812499,-45.,345.));
#7952=CARTESIAN_POINT('',(185.231676812499,-45.,325.));
#7953=CARTESIAN_POINT('',(165.231676812499,-45.,325.));
#7954=CARTESIAN_POINT('',(185.231676812499,-45.,325.));
#7955=CARTESIAN_POINT('Origin',(165.231676812499,0.,325.));
#7956=CARTESIAN_POINT('',(165.231676812499,45.,345.));
#7957=CARTESIAN_POINT('',(165.231676812499,0.,345.));
#7958=CARTESIAN_POINT('',(165.231676812499,45.,325.));
#7959=CARTESIAN_POINT('',(165.231676812499,45.,345.));
#7960=CARTESIAN_POINT('',(165.231676812499,0.,325.));
#7961=CARTESIAN_POINT('Origin',(185.231676812499,0.,325.));
#7962=CARTESIAN_POINT('',(185.231676812499,45.,325.));
#7963=CARTESIAN_POINT('',(165.231676812499,45.,325.));
#7964=CARTESIAN_POINT('',(185.231676812499,0.,325.));
#7965=CARTESIAN_POINT('Origin',(185.231676812499,0.,345.));
#7966=CARTESIAN_POINT('',(185.231676812499,45.,345.));
#7967=CARTESIAN_POINT('',(185.231676812499,45.,325.));
#7968=CARTESIAN_POINT('',(185.231676812499,0.,345.));
#7969=CARTESIAN_POINT('Origin',(165.231676812499,0.,345.));
#7970=CARTESIAN_POINT('',(185.231676812499,45.,345.));
#7971=CARTESIAN_POINT('Origin',(175.231676812499,45.,335.));
#7972=CARTESIAN_POINT('',(0.,0.,0.));
#7973=CARTESIAN_POINT('Origin',(175.231676812499,-118.,15.));
#7974=CARTESIAN_POINT('',(167.731676812499,-118.,15.));
#7975=CARTESIAN_POINT('Origin',(175.231676812499,-118.,15.));
#7976=CARTESIAN_POINT('Origin',(175.231676812499,0.,15.));
#7977=CARTESIAN_POINT('',(167.731676812499,118.,15.));
#7978=CARTESIAN_POINT('Origin',(175.231676812499,118.,15.));
#7979=CARTESIAN_POINT('',(167.731676812499,0.,15.));
#7980=CARTESIAN_POINT('Origin',(175.231676812499,118.,15.));
#7981=CARTESIAN_POINT('',(0.,0.,0.));
#7982=CARTESIAN_POINT('Origin',(185.231676812499,0.,335.));
#7983=CARTESIAN_POINT('',(184.668301620265,-5.91674928609117,334.997093448832));
#7984=CARTESIAN_POINT('',(185.231456596324,2.58392919827197,329.677290120548));
#7985=CARTESIAN_POINT('Ctrl Pts',(184.668301620294,-5.91674928609086,334.99709344821));
#7986=CARTESIAN_POINT('Ctrl Pts',(184.677270719926,-5.91665612605423,334.807451349904));
#7987=CARTESIAN_POINT('Ctrl Pts',(184.686239819557,-5.90744612029556,334.618059773088));
#7988=CARTESIAN_POINT('Ctrl Pts',(184.695208919188,-5.88918696321264,334.429555020334));
#7989=CARTESIAN_POINT('Ctrl Pts',(184.702645229547,-5.874048235298,334.273265102371));
#7990=CARTESIAN_POINT('Ctrl Pts',(184.710081539905,-5.85266154708832,334.117349686397));
#7991=CARTESIAN_POINT('Ctrl Pts',(184.717517850264,-5.82504996052314,333.962347110104));
#7992=CARTESIAN_POINT('Ctrl Pts',(184.724945525487,-5.7974704368756,333.80752452473));
#7993=CARTESIAN_POINT('Ctrl Pts',(184.732373200709,-5.76368046885996,333.653613031502));
#7994=CARTESIAN_POINT('Ctrl Pts',(184.739800875932,-5.72375497841269,333.501147268877));
#7995=CARTESIAN_POINT('Ctrl Pts',(184.747221528956,-5.68386723392797,333.348825648926));
#7996=CARTESIAN_POINT('Ctrl Pts',(184.754642181979,-5.63785560932689,333.197947395628));
#7997=CARTESIAN_POINT('Ctrl Pts',(184.762062835003,-5.58584629808054,333.049038263645));
#7998=CARTESIAN_POINT('Ctrl Pts',(184.769478073325,-5.53387493698251,332.900237787662));
#7999=CARTESIAN_POINT('Ctrl Pts',(184.776893311648,-5.47591472598483,332.753403921355));
#8000=CARTESIAN_POINT('Ctrl Pts',(184.78430854997,-5.41214201488629,332.609048437713));
#8001=CARTESIAN_POINT('Ctrl Pts',(184.791719976858,-5.34840208297505,332.46476715282));
#8002=CARTESIAN_POINT('Ctrl Pts',(184.799131403747,-5.27885575128642,332.322962052588));
#8003=CARTESIAN_POINT('Ctrl Pts',(184.806542830635,-5.20372789585258,332.184125970782));
#8004=CARTESIAN_POINT('Ctrl Pts',(184.813953122964,-5.12861154117879,332.04531114235));
#8005=CARTESIAN_POINT('Ctrl Pts',(184.821363415292,-5.0479155349489,331.909464757111));
#8006=CARTESIAN_POINT('Ctrl Pts',(184.828773707621,-4.96191127327889,331.777056147152));
#8007=CARTESIAN_POINT('Ctrl Pts',(184.836183730803,-4.87591013534358,331.644652346367));
#8008=CARTESIAN_POINT('Ctrl Pts',(184.843593753985,-4.78460132776732,331.515686384364));
#8009=CARTESIAN_POINT('Ctrl Pts',(184.851003777167,-4.68830011228147,331.390599409918));
#8010=CARTESIAN_POINT('Ctrl Pts',(184.858414979188,-4.59198357650121,331.265492535732));
#8011=CARTESIAN_POINT('Ctrl Pts',(184.86582618121,-4.49067327807438,331.14426617247));
#8012=CARTESIAN_POINT('Ctrl Pts',(184.873237383232,-4.38472528255571,331.027329014502));
#8013=CARTESIAN_POINT('Ctrl Pts',(184.880651212497,-4.27873972888114,330.910350402762));
#8014=CARTESIAN_POINT('Ctrl Pts',(184.888065041761,-4.16811345401209,330.79766429917));
#8015=CARTESIAN_POINT('Ctrl Pts',(184.895478871026,-4.05323984033218,330.689643012552));
#8016=CARTESIAN_POINT('Ctrl Pts',(184.902900803344,-3.93824067383906,330.581503662472));
#8017=CARTESIAN_POINT('Ctrl Pts',(184.910322735663,-3.81898516866113,330.478039566256));
#8018=CARTESIAN_POINT('Ctrl Pts',(184.917744667982,-3.69590085340995,330.379583628691));
#8019=CARTESIAN_POINT('Ctrl Pts',(184.92517116989,-3.57274075670458,330.281067073052));
#8020=CARTESIAN_POINT('Ctrl Pts',(184.932597671799,-3.44574745087061,330.187565040681));
#8021=CARTESIAN_POINT('Ctrl Pts',(184.940024173707,-3.31537756949373,330.099367170028));
#8022=CARTESIAN_POINT('Ctrl Pts',(184.947461126786,-3.18482422114322,330.011045180244));
#8023=CARTESIAN_POINT('Ctrl Pts',(184.954898079865,-3.05088512199134,329.928042455675));
#8024=CARTESIAN_POINT('Ctrl Pts',(184.962335032943,-2.91404232556548,329.850603153056));
#8025=CARTESIAN_POINT('Ctrl Pts',(184.96603900645,-2.84588778872343,329.812034518527));
#8026=CARTESIAN_POINT('Ctrl Pts',(184.969742979957,-2.77701331258672,329.774845169973));
#8027=CARTESIAN_POINT('Ctrl Pts',(184.973446953464,-2.70748021779954,329.739060784164));
#8028=CARTESIAN_POINT('Ctrl Pts',(184.98073525764,-2.57066003154614,329.668647891621));
#8029=CARTESIAN_POINT('Ctrl Pts',(184.988023561816,-2.43084361068165,329.603448846054));
#8030=CARTESIAN_POINT('Ctrl Pts',(184.995311865992,-2.28847483920939,329.543736308351));
#8031=CARTESIAN_POINT('Ctrl Pts',(185.002591396468,-2.14627745203645,329.484095652925));
#8032=CARTESIAN_POINT('Ctrl Pts',(185.009870926944,-2.00153417916713,329.429928515966));
#8033=CARTESIAN_POINT('Ctrl Pts',(185.01715045742,-1.85471492012095,329.381462545503));
#8034=CARTESIAN_POINT('Ctrl Pts',(185.02442294338,-1.70803774036211,329.333043476316));
#8035=CARTESIAN_POINT('Ctrl Pts',(185.031695429341,-1.55928893643624,329.290314718072));
#8036=CARTESIAN_POINT('Ctrl Pts',(185.038967915301,-1.40895960607995,329.253456396151));
#8037=CARTESIAN_POINT('Ctrl Pts',(185.04623507784,-1.25874031602008,329.216625054333));
#8038=CARTESIAN_POINT('Ctrl Pts',(185.053502240378,-1.10694317641211,329.185655689977));
#8039=CARTESIAN_POINT('Ctrl Pts',(185.060769402916,-0.954075423499419,329.160678922274));
#8040=CARTESIAN_POINT('Ctrl Pts',(185.06803359087,-0.801270242198636,329.135712378027));
#8041=CARTESIAN_POINT('Ctrl Pts',(185.075297778823,-0.647395700591261,329.116733615813));
#8042=CARTESIAN_POINT('Ctrl Pts',(185.082561966777,-0.492970065631674,329.103822333334));
#8043=CARTESIAN_POINT('Ctrl Pts',(185.089824724367,-0.338574838026922,329.090913593166));
#8044=CARTESIAN_POINT('Ctrl Pts',(185.097087481958,-0.18362911891612,329.084069989377));
#8045=CARTESIAN_POINT('Ctrl Pts',(185.104350239548,-0.0286568052247463,
329.083319397668));
#8046=CARTESIAN_POINT('Ctrl Pts',(185.111613114984,0.126318023040366,329.082568793779));
#8047=CARTESIAN_POINT('Ctrl Pts',(185.118875990419,0.2813190590681,329.08791140062));
#8048=CARTESIAN_POINT('Ctrl Pts',(185.126138865855,0.435822242651817,329.099322959583));
#8049=CARTESIAN_POINT('Ctrl Pts',(185.133403407354,0.590360868423202,329.110737136295));
#8050=CARTESIAN_POINT('Ctrl Pts',(185.140667948854,0.744401028100145,329.128223005766));
#8051=CARTESIAN_POINT('Ctrl Pts',(185.147932490353,0.897423966635176,329.151704454577));
#8052=CARTESIAN_POINT('Ctrl Pts',(185.155204498544,1.05060418625961,329.175210038254));
#8053=CARTESIAN_POINT('Ctrl Pts',(185.162476506734,1.20276471325446,329.204723448796));
#8054=CARTESIAN_POINT('Ctrl Pts',(185.169748514925,1.35339661489844,329.240117347959));
#8055=CARTESIAN_POINT('Ctrl Pts',(185.177024411585,1.50410906204926,329.275530172858));
#8056=CARTESIAN_POINT('Ctrl Pts',(185.184300308246,1.65329088351919,329.316829643947));
#8057=CARTESIAN_POINT('Ctrl Pts',(185.191576204906,1.80044935259379,329.363838833812));
#8058=CARTESIAN_POINT('Ctrl Pts',(185.198863103485,1.94783034071153,329.410919106504));
#8059=CARTESIAN_POINT('Ctrl Pts',(185.206150002065,2.09318150212912,329.463726209755));
#8060=CARTESIAN_POINT('Ctrl Pts',(185.213436900644,2.23603032721356,329.522035146308));
#8061=CARTESIAN_POINT('Ctrl Pts',(185.219443465871,2.35378011830126,329.570099000482));
#8062=CARTESIAN_POINT('Ctrl Pts',(185.225450031097,2.46982998827961,329.621900237034));
#8063=CARTESIAN_POINT('Ctrl Pts',(185.231456596324,2.58392919827197,329.677290120548));
#8064=CARTESIAN_POINT('',(185.231676812499,-2.58391981634259,329.677285566066));
#8065=CARTESIAN_POINT('Origin',(185.231676812499,0.,335.));
#8066=CARTESIAN_POINT('',(184.92005200467,-5.91674971498714,334.99816350889));
#8067=CARTESIAN_POINT('Ctrl Pts',(185.231676812499,-2.58391981634272,329.677285566066));
#8068=CARTESIAN_POINT('Ctrl Pts',(185.222990255087,-2.74992539420482,329.757873226288));
#8069=CARTESIAN_POINT('Ctrl Pts',(185.214303697674,-2.9120326743171,329.846169533597));
#8070=CARTESIAN_POINT('Ctrl Pts',(185.205617140262,-3.06960333180715,329.941792219782));
#8071=CARTESIAN_POINT('Ctrl Pts',(185.196915035362,-3.22745601446327,330.037586054608));
#8072=CARTESIAN_POINT('Ctrl Pts',(185.188212930462,-3.3807557423746,330.140732443059));
#8073=CARTESIAN_POINT('Ctrl Pts',(185.179510825562,-3.52889127698889,330.250804603126));
#8074=CARTESIAN_POINT('Ctrl Pts',(185.170808414404,-3.67703202502333,330.360880637026));
#8075=CARTESIAN_POINT('Ctrl Pts',(185.162106003246,-3.82000813672313,330.477882862259));
#8076=CARTESIAN_POINT('Ctrl Pts',(185.153403592088,-3.95723996846166,330.60134311471));
#8077=CARTESIAN_POINT('Ctrl Pts',(185.144712182513,-4.09429831178734,330.724647288771));
#8078=CARTESIAN_POINT('Ctrl Pts',(185.136020772939,-4.22562680319546,330.854393112017));
#8079=CARTESIAN_POINT('Ctrl Pts',(185.127329363365,-4.35068080432546,330.990073928191));
#8080=CARTESIAN_POINT('Ctrl Pts',(185.118669707585,-4.47527792455407,331.125259038726));
#8081=CARTESIAN_POINT('Ctrl Pts',(185.110010051805,-4.59364622847051,331.266335792731));
#8082=CARTESIAN_POINT('Ctrl Pts',(185.101350396025,-4.70528091083734,331.412764000988));
#8083=CARTESIAN_POINT('Ctrl Pts',(185.098419529137,-4.74306375144935,331.462322736108));
#8084=CARTESIAN_POINT('Ctrl Pts',(185.09548866225,-4.7800755565781,331.512494147303));
#8085=CARTESIAN_POINT('Ctrl Pts',(185.092557795362,-4.81629766947775,331.563256290981));
#8086=CARTESIAN_POINT('Ctrl Pts',(185.085133430901,-4.90805419681628,331.691845090786));
#8087=CARTESIAN_POINT('Ctrl Pts',(185.077709066439,-4.99468976033005,331.82415634738));
#8088=CARTESIAN_POINT('Ctrl Pts',(185.070284701978,-5.07589938186872,331.959740795977));
#8089=CARTESIAN_POINT('Ctrl Pts',(185.062861266599,-5.15709884087321,332.0953082776));
#8090=CARTESIAN_POINT('Ctrl Pts',(185.055437831219,-5.23287352017277,332.234147817386));
#8091=CARTESIAN_POINT('Ctrl Pts',(185.04801439584,-5.30296286537544,332.375782895615));
#8092=CARTESIAN_POINT('Ctrl Pts',(185.040590448726,-5.37305704218452,332.517427737452));
#8093=CARTESIAN_POINT('Ctrl Pts',(185.033166501612,-5.43746494147296,332.661868168696));
#8094=CARTESIAN_POINT('Ctrl Pts',(185.025742554498,-5.49597294178626,332.808605013775));
#8095=CARTESIAN_POINT('Ctrl Pts',(185.01831402987,-5.554517017412,332.955432334985));
#8096=CARTESIAN_POINT('Ctrl Pts',(185.010885505242,-5.60715379168083,333.104558553273));
#8097=CARTESIAN_POINT('Ctrl Pts',(185.003456980613,-5.65371843128783,333.255466118926));
#8098=CARTESIAN_POINT('Ctrl Pts',(184.996025702763,-5.70030032907097,333.406429615203));
#8099=CARTESIAN_POINT('Ctrl Pts',(184.988594424913,-5.74080550906829,333.559175417435));
#8100=CARTESIAN_POINT('Ctrl Pts',(184.981163147063,-5.77511970241285,333.713173288549));
#8101=CARTESIAN_POINT('Ctrl Pts',(184.973724976583,-5.8094657227244,333.86731399517));
#8102=CARTESIAN_POINT('Ctrl Pts',(184.966286806103,-5.8376092228219,334.022708725665));
#8103=CARTESIAN_POINT('Ctrl Pts',(184.958848635623,-5.85948739488292,334.178819123635));
#8104=CARTESIAN_POINT('Ctrl Pts',(184.957045349824,-5.86479146758363,334.216666019521));
#8105=CARTESIAN_POINT('Ctrl Pts',(184.955242064025,-5.86972753194538,334.254554963113));
#8106=CARTESIAN_POINT('Ctrl Pts',(184.953438778226,-5.874295153744,334.292478262384));
#8107=CARTESIAN_POINT('Ctrl Pts',(184.942309853718,-5.90248409539786,334.526520772377));
#8108=CARTESIAN_POINT('Ctrl Pts',(184.931180929211,-5.91667646850286,334.762180362099));
#8109=CARTESIAN_POINT('Ctrl Pts',(184.920052004703,-5.91674971498693,334.998163508196));
#8110=CARTESIAN_POINT('',(183.170052045876,-5.9141846117472,334.997236534231));
#8111=CARTESIAN_POINT('Ctrl Pts',(184.92005200467,-5.91674971498714,334.99816350889));
#8112=CARTESIAN_POINT('Ctrl Pts',(184.912619780223,-5.91679863113384,335.155760022943));
#8113=CARTESIAN_POINT('Ctrl Pts',(184.905187555776,-5.91054673781889,335.313517479779));
#8114=CARTESIAN_POINT('Ctrl Pts',(184.897755331329,-5.89798177210636,335.470894445074));
#8115=CARTESIAN_POINT('Ctrl Pts',(184.890328743703,-5.88542633603842,335.628152050986));
#8116=CARTESIAN_POINT('Ctrl Pts',(184.882902156077,-5.86656739122947,335.785029372013));
#8117=CARTESIAN_POINT('Ctrl Pts',(184.87547556845,-5.84144473319586,335.940985648944));
#8118=CARTESIAN_POINT('Ctrl Pts',(184.868053022074,-5.81633574590142,336.096857060747));
#8119=CARTESIAN_POINT('Ctrl Pts',(184.860630475698,-5.78496989265089,336.251808061564));
#8120=CARTESIAN_POINT('Ctrl Pts',(184.853207929321,-5.7474387245306,336.40530376441));
#8121=CARTESIAN_POINT('Ctrl Pts',(184.845786698478,-5.70991420823967,336.558772262476));
#8122=CARTESIAN_POINT('Ctrl Pts',(184.838365467636,-5.66622663380898,336.710785614705));
#8123=CARTESIAN_POINT('Ctrl Pts',(184.830944236793,-5.61651854641477,336.860819706548));
#8124=CARTESIAN_POINT('Ctrl Pts',(184.823523485506,-5.5668136711269,337.01084410328));
#8125=CARTESIAN_POINT('Ctrl Pts',(184.816102734218,-5.51108917306329,337.158889141963));
#8126=CARTESIAN_POINT('Ctrl Pts',(184.808681982931,-5.44953723355074,337.304446680365));
#8127=CARTESIAN_POINT('Ctrl Pts',(184.801260270523,-5.38797732195366,337.450023071088));
#8128=CARTESIAN_POINT('Ctrl Pts',(184.793838558114,-5.32058860997159,337.593110978218));
#8129=CARTESIAN_POINT('Ctrl Pts',(184.786416845706,-5.24761106128227,337.733223136154));
#8130=CARTESIAN_POINT('Ctrl Pts',(184.778992731212,-5.1746098929285,337.873380642313));
#8131=CARTESIAN_POINT('Ctrl Pts',(184.771568616717,-5.09601645692536,338.010560152565));
#8132=CARTESIAN_POINT('Ctrl Pts',(184.764144502223,-5.01211614933689,338.144299964707));
#8133=CARTESIAN_POINT('Ctrl Pts',(184.756711842999,-4.92811927731015,338.278193703696));
#8134=CARTESIAN_POINT('Ctrl Pts',(184.749279183775,-4.83880352864732,338.408639520922));
#8135=CARTESIAN_POINT('Ctrl Pts',(184.741846524551,-4.74449754696208,338.535204886477));
#8136=CARTESIAN_POINT('Ctrl Pts',(184.734409529676,-4.6501365543043,338.661844080688));
#8137=CARTESIAN_POINT('Ctrl Pts',(184.726972534801,-4.55077975997184,338.784598023861));
#8138=CARTESIAN_POINT('Ctrl Pts',(184.719535539926,-4.44679511124884,338.903068510938));
#8139=CARTESIAN_POINT('Ctrl Pts',(184.71208645424,-4.34264140785249,339.021731603267));
#8140=CARTESIAN_POINT('Ctrl Pts',(184.704637368554,-4.23384506932699,339.136097053411));
#8141=CARTESIAN_POINT('Ctrl Pts',(184.697188282868,-4.12081067877543,339.245803800482));
#8142=CARTESIAN_POINT('Ctrl Pts',(184.689859103229,-4.00959577420389,339.353744625809));
#8143=CARTESIAN_POINT('Ctrl Pts',(184.68252992359,-3.89427853114121,339.457175440066));
#8144=CARTESIAN_POINT('Ctrl Pts',(184.675200743952,-3.77527300229889,339.555792392176));
#8145=CARTESIAN_POINT('Ctrl Pts',(184.667838127936,-3.65572455952815,339.654859243694));
#8146=CARTESIAN_POINT('Ctrl Pts',(184.66047551192,-3.53206351088873,339.749391592085));
#8147=CARTESIAN_POINT('Ctrl Pts',(184.653112895905,-3.40467128147213,339.83902304475));
#8148=CARTESIAN_POINT('Ctrl Pts',(184.645759730408,-3.2774425703866,339.928539448124));
#8149=CARTESIAN_POINT('Ctrl Pts',(184.638406564911,-3.14649251509857,340.013167256584));
#8150=CARTESIAN_POINT('Ctrl Pts',(184.631053399415,-3.0122375759683,340.092578457758));
#8151=CARTESIAN_POINT('Ctrl Pts',(184.623708000047,-2.87812443171289,340.171905787893));
#8152=CARTESIAN_POINT('Ctrl Pts',(184.61636260068,-2.74071367435079,340.246027283195));
#8153=CARTESIAN_POINT('Ctrl Pts',(184.609017201312,-2.60045271628154,340.31465673707));
#8154=CARTESIAN_POINT('Ctrl Pts',(184.601677890707,-2.46030802359194,340.383229302488));
#8155=CARTESIAN_POINT('Ctrl Pts',(184.594338580102,-2.31731817234493,340.446318721519));
#8156=CARTESIAN_POINT('Ctrl Pts',(184.586999269496,-2.17195710676042,340.503683574561));
#8157=CARTESIAN_POINT('Ctrl Pts',(184.579664375719,-2.0266835200817,340.561013905191));
#8158=CARTESIAN_POINT('Ctrl Pts',(184.572329481942,-1.87904191250176,340.612626389189));
#8159=CARTESIAN_POINT('Ctrl Pts',(184.564994588165,-1.72952805167491,340.658326897677));
#8160=CARTESIAN_POINT('Ctrl Pts',(184.557661505516,-1.58005110871701,340.704016121823));
#8161=CARTESIAN_POINT('Ctrl Pts',(184.550328422866,-1.42870319402623,340.74379615947));
#8162=CARTESIAN_POINT('Ctrl Pts',(184.542995340217,-1.27599715176997,340.777522118623));
#8163=CARTESIAN_POINT('Ctrl Pts',(184.535662944991,-1.12330542461659,340.811244916207));
#8164=CARTESIAN_POINT('Ctrl Pts',(184.528330549766,-0.9692561943182,340.838914681973));
#8165=CARTESIAN_POINT('Ctrl Pts',(184.52099815454,-0.814374148435138,340.860437296726));
#8166=CARTESIAN_POINT('Ctrl Pts',(184.513664938763,-0.659474770038268,340.881962320029));
#8167=CARTESIAN_POINT('Ctrl Pts',(184.506331722985,-0.503742767188637,340.897338770723));
#8168=CARTESIAN_POINT('Ctrl Pts',(184.498998507207,-0.347709384272906,340.906524252603));
#8169=CARTESIAN_POINT('Ctrl Pts',(184.491662962579,-0.191626448962799,340.915712651569));
#8170=CARTESIAN_POINT('Ctrl Pts',(184.484327417951,-0.0352423224554345,
340.918706146454));
#8171=CARTESIAN_POINT('Ctrl Pts',(184.476991873322,0.120910551135107,340.915514449405));
#8172=CARTESIAN_POINT('Ctrl Pts',(184.469648295885,0.277234420369081,340.91231925728));
#8173=CARTESIAN_POINT('Ctrl Pts',(184.462304718448,0.433326150599635,340.902925355566));
#8174=CARTESIAN_POINT('Ctrl Pts',(184.454961141011,0.5886565605209,340.887394501497));
#8175=CARTESIAN_POINT('Ctrl Pts',(184.44761315717,0.744080174138074,340.871854328371));
#8176=CARTESIAN_POINT('Ctrl Pts',(184.440265173329,0.898741181947789,340.850169920815));
#8177=CARTESIAN_POINT('Ctrl Pts',(184.432917189488,1.05212010901704,340.822454279658));
#8178=CARTESIAN_POINT('Ctrl Pts',(184.425558330586,1.20572603784741,340.79469761918));
#8179=CARTESIAN_POINT('Ctrl Pts',(184.418199471683,1.35804572634777,340.760891980628));
#8180=CARTESIAN_POINT('Ctrl Pts',(184.41084061278,1.50857359387691,340.721200597284));
#8181=CARTESIAN_POINT('Ctrl Pts',(184.406214645079,1.60319927735646,340.696249574334));
#8182=CARTESIAN_POINT('Ctrl Pts',(184.401588677378,1.69711722968619,340.668973667477));
#8183=CARTESIAN_POINT('Ctrl Pts',(184.396962709677,1.79020608238217,340.639423086194));
#8184=CARTESIAN_POINT('Ctrl Pts',(184.38952595157,1.93985677705864,340.591917236793));
#8185=CARTESIAN_POINT('Ctrl Pts',(184.382089193462,2.08783569334246,340.538380481181));
#8186=CARTESIAN_POINT('Ctrl Pts',(184.374652435355,2.23362118212995,340.478947615851));
#8187=CARTESIAN_POINT('Ctrl Pts',(184.36722438968,2.37923587790224,340.41958437829));
#8188=CARTESIAN_POINT('Ctrl Pts',(184.359796344006,2.52266192055002,340.354338920509));
#8189=CARTESIAN_POINT('Ctrl Pts',(184.352368298332,2.66339208409924,340.283395988269));
#8190=CARTESIAN_POINT('Ctrl Pts',(184.344947351862,2.80398774764274,340.212520858301));
#8191=CARTESIAN_POINT('Ctrl Pts',(184.337526405392,2.94189233205641,340.135959261353));
#8192=CARTESIAN_POINT('Ctrl Pts',(184.330105458922,3.07661798277987,340.053944236983));
#8193=CARTESIAN_POINT('Ctrl Pts',(184.322690003926,3.21124393699783,339.971989903442));
#8194=CARTESIAN_POINT('Ctrl Pts',(184.315274548931,3.34269532561923,339.884590370821));
#8195=CARTESIAN_POINT('Ctrl Pts',(184.307859093935,3.47050841928556,339.792024819861));
#8196=CARTESIAN_POINT('Ctrl Pts',(184.300447526971,3.59825449867548,339.699507802375));
#8197=CARTESIAN_POINT('Ctrl Pts',(184.293035960007,3.72236578216018,339.601830378786));
#8198=CARTESIAN_POINT('Ctrl Pts',(184.285624393042,3.84240717485589,339.499315244025));
#8199=CARTESIAN_POINT('Ctrl Pts',(184.278214075443,3.96242833223092,339.396817390192));
#8200=CARTESIAN_POINT('Ctrl Pts',(184.270803757843,4.07838067841884,339.289483685316));
#8201=CARTESIAN_POINT('Ctrl Pts',(184.263393440243,4.18986180372311,339.177677420314));
#8202=CARTESIAN_POINT('Ctrl Pts',(184.255983463113,4.30133780698697,339.065876292291));
#8203=CARTESIAN_POINT('Ctrl Pts',(184.248573485983,4.40834273546606,338.949603276056));
#8204=CARTESIAN_POINT('Ctrl Pts',(184.241163508853,4.51051088298533,338.829258692877));
#8205=CARTESIAN_POINT('Ctrl Pts',(184.233752424211,4.6126943007808,338.708896122731));
#8206=CARTESIAN_POINT('Ctrl Pts',(184.22634133957,4.71003925753255,338.58446105728));
#8207=CARTESIAN_POINT('Ctrl Pts',(184.218930254928,4.80222029034206,338.456386964089));
#8208=CARTESIAN_POINT('Ctrl Pts',(184.211516614422,4.89443311367248,338.328268701919));
#8209=CARTESIAN_POINT('Ctrl Pts',(184.204102973916,4.9814782500839,338.19650921469));
#8210=CARTESIAN_POINT('Ctrl Pts',(184.196689333409,5.06307359867799,338.061570887121));
#8211=CARTESIAN_POINT('Ctrl Pts',(184.189267697252,5.14475694829225,337.926487027844));
#8212=CARTESIAN_POINT('Ctrl Pts',(184.181846061095,5.22097857950156,337.788217799716));
#8213=CARTESIAN_POINT('Ctrl Pts',(184.174424424938,5.29150204892088,337.647250768017));
#8214=CARTESIAN_POINT('Ctrl Pts',(184.166998280622,5.36206835673941,337.506198108058));
#8215=CARTESIAN_POINT('Ctrl Pts',(184.159572136306,5.42692945253008,337.362444716905));
#8216=CARTESIAN_POINT('Ctrl Pts',(184.152145991989,5.48589727294769,337.216497614067));
#8217=CARTESIAN_POINT('Ctrl Pts',(184.144709488946,5.54494734756367,337.070346929651));
#8218=CARTESIAN_POINT('Ctrl Pts',(184.137272985903,5.59808760342417,336.921996771054));
#8219=CARTESIAN_POINT('Ctrl Pts',(184.12983648286,5.64517975891654,336.771969540376));
#8220=CARTESIAN_POINT('Ctrl Pts',(184.126132547041,5.66863518151359,336.697244736216));
#8221=CARTESIAN_POINT('Ctrl Pts',(184.122428611222,5.69059099402034,336.622104058256));
#8222=CARTESIAN_POINT('Ctrl Pts',(184.118724675403,5.71103486732865,336.546612849635));
#8223=CARTESIAN_POINT('Ctrl Pts',(184.111291533105,5.75206209535312,336.395115382242));
#8224=CARTESIAN_POINT('Ctrl Pts',(184.103858390807,5.78711705717358,336.241762432013));
#8225=CARTESIAN_POINT('Ctrl Pts',(184.096425248508,5.81603124347139,336.087065378652));
#8226=CARTESIAN_POINT('Ctrl Pts',(184.089000704779,5.84491198218809,335.932547276973));
#8227=CARTESIAN_POINT('Ctrl Pts',(184.081576161049,5.8676660182781,335.776688529685));
#8228=CARTESIAN_POINT('Ctrl Pts',(184.07415161732,5.88417466538833,335.620015378601));
#8229=CARTESIAN_POINT('Ctrl Pts',(184.066734055716,5.90066778757921,335.463489564729));
#8230=CARTESIAN_POINT('Ctrl Pts',(184.059316494112,5.91092717525258,335.306151239589));
#8231=CARTESIAN_POINT('Ctrl Pts',(184.051898932508,5.91488524718123,335.148536443938));
#8232=CARTESIAN_POINT('Ctrl Pts',(184.044486742013,5.91884045304185,334.991035778282));
#8233=CARTESIAN_POINT('Ctrl Pts',(184.037074551518,5.91650341964218,334.833259411251));
#8234=CARTESIAN_POINT('Ctrl Pts',(184.029662361023,5.90785842858468,334.675748014191));
#8235=CARTESIAN_POINT('Ctrl Pts',(184.022253934834,5.89921782791392,334.518316609805));
#8236=CARTESIAN_POINT('Ctrl Pts',(184.014845508644,5.88427567030619,334.361150278058));
#8237=CARTESIAN_POINT('Ctrl Pts',(184.007437082454,5.86306832554752,334.204789101897));
#8238=CARTESIAN_POINT('Ctrl Pts',(184.000029708666,5.84186399339433,334.048450137594));
#8239=CARTESIAN_POINT('Ctrl Pts',(183.992622334879,5.81439628924412,333.892916470451));
#8240=CARTESIAN_POINT('Ctrl Pts',(183.985214961092,5.78075340524612,333.738722619629));
#8241=CARTESIAN_POINT('Ctrl Pts',(183.977807804681,5.74711150853291,333.584533293783));
#8242=CARTESIAN_POINT('Ctrl Pts',(183.970400648271,5.70729487142547,333.43168406971));
#8243=CARTESIAN_POINT('Ctrl Pts',(183.962993491861,5.6614426752963,333.280698573015));
#8244=CARTESIAN_POINT('Ctrl Pts',(183.955585101566,5.61558284110861,333.129687925157));
#8245=CARTESIAN_POINT('Ctrl Pts',(183.948176711272,5.56368555402802,332.980541978969));
#8246=CARTESIAN_POINT('Ctrl Pts',(183.940768320977,5.50593962476721,332.833768384748));
#8247=CARTESIAN_POINT('Ctrl Pts',(183.933357245087,5.44817276217845,332.686941584009));
#8248=CARTESIAN_POINT('Ctrl Pts',(183.925946169196,5.38455317201563,332.54248919366));
#8249=CARTESIAN_POINT('Ctrl Pts',(183.918535093305,5.31531741559422,332.400897975458));
#8250=CARTESIAN_POINT('Ctrl Pts',(183.911115809991,5.24600498378105,332.259149951542));
#8251=CARTESIAN_POINT('Ctrl Pts',(183.903696526677,5.17106412819874,332.120269762214));
#8252=CARTESIAN_POINT('Ctrl Pts',(183.896277243363,5.0907772599879,331.984719341141));
#8253=CARTESIAN_POINT('Ctrl Pts',(183.88885333492,5.01044034150579,331.849084418884));
#8254=CARTESIAN_POINT('Ctrl Pts',(183.881429426476,4.92475097110622,331.716783712901));
#8255=CARTESIAN_POINT('Ctrl Pts',(183.874005518033,4.83403404540267,331.58824892315));
#8256=CARTESIAN_POINT('Ctrl Pts',(183.866571048381,4.74318806632862,331.459531280555));
#8257=CARTESIAN_POINT('Ctrl Pts',(183.859136578729,4.64730047350111,331.334590548397));
#8258=CARTESIAN_POINT('Ctrl Pts',(183.851702109076,4.5467359840883,331.213824825302));
#8259=CARTESIAN_POINT('Ctrl Pts',(183.847963619761,4.49616623442231,331.153096705259));
#8260=CARTESIAN_POINT('Ctrl Pts',(183.844225130445,4.44441443244363,331.093423724049));
#8261=CARTESIAN_POINT('Ctrl Pts',(183.840486641129,4.39153029166857,331.03485280729));
#8262=CARTESIAN_POINT('Ctrl Pts',(183.833071341635,4.28663451446825,330.918677300895));
#8263=CARTESIAN_POINT('Ctrl Pts',(183.825656042141,4.17696364349042,330.806487844053));
#8264=CARTESIAN_POINT('Ctrl Pts',(183.818240742648,4.06285276260022,330.698702754757));
#8265=CARTESIAN_POINT('Ctrl Pts',(183.81083430635,3.94887827366561,330.591046496463));
#8266=CARTESIAN_POINT('Ctrl Pts',(183.803427870053,3.83047460714228,330.487784381869));
#8267=CARTESIAN_POINT('Ctrl Pts',(183.796021433756,3.70801650912296,330.389301123412));
#8268=CARTESIAN_POINT('Ctrl Pts',(183.788622225179,3.58567791431063,330.29091397183));
#8269=CARTESIAN_POINT('Ctrl Pts',(183.781223016603,3.45929305403203,330.197296625528));
#8270=CARTESIAN_POINT('Ctrl Pts',(183.773823808026,3.32927277795976,330.108796330919));
#8271=CARTESIAN_POINT('Ctrl Pts',(183.766430197456,3.1993508711017,330.020362992823));
#8272=CARTESIAN_POINT('Ctrl Pts',(183.759036586885,3.06579933267352,329.937039207934));
#8273=CARTESIAN_POINT('Ctrl Pts',(183.751642976315,2.92906117849915,329.859131282059));
#8274=CARTESIAN_POINT('Ctrl Pts',(183.744253338514,2.79239649710532,329.781265218032));
#8275=CARTESIAN_POINT('Ctrl Pts',(183.736863700713,2.65254893412756,329.708809402507));
#8276=CARTESIAN_POINT('Ctrl Pts',(183.729474062911,2.50998939743267,329.642026149068));
#8277=CARTESIAN_POINT('Ctrl Pts',(183.722085730066,2.36745503571489,329.575254689065));
#8278=CARTESIAN_POINT('Ctrl Pts',(183.714697397222,2.22220998950275,329.514153961201));
#8279=CARTESIAN_POINT('Ctrl Pts',(183.707309064377,2.07474870498796,329.458939778919));
#8280=CARTESIAN_POINT('Ctrl Pts',(183.699921103922,1.92729485287575,329.403728379564));
#8281=CARTESIAN_POINT('Ctrl Pts',(183.692533143466,1.77762533503827,329.354403067024));
#8282=CARTESIAN_POINT('Ctrl Pts',(183.685145183011,1.62625320201453,329.311130948472));
#8283=CARTESIAN_POINT('Ctrl Pts',(183.677756127613,1.47485863466583,329.267852416713));
#8284=CARTESIAN_POINT('Ctrl Pts',(183.670367072214,1.32176130954512,329.230628968008));
#8285=CARTESIAN_POINT('Ctrl Pts',(183.662978016816,1.1674878510558,329.199577370558));
#8286=CARTESIAN_POINT('Ctrl Pts',(183.655586398755,1.01316088765289,329.168515003836));
#8287=CARTESIAN_POINT('Ctrl Pts',(183.648194780694,0.857657345420576,329.143628823689));
#8288=CARTESIAN_POINT('Ctrl Pts',(183.640803162633,0.701512249812086,329.124984159522));
#8289=CARTESIAN_POINT('Ctrl Pts',(183.633403427034,0.545195674309636,329.106319019625));
#8290=CARTESIAN_POINT('Ctrl Pts',(183.626003691434,0.388236510204654,329.093909128754));
#8291=CARTESIAN_POINT('Ctrl Pts',(183.618603955834,0.231173818176808,329.087767830312));
#8292=CARTESIAN_POINT('Ctrl Pts',(183.611199675289,0.0740146576405804,329.081622759862));
#8293=CARTESIAN_POINT('Ctrl Pts',(183.603795394743,-0.0832477841853048,
329.081753953129));
#8294=CARTESIAN_POINT('Ctrl Pts',(183.596391114198,-0.240076805591269,329.088122659432));
#8295=CARTESIAN_POINT('Ctrl Pts',(183.588976229497,-0.397130432111038,329.094500486777));
#8296=CARTESIAN_POINT('Ctrl Pts',(183.581561344796,-0.553749026509288,329.107133638302));
#8297=CARTESIAN_POINT('Ctrl Pts',(183.574146460095,-0.709402527221167,329.12593168095));
#8298=CARTESIAN_POINT('Ctrl Pts',(183.570180509015,-0.792655901232077,329.135986067571));
#8299=CARTESIAN_POINT('Ctrl Pts',(183.566214557935,-0.875633368236423,329.147803228726));
#8300=CARTESIAN_POINT('Ctrl Pts',(183.562248606855,-0.958255423253487,329.1613634206));
#8301=CARTESIAN_POINT('Ctrl Pts',(183.554822205967,-1.11296850227204,329.186755418373));
#8302=CARTESIAN_POINT('Ctrl Pts',(183.547395805078,-1.26690385654412,329.218339191136));
#8303=CARTESIAN_POINT('Ctrl Pts',(183.539969404189,-1.41952706644195,329.256057671761));
#8304=CARTESIAN_POINT('Ctrl Pts',(183.532551750186,-1.57197051527248,329.2937317272));
#8305=CARTESIAN_POINT('Ctrl Pts',(183.525134096183,-1.72310453748313,329.337526019185));
#8306=CARTESIAN_POINT('Ctrl Pts',(183.517716442179,-1.87240167805583,329.387331960777));
#8307=CARTESIAN_POINT('Ctrl Pts',(183.510305911022,-2.02155545516595,329.437090075919));
#8308=CARTESIAN_POINT('Ctrl Pts',(183.502895379865,-2.16887551081852,329.492848230864));
#8309=CARTESIAN_POINT('Ctrl Pts',(183.495484848708,-2.31384650714532,329.55444723615));
#8310=CARTESIAN_POINT('Ctrl Pts',(183.488079821943,-2.45870982195383,329.616000486944));
#8311=CARTESIAN_POINT('Ctrl Pts',(183.480674795179,-2.60122720993012,329.683385804227));
#8312=CARTESIAN_POINT('Ctrl Pts',(183.473269768414,-2.74090048242339,329.756394836761));
#8313=CARTESIAN_POINT('Ctrl Pts',(183.465868631931,-2.88050037660378,329.829365513498));
#8314=CARTESIAN_POINT('Ctrl Pts',(183.458467495448,-3.01725880140435,329.907953849107));
#8315=CARTESIAN_POINT('Ctrl Pts',(183.451066358965,-3.15069957564894,329.991904279419));
#8316=CARTESIAN_POINT('Ctrl Pts',(183.44366644037,-3.28411839165312,330.075840895334));
#8317=CARTESIAN_POINT('Ctrl Pts',(183.436266521775,-3.41422032527419,330.165137656328));
#8318=CARTESIAN_POINT('Ctrl Pts',(183.42886660318,-3.54055564443255,330.259494089111));
#8319=CARTESIAN_POINT('Ctrl Pts',(183.42146700395,-3.6668855112183,330.353846449664));
#8320=CARTESIAN_POINT('Ctrl Pts',(183.414067404721,-3.78944878797824,330.453257824654));
#8321=CARTESIAN_POINT('Ctrl Pts',(183.406667805491,-3.90782670160056,330.55738578844));
#8322=CARTESIAN_POINT('Ctrl Pts',(183.399267068085,-4.02622282363367,330.661529768766));
#8323=CARTESIAN_POINT('Ctrl Pts',(183.391866330679,-4.14043202064027,330.770391536118));
#8324=CARTESIAN_POINT('Ctrl Pts',(183.384465593273,-4.25007055504534,330.883590054473));
#8325=CARTESIAN_POINT('Ctrl Pts',(183.377062259749,-4.35974754974122,330.996828281931));
#8326=CARTESIAN_POINT('Ctrl Pts',(183.369658926226,-4.46485043023356,331.114406021615));
#8327=CARTESIAN_POINT('Ctrl Pts',(183.362255592702,-4.56503420191328,331.2359073739));
#8328=CARTESIAN_POINT('Ctrl Pts',(183.354844149367,-4.6653277176057,331.357541822051));
#8329=CARTESIAN_POINT('Ctrl Pts',(183.347432706032,-4.76069112589044,331.48310817832));
#8330=CARTESIAN_POINT('Ctrl Pts',(183.340021262697,-4.85082098726279,331.612159048593));
#8331=CARTESIAN_POINT('Ctrl Pts',(183.332605261194,-4.94100628007502,331.741289287406));
#8332=CARTESIAN_POINT('Ctrl Pts',(183.325189259692,-5.02595141145103,331.873907997273));
#8333=CARTESIAN_POINT('Ctrl Pts',(183.31777325819,-5.10539803212959,332.009541590989));
#8334=CARTESIAN_POINT('Ctrl Pts',(183.310346732626,-5.18495739565542,332.14536766259));
#8335=CARTESIAN_POINT('Ctrl Pts',(183.302920207062,-5.25900248937629,332.284216834756));
#8336=CARTESIAN_POINT('Ctrl Pts',(183.295493681498,-5.32732202300773,332.425593150709));
#8337=CARTESIAN_POINT('Ctrl Pts',(183.291665978526,-5.36253457020601,332.498459868814));
#8338=CARTESIAN_POINT('Ctrl Pts',(183.287838275554,-5.3962269351572,332.571997616807));
#8339=CARTESIAN_POINT('Ctrl Pts',(183.284010572581,-5.42837534055216,332.646136850922));
#8340=CARTESIAN_POINT('Ctrl Pts',(183.275805271224,-5.4972906551283,332.805066308813));
#8341=CARTESIAN_POINT('Ctrl Pts',(183.267599969866,-5.55928544853722,332.967169333632));
#8342=CARTESIAN_POINT('Ctrl Pts',(183.259394668509,-5.61408642515934,333.131855419583));
#8343=CARTESIAN_POINT('Ctrl Pts',(183.251221118284,-5.66867534459627,333.295904238281));
#8344=CARTESIAN_POINT('Ctrl Pts',(183.24304756806,-5.71612589604507,333.462515953562));
#8345=CARTESIAN_POINT('Ctrl Pts',(183.234874017836,-5.75621375928746,333.631083012053));
#8346=CARTESIAN_POINT('Ctrl Pts',(183.226720710988,-5.79620233719068,333.799232581653));
#8347=CARTESIAN_POINT('Ctrl Pts',(183.21856740414,-5.82886453416691,333.969327605915));
#8348=CARTESIAN_POINT('Ctrl Pts',(183.210414097292,-5.85402514545746,334.140744415874));
#8349=CARTESIAN_POINT('Ctrl Pts',(183.202294040006,-5.87908315061312,334.311462180165));
#8350=CARTESIAN_POINT('Ctrl Pts',(183.19417398272,-5.89670053572695,334.48349074463));
#8351=CARTESIAN_POINT('Ctrl Pts',(183.186053925434,-5.90675291265045,334.656196871167));
#8352=CARTESIAN_POINT('Ctrl Pts',(183.180719971474,-5.9133561808052,334.769645150531));
#8353=CARTESIAN_POINT('Ctrl Pts',(183.175386017515,-5.91669614926623,334.883385452545));
#8354=CARTESIAN_POINT('Ctrl Pts',(183.170052063555,-5.91674935391449,334.997234958864));
#8355=CARTESIAN_POINT('',(181.420051985035,-5.91433197925221,335.005087499131));
#8356=CARTESIAN_POINT('Ctrl Pts',(183.170052004703,-5.90821144120066,334.997240203191));
#8357=CARTESIAN_POINT('Ctrl Pts',(183.115292182571,-5.90323267541164,336.164366188066));
#8358=CARTESIAN_POINT('Ctrl Pts',(182.967786349014,-5.00352060360718,339.315297141657));
#8359=CARTESIAN_POINT('Ctrl Pts',(182.727534504034,0.126099951212518,341.995542180405));
#8360=CARTESIAN_POINT('Ctrl Pts',(182.449296469759,5.95081939807114,338.679636353434));
#8361=CARTESIAN_POINT('Ctrl Pts',(182.171058435485,6.31467872490261,331.98709815247));
#8362=CARTESIAN_POINT('Ctrl Pts',(181.892820401213,0.883587563514807,328.059394286476));
#8363=CARTESIAN_POINT('Ctrl Pts',(181.642484924283,-4.73236743609919,330.256161176751));
#8364=CARTESIAN_POINT('Ctrl Pts',(181.484895458781,-5.90158033103822,333.625694798448));
#8365=CARTESIAN_POINT('Ctrl Pts',(181.420052004703,-5.91283370962365,335.005085791765));
#8366=CARTESIAN_POINT('',(179.670052004703,-5.92204575238021,335.000414748955));
#8367=CARTESIAN_POINT('Ctrl Pts',(181.420051953322,-5.91674781039664,335.005090252112));
#8368=CARTESIAN_POINT('Ctrl Pts',(181.411147422927,-5.91658474097863,335.194636978031));
#8369=CARTESIAN_POINT('Ctrl Pts',(181.402242892532,-5.90730958247142,335.383786698931));
#8370=CARTESIAN_POINT('Ctrl Pts',(181.393338362136,-5.88905914607669,335.571763007295));
#8371=CARTESIAN_POINT('Ctrl Pts',(181.384360339045,-5.87065808143897,335.761290760262));
#8372=CARTESIAN_POINT('Ctrl Pts',(181.375382315954,-5.84313306743074,335.949625655848));
#8373=CARTESIAN_POINT('Ctrl Pts',(181.366404292863,-5.80667280514391,336.1359936164));
#8374=CARTESIAN_POINT('Ctrl Pts',(181.357349481857,-5.76990070276834,336.323955558941));
#8375=CARTESIAN_POINT('Ctrl Pts',(181.348294670851,-5.7240398980615,336.509916787005));
#8376=CARTESIAN_POINT('Ctrl Pts',(181.339239859845,-5.66933204111301,336.693105067652));
#8377=CARTESIAN_POINT('Ctrl Pts',(181.338274684118,-5.66350058912769,336.712631580341));
#8378=CARTESIAN_POINT('Ctrl Pts',(181.337309508391,-5.65756866145798,336.732126607076));
#8379=CARTESIAN_POINT('Ctrl Pts',(181.336344332663,-5.65153658240612,336.751589227024));
#8380=CARTESIAN_POINT('Ctrl Pts',(181.328920381285,-5.60513895726375,336.901292063615));
#8381=CARTESIAN_POINT('Ctrl Pts',(181.321496429907,-5.55271903695615,337.049375946457));
#8382=CARTESIAN_POINT('Ctrl Pts',(181.314072478529,-5.49440646048727,337.19531961442));
#8383=CARTESIAN_POINT('Ctrl Pts',(181.306657288914,-5.43616270465071,337.341091039341));
#8384=CARTESIAN_POINT('Ctrl Pts',(181.2992420993,-5.37204027287378,337.484726933996));
#8385=CARTESIAN_POINT('Ctrl Pts',(181.291826909686,-5.30221888531639,337.625719987869));
#8386=CARTESIAN_POINT('Ctrl Pts',(181.284418855281,-5.23246468285505,337.766577372255));
#8387=CARTESIAN_POINT('Ctrl Pts',(181.277010800877,-5.15702260630546,337.904796646388));
#8388=CARTESIAN_POINT('Ctrl Pts',(181.269602746472,-5.07612084188826,338.039889432372));
#8389=CARTESIAN_POINT('Ctrl Pts',(181.262200206336,-4.9952792976128,338.174881660516));
#8390=CARTESIAN_POINT('Ctrl Pts',(181.2547976662,-4.90898634837258,338.30675171556));
#8391=CARTESIAN_POINT('Ctrl Pts',(181.247395126065,-4.81751652857495,338.435034942967));
#8392=CARTESIAN_POINT('Ctrl Pts',(181.23999648362,-4.72609487077569,338.563250624854));
#8393=CARTESIAN_POINT('Ctrl Pts',(181.232597841176,-4.62950198713847,338.687882937227));
#8394=CARTESIAN_POINT('Ctrl Pts',(181.225199198731,-4.5280561621734,338.80849549753));
#8395=CARTESIAN_POINT('Ctrl Pts',(181.217801777159,-4.42662707707912,338.929088155203));
#8396=CARTESIAN_POINT('Ctrl Pts',(181.210404355586,-4.32034687998087,339.045662091926));
#8397=CARTESIAN_POINT('Ctrl Pts',(181.203006934013,-4.20957471251635,339.157813283716));
#8398=CARTESIAN_POINT('Ctrl Pts',(181.195609833377,-4.09880735090034,339.269959609828));
#8399=CARTESIAN_POINT('Ctrl Pts',(181.188212732741,-3.98354866867682,339.377683307001));
#8400=CARTESIAN_POINT('Ctrl Pts',(181.180815632105,-3.8641951145148,339.480616774447));
#8401=CARTESIAN_POINT('Ctrl Pts',(181.173417392669,-3.74482318560877,339.583566088729));
#8402=CARTESIAN_POINT('Ctrl Pts',(181.166019153234,-3.62135541216968,339.681723461133));
#8403=CARTESIAN_POINT('Ctrl Pts',(181.158620913798,-3.4942216771828,339.77476129594));
#8404=CARTESIAN_POINT('Ctrl Pts',(181.151220075422,-3.36704328118306,339.867831814156));
#8405=CARTESIAN_POINT('Ctrl Pts',(181.143819237047,-3.23619666057628,339.955778993795));
#8406=CARTESIAN_POINT('Ctrl Pts',(181.136418398672,-3.10214090914292,340.038318404222));
#8407=CARTESIAN_POINT('Ctrl Pts',(181.129009433525,-2.9679379526995,340.120948450184));
#8408=CARTESIAN_POINT('Ctrl Pts',(181.121600468378,-2.83051914599176,340.198158672226));
#8409=CARTESIAN_POINT('Ctrl Pts',(181.114191503231,-2.69036906890002,340.269710128233));
#8410=CARTESIAN_POINT('Ctrl Pts',(181.106777973981,-2.55013265593105,340.341305661689));
#8411=CARTESIAN_POINT('Ctrl Pts',(181.09936444473,-2.40716195803917,340.407235326995));
#8412=CARTESIAN_POINT('Ctrl Pts',(181.091950915479,-2.26196129838316,340.467308446312));
#8413=CARTESIAN_POINT('Ctrl Pts',(181.084526831572,-2.11655391626657,340.527467091846));
#8414=CARTESIAN_POINT('Ctrl Pts',(181.077102747665,-1.96891058101614,340.581752410341));
#8415=CARTESIAN_POINT('Ctrl Pts',(181.069678663759,-1.81955130189638,340.630023412231));
#8416=CARTESIAN_POINT('Ctrl Pts',(181.065821208636,-1.74194620966027,340.655104381931));
#8417=CARTESIAN_POINT('Ctrl Pts',(181.061963753514,-1.66387805203984,340.678562502924));
#8418=CARTESIAN_POINT('Ctrl Pts',(181.058106298391,-1.58542071034248,340.700383472515));
#8419=CARTESIAN_POINT('Ctrl Pts',(181.050682308358,-1.43442309553192,340.742379725378));
#8420=CARTESIAN_POINT('Ctrl Pts',(181.043258318325,-1.28152788807992,340.778435516522));
#8421=CARTESIAN_POINT('Ctrl Pts',(181.035834328293,-1.12724358945137,340.808377781493));
#8422=CARTESIAN_POINT('Ctrl Pts',(181.028419099551,-0.973141366712676,340.838284710628));
#8423=CARTESIAN_POINT('Ctrl Pts',(181.021003870809,-0.81765367868449,340.862092404294));
#8424=CARTESIAN_POINT('Ctrl Pts',(181.013588642066,-0.661304396650291,340.879677462027));
#8425=CARTESIAN_POINT('Ctrl Pts',(181.006180548101,-0.505105550602682,340.897245599788));
#8426=CARTESIAN_POINT('Ctrl Pts',(180.998772454136,-0.348047129341617,340.90860297976));
#8427=CARTESIAN_POINT('Ctrl Pts',(180.991364360171,-0.190663310515679,340.913677203274));
#8428=CARTESIAN_POINT('Ctrl Pts',(180.983961780082,-0.0333966331472128,
340.918747650022));
#8429=CARTESIAN_POINT('Ctrl Pts',(180.976559199994,0.12419458812263,340.91754424009));
#8430=CARTESIAN_POINT('Ctrl Pts',(180.969156619905,0.281571043968763,340.910046388117));
#8431=CARTESIAN_POINT('Ctrl Pts',(180.961757937154,0.438864643663797,340.902552483642));
#8432=CARTESIAN_POINT('Ctrl Pts',(180.954359254404,0.59594333127363,340.888770754714));
#8433=CARTESIAN_POINT('Ctrl Pts',(180.946960571654,0.752267896746034,340.868732705962));
#8434=CARTESIAN_POINT('Ctrl Pts',(180.939563109374,0.908566675243656,340.848697962644));
#8435=CARTESIAN_POINT('Ctrl Pts',(180.932165647095,1.06411120867336,340.822408995151));
#8436=CARTESIAN_POINT('Ctrl Pts',(180.924768184816,1.2183673882307,340.789949176789));
#8437=CARTESIAN_POINT('Ctrl Pts',(180.91737104323,1.37261688052187,340.757490765614));
#8438=CARTESIAN_POINT('Ctrl Pts',(180.909973901643,1.52557776478184,340.718862112333));
#8439=CARTESIAN_POINT('Ctrl Pts',(180.902576760056,1.67672637260299,340.674197673144));
#8440=CARTESIAN_POINT('Ctrl Pts',(180.89517847946,1.82789825424608,340.629526356538));
#8441=CARTESIAN_POINT('Ctrl Pts',(180.887780198863,1.97725694588523,340.578817509257));
#8442=CARTESIAN_POINT('Ctrl Pts',(180.880381918267,2.12429432726241,340.522255352088));
#8443=CARTESIAN_POINT('Ctrl Pts',(180.872981038556,2.27138336483281,340.465673323878));
#8444=CARTESIAN_POINT('Ctrl Pts',(180.865580158844,2.41614912036067,340.403234025507));
#8445=CARTESIAN_POINT('Ctrl Pts',(180.858179279133,2.55810396458789,340.335169600759));
#8446=CARTESIAN_POINT('Ctrl Pts',(180.850770272591,2.70021468799824,340.267030435152));
#8447=CARTESIAN_POINT('Ctrl Pts',(180.843361266048,2.8395079992099,340.193253969033));
#8448=CARTESIAN_POINT('Ctrl Pts',(180.835952259506,2.97552072938724,340.114118394356));
#8449=CARTESIAN_POINT('Ctrl Pts',(180.828538688764,3.11161724802215,340.034934069479));
#8450=CARTESIAN_POINT('Ctrl Pts',(180.821125118022,3.24442884452244,339.950384257538));
#8451=CARTESIAN_POINT('Ctrl Pts',(180.81371154728,3.37352225236713,339.860789871542));
#8452=CARTESIAN_POINT('Ctrl Pts',(180.806287422088,3.50279944612216,339.771067933054));
#8453=CARTESIAN_POINT('Ctrl Pts',(180.798863296897,3.62834758206704,339.6762873013));
#8454=CARTESIAN_POINT('Ctrl Pts',(180.791439171705,3.74976668902281,339.576808969183));
#8455=CARTESIAN_POINT('Ctrl Pts',(180.787582202509,3.81284614192855,339.525128151203));
#8456=CARTESIAN_POINT('Ctrl Pts',(180.783725233312,3.87481177557784,339.472180039224));
#8457=CARTESIAN_POINT('Ctrl Pts',(180.779868264116,3.93561160099101,339.418019000485));
#8458=CARTESIAN_POINT('Ctrl Pts',(180.772444286588,4.05264041677785,339.313768664529));
#8459=CARTESIAN_POINT('Ctrl Pts',(180.76502030906,4.16570068763168,339.20470789023));
#8460=CARTESIAN_POINT('Ctrl Pts',(180.757596331532,4.2743717010055,339.091170630045));
#8461=CARTESIAN_POINT('Ctrl Pts',(180.750181115384,4.38291446668223,338.97776736044));
#8462=CARTESIAN_POINT('Ctrl Pts',(180.742765899235,4.4870780301344,338.859898387656));
#8463=CARTESIAN_POINT('Ctrl Pts',(180.735350683087,4.58647512470673,338.737937465093));
#8464=CARTESIAN_POINT('Ctrl Pts',(180.727942601792,4.68577658030326,338.616093892215));
#8465=CARTESIAN_POINT('Ctrl Pts',(180.720534520497,4.78032046319195,338.490166495232));
#8466=CARTESIAN_POINT('Ctrl Pts',(180.713126439202,4.86975681774697,338.360565294486));
#8467=CARTESIAN_POINT('Ctrl Pts',(180.705723871847,4.95912660355486,338.231060557753));
#8468=CARTESIAN_POINT('Ctrl Pts',(180.698321304492,5.04339621951318,338.097887767828));
#8469=CARTESIAN_POINT('Ctrl Pts',(180.690918737137,5.12225650378825,337.961489299643));
#8470=CARTESIAN_POINT('Ctrl Pts',(180.683520067171,5.20107526878811,337.825162644102));
#8471=CARTESIAN_POINT('Ctrl Pts',(180.676121397205,5.27449018766949,337.685614014833));
#8472=CARTESIAN_POINT('Ctrl Pts',(180.668722727239,5.34223595584715,337.543313892258));
#8473=CARTESIAN_POINT('Ctrl Pts',(180.66132527778,5.4099705484838,337.40103724393));
#8474=CARTESIAN_POINT('Ctrl Pts',(180.653927828321,5.47203768621696,337.256010339773));
#8475=CARTESIAN_POINT('Ctrl Pts',(180.646530378861,5.52821844247713,337.108727439655));
#8476=CARTESIAN_POINT('Ctrl Pts',(180.639133250115,5.5843967630473,336.961450924918));
#8477=CARTESIAN_POINT('Ctrl Pts',(180.631736121368,5.63468907655627,336.811918957398));
#8478=CARTESIAN_POINT('Ctrl Pts',(180.624338992622,5.67892506300316,336.660644661357));
#8479=CARTESIAN_POINT('Ctrl Pts',(180.616940724875,5.72316786085186,336.50934707229));
#8480=CARTESIAN_POINT('Ctrl Pts',(180.609542457128,5.76135237006233,336.356306978751));
#8481=CARTESIAN_POINT('Ctrl Pts',(180.60214418938,5.79335853271784,336.202051360752));
#8482=CARTESIAN_POINT('Ctrl Pts',(180.594743322517,5.82537593959296,336.047741550562));
#8483=CARTESIAN_POINT('Ctrl Pts',(180.587342455653,5.85121060259573,335.892215730893));
#8484=CARTESIAN_POINT('Ctrl Pts',(180.579941588789,5.87079385213348,335.736009584348));
#8485=CARTESIAN_POINT('Ctrl Pts',(180.572532595026,5.89039860605714,335.579631907677));
#8486=CARTESIAN_POINT('Ctrl Pts',(180.565123601263,5.90373819092342,335.422572782731));
#8487=CARTESIAN_POINT('Ctrl Pts',(180.557714607501,5.91079589696642,335.265372242152));
#8488=CARTESIAN_POINT('Ctrl Pts',(180.550301049519,5.91785795082189,335.108074860126));
#8489=CARTESIAN_POINT('Ctrl Pts',(180.542887491537,5.91863041279232,334.950636261208));
#8490=CARTESIAN_POINT('Ctrl Pts',(180.535473933555,5.91314868001698,334.79359445135));
#8491=CARTESIAN_POINT('Ctrl Pts',(180.528049820983,5.9076591429672,334.63632906303));
#8492=CARTESIAN_POINT('Ctrl Pts',(180.520625708411,5.89589765589368,334.479461963158));
#8493=CARTESIAN_POINT('Ctrl Pts',(180.51320159584,5.87795133799407,334.323524848443));
#8494=CARTESIAN_POINT('Ctrl Pts',(180.509344473841,5.86862751148914,334.242509310247));
#8495=CARTESIAN_POINT('Ctrl Pts',(180.505487351842,5.85763510645131,334.16174461945));
#8496=CARTESIAN_POINT('Ctrl Pts',(180.501630229842,5.8449917094733,334.081303924745));
#8497=CARTESIAN_POINT('Ctrl Pts',(180.494206255989,5.82065640231641,333.926476150457));
#8498=CARTESIAN_POINT('Ctrl Pts',(180.486782282135,5.79012829443469,333.772382401797));
#8499=CARTESIAN_POINT('Ctrl Pts',(180.479358308281,5.75346054108848,333.619557185307));
#8500=CARTESIAN_POINT('Ctrl Pts',(180.471943095889,5.71683606148139,333.466912326705));
#8501=CARTESIAN_POINT('Ctrl Pts',(180.464527883496,5.6740864454201,333.315533379716));
#8502=CARTESIAN_POINT('Ctrl Pts',(180.457112671104,5.62531641712912,333.165948264176));
#8503=CARTESIAN_POINT('Ctrl Pts',(180.449704593642,5.57659331544779,333.016507079706));
#8504=CARTESIAN_POINT('Ctrl Pts',(180.442296516181,5.52186144893766,332.868856642942));
#8505=CARTESIAN_POINT('Ctrl Pts',(180.434888438719,5.46127623062284,332.723513124278));
#8506=CARTESIAN_POINT('Ctrl Pts',(180.427485875272,5.40073610737101,332.578277788358));
#8507=CARTESIAN_POINT('Ctrl Pts',(180.420083311824,5.33435145030333,332.435346294556));
#8508=CARTESIAN_POINT('Ctrl Pts',(180.412680748376,5.2623269559899,332.295218017887));
#8509=CARTESIAN_POINT('Ctrl Pts',(180.405282082387,5.19034038266485,332.155163518936));
#8510=CARTESIAN_POINT('Ctrl Pts',(180.397883416398,5.11272005597363,332.017909628877));
#8511=CARTESIAN_POINT('Ctrl Pts',(180.390484750409,5.02971804069313,331.883934051785));
#8512=CARTESIAN_POINT('Ctrl Pts',(180.383087305019,4.94672971871036,331.749980577378));
#8513=CARTESIAN_POINT('Ctrl Pts',(180.375689859629,4.85836166658881,331.619304659494));
#8514=CARTESIAN_POINT('Ctrl Pts',(180.368292414238,4.76491104358145,331.492357870413));
#8515=CARTESIAN_POINT('Ctrl Pts',(180.360895289618,4.67146447280226,331.365416586028));
#8516=CARTESIAN_POINT('Ctrl Pts',(180.353498164997,4.57293599060056,331.242204409484));
#8517=CARTESIAN_POINT('Ctrl Pts',(180.346101040377,4.46966492353788,331.123142247413));
#8518=CARTESIAN_POINT('Ctrl Pts',(180.338702776809,4.36637795566442,331.004061753151));
#8519=CARTESIAN_POINT('Ctrl Pts',(180.331304513242,4.25834719351518,330.889132827614));
#8520=CARTESIAN_POINT('Ctrl Pts',(180.323906249674,4.14595081497659,330.778741609153));
#8521=CARTESIAN_POINT('Ctrl Pts',(180.31650538704,4.03351495073477,330.668311609417));
#8522=CARTESIAN_POINT('Ctrl Pts',(180.309104524407,3.916710682658,330.56242275202));
#8523=CARTESIAN_POINT('Ctrl Pts',(180.301703661773,3.79595131603305,330.461422671276));
#8524=CARTESIAN_POINT('Ctrl Pts',(180.294294672295,3.67505934425942,330.360311682939));
#8525=CARTESIAN_POINT('Ctrl Pts',(180.286885682818,3.55020388704537,330.264100431691));
#8526=CARTESIAN_POINT('Ctrl Pts',(180.27947669334,3.42183002618858,330.173095211797));
#8527=CARTESIAN_POINT('Ctrl Pts',(180.272063139682,3.29337708281574,330.082033929698));
#8528=CARTESIAN_POINT('Ctrl Pts',(180.264649586023,3.16140172898108,329.996185272524));
#8529=CARTESIAN_POINT('Ctrl Pts',(180.257236032365,3.02637554025923,329.915810619989));
#8530=CARTESIAN_POINT('Ctrl Pts',(180.249811924139,2.89115711673847,329.835321539243));
#8531=CARTESIAN_POINT('Ctrl Pts',(180.242387815914,2.75287951081335,329.76032220529));
#8532=CARTESIAN_POINT('Ctrl Pts',(180.234963707688,2.61203698228368,329.691027089381));
#8533=CARTESIAN_POINT('Ctrl Pts',(180.231106536981,2.53886271559002,329.655025042663));
#8534=CARTESIAN_POINT('Ctrl Pts',(180.227249366275,2.46499640991772,329.62056192608));
#8535=CARTESIAN_POINT('Ctrl Pts',(180.223392195568,2.39050909743196,329.587662536612));
#8536=CARTESIAN_POINT('Ctrl Pts',(180.215968216101,2.24714176408294,329.52434037369));
#8537=CARTESIAN_POINT('Ctrl Pts',(180.208544236634,2.10104040776048,329.466623103546));
#8538=CARTESIAN_POINT('Ctrl Pts',(180.201120257167,1.95268327283604,329.41475527855));
#8539=CARTESIAN_POINT('Ctrl Pts',(180.193705039089,1.80450122119061,329.36294866523));
#8540=CARTESIAN_POINT('Ctrl Pts',(180.186289821012,1.65406903887216,329.316977878085));
#8541=CARTESIAN_POINT('Ctrl Pts',(180.178874602934,1.5018873381933,329.277040539557));
#8542=CARTESIAN_POINT('Ctrl Pts',(180.171466519721,1.34985206555842,329.237141628424));
#8543=CARTESIAN_POINT('Ctrl Pts',(180.164058436509,1.19607098441952,329.203264702665));
#8544=CARTESIAN_POINT('Ctrl Pts',(180.156650353296,1.04106225727171,329.175558401101));
#8545=CARTESIAN_POINT('Ctrl Pts',(180.149247784037,0.886168905573019,329.147872721776));
#8546=CARTESIAN_POINT('Ctrl Pts',(180.141845214778,0.730050093102275,329.126348586912));
#8547=CARTESIAN_POINT('Ctrl Pts',(180.134442645519,0.573236528843565,329.111084102783));
#8548=CARTESIAN_POINT('Ctrl Pts',(180.127043973665,0.416505525911596,329.095827655306));
#8549=CARTESIAN_POINT('Ctrl Pts',(180.119645301811,0.259080870188701,329.086824331117));
#8550=CARTESIAN_POINT('Ctrl Pts',(180.112246629957,0.101500680689412,329.084120676153));
#8551=CARTESIAN_POINT('Ctrl Pts',(180.104849178638,-0.0560535132966765,
329.081417467203));
#8552=CARTESIAN_POINT('Ctrl Pts',(180.09745172732,-0.213762817343169,329.085011871325));
#8553=CARTESIAN_POINT('Ctrl Pts',(180.090054276002,-0.371086684064145,329.094898372135));
#8554=CARTESIAN_POINT('Ctrl Pts',(180.082657145415,-0.52840372969085,329.104784444296));
#8555=CARTESIAN_POINT('Ctrl Pts',(180.075260014828,-0.685334998743519,329.120962047307));
#8556=CARTESIAN_POINT('Ctrl Pts',(180.067862884241,-0.841342912134583,329.143373610456));
#8557=CARTESIAN_POINT('Ctrl Pts',(180.060464614674,-0.997374846995422,329.165788624447));
#8558=CARTESIAN_POINT('Ctrl Pts',(180.053066345106,-1.15248277366524,329.194439456751));
#8559=CARTESIAN_POINT('Ctrl Pts',(180.045668075539,-1.30613732580632,329.229217050639));
#8560=CARTESIAN_POINT('Ctrl Pts',(180.038267206877,-1.45984585850437,329.264006862284));
#8561=CARTESIAN_POINT('Ctrl Pts',(180.030866338216,-1.61209963632193,329.304927638603));
#8562=CARTESIAN_POINT('Ctrl Pts',(180.023465469554,-1.76238266236629,329.351819946754));
#8563=CARTESIAN_POINT('Ctrl Pts',(180.016056474035,-1.91283071344254,329.398763747111));
#8564=CARTESIAN_POINT('Ctrl Pts',(180.008647478517,-2.06130333449412,329.451692063365));
#8565=CARTESIAN_POINT('Ctrl Pts',(180.001238482999,-2.20730209629018,329.510396369663));
#8566=CARTESIAN_POINT('Ctrl Pts',(179.993824923283,-2.35339079836859,329.569136839842));
#8567=CARTESIAN_POINT('Ctrl Pts',(179.986411363568,-2.49700226482026,329.633660237673));
#8568=CARTESIAN_POINT('Ctrl Pts',(179.978997803852,-2.63766149872952,329.703711452289));
#8569=CARTESIAN_POINT('Ctrl Pts',(179.971573689596,-2.77852098645556,329.773862397457));
#8570=CARTESIAN_POINT('Ctrl Pts',(179.964149575339,-2.91641952105426,329.849556697965));
#8571=CARTESIAN_POINT('Ctrl Pts',(179.956725461083,-3.05090927621345,329.930494782445));
#8572=CARTESIAN_POINT('Ctrl Pts',(179.952868361153,-3.12078164175435,329.972545088941));
#8573=CARTESIAN_POINT('Ctrl Pts',(179.949011261224,-3.18973442331561,330.016010096609));
#8574=CARTESIAN_POINT('Ctrl Pts',(179.945154161294,-3.25770833231832,330.06084349468));
#8575=CARTESIAN_POINT('Ctrl Pts',(179.937744834982,-3.38828334508317,330.14696656177));
#8576=CARTESIAN_POINT('Ctrl Pts',(179.93033550867,-3.51564163243029,330.238403655687));
#8577=CARTESIAN_POINT('Ctrl Pts',(179.922926182357,-3.63931980341617,330.334886718314));
#8578=CARTESIAN_POINT('Ctrl Pts',(179.915525610116,-3.7628518494352,330.431255786821));
#8579=CARTESIAN_POINT('Ctrl Pts',(179.908125037876,-3.88271214065072,330.532658729572));
#8580=CARTESIAN_POINT('Ctrl Pts',(179.900724465635,-3.99846455809472,330.638783227107));
#8581=CARTESIAN_POINT('Ctrl Pts',(179.893331006724,-4.11410571587917,330.744805719209));
#8582=CARTESIAN_POINT('Ctrl Pts',(179.885937547813,-4.22564658549171,330.855540480191));
#8583=CARTESIAN_POINT('Ctrl Pts',(179.878544088903,-4.33268267761745,330.970633873973));
#8584=CARTESIAN_POINT('Ctrl Pts',(179.871156108305,-4.43963945947479,331.085641987287));
#8585=CARTESIAN_POINT('Ctrl Pts',(179.863768127707,-4.54209785545166,331.205002029864));
#8586=CARTESIAN_POINT('Ctrl Pts',(179.856380147109,-4.63968903768038,331.328322427537));
#8587=CARTESIAN_POINT('Ctrl Pts',(179.848616474509,-4.7422429057455,331.457913887583));
#8588=CARTESIAN_POINT('Ctrl Pts',(179.840852801909,-4.83942128334582,331.591878732752));
#8589=CARTESIAN_POINT('Ctrl Pts',(179.833089129308,-4.9308424271595,331.729721186042));
#8590=CARTESIAN_POINT('Ctrl Pts',(179.825706198374,-5.01778014665303,331.860803647259));
#8591=CARTESIAN_POINT('Ctrl Pts',(179.818323267439,-5.099511607423,331.99539212213));
#8592=CARTESIAN_POINT('Ctrl Pts',(179.810940336504,-5.17575203052851,332.133029215185));
#8593=CARTESIAN_POINT('Ctrl Pts',(179.803557579899,-5.25199065340122,332.270663058275));
#8594=CARTESIAN_POINT('Ctrl Pts',(179.796174823294,-5.32273831456115,332.411345048581));
#8595=CARTESIAN_POINT('Ctrl Pts',(179.788792066689,-5.38775575268492,332.554592362834));
#8596=CARTESIAN_POINT('Ctrl Pts',(179.781408012026,-5.45278462237157,332.697864863263));
#8597=CARTESIAN_POINT('Ctrl Pts',(179.774023957363,-5.51208110828031,332.843703244236));
#8598=CARTESIAN_POINT('Ctrl Pts',(179.766639902699,-5.56545380867749,332.991604006682));
#8599=CARTESIAN_POINT('Ctrl Pts',(179.759253077072,-5.61884653788094,333.13956027083));
#8600=CARTESIAN_POINT('Ctrl Pts',(179.751866251445,-5.66631092890013,333.289580104872));
#8601=CARTESIAN_POINT('Ctrl Pts',(179.744479425819,-5.70770527279833,333.441144303866));
#8602=CARTESIAN_POINT('Ctrl Pts',(179.737084455399,-5.74914525854128,333.592875619161));
#8603=CARTESIAN_POINT('Ctrl Pts',(179.729689484979,-5.7845017345088,333.746154337788));
#8604=CARTESIAN_POINT('Ctrl Pts',(179.72229451456,-5.81368385881868,333.900449840975));
#8605=CARTESIAN_POINT('Ctrl Pts',(179.714894800955,-5.84288470074761,334.05484431038));
#8606=CARTESIAN_POINT('Ctrl Pts',(179.707495087349,-5.86590324605129,334.210256493988));
#8607=CARTESIAN_POINT('Ctrl Pts',(179.700095373744,-5.8827005326052,334.366150643933));
#8608=CARTESIAN_POINT('Ctrl Pts',(179.692685469894,-5.89952095092716,334.522259477797));
#8609=CARTESIAN_POINT('Ctrl Pts',(179.685275566044,-5.91010297967495,334.678851230667));
#8610=CARTESIAN_POINT('Ctrl Pts',(179.677865662194,-5.91445973306567,334.835389464357));
#8611=CARTESIAN_POINT('Ctrl Pts',(179.675261109697,-5.91599111500422,334.890412047061));
#8612=CARTESIAN_POINT('Ctrl Pts',(179.6726565572,-5.91675383644239,334.945428057878));
#8613=CARTESIAN_POINT('Ctrl Pts',(179.670052004703,-5.91674998548957,335.000414378067));
#8614=CARTESIAN_POINT('',(177.920052775238,-5.91497190102853,334.994674821255));
#8615=CARTESIAN_POINT('Ctrl Pts',(179.670052004703,-5.92646392270013,335.00041505838));
#8616=CARTESIAN_POINT('Ctrl Pts',(179.669006712142,-5.92648621669284,335.022519108687));
#8617=CARTESIAN_POINT('Ctrl Pts',(179.667961419581,-5.92637327756805,335.044622924713));
#8618=CARTESIAN_POINT('Ctrl Pts',(179.574170115596,-5.90404367840924,337.027801861348));
#8619=CARTESIAN_POINT('Ctrl Pts',(179.388678092746,-3.71978762975183,340.92585884392));
#8620=CARTESIAN_POINT('Ctrl Pts',(179.110440058472,2.97019053767725,341.334871015977));
#8621=CARTESIAN_POINT('Ctrl Pts',(178.832202024198,6.93446874656139,335.930465615495));
#8622=CARTESIAN_POINT('Ctrl Pts',(178.553963989924,4.53508730863143,329.672185623518));
#8623=CARTESIAN_POINT('Ctrl Pts',(178.27572595565,-2.02607679839931,328.303162262213));
#8624=CARTESIAN_POINT('Ctrl Pts',(178.064422347311,-5.59683481069391,331.930651892861));
#8625=CARTESIAN_POINT('Ctrl Pts',(177.945864750396,-5.91882038961358,334.445878104145));
#8626=CARTESIAN_POINT('Ctrl Pts',(177.920053164906,-5.91407390179608,334.994667342421));
#8627=CARTESIAN_POINT('',(176.170051188577,-5.91178907071594,335.002177354139));
#8628=CARTESIAN_POINT('Ctrl Pts',(177.920052004703,-5.91674761691405,334.994689610001));
#8629=CARTESIAN_POINT('Ctrl Pts',(177.912714213781,-5.91688770210566,335.150770184837));
#8630=CARTESIAN_POINT('Ctrl Pts',(177.905376422858,-5.91084758222949,335.306982769653));
#8631=CARTESIAN_POINT('Ctrl Pts',(177.898038631936,-5.89862280926592,335.462795328961));
#8632=CARTESIAN_POINT('Ctrl Pts',(177.890589100901,-5.88621187707302,335.620980606849));
#8633=CARTESIAN_POINT('Ctrl Pts',(177.883139569866,-5.86742635957227,335.778753179454));
#8634=CARTESIAN_POINT('Ctrl Pts',(177.875690038832,-5.84231658479985,335.935557312767));
#8635=CARTESIAN_POINT('Ctrl Pts',(177.868356772245,-5.81759869699262,336.089914212026));
#8636=CARTESIAN_POINT('Ctrl Pts',(177.861023505659,-5.7867525997992,336.243332296058));
#8637=CARTESIAN_POINT('Ctrl Pts',(177.853690239072,-5.74987839465665,336.395288145567));
#8638=CARTESIAN_POINT('Ctrl Pts',(177.846356943828,-5.71300404541406,336.547244588902));
#8639=CARTESIAN_POINT('Ctrl Pts',(177.839023648584,-5.67010163064186,336.697738416624));
#8640=CARTESIAN_POINT('Ctrl Pts',(177.83169035334,-5.62132192356637,336.846258485189));
#8641=CARTESIAN_POINT('Ctrl Pts',(177.824355520482,-5.57253198857071,336.994809694806));
#8642=CARTESIAN_POINT('Ctrl Pts',(177.817020687624,-5.51786242740262,337.141385960352));
#8643=CARTESIAN_POINT('Ctrl Pts',(177.809685854766,-5.45751314636585,337.285493561519));
#8644=CARTESIAN_POINT('Ctrl Pts',(177.802149524128,-5.39550598894267,337.433559993428));
#8645=CARTESIAN_POINT('Ctrl Pts',(177.794613193489,-5.32750272876749,337.579019778803));
#8646=CARTESIAN_POINT('Ctrl Pts',(177.787076862851,-5.25377157600491,337.721362671469));
#8647=CARTESIAN_POINT('Ctrl Pts',(177.779730623447,-5.1819001672736,337.860115204631));
#8648=CARTESIAN_POINT('Ctrl Pts',(177.772384384044,-5.10458658987453,337.995905893275));
#8649=CARTESIAN_POINT('Ctrl Pts',(177.765038144641,-5.02212389008489,338.128290618715));
#8650=CARTESIAN_POINT('Ctrl Pts',(177.757406768385,-4.93646048399682,338.265813723393));
#8651=CARTESIAN_POINT('Ctrl Pts',(177.749775392128,-4.84524047988318,338.399660775208));
#8652=CARTESIAN_POINT('Ctrl Pts',(177.742144015872,-4.74883867014821,338.529371310503));
#8653=CARTESIAN_POINT('Ctrl Pts',(177.734512639616,-4.65243686041325,338.659081845799));
#8654=CARTESIAN_POINT('Ctrl Pts',(177.726881263359,-4.55085358558808,338.784655558879));
#8655=CARTESIAN_POINT('Ctrl Pts',(177.719249887103,-4.44450602610207,338.905674941216));
#8656=CARTESIAN_POINT('Ctrl Pts',(177.711825909658,-4.34104868676153,339.023405365551));
#8657=CARTESIAN_POINT('Ctrl Pts',(177.704401932212,-4.23275420849354,339.137199834385));
#8658=CARTESIAN_POINT('Ctrl Pts',(177.696977954767,-4.11995369376139,339.246635388606));
#8659=CARTESIAN_POINT('Ctrl Pts',(177.689562738732,-4.00728630060703,339.35594179241));
#8660=CARTESIAN_POINT('Ctrl Pts',(177.682147522697,-3.89012372141636,339.460899263816));
#8661=CARTESIAN_POINT('Ctrl Pts',(177.674732306662,-3.76883708465367,339.561118019942));
#8662=CARTESIAN_POINT('Ctrl Pts',(177.66732422551,-3.64766714928069,339.661240346087));
#8663=CARTESIAN_POINT('Ctrl Pts',(177.659916144359,-3.52238134195654,339.756632798064));
#8664=CARTESIAN_POINT('Ctrl Pts',(177.652508063207,-3.39338730933572,339.846942658144));
#8665=CARTESIAN_POINT('Ctrl Pts',(177.645105496026,-3.26448928932791,339.937185298948));
#8666=CARTESIAN_POINT('Ctrl Pts',(177.637702928844,-3.13188884420546,340.022352667362));
#8667=CARTESIAN_POINT('Ctrl Pts',(177.630300361662,-2.99602625007755,340.102132619929));
#8668=CARTESIAN_POINT('Ctrl Pts',(177.6229016919,-2.86023518700992,340.181870568701));
#8669=CARTESIAN_POINT('Ctrl Pts',(177.615503022138,-2.72118571647128,340.256226562082));
#8670=CARTESIAN_POINT('Ctrl Pts',(177.608104352375,-2.57934651572282,340.324932122979));
#8671=CARTESIAN_POINT('Ctrl Pts',(177.600706903163,-2.43753071403716,340.393626349591));
#8672=CARTESIAN_POINT('Ctrl Pts',(177.593309453952,-2.29292643108194,340.456671831188));
#8673=CARTESIAN_POINT('Ctrl Pts',(177.58591200474,-2.14602643635296,340.513846306978));
#8674=CARTESIAN_POINT('Ctrl Pts',(177.578514876269,-1.99913281095101,340.571018303783));
#8675=CARTESIAN_POINT('Ctrl Pts',(177.571117747798,-1.84994401948705,340.622319665558));
#8676=CARTESIAN_POINT('Ctrl Pts',(177.563720619326,-1.69897202381249,340.667576609522));
#8677=CARTESIAN_POINT('Ctrl Pts',(177.556322351882,-1.54797678221842,340.712840521926));
#8678=CARTESIAN_POINT('Ctrl Pts',(177.548924084438,-1.39519814722675,340.752058056221));
#8679=CARTESIAN_POINT('Ctrl Pts',(177.541525816993,-1.24116227569561,340.785105596952));
#8680=CARTESIAN_POINT('Ctrl Pts',(177.53412495046,-1.08707228974226,340.818164747632));
#8681=CARTESIAN_POINT('Ctrl Pts',(177.526724083926,-0.931724552542117,340.845049510853));
#8682=CARTESIAN_POINT('Ctrl Pts',(177.519323217392,-0.775654270532592,340.865687599515));
#8683=CARTESIAN_POINT('Ctrl Pts',(177.511914224,-0.619412608432403,340.886348350772));
#8684=CARTESIAN_POINT('Ctrl Pts',(177.504505230607,-0.462447187225275,340.900748679835));
#8685=CARTESIAN_POINT('Ctrl Pts',(177.497096237215,-0.305297914327727,340.908868228858));
#8686=CARTESIAN_POINT('Ctrl Pts',(177.489682679627,-0.148051832057079,340.916992779803));
#8687=CARTESIAN_POINT('Ctrl Pts',(177.482269122039,0.00937795527349783,
340.918828836519));
#8688=CARTESIAN_POINT('Ctrl Pts',(177.47485556445,0.166453214854142,340.914408160566));
#8689=CARTESIAN_POINT('Ctrl Pts',(177.467431452306,0.323752099822014,340.909981190971));
#8690=CARTESIAN_POINT('Ctrl Pts',(177.460007340161,0.48069507764046,340.899279723761));
#8691=CARTESIAN_POINT('Ctrl Pts',(177.452583228017,0.636749875160684,340.882387284002));
#8692=CARTESIAN_POINT('Ctrl Pts',(177.448726102954,0.717826623318829,340.873610981664));
#8693=CARTESIAN_POINT('Ctrl Pts',(177.444868977892,0.798663802018155,340.863164441332));
#8694=CARTESIAN_POINT('Ctrl Pts',(177.441011852829,0.879188145233416,340.851064755049));
#8695=CARTESIAN_POINT('Ctrl Pts',(177.433587875393,1.03417687320687,340.827775959252));
#8696=CARTESIAN_POINT('Ctrl Pts',(177.426163897958,1.18847342566624,340.798289538784));
#8697=CARTESIAN_POINT('Ctrl Pts',(177.418739920522,1.34154294873124,340.762655037325));
#8698=CARTESIAN_POINT('Ctrl Pts',(177.411324704496,1.49443182672829,340.72706258994));
#8699=CARTESIAN_POINT('Ctrl Pts',(177.403909488471,1.64609619779929,340.685336587869));
#8700=CARTESIAN_POINT('Ctrl Pts',(177.396494272445,1.79600744629644,340.637578187072));
#8701=CARTESIAN_POINT('Ctrl Pts',(177.389086191303,1.94577445094465,340.589865739167));
#8702=CARTESIAN_POINT('Ctrl Pts',(177.381678110161,2.09379133798909,340.536132560432));
#8703=CARTESIAN_POINT('Ctrl Pts',(177.374270029019,2.23954089857283,340.476530573832));
#8704=CARTESIAN_POINT('Ctrl Pts',(177.366867461847,2.38518197509642,340.41697295008));
#8705=CARTESIAN_POINT('Ctrl Pts',(177.359464894675,2.52855874147771,340.351555356964));
#8706=CARTESIAN_POINT('Ctrl Pts',(177.352062327504,2.66917045095894,340.280479113322));
#8707=CARTESIAN_POINT('Ctrl Pts',(177.344663657751,2.80970812898883,340.209440291012));
#8708=CARTESIAN_POINT('Ctrl Pts',(177.337264987998,2.94748331717329,340.132748919477));
#8709=CARTESIAN_POINT('Ctrl Pts',(177.329866318246,3.08201661923865,340.050653831064));
#8710=CARTESIAN_POINT('Ctrl Pts',(177.322468869044,3.21652772748755,339.96857228579));
#8711=CARTESIAN_POINT('Ctrl Pts',(177.315071419842,3.34779769277276,339.881088987085));
#8712=CARTESIAN_POINT('Ctrl Pts',(177.30767397064,3.47537294540474,339.788498037261));
#8713=CARTESIAN_POINT('Ctrl Pts',(177.300276842179,3.60294266659611,339.695911102019));
#8714=CARTESIAN_POINT('Ctrl Pts',(177.292879713718,3.72681769161282,339.598217175208));
#8715=CARTESIAN_POINT('Ctrl Pts',(177.285482585256,3.84657483087278,339.495752732635));
#8716=CARTESIAN_POINT('Ctrl Pts',(177.278084317822,3.96635040974271,339.393272513096));
#8717=CARTESIAN_POINT('Ctrl Pts',(177.270686050387,4.08200655677947,339.286020557874));
#8718=CARTESIAN_POINT('Ctrl Pts',(177.263287782953,4.19315458744328,339.174372428079));
#8719=CARTESIAN_POINT('Ctrl Pts',(177.255886916429,4.30434166557978,339.062685075121));
#8720=CARTESIAN_POINT('Ctrl Pts',(177.248486049906,4.411017210961,338.946598736973));
#8721=CARTESIAN_POINT('Ctrl Pts',(177.241085183382,4.51283080491,338.826524361448));
#8722=CARTESIAN_POINT('Ctrl Pts',(177.233676189999,4.61475619991864,338.70631813278));
#8723=CARTESIAN_POINT('Ctrl Pts',(177.226267196617,4.71180873994169,338.582115405971));
#8724=CARTESIAN_POINT('Ctrl Pts',(177.218858203234,4.8036791307486,338.454359183888));
#8725=CARTESIAN_POINT('Ctrl Pts',(177.211444645656,4.89560611688486,338.326524259565));
#8726=CARTESIAN_POINT('Ctrl Pts',(177.204031088078,4.98234438742863,338.195131788682));
#8727=CARTESIAN_POINT('Ctrl Pts',(177.1966175305,5.06362938269769,338.060651570692));
#8728=CARTESIAN_POINT('Ctrl Pts',(177.189193418365,5.14503010203933,337.925979895491));
#8729=CARTESIAN_POINT('Ctrl Pts',(177.18176930623,5.22096186071101,337.788212019519));
#8730=CARTESIAN_POINT('Ctrl Pts',(177.174345194096,5.29120685317979,337.647840742825));
#8731=CARTESIAN_POINT('Ctrl Pts',(177.170488068916,5.3277019551287,337.574912212639));
#8732=CARTESIAN_POINT('Ctrl Pts',(177.166630943735,5.36266287344064,337.501281279861));
#8733=CARTESIAN_POINT('Ctrl Pts',(177.162773818555,5.39606433272757,337.427018804947));
#8734=CARTESIAN_POINT('Ctrl Pts',(177.155349841118,5.46035358146345,337.284082573314));
#8735=CARTESIAN_POINT('Ctrl Pts',(177.147925863681,5.51905653950395,337.138374516508));
#8736=CARTESIAN_POINT('Ctrl Pts',(177.140501886244,5.57192542906149,336.990371215497));
#8737=CARTESIAN_POINT('Ctrl Pts',(177.133086670217,5.62473192537479,336.842542580649));
#8738=CARTESIAN_POINT('Ctrl Pts',(177.12567145419,5.67171793373778,336.692424441415));
#8739=CARTESIAN_POINT('Ctrl Pts',(177.118256238164,5.71268245409505,336.540516063264));
#8740=CARTESIAN_POINT('Ctrl Pts',(177.11084815702,5.75360755859698,336.38875385059));
#8741=CARTESIAN_POINT('Ctrl Pts',(177.103440075877,5.78852261303763,336.235205186225));
#8742=CARTESIAN_POINT('Ctrl Pts',(177.096031994734,5.81727548129005,336.080387216363));
#8743=CARTESIAN_POINT('Ctrl Pts',(177.088629427561,5.84600694825745,335.925684480345));
#8744=CARTESIAN_POINT('Ctrl Pts',(177.081226860388,5.86858529382467,335.769714685365));
#8745=CARTESIAN_POINT('Ctrl Pts',(177.073824293215,5.88490882849242,335.613007865228));
#8746=CARTESIAN_POINT('Ctrl Pts',(177.066425623461,5.90122376889044,335.456383550549));
#8747=CARTESIAN_POINT('Ctrl Pts',(177.059026953707,5.91129041828467,335.299023353787));
#8748=CARTESIAN_POINT('Ctrl Pts',(177.051628283953,5.91505859627196,335.141465066957));
#8749=CARTESIAN_POINT('Ctrl Pts',(177.04423083475,5.9188261526269,334.983932772352));
#8750=CARTESIAN_POINT('Ctrl Pts',(177.036833385547,5.9162972908433,334.826202825278));
#8751=CARTESIAN_POINT('Ctrl Pts',(177.029435936344,5.90747387524594,334.6688157978));
#8752=CARTESIAN_POINT('Ctrl Pts',(177.022038807882,5.89865084221655,334.51143559435));
#8753=CARTESIAN_POINT('Ctrl Pts',(177.014641679419,5.8835338189202,334.35439865356));
#8754=CARTESIAN_POINT('Ctrl Pts',(177.007244550957,5.86217674287609,334.198242930943));
#8755=CARTESIAN_POINT('Ctrl Pts',(176.999846283521,5.84081637837532,334.042063164243));
#8756=CARTESIAN_POINT('Ctrl Pts',(176.992448016085,5.81321409859842,333.886765255675));
#8757=CARTESIAN_POINT('Ctrl Pts',(176.98504974865,5.77947538138788,333.732879296029));
#8758=CARTESIAN_POINT('Ctrl Pts',(176.977648882125,5.74572481141134,333.578939274628));
#8759=CARTESIAN_POINT('Ctrl Pts',(176.9702480156,5.70583359169296,333.426412554071));
#8760=CARTESIAN_POINT('Ctrl Pts',(176.962847149075,5.65995766536272,333.27581619634));
#8761=CARTESIAN_POINT('Ctrl Pts',(176.955438155691,5.61403136287951,333.125054469412));
#8762=CARTESIAN_POINT('Ctrl Pts',(176.948029162308,5.56210733841011,332.976227695737));
#8763=CARTESIAN_POINT('Ctrl Pts',(176.940620168924,5.50439074565899,332.829835701703));
#8764=CARTESIAN_POINT('Ctrl Pts',(176.933206611345,5.44663859749561,332.68335352515));
#8765=CARTESIAN_POINT('Ctrl Pts',(176.925793053765,5.38308692079485,332.53930945766));
#8766=CARTESIAN_POINT('Ctrl Pts',(176.918379496186,5.31398761151646,332.398180208556));
#8767=CARTESIAN_POINT('Ctrl Pts',(176.91095538405,5.24478992672144,332.25685003613));
#8768=CARTESIAN_POINT('Ctrl Pts',(176.903531271915,5.17002901221364,332.11844329751));
#8769=CARTESIAN_POINT('Ctrl Pts',(176.896107159779,5.09000140699761,331.9834098324));
#8770=CARTESIAN_POINT('Ctrl Pts',(176.892250034613,5.04842384399744,331.913254510526));
#8771=CARTESIAN_POINT('Ctrl Pts',(176.888392909447,5.0054253808852,331.844009206049));
#8772=CARTESIAN_POINT('Ctrl Pts',(176.884535784281,4.96105192776692,331.775733520241));
#8773=CARTESIAN_POINT('Ctrl Pts',(176.877111806842,4.87564440255624,331.644320322773));
#8774=CARTESIAN_POINT('Ctrl Pts',(176.869687829403,4.78488292798476,331.516104762685));
#8775=CARTESIAN_POINT('Ctrl Pts',(176.862263851964,4.68903418437665,331.391553106911));
#8776=CARTESIAN_POINT('Ctrl Pts',(176.854848635935,4.59329855670691,331.267148440829));
#8777=CARTESIAN_POINT('Ctrl Pts',(176.847433419907,4.49248783594312,331.146399365049));
#8778=CARTESIAN_POINT('Ctrl Pts',(176.840018203878,4.38691309240689,331.029745085996));
#8779=CARTESIAN_POINT('Ctrl Pts',(176.832610122733,4.28143993235722,330.913203051104));
#8780=CARTESIAN_POINT('Ctrl Pts',(176.825202041588,4.17121212402109,330.800748244013));
#8781=CARTESIAN_POINT('Ctrl Pts',(176.817793960442,4.0565822170802,330.692788456719));
#8782=CARTESIAN_POINT('Ctrl Pts',(176.810391393267,3.94203763127248,330.584909025867));
#8783=CARTESIAN_POINT('Ctrl Pts',(176.802988826092,3.82309774149546,330.481518207766));
#8784=CARTESIAN_POINT('Ctrl Pts',(176.795586258917,3.7001532344614,330.382988346993));
#8785=CARTESIAN_POINT('Ctrl Pts',(176.788187589161,3.57727345717211,330.284510361759));
#8786=CARTESIAN_POINT('Ctrl Pts',(176.780788919405,3.45039355215038,330.190888469716));
#8787=CARTESIAN_POINT('Ctrl Pts',(176.773390249649,3.31993860467935,330.102455898753));
#8788=CARTESIAN_POINT('Ctrl Pts',(176.765992800444,3.18950517822406,330.014037916418));
#8789=CARTESIAN_POINT('Ctrl Pts',(176.758595351239,3.05549818844676,329.930807765335));
#8790=CARTESIAN_POINT('Ctrl Pts',(176.751197902034,2.91837322282364,329.853056412316));
#8791=CARTESIAN_POINT('Ctrl Pts',(176.743800773569,2.78125420269984,329.77530843046));
#8792=CARTESIAN_POINT('Ctrl Pts',(176.736403645105,2.64101780018663,329.70303895842));
#8793=CARTESIAN_POINT('Ctrl Pts',(176.72900651664,2.49814558223962,329.636493757584));
#8794=CARTESIAN_POINT('Ctrl Pts',(176.721608249202,2.35525136553741,329.569938310448));
#8795=CARTESIAN_POINT('Ctrl Pts',(176.714209981765,2.20972086363594,329.509109047073));
#8796=CARTESIAN_POINT('Ctrl Pts',(176.706811714327,2.06205692130117,329.454204131433));
#8797=CARTESIAN_POINT('Ctrl Pts',(176.6994108478,1.91434110307088,329.399279927119));
#8798=CARTESIAN_POINT('Ctrl Pts',(176.692009981273,1.76449070174616,329.350284344364));
#8799=CARTESIAN_POINT('Ctrl Pts',(176.684609114746,1.61302491555565,329.307366059169));
#8800=CARTESIAN_POINT('Ctrl Pts',(176.67720012136,1.46139280545063,329.264400645595));
#8801=CARTESIAN_POINT('Ctrl Pts',(176.669791127974,1.30814212730147,329.22752595863));
#8802=CARTESIAN_POINT('Ctrl Pts',(176.662382134588,1.15380421622146,329.196839964887));
#8803=CARTESIAN_POINT('Ctrl Pts',(176.654968577007,0.999371227664755,329.166135067514));
#8804=CARTESIAN_POINT('Ctrl Pts',(176.647555019426,0.843850039366241,329.141626518131));
#8805=CARTESIAN_POINT('Ctrl Pts',(176.640141461844,0.687777841723747,329.12336046682));
#8806=CARTESIAN_POINT('Ctrl Pts',(176.632717349706,0.531483446735364,329.105068410441));
#8807=CARTESIAN_POINT('Ctrl Pts',(176.625293237569,0.3746368467885,329.093036630397));
#8808=CARTESIAN_POINT('Ctrl Pts',(176.617869125431,0.217776795958029,329.087259194786));
#8809=CARTESIAN_POINT('Ctrl Pts',(176.61401200029,0.136281684561534,329.084257584394));
#8810=CARTESIAN_POINT('Ctrl Pts',(176.610154875148,0.0547828956273552,329.082943301829));
#8811=CARTESIAN_POINT('Ctrl Pts',(176.606297750007,-0.0266446062728537,
329.08330999397));
#8812=CARTESIAN_POINT('Ctrl Pts',(176.59887377257,-0.183371680141186,329.08401578237));
#8813=CARTESIAN_POINT('Ctrl Pts',(176.591449795132,-0.3403071217284,329.090954246073));
#8814=CARTESIAN_POINT('Ctrl Pts',(176.584025817694,-0.496914521196266,329.104153451698));
#8815=CARTESIAN_POINT('Ctrl Pts',(176.576610601667,-0.65333710036991,329.117337080274));
#8816=CARTESIAN_POINT('Ctrl Pts',(176.56919538564,-0.80943203975444,329.136766712572));
#8817=CARTESIAN_POINT('Ctrl Pts',(176.561780169613,-0.96466166329435,329.162418442722));
#8818=CARTESIAN_POINT('Ctrl Pts',(176.554372088469,-1.1197419256715,329.188045490907));
#8819=CARTESIAN_POINT('Ctrl Pts',(176.546964007325,-1.27395816400389,329.219882657757));
#8820=CARTESIAN_POINT('Ctrl Pts',(176.539555926182,-1.4267766724408,329.257854156373));
#8821=CARTESIAN_POINT('Ctrl Pts',(176.532153359008,-1.57948143527166,329.29579739211));
#8822=CARTESIAN_POINT('Ctrl Pts',(176.524750791834,-1.73079017906078,329.339865778638));
#8823=CARTESIAN_POINT('Ctrl Pts',(176.517348224661,-1.88017836831403,329.389932276182));
#8824=CARTESIAN_POINT('Ctrl Pts',(176.509949554906,-2.02948790533859,329.439972413934));
#8825=CARTESIAN_POINT('Ctrl Pts',(176.502550885152,-2.17687854864409,329.496004255101));
#8826=CARTESIAN_POINT('Ctrl Pts',(176.495152215398,-2.32184004175152,329.557850665131));
#8827=CARTESIAN_POINT('Ctrl Pts',(176.487754766194,-2.46677762071338,329.619686872423));
#8828=CARTESIAN_POINT('Ctrl Pts',(176.48035731699,-2.60928650186431,329.687335598518));
#8829=CARTESIAN_POINT('Ctrl Pts',(176.472959867787,-2.74887546047948,329.760571189025));
#8830=CARTESIAN_POINT('Ctrl Pts',(176.465562739324,-2.88845836676082,329.833803604165));
#8831=CARTESIAN_POINT('Ctrl Pts',(176.458165610861,-3.02512127174652,329.912622228679));
#8832=CARTESIAN_POINT('Ctrl Pts',(176.450768482397,-3.15839690593207,329.996755098229));
#8833=CARTESIAN_POINT('Ctrl Pts',(176.443370214961,-3.29169306123805,330.080900922141));
#8834=CARTESIAN_POINT('Ctrl Pts',(176.435971947525,-3.42160059164968,330.170362421119));
#8835=CARTESIAN_POINT('Ctrl Pts',(176.428573680089,-3.54768073869756,330.26482398017));
#8836=CARTESIAN_POINT('Ctrl Pts',(176.421172813563,-3.67380517902699,330.35931872456));
#8837=CARTESIAN_POINT('Ctrl Pts',(176.413771947038,-3.79609926040344,330.458816802721));
#8838=CARTESIAN_POINT('Ctrl Pts',(176.406371080513,-3.91415699005094,330.562962066904));
#8839=CARTESIAN_POINT('Ctrl Pts',(176.398962087128,-4.03234435837296,330.667221692543));
#8840=CARTESIAN_POINT('Ctrl Pts',(176.391553093744,-4.14628580479258,330.776138448235));
#8841=CARTESIAN_POINT('Ctrl Pts',(176.38414410036,-4.25561141117888,330.889318538302));
#8842=CARTESIAN_POINT('Ctrl Pts',(176.37673054278,-4.36500436590949,331.002568351209));
#8843=CARTESIAN_POINT('Ctrl Pts',(176.3693169852,-4.46977556674499,331.120086453936));
#8844=CARTESIAN_POINT('Ctrl Pts',(176.36190342762,-4.56959550054893,331.241446086077));
#8845=CARTESIAN_POINT('Ctrl Pts',(176.354479315484,-4.66955754630326,331.362978495873));
#8846=CARTESIAN_POINT('Ctrl Pts',(176.347055203347,-4.76455402192201,331.488363061336));
#8847=CARTESIAN_POINT('Ctrl Pts',(176.339631091211,-4.85429836492277,331.617143522582));
#8848=CARTESIAN_POINT('Ctrl Pts',(176.335773966052,-4.90092416433609,331.684050157069));
#8849=CARTESIAN_POINT('Ctrl Pts',(176.331916840892,-4.94613304389588,331.75187299399));
#8850=CARTESIAN_POINT('Ctrl Pts',(176.328059715733,-4.98988977844441,331.820545555999));
#8851=CARTESIAN_POINT('Ctrl Pts',(176.320453925922,-5.07617282917936,331.955959640553));
#8852=CARTESIAN_POINT('Ctrl Pts',(176.31284813611,-5.15705683796547,332.095071661292));
#8853=CARTESIAN_POINT('Ctrl Pts',(176.305242346299,-5.23221784202617,332.237423844293));
#8854=CARTESIAN_POINT('Ctrl Pts',(176.297646843112,-5.30727719286556,332.379583499823));
#8855=CARTESIAN_POINT('Ctrl Pts',(176.290051339925,-5.3766287945708,332.524974283587));
#8856=CARTESIAN_POINT('Ctrl Pts',(176.282455836739,-5.43999184926805,332.673109533649));
#8857=CARTESIAN_POINT('Ctrl Pts',(176.274869399746,-5.50327927214354,332.821067965548));
#8858=CARTESIAN_POINT('Ctrl Pts',(176.267282962753,-5.560592251189,332.971764019555));
#8859=CARTESIAN_POINT('Ctrl Pts',(176.25969652576,-5.61169576389038,333.124686368621));
#8860=CARTESIAN_POINT('Ctrl Pts',(176.252120196404,-5.66273118985307,333.277404974667));
#8861=CARTESIAN_POINT('Ctrl Pts',(176.244543867048,-5.70757353449418,333.432343632674));
#8862=CARTESIAN_POINT('Ctrl Pts',(176.236967537693,-5.74603589713926,333.588971286158));
#8863=CARTESIAN_POINT('Ctrl Pts',(176.22939711922,-5.78446825230645,333.745476742238));
#8864=CARTESIAN_POINT('Ctrl Pts',(176.221826700747,-5.81653045695088,333.903668231897));
#8865=CARTESIAN_POINT('Ctrl Pts',(176.214256282275,-5.8420852177126,334.062999001343));
#8866=CARTESIAN_POINT('Ctrl Pts',(176.206691491682,-5.86762098096063,334.222211323644));
#8867=CARTESIAN_POINT('Ctrl Pts',(176.19912670109,-5.88665888814513,334.382560894078));
#8868=CARTESIAN_POINT('Ctrl Pts',(176.191561910497,-5.89911259517965,334.543490249948));
#8869=CARTESIAN_POINT('Ctrl Pts',(176.184391941899,-5.91091631760589,334.696020371433));
#8870=CARTESIAN_POINT('Ctrl Pts',(176.177221973301,-5.91680553894543,334.849070998502));
#8871=CARTESIAN_POINT('Ctrl Pts',(176.170052004703,-5.91674960508396,335.002161767525));
#8872=CARTESIAN_POINT('',(174.420052004703,-5.922005427706,335.004419719925));
#8873=CARTESIAN_POINT('Ctrl Pts',(176.170050516938,-5.90770675093187,335.002190181294));
#8874=CARTESIAN_POINT('Ctrl Pts',(176.129974238446,-5.91049512676808,335.856578754585));
#8875=CARTESIAN_POINT('Ctrl Pts',(175.997151948527,-5.33684541281739,338.684647950317));
#8876=CARTESIAN_POINT('Ctrl Pts',(175.771583647186,-0.977291647241818,341.928024534987));
#8877=CARTESIAN_POINT('Ctrl Pts',(175.493345612911,5.29705504710014,339.570977001614));
#8878=CARTESIAN_POINT('Ctrl Pts',(175.215107578637,6.71037250910805,333.019211341358));
#8879=CARTESIAN_POINT('Ctrl Pts',(174.936869544363,1.96568016445112,328.285186196753));
#8880=CARTESIAN_POINT('Ctrl Pts',(174.671851019719,-4.27175548752083,329.64539726177));
#8881=CARTESIAN_POINT('Ctrl Pts',(174.499578506499,-5.90796248829746,333.31938805982));
#8882=CARTESIAN_POINT('Ctrl Pts',(174.420052004703,-5.922005427706,335.004419719925));
#8883=CARTESIAN_POINT('',(172.670052004703,-5.92176215774818,334.995489375811));
#8884=CARTESIAN_POINT('Ctrl Pts',(174.420052004703,-5.922005427706,335.004419719925));
#8885=CARTESIAN_POINT('Ctrl Pts',(174.406832495074,-5.9243397536042,335.284518702699));
#8886=CARTESIAN_POINT('Ctrl Pts',(174.300866974022,-5.77886390257711,337.527311927912));
#8887=CARTESIAN_POINT('Ctrl Pts',(174.102155441539,-2.91301564628694,341.361364850856));
#8888=CARTESIAN_POINT('Ctrl Pts',(173.823917407268,3.77300750184398,340.892116539262));
#8889=CARTESIAN_POINT('Ctrl Pts',(173.545679372993,6.99659735503171,335.015759847085));
#8890=CARTESIAN_POINT('Ctrl Pts',(173.26744133872,3.79951308511499,329.124940575853));
#8891=CARTESIAN_POINT('Ctrl Pts',(172.989203304447,-2.88432826229091,328.625576622425));
#8892=CARTESIAN_POINT('Ctrl Pts',(172.790073526441,-5.77348806552616,332.454722659356));
#8893=CARTESIAN_POINT('Ctrl Pts',(172.68368975986,-5.92420449000434,334.706497575313));
#8894=CARTESIAN_POINT('Ctrl Pts',(172.670052004703,-5.92176215774818,334.995489375811));
#8895=CARTESIAN_POINT('',(170.920052775829,-5.91174205618225,334.997960046411));
#8896=CARTESIAN_POINT('Ctrl Pts',(172.670052004703,-5.92176215774818,334.995489375811));
#8897=CARTESIAN_POINT('Ctrl Pts',(172.590943748435,-5.90759496939487,336.671838390109));
#8898=CARTESIAN_POINT('Ctrl Pts',(172.419089480741,-4.28600052805519,340.337495202448));
#8899=CARTESIAN_POINT('Ctrl Pts',(172.154489201625,1.93541011290003,341.723601015535));
#8900=CARTESIAN_POINT('Ctrl Pts',(171.87625116735,6.70138100159934,337.01099865555));
#8901=CARTESIAN_POINT('Ctrl Pts',(171.598013133077,5.31759345735263,330.452932511658));
#8902=CARTESIAN_POINT('Ctrl Pts',(171.319775098802,-0.946071115155991,328.067643087211));
#8903=CARTESIAN_POINT('Ctrl Pts',(171.093788525015,-5.32830294487111,331.297324785966));
#8904=CARTESIAN_POINT('Ctrl Pts',(170.960547962653,-5.91024973360072,334.134607831533));
#8905=CARTESIAN_POINT('Ctrl Pts',(170.920053411716,-5.90761268027711,334.997947902807));
#8906=CARTESIAN_POINT('',(169.170051282952,-5.91509985026952,335.005356513866));
#8907=CARTESIAN_POINT('Ctrl Pts',(170.920052004704,-5.91674965339537,334.997974772674));
#8908=CARTESIAN_POINT('Ctrl Pts',(170.912477675923,-5.91680501271475,335.159708336888));
#8909=CARTESIAN_POINT('Ctrl Pts',(170.904903347141,-5.91022456887072,335.321391389275));
#8910=CARTESIAN_POINT('Ctrl Pts',(170.89732901836,-5.89704707365479,335.482458675535));
#8911=CARTESIAN_POINT('Ctrl Pts',(170.889750598561,-5.88386246106037,335.643612956844));
#8912=CARTESIAN_POINT('Ctrl Pts',(170.882172178762,-5.86407372135668,335.804150462569));
#8913=CARTESIAN_POINT('Ctrl Pts',(170.874593758963,-5.83777137120097,335.963512314445));
#8914=CARTESIAN_POINT('Ctrl Pts',(170.867010072625,-5.81145074251618,336.122984913087));
#8915=CARTESIAN_POINT('Ctrl Pts',(170.859426386286,-5.77860753502681,336.281279886438));
#8916=CARTESIAN_POINT('Ctrl Pts',(170.851842699948,-5.73938316122999,336.437849606562));
#8917=CARTESIAN_POINT('Ctrl Pts',(170.84424690036,-5.70009613523716,336.594669411922));
#8918=CARTESIAN_POINT('Ctrl Pts',(170.836651100773,-5.65440765824046,336.749758119261));
#8919=CARTESIAN_POINT('Ctrl Pts',(170.829055301185,-5.60250914744104,336.902582932579));
#8920=CARTESIAN_POINT('Ctrl Pts',(170.821453175153,-5.55056741103452,337.055535031732));
#8921=CARTESIAN_POINT('Ctrl Pts',(170.813851049122,-5.49240544938,337.206219152313));
#8922=CARTESIAN_POINT('Ctrl Pts',(170.80624892309,-5.42826245886085,337.354123454754));
#8923=CARTESIAN_POINT('Ctrl Pts',(170.79863257236,-5.36399944735397,337.50230450794));
#8924=CARTESIAN_POINT('Ctrl Pts',(170.79101622163,-5.29373318599943,337.647695031932));
#8925=CARTESIAN_POINT('Ctrl Pts',(170.7833998709,-5.21774912932506,337.789807266807));
#8926=CARTESIAN_POINT('Ctrl Pts',(170.776699590685,-5.15090419404948,337.914826692695));
#8927=CARTESIAN_POINT('Ctrl Pts',(170.76999931047,-5.07963493900917,338.037309289029));
#8928=CARTESIAN_POINT('Ctrl Pts',(170.763299030255,-5.00416252374732,338.1569428247));
#8929=CARTESIAN_POINT('Ctrl Pts',(170.755875052817,-4.92053833339655,338.289497977792));
#8930=CARTESIAN_POINT('Ctrl Pts',(170.748451075379,-4.83151747874265,338.418928123214));
#8931=CARTESIAN_POINT('Ctrl Pts',(170.741027097941,-4.73736031598068,338.544763433443));
#8932=CARTESIAN_POINT('Ctrl Pts',(170.733611881913,-4.64331427283756,338.670450239072));
#8933=CARTESIAN_POINT('Ctrl Pts',(170.726196665886,-4.54414420874919,338.792550358252));
#8934=CARTESIAN_POINT('Ctrl Pts',(170.718781449858,-4.44015523147386,338.910620421738));
#8935=CARTESIAN_POINT('Ctrl Pts',(170.711373368714,-4.33626631186883,339.028576878804));
#8936=CARTESIAN_POINT('Ctrl Pts',(170.70396528757,-4.22756795497178,339.142510721752));
#8937=CARTESIAN_POINT('Ctrl Pts',(170.696557206426,-4.11440716855892,339.25200943247));
#8938=CARTESIAN_POINT('Ctrl Pts',(170.689154639252,-4.00133060978618,339.361426641297));
#8939=CARTESIAN_POINT('Ctrl Pts',(170.681752072078,-3.88379850207925,339.466415032553));
#8940=CARTESIAN_POINT('Ctrl Pts',(170.674349504904,-3.76219646569794,339.566597017035));
#8941=CARTESIAN_POINT('Ctrl Pts',(170.666950835149,-3.64065845225689,339.66672625614));
#8942=CARTESIAN_POINT('Ctrl Pts',(170.659552165394,-3.51505506497624,339.762053891506));
#8943=CARTESIAN_POINT('Ctrl Pts',(170.652153495639,-3.3858068480569,339.852240982283));
#8944=CARTESIAN_POINT('Ctrl Pts',(170.644756046435,-3.25657995308031,339.942413194991));
#8945=CARTESIAN_POINT('Ctrl Pts',(170.637358597231,-3.12370972758653,340.027446332818));
#8946=CARTESIAN_POINT('Ctrl Pts',(170.629961148028,-2.98764778617967,340.107043300016));
#8947=CARTESIAN_POINT('Ctrl Pts',(170.622564019564,-2.85159174418108,340.186636816028));
#8948=CARTESIAN_POINT('Ctrl Pts',(170.615166891101,-2.71234458356617,340.260794441613));
#8949=CARTESIAN_POINT('Ctrl Pts',(170.607769762637,-2.5703845068228,340.329263931312));
#8950=CARTESIAN_POINT('Ctrl Pts',(170.6003714952,-2.42840257177149,340.397743963603));
#8951=CARTESIAN_POINT('Ctrl Pts',(170.592973227764,-2.28370722502833,340.460533953971));
#8952=CARTESIAN_POINT('Ctrl Pts',(170.585574960327,-2.13679858804349,340.517428962536));
#8953=CARTESIAN_POINT('Ctrl Pts',(170.578174093801,-1.98983834050946,340.574343958916));
#8954=CARTESIAN_POINT('Ctrl Pts',(170.570773227276,-1.84066360243279,340.625359715499));
#8955=CARTESIAN_POINT('Ctrl Pts',(170.56337236075,-1.68979151587125,340.670320554906));
#8956=CARTESIAN_POINT('Ctrl Pts',(170.555963367365,-1.53875375733493,340.715330765613));
#8957=CARTESIAN_POINT('Ctrl Pts',(170.54855437398,-1.38601528598452,340.754272674328));
#8958=CARTESIAN_POINT('Ctrl Pts',(170.541145380596,-1.23210606479509,340.787041144453));
#8959=CARTESIAN_POINT('Ctrl Pts',(170.533731823015,-1.07810203021669,340.819829801086));
#8960=CARTESIAN_POINT('Ctrl Pts',(170.526318265435,-0.922926175652067,340.846437378122));
#8961=CARTESIAN_POINT('Ctrl Pts',(170.518904707855,-0.76711501892549,340.866810471648));
#8962=CARTESIAN_POINT('Ctrl Pts',(170.511480595718,-0.611082036491973,340.887212570003));
#8963=CARTESIAN_POINT('Ctrl Pts',(170.504056483582,-0.454412316186971,340.901362424364));
#8964=CARTESIAN_POINT('Ctrl Pts',(170.496632371445,-0.297644643054712,340.909258686922));
#8965=CARTESIAN_POINT('Ctrl Pts',(170.49277524629,-0.216197525288533,340.913361113229));
#8966=CARTESIAN_POINT('Ctrl Pts',(170.488918121135,-0.134723932638635,340.915776415404));
#8967=CARTESIAN_POINT('Ctrl Pts',(170.48506099598,-0.053298908672496,340.916509933131));
#8968=CARTESIAN_POINT('Ctrl Pts',(170.477637018542,0.103423395257105,340.917921766772));
#8969=CARTESIAN_POINT('Ctrl Pts',(170.470213041104,0.260438258282484,340.913104309305));
#8970=CARTESIAN_POINT('Ctrl Pts',(170.462789063666,0.417209698739794,340.902022249177));
#8971=CARTESIAN_POINT('Ctrl Pts',(170.455373847639,0.57379612530983,340.890953267547));
#8972=CARTESIAN_POINT('Ctrl Pts',(170.447958631611,0.730139332475785,340.873634425546));
#8973=CARTESIAN_POINT('Ctrl Pts',(170.440543415583,0.885701370265841,340.850082362259));
#8974=CARTESIAN_POINT('Ctrl Pts',(170.433135334439,1.04111372704623,340.826552960648));
#8975=CARTESIAN_POINT('Ctrl Pts',(170.425727253295,1.19574604428049,340.796802333297));
#8976=CARTESIAN_POINT('Ctrl Pts',(170.418319172151,1.34906364086855,340.760899049227));
#8977=CARTESIAN_POINT('Ctrl Pts',(170.410916604977,1.50226712036992,340.725022488627));
#8978=CARTESIAN_POINT('Ctrl Pts',(170.403514037803,1.65415746587748,340.683002474559));
#8979=CARTESIAN_POINT('Ctrl Pts',(170.396111470629,1.8042084733272,340.634958948145));
#8980=CARTESIAN_POINT('Ctrl Pts',(170.388712800874,1.95418047957709,340.586940716436));
#8981=CARTESIAN_POINT('Ctrl Pts',(170.38131413112,2.10231472186053,340.532905401836));
#8982=CARTESIAN_POINT('Ctrl Pts',(170.373915461365,2.24809859698889,340.473023228593));
#8983=CARTESIAN_POINT('Ctrl Pts',(170.366518012161,2.39385842230469,340.413150934049));
#8984=CARTESIAN_POINT('Ctrl Pts',(170.359120562957,2.53726830511264,340.347433836847));
#8985=CARTESIAN_POINT('Ctrl Pts',(170.351723113753,2.67783401668396,340.276090933787));
#8986=CARTESIAN_POINT('Ctrl Pts',(170.344325985289,2.81839363357107,340.204751124031));
#8987=CARTESIAN_POINT('Ctrl Pts',(170.336928856826,2.95610899161856,340.12778616233));
#8988=CARTESIAN_POINT('Ctrl Pts',(170.329531728362,3.09050918943231,340.045461674865));
#8989=CARTESIAN_POINT('Ctrl Pts',(170.322133460926,3.22493008152138,339.963124511485));
#8990=CARTESIAN_POINT('Ctrl Pts',(170.314735193489,3.3560344787274,339.875426374145));
#8991=CARTESIAN_POINT('Ctrl Pts',(170.307336926053,3.48337939831982,339.782676920916));
#8992=CARTESIAN_POINT('Ctrl Pts',(170.299936059527,3.61076905552088,339.689894883828));
#8993=CARTESIAN_POINT('Ctrl Pts',(170.292535193001,3.73439630402208,339.592058217247));
#8994=CARTESIAN_POINT('Ctrl Pts',(170.285134326476,3.85385037615274,339.489517550999));
#8995=CARTESIAN_POINT('Ctrl Pts',(170.277725333091,3.97343562027562,339.386864285295));
#8996=CARTESIAN_POINT('Ctrl Pts',(170.270316339706,4.088838253083,339.279496947496));
#8997=CARTESIAN_POINT('Ctrl Pts',(170.262907346321,4.19968306959087,339.167804299327));
#8998=CARTESIAN_POINT('Ctrl Pts',(170.255493788741,4.31059617032909,339.056042844635));
#8999=CARTESIAN_POINT('Ctrl Pts',(170.248080231161,4.41694560839942,338.939951044676));
#9000=CARTESIAN_POINT('Ctrl Pts',(170.240666673581,4.51839613473388,338.819951168814));
#9001=CARTESIAN_POINT('Ctrl Pts',(170.233242561444,4.61999109446562,338.69978045116));
#9002=CARTESIAN_POINT('Ctrl Pts',(170.225818449307,4.71667298423562,338.575690839066));
#9003=CARTESIAN_POINT('Ctrl Pts',(170.218394337171,4.80814910313857,338.448134678995));
#9004=CARTESIAN_POINT('Ctrl Pts',(170.214537212016,4.85567462979866,338.381864118341));
#9005=CARTESIAN_POINT('Ctrl Pts',(170.210680086861,4.90179574486097,338.314658294717));
#9006=CARTESIAN_POINT('Ctrl Pts',(170.206822961706,4.94647632820009,338.24658320347));
#9007=CARTESIAN_POINT('Ctrl Pts',(170.199398984268,5.03247500060989,338.115556098766));
#9008=CARTESIAN_POINT('Ctrl Pts',(170.19197500683,5.11339364974403,337.980911948022));
#9009=CARTESIAN_POINT('Ctrl Pts',(170.184551029392,5.18891253093172,337.843082360545));
#9010=CARTESIAN_POINT('Ctrl Pts',(170.177135813365,5.26434228847718,337.705415432718));
#9011=CARTESIAN_POINT('Ctrl Pts',(170.169720597337,5.33438478512638,337.564570875215));
#9012=CARTESIAN_POINT('Ctrl Pts',(170.162305381309,5.39876289744299,337.421010066004));
#9013=CARTESIAN_POINT('Ctrl Pts',(170.154897300165,5.46307906546404,337.277587390281));
#9014=CARTESIAN_POINT('Ctrl Pts',(170.147489219021,5.52174154787887,337.131454004233));
#9015=CARTESIAN_POINT('Ctrl Pts',(170.140081137877,5.57451865921723,336.983096639233));
#9016=CARTESIAN_POINT('Ctrl Pts',(170.132678570703,5.62725648758775,336.834849699331));
#9017=CARTESIAN_POINT('Ctrl Pts',(170.125276003529,5.67411754272069,336.684382426635));
#9018=CARTESIAN_POINT('Ctrl Pts',(170.117873436355,5.71491792645063,336.532202224393));
#9019=CARTESIAN_POINT('Ctrl Pts',(170.1104747666,5.75569682895688,336.380102144361));
#9020=CARTESIAN_POINT('Ctrl Pts',(170.103076096845,5.79042131855724,336.226291290444));
#9021=CARTESIAN_POINT('Ctrl Pts',(170.095677427091,5.8189571414556,336.071292839705));
#9022=CARTESIAN_POINT('Ctrl Pts',(170.088279977887,5.84748825682925,335.916319958898));
#9023=CARTESIAN_POINT('Ctrl Pts',(170.080882528683,5.86983266422436,335.760160236787));
#9024=CARTESIAN_POINT('Ctrl Pts',(170.073485079479,5.88590706719703,335.603347792587));
#9025=CARTESIAN_POINT('Ctrl Pts',(170.066087951015,5.9019807732116,335.446542147502));
#9026=CARTESIAN_POINT('Ctrl Pts',(170.058690822552,5.91178497728654,335.289084207867));
#9027=CARTESIAN_POINT('Ctrl Pts',(170.051293694088,5.91528821838032,335.131513710277));
#9028=CARTESIAN_POINT('Ctrl Pts',(170.043895426652,5.9187919988858,334.973918950764));
#9029=CARTESIAN_POINT('Ctrl Pts',(170.036497159215,5.91599287633608,334.816211971931));
#9030=CARTESIAN_POINT('Ctrl Pts',(170.029098891778,5.90691152543361,334.658932861155));
#9031=CARTESIAN_POINT('Ctrl Pts',(170.021698025253,5.89782698415703,334.501598496573));
#9032=CARTESIAN_POINT('Ctrl Pts',(170.014297158727,5.88245584186873,334.344692671681));
#9033=CARTESIAN_POINT('Ctrl Pts',(170.006896292201,5.86087066071359,334.188750555694));
#9034=CARTESIAN_POINT('Ctrl Pts',(169.999487298816,5.83926177696606,334.032637200356));
#9035=CARTESIAN_POINT('Ctrl Pts',(169.992078305431,5.8114252784424,333.877490037201));
#9036=CARTESIAN_POINT('Ctrl Pts',(169.984669312047,5.77748503822549,333.723834965382));
#9037=CARTESIAN_POINT('Ctrl Pts',(169.977255754466,5.74352388964973,333.570085236738));
#9038=CARTESIAN_POINT('Ctrl Pts',(169.969842196886,5.70345160162266,333.417829791094));
#9039=CARTESIAN_POINT('Ctrl Pts',(169.962428639306,5.65744184695399,333.267579060726));
#9040=CARTESIAN_POINT('Ctrl Pts',(169.955004527169,5.61136658897657,333.117114420937));
#9041=CARTESIAN_POINT('Ctrl Pts',(169.947580415032,5.55933710499126,332.968660547848));
#9042=CARTESIAN_POINT('Ctrl Pts',(169.940156302896,5.50157538553221,332.822708370519));
#9043=CARTESIAN_POINT('Ctrl Pts',(169.936299177741,5.47156584675026,332.746880338271));
#9044=CARTESIAN_POINT('Ctrl Pts',(169.932442052587,5.4400098176835,332.671727181239));
#9045=CARTESIAN_POINT('Ctrl Pts',(169.928584927432,5.40694324855453,332.597314987475));
#9046=CARTESIAN_POINT('Ctrl Pts',(169.921160949994,5.34329857711213,332.454090584456));
#9047=CARTESIAN_POINT('Ctrl Pts',(169.913736972556,5.27386316240172,332.313180690228));
#9048=CARTESIAN_POINT('Ctrl Pts',(169.906312995118,5.19882692171055,332.17508775347));
#9049=CARTESIAN_POINT('Ctrl Pts',(169.898897779091,5.12387923507308,332.037157787153));
#9050=CARTESIAN_POINT('Ctrl Pts',(169.891482563063,5.04334405585587,331.902038485706));
#9051=CARTESIAN_POINT('Ctrl Pts',(169.884067347035,4.95745939924524,331.770212566231));
#9052=CARTESIAN_POINT('Ctrl Pts',(169.876659265891,4.87165738041864,331.638513488991));
#9053=CARTESIAN_POINT('Ctrl Pts',(169.869251184747,4.78051633375831,331.510101795697));
#9054=CARTESIAN_POINT('Ctrl Pts',(169.861843103603,4.68432018376019,331.385435713877));
#9055=CARTESIAN_POINT('Ctrl Pts',(169.854440536429,4.5881956343136,331.260862423299));
#9056=CARTESIAN_POINT('Ctrl Pts',(169.847037969255,4.48702370044481,331.140029487235));
#9057=CARTESIAN_POINT('Ctrl Pts',(169.839635402081,4.38113155051904,331.023366134587));
#9058=CARTESIAN_POINT('Ctrl Pts',(169.832236732326,4.27529515234752,330.906764204685));
#9059=CARTESIAN_POINT('Ctrl Pts',(169.824838062572,4.16474373769147,330.794327761846));
#9060=CARTESIAN_POINT('Ctrl Pts',(169.817439392817,4.0498446048744,330.686452824082));
#9061=CARTESIAN_POINT('Ctrl Pts',(169.810041943613,3.93496442684627,330.578595682333));
#9062=CARTESIAN_POINT('Ctrl Pts',(169.802644494409,3.81573822596517,330.47529880738));
#9063=CARTESIAN_POINT('Ctrl Pts',(169.795247045205,3.69257007798922,330.376921287536));
#9064=CARTESIAN_POINT('Ctrl Pts',(169.787849916742,3.56940727036963,330.278548033169));
#9065=CARTESIAN_POINT('Ctrl Pts',(169.780452788278,3.44230314710271,330.185093942728));
#9066=CARTESIAN_POINT('Ctrl Pts',(169.773055659815,3.31169455883302,330.096877554915));
#9067=CARTESIAN_POINT('Ctrl Pts',(169.765657392378,3.18106586010079,330.00864758398));
#9068=CARTESIAN_POINT('Ctrl Pts',(169.758259124941,3.04693193124432,329.925657130378));
#9069=CARTESIAN_POINT('Ctrl Pts',(169.750860857505,2.9097581315298,329.84818108058));
#9070=CARTESIAN_POINT('Ctrl Pts',(169.743459990979,2.77253614121665,329.77067781263));
#9071=CARTESIAN_POINT('Ctrl Pts',(169.736059124453,2.63227247853844,329.698692989006));
#9072=CARTESIAN_POINT('Ctrl Pts',(169.728658257927,2.48945644624628,329.632455201422));
#9073=CARTESIAN_POINT('Ctrl Pts',(169.721249264543,2.34648358829712,329.566144678414));
#9074=CARTESIAN_POINT('Ctrl Pts',(169.713840271158,2.20095310227184,329.505593951563));
#9075=CARTESIAN_POINT('Ctrl Pts',(169.706431277773,2.05337426282041,329.450983447557));
#9076=CARTESIAN_POINT('Ctrl Pts',(169.699017720193,1.90570450971329,329.396339301597));
#9077=CARTESIAN_POINT('Ctrl Pts',(169.691604162613,1.75598424284574,329.34764278545));
#9078=CARTESIAN_POINT('Ctrl Pts',(169.684190605032,1.60473667993107,329.305024078138));
#9079=CARTESIAN_POINT('Ctrl Pts',(169.676766492896,1.45327378842125,329.262344695295));
#9080=CARTESIAN_POINT('Ctrl Pts',(169.669342380759,1.30027962018063,329.225760489368));
#9081=CARTESIAN_POINT('Ctrl Pts',(169.661918268622,1.14628713974621,329.195350453666));
#9082=CARTESIAN_POINT('Ctrl Pts',(169.658061143468,1.06628184632145,329.179551215791));
#9083=CARTESIAN_POINT('Ctrl Pts',(169.654204018313,0.986007175232782,329.165417668293));
#9084=CARTESIAN_POINT('Ctrl Pts',(169.650346893158,0.905538156062171,329.152955343901));
#9085=CARTESIAN_POINT('Ctrl Pts',(169.64292291572,0.750655916356401,329.128968563228));
#9086=CARTESIAN_POINT('Ctrl Pts',(169.635498938282,0.594586293016063,329.111103855623));
#9087=CARTESIAN_POINT('Ctrl Pts',(169.628074960844,0.437854580995084,329.099473419397));
#9088=CARTESIAN_POINT('Ctrl Pts',(169.620659744817,0.281307835975972,329.087856708836));
#9089=CARTESIAN_POINT('Ctrl Pts',(169.613244528789,0.124100926162767,329.082459652025));
#9090=CARTESIAN_POINT('Ctrl Pts',(169.605829312761,-0.0332314176589032,
329.08334332284));
#9091=CARTESIAN_POINT('Ctrl Pts',(169.598421231617,-0.190412377091678,329.084226143392));
#9092=CARTESIAN_POINT('Ctrl Pts',(169.591013150473,-0.347718159546598,329.091377658434));
#9093=CARTESIAN_POINT('Ctrl Pts',(169.583605069329,-0.504609783880745,329.104807083011));
#9094=CARTESIAN_POINT('Ctrl Pts',(169.576202502155,-0.661384630912652,329.118226511823));
#9095=CARTESIAN_POINT('Ctrl Pts',(169.568799934981,-0.817745563366454,329.137914514325));
#9096=CARTESIAN_POINT('Ctrl Pts',(169.561397367807,-0.973154583926014,329.163828248048));
#9097=CARTESIAN_POINT('Ctrl Pts',(169.553998698052,-1.12848178231773,329.189728338304));
#9098=CARTESIAN_POINT('Ctrl Pts',(169.546600028298,-1.28285769973831,329.221847570577));
#9099=CARTESIAN_POINT('Ctrl Pts',(169.539201358543,-1.43575054999479,329.260091383943));
#9100=CARTESIAN_POINT('Ctrl Pts',(169.531803909339,-1.58861817767728,329.298328888266));
#9101=CARTESIAN_POINT('Ctrl Pts',(169.524406460135,-1.74000286206222,329.342688877956));
#9102=CARTESIAN_POINT('Ctrl Pts',(169.517009010931,-1.88938396954852,329.393025880378));
#9103=CARTESIAN_POINT('Ctrl Pts',(169.509611882467,-2.03875860013019,329.443360700275));
#9104=CARTESIAN_POINT('Ctrl Pts',(169.502214754004,-2.18612947287106,329.499671898445));
#9105=CARTESIAN_POINT('Ctrl Pts',(169.49481762554,-2.33099231682914,329.561764497433));
#9106=CARTESIAN_POINT('Ctrl Pts',(169.487419358104,-2.47587746604872,329.62386665713));
#9107=CARTESIAN_POINT('Ctrl Pts',(169.480021090667,-2.61825347451373,329.691751843092));
#9108=CARTESIAN_POINT('Ctrl Pts',(169.472622823231,-2.75763735172414,329.765177481626));
#9109=CARTESIAN_POINT('Ctrl Pts',(169.465221956705,-2.8970701959568,329.838628915359));
#9110=CARTESIAN_POINT('Ctrl Pts',(169.457821090179,-3.03350848607352,329.917624503148));
#9111=CARTESIAN_POINT('Ctrl Pts',(169.450420223653,-3.16649520462957,330.001876483963));
#9112=CARTESIAN_POINT('Ctrl Pts',(169.443011230269,-3.29962795531663,330.086220981509));
#9113=CARTESIAN_POINT('Ctrl Pts',(169.435602236884,-3.4293012498449,330.175833199265));
#9114=CARTESIAN_POINT('Ctrl Pts',(169.428193243499,-3.55508776582668,330.270382516549));
#9115=CARTESIAN_POINT('Ctrl Pts',(169.420779685919,-3.68095177064158,330.364990079473));
#9116=CARTESIAN_POINT('Ctrl Pts',(169.413366128339,-3.80292393731364,330.464540566932));
#9117=CARTESIAN_POINT('Ctrl Pts',(169.405952570758,-3.92061165239879,330.568664441325));
#9118=CARTESIAN_POINT('Ctrl Pts',(169.398528458622,-4.03846691749119,330.672936555116));
#9119=CARTESIAN_POINT('Ctrl Pts',(169.391104346485,-4.1520252799831,330.781794802148));
#9120=CARTESIAN_POINT('Ctrl Pts',(169.383680234348,-4.26093189502371,330.894833748985));
#9121=CARTESIAN_POINT('Ctrl Pts',(169.379823109194,-4.31751326618876,330.953562032889));
#9122=CARTESIAN_POINT('Ctrl Pts',(169.375965984039,-4.3728396984905,331.013418242858));
#9123=CARTESIAN_POINT('Ctrl Pts',(169.372108858885,-4.42686593652754,331.074342278992));
#9124=CARTESIAN_POINT('Ctrl Pts',(169.364751936199,-4.5299133721978,331.190546292493));
#9125=CARTESIAN_POINT('Ctrl Pts',(169.357395013513,-4.62855304767428,331.311003372299));
#9126=CARTESIAN_POINT('Ctrl Pts',(169.350038090827,-4.72240849342267,331.435341729738));
#9127=CARTESIAN_POINT('Ctrl Pts',(169.342538670572,-4.81808184231687,331.562088419366));
#9128=CARTESIAN_POINT('Ctrl Pts',(169.335039250317,-4.90878340356712,331.692868053281));
#9129=CARTESIAN_POINT('Ctrl Pts',(169.327539830062,-4.99415331427621,331.827246742023));
#9130=CARTESIAN_POINT('Ctrl Pts',(169.320200871848,-5.07769659977142,331.958750184685));
#9131=CARTESIAN_POINT('Ctrl Pts',(169.312861913634,-5.15613383886759,332.093699900124));
#9132=CARTESIAN_POINT('Ctrl Pts',(169.30552295542,-5.22916830256277,332.231655833179));
#9133=CARTESIAN_POINT('Ctrl Pts',(169.298188967279,-5.30215330602424,332.369518340029));
#9134=CARTESIAN_POINT('Ctrl Pts',(169.290854979137,-5.36974263697946,332.51038267876));
#9135=CARTESIAN_POINT('Ctrl Pts',(169.283520990996,-5.43168370675522,332.653781196847));
#9136=CARTESIAN_POINT('Ctrl Pts',(169.276190456817,-5.49359560520898,332.797112180996));
#9137=CARTESIAN_POINT('Ctrl Pts',(169.268859922638,-5.54986438627201,332.942974620463));
#9138=CARTESIAN_POINT('Ctrl Pts',(169.261529388459,-5.60028423835156,333.090877947283));
#9139=CARTESIAN_POINT('Ctrl Pts',(169.253906273146,-5.65271648095285,333.244684489617));
#9140=CARTESIAN_POINT('Ctrl Pts',(169.246283157833,-5.69882306887463,333.400697811828));
#9141=CARTESIAN_POINT('Ctrl Pts',(169.23866004252,-5.73842853454316,333.558345215927));
#9142=CARTESIAN_POINT('Ctrl Pts',(169.231330355198,-5.77650951163725,333.70992447609));
#9143=CARTESIAN_POINT('Ctrl Pts',(169.224000667875,-5.80858045972651,333.863013962719));
#9144=CARTESIAN_POINT('Ctrl Pts',(169.216670980552,-5.8345369607319,334.017091552405));
#9145=CARTESIAN_POINT('Ctrl Pts',(169.209340465971,-5.86049639129298,334.171186531911));
#9146=CARTESIAN_POINT('Ctrl Pts',(169.20200995139,-5.88033994501261,334.326269460021));
#9147=CARTESIAN_POINT('Ctrl Pts',(169.19467943681,-5.89401481477528,334.48181091703));
#9148=CARTESIAN_POINT('Ctrl Pts',(169.187344914374,-5.90769716107801,334.637437414112));
#9149=CARTESIAN_POINT('Ctrl Pts',(169.180010391939,-5.91520406817465,334.793522560859));
#9150=CARTESIAN_POINT('Ctrl Pts',(169.172675869504,-5.91653478056043,334.949534636445));
#9151=CARTESIAN_POINT('Ctrl Pts',(169.171801247904,-5.9166934643475,334.968138646784));
#9152=CARTESIAN_POINT('Ctrl Pts',(169.170926626303,-5.91676438408337,334.986741620344));
#9153=CARTESIAN_POINT('Ctrl Pts',(169.170052004703,-5.91674758786482,335.005342658123));
#9154=CARTESIAN_POINT('',(167.420052004703,-5.92202873839451,334.999419944072));
#9155=CARTESIAN_POINT('Ctrl Pts',(169.170050945661,-5.91432982443071,335.005362988975));
#9156=CARTESIAN_POINT('Ctrl Pts',(169.144657571978,-5.91904404249479,335.545201194357));
#9157=CARTESIAN_POINT('Ctrl Pts',(169.026518186868,-5.60357054579488,338.0513146166));
#9158=CARTESIAN_POINT('Ctrl Pts',(168.815632790337,-2.05622536433816,341.687642347814));
#9159=CARTESIAN_POINT('Ctrl Pts',(168.537394756062,4.51103959403896,340.348190787755));
#9160=CARTESIAN_POINT('Ctrl Pts',(168.25915672179,6.93859009980183,334.100783480941));
#9161=CARTESIAN_POINT('Ctrl Pts',(167.980918687515,2.99869888439871,328.678573901253));
#9162=CARTESIAN_POINT('Ctrl Pts',(167.702680653241,-3.69305403649433,329.057443748289));
#9163=CARTESIAN_POINT('Ctrl Pts',(167.515725092304,-5.9122207605932,332.976298931997));
#9164=CARTESIAN_POINT('Ctrl Pts',(167.421515542791,-5.92647291942922,334.968470644554));
#9165=CARTESIAN_POINT('Ctrl Pts',(167.420052004703,-5.92642976230421,334.999419512997));
#9166=CARTESIAN_POINT('',(165.670052025949,-5.91423241416373,334.994968760502));
#9167=CARTESIAN_POINT('Ctrl Pts',(167.420052004703,-5.91674997161742,334.999420461121));
#9168=CARTESIAN_POINT('Ctrl Pts',(167.412648369967,-5.91676528161425,335.155726494585));
#9169=CARTESIAN_POINT('Ctrl Pts',(167.40524473523,-5.91058248256132,335.312274754108));
#9170=CARTESIAN_POINT('Ctrl Pts',(167.397841100494,-5.89816995282945,335.468531503786));
#9171=CARTESIAN_POINT('Ctrl Pts',(167.390446191951,-5.88577205295576,335.624604083585));
#9172=CARTESIAN_POINT('Ctrl Pts',(167.383051283407,-5.86715906595222,335.780385466768));
#9173=CARTESIAN_POINT('Ctrl Pts',(167.375656374863,-5.84235133423688,335.935340285586));
#9174=CARTESIAN_POINT('Ctrl Pts',(167.368268546698,-5.81756735509657,336.090146740338));
#9175=CARTESIAN_POINT('Ctrl Pts',(167.360880718532,-5.7866004971388,336.244127837844));
#9176=CARTESIAN_POINT('Ctrl Pts',(167.353492890367,-5.74952301007913,336.396751845916));
#9177=CARTESIAN_POINT('Ctrl Pts',(167.346110502519,-5.71247282648276,336.549263463308));
#9178=CARTESIAN_POINT('Ctrl Pts',(167.33872811467,-5.66932106103354,336.700419617601));
#9179=CARTESIAN_POINT('Ctrl Pts',(167.331345726822,-5.62019127066978,336.8496974465));
#9180=CARTESIAN_POINT('Ctrl Pts',(167.323631512567,-5.56885317560087,337.005685072641));
#9181=CARTESIAN_POINT('Ctrl Pts',(167.315917298312,-5.51098725448226,337.159621185502));
#9182=CARTESIAN_POINT('Ctrl Pts',(167.308203084056,-5.44679332156382,337.310924722848));
#9183=CARTESIAN_POINT('Ctrl Pts',(167.300825635713,-5.38540179050894,337.455623067213));
#9184=CARTESIAN_POINT('Ctrl Pts',(167.293448187371,-5.31822320842122,337.597913440029));
#9185=CARTESIAN_POINT('Ctrl Pts',(167.286070739028,-5.24548207423519,337.737306773341));
#9186=CARTESIAN_POINT('Ctrl Pts',(167.278693424878,-5.17274226317604,337.876697571153));
#9187=CARTESIAN_POINT('Ctrl Pts',(167.271316110727,-5.09444027467716,338.013191101186));
#9188=CARTESIAN_POINT('Ctrl Pts',(167.263938796577,-5.01084690302941,338.146322277978));
#9189=CARTESIAN_POINT('Ctrl Pts',(167.256560139632,-4.92723831599127,338.279477686869));
#9190=CARTESIAN_POINT('Ctrl Pts',(167.249181482687,-4.83833662812618,338.409269206145));
#9191=CARTESIAN_POINT('Ctrl Pts',(167.241802825742,-4.74445624796787,338.535260312002));
#9192=CARTESIAN_POINT('Ctrl Pts',(167.234421348463,-4.65053998403919,338.661299575269));
#9193=CARTESIAN_POINT('Ctrl Pts',(167.227039871184,-4.55164146360955,338.783535232465));
#9194=CARTESIAN_POINT('Ctrl Pts',(167.219658393905,-4.44811556479037,338.901563594864));
#9195=CARTESIAN_POINT('Ctrl Pts',(167.212268753758,-4.34447518098295,339.019722479923));
#9196=CARTESIAN_POINT('Ctrl Pts',(167.20487911361,-4.2361974492157,339.133664498197));
#9197=CARTESIAN_POINT('Ctrl Pts',(167.197489473462,-4.12367476806568,339.24302215051));
#9198=CARTESIAN_POINT('Ctrl Pts',(167.190095037495,-4.01107906057267,339.352450775087));
#9199=CARTESIAN_POINT('Ctrl Pts',(167.182700601529,-3.89423319378537,339.457288856403));
#9200=CARTESIAN_POINT('Ctrl Pts',(167.175306165562,-3.77356239496176,339.557209388851));
#9201=CARTESIAN_POINT('Ctrl Pts',(167.167901612578,-3.65272649517612,339.657266631888));
#9202=CARTESIAN_POINT('Ctrl Pts',(167.160497059595,-3.52805551274428,339.752392666968));
#9203=CARTESIAN_POINT('Ctrl Pts',(167.153092506612,-3.40000387323542,339.842303607219));
#9204=CARTESIAN_POINT('Ctrl Pts',(167.150796532639,-3.36029813648877,339.870182829523));
#9205=CARTESIAN_POINT('Ctrl Pts',(167.148500558666,-3.32026753858626,339.897560968234));
#9206=CARTESIAN_POINT('Ctrl Pts',(167.146204584693,-3.27992608558425,339.924430468146));
#9207=CARTESIAN_POINT('Ctrl Pts',(167.138780607255,-3.14948295319161,340.01131235944));
#9208=CARTESIAN_POINT('Ctrl Pts',(167.131356629817,-3.01538853812546,340.093138779107));
#9209=CARTESIAN_POINT('Ctrl Pts',(167.123932652379,-2.8780722797421,340.169587073943));
#9210=CARTESIAN_POINT('Ctrl Pts',(167.116517436352,-2.74091807520394,340.245945148289));
#9211=CARTESIAN_POINT('Ctrl Pts',(167.109102220324,-2.60054991871874,340.316937551828));
#9212=CARTESIAN_POINT('Ctrl Pts',(167.101687004296,-2.45742730556294,340.38228405051));
#9213=CARTESIAN_POINT('Ctrl Pts',(167.094278923152,-2.31444240426478,340.44756767312));
#9214=CARTESIAN_POINT('Ctrl Pts',(167.086870842008,-2.16870865982743,340.50721605192));
#9215=CARTESIAN_POINT('Ctrl Pts',(167.079462760864,-2.02071122731929,340.560994218509));
#9216=CARTESIAN_POINT('Ctrl Pts',(167.07206019369,-1.87282395200341,340.614732357026));
#9217=CARTESIAN_POINT('Ctrl Pts',(167.064657626516,-1.72267669277552,340.662608856343));
#9218=CARTESIAN_POINT('Ctrl Pts',(167.057255059342,-1.5707755989397,340.704436394621));
#9219=CARTESIAN_POINT('Ctrl Pts',(167.049856389587,-1.41895448036626,340.746241910883));
#9220=CARTESIAN_POINT('Ctrl Pts',(167.042457719833,-1.26538172507636,340.782004709896));
#9221=CARTESIAN_POINT('Ctrl Pts',(167.035059050078,-1.1105795912168,340.811587006496));
#9222=CARTESIAN_POINT('Ctrl Pts',(167.027661600874,-0.95580299490186,340.841164422935));
#9223=CARTESIAN_POINT('Ctrl Pts',(167.02026415167,-0.799797788749643,340.864563290536));
#9224=CARTESIAN_POINT('Ctrl Pts',(167.012866702466,-0.64309751706047,340.881696706398));
#9225=CARTESIAN_POINT('Ctrl Pts',(167.005469574002,-0.486404039621832,340.898829379385));
#9226=CARTESIAN_POINT('Ctrl Pts',(166.998072445539,-0.329015927568422,340.909697100217));
#9227=CARTESIAN_POINT('Ctrl Pts',(166.990675317076,-0.171472692638845,340.914264762266));
#9228=CARTESIAN_POINT('Ctrl Pts',(166.983277049639,-0.0139051999841216,
340.91883312762));
#9229=CARTESIAN_POINT('Ctrl Pts',(166.975878782202,0.143817090027833,340.917099491874));
#9230=CARTESIAN_POINT('Ctrl Pts',(166.968480514766,0.301153962671562,340.909080880583));
#9231=CARTESIAN_POINT('Ctrl Pts',(166.96107964824,0.458546109413887,340.901059452269));
#9232=CARTESIAN_POINT('Ctrl Pts',(166.953678781714,0.615552196711758,340.886748671313));
#9233=CARTESIAN_POINT('Ctrl Pts',(166.946277915188,0.771636577353052,340.866217482756));
#9234=CARTESIAN_POINT('Ctrl Pts',(166.938868921804,0.927892353566265,340.845663748991));
#9235=CARTESIAN_POINT('Ctrl Pts',(166.931459928419,1.0832240316166,340.818876015248));
#9236=CARTESIAN_POINT('Ctrl Pts',(166.924050935034,1.23710488750165,340.785974598961));
#9237=CARTESIAN_POINT('Ctrl Pts',(166.916637377454,1.39108053930175,340.753052914266));
#9238=CARTESIAN_POINT('Ctrl Pts',(166.909223819874,1.54360322729965,340.714010134631));
#9239=CARTESIAN_POINT('Ctrl Pts',(166.901810262293,1.69416135758378,340.66901648057));
#9240=CARTESIAN_POINT('Ctrl Pts',(166.894386150157,1.8449338349298,340.623958769804));
#9241=CARTESIAN_POINT('Ctrl Pts',(166.88696203802,1.99373581649814,340.572933384746));
#9242=CARTESIAN_POINT('Ctrl Pts',(166.879537925883,2.14007488472642,340.516158994288));
#9243=CARTESIAN_POINT('Ctrl Pts',(166.875680800729,2.21610392237841,340.486662412671));
#9244=CARTESIAN_POINT('Ctrl Pts',(166.871823675574,2.29146854785813,340.455614816797));
#9245=CARTESIAN_POINT('Ctrl Pts',(166.867966550419,2.36610243175137,340.423051709597));
#9246=CARTESIAN_POINT('Ctrl Pts',(166.860542572981,2.50975353144761,340.360376073347));
#9247=CARTESIAN_POINT('Ctrl Pts',(166.853118595543,2.65112929576347,340.291894189819));
#9248=CARTESIAN_POINT('Ctrl Pts',(166.845694618105,2.78972600446066,340.217792577569));
#9249=CARTESIAN_POINT('Ctrl Pts',(166.838279402078,2.92815914818906,340.14377841637));
#9250=CARTESIAN_POINT('Ctrl Pts',(166.83086418605,3.06381943867884,340.064157902056));
#9251=CARTESIAN_POINT('Ctrl Pts',(166.823448970022,3.19622256187971,339.979165783284));
#9252=CARTESIAN_POINT('Ctrl Pts',(166.816040888878,3.32849828746126,339.894255443502));
#9253=CARTESIAN_POINT('Ctrl Pts',(166.808632807734,3.45752277305123,339.803983989103));
#9254=CARTESIAN_POINT('Ctrl Pts',(166.80122472659,3.58283588346338,339.708632242453));
#9255=CARTESIAN_POINT('Ctrl Pts',(166.793822159416,3.70805572103873,339.613351467849));
#9256=CARTESIAN_POINT('Ctrl Pts',(166.786419592242,3.82956938813069,339.512998155247));
#9257=CARTESIAN_POINT('Ctrl Pts',(166.779017025068,3.94694545537717,339.407896565798));
#9258=CARTESIAN_POINT('Ctrl Pts',(166.771618355314,4.0642597246369,339.302850311878));
#9259=CARTESIAN_POINT('Ctrl Pts',(166.764219685559,4.17744045518329,339.193061008239));
#9260=CARTESIAN_POINT('Ctrl Pts',(166.756821015804,4.28608915668034,339.078893269441));
#9261=CARTESIAN_POINT('Ctrl Pts',(166.7494235666,4.39471993451602,338.964744364773));
#9262=CARTESIAN_POINT('Ctrl Pts',(166.742026117396,4.49881991009974,338.84621872858));
#9263=CARTESIAN_POINT('Ctrl Pts',(166.734628668192,4.59802727349437,338.723718001501));
#9264=CARTESIAN_POINT('Ctrl Pts',(166.727231539729,4.69723033543055,338.60122258584));
#9265=CARTESIAN_POINT('Ctrl Pts',(166.719834411265,4.79154097209094,338.474752712019));
#9266=CARTESIAN_POINT('Ctrl Pts',(166.712437282802,4.88063770080368,338.344743068756));
#9267=CARTESIAN_POINT('Ctrl Pts',(166.705039015365,4.96974814818885,338.214713407254));
#9268=CARTESIAN_POINT('Ctrl Pts',(166.697640747929,5.05364287813316,338.081143198947));
#9269=CARTESIAN_POINT('Ctrl Pts',(166.690242480492,5.13204386660433,337.944495935427));
#9270=CARTESIAN_POINT('Ctrl Pts',(166.682841613966,5.21047239816723,337.807800666288));
#9271=CARTESIAN_POINT('Ctrl Pts',(166.67544074744,5.28340315999887,337.668026513174));
#9272=CARTESIAN_POINT('Ctrl Pts',(166.668039880915,5.35060426001229,337.525661223371));
#9273=CARTESIAN_POINT('Ctrl Pts',(166.66063088753,5.417879153258,337.383139602869));
#9274=CARTESIAN_POINT('Ctrl Pts',(166.653221894145,5.47941166038539,337.238021501133));
#9275=CARTESIAN_POINT('Ctrl Pts',(166.64581290076,5.5350179183095,337.09081496228));
#9276=CARTESIAN_POINT('Ctrl Pts',(166.63839934318,5.59065843160656,336.943517739121));
#9277=CARTESIAN_POINT('Ctrl Pts',(166.6309857856,5.64036530349625,336.79412986852));
#9278=CARTESIAN_POINT('Ctrl Pts',(166.62357222802,5.68400482321869,336.643173676799));
#9279=CARTESIAN_POINT('Ctrl Pts',(166.616148115883,5.72770647178675,336.492002571304));
#9280=CARTESIAN_POINT('Ctrl Pts',(166.608724003746,5.76532342739506,336.339259046761));
#9281=CARTESIAN_POINT('Ctrl Pts',(166.60129989161,5.79677309798291,336.185475521891));
#9282=CARTESIAN_POINT('Ctrl Pts',(166.597442766455,5.8131124680383,336.105578789292));
#9283=CARTESIAN_POINT('Ctrl Pts',(166.5935856413,5.82778800556544,336.025401432252));
#9284=CARTESIAN_POINT('Ctrl Pts',(166.589728516145,5.8407936710839,335.945018441263));
#9285=CARTESIAN_POINT('Ctrl Pts',(166.582304538707,5.86582624417931,335.790301783764));
#9286=CARTESIAN_POINT('Ctrl Pts',(166.574880561269,5.88474490553512,335.634356410765));
#9287=CARTESIAN_POINT('Ctrl Pts',(166.567456583831,5.89743391065884,335.477706847252));
#9288=CARTESIAN_POINT('Ctrl Pts',(166.560041367804,5.91010794084733,335.321242153793));
#9289=CARTESIAN_POINT('Ctrl Pts',(166.552626151776,5.9165669191014,335.164075292416));
#9290=CARTESIAN_POINT('Ctrl Pts',(166.545210935748,5.91674616045239,335.006740569106));
#9291=CARTESIAN_POINT('Ctrl Pts',(166.537802854604,5.91692522933826,334.849557232474));
#9292=CARTESIAN_POINT('Ctrl Pts',(166.53039477346,5.91083659005377,334.692206726175));
#9293=CARTESIAN_POINT('Ctrl Pts',(166.522986692316,5.8984673865637,334.535227956796));
#9294=CARTESIAN_POINT('Ctrl Pts',(166.515584125142,5.88610738969763,334.378366029581));
#9295=CARTESIAN_POINT('Ctrl Pts',(166.508181557968,5.86747616590226,334.22187565882));
#9296=CARTESIAN_POINT('Ctrl Pts',(166.500778990794,5.84261292211522,334.066295118984));
#9297=CARTESIAN_POINT('Ctrl Pts',(166.493380321039,5.81776276871761,333.910796491624));
#9298=CARTESIAN_POINT('Ctrl Pts',(166.485981651285,5.78668718864312,333.756207108795));
#9299=CARTESIAN_POINT('Ctrl Pts',(166.47858298153,5.74947714806621,333.603059383379));
#9300=CARTESIAN_POINT('Ctrl Pts',(166.471185532326,5.71227324599036,333.449936922583));
#9301=CARTESIAN_POINT('Ctrl Pts',(166.463788083122,5.66893697992537,333.298256009495));
#9302=CARTESIAN_POINT('Ctrl Pts',(166.456390633918,5.6196103019363,333.148538248607));
#9303=CARTESIAN_POINT('Ctrl Pts',(166.448993505454,5.57028576266609,332.998826979221));
#9304=CARTESIAN_POINT('Ctrl Pts',(166.441596376991,5.51497144469301,332.851079047259));
#9305=CARTESIAN_POINT('Ctrl Pts',(166.434199248527,5.45385891431485,332.705800029368));
#9306=CARTESIAN_POINT('Ctrl Pts',(166.426800981091,5.3927369741325,332.560498642134));
#9307=CARTESIAN_POINT('Ctrl Pts',(166.419402713654,5.32581518862284,332.417667269937));
#9308=CARTESIAN_POINT('Ctrl Pts',(166.412004446218,5.25333286299755,332.277790531012));
#9309=CARTESIAN_POINT('Ctrl Pts',(166.404603579692,5.18082507356891,332.137864651917));
#9310=CARTESIAN_POINT('Ctrl Pts',(166.397202713166,5.10275302625763,332.000895803894));
#9311=CARTESIAN_POINT('Ctrl Pts',(166.38980184664,5.01940138804739,331.867342937989));
#9312=CARTESIAN_POINT('Ctrl Pts',(166.382392853256,4.93595822176967,331.733643418269));
#9313=CARTESIAN_POINT('Ctrl Pts',(166.374983859871,4.84722408440145,331.603367688563));
#9314=CARTESIAN_POINT('Ctrl Pts',(166.367574866486,4.75352670221447,331.476945295084));
#9315=CARTESIAN_POINT('Ctrl Pts',(166.360161308906,4.65977159920789,331.350445021049));
#9316=CARTESIAN_POINT('Ctrl Pts',(166.352747751325,4.56104739232786,331.227803103371));
#9317=CARTESIAN_POINT('Ctrl Pts',(166.345334193745,4.45772095835694,331.109414643023));
#9318=CARTESIAN_POINT('Ctrl Pts',(166.337910081608,4.35424742029131,330.990857635028));
#9319=CARTESIAN_POINT('Ctrl Pts',(166.330485969472,4.2461588250031,330.876566448983));
#9320=CARTESIAN_POINT('Ctrl Pts',(166.323061857335,4.13385819944831,330.766898660633));
#9321=CARTESIAN_POINT('Ctrl Pts',(166.31920473218,4.07551350317672,330.709921829288));
#9322=CARTESIAN_POINT('Ctrl Pts',(166.315347607026,4.01603242857411,330.654192288226));
#9323=CARTESIAN_POINT('Ctrl Pts',(166.311490481871,3.95547476843586,330.599755697831));
#9324=CARTESIAN_POINT('Ctrl Pts',(166.304066504433,3.83891679208092,330.494979212057));
#9325=CARTESIAN_POINT('Ctrl Pts',(166.296642526995,3.71801697418941,330.394679116637));
#9326=CARTESIAN_POINT('Ctrl Pts',(166.289218549557,3.59315376302699,330.299236594154));
#9327=CARTESIAN_POINT('Ctrl Pts',(166.28180333353,3.46843790924056,330.203906708207));
#9328=CARTESIAN_POINT('Ctrl Pts',(166.274388117502,3.33976826625009,330.113423208673));
#9329=CARTESIAN_POINT('Ctrl Pts',(166.266972901475,3.20755913860955,330.028129634149));
#9330=CARTESIAN_POINT('Ctrl Pts',(166.25956482033,3.07547722192567,329.942918128674));
#9331=CARTESIAN_POINT('Ctrl Pts',(166.252156739186,2.93986291216941,329.862886807614));
#9332=CARTESIAN_POINT('Ctrl Pts',(166.244748658042,2.80116243025032,329.788338115164));
#9333=CARTESIAN_POINT('Ctrl Pts',(166.237346090868,2.66256518563315,329.713844910667));
#9334=CARTESIAN_POINT('Ctrl Pts',(166.229943523694,2.52088667003073,329.644826385202));
#9335=CARTESIAN_POINT('Ctrl Pts',(166.22254095652,2.37660074705245,329.581540860022));
#9336=CARTESIAN_POINT('Ctrl Pts',(166.215142286765,2.23239078998174,329.518288654395));
#9337=CARTESIAN_POINT('Ctrl Pts',(166.207743617011,2.08557650044486,329.460763587261));
#9338=CARTESIAN_POINT('Ctrl Pts',(166.200344947256,1.93665482281105,329.409177282387));
#9339=CARTESIAN_POINT('Ctrl Pts',(166.192947498052,1.78775771263016,329.357599487651));
#9340=CARTESIAN_POINT('Ctrl Pts',(166.185550048848,1.63675425664227,329.311958632802));
#9341=CARTESIAN_POINT('Ctrl Pts',(166.178152599644,1.48415990159975,329.272417617442));
#9342=CARTESIAN_POINT('Ctrl Pts',(166.17075547118,1.33157216278268,329.232878316512));
#9343=CARTESIAN_POINT('Ctrl Pts',(166.163358342717,1.17739402334233,329.199438422816));
#9344=CARTESIAN_POINT('Ctrl Pts',(166.155961214253,1.02215430098216,329.1722104407));
#9345=CARTESIAN_POINT('Ctrl Pts',(166.148562946817,0.866890675579753,329.144978266155));
#9346=CARTESIAN_POINT('Ctrl Pts',(166.14116467938,0.710565509414855,329.123959972145));
#9347=CARTESIAN_POINT('Ctrl Pts',(166.133766411944,0.553715830082504,329.109216576548));
#9348=CARTESIAN_POINT('Ctrl Pts',(166.126365545418,0.396811047807554,329.094468001441));
#9349=CARTESIAN_POINT('Ctrl Pts',(166.118964678892,0.239381756829181,329.085998748683));
#9350=CARTESIAN_POINT('Ctrl Pts',(166.111563812366,0.0819679485124542,329.08381780048));
#9351=CARTESIAN_POINT('Ctrl Pts',(166.104154818982,-0.0756187152145948,
329.081634457388));
#9352=CARTESIAN_POINT('Ctrl Pts',(166.096745825597,-0.233189488929145,329.085753213996));
#9353=CARTESIAN_POINT('Ctrl Pts',(166.089336832212,-0.390205806565071,329.096130930396));
#9354=CARTESIAN_POINT('Ctrl Pts',(166.081923274632,-0.547318851668759,329.106515039828));
#9355=CARTESIAN_POINT('Ctrl Pts',(166.074509717052,-0.703876389831103,329.123165752734));
#9356=CARTESIAN_POINT('Ctrl Pts',(166.067096159471,-0.859347634135345,329.14598836641));
#9357=CARTESIAN_POINT('Ctrl Pts',(166.059672047335,-1.01504022021867,329.168843472255));
#9358=CARTESIAN_POINT('Ctrl Pts',(166.052247935198,-1.16964305789237,329.197887959206));
#9359=CARTESIAN_POINT('Ctrl Pts',(166.044823823061,-1.32263735307258,329.232976418051));
#9360=CARTESIAN_POINT('Ctrl Pts',(166.040966697907,-1.40212404906893,329.251206285105));
#9361=CARTESIAN_POINT('Ctrl Pts',(166.037109572752,-1.48117683157777,329.271066737282));
#9362=CARTESIAN_POINT('Ctrl Pts',(166.033252447597,-1.5597249464937,329.292532203001));
#9363=CARTESIAN_POINT('Ctrl Pts',(166.025828470159,-1.71090993779083,329.333847723447));
#9364=CARTESIAN_POINT('Ctrl Pts',(166.018404492721,-1.86068025652888,329.381236822746));
#9365=CARTESIAN_POINT('Ctrl Pts',(166.010980515283,-2.00851055807154,329.434587535446));
#9366=CARTESIAN_POINT('Ctrl Pts',(166.003565299256,-2.15616639761601,329.487875286277));
#9367=CARTESIAN_POINT('Ctrl Pts',(165.996150083228,-2.30188642963945,329.547110520575));
#9368=CARTESIAN_POINT('Ctrl Pts',(165.9887348672,-2.44515756123928,329.612130749247));
#9369=CARTESIAN_POINT('Ctrl Pts',(165.981326786056,-2.58829083807782,329.677088415782));
#9370=CARTESIAN_POINT('Ctrl Pts',(165.973918704912,-2.72897956790627,329.747819842039));
#9371=CARTESIAN_POINT('Ctrl Pts',(165.966510623768,-2.86672794321283,329.824113461241));
#9372=CARTESIAN_POINT('Ctrl Pts',(165.959108056594,-3.00437378988889,329.90035029371));
#9373=CARTESIAN_POINT('Ctrl Pts',(165.95170548942,-3.13908331470249,329.982140895648));
#9374=CARTESIAN_POINT('Ctrl Pts',(165.944302922246,-3.27038285501261,330.069226577489));
#9375=CARTESIAN_POINT('Ctrl Pts',(165.936904252491,-3.40161326668806,330.156266409099));
#9376=CARTESIAN_POINT('Ctrl Pts',(165.929505582737,-3.52943695915461,330.248595562702));
#9377=CARTESIAN_POINT('Ctrl Pts',(165.922106912982,-3.65340704836094,330.34591066894));
#9378=CARTESIAN_POINT('Ctrl Pts',(165.914709463778,-3.77735668635163,330.443209721207));
#9379=CARTESIAN_POINT('Ctrl Pts',(165.907312014574,-3.89745368950972,330.545492863434));
#9380=CARTESIAN_POINT('Ctrl Pts',(165.89991456537,-4.01328213427224,330.652414799773));
#9381=CARTESIAN_POINT('Ctrl Pts',(165.892517436906,-4.12910555691527,330.759332100163));
#9382=CARTESIAN_POINT('Ctrl Pts',(165.885120308443,-4.24066051492431,330.870887541605));
#9383=CARTESIAN_POINT('Ctrl Pts',(165.877723179979,-4.34756622739132,330.986697312568));
#9384=CARTESIAN_POINT('Ctrl Pts',(165.870324912543,-4.45448840066969,331.102524915345));
#9385=CARTESIAN_POINT('Ctrl Pts',(165.862926645106,-4.55675964985629,331.222607877707));
#9386=CARTESIAN_POINT('Ctrl Pts',(165.85552837767,-4.65403804727018,331.346527621965));
#9387=CARTESIAN_POINT('Ctrl Pts',(165.848127511144,-4.7513506196083,331.470490900534));
#9388=CARTESIAN_POINT('Ctrl Pts',(165.840726644618,-4.84366661757521,331.598293351291));
#9389=CARTESIAN_POINT('Ctrl Pts',(165.833325778092,-4.9306862675299,331.729485744765));
#9390=CARTESIAN_POINT('Ctrl Pts',(165.825916784708,-5.01780147337922,331.86082220003));
#9391=CARTESIAN_POINT('Ctrl Pts',(165.818507791323,-5.09960851014299,331.995555720806));
#9392=CARTESIAN_POINT('Ctrl Pts',(165.811098797938,-5.1758522060904,332.13321006992));
#9393=CARTESIAN_POINT('Ctrl Pts',(165.803685240358,-5.25214287078408,332.27094921886));
#9394=CARTESIAN_POINT('Ctrl Pts',(165.796271682778,-5.32286319824254,332.41161244888));
#9395=CARTESIAN_POINT('Ctrl Pts',(165.788858125198,-5.38780558673392,332.554702160869));
#9396=CARTESIAN_POINT('Ctrl Pts',(165.781434013061,-5.45284043260494,332.69799558726));
#9397=CARTESIAN_POINT('Ctrl Pts',(165.774009900924,-5.51208077046498,332.843722050228));
#9398=CARTESIAN_POINT('Ctrl Pts',(165.766585788787,-5.5653681287757,332.991366595491));
#9399=CARTESIAN_POINT('Ctrl Pts',(165.762728663633,-5.59305305680225,333.068073881022));
#9400=CARTESIAN_POINT('Ctrl Pts',(165.758871538478,-5.61913197552565,333.145298682617));
#9401=CARTESIAN_POINT('Ctrl Pts',(165.755014413324,-5.64358809952865,333.22296766339));
#9402=CARTESIAN_POINT('Ctrl Pts',(165.746023029526,-5.70059801969011,333.404022616836));
#9403=CARTESIAN_POINT('Ctrl Pts',(165.737031645728,-5.74892617985712,333.587933734667));
#9404=CARTESIAN_POINT('Ctrl Pts',(165.72804026193,-5.78832629189741,333.773945637001));
#9405=CARTESIAN_POINT('Ctrl Pts',(165.719102717181,-5.8274904820159,333.95884372815));
#9406=CARTESIAN_POINT('Ctrl Pts',(165.710165172431,-5.85783316547064,334.145817522432));
#9407=CARTESIAN_POINT('Ctrl Pts',(165.701227627682,-5.87915919723639,334.334103839889));
#9408=CARTESIAN_POINT('Ctrl Pts',(165.692387285589,-5.90025329204519,334.520342399189));
#9409=CARTESIAN_POINT('Ctrl Pts',(165.683546943495,-5.91252573367141,334.707865066868));
#9410=CARTESIAN_POINT('Ctrl Pts',(165.674706601402,-5.91583437631538,334.895912563173));
#9411=CARTESIAN_POINT('Ctrl Pts',(165.67315508713,-5.91641505591232,334.928915627));
#9412=CARTESIAN_POINT('Ctrl Pts',(165.671603572858,-5.9167197549969,334.961934804774));
#9413=CARTESIAN_POINT('Ctrl Pts',(165.670052058585,-5.91674785846066,334.994965925983));
#9414=CARTESIAN_POINT('',(163.92005197593,-5.91236359159777,335.002943397715));
#9415=CARTESIAN_POINT('Ctrl Pts',(165.670052004703,-5.9125949101779,334.994970605717));
#9416=CARTESIAN_POINT('Ctrl Pts',(165.605626796152,-5.90157047433765,336.365605316277));
#9417=CARTESIAN_POINT('Ctrl Pts',(165.448455576177,-4.74432772518099,339.726187368728));
#9418=CARTESIAN_POINT('Ctrl Pts',(165.198538344775,0.852320882572409,341.944506608418));
#9419=CARTESIAN_POINT('Ctrl Pts',(164.920300310502,6.30102349729095,338.041336187897));
#9420=CARTESIAN_POINT('Ctrl Pts',(164.642062276227,5.96736985149999,331.347176437792));
#9421=CARTESIAN_POINT('Ctrl Pts',(164.363824241953,0.157548971222278,328.005158955138));
#9422=CARTESIAN_POINT('Ctrl Pts',(164.123154151445,-4.99288378853887,330.666738550612));
#9423=CARTESIAN_POINT('Ctrl Pts',(163.975230072362,-5.90312434765324,333.826940535229));
#9424=CARTESIAN_POINT('Ctrl Pts',(163.920052004703,-5.90839865240753,335.00294081012));
#9425=CARTESIAN_POINT('',(162.170052004703,-5.92027431987653,335.003792543636));
#9426=CARTESIAN_POINT('Ctrl Pts',(163.920051944103,-5.91674926645136,335.002946259889));
#9427=CARTESIAN_POINT('Ctrl Pts',(163.911914879253,-5.91666278780247,335.17661474182));
#9428=CARTESIAN_POINT('Ctrl Pts',(163.903777814403,-5.90892594379626,335.350022803605));
#9429=CARTESIAN_POINT('Ctrl Pts',(163.895640749552,-5.8936319271713,335.522525855367));
#9430=CARTESIAN_POINT('Ctrl Pts',(163.887462804686,-5.87826107453063,335.695895549786));
#9431=CARTESIAN_POINT('Ctrl Pts',(163.87928485982,-5.85525700650048,335.868350886963));
#9432=CARTESIAN_POINT('Ctrl Pts',(163.871106914954,-5.82476469640279,336.03925299809));
#9433=CARTESIAN_POINT('Ctrl Pts',(163.862908238715,-5.79419508724312,336.210588351987));
#9434=CARTESIAN_POINT('Ctrl Pts',(163.854709562475,-5.75609933448853,336.380362378213));
#9435=CARTESIAN_POINT('Ctrl Pts',(163.846510886235,-5.71067252318331,336.547950223831));
#9436=CARTESIAN_POINT('Ctrl Pts',(163.838282869471,-5.66508314337878,336.716137814485));
#9437=CARTESIAN_POINT('Ctrl Pts',(163.830054852706,-5.61211025401772,336.882123336397));
#9438=CARTESIAN_POINT('Ctrl Pts',(163.821826835942,-5.55199864370271,337.045297441162));
#9439=CARTESIAN_POINT('Ctrl Pts',(163.817000615097,-5.5167396116611,337.141008751475));
#9440=CARTESIAN_POINT('Ctrl Pts',(163.812174394251,-5.47902537499804,337.235753222751));
#9441=CARTESIAN_POINT('Ctrl Pts',(163.807348173406,-5.43891266166284,337.329411861673));
#9442=CARTESIAN_POINT('Ctrl Pts',(163.799924195968,-5.37720892113168,337.473483101787));
#9443=CARTESIAN_POINT('Ctrl Pts',(163.79250021853,-5.30968369431148,337.615318283778));
#9444=CARTESIAN_POINT('Ctrl Pts',(163.785076241092,-5.23652009251177,337.754412438837));
#9445=CARTESIAN_POINT('Ctrl Pts',(163.777661025064,-5.16344283477019,337.893342441866));
#9446=CARTESIAN_POINT('Ctrl Pts',(163.770245809037,-5.08474061925313,338.029537529839));
#9447=CARTESIAN_POINT('Ctrl Pts',(163.762830593009,-5.00064491737444,338.162511813865));
#9448=CARTESIAN_POINT('Ctrl Pts',(163.755422511865,-4.91663013195663,338.295358150705));
#9449=CARTESIAN_POINT('Ctrl Pts',(163.748014430721,-4.82723238982313,338.424989539893));
#9450=CARTESIAN_POINT('Ctrl Pts',(163.740606349577,-4.73272939838828,338.550943959588));
#9451=CARTESIAN_POINT('Ctrl Pts',(163.733203782403,-4.63829674725599,338.676804629107));
#9452=CARTESIAN_POINT('Ctrl Pts',(163.725801215229,-4.53876663606076,338.798993481325));
#9453=CARTESIAN_POINT('Ctrl Pts',(163.718398648055,-4.43446040394281,338.917076906108));
#9454=CARTESIAN_POINT('Ctrl Pts',(163.7109999783,-4.33020908860024,339.035098160484));
#9455=CARTESIAN_POINT('Ctrl Pts',(163.703601308545,-4.22118690677906,339.149018013152));
#9456=CARTESIAN_POINT('Ctrl Pts',(163.69620263879,-4.10775577263092,339.258435519638));
#9457=CARTESIAN_POINT('Ctrl Pts',(163.688805189586,-3.99434335109758,339.367834975634));
#9458=CARTESIAN_POINT('Ctrl Pts',(163.681407740382,-3.87652368912112,339.472733300709));
#9459=CARTESIAN_POINT('Ctrl Pts',(163.674010291178,-3.75469597389218,339.572765979813));
#9460=CARTESIAN_POINT('Ctrl Pts',(163.666613162715,-3.63287354090064,339.672794321675));
#9461=CARTESIAN_POINT('Ctrl Pts',(163.659216034251,-3.50704368862962,339.767957200201));
#9462=CARTESIAN_POINT('Ctrl Pts',(163.651818905788,-3.377638924035,339.857930203424));
#9463=CARTESIAN_POINT('Ctrl Pts',(163.644420638351,-3.24821423433705,339.947917060244));
#9464=CARTESIAN_POINT('Ctrl Pts',(163.637022370915,-3.11521384274522,340.03271223756));
#9465=CARTESIAN_POINT('Ctrl Pts',(163.629624103478,-2.97909935202512,340.11203458647));
#9466=CARTESIAN_POINT('Ctrl Pts',(163.622223236952,-2.84293704285288,340.191384802155));
#9467=CARTESIAN_POINT('Ctrl Pts',(163.614822370427,-2.70365877861787,340.265258173621));
#9468=CARTESIAN_POINT('Ctrl Pts',(163.607421503901,-2.56175072887888,340.333419518994));
#9469=CARTESIAN_POINT('Ctrl Pts',(163.600012510516,-2.41968685053427,340.401655712041));
#9470=CARTESIAN_POINT('Ctrl Pts',(163.592603517131,-2.27498775630009,340.46416719109));
#9471=CARTESIAN_POINT('Ctrl Pts',(163.585194523746,-2.12816023657423,340.520766665053));
#9472=CARTESIAN_POINT('Ctrl Pts',(163.577780966166,-1.98124226603168,340.577401006245));
#9473=CARTESIAN_POINT('Ctrl Pts',(163.570367408586,-1.83219360978396,340.628115965247));
#9474=CARTESIAN_POINT('Ctrl Pts',(163.562953851006,-1.68153567892164,340.672774305665));
#9475=CARTESIAN_POINT('Ctrl Pts',(163.555529738869,-1.53066325891303,340.717496225407));
#9476=CARTESIAN_POINT('Ctrl Pts',(163.548105626732,-1.37817734930732,340.756144213852));
#9477=CARTESIAN_POINT('Ctrl Pts',(163.540681514596,-1.22460979870516,340.788632083957));
#9478=CARTESIAN_POINT('Ctrl Pts',(163.536824389441,-1.14482527344265,340.805510840458));
#9479=CARTESIAN_POINT('Ctrl Pts',(163.532967264287,-1.06474888976958,340.820727698219));
#9480=CARTESIAN_POINT('Ctrl Pts',(163.529110139132,-0.984455595665917,340.834276111281));
#9481=CARTESIAN_POINT('Ctrl Pts',(163.521686161694,-0.829911581668405,340.860353334308));
#9482=CARTESIAN_POINT('Ctrl Pts',(163.514262184256,-0.674097576382707,340.880325085964));
#9483=CARTESIAN_POINT('Ctrl Pts',(163.506838206818,-0.517537310889843,340.894072080857));
#9484=CARTESIAN_POINT('Ctrl Pts',(163.499422990791,-0.361161810065995,340.907802852228));
#9485=CARTESIAN_POINT('Ctrl Pts',(163.492007774763,-0.204042170246386,340.915323457136));
#9486=CARTESIAN_POINT('Ctrl Pts',(163.484592558736,-0.0467122482306003,
340.916565602473));
#9487=CARTESIAN_POINT('Ctrl Pts',(163.477184477591,0.110466291726413,340.917806552623));
#9488=CARTESIAN_POINT('Ctrl Pts',(163.469776396447,0.267854340367967,340.912781066983));
#9489=CARTESIAN_POINT('Ctrl Pts',(163.462368315303,0.424913090254497,340.901472649113));
#9490=CARTESIAN_POINT('Ctrl Pts',(163.454965748129,0.581854938444996,340.890172648305));
#9491=CARTESIAN_POINT('Ctrl Pts',(163.447563180955,0.738467605263232,340.872599053549));
#9492=CARTESIAN_POINT('Ctrl Pts',(163.440160613781,0.894212563651498,340.848787434461));
#9493=CARTESIAN_POINT('Ctrl Pts',(163.432761944026,1.04987552300004,340.824988352086));
#9494=CARTESIAN_POINT('Ctrl Pts',(163.425363274272,1.20467131575669,340.794957842505));
#9495=CARTESIAN_POINT('Ctrl Pts',(163.417964604517,1.35806692664593,340.758783272988));
#9496=CARTESIAN_POINT('Ctrl Pts',(163.410567155313,1.51143723202248,340.722614671152));
#9497=CARTESIAN_POINT('Ctrl Pts',(163.403169706109,1.66340745107125,340.680304106587));
#9498=CARTESIAN_POINT('Ctrl Pts',(163.395772256905,1.81345503221666,340.631990004308));
#9499=CARTESIAN_POINT('Ctrl Pts',(163.388375128442,1.96349610756049,340.583677996845));
#9500=CARTESIAN_POINT('Ctrl Pts',(163.380977999978,2.11161435550307,340.529363083624));
#9501=CARTESIAN_POINT('Ctrl Pts',(163.373580871515,2.25730291676891,340.469233411041));
#9502=CARTESIAN_POINT('Ctrl Pts',(163.366182604078,2.40301391043637,340.40909447999));
#9503=CARTESIAN_POINT('Ctrl Pts',(163.358784336641,2.54629412751842,340.343139149254));
#9504=CARTESIAN_POINT('Ctrl Pts',(163.351386069205,2.68665734416086,340.271603444642));
#9505=CARTESIAN_POINT('Ctrl Pts',(163.343985202679,2.82706987187757,340.200042608786));
#9506=CARTESIAN_POINT('Ctrl Pts',(163.336584336153,2.96456302652566,340.122897665174));
#9507=CARTESIAN_POINT('Ctrl Pts',(163.329183469627,3.09867594440411,340.040450173751));
#9508=CARTESIAN_POINT('Ctrl Pts',(163.321774476243,3.23293613108799,339.957912147102));
#9509=CARTESIAN_POINT('Ctrl Pts',(163.314365482858,3.36380835016669,339.870060139962));
#9510=CARTESIAN_POINT('Ctrl Pts',(163.306956489473,3.49086085120392,339.777218969236));
#9511=CARTESIAN_POINT('Ctrl Pts',(163.299542931893,3.61799162096432,339.684320605147));
#9512=CARTESIAN_POINT('Ctrl Pts',(163.292129374313,3.74129769225111,339.586427184635));
#9513=CARTESIAN_POINT('Ctrl Pts',(163.284715816732,3.86038149459243,339.483902906923));
#9514=CARTESIAN_POINT('Ctrl Pts',(163.277291704596,3.9796348345275,339.381232667131));
#9515=CARTESIAN_POINT('Ctrl Pts',(163.269867592459,4.09465362785683,339.273918656769));
#9516=CARTESIAN_POINT('Ctrl Pts',(163.262443480322,4.20507758426156,339.162361477916));
#9517=CARTESIAN_POINT('Ctrl Pts',(163.258586355168,4.26244727535505,339.104403032137));
#9518=CARTESIAN_POINT('Ctrl Pts',(163.254729230013,4.31857738167461,339.045299807624));
#9519=CARTESIAN_POINT('Ctrl Pts',(163.250872104858,4.37342183993305,338.985111287342));
#9520=CARTESIAN_POINT('Ctrl Pts',(163.24344812742,4.47898336681745,338.86926381061));
#9521=CARTESIAN_POINT('Ctrl Pts',(163.236024149982,4.5800979377291,338.749044350219));
#9522=CARTESIAN_POINT('Ctrl Pts',(163.228600172544,4.67638182209828,338.624828770639));
#9523=CARTESIAN_POINT('Ctrl Pts',(163.221184956517,4.77255207699727,338.500759784131));
#9524=CARTESIAN_POINT('Ctrl Pts',(163.213769740489,4.8639027667394,338.372704357855));
#9525=CARTESIAN_POINT('Ctrl Pts',(163.206354524461,4.95008756164463,338.241074466061));
#9526=CARTESIAN_POINT('Ctrl Pts',(163.198946443317,5.03618942997412,338.109571227886));
#9527=CARTESIAN_POINT('Ctrl Pts',(163.191538362173,5.11713509592958,337.974500681415));
#9528=CARTESIAN_POINT('Ctrl Pts',(163.184130281029,5.19261910768074,337.836306994147));
#9529=CARTESIAN_POINT('Ctrl Pts',(163.176727713855,5.26804693530333,337.698216166965));
#9530=CARTESIAN_POINT('Ctrl Pts',(163.169325146681,5.3380210250051,337.557007153758));
#9531=CARTESIAN_POINT('Ctrl Pts',(163.161922579507,5.40227986014308,337.413152062178));
#9532=CARTESIAN_POINT('Ctrl Pts',(163.154523909752,5.46650486328523,337.269372709674));
#9533=CARTESIAN_POINT('Ctrl Pts',(163.147125239998,5.52502045274703,337.122950393237));
#9534=CARTESIAN_POINT('Ctrl Pts',(163.139726570243,5.57761165238015,336.974380616227));
#9535=CARTESIAN_POINT('Ctrl Pts',(163.132329121039,5.63019417609838,336.825835348617));
#9536=CARTESIAN_POINT('Ctrl Pts',(163.124931671835,5.67685412527571,336.67514367501));
#9537=CARTESIAN_POINT('Ctrl Pts',(163.117534222631,5.7174251218197,336.522819929895));
#9538=CARTESIAN_POINT('Ctrl Pts',(163.110137094167,5.757994359276,336.370502789272));
#9539=CARTESIAN_POINT('Ctrl Pts',(163.102739965704,5.79247507297557,336.21655407848));
#9540=CARTESIAN_POINT('Ctrl Pts',(163.095342837241,5.82075118859921,336.061501843108));
#9541=CARTESIAN_POINT('Ctrl Pts',(163.087944569804,5.8490316580388,335.906425733562));
#9542=CARTESIAN_POINT('Ctrl Pts',(163.080546302367,5.87110556020794,335.750246128291));
#9543=CARTESIAN_POINT('Ctrl Pts',(163.073148034931,5.88690825061817,335.593499630416));
#9544=CARTESIAN_POINT('Ctrl Pts',(163.065747168405,5.90271649267974,335.436698065847));
#9545=CARTESIAN_POINT('Ctrl Pts',(163.058346301879,5.91224909911652,335.279329583252));
#9546=CARTESIAN_POINT('Ctrl Pts',(163.050945435354,5.91549343990135,335.12193410099));
#9547=CARTESIAN_POINT('Ctrl Pts',(163.043536441969,5.91874134328252,334.96436578344));
#9548=CARTESIAN_POINT('Ctrl Pts',(163.036127448584,5.91568718342874,334.806770780371));
#9549=CARTESIAN_POINT('Ctrl Pts',(163.028718455199,5.90637046086806,334.649687936997));
#9550=CARTESIAN_POINT('Ctrl Pts',(163.021304897619,5.89704799888492,334.492508325174));
#9551=CARTESIAN_POINT('Ctrl Pts',(163.013891340039,5.88145532358617,334.335841872247));
#9552=CARTESIAN_POINT('Ctrl Pts',(163.006477782459,5.85968354967255,334.180219992805));
#9553=CARTESIAN_POINT('Ctrl Pts',(162.999053670322,5.83788077965292,334.024376557127));
#9554=CARTESIAN_POINT('Ctrl Pts',(162.991629558185,5.80988140774299,333.869581031314));
#9555=CARTESIAN_POINT('Ctrl Pts',(162.984205446049,5.77582733501344,333.716353179955));
#9556=CARTESIAN_POINT('Ctrl Pts',(162.980348320894,5.75813487319067,333.636745142118));
#9557=CARTESIAN_POINT('Ctrl Pts',(162.976491195739,5.73880893206018,333.557559992103));
#9558=CARTESIAN_POINT('Ctrl Pts',(162.972634070584,5.71787460462632,333.478868655155));
#9559=CARTESIAN_POINT('Ctrl Pts',(162.965210093146,5.67758138926146,333.327407998155));
#9560=CARTESIAN_POINT('Ctrl Pts',(162.957786115708,5.63120517652213,333.177320950082));
#9561=CARTESIAN_POINT('Ctrl Pts',(162.95036213827,5.57885438022989,333.02913359999));
#9562=CARTESIAN_POINT('Ctrl Pts',(162.942946922243,5.52656536575387,332.881121133266));
#9563=CARTESIAN_POINT('Ctrl Pts',(162.935531706215,5.46831592577613,332.735004250404));
#9564=CARTESIAN_POINT('Ctrl Pts',(162.928116490187,5.40426507937176,332.591297130325));
#9565=CARTESIAN_POINT('Ctrl Pts',(162.920708409043,5.34027586236931,332.447728284513));
#9566=CARTESIAN_POINT('Ctrl Pts',(162.913300327899,5.27049650274748,332.306564924069));
#9567=CARTESIAN_POINT('Ctrl Pts',(162.905892246755,5.19513521292146,332.168304274474));
#9568=CARTESIAN_POINT('Ctrl Pts',(162.898489679581,5.1198300158798,332.030146534805));
#9569=CARTESIAN_POINT('Ctrl Pts',(162.891087112407,5.03895133916165,331.894887530325));
#9570=CARTESIAN_POINT('Ctrl Pts',(162.883684545233,4.95275466650203,331.763002660498));
#9571=CARTESIAN_POINT('Ctrl Pts',(162.876285875478,4.86660337601388,331.631187227478));
#9572=CARTESIAN_POINT('Ctrl Pts',(162.868887205724,4.77513986942057,331.50274270279));
#9573=CARTESIAN_POINT('Ctrl Pts',(162.861488535969,4.67866449013922,331.378118009762));
#9574=CARTESIAN_POINT('Ctrl Pts',(162.854091086765,4.58220502629965,331.253513875939));
#9575=CARTESIAN_POINT('Ctrl Pts',(162.846693637561,4.48073555894519,331.132728617954));
#9576=CARTESIAN_POINT('Ctrl Pts',(162.839296188357,4.37459856618621,331.016180482599));
#9577=CARTESIAN_POINT('Ctrl Pts',(162.831899059893,4.26846617534221,330.899637400569));
#9578=CARTESIAN_POINT('Ctrl Pts',(162.82450193143,4.15766691277109,330.78733135182));
#9579=CARTESIAN_POINT('Ctrl Pts',(162.817104802967,4.04258200879939,330.679645701493));
#9580=CARTESIAN_POINT('Ctrl Pts',(162.80970653553,3.92747938462536,330.571943470263));
#9581=CARTESIAN_POINT('Ctrl Pts',(162.802308268093,3.80809007767113,330.468863309007));
#9582=CARTESIAN_POINT('Ctrl Pts',(162.794910000657,3.68483034610691,330.370749965393));
#9583=CARTESIAN_POINT('Ctrl Pts',(162.787509134131,3.56152731210267,330.272602153529));
#9584=CARTESIAN_POINT('Ctrl Pts',(162.780108267605,3.43435143810209,330.179424865673));
#9585=CARTESIAN_POINT('Ctrl Pts',(162.772707401079,3.30374991814138,330.091520903489));
#9586=CARTESIAN_POINT('Ctrl Pts',(162.765298407695,3.17300498522576,330.003520414351));
#9587=CARTESIAN_POINT('Ctrl Pts',(162.75788941431,3.03882720385781,329.92080502357));
#9588=CARTESIAN_POINT('Ctrl Pts',(162.750480420925,2.90169107647838,329.843633114373));
#9589=CARTESIAN_POINT('Ctrl Pts',(162.743066863345,2.7644704685141,329.766413664619));
#9590=CARTESIAN_POINT('Ctrl Pts',(162.735653305765,2.62428821460374,329.694744670735));
#9591=CARTESIAN_POINT('Ctrl Pts',(162.728239748184,2.48164050000462,329.628837091352));
#9592=CARTESIAN_POINT('Ctrl Pts',(162.720815636048,2.33878970026872,329.562835680463));
#9593=CARTESIAN_POINT('Ctrl Pts',(162.713391523911,2.19346677345098,329.50261220846));
#9594=CARTESIAN_POINT('Ctrl Pts',(162.705967411774,2.04618559149351,329.448328622148));
#9595=CARTESIAN_POINT('Ctrl Pts',(162.70211028662,1.96966708782925,329.420126113565));
#9596=CARTESIAN_POINT('Ctrl Pts',(162.698253161465,1.89262023017412,329.393526081447));
#9597=CARTESIAN_POINT('Ctrl Pts',(162.69439603631,1.81511824034429,329.368545806271));
#9598=CARTESIAN_POINT('Ctrl Pts',(162.686972058872,1.66594677174351,329.320465178376));
#9599=CARTESIAN_POINT('Ctrl Pts',(162.679548081434,1.5146385412722,329.278243211356));
#9600=CARTESIAN_POINT('Ctrl Pts',(162.672124103996,1.36169461737936,329.24207343469));
#9601=CARTESIAN_POINT('Ctrl Pts',(162.664708887969,1.20893119032833,329.205946343803));
#9602=CARTESIAN_POINT('Ctrl Pts',(162.657293671941,1.05453627193794,329.175857311075));
#9603=CARTESIAN_POINT('Ctrl Pts',(162.649878455913,0.899028300580285,329.151950865694));
#9604=CARTESIAN_POINT('Ctrl Pts',(162.642470374769,0.743669958209789,329.128067422974));
#9605=CARTESIAN_POINT('Ctrl Pts',(162.635062293625,0.587201061394004,329.110354780869));
#9606=CARTESIAN_POINT('Ctrl Pts',(162.627654212481,0.430152413333387,329.098906926357));
#9607=CARTESIAN_POINT('Ctrl Pts',(162.620251645307,0.273220659449661,329.087467592691));
#9608=CARTESIAN_POINT('Ctrl Pts',(162.612849078133,0.115710384168476,329.08228378893));
#9609=CARTESIAN_POINT('Ctrl Pts',(162.605446510959,-0.0418403820498371,
329.083397939279));
#9610=CARTESIAN_POINT('Ctrl Pts',(162.598047841204,-0.199308198478223,329.084511503033));
#9611=CARTESIAN_POINT('Ctrl Pts',(162.59064917145,-0.356816091125044,329.091916414561));
#9612=CARTESIAN_POINT('Ctrl Pts',(162.583250501695,-0.513824017728563,329.10560304685));
#9613=CARTESIAN_POINT('Ctrl Pts',(162.575853052491,-0.670806042899634,329.119287421269));
#9614=CARTESIAN_POINT('Ctrl Pts',(162.568455603287,-0.827287894281514,329.139251427372));
#9615=CARTESIAN_POINT('Ctrl Pts',(162.561058154083,-0.982732524667903,329.165433405345));
#9616=CARTESIAN_POINT('Ctrl Pts',(162.55366102562,-1.13817041524606,329.191614248114));
#9617=CARTESIAN_POINT('Ctrl Pts',(162.546263897156,-1.29257080622066,329.224012464711));
#9618=CARTESIAN_POINT('Ctrl Pts',(162.538866768693,-1.44540501206314,329.262514931296));
#9619=CARTESIAN_POINT('Ctrl Pts',(162.531468501256,-1.598262750558,329.3010233263));
#9620=CARTESIAN_POINT('Ctrl Pts',(162.524070233819,-1.74955346182676,329.345637751582));
#9621=CARTESIAN_POINT('Ctrl Pts',(162.516671966383,-1.89876197901937,329.396194729514));
#9622=CARTESIAN_POINT('Ctrl Pts',(162.509271099857,-2.04802291473358,329.446769468643));
#9623=CARTESIAN_POINT('Ctrl Pts',(162.501870233331,-2.19519984671405,329.503290797298));
#9624=CARTESIAN_POINT('Ctrl Pts',(162.494469366805,-2.33979614022765,329.565546523828));
#9625=CARTESIAN_POINT('Ctrl Pts',(162.487060373421,-2.4845512142954,329.627870613098));
#9626=CARTESIAN_POINT('Ctrl Pts',(162.479651380036,-2.62671964767688,329.695941527848));
#9627=CARTESIAN_POINT('Ctrl Pts',(162.472242386651,-2.76582737990481,329.769500074843));
#9628=CARTESIAN_POINT('Ctrl Pts',(162.464828829071,-2.90502080729398,329.84310393644));
#9629=CARTESIAN_POINT('Ctrl Pts',(162.457415271491,-3.0411494544888,329.922201979454));
#9630=CARTESIAN_POINT('Ctrl Pts',(162.45000171391,-3.17376740756234,330.006491112935));
#9631=CARTESIAN_POINT('Ctrl Pts',(162.442577601774,-3.30657416657106,330.090900247429));
#9632=CARTESIAN_POINT('Ctrl Pts',(162.435153489637,-3.43585994331866,330.180515020596));
#9633=CARTESIAN_POINT('Ctrl Pts',(162.4277293775,-3.56121046768816,330.274990945265));
#9634=CARTESIAN_POINT('Ctrl Pts',(162.423872252346,-3.62633511179299,330.324074991794));
#9635=CARTESIAN_POINT('Ctrl Pts',(162.420015127191,-3.69039812191298,330.37447053443));
#9636=CARTESIAN_POINT('Ctrl Pts',(162.416158002036,-3.75334534200005,330.426125350845));
#9637=CARTESIAN_POINT('Ctrl Pts',(162.408834076206,-3.87286979418515,330.524207738377));
#9638=CARTESIAN_POINT('Ctrl Pts',(162.401510150377,-3.98875087258847,330.62714595177));
#9639=CARTESIAN_POINT('Ctrl Pts',(162.394186224547,-4.10056070490289,330.734635716858));
#9640=CARTESIAN_POINT('Ctrl Pts',(162.386870990571,-4.21223784407263,330.84199791575));
#9641=CARTESIAN_POINT('Ctrl Pts',(162.379555756595,-4.31985307605865,330.953900655882));
#9642=CARTESIAN_POINT('Ctrl Pts',(162.372240522619,-4.42300982275395,331.069998133547));
#9643=CARTESIAN_POINT('Ctrl Pts',(162.364932271489,-4.52606809992302,331.185984788955));
#9644=CARTESIAN_POINT('Ctrl Pts',(162.357624020358,-4.62467610732625,331.306157928751));
#9645=CARTESIAN_POINT('Ctrl Pts',(162.350315769228,-4.71847271683409,331.43013364634));
#9646=CARTESIAN_POINT('Ctrl Pts',(162.342804779039,-4.81487134916897,331.55754858896));
#9647=CARTESIAN_POINT('Ctrl Pts',(162.335293788851,-4.90618744902999,331.688979879911));
#9648=CARTESIAN_POINT('Ctrl Pts',(162.327782798662,-4.99207144355252,331.823972093169));
#9649=CARTESIAN_POINT('Ctrl Pts',(162.320483051653,-5.07553998983188,331.955167711892));
#9650=CARTESIAN_POINT('Ctrl Pts',(162.313183304644,-5.15387765041819,332.089726301311));
#9651=CARTESIAN_POINT('Ctrl Pts',(162.305883557635,-5.22680629540618,332.22719879674));
#9652=CARTESIAN_POINT('Ctrl Pts',(162.298585222039,-5.29972083956195,332.364644711712));
#9653=CARTESIAN_POINT('Ctrl Pts',(162.291286886444,-5.36722826889103,332.505003072579));
#9654=CARTESIAN_POINT('Ctrl Pts',(162.283988550849,-5.42909594822425,332.647799381967));
#9655=CARTESIAN_POINT('Ctrl Pts',(162.276690094723,-5.49096464928864,332.790598049604));
#9656=CARTESIAN_POINT('Ctrl Pts',(162.269391638598,-5.54719326293106,332.935834393082));
#9657=CARTESIAN_POINT('Ctrl Pts',(162.262093182472,-5.59759705042366,333.083013348093));
#9658=CARTESIAN_POINT('Ctrl Pts',(162.254423084325,-5.65056743079071,333.237686748979));
#9659=CARTESIAN_POINT('Ctrl Pts',(162.246752986177,-5.69710406747602,333.39450534185));
#9660=CARTESIAN_POINT('Ctrl Pts',(162.23908288803,-5.73705189812322,333.552876618688));
#9661=CARTESIAN_POINT('Ctrl Pts',(162.231776197098,-5.77510701115041,333.703744306437));
#9662=CARTESIAN_POINT('Ctrl Pts',(162.224469506166,-5.80718324959507,333.856020543179));
#9663=CARTESIAN_POINT('Ctrl Pts',(162.217162815235,-5.8331992311469,334.009183522418));
#9664=CARTESIAN_POINT('Ctrl Pts',(162.209852166545,-5.85922930457227,334.162429464252));
#9665=CARTESIAN_POINT('Ctrl Pts',(162.202541517855,-5.87919253479397,334.316562725204));
#9666=CARTESIAN_POINT('Ctrl Pts',(162.195230869165,-5.89305947556703,334.4710571109));
#9667=CARTESIAN_POINT('Ctrl Pts',(162.187911768722,-5.90694244774457,334.625730105708));
#9668=CARTESIAN_POINT('Ctrl Pts',(162.180592668278,-5.91471504814765,334.780764676496));
#9669=CARTESIAN_POINT('Ctrl Pts',(162.173273567835,-5.91639989463546,334.93563503082));
#9670=CARTESIAN_POINT('Ctrl Pts',(162.172199713458,-5.9166470943822,334.958357523725));
#9671=CARTESIAN_POINT('Ctrl Pts',(162.17112585908,-5.91676333648397,334.981076491471));
#9672=CARTESIAN_POINT('Ctrl Pts',(162.170052004703,-5.91674878596669,335.00379028517));
#9673=CARTESIAN_POINT('',(160.420052004703,-5.91893227834984,334.995030093563));
#9674=CARTESIAN_POINT('Ctrl Pts',(162.170052004703,-5.92337931611586,335.003794532705));
#9675=CARTESIAN_POINT('Ctrl Pts',(162.159341325723,-5.92507004615438,335.230598138262));
#9676=CARTESIAN_POINT('Ctrl Pts',(162.055884635312,-5.8101798197072,337.419612438354));
#9677=CARTESIAN_POINT('Ctrl Pts',(161.859681933494,-3.08383468430733,341.280333316078));
#9678=CARTESIAN_POINT('Ctrl Pts',(161.581443899212,3.61242637245241,340.991911099545));
#9679=CARTESIAN_POINT('Ctrl Pts',(161.303205864942,6.99361706653863,335.204800507416));
#9680=CARTESIAN_POINT('Ctrl Pts',(161.024967830666,3.95686860428096,329.229747512485));
#9681=CARTESIAN_POINT('Ctrl Pts',(160.746729796393,-2.71103977284048,328.549970056558));
#9682=CARTESIAN_POINT('Ctrl Pts',(160.545091187738,-5.74029804598019,332.346895813797));
#9683=CARTESIAN_POINT('Ctrl Pts',(160.436198590508,-5.92331568745704,334.65264523622));
#9684=CARTESIAN_POINT('Ctrl Pts',(160.420052004703,-5.92023889988851,334.995028996442));
#9685=CARTESIAN_POINT('',(158.670052029646,-5.9115263163086,334.998821163383));
#9686=CARTESIAN_POINT('Ctrl Pts',(160.420052004703,-5.91674791424796,334.995031927692));
#9687=CARTESIAN_POINT('Ctrl Pts',(160.412749604594,-5.91687785434,335.149784660933));
#9688=CARTESIAN_POINT('Ctrl Pts',(160.405447204486,-5.91093230913336,335.304751775812));
#9689=CARTESIAN_POINT('Ctrl Pts',(160.398144804377,-5.89888753872582,335.459408715596));
#9690=CARTESIAN_POINT('Ctrl Pts',(160.390848879078,-5.88685344803854,335.61392852592));
#9691=CARTESIAN_POINT('Ctrl Pts',(160.383552953779,-5.86873092290481,335.768138326656));
#9692=CARTESIAN_POINT('Ctrl Pts',(160.376257028479,-5.84454826906993,335.921512936975));
#9693=CARTESIAN_POINT('Ctrl Pts',(160.368965870975,-5.82038141829307,336.074787318928));
#9694=CARTESIAN_POINT('Ctrl Pts',(160.36167471347,-5.79016238049308,336.227227217478));
#9695=CARTESIAN_POINT('Ctrl Pts',(160.354383555966,-5.75397132106502,336.378312228365));
#9696=CARTESIAN_POINT('Ctrl Pts',(160.347094686519,-5.71779161884968,336.529349826863));
#9697=CARTESIAN_POINT('Ctrl Pts',(160.339805817072,-5.67564370952146,336.679033008618));
#9698=CARTESIAN_POINT('Ctrl Pts',(160.332516947625,-5.6276589060248,336.826851334931));
#9699=CARTESIAN_POINT('Ctrl Pts',(160.325229030337,-5.57968037087738,336.974650351445));
#9700=CARTESIAN_POINT('Ctrl Pts',(160.317941113049,-5.52586657691341,337.120584630543));
#9701=CARTESIAN_POINT('Ctrl Pts',(160.310653195762,-5.46639867417403,337.264159026546));
#9702=CARTESIAN_POINT('Ctrl Pts',(160.303364692781,-5.40692599230215,337.407744960892));
#9703=CARTESIAN_POINT('Ctrl Pts',(160.296076189801,-5.34179844518155,337.548970278778));
#9704=CARTESIAN_POINT('Ctrl Pts',(160.28878768682,-5.27124515581358,337.687360241912));
#9705=CARTESIAN_POINT('Ctrl Pts',(160.281497059991,-5.20067130742247,337.825790531479));
#9706=CARTESIAN_POINT('Ctrl Pts',(160.274206433162,-5.12466874639831,337.961383479486));
#9707=CARTESIAN_POINT('Ctrl Pts',(160.266915806333,-5.04351216682569,338.093689639505));
#9708=CARTESIAN_POINT('Ctrl Pts',(160.259617581489,-4.96227100894461,338.226133683985));
#9709=CARTESIAN_POINT('Ctrl Pts',(160.252319356645,-4.87586531029611,338.355283773128));
#9710=CARTESIAN_POINT('Ctrl Pts',(160.245021131802,-4.78461294959435,338.480719679186));
#9711=CARTESIAN_POINT('Ctrl Pts',(160.237718620924,-4.69330699905403,338.606229250078));
#9712=CARTESIAN_POINT('Ctrl Pts',(160.230416110047,-4.5971489570975,338.72801999315));
#9713=CARTESIAN_POINT('Ctrl Pts',(160.223113599169,-4.49649592147139,338.845706045799));
#9714=CARTESIAN_POINT('Ctrl Pts',(160.215800846283,-4.39570171668679,338.963557156966));
#9715=CARTESIAN_POINT('Ctrl Pts',(160.208488093396,-4.29040019302738,339.077291802976));
#9716=CARTESIAN_POINT('Ctrl Pts',(160.201175340509,-4.18098452699986,339.186561709504));
#9717=CARTESIAN_POINT('Ctrl Pts',(160.197534802954,-4.12651368032173,339.240959992137));
#9718=CARTESIAN_POINT('Ctrl Pts',(160.193894265399,-4.07102369912965,339.294252372113));
#9719=CARTESIAN_POINT('Ctrl Pts',(160.190253727844,-4.01456592510909,339.346399774003));
#9720=CARTESIAN_POINT('Ctrl Pts',(160.182829750406,-3.89943423529873,339.452741524152));
#9721=CARTESIAN_POINT('Ctrl Pts',(160.175405772968,-3.77990061924428,339.55466595567));
#9722=CARTESIAN_POINT('Ctrl Pts',(160.16798179553,-3.656338340465,339.651786807512));
#9723=CARTESIAN_POINT('Ctrl Pts',(160.160566579503,-3.5329218837653,339.748793042137));
#9724=CARTESIAN_POINT('Ctrl Pts',(160.153151363475,-3.40548651867336,339.841006752827));
#9725=CARTESIAN_POINT('Ctrl Pts',(160.145736147447,-3.274441870336,339.928078834626));
#9726=CARTESIAN_POINT('Ctrl Pts',(160.138328066303,-3.14352331249969,340.015067136106));
#9727=CARTESIAN_POINT('Ctrl Pts',(160.130919985159,-3.00900269395467,340.096923452584));
#9728=CARTESIAN_POINT('Ctrl Pts',(160.123511904015,-2.87132210852129,340.173339338533));
#9729=CARTESIAN_POINT('Ctrl Pts',(160.116109336841,-2.73374400126222,340.249698346743));
#9730=CARTESIAN_POINT('Ctrl Pts',(160.108706769667,-2.59301093525265,340.320624807053));
#9731=CARTESIAN_POINT('Ctrl Pts',(160.101304202493,-2.44959324063972,340.385854019365));
#9732=CARTESIAN_POINT('Ctrl Pts',(160.093905532738,-2.30625105481628,340.451048888782));
#9733=CARTESIAN_POINT('Ctrl Pts',(160.086506862983,-2.16022739421783,340.510552329911));
#9734=CARTESIAN_POINT('Ctrl Pts',(160.079108193229,-2.01201629857973,340.564146024032));
#9735=CARTESIAN_POINT('Ctrl Pts',(160.071710744025,-1.86382965316995,340.617730876857));
#9736=CARTESIAN_POINT('Ctrl Pts',(160.064313294821,-1.71345663953757,340.665407790796));
#9737=CARTESIAN_POINT('Ctrl Pts',(160.056915845617,-1.56141045642998,340.707006916857));
#9738=CARTESIAN_POINT('Ctrl Pts',(160.049518717153,-1.40937086577999,340.748604239252));
#9739=CARTESIAN_POINT('Ctrl Pts',(160.04212158869,-1.25565860988089,340.784124199249));
#9740=CARTESIAN_POINT('Ctrl Pts',(160.034724460226,-1.1008009381068,340.813447157854));
#9741=CARTESIAN_POINT('Ctrl Pts',(160.02732619279,-0.945919422116997,340.842774631463));
#9742=CARTESIAN_POINT('Ctrl Pts',(160.019927925353,-0.789892505802936,340.865903134335));
#9743=CARTESIAN_POINT('Ctrl Pts',(160.012529657917,-0.63325634332054,340.88276439832));
#9744=CARTESIAN_POINT('Ctrl Pts',(160.005128791391,-0.476565152907182,340.899631585845));
#9745=CARTESIAN_POINT('Ctrl Pts',(159.997727924865,-0.319264661016791,340.910227110891));
#9746=CARTESIAN_POINT('Ctrl Pts',(159.990327058339,-0.161894688364802,340.914534696185));
#9747=CARTESIAN_POINT('Ctrl Pts',(159.982918064955,-0.00435190843748323,
340.91884701162));
#9748=CARTESIAN_POINT('Ctrl Pts',(159.97550907157,0.153260131325582,340.916857587913));
#9749=CARTESIAN_POINT('Ctrl Pts',(159.968100078185,0.310402331149898,340.908602284408));
#9750=CARTESIAN_POINT('Ctrl Pts',(159.960686520605,0.467641335989746,340.900341895352));
#9751=CARTESIAN_POINT('Ctrl Pts',(159.953272963025,0.624409553398733,340.885807969313));
#9752=CARTESIAN_POINT('Ctrl Pts',(159.945859405444,0.780174965370762,340.865088028829));
#9753=CARTESIAN_POINT('Ctrl Pts',(159.938435293308,0.936162137923267,340.844338589716));
#9754=CARTESIAN_POINT('Ctrl Pts',(159.931011181171,1.09114328698146,340.817385610743));
#9755=CARTESIAN_POINT('Ctrl Pts',(159.923587069034,1.24459770117596,340.784367478362));
#9756=CARTESIAN_POINT('Ctrl Pts',(159.91972994388,1.32432344752623,340.767213229258));
#9757=CARTESIAN_POINT('Ctrl Pts',(159.915872818725,1.40363735102046,340.748422681214));
#9758=CARTESIAN_POINT('Ctrl Pts',(159.91201569357,1.48246831851101,340.728020447512));
#9759=CARTESIAN_POINT('Ctrl Pts',(159.904591716132,1.63419772852416,340.688751376217));
#9760=CARTESIAN_POINT('Ctrl Pts',(159.897167738694,1.78459465593474,340.643390166656));
#9761=CARTESIAN_POINT('Ctrl Pts',(159.889743761256,1.93313229128134,340.59204167607));
#9762=CARTESIAN_POINT('Ctrl Pts',(159.882328545229,2.08149462986962,340.540753784429));
#9763=CARTESIAN_POINT('Ctrl Pts',(159.874913329201,2.22800169477283,340.483492797285));
#9764=CARTESIAN_POINT('Ctrl Pts',(159.867498113173,2.37213824451428,340.42041425644));
#9765=CARTESIAN_POINT('Ctrl Pts',(159.860090032029,2.5161361067931,340.357396409449));
#9766=CARTESIAN_POINT('Ctrl Pts',(159.852681950885,2.6577676551336,340.288572301203));
#9767=CARTESIAN_POINT('Ctrl Pts',(159.845273869741,2.79653426877775,340.214146780256));
#9768=CARTESIAN_POINT('Ctrl Pts',(159.837871302567,2.93519759589714,340.139776655583));
#9769=CARTESIAN_POINT('Ctrl Pts',(159.830468735393,3.070999906801,340.0598135954));
#9770=CARTESIAN_POINT('Ctrl Pts',(159.823066168219,3.20346408689925,339.974509865951));
#9771=CARTESIAN_POINT('Ctrl Pts',(159.815667498464,3.33585852518593,339.889251048543));
#9772=CARTESIAN_POINT('Ctrl Pts',(159.80826882871,3.46491801986771,339.798657363369));
#9773=CARTESIAN_POINT('Ctrl Pts',(159.800870158955,3.59019162882605,339.703026114196));
#9774=CARTESIAN_POINT('Ctrl Pts',(159.793472709751,3.71544457152872,339.607410641209));
#9775=CARTESIAN_POINT('Ctrl Pts',(159.786075260547,3.83691257168035,339.506759479811));
#9776=CARTESIAN_POINT('Ctrl Pts',(159.778677811343,3.954175078351,339.401412274742));
#9777=CARTESIAN_POINT('Ctrl Pts',(159.771280682879,4.07143250072357,339.296069637344));
#9778=CARTESIAN_POINT('Ctrl Pts',(159.763883554416,4.18448451454465,339.186031610541));
#9779=CARTESIAN_POINT('Ctrl Pts',(159.756486425953,4.29294518794165,339.071676826054));
#9780=CARTESIAN_POINT('Ctrl Pts',(159.749088158516,4.40142256157498,338.957304433786));
#9781=CARTESIAN_POINT('Ctrl Pts',(159.741689891079,4.50530693030502,338.838614231186));
#9782=CARTESIAN_POINT('Ctrl Pts',(159.734291623643,4.6042507422102,338.716020137911));
#9783=CARTESIAN_POINT('Ctrl Pts',(159.726890757117,4.70322931411653,338.593382976041));
#9784=CARTESIAN_POINT('Ctrl Pts',(159.719489890591,4.7972636392349,338.466839483126));
#9785=CARTESIAN_POINT('Ctrl Pts',(159.712089024066,4.88604790169609,338.336834797354));
#9786=CARTESIAN_POINT('Ctrl Pts',(159.704680030681,4.97492965776604,338.206687354007));
#9787=CARTESIAN_POINT('Ctrl Pts',(159.697271037296,5.0585496274213,338.073071435944));
#9788=CARTESIAN_POINT('Ctrl Pts',(159.689862043911,5.13664622772738,337.936459789215));
#9789=CARTESIAN_POINT('Ctrl Pts',(159.682448486331,5.21479093823327,337.799763984998));
#9790=CARTESIAN_POINT('Ctrl Pts',(159.675034928751,5.28740532755787,337.660069105139));
#9791=CARTESIAN_POINT('Ctrl Pts',(159.66762137117,5.35427508979995,337.517869898396));
#9792=CARTESIAN_POINT('Ctrl Pts',(159.660197259034,5.42124005339057,337.375468245049));
#9793=CARTESIAN_POINT('Ctrl Pts',(159.652773146897,5.48244391092731,337.230555486944));
#9794=CARTESIAN_POINT('Ctrl Pts',(159.64534903476,5.53772124773015,337.08364439023));
#9795=CARTESIAN_POINT('Ctrl Pts',(159.641491909606,5.56644004970121,337.00731816075));
#9796=CARTESIAN_POINT('Ctrl Pts',(159.637634784451,5.5935599811839,336.930452763466));
#9797=CARTESIAN_POINT('Ctrl Pts',(159.633777659296,5.61906326742996,336.853121301782));
#9798=CARTESIAN_POINT('Ctrl Pts',(159.626353681858,5.66815055759916,336.704278056161));
#9799=CARTESIAN_POINT('Ctrl Pts',(159.61892970442,5.71139375593611,336.553258518005));
#9800=CARTESIAN_POINT('Ctrl Pts',(159.611505726982,5.74859595230427,336.400562436898));
#9801=CARTESIAN_POINT('Ctrl Pts',(159.604090510955,5.78575424448335,336.248046560142));
#9802=CARTESIAN_POINT('Ctrl Pts',(159.596675294927,5.81688563817707,336.093858437896));
#9803=CARTESIAN_POINT('Ctrl Pts',(159.589260078899,5.84184210507707,335.938515520303));
#9804=CARTESIAN_POINT('Ctrl Pts',(159.581851997755,5.86677455899026,335.783322072882));
#9805=CARTESIAN_POINT('Ctrl Pts',(159.574443916611,5.88554385569258,335.626976408208));
#9806=CARTESIAN_POINT('Ctrl Pts',(159.567035835467,5.89805242439832,335.470008682419));
#9807=CARTESIAN_POINT('Ctrl Pts',(159.559633268293,5.91055168274794,335.313157790574));
#9808=CARTESIAN_POINT('Ctrl Pts',(159.552230701119,5.91679946226846,335.155686129975));
#9809=CARTESIAN_POINT('Ctrl Pts',(159.544828133945,5.91674970494396,334.9981314322));
#9810=CARTESIAN_POINT('Ctrl Pts',(159.53742946419,5.91669997381647,334.840659686284));
#9811=CARTESIAN_POINT('Ctrl Pts',(159.530030794436,5.91035930922668,334.68310536253));
#9812=CARTESIAN_POINT('Ctrl Pts',(159.522632124681,5.8977336895992,334.526008555914));
#9813=CARTESIAN_POINT('Ctrl Pts',(159.515234675477,5.88511015280691,334.368937665393));
#9814=CARTESIAN_POINT('Ctrl Pts',(159.507837226273,5.86620374860339,334.212324513865));
#9815=CARTESIAN_POINT('Ctrl Pts',(159.500439777069,5.84107250725722,334.056706552835));
#9816=CARTESIAN_POINT('Ctrl Pts',(159.493042648605,5.81594235555791,333.901095339129));
#9817=CARTESIAN_POINT('Ctrl Pts',(159.485645520142,5.78458796286248,333.746479598564));
#9818=CARTESIAN_POINT('Ctrl Pts',(159.478248391679,5.74711887878303,333.593388768836));
#9819=CARTESIAN_POINT('Ctrl Pts',(159.470850124242,5.70964402539995,333.440274366942));
#9820=CARTESIAN_POINT('Ctrl Pts',(159.463451856805,5.66605269469313,333.288685705932));
#9821=CARTESIAN_POINT('Ctrl Pts',(159.456053589369,5.61650488024397,333.139139045308));
#9822=CARTESIAN_POINT('Ctrl Pts',(159.448652722843,5.56693965912644,332.98953984737));
#9823=CARTESIAN_POINT('Ctrl Pts',(159.441251856317,5.51141390525624,332.841984432162));
#9824=CARTESIAN_POINT('Ctrl Pts',(159.433850989791,5.45013645031971,332.69697085659));
#9825=CARTESIAN_POINT('Ctrl Pts',(159.426441996407,5.3887917068794,332.551798042248));
#9826=CARTESIAN_POINT('Ctrl Pts',(159.419033003022,5.32168279450289,332.409172985668));
#9827=CARTESIAN_POINT('Ctrl Pts',(159.411624009637,5.24906569789374,332.269571487533));
#9828=CARTESIAN_POINT('Ctrl Pts',(159.404210452057,5.17640386664838,332.129883990059));
#9829=CARTESIAN_POINT('Ctrl Pts',(159.396796894477,5.09822727459202,331.993224085735));
#9830=CARTESIAN_POINT('Ctrl Pts',(159.389383336897,5.01483599329072,331.860039725905));
#9831=CARTESIAN_POINT('Ctrl Pts',(159.38195922476,4.93132598923354,331.726665753756));
#9832=CARTESIAN_POINT('Ctrl Pts',(159.374535112623,4.84258667855479,331.596777515723));
#9833=CARTESIAN_POINT('Ctrl Pts',(159.367111000487,4.74895974187416,331.470791599727));
#9834=CARTESIAN_POINT('Ctrl Pts',(159.363253875332,4.70031677878593,331.40533684409));
#9835=CARTESIAN_POINT('Ctrl Pts',(159.359396750177,4.65035517742486,331.340934838121));
#9836=CARTESIAN_POINT('Ctrl Pts',(159.355539625023,4.59912679306621,331.277640089432));
#9837=CARTESIAN_POINT('Ctrl Pts',(159.348115647585,4.50052528173033,331.155813919068));
#9838=CARTESIAN_POINT('Ctrl Pts',(159.340691670147,4.3969311061483,331.037724453438));
#9839=CARTESIAN_POINT('Ctrl Pts',(159.333267692709,4.28865795703438,330.923807721652));
#9840=CARTESIAN_POINT('Ctrl Pts',(159.325852476681,4.18051258652741,330.810025428749));
#9841=CARTESIAN_POINT('Ctrl Pts',(159.318437260653,4.06769948851795,330.700406335373));
#9842=CARTESIAN_POINT('Ctrl Pts',(159.311022044626,3.95057369125965,330.59535494365));
#9843=CARTESIAN_POINT('Ctrl Pts',(159.303613963482,3.83356059185371,330.490404631847));
#9844=CARTESIAN_POINT('Ctrl Pts',(159.296205882338,3.71224333036871,330.390013519557));
#9845=CARTESIAN_POINT('Ctrl Pts',(159.288797801194,3.58701492526119,330.294550554043));
#9846=CARTESIAN_POINT('Ctrl Pts',(159.28139523402,3.46187972994267,330.199158643358));
#9847=CARTESIAN_POINT('Ctrl Pts',(159.273992666846,3.33283948303129,330.108687800997));
#9848=CARTESIAN_POINT('Ctrl Pts',(159.266590099672,3.2003214498467,330.02346775554));
#9849=CARTESIAN_POINT('Ctrl Pts',(159.259191429917,3.06787318682628,329.938292578063));
#9850=CARTESIAN_POINT('Ctrl Pts',(159.251792760162,2.93195109727048,329.858362893141));
#9851=CARTESIAN_POINT('Ctrl Pts',(159.244394090408,2.79301259383497,329.783965949768));
#9852=CARTESIAN_POINT('Ctrl Pts',(159.236996641204,2.65409701093913,329.709581279582));
#9853=CARTESIAN_POINT('Ctrl Pts',(159.229599192,2.51216633046017,329.640727715474));
#9854=CARTESIAN_POINT('Ctrl Pts',(159.222201742796,2.36770391034426,329.577647304404));
#9855=CARTESIAN_POINT('Ctrl Pts',(159.214804614332,2.22324775386717,329.51456962839));
#9856=CARTESIAN_POINT('Ctrl Pts',(159.207407485869,2.07626041804183,329.457264757055));
#9857=CARTESIAN_POINT('Ctrl Pts',(159.200010357405,1.92724640190293,329.40592707691));
#9858=CARTESIAN_POINT('Ctrl Pts',(159.192612089969,1.77820944132487,329.354581492043));
#9859=CARTESIAN_POINT('Ctrl Pts',(159.185213822532,1.62714553196356,329.309205049386));
#9860=CARTESIAN_POINT('Ctrl Pts',(159.177815555096,1.47457538915518,329.269942584564));
#9861=CARTESIAN_POINT('Ctrl Pts',(159.17041468857,1.32195164685127,329.230666326424));
#9862=CARTESIAN_POINT('Ctrl Pts',(159.163013822044,1.16782097875985,329.197508415547));
#9863=CARTESIAN_POINT('Ctrl Pts',(159.155612955518,1.0127152223666,329.170562768081));
#9864=CARTESIAN_POINT('Ctrl Pts',(159.148203962134,0.85743914502415,329.143587531718));
#9865=CARTESIAN_POINT('Ctrl Pts',(159.140794968749,0.701186208977727,329.122838245901));
#9866=CARTESIAN_POINT('Ctrl Pts',(159.133385975364,0.544495053184813,329.108357130684));
#9867=CARTESIAN_POINT('Ctrl Pts',(159.125972417784,0.387707370235105,329.093867094601));
#9868=CARTESIAN_POINT('Ctrl Pts',(159.118558860204,0.230481301443147,329.085652942912));
#9869=CARTESIAN_POINT('Ctrl Pts',(159.111145302623,0.0733559245951565,329.083704751212));
#9870=CARTESIAN_POINT('Ctrl Pts',(159.103721190487,-0.083993148992508,329.081753785905));
#9871=CARTESIAN_POINT('Ctrl Pts',(159.09629707835,-0.24124087226726,329.08608658684));
#9872=CARTESIAN_POINT('Ctrl Pts',(159.088872966213,-0.397852024571218,329.096641267122));
#9873=CARTESIAN_POINT('Ctrl Pts',(159.085015841059,-0.479217823460725,329.102124848467));
#9874=CARTESIAN_POINT('Ctrl Pts',(159.081158715904,-0.560411933527618,329.10928700412));
#9875=CARTESIAN_POINT('Ctrl Pts',(159.077301590749,-0.641360456293825,329.118113625069));
#9876=CARTESIAN_POINT('Ctrl Pts',(159.069877613312,-0.797165617537513,329.135102608354));
#9877=CARTESIAN_POINT('Ctrl Pts',(159.062453635874,-0.952530321154162,329.158312174861));
#9878=CARTESIAN_POINT('Ctrl Pts',(159.055029658436,-1.10691814491711,329.187714495747));
#9879=CARTESIAN_POINT('Ctrl Pts',(159.047614442408,-1.26112376781904,329.21708211747));
#9880=CARTESIAN_POINT('Ctrl Pts',(159.04019922638,-1.41435444260713,329.25262787698));
#9881=CARTESIAN_POINT('Ctrl Pts',(159.032784010353,-1.56607788865388,329.294272122755));
#9882=CARTESIAN_POINT('Ctrl Pts',(159.025375929209,-1.71765534716503,329.335876298646));
#9883=CARTESIAN_POINT('Ctrl Pts',(159.017967848064,-1.86772810661278,329.383567180719));
#9884=CARTESIAN_POINT('Ctrl Pts',(159.01055976692,-2.01577322653504,329.437213929901));
#9885=CARTESIAN_POINT('Ctrl Pts',(159.003157199746,-2.16370815376932,329.490820748828));
#9886=CARTESIAN_POINT('Ctrl Pts',(158.995754632573,-2.30961809715199,329.550374481391));
#9887=CARTESIAN_POINT('Ctrl Pts',(158.988352065399,-2.45299456310526,329.615694266122));
#9888=CARTESIAN_POINT('Ctrl Pts',(158.980953395644,-2.59629554197724,329.680979660272));
#9889=CARTESIAN_POINT('Ctrl Pts',(158.973554725889,-2.73706536111975,329.752024906273));
#9890=CARTESIAN_POINT('Ctrl Pts',(158.966156056134,-2.87481493448873,329.82860080298));
#9891=CARTESIAN_POINT('Ctrl Pts',(158.95875860693,-3.01254178345519,329.905164067041));
#9892=CARTESIAN_POINT('Ctrl Pts',(158.951361157726,-3.14724904962742,329.987255989859));
#9893=CARTESIAN_POINT('Ctrl Pts',(158.943963708522,-3.27847161783451,330.074601090921));
#9894=CARTESIAN_POINT('Ctrl Pts',(158.936566580059,-3.40968849645989,330.161942404852));
#9895=CARTESIAN_POINT('Ctrl Pts',(158.929169451595,-3.53742066685793,330.254536237353));
#9896=CARTESIAN_POINT('Ctrl Pts',(158.921772323132,-3.66123165188905,330.352063538117));
#9897=CARTESIAN_POINT('Ctrl Pts',(158.914374055695,-3.78506170072144,330.44960585565));
#9898=CARTESIAN_POINT('Ctrl Pts',(158.906975788259,-3.90496906881592,330.552082923018));
#9899=CARTESIAN_POINT('Ctrl Pts',(158.899577520822,-4.02055017185975,330.659135238451));
#9900=CARTESIAN_POINT('Ctrl Pts',(158.892176654296,-4.13617187976178,330.76622516249));
#9901=CARTESIAN_POINT('Ctrl Pts',(158.88477578777,-4.24746402293306,330.877893281346));
#9902=CARTESIAN_POINT('Ctrl Pts',(158.877374921244,-4.35405981749925,330.993743184949));
#9903=CARTESIAN_POINT('Ctrl Pts',(158.86996592786,-4.46077266443758,331.109720302822));
#9904=CARTESIAN_POINT('Ctrl Pts',(158.862556934475,-4.56277861103342,331.229888101104));
#9905=CARTESIAN_POINT('Ctrl Pts',(158.85514794109,-4.65975066509635,331.353816474499));
#9906=CARTESIAN_POINT('Ctrl Pts',(158.84773438351,-4.75678245728948,331.477821192047));
#9907=CARTESIAN_POINT('Ctrl Pts',(158.84032082593,-4.84877396013921,331.605590798758));
#9908=CARTESIAN_POINT('Ctrl Pts',(158.832907268349,-4.93544179336682,331.736666601956));
#9909=CARTESIAN_POINT('Ctrl Pts',(158.825483156213,-5.0222330141217,331.867929015557));
#9910=CARTESIAN_POINT('Ctrl Pts',(158.818059044076,-5.10368523531542,332.002506707993));
#9911=CARTESIAN_POINT('Ctrl Pts',(158.810634931939,-5.1795608603498,332.139916110246));
#9912=CARTESIAN_POINT('Ctrl Pts',(158.806777806785,-5.21898130235845,332.21130582691));
#9913=CARTESIAN_POINT('Ctrl Pts',(158.80292068163,-5.25689728474739,332.283459539655));
#9914=CARTESIAN_POINT('Ctrl Pts',(158.799063556475,-5.29328068137832,332.356307470479));
#9915=CARTESIAN_POINT('Ctrl Pts',(158.791118272457,-5.36822676381,332.506366770435));
#9916=CARTESIAN_POINT('Ctrl Pts',(158.783172988438,-5.43686838976672,332.65977603528));
#9917=CARTESIAN_POINT('Ctrl Pts',(158.775227704419,-5.49891546224878,332.815999244153));
#9918=CARTESIAN_POINT('Ctrl Pts',(158.767297571479,-5.56084421548026,332.971924546738));
#9919=CARTESIAN_POINT('Ctrl Pts',(158.759367438539,-5.61620338153345,333.13065282336));
#9920=CARTESIAN_POINT('Ctrl Pts',(158.751437305598,-5.66474934606599,333.291624921528));
#9921=CARTESIAN_POINT('Ctrl Pts',(158.743528739818,-5.71316328272739,333.452159232464));
#9922=CARTESIAN_POINT('Ctrl Pts',(158.735620174037,-5.75480089439849,333.614924913133));
#9923=CARTESIAN_POINT('Ctrl Pts',(158.727711608256,-5.78946735267797,333.779345120529));
#9924=CARTESIAN_POINT('Ctrl Pts',(158.719816288477,-5.82407574835078,333.943489941679));
#9925=CARTESIAN_POINT('Ctrl Pts',(158.711920968697,-5.85173620522388,334.109283480948));
#9926=CARTESIAN_POINT('Ctrl Pts',(158.704025648917,-5.87230346456176,334.27613358788));
#9927=CARTESIAN_POINT('Ctrl Pts',(158.696148894247,-5.89282236190352,334.442591362314));
#9928=CARTESIAN_POINT('Ctrl Pts',(158.688272139577,-5.90628129190153,334.610100459849));
#9929=CARTESIAN_POINT('Ctrl Pts',(158.680395384907,-5.91258595816309,334.778058904588));
#9930=CARTESIAN_POINT('Ctrl Pts',(158.676947609815,-5.91534560629397,334.851576865549));
#9931=CARTESIAN_POINT('Ctrl Pts',(158.673499834723,-5.91673518973076,334.925180763386));
#9932=CARTESIAN_POINT('Ctrl Pts',(158.67005205963,-5.91674988223068,334.998819481802));
#9933=CARTESIAN_POINT('',(156.920052004703,-5.91590632165756,335.005448065324));
#9934=CARTESIAN_POINT('Ctrl Pts',(158.670052004703,-5.90718086102098,334.998822562282));
#9935=CARTESIAN_POINT('Ctrl Pts',(158.620309843869,-5.90529945334112,336.059514263974));
#9936=CARTESIAN_POINT('Ctrl Pts',(158.477821671611,-5.12528683190018,339.100484283673));
#9937=CARTESIAN_POINT('Ctrl Pts',(158.242587487927,-0.252042696482904,341.992073898377));
#9938=CARTESIAN_POINT('Ctrl Pts',(157.964349453653,5.74338934522624,338.995760472095));
#9939=CARTESIAN_POINT('Ctrl Pts',(157.686111419379,6.46819775710926,332.3325966379));
#9940=CARTESIAN_POINT('Ctrl Pts',(157.407873385105,1.25723655773474,328.117269498293));
#9941=CARTESIAN_POINT('Ctrl Pts',(157.15252024688,-4.5839789583817,330.045328763812));
#9942=CARTESIAN_POINT('Ctrl Pts',(156.989913120079,-5.90237610370384,333.521276051786));
#9943=CARTESIAN_POINT('Ctrl Pts',(156.920052004703,-5.91590632165756,335.005448065324));
#9944=CARTESIAN_POINT('',(155.170051131044,-5.92181705319278,334.998466635511));
#9945=CARTESIAN_POINT('Ctrl Pts',(156.920051980179,-5.91674749055292,335.005449361037));
#9946=CARTESIAN_POINT('Ctrl Pts',(156.910500549411,-5.91656057844607,335.208392739462));
#9947=CARTESIAN_POINT('Ctrl Pts',(156.900949118643,-5.90592887574173,335.410870699688));
#9948=CARTESIAN_POINT('Ctrl Pts',(156.891397687875,-5.88501638256968,335.61197445975));
#9949=CARTESIAN_POINT('Ctrl Pts',(156.88162723986,-5.86362435949407,335.817689590914));
#9950=CARTESIAN_POINT('Ctrl Pts',(156.871856791845,-5.83147464020149,336.021967055827));
#9951=CARTESIAN_POINT('Ctrl Pts',(156.86208634383,-5.78879070814869,336.223859754936));
#9952=CARTESIAN_POINT('Ctrl Pts',(156.858523334739,-5.77322507208986,336.29748437493));
#9953=CARTESIAN_POINT('Ctrl Pts',(156.854960325648,-5.75625899132762,336.370792075941));
#9954=CARTESIAN_POINT('Ctrl Pts',(156.851397316557,-5.73790486259783,336.443737632077));
#9955=CARTESIAN_POINT('Ctrl Pts',(156.843973339119,-5.69966172762065,336.595728870147));
#9956=CARTESIAN_POINT('Ctrl Pts',(156.836549361681,-5.65531759153176,336.746428812752));
#9957=CARTESIAN_POINT('Ctrl Pts',(156.829125384243,-5.60497375020673,336.895309954069));
#9958=CARTESIAN_POINT('Ctrl Pts',(156.821710168216,-5.55468932218909,337.044015393239));
#9959=CARTESIAN_POINT('Ctrl Pts',(156.814294952188,-5.49841940128052,337.190905953574));
#9960=CARTESIAN_POINT('Ctrl Pts',(156.80687973616,-5.43631604491004,337.335465354561));
#9961=CARTESIAN_POINT('Ctrl Pts',(156.799471655016,-5.37427244407629,337.479885661219));
#9962=CARTESIAN_POINT('Ctrl Pts',(156.792063573872,-5.30640672835238,337.621978933368));
#9963=CARTESIAN_POINT('Ctrl Pts',(156.784655492728,-5.23292037307704,337.76124517773));
#9964=CARTESIAN_POINT('Ctrl Pts',(156.777252925554,-5.15948871503811,337.900407763682));
#9965=CARTESIAN_POINT('Ctrl Pts',(156.76985035838,-5.0804449209197,338.036747182969));
#9966=CARTESIAN_POINT('Ctrl Pts',(156.762447791207,-4.99603802795934,338.16978462765));
#9967=CARTESIAN_POINT('Ctrl Pts',(156.755049121452,-4.91167557485941,338.302752028697));
#9968=CARTESIAN_POINT('Ctrl Pts',(156.747650451697,-4.82195584581747,338.432420603074));
#9969=CARTESIAN_POINT('Ctrl Pts',(156.740251781943,-4.72717309138047,338.558337410453));
#9970=CARTESIAN_POINT('Ctrl Pts',(156.732854332739,-4.63240597315461,338.684233445469));
#9971=CARTESIAN_POINT('Ctrl Pts',(156.725456883535,-4.53257771145043,338.806378643967));
#9972=CARTESIAN_POINT('Ctrl Pts',(156.718059434331,-4.42802510213637,338.924350170073));
#9973=CARTESIAN_POINT('Ctrl Pts',(156.710662305868,-4.32347702604129,339.042316581139));
#9974=CARTESIAN_POINT('Ctrl Pts',(156.703265177404,-4.21420525716126,339.156109400319));
#9975=CARTESIAN_POINT('Ctrl Pts',(156.695868048941,-4.10058581133365,339.265340146622));
#9976=CARTESIAN_POINT('Ctrl Pts',(156.688469781504,-3.98694887094747,339.374587711734));
#9977=CARTESIAN_POINT('Ctrl Pts',(156.681071514068,-3.86896318974458,339.479271546638));
#9978=CARTESIAN_POINT('Ctrl Pts',(156.673673246631,-3.74704032997384,339.579041311022));
#9979=CARTESIAN_POINT('Ctrl Pts',(156.666272380106,-3.62507463742024,339.678846125574));
#9980=CARTESIAN_POINT('Ctrl Pts',(156.65887151358,-3.49916930105579,339.773733196214));
#9981=CARTESIAN_POINT('Ctrl Pts',(156.651470647054,-3.36976738290881,339.863393706825));
#9982=CARTESIAN_POINT('Ctrl Pts',(156.64406165367,-3.24022336908449,339.953152673249));
#9983=CARTESIAN_POINT('Ctrl Pts',(156.636652660285,-3.10717541258079,340.037673405348));
#9984=CARTESIAN_POINT('Ctrl Pts',(156.6292436669,-2.97109448148061,340.116691132423));
#9985=CARTESIAN_POINT('Ctrl Pts',(156.62183010932,-2.83492971983294,340.195757537143));
#9986=CARTESIAN_POINT('Ctrl Pts',(156.61441655174,-2.69572858972507,340.269314007776));
#9987=CARTESIAN_POINT('Ctrl Pts',(156.60700299416,-2.55398438083638,340.33714290093));
#9988=CARTESIAN_POINT('Ctrl Pts',(156.599578882023,-2.41203837311668,340.405068360931));
#9989=CARTESIAN_POINT('Ctrl Pts',(156.592154769887,-2.26754239756873,340.467249810648));
#9990=CARTESIAN_POINT('Ctrl Pts',(156.58473065775,-2.12100809114677,340.523518375075));
#9991=CARTESIAN_POINT('Ctrl Pts',(156.580873532595,-2.04487761937375,340.552752159712));
#9992=CARTESIAN_POINT('Ctrl Pts',(156.577016407439,-1.96819719059255,340.580390752808));
#9993=CARTESIAN_POINT('Ctrl Pts',(156.573159282284,-1.89103978645724,340.606415886155));
#9994=CARTESIAN_POINT('Ctrl Pts',(156.565735304846,-1.74253155704533,340.656507598247));
#9995=CARTESIAN_POINT('Ctrl Pts',(156.558311327408,-1.59180760376044,340.700770054274));
#9996=CARTESIAN_POINT('Ctrl Pts',(156.55088734997,-1.43936633451521,340.73900297243));
#9997=CARTESIAN_POINT('Ctrl Pts',(156.543472133942,-1.28710496890372,340.777190769991));
#9998=CARTESIAN_POINT('Ctrl Pts',(156.536056917914,-1.13313067997221,340.809363103809));
#9999=CARTESIAN_POINT('Ctrl Pts',(156.528641701887,-0.977959906019541,340.83536845321));
#10000=CARTESIAN_POINT('Ctrl Pts',(156.521233620743,-0.822938436604197,
340.861348780395));
#10001=CARTESIAN_POINT('Ctrl Pts',(156.513825539599,-0.666723139713503,
340.881173875061));
#10002=CARTESIAN_POINT('Ctrl Pts',(156.506417458454,-0.509843500227656,
340.894742587067));
#10003=CARTESIAN_POINT('Ctrl Pts',(156.49901489128,-0.35308062912281,340.908301199632));
#10004=CARTESIAN_POINT('Ctrl Pts',(156.491612324106,-0.195654770239612,
340.915612669762));
#10005=CARTESIAN_POINT('Ctrl Pts',(156.484209756932,-0.0381033317290172,
340.916627307733));
#10006=CARTESIAN_POINT('Ctrl Pts',(156.476811087178,0.119365156638028,340.917641411501));
#10007=CARTESIAN_POINT('Ctrl Pts',(156.469412417423,0.276958720692679,340.912365283239));
#10008=CARTESIAN_POINT('Ctrl Pts',(156.462013747668,0.434137237396164,340.900801252509));
#10009=CARTESIAN_POINT('Ctrl Pts',(156.454616298464,0.59128982452499,340.889239129484));
#10010=CARTESIAN_POINT('Ctrl Pts',(156.44721884926,0.748027128349952,340.871391190071));
#10011=CARTESIAN_POINT('Ctrl Pts',(156.439821400056,0.903811317593196,340.847311832346));
#10012=CARTESIAN_POINT('Ctrl Pts',(156.432424271593,1.05958875230547,340.82323351866));
#10013=CARTESIAN_POINT('Ctrl Pts',(156.425027143129,1.21441278577318,340.792924380886));
#10014=CARTESIAN_POINT('Ctrl Pts',(156.417630014666,1.36775325229648,340.756490389407));
#10015=CARTESIAN_POINT('Ctrl Pts',(156.410231747229,1.52111732942384,340.720050788003));
#10016=CARTESIAN_POINT('Ctrl Pts',(156.402833479792,1.67299702164339,340.677484541387));
#10017=CARTESIAN_POINT('Ctrl Pts',(156.395435212356,1.822875000364,340.628948151791));
#10018=CARTESIAN_POINT('Ctrl Pts',(156.38803434583,1.97280563279464,340.58039471085));
#10019=CARTESIAN_POINT('Ctrl Pts',(156.380633479304,2.12073279677664,340.525867065969));
#10020=CARTESIAN_POINT('Ctrl Pts',(156.373232612778,2.26615703596342,340.465570679339));
#10021=CARTESIAN_POINT('Ctrl Pts',(156.365823619394,2.41174096486809,340.405208081513));
#10022=CARTESIAN_POINT('Ctrl Pts',(156.358414626009,2.55481613521681,340.339064234371));
#10023=CARTESIAN_POINT('Ctrl Pts',(156.351005632624,2.69490502782445,340.267391902404));
#10024=CARTESIAN_POINT('Ctrl Pts',(156.343592075044,2.83508022002213,340.195675417808));
#10025=CARTESIAN_POINT('Ctrl Pts',(156.336178517463,2.97226514429686,340.1184238447));
#10026=CARTESIAN_POINT('Ctrl Pts',(156.328764959883,3.10600983232754,340.03593422157));
#10027=CARTESIAN_POINT('Ctrl Pts',(156.321340847746,3.23994493040673,339.95332715936));
#10028=CARTESIAN_POINT('Ctrl Pts',(156.31391673561,3.37042970160363,339.865467361246));
#10029=CARTESIAN_POINT('Ctrl Pts',(156.306492623473,3.49704525920953,339.772693685702));
#10030=CARTESIAN_POINT('Ctrl Pts',(156.302635498318,3.56282713901046,339.724494026128));
#10031=CARTESIAN_POINT('Ctrl Pts',(156.298778373164,3.62756520150735,339.6749686463));
#10032=CARTESIAN_POINT('Ctrl Pts',(156.294921248009,3.69120459001352,339.624169032071));
#10033=CARTESIAN_POINT('Ctrl Pts',(156.287497270571,3.81369410370632,339.526392793349));
#10034=CARTESIAN_POINT('Ctrl Pts',(156.280073293133,3.932480726939,339.423598760212));
#10035=CARTESIAN_POINT('Ctrl Pts',(156.272649315695,4.04712632134682,339.316097670531));
#10036=CARTESIAN_POINT('Ctrl Pts',(156.265234099668,4.16163661670388,339.208723448309));
#10037=CARTESIAN_POINT('Ctrl Pts',(156.25781888364,4.27201534136185,339.096653479727));
#10038=CARTESIAN_POINT('Ctrl Pts',(156.250403667612,4.37785560395626,338.980240052234));
#10039=CARTESIAN_POINT('Ctrl Pts',(156.242995586468,4.48359402758291,338.863938637156));
#10040=CARTESIAN_POINT('Ctrl Pts',(156.235587505324,4.58480243341674,338.74330235758));
#10041=CARTESIAN_POINT('Ctrl Pts',(156.22817942418,4.68110922749544,338.618721730495));
#10042=CARTESIAN_POINT('Ctrl Pts',(156.220776857006,4.77734433866842,338.494233831046));
#10043=CARTESIAN_POINT('Ctrl Pts',(156.213374289832,4.86868487522002,338.365807723797));
#10044=CARTESIAN_POINT('Ctrl Pts',(156.205971722658,4.95479822961385,338.233868436767));
#10045=CARTESIAN_POINT('Ctrl Pts',(156.198573052903,5.04086624570299,338.101998615194));
#10046=CARTESIAN_POINT('Ctrl Pts',(156.191174383148,5.1217123571128,337.966619609323));
#10047=CARTESIAN_POINT('Ctrl Pts',(156.183775713394,5.19704623125318,337.828186880798));
#10048=CARTESIAN_POINT('Ctrl Pts',(156.17637826419,5.27236767764358,337.689776989375));
#10049=CARTESIAN_POINT('Ctrl Pts',(156.168980814986,5.34217851330621,337.548314702613));
#10050=CARTESIAN_POINT('Ctrl Pts',(156.161583365782,5.40623343137915,337.404281732231));
#10051=CARTESIAN_POINT('Ctrl Pts',(156.154186237318,5.47028557214251,337.260255006866));
#10052=CARTESIAN_POINT('Ctrl Pts',(156.146789108855,5.52858213988165,337.11365816051));
#10053=CARTESIAN_POINT('Ctrl Pts',(156.139391980391,5.5809253442718,336.964994367464));
#10054=CARTESIAN_POINT('Ctrl Pts',(156.131993712955,5.63327660820878,336.816307683905));
#10055=CARTESIAN_POINT('Ctrl Pts',(156.124595445518,5.67967255963381,336.665553772012));
#10056=CARTESIAN_POINT('Ctrl Pts',(156.117197178081,5.71996484842579,336.513252356771));
#10057=CARTESIAN_POINT('Ctrl Pts',(156.109796311556,5.76027129232258,336.360897436441));
#10058=CARTESIAN_POINT('Ctrl Pts',(156.10239544503,5.79446970893535,336.20699429092));
#10059=CARTESIAN_POINT('Ctrl Pts',(156.094994578504,5.82246259131658,336.052074111087));
#10060=CARTESIAN_POINT('Ctrl Pts',(156.087585585119,5.85048621255889,335.896983814085));
#10061=CARTESIAN_POINT('Ctrl Pts',(156.080176591735,5.87229062470748,335.740874619942));
#10062=CARTESIAN_POINT('Ctrl Pts',(156.07276759835,5.88782996978299,335.584284870098));
#10063=CARTESIAN_POINT('Ctrl Pts',(156.06535404077,5.90337888763107,335.427598655566));
#10064=CARTESIAN_POINT('Ctrl Pts',(156.057940483189,5.91265502590962,335.270431667129));
#10065=CARTESIAN_POINT('Ctrl Pts',(156.050526925609,5.91566466694261,335.113323037317));
#10066=CARTESIAN_POINT('Ctrl Pts',(156.043102813472,5.9186785927506,334.955990734608));
#10067=CARTESIAN_POINT('Ctrl Pts',(156.035678701336,5.91540821101888,334.798717328585));
#10068=CARTESIAN_POINT('Ctrl Pts',(156.028254589199,5.90591179143411,334.64203844578));
#10069=CARTESIAN_POINT('Ctrl Pts',(156.024397464045,5.90097801912786,334.560637458171));
#10070=CARTESIAN_POINT('Ctrl Pts',(156.02054033889,5.89436455093886,334.479396815501));
#10071=CARTESIAN_POINT('Ctrl Pts',(156.016683213735,5.88608499631948,334.39839050988));
#10072=CARTESIAN_POINT('Ctrl Pts',(156.009259236297,5.87014897551951,334.242474131445));
#10073=CARTESIAN_POINT('Ctrl Pts',(156.001835258859,5.84798953784702,334.086956176117));
#10074=CARTESIAN_POINT('Ctrl Pts',(155.994411281421,5.81963088759558,333.932373241885));
#10075=CARTESIAN_POINT('Ctrl Pts',(155.986996065394,5.79130570481823,333.777972738774));
#10076=CARTESIAN_POINT('Ctrl Pts',(155.979580849366,5.75679593877136,333.624505423809));
#10077=CARTESIAN_POINT('Ctrl Pts',(155.972165633339,5.71617764322439,333.472504103573));
#10078=CARTESIAN_POINT('Ctrl Pts',(155.964757552194,5.67559843039689,333.320649038242));
#10079=CARTESIAN_POINT('Ctrl Pts',(155.95734947105,5.62892248497393,333.170257517604));
#10080=CARTESIAN_POINT('Ctrl Pts',(155.949941389906,5.5762771102056,333.021853354097));
#10081=CARTESIAN_POINT('Ctrl Pts',(155.942538822732,5.52367092035119,332.87355965052));
#10082=CARTESIAN_POINT('Ctrl Pts',(155.935136255558,5.46510427236193,332.727250708948));
#10083=CARTESIAN_POINT('Ctrl Pts',(155.927733688384,5.40075458834285,332.583436233203));
#10084=CARTESIAN_POINT('Ctrl Pts',(155.92033501863,5.33643878415119,332.439697475152));
#10085=CARTESIAN_POINT('Ctrl Pts',(155.912936348875,5.26634615976231,332.298450907169));
#10086=CARTESIAN_POINT('Ctrl Pts',(155.90553767912,5.19070260696743,332.160187152554));
#10087=CARTESIAN_POINT('Ctrl Pts',(155.898140229916,5.11507153300986,332.021946207164));
#10088=CARTESIAN_POINT('Ctrl Pts',(155.890742780712,5.03389152702902,331.886687425636));
#10089=CARTESIAN_POINT('Ctrl Pts',(155.883345331508,4.94743492106539,331.754877773593));
#10090=CARTESIAN_POINT('Ctrl Pts',(155.875948203045,4.86098206370951,331.623073836586));
#10091=CARTESIAN_POINT('Ctrl Pts',(155.868551074581,4.769253265962,331.494719043783));
#10092=CARTESIAN_POINT('Ctrl Pts',(155.861153946118,4.67256462213479,331.370252017774));
#10093=CARTESIAN_POINT('Ctrl Pts',(155.853755678681,4.57586109067005,331.24576582695));
#10094=CARTESIAN_POINT('Ctrl Pts',(155.846357411244,4.47419642148117,331.1251688896));
#10095=CARTESIAN_POINT('Ctrl Pts',(155.838959143808,4.36792738163358,331.008867209516));
#10096=CARTESIAN_POINT('Ctrl Pts',(155.831558277282,4.2616210083546,330.892524671429));
#10097=CARTESIAN_POINT('Ctrl Pts',(155.824157410756,4.15070729544045,330.780480670306));
#10098=CARTESIAN_POINT('Ctrl Pts',(155.816756544231,4.03558016602919,330.673104659684));
#10099=CARTESIAN_POINT('Ctrl Pts',(155.809347550846,3.9203266160233,330.565610739936));
#10100=CARTESIAN_POINT('Ctrl Pts',(155.801938557461,3.80085068277585,330.462795302089));
#10101=CARTESIAN_POINT('Ctrl Pts',(155.794529564076,3.67758025270406,330.364988236539));
#10102=CARTESIAN_POINT('Ctrl Pts',(155.787116006496,3.55423388379526,330.267120918463));
#10103=CARTESIAN_POINT('Ctrl Pts',(155.779702448916,3.42708866089523,330.174268340203));
#10104=CARTESIAN_POINT('Ctrl Pts',(155.772288891336,3.29660135177702,330.086716974368));
#10105=CARTESIAN_POINT('Ctrl Pts',(155.764864779199,3.16592827008551,329.999040963135));
#10106=CARTESIAN_POINT('Ctrl Pts',(155.757440667062,3.03190391646984,329.916681432558));
#10107=CARTESIAN_POINT('Ctrl Pts',(155.750016554925,2.89501024378064,329.839879240666));
#10108=CARTESIAN_POINT('Ctrl Pts',(155.746159429771,2.82388846938806,329.799977409871));
#10109=CARTESIAN_POINT('Ctrl Pts',(155.742302304616,2.75199255265327,329.761574843026));
#10110=CARTESIAN_POINT('Ctrl Pts',(155.738445179461,2.6793920799741,329.724700137028));
#10111=CARTESIAN_POINT('Ctrl Pts',(155.731021202023,2.53965477575423,329.653725778048));
#10112=CARTESIAN_POINT('Ctrl Pts',(155.723597224585,2.39688466605584,329.588200432691));
#10113=CARTESIAN_POINT('Ctrl Pts',(155.716173247147,2.25154608590787,329.528394131013));
#10114=CARTESIAN_POINT('Ctrl Pts',(155.70875803112,2.10637902715177,329.468658409769));
#10115=CARTESIAN_POINT('Ctrl Pts',(155.701342815092,1.95864987333785,329.414628438191));
#10116=CARTESIAN_POINT('Ctrl Pts',(155.693927599064,1.80884782994775,329.366528593257));
#10117=CARTESIAN_POINT('Ctrl Pts',(155.68651951792,1.65918992532954,329.318475029751));
#10118=CARTESIAN_POINT('Ctrl Pts',(155.679111436776,1.50746345482844,329.276340346764));
#10119=CARTESIAN_POINT('Ctrl Pts',(155.671703355632,1.35417779459332,329.240300957244));
#10120=CARTESIAN_POINT('Ctrl Pts',(155.664300788458,1.20100622767464,329.204288392499));
#10121=CARTESIAN_POINT('Ctrl Pts',(155.656898221284,1.04627814356175,329.174362172768));
#10122=CARTESIAN_POINT('Ctrl Pts',(155.64949565411,0.890518176354073,329.150648930002));
#10123=CARTESIAN_POINT('Ctrl Pts',(155.642096984355,0.734840216088303,329.126948172155));
#10124=CARTESIAN_POINT('Ctrl Pts',(155.6346983146,0.578131822736678,329.109453932702));
#10125=CARTESIAN_POINT('Ctrl Pts',(155.627299644846,0.420927814909075,329.098241758837));
#10126=CARTESIAN_POINT('Ctrl Pts',(155.619902195642,0.263749740861374,329.087031434632));
#10127=CARTESIAN_POINT('Ctrl Pts',(155.612504746438,0.106076586510544,329.082101145729));
#10128=CARTESIAN_POINT('Ctrl Pts',(155.605107297234,-0.0515515922944678,
329.083474584198));
#10129=CARTESIAN_POINT('Ctrl Pts',(155.59771016877,-0.209172936616341,329.084847963117));
#10130=CARTESIAN_POINT('Ctrl Pts',(155.590313040307,-0.36674893607263,329.092524522709));
#10131=CARTESIAN_POINT('Ctrl Pts',(155.582915911843,-0.523739686799201,
329.106475816375));
#10132=CARTESIAN_POINT('Ctrl Pts',(155.575517644407,-0.680754610182395,
329.120429258192));
#10133=CARTESIAN_POINT('Ctrl Pts',(155.56811937697,-0.837183733638758,329.140659324783));
#10134=CARTESIAN_POINT('Ctrl Pts',(155.560721109533,-0.992492572786399,
329.167085715059));
#10135=CARTESIAN_POINT('Ctrl Pts',(155.553320243008,-1.14785597356264,329.193521389205));
#10136=CARTESIAN_POINT('Ctrl Pts',(155.545919376482,-1.30209793874623,329.226157658543));
#10137=CARTESIAN_POINT('Ctrl Pts',(155.538518509956,-1.45469461256303,329.264863197213));
#10138=CARTESIAN_POINT('Ctrl Pts',(155.531109516571,-1.60745885211655,329.303611238265));
#10139=CARTESIAN_POINT('Ctrl Pts',(155.523700523187,-1.75857383028098,329.348441766472));
#10140=CARTESIAN_POINT('Ctrl Pts',(155.516291529802,-1.90753058129199,329.399173485642));
#10141=CARTESIAN_POINT('Ctrl Pts',(155.508877972222,-2.05657909479966,329.4499364573));
#10142=CARTESIAN_POINT('Ctrl Pts',(155.501464414641,-2.20346638448349,329.506607729786));
#10143=CARTESIAN_POINT('Ctrl Pts',(155.494050857061,-2.3477043661648,329.568958224098));
#10144=CARTESIAN_POINT('Ctrl Pts',(155.486626744924,-2.49214769701924,329.631397485754));
#10145=CARTESIAN_POINT('Ctrl Pts',(155.479202632788,-2.63393385140219,329.69953195621));
#10146=CARTESIAN_POINT('Ctrl Pts',(155.471778520651,-2.77259947431645,329.773086693131));
#10147=CARTESIAN_POINT('Ctrl Pts',(155.467921395497,-2.84464184818796,329.811301340323));
#10148=CARTESIAN_POINT('Ctrl Pts',(155.464064270342,-2.91584239185996,329.850978318078));
#10149=CARTESIAN_POINT('Ctrl Pts',(155.460207145187,-2.98613940039932,329.892074585129));
#10150=CARTESIAN_POINT('Ctrl Pts',(155.452783167749,-3.12144312647544,329.97117436726));
#10151=CARTESIAN_POINT('Ctrl Pts',(155.445359190311,-3.25380588581258,330.055773274156));
#10152=CARTESIAN_POINT('Ctrl Pts',(155.437935212873,-3.38274932604893,330.145626965342));
#10153=CARTESIAN_POINT('Ctrl Pts',(155.430519996846,-3.51154059362524,330.235374615653));
#10154=CARTESIAN_POINT('Ctrl Pts',(155.423104780818,-3.63692027122958,330.330364494898));
#10155=CARTESIAN_POINT('Ctrl Pts',(155.415689564791,-3.75843493831792,330.430306643009));
#10156=CARTESIAN_POINT('Ctrl Pts',(155.408281483646,-3.8798326846054,330.530152627287));
#10157=CARTESIAN_POINT('Ctrl Pts',(155.400873402502,-3.99737253768446,330.634941158621));
#10158=CARTESIAN_POINT('Ctrl Pts',(155.393465321358,-4.1106304954809,330.74433935891));
#10159=CARTESIAN_POINT('Ctrl Pts',(155.386062754184,-4.22380415331075,330.85365613212));
#10160=CARTESIAN_POINT('Ctrl Pts',(155.37866018701,-4.33270199453921,330.967575484366));
#10161=CARTESIAN_POINT('Ctrl Pts',(155.371257619836,-4.43693362204194,331.085724767458));
#10162=CARTESIAN_POINT('Ctrl Pts',(155.363858950082,-4.54111037204843,331.203811845468));
#10163=CARTESIAN_POINT('Ctrl Pts',(155.356460280327,-4.6406255547957,331.326124139877));
#10164=CARTESIAN_POINT('Ctrl Pts',(155.349061610572,-4.7351262199996,331.452252793226));
#10165=CARTESIAN_POINT('Ctrl Pts',(155.341664161368,-4.8296112955282,331.578360639264));
#10166=CARTESIAN_POINT('Ctrl Pts',(155.334266712164,-4.919083271753,331.708283296341));
#10167=CARTESIAN_POINT('Ctrl Pts',(155.32686926296,-5.00322997029795,331.841579441111));
#10168=CARTESIAN_POINT('Ctrl Pts',(155.319472134497,-5.08737302038871,331.974869806392));
#10169=CARTESIAN_POINT('Ctrl Pts',(155.312075006033,-5.16619105267054,332.111533052947));
#10170=CARTESIAN_POINT('Ctrl Pts',(155.30467787757,-5.23941581553427,332.251099770012));
#10171=CARTESIAN_POINT('Ctrl Pts',(155.297279610133,-5.3126518531836,332.390687976867));
#10172=CARTESIAN_POINT('Ctrl Pts',(155.289881342697,-5.38029273320159,332.533180213883));
#10173=CARTESIAN_POINT('Ctrl Pts',(155.28248307526,-5.4421167423182,332.678083566215));
#10174=CARTESIAN_POINT('Ctrl Pts',(155.275082208734,-5.50396247085949,332.823037824619));
#10175=CARTESIAN_POINT('Ctrl Pts',(155.267681342209,-5.55998711347135,332.970404541758));
#10176=CARTESIAN_POINT('Ctrl Pts',(155.260280475683,-5.61001761645535,333.119672128175));
#10177=CARTESIAN_POINT('Ctrl Pts',(155.252871482298,-5.66010305771464,333.269103624673));
#10178=CARTESIAN_POINT('Ctrl Pts',(155.245462488913,-5.70418109578791,333.420439804896));
#10179=CARTESIAN_POINT('Ctrl Pts',(155.238053495529,-5.74212875593335,333.573154558902));
#10180=CARTESIAN_POINT('Ctrl Pts',(155.230639937948,-5.7800997931464,333.725963390464));
#10181=CARTESIAN_POINT('Ctrl Pts',(155.223226380368,-5.81193285192409,333.8801521234));
#10182=CARTESIAN_POINT('Ctrl Pts',(155.215812822788,-5.83755643932879,334.035186349521));
#10183=CARTESIAN_POINT('Ctrl Pts',(155.208388710651,-5.86321650660119,334.190441295245));
#10184=CARTESIAN_POINT('Ctrl Pts',(155.200964598515,-5.88264940063449,334.346543768859));
#10185=CARTESIAN_POINT('Ctrl Pts',(155.193540486378,-5.89583557832674,334.502955338187));
#10186=CARTESIAN_POINT('Ctrl Pts',(155.189683361223,-5.90268632852227,334.584217445688));
#10187=CARTESIAN_POINT('Ctrl Pts',(155.185826236068,-5.90785181112512,334.665562991191));
#10188=CARTESIAN_POINT('Ctrl Pts',(155.181969110914,-5.91133482837328,334.746916793601));
#10189=CARTESIAN_POINT('Ctrl Pts',(155.177996742177,-5.91492191156897,334.830701293287));
#10190=CARTESIAN_POINT('Ctrl Pts',(155.17402437344,-5.91672781384456,334.914562595738));
#10191=CARTESIAN_POINT('Ctrl Pts',(155.170052004703,-5.91674979683974,334.998449484974));
#10192=CARTESIAN_POINT('',(153.420053188954,-5.91355359401508,334.995357850205));
#10193=CARTESIAN_POINT('Ctrl Pts',(155.170050408738,-5.92600646020268,334.998480814896));
#10194=CARTESIAN_POINT('Ctrl Pts',(155.081277298038,-5.91942332648537,336.876090608429));
#10195=CARTESIAN_POINT('Ctrl Pts',(154.899758175916,-3.93940018579113,340.727255971215));
#10196=CARTESIAN_POINT('Ctrl Pts',(154.625493042366,2.62364521063082,341.486070361163));
#10197=CARTESIAN_POINT('Ctrl Pts',(154.347255008092,6.87407990914849,336.303705612426));
#10198=CARTESIAN_POINT('Ctrl Pts',(154.069016973818,4.816272936292,329.924949465835));
#10199=CARTESIAN_POINT('Ctrl Pts',(153.790778939544,-1.66135662212457,328.203492286818));
#10200=CARTESIAN_POINT('Ctrl Pts',(153.574457964201,-5.51217327151609,331.714221820233));
#10201=CARTESIAN_POINT('Ctrl Pts',(153.450883000283,-5.91599721235804,334.339080779984));
#10202=CARTESIAN_POINT('Ctrl Pts',(153.420054047789,-5.91123682344908,334.995341376946));
#10203=CARTESIAN_POINT('',(151.670050828726,-5.91258510326799,335.00367452382));
#10204=CARTESIAN_POINT('Ctrl Pts',(153.420052004703,-5.91674819671435,334.995380565238));
#10205=CARTESIAN_POINT('Ctrl Pts',(153.412312457465,-5.91687694484536,335.160286081005));
#10206=CARTESIAN_POINT('Ctrl Pts',(153.404572910228,-5.91010641488316,335.325274474005));
#10207=CARTESIAN_POINT('Ctrl Pts',(153.39683336299,-5.89644802442704,335.489725696416));
#10208=CARTESIAN_POINT('Ctrl Pts',(153.389442957064,-5.88340578220499,335.646758304562));
#10209=CARTESIAN_POINT('Ctrl Pts',(153.382052551138,-5.86408354313905,335.803300738551));
#10210=CARTESIAN_POINT('Ctrl Pts',(153.374662145212,-5.83854450795694,335.958816244703));
#10211=CARTESIAN_POINT('Ctrl Pts',(153.367271414372,-5.81300434996728,336.114338587995));
#10212=CARTESIAN_POINT('Ctrl Pts',(153.359880683532,-5.78124691155268,336.268833544905));
#10213=CARTESIAN_POINT('Ctrl Pts',(153.352489952691,-5.74338682147282,336.421772971129));
#10214=CARTESIAN_POINT('Ctrl Pts',(153.345097436661,-5.70551758649693,336.574749339027));
#10215=CARTESIAN_POINT('Ctrl Pts',(153.33770492063,-5.6615428544831,336.726169065647));
#10216=CARTESIAN_POINT('Ctrl Pts',(153.3303124046,-5.61162754100708,336.875517769447));
#10217=CARTESIAN_POINT('Ctrl Pts',(153.322916642304,-5.56169030829144,337.024932056527));
#10218=CARTESIAN_POINT('Ctrl Pts',(153.315520880009,-5.50580741819643,337.172273156199));
#10219=CARTESIAN_POINT('Ctrl Pts',(153.308125117713,-5.44419240269467,337.317045455951));
#10220=CARTESIAN_POINT('Ctrl Pts',(153.300720589961,-5.38250436108227,337.461989339818));
#10221=CARTESIAN_POINT('Ctrl Pts',(153.293316062208,-5.31507077499611,337.604358001018));
#10222=CARTESIAN_POINT('Ctrl Pts',(153.285911534456,-5.24215205157905,337.743678631076));
#10223=CARTESIAN_POINT('Ctrl Pts',(153.27850187318,-5.1691827739551,337.88309585147));
#10224=CARTESIAN_POINT('Ctrl Pts',(153.271092211903,-5.09072096791304,338.019460507959));
#10225=CARTESIAN_POINT('Ctrl Pts',(153.263682550627,-5.00707077070543,338.152328164968));
#10226=CARTESIAN_POINT('Ctrl Pts',(153.256262281163,-4.9233008140486,338.285386044569));
#10227=CARTESIAN_POINT('Ctrl Pts',(153.248842011699,-4.83432784604431,338.414936622404));
#10228=CARTESIAN_POINT('Ctrl Pts',(153.241421742236,-4.74049713056373,338.540567400519));
#10229=CARTESIAN_POINT('Ctrl Pts',(153.239048785156,-4.71049063798626,338.58074335987));
#10230=CARTESIAN_POINT('Ctrl Pts',(153.236675828076,-4.6799876412276,338.620518724397));
#10231=CARTESIAN_POINT('Ctrl Pts',(153.234302870997,-4.64900022323675,338.659880802273));
#10232=CARTESIAN_POINT('Ctrl Pts',(153.226878893559,-4.55205371965221,338.783028068852));
#10233=CARTESIAN_POINT('Ctrl Pts',(153.219454916121,-4.45006452049861,338.902506428246));
#10234=CARTESIAN_POINT('Ctrl Pts',(153.212030938683,-4.34334039661702,339.017875652831));
#10235=CARTESIAN_POINT('Ctrl Pts',(153.204615722655,-4.23674222325905,339.133108724374));
#10236=CARTESIAN_POINT('Ctrl Pts',(153.197200506627,-4.12542049899519,339.24424204261));
#10237=CARTESIAN_POINT('Ctrl Pts',(153.1897852906,-4.00972475439736,339.350866345508));
#10238=CARTESIAN_POINT('Ctrl Pts',(153.182377209456,-3.89414033166249,339.457388055039));
#10239=CARTESIAN_POINT('Ctrl Pts',(153.174969128312,-3.77419053985757,339.559409135248));
#10240=CARTESIAN_POINT('Ctrl Pts',(153.167561047168,-3.65026337667555,339.656555362433));
#10241=CARTESIAN_POINT('Ctrl Pts',(153.160158479993,-3.52642845474449,339.753629281907));
#10242=CARTESIAN_POINT('Ctrl Pts',(153.152755912819,-3.3986223485477,339.845835343851));
#10243=CARTESIAN_POINT('Ctrl Pts',(153.145353345645,-3.26726782940339,339.932838076954));
#10244=CARTESIAN_POINT('Ctrl Pts',(153.137954675891,-3.13598246783996,340.019795003497));
#10245=CARTESIAN_POINT('Ctrl Pts',(153.130556006136,-3.00115272437315,340.101553851564));
#10246=CARTESIAN_POINT('Ctrl Pts',(153.123157336381,-2.86323208885197,340.177821218222));
#10247=CARTESIAN_POINT('Ctrl Pts',(153.115759887177,-2.7253342059523,340.254076003133));
#10248=CARTESIAN_POINT('Ctrl Pts',(153.108362437973,-2.58434676927163,340.324840924172));
#10249=CARTESIAN_POINT('Ctrl Pts',(153.100964988769,-2.44074982231113,340.389867425771));
#10250=CARTESIAN_POINT('Ctrl Pts',(153.093567860306,-2.29715910146383,340.454891107934));
#10251=CARTESIAN_POINT('Ctrl Pts',(153.086170731842,-2.15095943528097,340.514176711413));
#10252=CARTESIAN_POINT('Ctrl Pts',(153.078773603379,-2.00265265036829,340.567523051095));
#10253=CARTESIAN_POINT('Ctrl Pts',(153.071375335942,-1.8543230299127,340.620877604782));
#10254=CARTESIAN_POINT('Ctrl Pts',(153.063977068506,-1.70388599592165,340.668290947457));
#10255=CARTESIAN_POINT('Ctrl Pts',(153.056578801069,-1.55186025930991,340.709611221272));
#10256=CARTESIAN_POINT('Ctrl Pts',(153.049177934543,-1.3997811144589,340.750946011333));
#10257=CARTESIAN_POINT('Ctrl Pts',(153.041777068017,-1.24611251567413,340.78618337286));
#10258=CARTESIAN_POINT('Ctrl Pts',(153.034376201492,-1.09138498298361,340.815222212557));
#10259=CARTESIAN_POINT('Ctrl Pts',(153.026967208107,-0.936487544669095,
340.844292939676));
#10260=CARTESIAN_POINT('Ctrl Pts',(153.019558214722,-0.780529217279805,
340.867151483));
#10261=CARTESIAN_POINT('Ctrl Pts',(153.012149221337,-0.624048020166595,
340.883748348717));
#10262=CARTESIAN_POINT('Ctrl Pts',(153.004735663757,-0.467470425238686,
340.900355438675));
#10263=CARTESIAN_POINT('Ctrl Pts',(152.997322106177,-0.310369690284292,
340.910693140179));
#10264=CARTESIAN_POINT('Ctrl Pts',(152.989908548597,-0.15328497797278,340.914764093185));
#10265=CARTESIAN_POINT('Ctrl Pts',(152.98248443646,0.00402337318518967,
340.918840841938));
#10266=CARTESIAN_POINT('Ctrl Pts',(152.975060324323,0.161315283973783,340.916633028671));
#10267=CARTESIAN_POINT('Ctrl Pts',(152.967636212186,0.31805474642866,340.908195303202));
#10268=CARTESIAN_POINT('Ctrl Pts',(152.963779087032,0.399487207609809,340.903811565112));
#10269=CARTESIAN_POINT('Ctrl Pts',(152.959921961877,0.480770675051538,340.897747086226));
#10270=CARTESIAN_POINT('Ctrl Pts',(152.956064836722,0.561831066392708,340.890014975816));
#10271=CARTESIAN_POINT('Ctrl Pts',(152.948640859284,0.717851545969991,340.875132644824));
#10272=CARTESIAN_POINT('Ctrl Pts',(152.941216881846,0.873515655144116,340.854024347346));
#10273=CARTESIAN_POINT('Ctrl Pts',(152.933792904408,1.02828664465397,340.826710662022));
#10274=CARTESIAN_POINT('Ctrl Pts',(152.926377688381,1.18287498110973,340.799429210957));
#10275=CARTESIAN_POINT('Ctrl Pts',(152.918962472353,1.33657193197829,340.765957013405));
#10276=CARTESIAN_POINT('Ctrl Pts',(152.911547256325,1.48884418903739,340.726366521912));
#10277=CARTESIAN_POINT('Ctrl Pts',(152.904139175181,1.64096993049717,340.68681412419));
#10278=CARTESIAN_POINT('Ctrl Pts',(152.896731094037,1.7916733484325,340.641155245714));
#10279=CARTESIAN_POINT('Ctrl Pts',(152.889323012893,1.94042978233305,340.589513648103));
#10280=CARTESIAN_POINT('Ctrl Pts',(152.881920445719,2.08907549410281,340.537910488277));
#10281=CARTESIAN_POINT('Ctrl Pts',(152.874517878545,2.23577675629784,340.480333597854));
#10282=CARTESIAN_POINT('Ctrl Pts',(152.867115311371,2.38002267811506,340.416956951477));
#10283=CARTESIAN_POINT('Ctrl Pts',(152.859716641616,2.52419265508479,340.353613672628));
#10284=CARTESIAN_POINT('Ctrl Pts',(152.852317971862,2.66590952539194,340.284476868891));
#10285=CARTESIAN_POINT('Ctrl Pts',(152.844919302107,2.80468115087269,340.209769112393));
#10286=CARTESIAN_POINT('Ctrl Pts',(152.837521852903,2.94342988334475,340.135073680354));
#10287=CARTESIAN_POINT('Ctrl Pts',(152.830124403699,3.0792340069957,340.054809296279));
#10288=CARTESIAN_POINT('Ctrl Pts',(152.822726954495,3.211624727061,339.969245131308));
#10289=CARTESIAN_POINT('Ctrl Pts',(152.815329826032,3.3440097068956,339.88368467625));
#10290=CARTESIAN_POINT('Ctrl Pts',(152.807932697568,3.4729812639703,339.792825099774));
#10291=CARTESIAN_POINT('Ctrl Pts',(152.800535569105,3.59809865026128,339.696979525768));
#10292=CARTESIAN_POINT('Ctrl Pts',(152.793137301668,3.72323530150648,339.601119193937));
#10293=CARTESIAN_POINT('Ctrl Pts',(152.785739034231,3.84451630404892,339.50027156292));
#10294=CARTESIAN_POINT('Ctrl Pts',(152.778340766795,3.96153325314481,339.394790648794));
#10295=CARTESIAN_POINT('Ctrl Pts',(152.770939900269,4.07859131152499,339.289272678115));
#10296=CARTESIAN_POINT('Ctrl Pts',(152.763539033743,4.19138205689374,339.179118433262));
#10297=CARTESIAN_POINT('Ctrl Pts',(152.756138167218,4.29953338291418,339.064719332464));
#10298=CARTESIAN_POINT('Ctrl Pts',(152.748729173833,4.40780346943071,338.950194610516));
#10299=CARTESIAN_POINT('Ctrl Pts',(152.741320180448,4.51142370601488,338.831415995204));
#10300=CARTESIAN_POINT('Ctrl Pts',(152.733911187063,4.61006131912147,338.708809134539));
#10301=CARTESIAN_POINT('Ctrl Pts',(152.726497629483,4.70875969640019,338.586126743818));
#10302=CARTESIAN_POINT('Ctrl Pts',(152.719084071903,4.80246911226237,338.459611707658));
#10303=CARTESIAN_POINT('Ctrl Pts',(152.711670514323,4.89090001484624,338.329718848083));
#10304=CARTESIAN_POINT('Ctrl Pts',(152.704246402186,4.97945681500932,338.199641062241));
#10305=CARTESIAN_POINT('Ctrl Pts',(152.696822290049,5.06271989606705,338.06617616434));
#10306=CARTESIAN_POINT('Ctrl Pts',(152.689398177913,5.1404451495519,337.929804469064));
#10307=CARTESIAN_POINT('Ctrl Pts',(152.685541052758,5.18082654800784,337.858953882953));
#10308=CARTESIAN_POINT('Ctrl Pts',(152.681683927603,5.21971394660945,337.78731904357));
#10309=CARTESIAN_POINT('Ctrl Pts',(152.677826802448,5.25707827900714,337.714969342532));
#10310=CARTESIAN_POINT('Ctrl Pts',(152.67040282501,5.32899504332747,337.575714709457));
#10311=CARTESIAN_POINT('Ctrl Pts',(152.662978847572,5.39548340713141,337.433390528146));
#10312=CARTESIAN_POINT('Ctrl Pts',(152.655554870134,5.45627020961228,337.288459298785));
#10313=CARTESIAN_POINT('Ctrl Pts',(152.648139654107,5.51698527452039,337.143699110082));
#10314=CARTESIAN_POINT('Ctrl Pts',(152.640724438079,5.57201202874473,336.996338338386));
#10315=CARTESIAN_POINT('Ctrl Pts',(152.633309222052,5.62112279549672,336.84686466219));
#10316=CARTESIAN_POINT('Ctrl Pts',(152.625901140908,5.67018630811622,336.697534808813));
#10317=CARTESIAN_POINT('Ctrl Pts',(152.618493059763,5.7133450499217,336.546096450506));
#10318=CARTESIAN_POINT('Ctrl Pts',(152.611084978619,5.7504191707918,336.393057759998));
#10319=CARTESIAN_POINT('Ctrl Pts',(152.603682411445,5.78746569671659,336.240132978983));
#10320=CARTESIAN_POINT('Ctrl Pts',(152.596279844271,5.81843653190088,336.085610598699));
#10321=CARTESIAN_POINT('Ctrl Pts',(152.588877277097,5.843201503006,335.930014385786));
#10322=CARTESIAN_POINT('Ctrl Pts',(152.581478607343,5.86795343546202,335.774500093599));
#10323=CARTESIAN_POINT('Ctrl Pts',(152.574079937588,5.88650595246598,335.617913462389));
#10324=CARTESIAN_POINT('Ctrl Pts',(152.566681267833,5.89877989546819,335.460788788189));
#10325=CARTESIAN_POINT('Ctrl Pts',(152.559283818629,5.91105181365097,335.303690034679));
#10326=CARTESIAN_POINT('Ctrl Pts',(152.551886369425,5.91704718446333,335.146053786055));
#10327=CARTESIAN_POINT('Ctrl Pts',(152.544488920221,5.91673866791336,334.988419925784));
#10328=CARTESIAN_POINT('Ctrl Pts',(152.537091791758,5.91643016474013,334.830792900242));
#10329=CARTESIAN_POINT('Ctrl Pts',(152.529694663294,5.90981831839625,334.673168636057));
#10330=CARTESIAN_POINT('Ctrl Pts',(152.522297534831,5.89692792739588,334.516087216951));
#10331=CARTESIAN_POINT('Ctrl Pts',(152.514899267394,5.88403555159709,334.358981611227));
#10332=CARTESIAN_POINT('Ctrl Pts',(152.507500999958,5.86486273676256,334.202419388993));
#10333=CARTESIAN_POINT('Ctrl Pts',(152.500102732521,5.83948617132484,334.046935564924));
#10334=CARTESIAN_POINT('Ctrl Pts',(152.492701865995,5.81410069083268,333.891397117753));
#10335=CARTESIAN_POINT('Ctrl Pts',(152.485300999469,5.78250718054896,333.736938191147));
#10336=CARTESIAN_POINT('Ctrl Pts',(152.477900132944,5.74483342432099,333.584083516127));
#10337=CARTESIAN_POINT('Ctrl Pts',(152.470491139559,5.70711829870718,333.431060992061));
#10338=CARTESIAN_POINT('Ctrl Pts',(152.463082146174,5.66330968280516,333.279646600216));
#10339=CARTESIAN_POINT('Ctrl Pts',(152.455673152789,5.61358543024608,333.130350519528));
#10340=CARTESIAN_POINT('Ctrl Pts',(152.448259595209,5.56383054583228,332.980962467304));
#10341=CARTESIAN_POINT('Ctrl Pts',(152.440846037629,5.50815289481398,332.833695674806));
#10342=CARTESIAN_POINT('Ctrl Pts',(152.433432480049,5.44677825360676,332.689039762666));
#10343=CARTESIAN_POINT('Ctrl Pts',(152.426008367912,5.38531623436161,332.544177906353));
#10344=CARTESIAN_POINT('Ctrl Pts',(152.418584255775,5.31814118516296,332.401934690683));
#10345=CARTESIAN_POINT('Ctrl Pts',(152.411160143639,5.24552491177776,332.262775317512));
#10346=CARTESIAN_POINT('Ctrl Pts',(152.407303018484,5.20779783417411,332.1904764205));
#10347=CARTESIAN_POINT('Ctrl Pts',(152.403445893329,5.16860277221613,332.119009455393));
#10348=CARTESIAN_POINT('Ctrl Pts',(152.399588768174,5.12798234932573,332.04843641649));
#10349=CARTESIAN_POINT('Ctrl Pts',(152.392164790736,5.04979844526201,331.912601402709));
#10350=CARTESIAN_POINT('Ctrl Pts',(152.384740813298,4.96609567359945,331.779670138052));
#10351=CARTESIAN_POINT('Ctrl Pts',(152.37731683586,4.87711513762627,331.650122614656));
#10352=CARTESIAN_POINT('Ctrl Pts',(152.369901619833,4.78823961207352,331.52072797683));
#10353=CARTESIAN_POINT('Ctrl Pts',(152.362486403805,4.69409892949561,331.394709436135));
#10354=CARTESIAN_POINT('Ctrl Pts',(152.355071187777,4.59497998016596,331.272522361653));
#10355=CARTESIAN_POINT('Ctrl Pts',(152.347663106633,4.49595640259028,331.15045285496));
#10356=CARTESIAN_POINT('Ctrl Pts',(152.340255025489,4.39196432793274,331.032207763013));
#10357=CARTESIAN_POINT('Ctrl Pts',(152.332846944345,4.28333376226275,330.918213327039));
#10358=CARTESIAN_POINT('Ctrl Pts',(152.325444377171,4.17478405230648,330.804303739206));
#10359=CARTESIAN_POINT('Ctrl Pts',(152.318041809997,4.06160298215941,330.694638776702));
#10360=CARTESIAN_POINT('Ctrl Pts',(152.310639242823,3.94416055409882,330.589611345245));
#10361=CARTESIAN_POINT('Ctrl Pts',(152.303240573068,3.82677995896376,330.484639210273));
#10362=CARTESIAN_POINT('Ctrl Pts',(152.295841903314,3.70514275164424,330.384299991837));
#10363=CARTESIAN_POINT('Ctrl Pts',(152.288443233559,3.57965539583741,330.288949394291));
#10364=CARTESIAN_POINT('Ctrl Pts',(152.281045784355,3.45418874154727,330.193614526632));
#10365=CARTESIAN_POINT('Ctrl Pts',(152.273648335151,3.32487349621752,330.103266872114));
#10366=CARTESIAN_POINT('Ctrl Pts',(152.266250885947,3.19214886413591,330.018221583441));
#10367=CARTESIAN_POINT('Ctrl Pts',(152.258853757483,3.0594299867632,329.933179982183));
#10368=CARTESIAN_POINT('Ctrl Pts',(152.25145662902,2.9233023307996,329.853440491003));
#10369=CARTESIAN_POINT('Ctrl Pts',(152.244059500556,2.78423348406682,329.779274526591));
#10370=CARTESIAN_POINT('Ctrl Pts',(152.23666123312,2.64514322420307,329.705097142472));
#10371=CARTESIAN_POINT('Ctrl Pts',(152.229262965683,2.50311120117458,329.636495169511));
#10372=CARTESIAN_POINT('Ctrl Pts',(152.221864698246,2.35862882074756,329.57369364591));
#10373=CARTESIAN_POINT('Ctrl Pts',(152.214463831721,2.21409568214128,329.510870059473));
#10374=CARTESIAN_POINT('Ctrl Pts',(152.207062965195,2.06711081427276,329.453851128251));
#10375=CARTESIAN_POINT('Ctrl Pts',(152.199662098669,1.91818462582289,329.402813358145));
#10376=CARTESIAN_POINT('Ctrl Pts',(152.192253105284,1.76909490217986,329.351719543688));
#10377=CARTESIAN_POINT('Ctrl Pts',(152.1848441119,1.61805995399045,329.306620127833));
#10378=CARTESIAN_POINT('Ctrl Pts',(152.177435118515,1.46560504840998,329.267641636763));
#10379=CARTESIAN_POINT('Ctrl Pts',(152.170021560935,1.31305622534886,329.228639133597));
#10380=CARTESIAN_POINT('Ctrl Pts',(152.162608003354,1.15908606598829,329.195765146582));
#10381=CARTESIAN_POINT('Ctrl Pts',(152.155194445774,1.00422848333707,329.16909477733));
#10382=CARTESIAN_POINT('Ctrl Pts',(152.147770333637,0.849150432566782,329.142386437926));
#10383=CARTESIAN_POINT('Ctrl Pts',(152.140346221501,0.693182804258974,329.121899404001));
#10384=CARTESIAN_POINT('Ctrl Pts',(152.132922109364,0.536863886274555,329.107656855705));
#10385=CARTESIAN_POINT('Ctrl Pts',(152.12906498421,0.455649914880493,329.100257278452));
#10386=CARTESIAN_POINT('Ctrl Pts',(152.125207859055,0.374341122206674,329.094542366649));
#10387=CARTESIAN_POINT('Ctrl Pts',(152.1213507339,0.293012706561376,329.090509826026));
#10388=CARTESIAN_POINT('Ctrl Pts',(152.113926756462,0.136476348880449,329.082748218766));
#10389=CARTESIAN_POINT('Ctrl Pts',(152.106502779024,-0.0206047601445989,
329.081198930277));
#10390=CARTESIAN_POINT('Ctrl Pts',(152.099078801586,-0.177696510059613,
329.085918962948));
#10391=CARTESIAN_POINT('Ctrl Pts',(152.091663585559,-0.334602868073692,
329.090633425272));
#10392=CARTESIAN_POINT('Ctrl Pts',(152.084248369531,-0.491519472565919,
329.101602470342));
#10393=CARTESIAN_POINT('Ctrl Pts',(152.076833153504,-0.647908141170273,
329.118831272349));
#10394=CARTESIAN_POINT('Ctrl Pts',(152.069425072359,-0.804146333385481,
329.136043496889));
#10395=CARTESIAN_POINT('Ctrl Pts',(152.062016991215,-0.959857232513241,
329.159503446887));
#10396=CARTESIAN_POINT('Ctrl Pts',(152.054608910071,-1.11450381799239,329.189164276786));
#10397=CARTESIAN_POINT('Ctrl Pts',(152.047206342897,-1.26903529719323,329.218803029587));
#10398=CARTESIAN_POINT('Ctrl Pts',(152.039803775723,-1.42250367514679,329.254633402301));
#10399=CARTESIAN_POINT('Ctrl Pts',(152.032401208549,-1.57437831958847,329.296556875947));
#10400=CARTESIAN_POINT('Ctrl Pts',(152.025002538794,-1.72617300269303,329.338458277067));
#10401=CARTESIAN_POINT('Ctrl Pts',(152.01760386904,-1.87637526454022,329.386446291159));
#10402=CARTESIAN_POINT('Ctrl Pts',(152.010205199285,-2.02446602492158,329.440371606264));
#10403=CARTESIAN_POINT('Ctrl Pts',(152.002807750081,-2.17253235492683,329.494288025366));
#10404=CARTESIAN_POINT('Ctrl Pts',(151.995410300877,-2.31848752444893,329.554139673976));
#10405=CARTESIAN_POINT('Ctrl Pts',(151.988012851673,-2.46182883621265,329.61972776305));
#10406=CARTESIAN_POINT('Ctrl Pts',(151.98061572321,-2.6051639329473,329.685313008339));
#10407=CARTESIAN_POINT('Ctrl Pts',(151.973218594746,-2.7458850578937,329.756634044267));
#10408=CARTESIAN_POINT('Ctrl Pts',(151.965821466283,-2.88351093236498,329.833444545402));
#10409=CARTESIAN_POINT('Ctrl Pts',(151.958423198846,-3.0211579977855,329.910266873438));
#10410=CARTESIAN_POINT('Ctrl Pts',(151.951024931409,-3.15570853786383,329.992580167774));
#10411=CARTESIAN_POINT('Ctrl Pts',(151.943626663973,-3.28670738531855,330.0800929759));
#10412=CARTESIAN_POINT('Ctrl Pts',(151.936225797447,-3.41775225404523,330.167636528195));
#10413=CARTESIAN_POINT('Ctrl Pts',(151.928824930921,-3.54524263574842,330.26038302394));
#10414=CARTESIAN_POINT('Ctrl Pts',(151.921424064396,-3.66875389142648,330.357998767057));
#10415=CARTESIAN_POINT('Ctrl Pts',(151.914015071011,-3.79240077427206,330.455721701593));
#10416=CARTESIAN_POINT('Ctrl Pts',(151.906606077626,-3.91205951206739,330.558324329992));
#10417=CARTESIAN_POINT('Ctrl Pts',(151.899197084241,-4.0273394540485,330.665433414473));
#10418=CARTESIAN_POINT('Ctrl Pts',(151.891783526661,-4.14269041244969,330.772608481845));
#10419=CARTESIAN_POINT('Ctrl Pts',(151.884369969081,-4.25365693750218,330.884295272977));
#10420=CARTESIAN_POINT('Ctrl Pts',(151.876956411501,-4.35988694369155,331.000085450822));
#10421=CARTESIAN_POINT('Ctrl Pts',(151.869532299364,-4.46626818774307,331.116040477183));
#10422=CARTESIAN_POINT('Ctrl Pts',(151.862108187227,-4.56789920474008,331.236110273648));
#10423=CARTESIAN_POINT('Ctrl Pts',(151.854684075091,-4.66446920355254,331.359854726579));
#10424=CARTESIAN_POINT('Ctrl Pts',(151.850826949936,-4.7146412059084,331.424144951911));
#10425=CARTESIAN_POINT('Ctrl Pts',(151.846969824781,-4.76344785038058,331.489426583622));
#10426=CARTESIAN_POINT('Ctrl Pts',(151.843112699626,-4.81085037215204,331.555635144288));
#10427=CARTESIAN_POINT('Ctrl Pts',(151.83562238215,-4.90290337095759,331.684208400059));
#10428=CARTESIAN_POINT('Ctrl Pts',(151.828132064673,-4.98993472057112,331.816664597315));
#10429=CARTESIAN_POINT('Ctrl Pts',(151.820641747196,-5.07160260010362,331.952578527817));
#10430=CARTESIAN_POINT('Ctrl Pts',(151.813160572798,-5.15317079149597,332.088326554576));
#10431=CARTESIAN_POINT('Ctrl Pts',(151.8056793984,-5.22938835994049,332.227523603511));
#10432=CARTESIAN_POINT('Ctrl Pts',(151.798198224001,-5.29995476856217,332.369712940819));
#10433=CARTESIAN_POINT('Ctrl Pts',(151.790724794843,-5.37044811997292,332.511755069893));
#10434=CARTESIAN_POINT('Ctrl Pts',(151.783251365684,-5.43530179937797,332.656782995412));
#10435=CARTESIAN_POINT('Ctrl Pts',(151.775777936525,-5.49425952383021,332.80431267087));
#10436=CARTESIAN_POINT('Ctrl Pts',(151.768310859863,-5.55316713357213,332.951716944492));
#10437=CARTESIAN_POINT('Ctrl Pts',(151.7608437832,-5.60618863382233,333.101618396629));
#10438=CARTESIAN_POINT('Ctrl Pts',(151.753376706538,-5.65311452289628,333.253510162206));
#10439=CARTESIAN_POINT('Ctrl Pts',(151.745915097621,-5.70000605062241,333.405290705472));
#10440=CARTESIAN_POINT('Ctrl Pts',(151.738453488704,-5.74081075387373,333.55905831107));
#10441=CARTESIAN_POINT('Ctrl Pts',(151.730991879787,-5.77536800135642,333.714288130486));
#10442=CARTESIAN_POINT('Ctrl Pts',(151.723533523754,-5.80991018362923,333.869450277563));
#10443=CARTESIAN_POINT('Ctrl Pts',(151.716075167721,-5.8382102557323,334.026073013779));
#10444=CARTESIAN_POINT('Ctrl Pts',(151.708616811688,-5.86015796662616,334.18361824574));
#10445=CARTESIAN_POINT('Ctrl Pts',(151.70115959323,-5.88210232997663,334.341139448339));
#10446=CARTESIAN_POINT('Ctrl Pts',(151.693702374772,-5.89769620725362,334.499582506367));
#10447=CARTESIAN_POINT('Ctrl Pts',(151.686245156313,-5.90688078937849,334.65840096228));
#10448=CARTESIAN_POINT('Ctrl Pts',(151.68084743911,-5.91352881467381,334.773357647071));
#10449=CARTESIAN_POINT('Ctrl Pts',(151.675449721906,-5.91681994241088,334.888510813414));
#10450=CARTESIAN_POINT('Ctrl Pts',(151.670052004703,-5.9167488729118,335.003652040113));
#10451=CARTESIAN_POINT('',(149.920053353871,-5.92109797199052,335.003013532025));
#10452=CARTESIAN_POINT('Ctrl Pts',(151.670049900736,-5.90929938065838,335.003692266209));
#10453=CARTESIAN_POINT('Ctrl Pts',(151.634991488942,-5.9134882699069,335.750600828835));
#10454=CARTESIAN_POINT('Ctrl Pts',(151.507187065722,-5.43515578827606,338.468256395567));
#10455=CARTESIAN_POINT('Ctrl Pts',(151.286636631079,-1.35011516578284,341.865115582446));
#10456=CARTESIAN_POINT('Ctrl Pts',(151.008398596804,5.04239736829986,339.850448608261));
#10457=CARTESIAN_POINT('Ctrl Pts',(150.73016056253,6.80757626315719,333.384596538777));
#10458=CARTESIAN_POINT('Ctrl Pts',(150.451922528256,2.32554290097631,328.401176382346));
#10459=CARTESIAN_POINT('Ctrl Pts',(150.181887150958,-4.095558012434,329.44178936122));
#10460=CARTESIAN_POINT('Ctrl Pts',(150.004597785083,-5.91334784080282,333.213692926844));
#10461=CARTESIAN_POINT('Ctrl Pts',(149.920054430632,-5.92456868112744,335.002992526362));
#10462=CARTESIAN_POINT('',(148.170052004658,-5.91674764560021,334.994721668406));
#10463=CARTESIAN_POINT('Ctrl Pts',(149.920052004703,-5.91674921910679,335.003039851844));
#10464=CARTESIAN_POINT('Ctrl Pts',(149.911850156372,-5.91666015362462,335.176396366927));
#10465=CARTESIAN_POINT('Ctrl Pts',(149.90364830804,-5.9089529647869,335.349551836332));
#10466=CARTESIAN_POINT('Ctrl Pts',(149.895446459709,-5.89367613405626,335.5220270006));
#10467=CARTESIAN_POINT('Ctrl Pts',(149.888022482271,-5.87984817210363,335.678144460519));
#10468=CARTESIAN_POINT('Ctrl Pts',(149.880598504833,-5.85979197820686,335.833947619004));
#10469=CARTESIAN_POINT('Ctrl Pts',(149.873174527395,-5.83352450441269,335.988899600018));
#10470=CARTESIAN_POINT('Ctrl Pts',(149.865759311367,-5.80728803018976,336.143668714382));
#10471=CARTESIAN_POINT('Ctrl Pts',(149.858344095339,-5.77485492880872,336.297588286399));
#10472=CARTESIAN_POINT('Ctrl Pts',(149.850928879312,-5.73629404828548,336.450124530551));
#10473=CARTESIAN_POINT('Ctrl Pts',(149.843520798168,-5.69777027084729,336.602514005096));
#10474=CARTESIAN_POINT('Ctrl Pts',(149.836112717024,-5.65313054319746,336.7535224422));
#10475=CARTESIAN_POINT('Ctrl Pts',(149.82870463588,-5.6024950796755,336.902624357227));
#10476=CARTESIAN_POINT('Ctrl Pts',(149.821302068706,-5.55189730505386,337.051615292975));
#10477=CARTESIAN_POINT('Ctrl Pts',(149.813899501532,-5.49531280001478,337.198702180324));
#10478=CARTESIAN_POINT('Ctrl Pts',(149.806496934358,-5.43291208380104,337.343372964807));
#10479=CARTESIAN_POINT('Ctrl Pts',(149.799098264603,-5.37054422129158,337.487967580755));
#10480=CARTESIAN_POINT('Ctrl Pts',(149.791699594848,-5.30236639362072,337.630148285406));
#10481=CARTESIAN_POINT('Ctrl Pts',(149.784300925093,-5.2285978430923,337.769421448193));
#10482=CARTESIAN_POINT('Ctrl Pts',(149.776903475889,-5.15484146208413,337.908671635233));
#10483=CARTESIAN_POINT('Ctrl Pts',(149.769506026685,-5.0754963631945,338.045014902884));
#10484=CARTESIAN_POINT('Ctrl Pts',(149.762108577482,-4.99082854437905,338.177980648637));
#10485=CARTESIAN_POINT('Ctrl Pts',(149.754711449018,-4.90616439661264,338.310940629227));
#10486=CARTESIAN_POINT('Ctrl Pts',(149.747314320555,-4.8161781882525,338.44052306429));
#10487=CARTESIAN_POINT('Ctrl Pts',(149.739917192091,-4.72118005847716,338.566285100484));
#10488=CARTESIAN_POINT('Ctrl Pts',(149.732518924655,-4.62616730136124,338.692066500893));
#10489=CARTESIAN_POINT('Ctrl Pts',(149.725120657218,-4.52614131121688,338.814026033343));
#10490=CARTESIAN_POINT('Ctrl Pts',(149.717722389781,-4.42145333697985,338.931752910778));
#10491=CARTESIAN_POINT('Ctrl Pts',(149.710321523256,-4.31672858475645,339.049521146903));
#10492=CARTESIAN_POINT('Ctrl Pts',(149.70292065673,-4.20733883542256,339.16305348873));
#10493=CARTESIAN_POINT('Ctrl Pts',(149.695519790204,-4.09367298442977,339.271975194105));
#10494=CARTESIAN_POINT('Ctrl Pts',(149.68811079682,-3.97988231746572,339.381016505926));
#10495=CARTESIAN_POINT('Ctrl Pts',(149.680701803435,-3.86180644116627,339.485436812003));
#10496=CARTESIAN_POINT('Ctrl Pts',(149.67329281005,-3.73986874570421,339.584900470829));
#10497=CARTESIAN_POINT('Ctrl Pts',(149.66587925247,-3.61785593241605,339.684425402699));
#10498=CARTESIAN_POINT('Ctrl Pts',(149.65846569489,-3.49197685716381,339.77898737925));
#10499=CARTESIAN_POINT('Ctrl Pts',(149.651052137309,-3.36268437546262,339.868293782581));
#10500=CARTESIAN_POINT('Ctrl Pts',(149.643628025173,-3.23320782224322,339.957727329927));
#10501=CARTESIAN_POINT('Ctrl Pts',(149.636203913036,-3.10030847141647,340.041890161325));
#10502=CARTESIAN_POINT('Ctrl Pts',(149.628779800899,-2.96446497757998,340.120534929009));
#10503=CARTESIAN_POINT('Ctrl Pts',(149.624922675745,-2.89388881338412,340.161394052111));
#10504=CARTESIAN_POINT('Ctrl Pts',(149.62106555059,-2.82251832078065,340.20076450764));
#10505=CARTESIAN_POINT('Ctrl Pts',(149.617208425435,-2.75042269343963,340.238616761122));
#10506=CARTESIAN_POINT('Ctrl Pts',(149.609784447997,-2.61165708711303,340.31147264849));
#10507=CARTESIAN_POINT('Ctrl Pts',(149.60236047056,-2.46978532988706,340.378920996201));
#10508=CARTESIAN_POINT('Ctrl Pts',(149.594936493122,-2.32526806599919,340.440685525165));
#10509=CARTESIAN_POINT('Ctrl Pts',(149.587521277094,-2.18092135422653,340.502377162692));
#10510=CARTESIAN_POINT('Ctrl Pts',(149.580106061066,-2.03393569021874,340.558398188133));
#10511=CARTESIAN_POINT('Ctrl Pts',(149.572690845039,-1.88479720321985,340.608517635279));
#10512=CARTESIAN_POINT('Ctrl Pts',(149.565282763895,-1.73580221652222,340.658588857745));
#10513=CARTESIAN_POINT('Ctrl Pts',(149.55787468275,-1.5846588820798,340.702769688597));
#10514=CARTESIAN_POINT('Ctrl Pts',(149.550466601606,-1.43187414601021,340.740876848748));
#10515=CARTESIAN_POINT('Ctrl Pts',(149.543064034432,-1.27920313041009,340.778955645044));
#10516=CARTESIAN_POINT('Ctrl Pts',(149.535661467258,-1.12489350638225,340.810969682167));
#10517=CARTESIAN_POINT('Ctrl Pts',(149.528258900084,-0.969468149198965,
340.836785251334));
#10518=CARTESIAN_POINT('Ctrl Pts',(149.52086023033,-0.814124622786566,340.862587228716));
#10519=CARTESIAN_POINT('Ctrl Pts',(149.513461560575,-0.657666900357778,
340.882197176531));
#10520=CARTESIAN_POINT('Ctrl Pts',(149.50606289082,-0.500628730977748,340.895532328486));
#10521=CARTESIAN_POINT('Ctrl Pts',(149.498665441616,-0.343616468019706,
340.908865280554));
#10522=CARTESIAN_POINT('Ctrl Pts',(149.491267992412,-0.186024319665954,
340.915925459645));
#10523=CARTESIAN_POINT('Ctrl Pts',(149.483870543208,-0.0283919723632106,
340.916681879094));
#10524=CARTESIAN_POINT('Ctrl Pts',(149.476473414745,0.129233540275767,340.917438265747));
#10525=CARTESIAN_POINT('Ctrl Pts',(149.469076286281,0.286898875191166,340.911891434416));
#10526=CARTESIAN_POINT('Ctrl Pts',(149.461679157818,0.444063793455606,340.900062534401));
#10527=CARTESIAN_POINT('Ctrl Pts',(149.454280890381,0.601252911194095,340.88823181303));
#10528=CARTESIAN_POINT('Ctrl Pts',(149.446882622944,0.757941086680273,340.870117125002));
#10529=CARTESIAN_POINT('Ctrl Pts',(149.439484355508,0.913592799362333,340.845791542593));
#10530=CARTESIAN_POINT('Ctrl Pts',(149.432083488982,1.06929919412793,340.821457414351));
#10531=CARTESIAN_POINT('Ctrl Pts',(149.424682622456,1.22396803262342,340.790908105056));
#10532=CARTESIAN_POINT('Ctrl Pts',(149.41728175593,1.3770737325329,340.754267850706));
#10533=CARTESIAN_POINT('Ctrl Pts',(149.409872762546,1.53034755713853,340.717587361854));
#10534=CARTESIAN_POINT('Ctrl Pts',(149.402463769161,1.6820544520858,340.67480265769));
#10535=CARTESIAN_POINT('Ctrl Pts',(149.395054775776,1.83168304855458,340.626088141163));
#10536=CARTESIAN_POINT('Ctrl Pts',(149.387641218196,1.98140382139997,340.577343614815));
#10537=CARTESIAN_POINT('Ctrl Pts',(149.380227660616,2.12904339543219,340.522662126399));
#10538=CARTESIAN_POINT('Ctrl Pts',(149.372814103035,2.27411063591168,340.462266139446));
#10539=CARTESIAN_POINT('Ctrl Pts',(149.365389990899,2.41938440616606,340.401784167747));
#10540=CARTESIAN_POINT('Ctrl Pts',(149.357965878762,2.56207819111879,340.335571605685));
#10541=CARTESIAN_POINT('Ctrl Pts',(149.350541766625,2.70172496328973,340.263897110054));
#10542=CARTESIAN_POINT('Ctrl Pts',(149.346684641471,2.77427708370367,340.226659323911));
#10543=CARTESIAN_POINT('Ctrl Pts',(149.342827516316,2.84600720847702,340.187947966621));
#10544=CARTESIAN_POINT('Ctrl Pts',(149.338970391161,2.91685305677357,340.147805241818));
#10545=CARTESIAN_POINT('Ctrl Pts',(149.331546413723,3.05321315872498,340.070540784148));
#10546=CARTESIAN_POINT('Ctrl Pts',(149.324122436285,3.18670686169737,339.987737967928));
#10547=CARTESIAN_POINT('Ctrl Pts',(149.316698458847,3.31685255568017,339.899634648255));
#10548=CARTESIAN_POINT('Ctrl Pts',(149.30928324282,3.44684465816264,339.811635303754));
#10549=CARTESIAN_POINT('Ctrl Pts',(149.301868026792,3.57349631044197,339.71834811444));
#10550=CARTESIAN_POINT('Ctrl Pts',(149.294452810764,3.69635021567802,339.620056887697));
#10551=CARTESIAN_POINT('Ctrl Pts',(149.28704472962,3.81908591150498,339.521860236277));
#10552=CARTESIAN_POINT('Ctrl Pts',(149.279636648476,3.93803084559408,339.418669364512));
#10553=CARTESIAN_POINT('Ctrl Pts',(149.272228567332,4.0527565570192,339.310811391378));
#10554=CARTESIAN_POINT('Ctrl Pts',(149.264826000158,4.167396876002,339.203033698904));
#10555=CARTESIAN_POINT('Ctrl Pts',(149.257423432984,4.2778239546545,339.09059607646));
#10556=CARTESIAN_POINT('Ctrl Pts',(149.25002086581,4.38364239659471,338.973865863523));
#10557=CARTESIAN_POINT('Ctrl Pts',(149.242622196055,4.48940512558775,338.857197108534));
#10558=CARTESIAN_POINT('Ctrl Pts',(149.235223526301,4.59056380021348,338.736240539846));
#10559=CARTESIAN_POINT('Ctrl Pts',(149.227824856546,4.68675997828438,338.611400208846));
#10560=CARTESIAN_POINT('Ctrl Pts',(149.220427407342,4.78294028697303,338.486580472624));
#10561=CARTESIAN_POINT('Ctrl Pts',(149.213029958138,4.87415949630309,338.357878541011));
#10562=CARTESIAN_POINT('Ctrl Pts',(149.205632508934,4.96009949362319,338.225731479193));
#10563=CARTESIAN_POINT('Ctrl Pts',(149.198235380471,5.04603576473476,338.093590147042));
#10564=CARTESIAN_POINT('Ctrl Pts',(149.190838252007,5.12669307549016,337.958004294559));
#10565=CARTESIAN_POINT('Ctrl Pts',(149.183441123544,5.20179685650292,337.819439665284));
#10566=CARTESIAN_POINT('Ctrl Pts',(149.176042856107,5.27691220162313,337.680853700515));
#10567=CARTESIAN_POINT('Ctrl Pts',(149.168644588671,5.34647213652136,337.53928837384));
#10568=CARTESIAN_POINT('Ctrl Pts',(149.161246321234,5.41024830833589,337.39523355952));
#10569=CARTESIAN_POINT('Ctrl Pts',(149.153845454708,5.47404688539028,337.251128137227));
#10570=CARTESIAN_POINT('Ctrl Pts',(149.146444588182,5.53205750286878,337.104531827043));
#10571=CARTESIAN_POINT('Ctrl Pts',(149.139043721657,5.58410021072489,336.955953833576));
#10572=CARTESIAN_POINT('Ctrl Pts',(149.131634728272,5.63620006644974,336.807212687268));
#10573=CARTESIAN_POINT('Ctrl Pts',(149.124225734887,5.68231880174213,336.656485864374));
#10574=CARTESIAN_POINT('Ctrl Pts',(149.116816741502,5.72232634475302,336.504297765286));
#10575=CARTESIAN_POINT('Ctrl Pts',(149.109403183922,5.76235853379041,336.352015913081));
#10576=CARTESIAN_POINT('Ctrl Pts',(149.101989626342,5.79627194866979,336.19827135452));
#10577=CARTESIAN_POINT('Ctrl Pts',(149.094576068762,5.8239878825285,336.043597483066));
#10578=CARTESIAN_POINT('Ctrl Pts',(149.087151956625,5.85174327509312,335.888703405038));
#10579=CARTESIAN_POINT('Ctrl Pts',(149.079727844488,5.87328351387791,335.732877740426));
#10580=CARTESIAN_POINT('Ctrl Pts',(149.072303732352,5.88858178274542,335.576658608207));
#10581=CARTESIAN_POINT('Ctrl Pts',(149.068446607197,5.89652984934074,335.495496479531));
#10582=CARTESIAN_POINT('Ctrl Pts',(149.064589482042,5.9027939295139,335.414228150625));
#10583=CARTESIAN_POINT('Ctrl Pts',(149.060732356887,5.90737580946663,335.332928833579));
#10584=CARTESIAN_POINT('Ctrl Pts',(149.053308379449,5.91619475415412,335.176448483254));
#10585=CARTESIAN_POINT('Ctrl Pts',(149.045884402011,5.91880520201925,335.019381425379));
#10586=CARTESIAN_POINT('Ctrl Pts',(149.038460424573,5.91514654367648,334.862261373129));
#10587=CARTESIAN_POINT('Ctrl Pts',(149.031045208546,5.91149220310102,334.705326746181));
#10588=CARTESIAN_POINT('Ctrl Pts',(149.023629992518,5.90158349173057,334.548339618829));
#10589=CARTESIAN_POINT('Ctrl Pts',(149.01621477649,5.88541159968937,334.391838126202));
#10590=CARTESIAN_POINT('Ctrl Pts',(149.008806695346,5.86925526816128,334.235487218523));
#10591=CARTESIAN_POINT('Ctrl Pts',(149.001398614202,5.84684779150791,334.079621384065));
#10592=CARTESIAN_POINT('Ctrl Pts',(148.993990533058,5.8182323862625,333.92477794761));
#10593=CARTESIAN_POINT('Ctrl Pts',(148.986587965884,5.78963827998582,333.770049763952));
#10594=CARTESIAN_POINT('Ctrl Pts',(148.97918539871,5.75484551308457,333.61634282848));
#10595=CARTESIAN_POINT('Ctrl Pts',(148.971782831536,5.71394901749076,333.464188426917));
#10596=CARTESIAN_POINT('Ctrl Pts',(148.964384161781,5.67307405372311,333.31211413398));
#10597=CARTESIAN_POINT('Ctrl Pts',(148.956985492026,5.62610185794155,333.161591106558));
#10598=CARTESIAN_POINT('Ctrl Pts',(148.949586822272,5.5731782319411,333.013139421721));
#10599=CARTESIAN_POINT('Ctrl Pts',(148.942189373068,5.52026333669559,332.864712226803));
#10600=CARTESIAN_POINT('Ctrl Pts',(148.934791923864,5.46139908499283,332.71835604749));
#10601=CARTESIAN_POINT('Ctrl Pts',(148.92739447466,5.39678086526162,332.574574912547));
#10602=CARTESIAN_POINT('Ctrl Pts',(148.919997346196,5.33216544726379,332.430800011704));
#10603=CARTESIAN_POINT('Ctrl Pts',(148.912600217733,5.26179671027868,332.289600273648));
#10604=CARTESIAN_POINT('Ctrl Pts',(148.905203089269,5.18591772273406,332.151458630188));
#10605=CARTESIAN_POINT('Ctrl Pts',(148.897804821833,5.11002705171953,332.013295716363));
#10606=CARTESIAN_POINT('Ctrl Pts',(148.890406554396,5.02862462047629,331.87819216183));
#10607=CARTESIAN_POINT('Ctrl Pts',(148.883008286959,4.94199879988343,331.746605092453));
#10608=CARTESIAN_POINT('Ctrl Pts',(148.875607420434,4.8553425467288,331.614971795155));
#10609=CARTESIAN_POINT('Ctrl Pts',(148.868206553908,4.7634594557651,331.48685775418));
#10610=CARTESIAN_POINT('Ctrl Pts',(148.860805687382,4.66668034671686,331.362689853193));
#10611=CARTESIAN_POINT('Ctrl Pts',(148.853396693997,4.5697949649544,331.238385603979));
#10612=CARTESIAN_POINT('Ctrl Pts',(148.845987700613,4.46800305792502,331.118036443));
#10613=CARTESIAN_POINT('Ctrl Pts',(148.838578707228,4.36167521576677,331.002035533591));
#10614=CARTESIAN_POINT('Ctrl Pts',(148.831165149647,4.25528187199012,330.885963163621));
#10615=CARTESIAN_POINT('Ctrl Pts',(148.823751592067,4.14434728744243,330.77424464704));
#10616=CARTESIAN_POINT('Ctrl Pts',(148.816338034487,4.0292774112641,330.667234819936));
#10617=CARTESIAN_POINT('Ctrl Pts',(148.80891392235,3.91404371205071,330.560072644752));
#10618=CARTESIAN_POINT('Ctrl Pts',(148.801489810214,3.7946632454675,330.45763279002));
#10619=CARTESIAN_POINT('Ctrl Pts',(148.794065698077,3.67157401549325,330.360229013059));
#10620=CARTESIAN_POINT('Ctrl Pts',(148.790208572922,3.60762420487052,330.30962382939));
#10621=CARTESIAN_POINT('Ctrl Pts',(148.786351447768,3.54267378652824,330.260377274791));
#10622=CARTESIAN_POINT('Ctrl Pts',(148.782494322613,3.47678697453515,330.212528548785));
#10623=CARTESIAN_POINT('Ctrl Pts',(148.775070345175,3.34997174658619,330.120432013651));
#10624=CARTESIAN_POINT('Ctrl Pts',(148.767646367737,3.21930336986818,330.033238834829));
#10625=CARTESIAN_POINT('Ctrl Pts',(148.760222390299,3.08519785595913,329.951288802864));
#10626=CARTESIAN_POINT('Ctrl Pts',(148.752807174272,2.95125060673366,329.869435484267));
#10627=CARTESIAN_POINT('Ctrl Pts',(148.745391958244,2.81387460988558,329.792813188522));
#10628=CARTESIAN_POINT('Ctrl Pts',(148.737976742216,2.67351762719648,329.721720539838));
#10629=CARTESIAN_POINT('Ctrl Pts',(148.730568661072,2.53329569528947,329.650696296142));
#10630=CARTESIAN_POINT('Ctrl Pts',(148.723160579928,2.39009881848453,329.585191274698));
#10631=CARTESIAN_POINT('Ctrl Pts',(148.715752498784,2.24440223159955,329.525459911071));
#10632=CARTESIAN_POINT('Ctrl Pts',(148.70834993161,2.09881408934519,329.465773006589));
#10633=CARTESIAN_POINT('Ctrl Pts',(148.700947364436,1.95073028553513,329.411851344062));
#10634=CARTESIAN_POINT('Ctrl Pts',(148.693544797262,1.80064896278255,329.363902602391));
#10635=CARTESIAN_POINT('Ctrl Pts',(148.686146127507,1.6506466571902,329.315979105524));
#10636=CARTESIAN_POINT('Ctrl Pts',(148.678747457753,1.49864928176157,329.274022379917));
#10637=CARTESIAN_POINT('Ctrl Pts',(148.671348787998,1.34517308211892,329.238191261275));
#10638=CARTESIAN_POINT('Ctrl Pts',(148.663951338794,1.19172220128368,329.202366053656));
#10639=CARTESIAN_POINT('Ctrl Pts',(148.65655388959,1.03679334350103,329.172664532185));
#10640=CARTESIAN_POINT('Ctrl Pts',(148.649156440386,0.880916093202752,329.149195149449));
#10641=CARTESIAN_POINT('Ctrl Pts',(148.641759311922,0.725045601470463,329.125726784304));
#10642=CARTESIAN_POINT('Ctrl Pts',(148.634362183459,0.568227168035613,329.108490076185));
#10643=CARTESIAN_POINT('Ctrl Pts',(148.626965054995,0.410998438831725,329.097541965776));
#10644=CARTESIAN_POINT('Ctrl Pts',(148.619566787559,0.253745500328273,329.086592169631));
#10645=CARTESIAN_POINT('Ctrl Pts',(148.612168520122,0.0960825125978685,
329.08193292511));
#10646=CARTESIAN_POINT('Ctrl Pts',(148.604770252686,-0.0614500634389803,
329.083569112023));
#10647=CARTESIAN_POINT('Ctrl Pts',(148.59736938616,-0.219037982326384,329.085205873746));
#10648=CARTESIAN_POINT('Ctrl Pts',(148.589968519634,-0.376495025346606,
329.093142466423));
#10649=CARTESIAN_POINT('Ctrl Pts',(148.582567653108,-0.533283191382411,
329.107331707937));
#10650=CARTESIAN_POINT('Ctrl Pts',(148.575158659724,-0.690243525814229,
329.121536530594));
#10651=CARTESIAN_POINT('Ctrl Pts',(148.567749666339,-0.846533144530133,
329.14200768021));
#10652=CARTESIAN_POINT('Ctrl Pts',(148.560340672954,-1.00162088050476,329.168646282874));
#10653=CARTESIAN_POINT('Ctrl Pts',(148.552927115374,-1.15680415587419,329.195301295836));
#10654=CARTESIAN_POINT('Ctrl Pts',(148.545513557794,-1.31078370900066,329.228131254938));
#10655=CARTESIAN_POINT('Ctrl Pts',(148.538100000213,-1.46304146827509,329.266986811056));
#10656=CARTESIAN_POINT('Ctrl Pts',(148.530675888077,-1.61551599434436,329.305897685171));
#10657=CARTESIAN_POINT('Ctrl Pts',(148.52325177594,-1.7662634741643,329.350851182998));
#10658=CARTESIAN_POINT('Ctrl Pts',(148.515827663803,-1.9147830334263,329.401648769736));
#10659=CARTESIAN_POINT('Ctrl Pts',(148.511970538649,-1.99194492395807,329.42804016119));
#10660=CARTESIAN_POINT('Ctrl Pts',(148.508113413494,-2.06850580057166,329.456008217171));
#10661=CARTESIAN_POINT('Ctrl Pts',(148.504256288339,-2.14439794963443,329.485520151809));
#10662=CARTESIAN_POINT('Ctrl Pts',(148.496832310901,-2.29047088732067,329.542323062817));
#10663=CARTESIAN_POINT('Ctrl Pts',(148.489408333463,-2.43450564796971,329.605019656282));
#10664=CARTESIAN_POINT('Ctrl Pts',(148.481984356025,-2.5759913667248,329.673443979356));
#10665=CARTESIAN_POINT('Ctrl Pts',(148.474569139998,-2.71731011104409,329.741787551434));
#10666=CARTESIAN_POINT('Ctrl Pts',(148.46715392397,-2.85608546872859,329.815845237157));
#10667=CARTESIAN_POINT('Ctrl Pts',(148.459738707943,-2.99182401071739,329.895402106787));
#10668=CARTESIAN_POINT('Ctrl Pts',(148.452330626798,-3.12743194576445,329.974882427197));
#10669=CARTESIAN_POINT('Ctrl Pts',(148.444922545654,-3.26000856245942,330.059851210093));
#10670=CARTESIAN_POINT('Ctrl Pts',(148.43751446451,-3.38908272367766,330.150046510061));
#10671=CARTESIAN_POINT('Ctrl Pts',(148.430111897336,-3.51806081264043,330.240174676021));
#10672=CARTESIAN_POINT('Ctrl Pts',(148.422709330162,-3.64354133231631,330.335521400256));
#10673=CARTESIAN_POINT('Ctrl Pts',(148.415306762988,-3.76508006753448,330.435780170987));
#10674=CARTESIAN_POINT('Ctrl Pts',(148.407908093233,-3.88655481313961,330.535986155913));
#10675=CARTESIAN_POINT('Ctrl Pts',(148.400509423479,-4.00409162026188,330.64109879993));
#10676=CARTESIAN_POINT('Ctrl Pts',(148.393110753724,-4.11727755043953,330.750769936195));
#10677=CARTESIAN_POINT('Ctrl Pts',(148.38571330452,-4.2304448084536,330.860422980127));
#10678=CARTESIAN_POINT('Ctrl Pts',(148.378315855316,-4.33926234627553,330.974632764358));
#10679=CARTESIAN_POINT('Ctrl Pts',(148.370918406112,-4.44335237528694,331.093012639957));
#10680=CARTESIAN_POINT('Ctrl Pts',(148.363521277649,-4.54743789113605,331.211387382812));
#10681=CARTESIAN_POINT('Ctrl Pts',(148.356124149185,-4.64679605929418,331.333931577257));
#10682=CARTESIAN_POINT('Ctrl Pts',(148.348727020722,-4.74108804605963,331.460223919227));
#10683=CARTESIAN_POINT('Ctrl Pts',(148.341328753285,-4.83539455143715,331.586535707066));
#10684=CARTESIAN_POINT('Ctrl Pts',(148.333930485848,-4.92463309891664,331.716596492483));
#10685=CARTESIAN_POINT('Ctrl Pts',(148.326532218412,-5.00850711054575,331.849954431105));
#10686=CARTESIAN_POINT('Ctrl Pts',(148.319131351886,-5.09241058799718,331.983359219774));
#10687=CARTESIAN_POINT('Ctrl Pts',(148.31173048536,-5.1709455787568,332.120063152147));
#10688=CARTESIAN_POINT('Ctrl Pts',(148.304329618834,-5.24386061599907,332.259588278657));
#10689=CARTESIAN_POINT('Ctrl Pts',(148.29692062545,-5.31685572092326,332.399266617095));
#10690=CARTESIAN_POINT('Ctrl Pts',(148.289511632065,-5.38421837506148,332.541772005458));
#10691=CARTESIAN_POINT('Ctrl Pts',(148.28210263868,-5.44574427864021,332.686604267714));
#10692=CARTESIAN_POINT('Ctrl Pts',(148.2746890811,-5.50730808429778,332.83152575164));
#10693=CARTESIAN_POINT('Ctrl Pts',(148.26727552352,-5.56302784283388,332.978776617527));
#10694=CARTESIAN_POINT('Ctrl Pts',(148.259861965939,-5.61274878683966,333.127840386524));
#10695=CARTESIAN_POINT('Ctrl Pts',(148.252437853803,-5.66254051771185,333.277116375086));
#10696=CARTESIAN_POINT('Ctrl Pts',(148.245013741666,-5.70631627356744,333.428210064029));
#10697=CARTESIAN_POINT('Ctrl Pts',(148.237589629529,-5.7439719547281,333.580592818886));
#10698=CARTESIAN_POINT('Ctrl Pts',(148.233732504375,-5.763535597134,333.659761795067));
#10699=CARTESIAN_POINT('Ctrl Pts',(148.22987537922,-5.78144814558562,333.739278589465));
#10700=CARTESIAN_POINT('Ctrl Pts',(148.226018254065,-5.79770052668763,333.819068517929));
#10701=CARTESIAN_POINT('Ctrl Pts',(148.215400427831,-5.84243979531541,334.038712828564));
#10702=CARTESIAN_POINT('Ctrl Pts',(148.204782601597,-5.87470894321651,334.260975959509));
#10703=CARTESIAN_POINT('Ctrl Pts',(148.194164775363,-5.8942673528667,334.484691417275));
#10704=CARTESIAN_POINT('Ctrl Pts',(148.186127185143,-5.90907287695997,334.654041822509));
#10705=CARTESIAN_POINT('Ctrl Pts',(148.178089594923,-5.91659554481408,334.82422426963));
#10706=CARTESIAN_POINT('Ctrl Pts',(148.170052004703,-5.91674764559936,334.994721667458));
#10707=CARTESIAN_POINT('',(146.420052004731,-5.91674999222498,334.999696675565));
#10708=CARTESIAN_POINT('Ctrl Pts',(148.170052004658,-5.91674764560021,334.994721668406));
#10709=CARTESIAN_POINT('Ctrl Pts',(148.162748410747,-5.91688585644941,335.149649168135));
#10710=CARTESIAN_POINT('Ctrl Pts',(148.155444816836,-5.9109348501119,335.304773595374));
#10711=CARTESIAN_POINT('Ctrl Pts',(148.148141222925,-5.89887502142363,335.45956941165));
#10712=CARTESIAN_POINT('Ctrl Pts',(148.140843472054,-5.88682484087063,335.614241387778));
#10713=CARTESIAN_POINT('Ctrl Pts',(148.133545721183,-5.86867559334,335.768584894349));
#10714=CARTESIAN_POINT('Ctrl Pts',(148.126247970312,-5.84445973527854,335.922074273152));
#10715=CARTESIAN_POINT('Ctrl Pts',(148.118811814041,-5.81978461167114,336.078474652802));
#10716=CARTESIAN_POINT('Ctrl Pts',(148.111375657769,-5.78881043696119,336.233987774095));
#10717=CARTESIAN_POINT('Ctrl Pts',(148.103939501497,-5.75162705930377,336.388062222375));
#10718=CARTESIAN_POINT('Ctrl Pts',(148.096647403661,-5.71516402412085,336.539151832366));
#10719=CARTESIAN_POINT('Ctrl Pts',(148.089355305825,-5.67273027635409,336.688857615709));
#10720=CARTESIAN_POINT('Ctrl Pts',(148.082063207988,-5.62446214253966,336.83666985864));
#10721=CARTESIAN_POINT('Ctrl Pts',(148.074771469774,-5.57619638915013,336.98447481196));
#10722=CARTESIAN_POINT('Ctrl Pts',(148.06747973156,-5.52209694138336,337.130386044619));
#10723=CARTESIAN_POINT('Ctrl Pts',(148.060187993346,-5.46234978476907,337.27390971486));
#10724=CARTESIAN_POINT('Ctrl Pts',(148.052895079054,-5.40259299158463,337.417456533916));
#10725=CARTESIAN_POINT('Ctrl Pts',(148.045602164761,-5.3371868253239,337.558614669072));
#10726=CARTESIAN_POINT('Ctrl Pts',(148.038309250468,-5.2663650035639,337.69691123542));
#10727=CARTESIAN_POINT('Ctrl Pts',(148.030765164579,-5.19310404302206,337.839970804329));
#10728=CARTESIAN_POINT('Ctrl Pts',(148.023221078689,-5.11404791220634,337.97996776799));
#10729=CARTESIAN_POINT('Ctrl Pts',(148.015676992799,-5.02950589739266,338.116408347857));
#10730=CARTESIAN_POINT('Ctrl Pts',(148.008373354424,-4.94765843267006,338.248500249996));
#10731=CARTESIAN_POINT('Ctrl Pts',(148.001069716048,-4.86066969174803,338.37725871238));
#10732=CARTESIAN_POINT('Ctrl Pts',(147.993766077673,-4.76886283938269,338.502267520001));
#10733=CARTESIAN_POINT('Ctrl Pts',(147.986101768026,-4.67252234330752,338.63344956393));
#10734=CARTESIAN_POINT('Ctrl Pts',(147.978437458379,-4.57087609919874,338.760501823122));
#10735=CARTESIAN_POINT('Ctrl Pts',(147.970773148732,-4.46434240320478,338.882985638584));
#10736=CARTESIAN_POINT('Ctrl Pts',(147.963108839085,-4.35780870721077,339.005469454045));
#10737=CARTESIAN_POINT('Ctrl Pts',(147.955444529438,-4.24638794587433,339.123384529299));
#10738=CARTESIAN_POINT('Ctrl Pts',(147.947780219791,-4.13053890431873,339.236340274625));
#10739=CARTESIAN_POINT('Ctrl Pts',(147.940356242353,-4.01832257821205,339.345754030517));
#10740=CARTESIAN_POINT('Ctrl Pts',(147.932932264915,-3.90158657809671,339.450871019555));
#10741=CARTESIAN_POINT('Ctrl Pts',(147.925508287477,-3.78069359453069,339.551295036226));
#10742=CARTESIAN_POINT('Ctrl Pts',(147.91809307145,-3.65994328287461,339.651600537447));
#10743=CARTESIAN_POINT('Ctrl Pts',(147.910677855422,-3.53504603726267,339.747223854446));
#10744=CARTESIAN_POINT('Ctrl Pts',(147.903262639394,-3.40640190055357,339.837804941748));
#10745=CARTESIAN_POINT('Ctrl Pts',(147.89585455825,-3.27788154458527,339.928298872385));
#10746=CARTESIAN_POINT('Ctrl Pts',(147.888446477106,-3.1456217779952,340.013760018542));
#10747=CARTESIAN_POINT('Ctrl Pts',(147.881038395962,-3.01005619906946,340.093868102036));
#10748=CARTESIAN_POINT('Ctrl Pts',(147.873635828788,-2.8745915240796,340.173916559621));
#10749=CARTESIAN_POINT('Ctrl Pts',(147.866233261614,-2.73582625605024,340.248619698975));
#10750=CARTESIAN_POINT('Ctrl Pts',(147.85883069444,-2.59422340127637,340.317700208433));
#10751=CARTESIAN_POINT('Ctrl Pts',(147.851432024685,-2.45269509978787,340.386744347304));
#10752=CARTESIAN_POINT('Ctrl Pts',(147.844033354931,-2.30833252147898,340.450171588648));
#10753=CARTESIAN_POINT('Ctrl Pts',(147.836634685176,-2.16162362679046,340.507750344615));
#10754=CARTESIAN_POINT('Ctrl Pts',(147.829237235972,-2.01493893451307,340.565319601875));
#10755=CARTESIAN_POINT('Ctrl Pts',(147.821839786768,-1.86590904113859,340.617042152395));
#10756=CARTESIAN_POINT('Ctrl Pts',(147.814442337564,-1.71504236876553,340.662734342686));
#10757=CARTESIAN_POINT('Ctrl Pts',(147.807045209101,-1.56418223770847,340.708424551844));
#10758=CARTESIAN_POINT('Ctrl Pts',(147.799648080637,-1.41148584319119,340.748084812473));
#10759=CARTESIAN_POINT('Ctrl Pts',(147.792250952174,-1.25747700947135,340.781581283105));
#10760=CARTESIAN_POINT('Ctrl Pts',(147.784852684737,-1.10344446223524,340.815082911358));
#10761=CARTESIAN_POINT('Ctrl Pts',(147.7774544173,-0.948099438130381,340.842418780568));
#10762=CARTESIAN_POINT('Ctrl Pts',(147.770056149864,-0.791976050973206,
340.863506160753));
#10763=CARTESIAN_POINT('Ctrl Pts',(147.762655283338,-0.635797816028739,
340.884600949155));
#10764=CARTESIAN_POINT('Ctrl Pts',(147.755254416812,-0.478841043219018,
340.899442828048));
#10765=CARTESIAN_POINT('Ctrl Pts',(147.747853550287,-0.321644916362601,
340.908000940274));
#10766=CARTESIAN_POINT('Ctrl Pts',(147.740444556902,-0.164276173130186,
340.916568450125));
#10767=CARTESIAN_POINT('Ctrl Pts',(147.733035563517,-0.00666792383998877,
340.918838392987));
#10768=CARTESIAN_POINT('Ctrl Pts',(147.725626570132,0.150639959648062,340.914832048762));
#10769=CARTESIAN_POINT('Ctrl Pts',(147.718213012552,0.308044750218301,340.91082323649));
#10770=CARTESIAN_POINT('Ctrl Pts',(147.710799454972,0.465148434735534,340.900530457142));
#10771=CARTESIAN_POINT('Ctrl Pts',(147.703385897392,0.621416824595331,340.884026826299));
#10772=CARTESIAN_POINT('Ctrl Pts',(147.695961785255,0.777907691116904,340.867499699516));
#10773=CARTESIAN_POINT('Ctrl Pts',(147.688537673118,0.933560519631203,340.84474411527));
#10774=CARTESIAN_POINT('Ctrl Pts',(147.681113560982,1.08785104971144,340.81588433999));
#10775=CARTESIAN_POINT('Ctrl Pts',(147.677256435827,1.16801119192923,340.800890524818));
#10776=CARTESIAN_POINT('Ctrl Pts',(147.673399310672,1.24780385406735,340.784249880222));
#10777=CARTESIAN_POINT('Ctrl Pts',(147.669542185517,1.32715730388919,340.765985089578));
#10778=CARTESIAN_POINT('Ctrl Pts',(147.662118208079,1.47989235848651,340.730830048398));
#10779=CARTESIAN_POINT('Ctrl Pts',(147.654694230641,1.63146002511382,340.689549089827));
#10780=CARTESIAN_POINT('Ctrl Pts',(147.647270253203,1.7813308534301,340.642232798557));
#10781=CARTESIAN_POINT('Ctrl Pts',(147.639855037176,1.93102481161985,340.59497234763));
#10782=CARTESIAN_POINT('Ctrl Pts',(147.632439821148,2.0790255651209,340.541690852922));
#10783=CARTESIAN_POINT('Ctrl Pts',(147.625024605121,2.22481385786861,340.482529877742));
#10784=CARTESIAN_POINT('Ctrl Pts',(147.617616523976,2.37046187385489,340.423425826955));
#10785=CARTESIAN_POINT('Ctrl Pts',(147.610208442832,2.51390132365814,340.358453697536));
#10786=CARTESIAN_POINT('Ctrl Pts',(147.602800361688,2.65462823360733,340.287804790632));
#10787=CARTESIAN_POINT('Ctrl Pts',(147.595397794514,2.79525039794722,340.217208469));
#10788=CARTESIAN_POINT('Ctrl Pts',(147.58799522734,2.93316371043148,340.140943949857));
#10789=CARTESIAN_POINT('Ctrl Pts',(147.580592660166,3.06788441449027,340.05925051582));
#10790=CARTESIAN_POINT('Ctrl Pts',(147.573193990412,3.20253418868727,339.977600093019));
#10791=CARTESIAN_POINT('Ctrl Pts',(147.565795320657,3.3339943837407,339.890526640824));
#10792=CARTESIAN_POINT('Ctrl Pts',(147.558396650902,3.46180618909339,339.798315170104));
#10793=CARTESIAN_POINT('Ctrl Pts',(147.550999201698,3.58959690946702,339.706118911415));
#10794=CARTESIAN_POINT('Ctrl Pts',(147.543601752494,3.71374013229002,339.608786534589));
#10795=CARTESIAN_POINT('Ctrl Pts',(147.53620430329,3.83380628305483,339.506646197175));
#10796=CARTESIAN_POINT('Ctrl Pts',(147.528807174827,3.95386722796063,339.404510288388));
#10797=CARTESIAN_POINT('Ctrl Pts',(147.521410046363,4.0698511680286,339.297567075335));
#10798=CARTESIAN_POINT('Ctrl Pts',(147.5140129179,4.18136208175002,339.186184623712));
#10799=CARTESIAN_POINT('Ctrl Pts',(147.506614650463,4.29289016536814,339.074785021972));
#10800=CARTESIAN_POINT('Ctrl Pts',(147.499216383027,4.39994358721055,338.958945084424));
#10801=CARTESIAN_POINT('Ctrl Pts',(147.49181811559,4.50216373823538,338.839069188829));
#10802=CARTESIAN_POINT('Ctrl Pts',(147.484417249064,4.6044198002745,338.719151179571));
#10803=CARTESIAN_POINT('Ctrl Pts',(147.477016382539,4.70183896881829,338.595194673086));
#10804=CARTESIAN_POINT('Ctrl Pts',(147.469615516013,4.7941035121219,338.46763638197));
#10805=CARTESIAN_POINT('Ctrl Pts',(147.462206522628,4.88646937071502,338.339938019655));
#10806=CARTESIAN_POINT('Ctrl Pts',(147.454797529243,4.97366908134501,338.208630276734));
#10807=CARTESIAN_POINT('Ctrl Pts',(147.447388535859,5.05542838309439,338.074178658748));
#10808=CARTESIAN_POINT('Ctrl Pts',(147.439974978278,5.13723805139403,337.939644213928));
#10809=CARTESIAN_POINT('Ctrl Pts',(147.432561420698,5.21360045195357,337.801962360452));
#10810=CARTESIAN_POINT('Ctrl Pts',(147.425147863118,5.28428798911991,337.661621875951));
#10811=CARTESIAN_POINT('Ctrl Pts',(147.417723750981,5.35507616293637,337.521081591078));
#10812=CARTESIAN_POINT('Ctrl Pts',(147.410299638844,5.42017318354134,337.377875454523));
#10813=CARTESIAN_POINT('Ctrl Pts',(147.402875526708,5.47939984182708,337.232511575756));
#10814=CARTESIAN_POINT('Ctrl Pts',(147.399018401553,5.51017047531185,337.156989188289));
#10815=CARTESIAN_POINT('Ctrl Pts',(147.395161276398,5.53935739024372,337.080884628764));
#10816=CARTESIAN_POINT('Ctrl Pts',(147.391304151243,5.56694084312725,337.004270493626));
#10817=CARTESIAN_POINT('Ctrl Pts',(147.383880173805,5.62003192097725,336.856807917777));
#10818=CARTESIAN_POINT('Ctrl Pts',(147.376456196367,5.667339843588,336.707011937972));
#10819=CARTESIAN_POINT('Ctrl Pts',(147.369032218929,5.70865426959873,336.555376800872));
#10820=CARTESIAN_POINT('Ctrl Pts',(147.361617002902,5.74991993837071,336.403920616049));
#10821=CARTESIAN_POINT('Ctrl Pts',(147.354201786874,5.78520609276058,336.250629950894));
#10822=CARTESIAN_POINT('Ctrl Pts',(147.346786570846,5.81435077712405,336.096018066939));
#10823=CARTESIAN_POINT('Ctrl Pts',(147.339378489702,5.843467418619,335.941554949761));
#10824=CARTESIAN_POINT('Ctrl Pts',(147.331970408558,5.86645428571385,335.785773508945));
#10825=CARTESIAN_POINT('Ctrl Pts',(147.324562327414,5.88319951855191,335.629201070732));
#10826=CARTESIAN_POINT('Ctrl Pts',(147.31715976024,5.89993228760728,335.472745172245));
#10827=CARTESIAN_POINT('Ctrl Pts',(147.309757193066,5.91043263327722,335.31549981816));
#10828=CARTESIAN_POINT('Ctrl Pts',(147.302354625892,5.91463998498093,335.15800129925));
#10829=CARTESIAN_POINT('Ctrl Pts',(147.294955956137,5.91884512153238,335.000585702622));
#10830=CARTESIAN_POINT('Ctrl Pts',(147.287557286382,5.91676385267814,334.842917578764));
#10831=CARTESIAN_POINT('Ctrl Pts',(147.280158616628,5.90838756142093,334.685536986998));
#10832=CARTESIAN_POINT('Ctrl Pts',(147.272761167424,5.90001265199168,334.528182358142));
#10833=CARTESIAN_POINT('Ctrl Pts',(147.26536371822,5.88534480102928,334.371115539559));
#10834=CARTESIAN_POINT('Ctrl Pts',(147.257966269016,5.8644274958022,334.214875354495));
#10835=CARTESIAN_POINT('Ctrl Pts',(147.250569140552,5.84351109751306,334.058641943734));
#10836=CARTESIAN_POINT('Ctrl Pts',(147.243172012089,5.81634583325121,333.903235465139));
#10837=CARTESIAN_POINT('Ctrl Pts',(147.235774883625,5.78302690735014,333.749188123112));
#10838=CARTESIAN_POINT('Ctrl Pts',(147.228376616189,5.74970285116603,333.595117061639));
#10839=CARTESIAN_POINT('Ctrl Pts',(147.220978348752,5.71022332562729,333.442405918224));
#10840=CARTESIAN_POINT('Ctrl Pts',(147.213580081315,5.6647343166913,333.291575086871));
#10841=CARTESIAN_POINT('Ctrl Pts',(147.206179214789,5.61922932698793,333.14069126706));
#10842=CARTESIAN_POINT('Ctrl Pts',(147.198778348264,5.56771075819675,332.991689431601));
#10843=CARTESIAN_POINT('Ctrl Pts',(147.191377481738,5.51037390837914,332.845073098141));
#10844=CARTESIAN_POINT('Ctrl Pts',(147.183968488353,5.45297409721925,332.698295765932));
#10845=CARTESIAN_POINT('Ctrl Pts',(147.176559494968,5.38974338180881,332.553909514807));
#10846=CARTESIAN_POINT('Ctrl Pts',(147.169150501583,5.32092479736872,332.412396888384));
#10847=CARTESIAN_POINT('Ctrl Pts',(147.161736944003,5.25206381830673,332.270797085301));
#10848=CARTESIAN_POINT('Ctrl Pts',(147.154323386423,5.17760828702107,332.132074762451));
#10849=CARTESIAN_POINT('Ctrl Pts',(147.146909828843,5.09784606198155,331.996685815497));
#10850=CARTESIAN_POINT('Ctrl Pts',(147.139485716706,5.01797028081234,331.86110411759));
#10851=CARTESIAN_POINT('Ctrl Pts',(147.132061604569,4.93277291852831,331.728865586523));
#10852=CARTESIAN_POINT('Ctrl Pts',(147.124637492433,4.84258427489381,331.600395890247));
#10853=CARTESIAN_POINT('Ctrl Pts',(147.120780367278,4.79572764347448,331.533650710761));
#10854=CARTESIAN_POINT('Ctrl Pts',(147.116923242124,4.74752441016964,331.467922267288));
#10855=CARTESIAN_POINT('Ctrl Pts',(147.113066116969,4.69802493853934,331.403266448656));
#10856=CARTESIAN_POINT('Ctrl Pts',(147.105642139531,4.60275114112179,331.278820567451));
#10857=CARTESIAN_POINT('Ctrl Pts',(147.098218162093,4.50238553739962,331.157975126094));
#10858=CARTESIAN_POINT('Ctrl Pts',(147.090794184655,4.39722992215444,331.04117447035));
#10859=CARTESIAN_POINT('Ctrl Pts',(147.083378968628,4.29219840635662,330.924511656953));
#10860=CARTESIAN_POINT('Ctrl Pts',(147.0759637526,4.18238837857425,330.811884402198));
#10861=CARTESIAN_POINT('Ctrl Pts',(147.068548536572,4.06814380788774,330.703706653306));
#10862=CARTESIAN_POINT('Ctrl Pts',(147.061140455428,3.95400916275233,330.5956329925));
#10863=CARTESIAN_POINT('Ctrl Pts',(147.053732374284,3.83544873849147,330.492000569195));
#10864=CARTESIAN_POINT('Ctrl Pts',(147.04632429314,3.71284544120223,330.393188815217));
#10865=CARTESIAN_POINT('Ctrl Pts',(147.038921725966,3.590333399786,330.294450608631));
#10866=CARTESIAN_POINT('Ctrl Pts',(147.031519158792,3.46378476640493,330.20052616011));
#10867=CARTESIAN_POINT('Ctrl Pts',(147.024116591618,3.33361774119527,330.111756622458));
#10868=CARTESIAN_POINT('Ctrl Pts',(147.016717921863,3.20351924835548,330.023033821579));
#10869=CARTESIAN_POINT('Ctrl Pts',(147.009319252109,3.06980646530157,329.939460736146));
#10870=CARTESIAN_POINT('Ctrl Pts',(147.001920582354,2.93292887628733,329.861336869463));
#10871=CARTESIAN_POINT('Ctrl Pts',(146.99452313315,2.79607386782491,329.783225890793));
#10872=CARTESIAN_POINT('Ctrl Pts',(146.987125683946,2.65605541340817,329.710562531564));
#10873=CARTESIAN_POINT('Ctrl Pts',(146.979728234742,2.5133501544572,329.643601810583));
#10874=CARTESIAN_POINT('Ctrl Pts',(146.972331106278,2.37065108295752,329.576643992902));
#10875=CARTESIAN_POINT('Ctrl Pts',(146.964933977815,2.22526577642031,329.515388480375));
#10876=CARTESIAN_POINT('Ctrl Pts',(146.957536849351,2.07769329740963,329.460043219988));
#10877=CARTESIAN_POINT('Ctrl Pts',(146.950138581915,1.93009809592073,329.404689437813));
#10878=CARTESIAN_POINT('Ctrl Pts',(146.942740314478,1.78031540087056,329.355247850831));
#10879=CARTESIAN_POINT('Ctrl Pts',(146.935342047042,1.62886182405741,329.311877311395));
#10880=CARTESIAN_POINT('Ctrl Pts',(146.927941180516,1.47735504001039,329.268491535431));
#10881=CARTESIAN_POINT('Ctrl Pts',(146.92054031399,1.3241765640518,329.231181156138));
#10882=CARTESIAN_POINT('Ctrl Pts',(146.913139447464,1.16985550190098,329.200054425499));
#10883=CARTESIAN_POINT('Ctrl Pts',(146.90573045408,1.01536498047001,329.168893514734));
#10884=CARTESIAN_POINT('Ctrl Pts',(146.898321460695,0.859729733267863,329.143929886926));
#10885=CARTESIAN_POINT('Ctrl Pts',(146.89091246731,0.703487061818735,329.125220300611));
#10886=CARTESIAN_POINT('Ctrl Pts',(146.88349890973,0.54714813949461,329.106499188545));
#10887=CARTESIAN_POINT('Ctrl Pts',(146.87608535215,0.390201418463485,329.094039824463));
#10888=CARTESIAN_POINT('Ctrl Pts',(146.868671794569,0.233186047849093,329.087846853338));
#10889=CARTESIAN_POINT('Ctrl Pts',(146.861247682433,0.0759471371091804,
329.081645065384));
#10890=CARTESIAN_POINT('Ctrl Pts',(146.853823570296,-0.081360246206188,
329.081727487929));
#10891=CARTESIAN_POINT('Ctrl Pts',(146.846399458159,-0.238199404679093,
329.088046718206));
#10892=CARTESIAN_POINT('Ctrl Pts',(146.842542333005,-0.31968366195242,329.091329812752));
#10893=CARTESIAN_POINT('Ctrl Pts',(146.83868520785,-0.401041647769633,329.096295507749));
#10894=CARTESIAN_POINT('Ctrl Pts',(146.834828082695,-0.482199109410888,
329.102931696056));
#10895=CARTESIAN_POINT('Ctrl Pts',(146.827404105257,-0.638406424444336,
329.115704657858));
#10896=CARTESIAN_POINT('Ctrl Pts',(146.819980127819,-0.794341521357021,
329.134707832806));
#10897=CARTESIAN_POINT('Ctrl Pts',(146.812556150381,-0.94946742184152,329.159927896219));
#10898=CARTESIAN_POINT('Ctrl Pts',(146.805140934354,-1.10441025042355,329.185118196163));
#10899=CARTESIAN_POINT('Ctrl Pts',(146.797725718326,-1.25854541867509,329.21651072112));
#10900=CARTESIAN_POINT('Ctrl Pts',(146.790310502299,-1.41133868813917,329.254040230748));
#10901=CARTESIAN_POINT('Ctrl Pts',(146.782902421154,-1.56398494068897,329.291533629671));
#10902=CARTESIAN_POINT('Ctrl Pts',(146.77549434001,-1.71529150491061,329.33515216913));
#10903=CARTESIAN_POINT('Ctrl Pts',(146.768086258866,-1.86473209602684,329.384779187552));
#10904=CARTESIAN_POINT('Ctrl Pts',(146.760683691692,-2.01406145578125,329.434369267678));
#10905=CARTESIAN_POINT('Ctrl Pts',(146.753281124518,-2.1615272552138,329.489958804806));
#10906=CARTESIAN_POINT('Ctrl Pts',(146.745878557344,-2.30661629956362,329.551380742877));
#10907=CARTESIAN_POINT('Ctrl Pts',(146.73847988759,-2.45162895516745,329.612770342568));
#10908=CARTESIAN_POINT('Ctrl Pts',(146.731081217835,-2.59426700501119,329.679986082525));
#10909=CARTESIAN_POINT('Ctrl Pts',(146.72368254808,-2.73403534865528,329.752812060274));
#10910=CARTESIAN_POINT('Ctrl Pts',(146.716285098876,-2.87378063486127,329.825626023998));
#10911=CARTESIAN_POINT('Ctrl Pts',(146.708887649672,-3.0106568237829,329.904048216378));
#10912=CARTESIAN_POINT('Ctrl Pts',(146.701490200468,-3.14419152664447,329.987815824785));
#10913=CARTESIAN_POINT('Ctrl Pts',(146.694093072005,-3.27772043967407,330.071579801174));
#10914=CARTESIAN_POINT('Ctrl Pts',(146.686695943541,-3.40790783856087,330.160688534431));
#10915=CARTESIAN_POINT('Ctrl Pts',(146.679298815078,-3.5343087848591,330.254834884246));
#10916=CARTESIAN_POINT('Ctrl Pts',(146.671900547641,-3.66072919374794,330.348995730249));
#10917=CARTESIAN_POINT('Ctrl Pts',(146.664502280204,-3.78336168985092,330.448195514316));
#10918=CARTESIAN_POINT('Ctrl Pts',(146.657104012768,-3.90179312255097,330.552085770688));
#10919=CARTESIAN_POINT('Ctrl Pts',(146.649703146242,-4.02026616145841,330.656012524799));
#10920=CARTESIAN_POINT('Ctrl Pts',(146.642302279716,-4.13453491810818,330.764632786047));
#10921=CARTESIAN_POINT('Ctrl Pts',(146.634901413191,-4.24422203163209,330.877560199505));
#10922=CARTESIAN_POINT('Ctrl Pts',(146.627492419806,-4.35402959209327,330.990611618058));
#10923=CARTESIAN_POINT('Ctrl Pts',(146.620083426421,-4.45924520190224,331.107979366343));
#10924=CARTESIAN_POINT('Ctrl Pts',(146.612674433037,-4.55953036690967,331.229242331344));
#10925=CARTESIAN_POINT('Ctrl Pts',(146.605260875456,-4.65987731103766,331.350579998514));
#10926=CARTESIAN_POINT('Ctrl Pts',(146.597847317876,-4.75528753245377,331.475817367716));
#10927=CARTESIAN_POINT('Ctrl Pts',(146.590433760296,-4.84546536057333,331.604503570612));
#10928=CARTESIAN_POINT('Ctrl Pts',(146.583009648159,-4.93577157334081,331.733372981878));
#10929=CARTESIAN_POINT('Ctrl Pts',(146.575585536023,-5.02083031387259,331.865700720081));
#10930=CARTESIAN_POINT('Ctrl Pts',(146.568161423886,-5.10039100639596,332.001009812558));
#10931=CARTESIAN_POINT('Ctrl Pts',(146.564304298731,-5.14172598932963,332.071308333736));
#10932=CARTESIAN_POINT('Ctrl Pts',(146.560447173576,-5.18157770491679,332.142411222204));
#10933=CARTESIAN_POINT('Ctrl Pts',(146.556590048422,-5.21991615190281,332.214249485398));
#10934=CARTESIAN_POINT('Ctrl Pts',(146.548750793122,-5.2978355508435,332.360254207266));
#10935=CARTESIAN_POINT('Ctrl Pts',(146.540911537823,-5.36971495926341,332.509698015299));
#10936=CARTESIAN_POINT('Ctrl Pts',(146.533072282524,-5.43525564688561,332.6620678762));
#10937=CARTESIAN_POINT('Ctrl Pts',(146.525246388352,-5.50068462779268,332.814178039846));
#10938=CARTESIAN_POINT('Ctrl Pts',(146.517420494179,-5.55979630146954,332.96920403031));
#10939=CARTESIAN_POINT('Ctrl Pts',(146.509594600007,-5.61233759419056,333.126608078555));
#10940=CARTESIAN_POINT('Ctrl Pts',(146.501787024606,-5.66475589880413,333.283643677054));
#10941=CARTESIAN_POINT('Ctrl Pts',(146.493979449205,-5.71063440139223,333.443045935796));
#10942=CARTESIAN_POINT('Ctrl Pts',(146.486171873804,-5.74976815257897,333.60425763334));
#10943=CARTESIAN_POINT('Ctrl Pts',(146.478375127486,-5.78884762537151,333.76524573075));
#10944=CARTESIAN_POINT('Ctrl Pts',(146.470578381168,-5.82120091784066,333.928037964224));
#10945=CARTESIAN_POINT('Ctrl Pts',(146.462781634851,-5.84667224702013,334.092060465436));
#10946=CARTESIAN_POINT('Ctrl Pts',(146.454999902127,-5.87209452802309,334.255767121152));
#10947=CARTESIAN_POINT('Ctrl Pts',(146.447218169403,-5.89066123051592,334.420699012688));
#10948=CARTESIAN_POINT('Ctrl Pts',(146.439436436679,-5.90226727024812,334.586271063306));
#10949=CARTESIAN_POINT('Ctrl Pts',(146.432974959363,-5.91190421938478,334.72375201866));
#10950=CARTESIAN_POINT('Ctrl Pts',(146.426513482047,-5.91674291643995,334.861673996697));
#10951=CARTESIAN_POINT('Ctrl Pts',(146.420052004731,-5.91674999222498,334.999696675565));
#10952=CARTESIAN_POINT('',(144.670052004703,-5.91674753464347,335.005401276743));
#10953=CARTESIAN_POINT('Ctrl Pts',(146.420052004703,-5.91674999222501,334.999696676165));
#10954=CARTESIAN_POINT('Ctrl Pts',(146.412332577533,-5.91675844553942,335.164590239239));
#10955=CARTESIAN_POINT('Ctrl Pts',(146.404613150363,-5.90986946465992,335.329362352071));
#10956=CARTESIAN_POINT('Ctrl Pts',(146.396893723193,-5.89613935317849,335.493428100537));
#10957=CARTESIAN_POINT('Ctrl Pts',(146.389165601203,-5.88239377670883,335.657678645382));
#10958=CARTESIAN_POINT('Ctrl Pts',(146.381437479213,-5.86179171970293,335.821220916174));
#10959=CARTESIAN_POINT('Ctrl Pts',(146.373709357223,-5.83444099740712,335.983477915499));
#10960=CARTESIAN_POINT('Ctrl Pts',(146.365762911967,-5.80631760368707,336.150318755259));
#10961=CARTESIAN_POINT('Ctrl Pts',(146.357816466711,-5.77105872154076,336.315800268683));
#10962=CARTESIAN_POINT('Ctrl Pts',(146.349870021454,-5.72883659731168,336.479311259946));
#10963=CARTESIAN_POINT('Ctrl Pts',(146.342116297545,-5.68763846612262,336.638856697128));
#10964=CARTESIAN_POINT('Ctrl Pts',(146.334362573635,-5.63981109997439,336.796525808012));
#10965=CARTESIAN_POINT('Ctrl Pts',(146.326608849725,-5.58556378549572,336.951770416995));
#10966=CARTESIAN_POINT('Ctrl Pts',(146.318566043796,-5.5292939688721,337.11280300936));
#10967=CARTESIAN_POINT('Ctrl Pts',(146.310523237866,-5.46611644690042,337.271226466518));
#10968=CARTESIAN_POINT('Ctrl Pts',(146.302480431937,-5.39631743291392,337.426456001194));
#10969=CARTESIAN_POINT('Ctrl Pts',(146.294437626007,-5.32651841892745,337.581685535869));
#10970=CARTESIAN_POINT('Ctrl Pts',(146.286394820077,-5.2500981463478,337.733720838905));
#10971=CARTESIAN_POINT('Ctrl Pts',(146.278352014148,-5.16739318762945,337.882009404381));
#10972=CARTESIAN_POINT('Ctrl Pts',(146.27092803671,-5.09105170271556,338.018888371007));
#10973=CARTESIAN_POINT('Ctrl Pts',(146.263504059272,-5.00915262107096,338.15293841962));
#10974=CARTESIAN_POINT('Ctrl Pts',(146.256080081834,-4.92193053874683,338.283676344321));
#10975=CARTESIAN_POINT('Ctrl Pts',(146.248664865806,-4.83481139160302,338.414259978599));
#10976=CARTESIAN_POINT('Ctrl Pts',(146.241249649779,-4.74238195319509,338.541538962061));
#10977=CARTESIAN_POINT('Ctrl Pts',(146.233834433751,-4.64492293506497,338.66505409098));
#10978=CARTESIAN_POINT('Ctrl Pts',(146.226426352607,-4.54755769151149,338.788450374263));
#10979=CARTESIAN_POINT('Ctrl Pts',(146.219018271463,-4.44517273228715,338.908089721829));
#10980=CARTESIAN_POINT('Ctrl Pts',(146.211610190318,-4.33809227434411,339.023541472605));
#10981=CARTESIAN_POINT('Ctrl Pts',(146.204207623144,-4.23109151834172,339.138907290536));
#10982=CARTESIAN_POINT('Ctrl Pts',(146.19680505597,-4.11940247527218,339.250091445427));
#10983=CARTESIAN_POINT('Ctrl Pts',(146.189402488796,-4.0033898050446,339.35669606828));
#10984=CARTESIAN_POINT('Ctrl Pts',(146.182003819042,-3.88743821498054,339.463244564265));
#10985=CARTESIAN_POINT('Ctrl Pts',(146.174605149287,-3.76716780540146,339.565218078183));
#10986=CARTESIAN_POINT('Ctrl Pts',(146.167206479532,-3.64298019694015,339.662255446369));
#10987=CARTESIAN_POINT('Ctrl Pts',(146.159809030328,-3.51881307557818,339.759276806403));
#10988=CARTESIAN_POINT('Ctrl Pts',(146.152411581124,-3.39073033165982,339.851363407286));
#10989=CARTESIAN_POINT('Ctrl Pts',(146.14501413192,-3.25916687131794,339.938194190937));
#10990=CARTESIAN_POINT('Ctrl Pts',(146.137617003456,-3.12760911533824,340.025021209757));
#10991=CARTESIAN_POINT('Ctrl Pts',(146.130219874993,-2.99257125449617,340.106592658875));
#10992=CARTESIAN_POINT('Ctrl Pts',(146.122822746529,-2.85451716679003,340.182630828739));
#10993=CARTESIAN_POINT('Ctrl Pts',(146.115424479093,-2.71644182220059,340.258680706584));
#10994=CARTESIAN_POINT('Ctrl Pts',(146.108026211656,-2.57534965294356,340.329195428693));
#10995=CARTESIAN_POINT('Ctrl Pts',(146.100627944219,-2.43172897941287,340.393943337966));
#10996=CARTESIAN_POINT('Ctrl Pts',(146.093227077694,-2.28805785043014,340.458713993859));
#10997=CARTESIAN_POINT('Ctrl Pts',(146.085826211168,-2.14185678860945,340.51771364998));
#10998=CARTESIAN_POINT('Ctrl Pts',(146.078425344642,-1.99363377125032,340.570758920347));
#10999=CARTESIAN_POINT('Ctrl Pts',(146.071016351257,-1.84524799084639,340.623862439494));
#11000=CARTESIAN_POINT('Ctrl Pts',(146.063607357873,-1.69483617244212,340.670998389356));
#11001=CARTESIAN_POINT('Ctrl Pts',(146.056198364488,-1.54292182573692,340.712033158357));
#11002=CARTESIAN_POINT('Ctrl Pts',(146.048784806908,-1.39091389455423,340.75309320619));
#11003=CARTESIAN_POINT('Ctrl Pts',(146.041371249327,-1.23740195372028,340.788044501119));
#11004=CARTESIAN_POINT('Ctrl Pts',(146.033957691747,-1.08291885280208,340.816804734624));
#11005=CARTESIAN_POINT('Ctrl Pts',(146.02653357961,-0.928215816907973,340.845605913587));
#11006=CARTESIAN_POINT('Ctrl Pts',(146.019109467474,-0.772539227898603,
340.868198374132));
#11007=CARTESIAN_POINT('Ctrl Pts',(146.011685355337,-0.616427011310677,
340.884551665355));
#11008=CARTESIAN_POINT('Ctrl Pts',(146.007828230182,-0.535320429616164,
340.893047858539));
#11009=CARTESIAN_POINT('Ctrl Pts',(146.003971105028,-0.454096273587397,
340.899860821188));
#11010=CARTESIAN_POINT('Ctrl Pts',(146.000113979873,-0.372829765666778,
340.904991831352));
#11011=CARTESIAN_POINT('Ctrl Pts',(145.992690002435,-0.216412564486505,
340.914867710968));
#11012=CARTESIAN_POINT('Ctrl Pts',(145.985266024998,-0.0593667263293222,
340.918539199068));
#11013=CARTESIAN_POINT('Ctrl Pts',(145.97784204756,0.0977744572697015,340.915942082036));
#11014=CARTESIAN_POINT('Ctrl Pts',(145.970426831532,0.254730190628689,340.913348029993));
#11015=CARTESIAN_POINT('Ctrl Pts',(145.963011615504,0.411780675921287,340.904500104558));
#11016=CARTESIAN_POINT('Ctrl Pts',(145.955596399477,0.568387849815455,340.88938586057));
#11017=CARTESIAN_POINT('Ctrl Pts',(145.948188318333,0.724844337075537,340.874286159432));
#11018=CARTESIAN_POINT('Ctrl Pts',(145.940780237189,0.880857993120239,340.852932178805));
#11019=CARTESIAN_POINT('Ctrl Pts',(145.933372156045,1.03589121347152,340.825363504225));
#11020=CARTESIAN_POINT('Ctrl Pts',(145.925969588871,1.19080903976526,340.797815349513));
#11021=CARTESIAN_POINT('Ctrl Pts',(145.918567021697,1.34474751754345,340.764061776372));
#11022=CARTESIAN_POINT('Ctrl Pts',(145.911164454523,1.49717473187592,340.724194125354));
#11023=CARTESIAN_POINT('Ctrl Pts',(145.903765784768,1.64952169394666,340.684347464479));
#11024=CARTESIAN_POINT('Ctrl Pts',(145.896367115013,1.80035861704678,340.638393230828));
#11025=CARTESIAN_POINT('Ctrl Pts',(145.888968445259,1.94916445097795,340.586473709376));
#11026=CARTESIAN_POINT('Ctrl Pts',(145.881570996055,2.09794573656686,340.534562753032));
#11027=CARTESIAN_POINT('Ctrl Pts',(145.874173546851,2.24469624595006,340.476688584811));
#11028=CARTESIAN_POINT('Ctrl Pts',(145.866776097647,2.38891064187642,340.41304318361));
#11029=CARTESIAN_POINT('Ctrl Pts',(145.859378969183,2.53311878491825,340.349400541963));
#11030=CARTESIAN_POINT('Ctrl Pts',(145.85198184072,2.67479069170389,340.279987315561));
#11031=CARTESIAN_POINT('Ctrl Pts',(145.844584712256,2.81344179934591,340.205043304738));
#11032=CARTESIAN_POINT('Ctrl Pts',(145.83718644482,2.95211425579716,340.130087754408));
#11033=CARTESIAN_POINT('Ctrl Pts',(145.829788177383,3.0877646586355,340.049599901478));
#11034=CARTESIAN_POINT('Ctrl Pts',(145.822389909947,3.21993394427832,339.963865022035));
#11035=CARTESIAN_POINT('Ctrl Pts',(145.814989043421,3.35214966238097,339.878100023028));
#11036=CARTESIAN_POINT('Ctrl Pts',(145.807588176895,3.48088151548179,339.787084530407));
#11037=CARTESIAN_POINT('Ctrl Pts',(145.80018731037,3.60570039473357,339.691146472443));
#11038=CARTESIAN_POINT('Ctrl Pts',(145.792778316985,3.73065633704814,339.59510306532));
#11039=CARTESIAN_POINT('Ctrl Pts',(145.7853693236,3.85169042845558,339.49412652546));
#11040=CARTESIAN_POINT('Ctrl Pts',(145.777960330215,3.96840701099144,339.388584778447));
#11041=CARTESIAN_POINT('Ctrl Pts',(145.770546772635,4.0851954949682,339.282978014076));
#11042=CARTESIAN_POINT('Ctrl Pts',(145.763133215055,4.19766090422563,339.172800699187));
#11043=CARTESIAN_POINT('Ctrl Pts',(145.755719657475,4.30544566829836,339.058456376485));
#11044=CARTESIAN_POINT('Ctrl Pts',(145.748295545338,4.41338388371535,338.943949263706));
#11045=CARTESIAN_POINT('Ctrl Pts',(145.740871433202,4.51662790080987,338.82526357555));
#11046=CARTESIAN_POINT('Ctrl Pts',(145.733447321065,4.61486101039442,338.702835186346));
#11047=CARTESIAN_POINT('Ctrl Pts',(145.72959019591,4.66589706575485,338.639228709105));
#11048=CARTESIAN_POINT('Ctrl Pts',(145.725733070755,4.71558128286669,338.574612468472));
#11049=CARTESIAN_POINT('Ctrl Pts',(145.721875945601,4.76387402928941,338.509050412229));
#11050=CARTESIAN_POINT('Ctrl Pts',(145.714451968163,4.85682518992741,338.38286025588));
#11051=CARTESIAN_POINT('Ctrl Pts',(145.707027990725,4.94489913691349,338.252783913028));
#11052=CARTESIAN_POINT('Ctrl Pts',(145.699604013287,5.02775327699906,338.119235090231));
#11053=CARTESIAN_POINT('Ctrl Pts',(145.692188797259,5.1105096367333,337.985843875138));
#11054=CARTESIAN_POINT('Ctrl Pts',(145.684773581231,5.18805825661972,337.848988651383));
#11055=CARTESIAN_POINT('Ctrl Pts',(145.677358365204,5.26009749431416,337.70911515311));
#11056=CARTESIAN_POINT('Ctrl Pts',(145.66995028406,5.33206741621664,337.569376240413));
#11057=CARTESIAN_POINT('Ctrl Pts',(145.662542202915,5.3985383396877,337.426625164432));
#11058=CARTESIAN_POINT('Ctrl Pts',(145.655134121771,5.45925262441788,337.281335430244));
#11059=CARTESIAN_POINT('Ctrl Pts',(145.647731554597,5.51992171839747,337.136153837858));
#11060=CARTESIAN_POINT('Ctrl Pts',(145.640328987423,5.5748425619563,336.988437692554));
#11061=CARTESIAN_POINT('Ctrl Pts',(145.632926420249,5.62380411562351,336.838683722557));
#11062=CARTESIAN_POINT('Ctrl Pts',(145.625527750494,5.6727398912467,336.689008597371));
#11063=CARTESIAN_POINT('Ctrl Pts',(145.61812908074,5.7157225098888,336.537298138089));
#11064=CARTESIAN_POINT('Ctrl Pts',(145.610730410985,5.75258965186223,336.384067505502));
#11065=CARTESIAN_POINT('Ctrl Pts',(145.603332961781,5.78945071190187,336.230862151213));
#11066=CARTESIAN_POINT('Ctrl Pts',(145.595935512577,5.82019821032344,336.076137483844));
#11067=CARTESIAN_POINT('Ctrl Pts',(145.588538063373,5.84472011929416,335.920422343068));
#11068=CARTESIAN_POINT('Ctrl Pts',(145.581140934909,5.86924096503766,335.764713953828));
#11069=CARTESIAN_POINT('Ctrl Pts',(145.573743806446,5.88753669998392,335.608015545238));
#11070=CARTESIAN_POINT('Ctrl Pts',(145.566346677982,5.89954675256604,335.450864366287));
#11071=CARTESIAN_POINT('Ctrl Pts',(145.558948410546,5.91155865439647,335.293688989977));
#11072=CARTESIAN_POINT('Ctrl Pts',(145.551550143109,5.91728291832859,335.136061076643));
#11073=CARTESIAN_POINT('Ctrl Pts',(145.544151875672,5.91671101346509,334.978521041905));
#11074=CARTESIAN_POINT('Ctrl Pts',(145.536751009147,5.91613890768541,334.820925661695));
#11075=CARTESIAN_POINT('Ctrl Pts',(145.529350142621,5.90926623055444,334.663418594523));
#11076=CARTESIAN_POINT('Ctrl Pts',(145.521949276095,5.89613652853275,334.506538147977));
#11077=CARTESIAN_POINT('Ctrl Pts',(145.51454028271,5.88299240884299,334.349485431702));
#11078=CARTESIAN_POINT('Ctrl Pts',(145.507131289326,5.86357757402966,334.193061082338));
#11079=CARTESIAN_POINT('Ctrl Pts',(145.499722295941,5.83798730733733,334.037796922751));
#11080=CARTESIAN_POINT('Ctrl Pts',(145.49230873836,5.81238127615806,333.882437115086));
#11081=CARTESIAN_POINT('Ctrl Pts',(145.48489518078,5.7805923077503,333.728239286037));
#11082=CARTESIAN_POINT('Ctrl Pts',(145.4774816232,5.74276624788869,333.575722504352));
#11083=CARTESIAN_POINT('Ctrl Pts',(145.470057511063,5.70488633570577,333.422988587105));
#11084=CARTESIAN_POINT('Ctrl Pts',(145.462633398927,5.66095227027687,333.27194085447));
#11085=CARTESIAN_POINT('Ctrl Pts',(145.45520928679,5.61115919811044,333.123081510571));
#11086=CARTESIAN_POINT('Ctrl Pts',(145.451352161635,5.58528969241902,333.045743088243));
#11087=CARTESIAN_POINT('Ctrl Pts',(145.447495036481,5.55783949790399,332.968995014626));
#11088=CARTESIAN_POINT('Ctrl Pts',(145.443637911326,5.52884094223238,332.8929052233));
#11089=CARTESIAN_POINT('Ctrl Pts',(145.436213933888,5.47302615416728,332.746451874904));
#11090=CARTESIAN_POINT('Ctrl Pts',(145.42878995645,5.41130404880225,332.601996841012));
#11091=CARTESIAN_POINT('Ctrl Pts',(145.421365979012,5.34383712394275,332.460052095953));
#11092=CARTESIAN_POINT('Ctrl Pts',(145.413950762985,5.27644982020538,332.31827486705));
#11093=CARTESIAN_POINT('Ctrl Pts',(145.406535546957,5.20333135083097,332.179002363835));
#11094=CARTESIAN_POINT('Ctrl Pts',(145.399120330929,5.12469330719028,332.042729456113));
#11095=CARTESIAN_POINT('Ctrl Pts',(145.391712249785,5.04613092867937,331.906587669497));
#11096=CARTESIAN_POINT('Ctrl Pts',(145.384304168641,4.96205973421642,331.773440053587));
#11097=CARTESIAN_POINT('Ctrl Pts',(145.376896087497,4.87273848036978,331.643759504382));
#11098=CARTESIAN_POINT('Ctrl Pts',(145.369493520323,4.78348370996359,331.514175478779));
#11099=CARTESIAN_POINT('Ctrl Pts',(145.362090953149,4.68898687179859,331.388053687571));
#11100=CARTESIAN_POINT('Ctrl Pts',(145.354688385975,4.58955146967069,331.265840406498));
#11101=CARTESIAN_POINT('Ctrl Pts',(145.34728971622,4.49016841984711,331.143691470183));
#11102=CARTESIAN_POINT('Ctrl Pts',(145.339891046465,4.38585221932509,331.02544723451));
#11103=CARTESIAN_POINT('Ctrl Pts',(145.332492376711,4.27694823730927,330.911522980635));
#11104=CARTESIAN_POINT('Ctrl Pts',(145.325094927507,4.16806222106933,330.797617520724));
#11105=CARTESIAN_POINT('Ctrl Pts',(145.317697478303,4.05459018305988,330.68803089772));
#11106=CARTESIAN_POINT('Ctrl Pts',(145.310300029099,3.9369162111551,330.583143503707));
#11107=CARTESIAN_POINT('Ctrl Pts',(145.302902900635,3.81924734138875,330.478260657429));
#11108=CARTESIAN_POINT('Ctrl Pts',(145.295505772172,3.69737717858029,330.37807688335));
#11109=CARTESIAN_POINT('Ctrl Pts',(145.288108643708,3.57172472811626,330.282933853648));
#11110=CARTESIAN_POINT('Ctrl Pts',(145.280710376272,3.44605293031148,330.187776174294));
#11111=CARTESIAN_POINT('Ctrl Pts',(145.273312108835,3.31659798281694,330.097661010039));
#11112=CARTESIAN_POINT('Ctrl Pts',(145.265913841398,3.18380971609918,330.012887984597));
#11113=CARTESIAN_POINT('Ctrl Pts',(145.258512974873,3.05097479946708,329.928085177501));
#11114=CARTESIAN_POINT('Ctrl Pts',(145.251112108347,2.91480454646711,329.848628446522));
#11115=CARTESIAN_POINT('Ctrl Pts',(145.243711241821,2.77577519692348,329.774772481638));
#11116=CARTESIAN_POINT('Ctrl Pts',(145.236302248437,2.63659317986197,329.700835415844));
#11117=CARTESIAN_POINT('Ctrl Pts',(145.228893255052,2.49454612617375,329.632511573567));
#11118=CARTESIAN_POINT('Ctrl Pts',(145.221484261667,2.3501328202853,329.570008628965));
#11119=CARTESIAN_POINT('Ctrl Pts',(145.214070704087,2.20563055081888,329.507467180393));
#11120=CARTESIAN_POINT('Ctrl Pts',(145.206657146507,2.05875947184938,329.450753908947));
#11121=CARTESIAN_POINT('Ctrl Pts',(145.199243588926,1.91003500487676,329.400027067686));
#11122=CARTESIAN_POINT('Ctrl Pts',(145.19181947679,1.76109880139785,329.349228007481));
#11123=CARTESIAN_POINT('Ctrl Pts',(145.184395364653,1.6103042968242,329.304432505147));
#11124=CARTESIAN_POINT('Ctrl Pts',(145.176971252516,1.45817941028974,329.265748229289));
#11125=CARTESIAN_POINT('Ctrl Pts',(145.173114127362,1.37914440708806,329.245650190526));
#11126=CARTESIAN_POINT('Ctrl Pts',(145.169257002207,1.29975043929005,329.22720085828));
#11127=CARTESIAN_POINT('Ctrl Pts',(145.165399877052,1.22007212804745,329.210409810283));
#11128=CARTESIAN_POINT('Ctrl Pts',(145.157975899614,1.06671179846213,329.178091346015));
#11129=CARTESIAN_POINT('Ctrl Pts',(145.150551922176,0.911835105823138,329.151821873533));
#11130=CARTESIAN_POINT('Ctrl Pts',(145.143127944738,0.75596051715238,329.131741803652));
#11131=CARTESIAN_POINT('Ctrl Pts',(145.135712728711,0.600269883949183,329.111685431275));
#11132=CARTESIAN_POINT('Ctrl Pts',(145.128297512683,0.44358406543299,329.097803969142));
#11133=CARTESIAN_POINT('Ctrl Pts',(145.120882296656,0.286433712411587,329.090187288002));
#11134=CARTESIAN_POINT('Ctrl Pts',(145.113474215512,0.129434568667987,329.082577935594));
#11135=CARTESIAN_POINT('Ctrl Pts',(145.106066134367,-0.028027849459076,
329.081221381621));
#11136=CARTESIAN_POINT('Ctrl Pts',(145.098658053223,-0.185415845606974,
329.086155943323));
#11137=CARTESIAN_POINT('Ctrl Pts',(145.091255486049,-0.342686694995031,
329.09108683214));
#11138=CARTESIAN_POINT('Ctrl Pts',(145.083852918875,-0.499882861270552,
329.102299501265));
#11139=CARTESIAN_POINT('Ctrl Pts',(145.076450351701,-0.656464818324627,
329.11978023329));
#11140=CARTESIAN_POINT('Ctrl Pts',(145.069051681946,-0.812964335664323,
329.137251761787));
#11141=CARTESIAN_POINT('Ctrl Pts',(145.061653012192,-0.968849917837054,
329.160984739519));
#11142=CARTESIAN_POINT('Ctrl Pts',(145.054254342437,-1.12358544696739,329.190913470617));
#11143=CARTESIAN_POINT('Ctrl Pts',(145.046856893233,-1.27829544953845,329.220837264402));
#11144=CARTESIAN_POINT('Ctrl Pts',(145.039459444029,-1.43185540954218,329.256954712197));
#11145=CARTESIAN_POINT('Ctrl Pts',(145.032061994825,-1.58373759517044,329.299148678299));
#11146=CARTESIAN_POINT('Ctrl Pts',(145.024664866361,-1.7356131954517,329.341340814943));
#11147=CARTESIAN_POINT('Ctrl Pts',(145.017267737898,-1.88581080640624,329.389608846136));
#11148=CARTESIAN_POINT('Ctrl Pts',(145.009870609434,-2.03381636075276,329.443785319731));
#11149=CARTESIAN_POINT('Ctrl Pts',(145.002472341998,-2.18184470426047,329.497970135151));
#11150=CARTESIAN_POINT('Ctrl Pts',(144.995074074561,-2.32767996861832,329.558065076114));
#11151=CARTESIAN_POINT('Ctrl Pts',(144.987675807125,-2.47082676477559,329.623854014169));
#11152=CARTESIAN_POINT('Ctrl Pts',(144.980274940599,-2.61402384990777,329.68966606457));
#11153=CARTESIAN_POINT('Ctrl Pts',(144.972874074073,-2.75453024746913,329.761175939024));
#11154=CARTESIAN_POINT('Ctrl Pts',(144.965473207547,-2.89187406252918,329.838120984664));
#11155=CARTESIAN_POINT('Ctrl Pts',(144.958064214162,-3.02936869422832,329.915150523319));
#11156=CARTESIAN_POINT('Ctrl Pts',(144.950655220778,-3.16369348223284,329.997626969729));
#11157=CARTESIAN_POINT('Ctrl Pts',(144.943246227393,-3.29440386804054,330.085243269831));
#11158=CARTESIAN_POINT('Ctrl Pts',(144.935832669813,-3.42519477595524,330.172913544597));
#11159=CARTESIAN_POINT('Ctrl Pts',(144.928419112232,-3.55236654413012,330.265729762873));
#11160=CARTESIAN_POINT('Ctrl Pts',(144.921005554652,-3.67550717004287,330.363344135537));
#11161=CARTESIAN_POINT('Ctrl Pts',(144.913581442515,-3.79882310917973,330.46109748013));
#11162=CARTESIAN_POINT('Ctrl Pts',(144.906157330379,-3.918096161774,330.563662379406));
#11163=CARTESIAN_POINT('Ctrl Pts',(144.898733218242,-4.03295009966337,330.670653160565));
#11164=CARTESIAN_POINT('Ctrl Pts',(144.894876093087,-4.09262134449154,330.726239178896));
#11165=CARTESIAN_POINT('Ctrl Pts',(144.891018967933,-4.15110041317695,330.783019267912));
#11166=CARTESIAN_POINT('Ctrl Pts',(144.887161842778,-4.20833886981271,330.840935860158));
#11167=CARTESIAN_POINT('Ctrl Pts',(144.879838375853,-4.31701668741422,330.950901243888));
#11168=CARTESIAN_POINT('Ctrl Pts',(144.872514908928,-4.42156715453316,331.065317389096));
#11169=CARTESIAN_POINT('Ctrl Pts',(144.865191442003,-4.52159625809774,331.18383728842));
#11170=CARTESIAN_POINT('Ctrl Pts',(144.857876798109,-4.62150485043848,331.302214399518));
#11171=CARTESIAN_POINT('Ctrl Pts',(144.850562154216,-4.71690267209603,331.42468513694));
#11172=CARTESIAN_POINT('Ctrl Pts',(144.843247510322,-4.80743116996394,331.550864440391));
#11173=CARTESIAN_POINT('Ctrl Pts',(144.83594119061,-4.89785664495903,331.676900149785));
#11174=CARTESIAN_POINT('Ctrl Pts',(144.828634870898,-4.98342360892149,331.806635710497));
#11175=CARTESIAN_POINT('Ctrl Pts',(144.821328551186,-5.06381289989766,331.939652065969));
#11176=CARTESIAN_POINT('Ctrl Pts',(144.814026936671,-5.14415042097581,332.07258276024));
#11177=CARTESIAN_POINT('Ctrl Pts',(144.806725322155,-5.21931670374757,332.208789719243));
#11178=CARTESIAN_POINT('Ctrl Pts',(144.79942370764,-5.28903506488595,332.347823790751));
#11179=CARTESIAN_POINT('Ctrl Pts',(144.792125261801,-5.35872317040015,332.486797525748));
#11180=CARTESIAN_POINT('Ctrl Pts',(144.784826815961,-5.42296788641329,332.62859558944));
#11181=CARTESIAN_POINT('Ctrl Pts',(144.777528370122,-5.48153793665166,332.772743299135));
#11182=CARTESIAN_POINT('Ctrl Pts',(144.770231559051,-5.54009486787256,332.916858721401));
#11183=CARTESIAN_POINT('Ctrl Pts',(144.762934747979,-5.59297951911299,333.063322386253));
#11184=CARTESIAN_POINT('Ctrl Pts',(144.755637936908,-5.64000844513282,333.211638934295));
#11185=CARTESIAN_POINT('Ctrl Pts',(144.748338731286,-5.68705280435101,333.360004154481));
#11186=CARTESIAN_POINT('Ctrl Pts',(144.741039525664,-5.728237476805,333.510223107999));
#11187=CARTESIAN_POINT('Ctrl Pts',(144.733740320043,-5.76342861060435,333.661784317471));
#11188=CARTESIAN_POINT('Ctrl Pts',(144.726440090971,-5.79862467869001,333.813366777932));
#11189=CARTESIAN_POINT('Ctrl Pts',(144.719139861899,-5.82782545587922,333.96629149277));
#11190=CARTESIAN_POINT('Ctrl Pts',(144.711839632827,-5.8509482308236,334.120036726492));
#11191=CARTESIAN_POINT('Ctrl Pts',(144.704532809083,-5.87409189375922,334.273920846188));
#11192=CARTESIAN_POINT('Ctrl Pts',(144.697225985339,-5.89114653610034,334.428626584007));
#11193=CARTESIAN_POINT('Ctrl Pts',(144.689919161595,-5.90208129648768,334.583626451188));
#11194=CARTESIAN_POINT('Ctrl Pts',(144.683296775964,-5.91199178599715,334.72410731252));
#11195=CARTESIAN_POINT('Ctrl Pts',(144.676674390334,-5.91687585969667,334.864829523397));
#11196=CARTESIAN_POINT('Ctrl Pts',(144.670052004703,-5.91674753464347,335.005401276743));
#11197=CARTESIAN_POINT('',(142.920052004703,-5.92143889851083,334.997534891889));
#11198=CARTESIAN_POINT('Ctrl Pts',(144.670052004703,-5.91752625365133,335.00540198762));
#11199=CARTESIAN_POINT('Ctrl Pts',(144.649675939304,-5.9215386892976,335.437980671748));
#11200=CARTESIAN_POINT('Ctrl Pts',(144.536553862478,-5.68061954799383,337.83510250118));
#11201=CARTESIAN_POINT('Ctrl Pts',(144.330685774231,-2.41448809603895,341.566800602679));
#11202=CARTESIAN_POINT('Ctrl Pts',(144.052447739956,4.21554467127444,340.584067159849));
#11203=CARTESIAN_POINT('Ctrl Pts',(143.774209705683,6.97703431509326,334.476917705129));
#11204=CARTESIAN_POINT('Ctrl Pts',(143.495971671408,3.33580254881362,328.849793151726));
#11205=CARTESIAN_POINT('Ctrl Pts',(143.217733637134,-3.36664598015081,328.866622646082));
#11206=CARTESIAN_POINT('Ctrl Pts',(143.025760414899,-5.85942263800703,332.76168318681));
#11207=CARTESIAN_POINT('Ctrl Pts',(142.926533204089,-5.92597114832854,334.860405114397));
#11208=CARTESIAN_POINT('Ctrl Pts',(142.920052004703,-5.92525056693463,334.997533305083));
#11209=CARTESIAN_POINT('',(141.170052034586,-5.91294937614417,334.995918982415));
#11210=CARTESIAN_POINT('Ctrl Pts',(142.920052004703,-5.9167494872914,334.997536844101));
#11211=CARTESIAN_POINT('Ctrl Pts',(142.912703801634,-5.91681411766519,335.152785535897));
#11212=CARTESIAN_POINT('Ctrl Pts',(142.905355598564,-5.91076423044876,335.308283265996));
#11213=CARTESIAN_POINT('Ctrl Pts',(142.898007395495,-5.89856727785858,335.463502568575));
#11214=CARTESIAN_POINT('Ctrl Pts',(142.890667476036,-5.88638407486273,335.618546892821));
#11215=CARTESIAN_POINT('Ctrl Pts',(142.883327556578,-5.86806762495496,335.773313037574));
#11216=CARTESIAN_POINT('Ctrl Pts',(142.87598763712,-5.84363735587839,335.927271813161));
#11217=CARTESIAN_POINT('Ctrl Pts',(142.868654312993,-5.81922903877642,336.081092248104));
#11218=CARTESIAN_POINT('Ctrl Pts',(142.861320988866,-5.78871789525807,336.234106383423));
#11219=CARTESIAN_POINT('Ctrl Pts',(142.85398766474,-5.75217527315325,336.38578865251));
#11220=CARTESIAN_POINT('Ctrl Pts',(142.846659253752,-5.7156571336669,336.537369298371));
#11221=CARTESIAN_POINT('Ctrl Pts',(142.839330842764,-5.67311564843692,336.687619484875));
#11222=CARTESIAN_POINT('Ctrl Pts',(142.832002431776,-5.62467346985876,336.836022581552));
#11223=CARTESIAN_POINT('Ctrl Pts',(142.824676508245,-5.57624773383889,336.984375306287));
#11224=CARTESIAN_POINT('Ctrl Pts',(142.817350584714,-5.52192540487572,337.130881825851));
#11225=CARTESIAN_POINT('Ctrl Pts',(142.810024661183,-5.46187932651101,337.275039512873));
#11226=CARTESIAN_POINT('Ctrl Pts',(142.802699862899,-5.4018424711084,337.419175057551));
#11227=CARTESIAN_POINT('Ctrl Pts',(142.795375064616,-5.33608376158648,337.560962135352));
#11228=CARTESIAN_POINT('Ctrl Pts',(142.788050266333,-5.26482452840527,337.699917266807));
#11229=CARTESIAN_POINT('Ctrl Pts',(142.780725077479,-5.19356149555998,337.838879807587));
#11230=CARTESIAN_POINT('Ctrl Pts',(142.773399888624,-5.11679752930673,337.975009762055));
#11231=CARTESIAN_POINT('Ctrl Pts',(142.76607469977,-5.034800216519,338.107847702549));
#11232=CARTESIAN_POINT('Ctrl Pts',(142.758747604471,-4.9527815632026,338.240720215297));
#11233=CARTESIAN_POINT('Ctrl Pts',(142.751420509171,-4.86552705324495,338.370298684702));
#11234=CARTESIAN_POINT('Ctrl Pts',(142.744093413872,-4.77334779151031,338.496152374223));
#11235=CARTESIAN_POINT('Ctrl Pts',(142.736758692233,-4.68107258584562,338.62213705739));
#11236=CARTESIAN_POINT('Ctrl Pts',(142.729423970594,-4.58386261690172,338.744388909976));
#11237=CARTESIAN_POINT('Ctrl Pts',(142.722089248956,-4.48206990839239,338.862509533811));
#11238=CARTESIAN_POINT('Ctrl Pts',(142.714750479452,-4.38022102281612,338.980695345716));
#11239=CARTESIAN_POINT('Ctrl Pts',(142.707411709948,-4.27378461970932,339.09474510919));
#11240=CARTESIAN_POINT('Ctrl Pts',(142.700072940444,-4.16314930902,339.204297609983));
#11241=CARTESIAN_POINT('Ctrl Pts',(142.692723289544,-4.05234995630737,339.314012547286));
#11242=CARTESIAN_POINT('Ctrl Pts',(142.685373638645,-3.93733954111777,339.419216645527));
#11243=CARTESIAN_POINT('Ctrl Pts',(142.678023987745,-3.81854009505559,339.519588709712));
#11244=CARTESIAN_POINT('Ctrl Pts',(142.672435181359,-3.72820286518126,339.595913427846));
#11245=CARTESIAN_POINT('Ctrl Pts',(142.666846374973,-3.63567536819131,339.669444924152));
#11246=CARTESIAN_POINT('Ctrl Pts',(142.661257568587,-3.5411536962794,339.740059183368));
#11247=CARTESIAN_POINT('Ctrl Pts',(142.653833591149,-3.41559437087036,339.833860727204));
#11248=CARTESIAN_POINT('Ctrl Pts',(142.646409613711,-3.28611599859085,339.922811422643));
#11249=CARTESIAN_POINT('Ctrl Pts',(142.638985636273,-3.15312996209623,340.006565889373));
#11250=CARTESIAN_POINT('Ctrl Pts',(142.631570420246,-3.0203008691336,340.09022151323));
#11251=CARTESIAN_POINT('Ctrl Pts',(142.624155204218,-2.88397266456738,340.168692917926));
#11252=CARTESIAN_POINT('Ctrl Pts',(142.61673998819,-2.74458903456155,340.241675456747));
#11253=CARTESIAN_POINT('Ctrl Pts',(142.609331907046,-2.60533951878256,340.314587772137));
#11254=CARTESIAN_POINT('Ctrl Pts',(142.601923825902,-2.46304075880642,340.382021563891));
#11255=CARTESIAN_POINT('Ctrl Pts',(142.594515744758,-2.3181645083636,340.443715998715));
#11256=CARTESIAN_POINT('Ctrl Pts',(142.587113177584,-2.17339609195958,340.505364513244));
#11257=CARTESIAN_POINT('Ctrl Pts',(142.57971061041,-2.02605434695135,340.561282031238));
#11258=CARTESIAN_POINT('Ctrl Pts',(142.572308043236,-1.8766345645083,340.611254162288));
#11259=CARTESIAN_POINT('Ctrl Pts',(142.564909373481,-1.7272934509288,340.661199983229));
#11260=CARTESIAN_POINT('Ctrl Pts',(142.557510703726,-1.5758768318851,340.705206533172));
#11261=CARTESIAN_POINT('Ctrl Pts',(142.550112033972,-1.42289875982937,340.743108015855));
#11262=CARTESIAN_POINT('Ctrl Pts',(142.542714584768,-1.26994592440439,340.78100324597));
#11263=CARTESIAN_POINT('Ctrl Pts',(142.535317135564,-1.11543250910901,340.812795318021));
#11264=CARTESIAN_POINT('Ctrl Pts',(142.52791968636,-0.959886584719471,340.838368634043));
#11265=CARTESIAN_POINT('Ctrl Pts',(142.520522557896,-0.804347404530152,
340.86394084125));
#11266=CARTESIAN_POINT('Ctrl Pts',(142.513125429433,-0.647776172527041,
340.883294768003));
#11267=CARTESIAN_POINT('Ctrl Pts',(142.505728300969,-0.490709716235529,
340.896366214618));
#11268=CARTESIAN_POINT('Ctrl Pts',(142.498330033532,-0.333619075630934,
340.90943967391));
#11269=CARTESIAN_POINT('Ctrl Pts',(142.490931766096,-0.17603343085798,340.916228695997));
#11270=CARTESIAN_POINT('Ctrl Pts',(142.483533498659,-0.0184931275726032,
340.916721099286));
#11271=CARTESIAN_POINT('Ctrl Pts',(142.476132632133,0.139102521278442,340.917213675561));
#11272=CARTESIAN_POINT('Ctrl Pts',(142.468731765608,0.296652423953073,340.911405227647));
#11273=CARTESIAN_POINT('Ctrl Pts',(142.461330899082,0.453617990959382,340.899335664359));
#11274=CARTESIAN_POINT('Ctrl Pts',(142.453921905697,0.610755921164594,340.887252847537));
#11275=CARTESIAN_POINT('Ctrl Pts',(142.446512912312,0.767307861944534,340.868895213624));
#11276=CARTESIAN_POINT('Ctrl Pts',(142.439103918928,0.922741358861505,340.844354450848));
#11277=CARTESIAN_POINT('Ctrl Pts',(142.431690361347,1.078270608174,340.819798570115));
#11278=CARTESIAN_POINT('Ctrl Pts',(142.424276803767,1.23267967552981,340.789052043257));
#11279=CARTESIAN_POINT('Ctrl Pts',(142.416863246187,1.38544851873577,340.752257206039));
#11280=CARTESIAN_POINT('Ctrl Pts',(142.40943913405,1.53843485635821,340.715409984635));
#11281=CARTESIAN_POINT('Ctrl Pts',(142.402015021913,1.68977594796262,340.672497356763));
#11282=CARTESIAN_POINT('Ctrl Pts',(142.394590909777,1.83896828253318,340.623711071733));
#11283=CARTESIAN_POINT('Ctrl Pts',(142.390733784622,1.91647970692796,340.598364632491));
#11284=CARTESIAN_POINT('Ctrl Pts',(142.386876659467,1.99341147476138,340.571433552271));
#11285=CARTESIAN_POINT('Ctrl Pts',(142.383019534312,2.06969543560795,340.542949699061));
#11286=CARTESIAN_POINT('Ctrl Pts',(142.375595556874,2.21652251056,340.488125581335));
#11287=CARTESIAN_POINT('Ctrl Pts',(142.368171579436,2.36139122474337,340.427380781077));
#11288=CARTESIAN_POINT('Ctrl Pts',(142.360747601998,2.50378851772458,340.360874333633));
#11289=CARTESIAN_POINT('Ctrl Pts',(142.35333238597,2.6460177604755,340.294446373804));
#11290=CARTESIAN_POINT('Ctrl Pts',(142.345917169943,2.78578105280035,340.222270457918));
#11291=CARTESIAN_POINT('Ctrl Pts',(142.338501953915,2.9225821067375,340.14455482932));
#11292=CARTESIAN_POINT('Ctrl Pts',(142.331093872771,3.05925153138926,340.066913978308));
#11293=CARTESIAN_POINT('Ctrl Pts',(142.323685791627,3.19296406963677,339.983744209301));
#11294=CARTESIAN_POINT('Ctrl Pts',(142.316277710483,3.3232450881857,339.895301078213));
#11295=CARTESIAN_POINT('Ctrl Pts',(142.308875143309,3.45342913619271,339.806923776962));
#11296=CARTESIAN_POINT('Ctrl Pts',(142.301472576135,3.58018644271276,339.71328113772));
#11297=CARTESIAN_POINT('Ctrl Pts',(142.294070008961,3.70306869180658,339.614673642443));
#11298=CARTESIAN_POINT('Ctrl Pts',(142.286671339206,3.82588624393301,339.516118063583));
#11299=CARTESIAN_POINT('Ctrl Pts',(142.279272669451,3.94483251146716,339.412603067566));
#11300=CARTESIAN_POINT('Ctrl Pts',(142.271873999696,4.05948988951751,339.304471210196));
#11301=CARTESIAN_POINT('Ctrl Pts',(142.264476550492,4.17412835266133,339.196357191224));
#11302=CARTESIAN_POINT('Ctrl Pts',(142.257079101288,4.28447905929744,339.083628078318));
#11303=CARTESIAN_POINT('Ctrl Pts',(142.249681652085,4.39015903123336,338.966665380768));
#11304=CARTESIAN_POINT('Ctrl Pts',(142.242284523621,4.49583442106978,338.849707754516));
#11305=CARTESIAN_POINT('Ctrl Pts',(142.234887395158,4.59683922866674,338.728517185517));
#11306=CARTESIAN_POINT('Ctrl Pts',(142.227490266694,4.69282895896306,338.603510361358));
#11307=CARTESIAN_POINT('Ctrl Pts',(142.220091999258,4.78883346928186,338.478484289269));
#11308=CARTESIAN_POINT('Ctrl Pts',(142.212693731821,4.87982113744197,338.349641088041));
#11309=CARTESIAN_POINT('Ctrl Pts',(142.205295464384,4.9654893076409,338.217428553706));
#11310=CARTESIAN_POINT('Ctrl Pts',(142.197894597858,5.05118757396939,338.085169571717));
#11311=CARTESIAN_POINT('Ctrl Pts',(142.190493731333,5.13156241874969,337.949539212921));
#11312=CARTESIAN_POINT('Ctrl Pts',(142.183092864807,5.20635594047811,337.811011985664));
#11313=CARTESIAN_POINT('Ctrl Pts',(142.175683871422,5.28123159264351,337.672332642269));
#11314=CARTESIAN_POINT('Ctrl Pts',(142.168274878037,5.35051350474745,337.530750406306));
#11315=CARTESIAN_POINT('Ctrl Pts',(142.160865884653,5.41399063772855,337.386762647832));
#11316=CARTESIAN_POINT('Ctrl Pts',(142.153452327072,5.47750687481307,337.242686187933));
#11317=CARTESIAN_POINT('Ctrl Pts',(142.146038769492,5.53521107076559,337.096201599101));
#11318=CARTESIAN_POINT('Ctrl Pts',(142.138625211912,5.58694149409885,336.947823221963));
#11319=CARTESIAN_POINT('Ctrl Pts',(142.131201099775,5.63874556516032,336.799233601039));
#11320=CARTESIAN_POINT('Ctrl Pts',(142.123776987638,5.68455876949909,336.64874516312));
#11321=CARTESIAN_POINT('Ctrl Pts',(142.116352875502,5.72426987449761,336.496885087914));
#11322=CARTESIAN_POINT('Ctrl Pts',(142.112495750347,5.74490139233848,336.417987664862));
#11323=CARTESIAN_POINT('Ctrl Pts',(142.108638625193,5.76388666634816,336.338720147219));
#11324=CARTESIAN_POINT('Ctrl Pts',(142.104781500038,5.78121561489331,336.259157089729));
#11325=CARTESIAN_POINT('Ctrl Pts',(142.0973575226,5.81456939986825,336.106018594075));
#11326=CARTESIAN_POINT('Ctrl Pts',(142.089933545162,5.84188457520743,335.951322904724));
#11327=CARTESIAN_POINT('Ctrl Pts',(142.082509567724,5.8630172306863,335.795587528293));
#11328=CARTESIAN_POINT('Ctrl Pts',(142.075094351697,5.88412494645215,335.640035943037));
#11329=CARTESIAN_POINT('Ctrl Pts',(142.067679135669,5.89906461607092,335.483447479264));
#11330=CARTESIAN_POINT('Ctrl Pts',(142.060263919642,5.90774278592052,335.32635216853));
#11331=CARTESIAN_POINT('Ctrl Pts',(142.052855838497,5.91641260567876,335.169408014113));
#11332=CARTESIAN_POINT('Ctrl Pts',(142.045447757353,5.91883289944102,335.01195835378));
#11333=CARTESIAN_POINT('Ctrl Pts',(142.038039676209,5.91496171831772,334.854540612761));
#11334=CARTESIAN_POINT('Ctrl Pts',(142.030637109035,5.91109341858522,334.697240040642));
#11335=CARTESIAN_POINT('Ctrl Pts',(142.023234541861,5.90094297735857,334.539971712033));
#11336=CARTESIAN_POINT('Ctrl Pts',(142.015831974687,5.88452046684895,334.383275233402));
#11337=CARTESIAN_POINT('Ctrl Pts',(142.008433304932,5.86810660271929,334.226661254781));
#11338=CARTESIAN_POINT('Ctrl Pts',(142.001034635178,5.84542728467107,334.070618896769));
#11339=CARTESIAN_POINT('Ctrl Pts',(141.993635965423,5.81654458521853,333.91568470883));
#11340=CARTESIAN_POINT('Ctrl Pts',(141.986238516219,5.78766665051466,333.760776080222));
#11341=CARTESIAN_POINT('Ctrl Pts',(141.978841067015,5.75258743378497,333.606975625394));
#11342=CARTESIAN_POINT('Ctrl Pts',(141.971443617811,5.7114205028552,333.454811855448));
#11343=CARTESIAN_POINT('Ctrl Pts',(141.964046489348,5.67025535685187,333.302654683057));
#11344=CARTESIAN_POINT('Ctrl Pts',(141.956649360884,5.62300311893932,333.152134414708));
#11345=CARTESIAN_POINT('Ctrl Pts',(141.949252232421,5.56982776455352,333.003766237208));
#11346=CARTESIAN_POINT('Ctrl Pts',(141.941853964984,5.51664422249044,332.855375214713));
#11347=CARTESIAN_POINT('Ctrl Pts',(141.934455697547,5.45753587394222,332.709137294216));
#11348=CARTESIAN_POINT('Ctrl Pts',(141.927057430111,5.39271549572256,332.565549313563));
#11349=CARTESIAN_POINT('Ctrl Pts',(141.919656563585,5.32787234542219,332.421910888942));
#11350=CARTESIAN_POINT('Ctrl Pts',(141.912255697059,5.25731332358313,332.280924597633));
#11351=CARTESIAN_POINT('Ctrl Pts',(141.904854830533,5.18129788909323,332.143064098203));
#11352=CARTESIAN_POINT('Ctrl Pts',(141.897445837149,5.10519898238911,332.005052214765));
#11353=CARTESIAN_POINT('Ctrl Pts',(141.890036843764,5.02363187767832,331.870173304945));
#11354=CARTESIAN_POINT('Ctrl Pts',(141.882627850379,4.93690061870751,331.738873991471));
#11355=CARTESIAN_POINT('Ctrl Pts',(141.875214292799,4.85011593028928,331.60749379309));
#11356=CARTESIAN_POINT('Ctrl Pts',(141.867800735219,4.75816096592499,331.479697887347));
#11357=CARTESIAN_POINT('Ctrl Pts',(141.860387177638,4.661380723432,331.355900616927));
#11358=CARTESIAN_POINT('Ctrl Pts',(141.852963065502,4.56446269654597,331.231927098428));
#11359=CARTESIAN_POINT('Ctrl Pts',(141.845538953365,4.46270591219901,331.111963868735));
#11360=CARTESIAN_POINT('Ctrl Pts',(141.838114841228,4.35649349270314,330.996389752919));
#11361=CARTESIAN_POINT('Ctrl Pts',(141.834257716074,4.30131186459401,330.936344346663));
#11362=CARTESIAN_POINT('Ctrl Pts',(141.830400590919,4.24492813904903,330.877483022547));
#11363=CARTESIAN_POINT('Ctrl Pts',(141.826543465765,4.1873995549931,330.819854604282));
#11364=CARTESIAN_POINT('Ctrl Pts',(141.819119488327,4.07667177382124,330.708934667842));
#11365=CARTESIAN_POINT('Ctrl Pts',(141.811695510889,3.96136667707952,330.602250040211));
#11366=CARTESIAN_POINT('Ctrl Pts',(141.804271533451,3.8418415690413,330.500201791093));
#11367=CARTESIAN_POINT('Ctrl Pts',(141.796856317423,3.72245751861409,330.398273974262));
#11368=CARTESIAN_POINT('Ctrl Pts',(141.789441101395,3.59886365122774,330.300971884564));
#11369=CARTESIAN_POINT('Ctrl Pts',(141.782025885368,3.47145510860933,330.208660939632));
#11370=CARTESIAN_POINT('Ctrl Pts',(141.774617804224,3.34416915784892,330.116438815826));
#11371=CARTESIAN_POINT('Ctrl Pts',(141.76720972308,3.21307613926443,330.0291984935));
#11372=CARTESIAN_POINT('Ctrl Pts',(141.759801641936,3.07860528424778,329.947266080002));
#11373=CARTESIAN_POINT('Ctrl Pts',(141.752399074762,2.9442345183446,329.865394650295));
#11374=CARTESIAN_POINT('Ctrl Pts',(141.744996507588,2.80649123946498,329.788823456208));
#11375=CARTESIAN_POINT('Ctrl Pts',(141.737593940414,2.66583466485106,329.717836039824));
#11376=CARTESIAN_POINT('Ctrl Pts',(141.730195270659,2.52525214530864,329.646885998006));
#11377=CARTESIAN_POINT('Ctrl Pts',(141.722796600904,2.38175971710454,329.581514046766));
#11378=CARTESIAN_POINT('Ctrl Pts',(141.71539793115,2.23584216712864,329.521958345705));
#11379=CARTESIAN_POINT('Ctrl Pts',(141.708000481946,2.08994868901739,329.462412469486));
#11380=CARTESIAN_POINT('Ctrl Pts',(141.700603032742,1.94163122834648,329.408681080041));
#11381=CARTESIAN_POINT('Ctrl Pts',(141.693205583538,1.79139567944247,329.360954683444));
#11382=CARTESIAN_POINT('Ctrl Pts',(141.685808455074,1.64116664449027,329.31323035618));
#11383=CARTESIAN_POINT('Ctrl Pts',(141.678411326611,1.48902004235882,329.271510617068));
#11384=CARTESIAN_POINT('Ctrl Pts',(141.671014198147,1.33547784114391,329.235936372808));
#11385=CARTESIAN_POINT('Ctrl Pts',(141.663615930711,1.18191199826283,329.200356651003));
#11386=CARTESIAN_POINT('Ctrl Pts',(141.656217663274,1.02695049203155,329.170924392407));
#11387=CARTESIAN_POINT('Ctrl Pts',(141.648819395838,0.871126269738591,329.147729535926));
#11388=CARTESIAN_POINT('Ctrl Pts',(141.641418529312,0.715247304758272,329.124526530848));
#11389=CARTESIAN_POINT('Ctrl Pts',(141.634017662786,0.558505389193618,329.107565345604));
#11390=CARTESIAN_POINT('Ctrl Pts',(141.626616796261,0.40143924073227,329.096884119509));
#11391=CARTESIAN_POINT('Ctrl Pts',(141.619207802876,0.244200618622956,329.086191164407));
#11392=CARTESIAN_POINT('Ctrl Pts',(141.611798809491,0.0866374251619905,
329.081791965463));
#11393=CARTESIAN_POINT('Ctrl Pts',(141.604389816106,-0.0707102295546171,
329.083672538987));
#11394=CARTESIAN_POINT('Ctrl Pts',(141.596976258526,-0.22815481585403,329.08555427101));
#11395=CARTESIAN_POINT('Ctrl Pts',(141.589562700946,-0.385383226991015,
329.093723464792));
#11396=CARTESIAN_POINT('Ctrl Pts',(141.582149143366,-0.541860335248411,
329.108114228909));
#11397=CARTESIAN_POINT('Ctrl Pts',(141.574725031229,-0.698560217315989,
329.122525480914));
#11398=CARTESIAN_POINT('Ctrl Pts',(141.567300919092,-0.854506291280839,
329.143175944681));
#11399=CARTESIAN_POINT('Ctrl Pts',(141.559876806956,-1.00917266559218,329.169948448468));
#11400=CARTESIAN_POINT('Ctrl Pts',(141.556019681801,-1.08952807402006,329.183857842064));
#11401=CARTESIAN_POINT('Ctrl Pts',(141.552162556646,-1.16953828641434,329.199418879829));
#11402=CARTESIAN_POINT('Ctrl Pts',(141.548305431491,-1.24913127060842,329.216609849639));
#11403=CARTESIAN_POINT('Ctrl Pts',(141.540881454053,-1.40232736748535,329.249698060908));
#11404=CARTESIAN_POINT('Ctrl Pts',(141.533457476615,-1.55443895092883,329.288927403111));
#11405=CARTESIAN_POINT('Ctrl Pts',(141.526033499177,-1.70493539502551,329.334214453292));
#11406=CARTESIAN_POINT('Ctrl Pts',(141.51861828315,-1.85525423067496,329.379448057939));
#11407=CARTESIAN_POINT('Ctrl Pts',(141.511203067122,-2.00396136720902,329.430725033856));
#11408=CARTESIAN_POINT('Ctrl Pts',(141.503787851094,-2.15053568328211,329.487910846382));
#11409=CARTESIAN_POINT('Ctrl Pts',(141.49637976995,-2.29696896628602,329.545041635008));
#11410=CARTESIAN_POINT('Ctrl Pts',(141.488971688806,-2.4412731689922,329.608069806823));
#11411=CARTESIAN_POINT('Ctrl Pts',(141.481563607662,-2.58294177904009,329.676810887392));
#11412=CARTESIAN_POINT('Ctrl Pts',(141.474161040488,-2.72450494255493,329.745500802719));
#11413=CARTESIAN_POINT('Ctrl Pts',(141.466758473314,-2.8634360851482,329.819894997779));
#11414=CARTESIAN_POINT('Ctrl Pts',(141.45935590614,-2.99924826143191,329.899760747887));
#11415=CARTESIAN_POINT('Ctrl Pts',(141.451957236385,-3.13498893319731,329.979584449026));
#11416=CARTESIAN_POINT('Ctrl Pts',(141.44455856663,-3.26761358813892,330.064873779321));
#11417=CARTESIAN_POINT('Ctrl Pts',(141.437159896875,-3.39665960676462,330.155349952961));
#11418=CARTESIAN_POINT('Ctrl Pts',(141.429762447671,-3.5256843368049,330.245811200842));
#11419=CARTESIAN_POINT('Ctrl Pts',(141.422364998467,-3.65113129692158,330.341457379799));
#11420=CARTESIAN_POINT('Ctrl Pts',(141.414967549263,-3.77256651804377,330.441966166269));
#11421=CARTESIAN_POINT('Ctrl Pts',(141.4075704208,-3.89399647394623,330.542470594853));
#11422=CARTESIAN_POINT('Ctrl Pts',(141.400173292336,-4.01141474920077,330.647836973779));
#11423=CARTESIAN_POINT('Ctrl Pts',(141.392776163873,-4.12442038546909,330.757702621642));
#11424=CARTESIAN_POINT('Ctrl Pts',(141.385377896436,-4.2374434217844,330.867585186071));
#11425=CARTESIAN_POINT('Ctrl Pts',(141.377979628999,-4.34605219865847,330.981968138671));
#11426=CARTESIAN_POINT('Ctrl Pts',(141.370581361563,-4.44988267618832,331.100451983799));
#11427=CARTESIAN_POINT('Ctrl Pts',(141.363180495037,-4.55374963045635,331.218977453547));
#11428=CARTESIAN_POINT('Ctrl Pts',(141.355779628511,-4.65283469734034,331.341606403719));
#11429=CARTESIAN_POINT('Ctrl Pts',(141.348378761986,-4.74681427362334,331.467906454491));
#11430=CARTESIAN_POINT('Ctrl Pts',(141.340969768601,-4.84089704846656,331.594345194794));
#11431=CARTESIAN_POINT('Ctrl Pts',(141.333560775216,-4.92986291366767,331.724462786665));
#11432=CARTESIAN_POINT('Ctrl Pts',(141.326151781831,-5.01343134384435,331.857797472622));
#11433=CARTESIAN_POINT('Ctrl Pts',(141.318738224251,-5.09705125505637,331.991214297345));
#11434=CARTESIAN_POINT('Ctrl Pts',(141.311324666671,-5.17526692075334,332.127851842095));
#11435=CARTESIAN_POINT('Ctrl Pts',(141.30391110909,-5.24784416212585,332.267224448927));
#11436=CARTESIAN_POINT('Ctrl Pts',(141.296486996954,-5.3205247304886,332.406795478181));
#11437=CARTESIAN_POINT('Ctrl Pts',(141.289062884817,-5.38755068375463,332.54910900961));
#11438=CARTESIAN_POINT('Ctrl Pts',(141.28163877268,-5.44873596404843,332.693659401436));
#11439=CARTESIAN_POINT('Ctrl Pts',(141.277781647526,-5.48052418052112,332.768759149684));
#11440=CARTESIAN_POINT('Ctrl Pts',(141.273924522371,-5.51073668879568,332.844462414655));
#11441=CARTESIAN_POINT('Ctrl Pts',(141.270067397216,-5.53935276631987,332.920696873286));
#11442=CARTESIAN_POINT('Ctrl Pts',(141.261553144537,-5.60252015264225,333.088977501382));
#11443=CARTESIAN_POINT('Ctrl Pts',(141.253038891857,-5.65806380752951,333.260267546807));
#11444=CARTESIAN_POINT('Ctrl Pts',(141.244524639177,-5.70572547026194,333.433913341956));
#11445=CARTESIAN_POINT('Ctrl Pts',(141.23603957969,-5.75322371335498,333.606963750129));
#11446=CARTESIAN_POINT('Ctrl Pts',(141.227554520203,-5.79289382508951,333.782353644897));
#11447=CARTESIAN_POINT('Ctrl Pts',(141.219069460716,-5.82452667773354,333.959413846493));
#11448=CARTESIAN_POINT('Ctrl Pts',(141.210642121583,-5.85594434515345,334.135269580709));
#11449=CARTESIAN_POINT('Ctrl Pts',(141.202214782449,-5.87943365279655,334.312772823345));
#11450=CARTESIAN_POINT('Ctrl Pts',(141.193787443315,-5.89483690462232,334.491248164227));
#11451=CARTESIAN_POINT('Ctrl Pts',(141.18587565336,-5.90929785025902,334.658805134091));
#11452=CARTESIAN_POINT('Ctrl Pts',(141.177963863405,-5.91663213484256,334.827218636702));
#11453=CARTESIAN_POINT('Ctrl Pts',(141.170052073449,-5.91674859019896,334.995915532029));
#11454=CARTESIAN_POINT('',(139.420051969975,-5.91362844489661,335.004262364622));
#11455=CARTESIAN_POINT('Ctrl Pts',(141.170052004703,-5.91002799473302,334.995921635567));
#11456=CARTESIAN_POINT('Ctrl Pts',(141.11064445745,-5.90202012525986,336.261189543943));
#11457=CARTESIAN_POINT('Ctrl Pts',(140.958490898771,-4.88291250323578,339.513541639599));
#11458=CARTESIAN_POINT('Ctrl Pts',(140.71359132867,0.475935523755951,341.980408891924));
#11459=CARTESIAN_POINT('Ctrl Pts',(140.435353294395,6.12753077878764,338.377275451633));
#11460=CARTESIAN_POINT('Ctrl Pts',(140.157115260122,6.15598148033646,331.674866177885));
#11461=CARTESIAN_POINT('Ctrl Pts',(139.878877225847,0.535178839515167,328.023883133794));
#11462=CARTESIAN_POINT('Ctrl Pts',(139.633189474041,-4.86173227124819,330.452959959149));
#11463=CARTESIAN_POINT('Ctrl Pts',(139.48024773366,-5.90188289997479,333.722401776941));
#11464=CARTESIAN_POINT('Ctrl Pts',(139.420052004703,-5.91038989499448,335.004259290461));
#11465=CARTESIAN_POINT('',(137.670052004703,-5.92107572873037,335.002186220721));
#11466=CARTESIAN_POINT('Ctrl Pts',(139.420051936518,-5.91674846258414,335.004265326268));
#11467=CARTESIAN_POINT('Ctrl Pts',(139.4115646907,-5.91661803343069,335.185193218922));
#11468=CARTESIAN_POINT('Ctrl Pts',(139.403077444883,-5.90818479430956,335.365788285949));
#11469=CARTESIAN_POINT('Ctrl Pts',(139.394590199065,-5.89156394627951,335.545348356007));
#11470=CARTESIAN_POINT('Ctrl Pts',(139.386063051631,-5.87486495762325,335.725752602986));
#11471=CARTESIAN_POINT('Ctrl Pts',(139.377535904197,-5.84990129915733,335.905111962886));
#11472=CARTESIAN_POINT('Ctrl Pts',(139.369008756763,-5.81683933887567,336.082732962557));
#11473=CARTESIAN_POINT('Ctrl Pts',(139.36042855897,-5.78357168860522,336.261459004432));
#11474=CARTESIAN_POINT('Ctrl Pts',(139.351848361177,-5.74210474159252,336.438424854248));
#11475=CARTESIAN_POINT('Ctrl Pts',(139.343268163383,-5.69265661404864,336.612944895844));
#11476=CARTESIAN_POINT('Ctrl Pts',(139.336312494689,-5.65257073245615,336.754422239283));
#11477=CARTESIAN_POINT('Ctrl Pts',(139.329356825994,-5.60724073314045,336.894292621023));
#11478=CARTESIAN_POINT('Ctrl Pts',(139.322401157299,-5.55680547474913,337.032201633278));
#11479=CARTESIAN_POINT('Ctrl Pts',(139.314977179861,-5.50297452954355,337.179395733574));
#11480=CARTESIAN_POINT('Ctrl Pts',(139.307553202423,-5.44320980679537,337.324671516216));
#11481=CARTESIAN_POINT('Ctrl Pts',(139.300129224985,-5.37766687213299,337.467514858084));
#11482=CARTESIAN_POINT('Ctrl Pts',(139.292714008957,-5.31220128799499,337.610189623316));
#11483=CARTESIAN_POINT('Ctrl Pts',(139.28529879293,-5.24097121971824,337.750437325931));
#11484=CARTESIAN_POINT('Ctrl Pts',(139.277883576902,-5.16418155311644,337.88776028246));
#11485=CARTESIAN_POINT('Ctrl Pts',(139.270475495758,-5.08746577314524,338.024951107532));
#11486=CARTESIAN_POINT('Ctrl Pts',(139.263067414614,-5.00520122547612,338.159222465453));
#11487=CARTESIAN_POINT('Ctrl Pts',(139.25565933347,-4.9176402537058,338.290098007299));
#11488=CARTESIAN_POINT('Ctrl Pts',(139.248256766296,-4.83014445516577,338.420876136089));
#11489=CARTESIAN_POINT('Ctrl Pts',(139.240854199122,-4.73736028870984,338.548263172698));
#11490=CARTESIAN_POINT('Ctrl Pts',(139.233451631948,-4.63958520074719,338.671808781446));
#11491=CARTESIAN_POINT('Ctrl Pts',(139.226052962193,-4.54186159094163,338.795289343972));
#11492=CARTESIAN_POINT('Ctrl Pts',(139.218654292438,-4.43915252387025,338.914932214641));
#11493=CARTESIAN_POINT('Ctrl Pts',(139.211255622683,-4.33179772630097,339.030317483886));
#11494=CARTESIAN_POINT('Ctrl Pts',(139.203858173479,-4.22446063893921,339.145683718144));
#11495=CARTESIAN_POINT('Ctrl Pts',(139.196460724275,-4.11247959611186,339.256793471987));
#11496=CARTESIAN_POINT('Ctrl Pts',(139.189063275071,-3.99623351111238,339.363261198595));
#11497=CARTESIAN_POINT('Ctrl Pts',(139.181666146608,-3.87999246634052,339.469724308947));
#11498=CARTESIAN_POINT('Ctrl Pts',(139.174269018144,-3.7594870223097,339.571545540186));
#11499=CARTESIAN_POINT('Ctrl Pts',(139.166871889681,-3.63513152978765,339.668377590089));
#11500=CARTESIAN_POINT('Ctrl Pts',(139.159473622244,-3.51075688962381,339.76522454971));
#11501=CARTESIAN_POINT('Ctrl Pts',(139.152075354808,-3.38253131508879,339.857080569083));
#11502=CARTESIAN_POINT('Ctrl Pts',(139.144677087371,-3.25090054733828,339.94363997413));
#11503=CARTESIAN_POINT('Ctrl Pts',(139.137276220845,-3.1192235363147,340.030229788406));
#11504=CARTESIAN_POINT('Ctrl Pts',(139.129875354319,-2.9841392619177,340.111519078666));
#11505=CARTESIAN_POINT('Ctrl Pts',(139.122474487794,-2.84612047935495,340.187246743649));
#11506=CARTESIAN_POINT('Ctrl Pts',(139.115065494409,-2.70795013897403,340.263057564848));
#11507=CARTESIAN_POINT('Ctrl Pts',(139.107656501024,-2.56683918257287,340.333294384741));
#11508=CARTESIAN_POINT('Ctrl Pts',(139.100247507639,-2.42328354313969,340.397742808994));
#11509=CARTESIAN_POINT('Ctrl Pts',(139.092833950059,-2.27963946848091,340.4622309357));
#11510=CARTESIAN_POINT('Ctrl Pts',(139.085420392479,-2.13354805536722,340.52092342253));
#11511=CARTESIAN_POINT('Ctrl Pts',(139.078006834899,-1.98552254007584,340.573655066951));
#11512=CARTESIAN_POINT('Ctrl Pts',(139.070582722762,-1.83728628336381,340.626461784522));
#11513=CARTESIAN_POINT('Ctrl Pts',(139.063158610625,-1.68711078041681,340.673290599943));
#11514=CARTESIAN_POINT('Ctrl Pts',(139.055734498488,-1.53552244745772,340.714026721661));
#11515=CARTESIAN_POINT('Ctrl Pts',(139.051877373334,-1.45676620544673,340.735190776954));
#11516=CARTESIAN_POINT('Ctrl Pts',(139.04802024818,-1.37762875574112,340.754711126236));
#11517=CARTESIAN_POINT('Ctrl Pts',(139.044163123025,-1.29818458327537,340.772577184434));
#11518=CARTESIAN_POINT('Ctrl Pts',(139.036739145587,-1.14527491081934,340.806964767843));
#11519=CARTESIAN_POINT('Ctrl Pts',(139.029315168149,-0.990767285094664,
340.83532439937));
#11520=CARTESIAN_POINT('Ctrl Pts',(139.021891190711,-0.835178228691196,
340.857508675949));
#11521=CARTESIAN_POINT('Ctrl Pts',(139.014475974684,-0.679772790783808,
340.879666771744));
#11522=CARTESIAN_POINT('Ctrl Pts',(139.007060758656,-0.523288828476869,
340.895663967));
#11523=CARTESIAN_POINT('Ctrl Pts',(138.999645542629,-0.366255729886668,
340.905403229486));
#11524=CARTESIAN_POINT('Ctrl Pts',(138.992237461484,-0.209373727753261,
340.915133120903));
#11525=CARTESIAN_POINT('Ctrl Pts',(138.98482938034,-0.0519440112410602,
340.918617043992));
#11526=CARTESIAN_POINT('Ctrl Pts',(138.977421299196,0.105496290076524,340.915809420128));
#11527=CARTESIAN_POINT('Ctrl Pts',(138.970018732022,0.262819405702351,340.913003886031));
#11528=CARTESIAN_POINT('Ctrl Pts',(138.962616164848,0.42015271889278,340.903916135971));
#11529=CARTESIAN_POINT('Ctrl Pts',(138.955213597674,0.576956567449006,340.888552596503));
#11530=CARTESIAN_POINT('Ctrl Pts',(138.947814927919,0.733677859464217,340.873197145871));
#11531=CARTESIAN_POINT('Ctrl Pts',(138.940416258165,0.889869871516724,340.851572522595));
#11532=CARTESIAN_POINT('Ctrl Pts',(138.93301758841,1.04499564704305,340.823737172998));
#11533=CARTESIAN_POINT('Ctrl Pts',(138.925620139206,1.20009583163343,340.79590641537));
#11534=CARTESIAN_POINT('Ctrl Pts',(138.918222690002,1.35412976180707,340.761867030727));
#11535=CARTESIAN_POINT('Ctrl Pts',(138.910825240798,1.5065681712928,340.721729013834));
#11536=CARTESIAN_POINT('Ctrl Pts',(138.903428112334,1.6589999713148,340.681592737255));
#11537=CARTESIAN_POINT('Ctrl Pts',(138.896030983871,1.80983602728958,340.635358449223));
#11538=CARTESIAN_POINT('Ctrl Pts',(138.888633855407,1.95856005639423,340.583186640978));
#11539=CARTESIAN_POINT('Ctrl Pts',(138.881235587971,2.10730698528692,340.531006799577));
#11540=CARTESIAN_POINT('Ctrl Pts',(138.873837320534,2.25394088760211,340.472887741158));
#11541=CARTESIAN_POINT('Ctrl Pts',(138.866439053098,2.39796349937133,340.409038881186));
#11542=CARTESIAN_POINT('Ctrl Pts',(138.859038186572,2.54203670779859,340.345167590438));
#11543=CARTESIAN_POINT('Ctrl Pts',(138.851637320046,2.68349645821875,340.27556264154));
#11544=CARTESIAN_POINT('Ctrl Pts',(138.84423645352,2.82186735004229,340.200480287557));
#11545=CARTESIAN_POINT('Ctrl Pts',(138.836827460135,2.96039018633387,340.125315485971));
#11546=CARTESIAN_POINT('Ctrl Pts',(138.829418466751,3.09581706207243,340.044661445695));
#11547=CARTESIAN_POINT('Ctrl Pts',(138.822009473366,3.2276993106918,339.958819186284));
#11548=CARTESIAN_POINT('Ctrl Pts',(138.814595915786,3.35966280332542,339.87292404508));
#11549=CARTESIAN_POINT('Ctrl Pts',(138.807182358205,3.4880770140096,339.781834531468));
#11550=CARTESIAN_POINT('Ctrl Pts',(138.799768800625,3.61252527881023,339.685892836211));
#11551=CARTESIAN_POINT('Ctrl Pts',(138.792344688488,3.73715071849896,339.589814550387));
#11552=CARTESIAN_POINT('Ctrl Pts',(138.784920576352,3.85779865014862,339.488870525167));
#11553=CARTESIAN_POINT('Ctrl Pts',(138.777496464215,3.9740876690689,339.383441314887));
#11554=CARTESIAN_POINT('Ctrl Pts',(138.77363933906,4.0345044962691,339.328666595498));
#11555=CARTESIAN_POINT('Ctrl Pts',(138.769782213906,4.09374538937467,339.272681806787));
#11556=CARTESIAN_POINT('Ctrl Pts',(138.765925088751,4.15176113909933,339.215543856534));
#11557=CARTESIAN_POINT('Ctrl Pts',(138.758501111313,4.26342658933596,339.105567945323));
#11558=CARTESIAN_POINT('Ctrl Pts',(138.751077133875,4.37088775043844,338.990986210471));
#11559=CARTESIAN_POINT('Ctrl Pts',(138.743653156437,4.47374114801233,338.872153238585));
#11560=CARTESIAN_POINT('Ctrl Pts',(138.73623794041,4.57647316310195,338.753460507485));
#11561=CARTESIAN_POINT('Ctrl Pts',(138.728822724382,4.67460799692951,338.630526805414));
#11562=CARTESIAN_POINT('Ctrl Pts',(138.721407508354,4.76777757073667,338.503744796426));
#11563=CARTESIAN_POINT('Ctrl Pts',(138.71399942721,4.86085749724903,338.377084776448));
#11564=CARTESIAN_POINT('Ctrl Pts',(138.706591346066,4.94898145541993,338.246584119908));
#11565=CARTESIAN_POINT('Ctrl Pts',(138.699183264922,5.03182044558077,338.112669845315));
#11566=CARTESIAN_POINT('Ctrl Pts',(138.691780697748,5.11459777716832,337.978855245563));
#11567=CARTESIAN_POINT('Ctrl Pts',(138.684378130574,5.19209777781471,337.841632402929));
#11568=CARTESIAN_POINT('Ctrl Pts',(138.6769755634,5.26403380956595,337.701458608649));
#11569=CARTESIAN_POINT('Ctrl Pts',(138.669576893645,5.33593196731082,337.56135861526));
#11570=CARTESIAN_POINT('Ctrl Pts',(138.662178223891,5.40227182027408,337.418311095639));
#11571=CARTESIAN_POINT('Ctrl Pts',(138.654779554136,5.46281193920951,337.272799216678));
#11572=CARTESIAN_POINT('Ctrl Pts',(138.647382104932,5.52334207090526,337.127311342657));
#11573=CARTESIAN_POINT('Ctrl Pts',(138.639984655728,5.57807422424232,336.979360260395));
#11574=CARTESIAN_POINT('Ctrl Pts',(138.632587206524,5.6268144798169,336.829450565668));
#11575=CARTESIAN_POINT('Ctrl Pts',(138.625190078061,5.67555262209895,336.679547370764));
#11576=CARTESIAN_POINT('Ctrl Pts',(138.617792949597,5.71829926778662,336.527686087172));
#11577=CARTESIAN_POINT('Ctrl Pts',(138.610395821134,5.75490998712807,336.374387719151));
#11578=CARTESIAN_POINT('Ctrl Pts',(138.602997553697,5.79152634360639,336.221065747008));
#11579=CARTESIAN_POINT('Ctrl Pts',(138.59559928626,5.82200480586053,336.066306612873));
#11580=CARTESIAN_POINT('Ctrl Pts',(138.588201018824,5.84625183659871,335.910642644272));
#11581=CARTESIAN_POINT('Ctrl Pts',(138.580800152298,5.87050738557378,335.754923989281));
#11582=CARTESIAN_POINT('Ctrl Pts',(138.573399285772,5.8885270869998,335.598300235461));
#11583=CARTESIAN_POINT('Ctrl Pts',(138.565998419247,5.9002691630095,335.441309830549));
#11584=CARTESIAN_POINT('Ctrl Pts',(138.558589425862,5.91202413294125,335.284147035163));
#11585=CARTESIAN_POINT('Ctrl Pts',(138.551180432477,5.91748768304993,335.126617157028));
#11586=CARTESIAN_POINT('Ctrl Pts',(138.543771439092,5.91667014787691,334.969260388385));
#11587=CARTESIAN_POINT('Ctrl Pts',(138.536357881512,5.91585210907402,334.811806682545));
#11588=CARTESIAN_POINT('Ctrl Pts',(138.528944323932,5.90874529157503,334.654526670653));
#11589=CARTESIAN_POINT('Ctrl Pts',(138.521530766352,5.89541197013135,334.497955913358));
#11590=CARTESIAN_POINT('Ctrl Pts',(138.514106654215,5.88205966626361,334.341162248927));
#11591=CARTESIAN_POINT('Ctrl Pts',(138.506682542078,5.86246320050229,334.185080225078));
#11592=CARTESIAN_POINT('Ctrl Pts',(138.499258429942,5.83673618914445,334.030236512942));
#11593=CARTESIAN_POINT('Ctrl Pts',(138.495401304787,5.82336997095747,333.949788970376));
#11594=CARTESIAN_POINT('Ctrl Pts',(138.491544179632,5.80834981424833,333.869675457934));
#11595=CARTESIAN_POINT('Ctrl Pts',(138.487687054477,5.79169694401467,333.789968152819));
#11596=CARTESIAN_POINT('Ctrl Pts',(138.480263077039,5.75964443652942,333.636552017465));
#11597=CARTESIAN_POINT('Ctrl Pts',(138.472839099601,5.72144361159046,333.484178883083));
#11598=CARTESIAN_POINT('Ctrl Pts',(138.465415122163,5.67717430549523,333.333379927061));
#11599=CARTESIAN_POINT('Ctrl Pts',(138.457999906136,5.63295724384186,333.182758936495));
#11600=CARTESIAN_POINT('Ctrl Pts',(138.450584690108,5.58268606065472,333.033708780989));
#11601=CARTESIAN_POINT('Ctrl Pts',(138.443169474081,5.52649176697713,332.886751478876));
#11602=CARTESIAN_POINT('Ctrl Pts',(138.435761392936,5.47035154316597,332.739935578338));
#11603=CARTESIAN_POINT('Ctrl Pts',(138.428353311792,5.4082996872901,332.59520886849));
#11604=CARTESIAN_POINT('Ctrl Pts',(138.420945230648,5.34051724772555,332.45307909639));
#11605=CARTESIAN_POINT('Ctrl Pts',(138.413542663474,5.27278525986872,332.311055114075));
#11606=CARTESIAN_POINT('Ctrl Pts',(138.4061400963,5.19933134127639,332.171624556147));
#11607=CARTESIAN_POINT('Ctrl Pts',(138.398737529126,5.120384921659,332.035275929105));
#11608=CARTESIAN_POINT('Ctrl Pts',(138.391338859372,5.04148006698646,331.898999089018));
#11609=CARTESIAN_POINT('Ctrl Pts',(138.383940189617,4.95708865697102,331.76580127043));
#11610=CARTESIAN_POINT('Ctrl Pts',(138.376541519862,4.8674863457395,331.636146965675));
#11611=CARTESIAN_POINT('Ctrl Pts',(138.369144070658,4.77789881610706,331.506514049853));
#11612=CARTESIAN_POINT('Ctrl Pts',(138.361746621454,4.68310230333574,331.380423794409));
#11613=CARTESIAN_POINT('Ctrl Pts',(138.35434917225,4.58341619186373,331.258312336036));
#11614=CARTESIAN_POINT('Ctrl Pts',(138.346952043787,4.48373440260772,331.136206172202));
#11615=CARTESIAN_POINT('Ctrl Pts',(138.339554915323,4.37916367220048,331.018078751534));
#11616=CARTESIAN_POINT('Ctrl Pts',(138.33215778686,4.27006396501272,330.904333473389));
#11617=CARTESIAN_POINT('Ctrl Pts',(138.324759519423,4.1609474591935,330.790570681311));
#11618=CARTESIAN_POINT('Ctrl Pts',(138.317361251987,4.04730084643777,330.681191644615));
#11619=CARTESIAN_POINT('Ctrl Pts',(138.30996298455,3.9295211539225,330.576563093773));
#11620=CARTESIAN_POINT('Ctrl Pts',(138.302562118024,3.8117000841626,330.47189778582));
#11621=CARTESIAN_POINT('Ctrl Pts',(138.295161251498,3.68974332256651,330.371986534196));
#11622=CARTESIAN_POINT('Ctrl Pts',(138.287760384973,3.56408105292134,330.277155855768));
#11623=CARTESIAN_POINT('Ctrl Pts',(138.280351391588,3.43828079409031,330.182221044188));
#11624=CARTESIAN_POINT('Ctrl Pts',(138.272942398203,3.30876719927659,330.092378172221));
#11625=CARTESIAN_POINT('Ctrl Pts',(138.265533404818,3.17600012027299,330.007910878347));
#11626=CARTESIAN_POINT('Ctrl Pts',(138.258119847238,3.04315125216899,329.923391549706));
#11627=CARTESIAN_POINT('Ctrl Pts',(138.250706289658,2.90704522800942,329.844254584999));
#11628=CARTESIAN_POINT('Ctrl Pts',(138.243292732078,2.76816611261098,329.770737438654));
#11629=CARTESIAN_POINT('Ctrl Pts',(138.235868619941,2.6290892773668,329.697115627193));
#11630=CARTESIAN_POINT('Ctrl Pts',(138.228444507804,2.48723180158059,329.629129774235));
#11631=CARTESIAN_POINT('Ctrl Pts',(138.221020395668,2.34309805853791,329.56696934938));
#11632=CARTESIAN_POINT('Ctrl Pts',(138.217163270513,2.26821477610547,329.534674506047));
#11633=CARTESIAN_POINT('Ctrl Pts',(138.213306145358,2.19271734569308,329.50395125777));
#11634=CARTESIAN_POINT('Ctrl Pts',(138.209449020203,2.11667794871525,329.47482081522));
#11635=CARTESIAN_POINT('Ctrl Pts',(138.202025042765,1.97032159653299,329.418752178719));
#11636=CARTESIAN_POINT('Ctrl Pts',(138.194601065327,1.82151511875569,329.368418221206));
#11637=CARTESIAN_POINT('Ctrl Pts',(138.187177087889,1.67074839778092,329.3240392572));
#11638=CARTESIAN_POINT('Ctrl Pts',(138.179761871862,1.52015960422103,329.279712667048));
#11639=CARTESIAN_POINT('Ctrl Pts',(138.172346655834,1.36761552682853,329.241327185838));
#11640=CARTESIAN_POINT('Ctrl Pts',(138.164931439806,1.21362603954763,329.209055137663));
#11641=CARTESIAN_POINT('Ctrl Pts',(138.157523358662,1.05978472017605,329.176814141489));
#11642=CARTESIAN_POINT('Ctrl Pts',(138.150115277518,0.904501122506735,329.150674943798));
#11643=CARTESIAN_POINT('Ctrl Pts',(138.142707196374,0.74830019753795,329.130760068215));
#11644=CARTESIAN_POINT('Ctrl Pts',(138.1353046292,0.592215535770415,329.110860015637));
#11645=CARTESIAN_POINT('Ctrl Pts',(138.127902062026,0.43521527485345,329.097175107434));
#11646=CARTESIAN_POINT('Ctrl Pts',(138.120499494852,0.277834367903025,329.089776770162));
#11647=CARTESIAN_POINT('Ctrl Pts',(138.113100825097,0.120536321312057,329.082382328083));
#11648=CARTESIAN_POINT('Ctrl Pts',(138.105702155343,-0.0371416003263249,
329.08126788265));
#11649=CARTESIAN_POINT('Ctrl Pts',(138.098303485588,-0.19465962323581,329.086452993881));
#11650=CARTESIAN_POINT('Ctrl Pts',(138.090906036384,-0.352151660562655,
329.091637249729));
#11651=CARTESIAN_POINT('Ctrl Pts',(138.08350858718,-0.509483478866495,329.103118987435));
#11652=CARTESIAN_POINT('Ctrl Pts',(138.076111137976,-0.666115484251976,
329.120865648402));
#11653=CARTESIAN_POINT('Ctrl Pts',(138.068714009513,-0.822740698346717,
329.138611539905));
#11654=CARTESIAN_POINT('Ctrl Pts',(138.061316881049,-0.978665789015709,
329.162621772549));
#11655=CARTESIAN_POINT('Ctrl Pts',(138.053919752586,-1.13335673175562,329.192811947157));
#11656=CARTESIAN_POINT('Ctrl Pts',(138.046521485149,-1.28807149303932,329.223006770298));
#11657=CARTESIAN_POINT('Ctrl Pts',(138.039123217712,-1.4415513617005,329.259383358584));
#11658=CARTESIAN_POINT('Ctrl Pts',(138.031724950276,-1.59327309207363,329.301806302294));
#11659=CARTESIAN_POINT('Ctrl Pts',(138.02432408375,-1.74504812388613,329.34424414963));
#11660=CARTESIAN_POINT('Ctrl Pts',(138.016923217224,-1.89506342846661,329.39273248113));
#11661=CARTESIAN_POINT('Ctrl Pts',(138.009522350698,-2.04281163368548,329.447086243081));
#11662=CARTESIAN_POINT('Ctrl Pts',(138.002113357314,-2.19072208055903,329.501499690659));
#11663=CARTESIAN_POINT('Ctrl Pts',(137.994704363929,-2.33636010595233,329.561791302385));
#11664=CARTESIAN_POINT('Ctrl Pts',(137.987295370544,-2.47923834002398,329.627727872133));
#11665=CARTESIAN_POINT('Ctrl Pts',(137.979881812964,-2.62220459201622,329.693705061083));
#11666=CARTESIAN_POINT('Ctrl Pts',(137.972468255384,-2.76240733338685,329.765333968012));
#11667=CARTESIAN_POINT('Ctrl Pts',(137.965054697803,-2.89938492839136,329.842336032707));
#11668=CARTESIAN_POINT('Ctrl Pts',(137.957630585667,-3.03655753607932,329.919447723937));
#11669=CARTESIAN_POINT('Ctrl Pts',(137.95020647353,-3.17049551017452,330.00194765566));
#11670=CARTESIAN_POINT('Ctrl Pts',(137.942782361393,-3.30076657632252,330.08951422249));
#11671=CARTESIAN_POINT('Ctrl Pts',(137.938925236239,-3.36844763998588,330.135008579446));
#11672=CARTESIAN_POINT('Ctrl Pts',(137.935068111084,-3.43513946655055,330.181869866803));
#11673=CARTESIAN_POINT('Ctrl Pts',(137.931210985929,-3.50078515800388,330.230048863982));
#11674=CARTESIAN_POINT('Ctrl Pts',(137.923853689573,-3.62600142327591,330.321948179196));
#11675=CARTESIAN_POINT('Ctrl Pts',(137.916496393216,-3.74780208890084,330.418932458763));
#11676=CARTESIAN_POINT('Ctrl Pts',(137.90913909686,-3.86574122611928,330.520717095876));
#11677=CARTESIAN_POINT('Ctrl Pts',(137.901790515492,-3.9835406600795,330.622381165331));
#11678=CARTESIAN_POINT('Ctrl Pts',(137.894441934124,-4.09748738239249,330.728834031429));
#11679=CARTESIAN_POINT('Ctrl Pts',(137.887093352756,-4.20716463146982,330.839748045345));
#11680=CARTESIAN_POINT('Ctrl Pts',(137.879751801412,-4.31673695776895,330.950555953332));
#11681=CARTESIAN_POINT('Ctrl Pts',(137.872410250067,-4.42204767382149,331.065816246674));
#11682=CARTESIAN_POINT('Ctrl Pts',(137.865068698722,-4.52271347061143,331.185161415571));
#11683=CARTESIAN_POINT('Ctrl Pts',(137.857732498819,-4.62330588956094,331.304419590761));
#11684=CARTESIAN_POINT('Ctrl Pts',(137.850396298917,-4.71925988458935,331.427756424704));
#11685=CARTESIAN_POINT('Ctrl Pts',(137.843060099014,-4.81022952951789,331.554768159346));
#11686=CARTESIAN_POINT('Ctrl Pts',(137.835727033594,-4.90116030653324,331.681725626644));
#11687=CARTESIAN_POINT('Ctrl Pts',(137.828393968174,-4.98711074909594,331.81235456212));
#11688=CARTESIAN_POINT('Ctrl Pts',(137.821060902754,-5.06777577911225,331.946218865874));
#11689=CARTESIAN_POINT('Ctrl Pts',(137.81372937577,-5.14842388606251,332.080055085656));
#11690=CARTESIAN_POINT('Ctrl Pts',(137.806397848785,-5.2237885900084,332.217124997622));
#11691=CARTESIAN_POINT('Ctrl Pts',(137.799066321801,-5.2936087853043,332.356964512034));
#11692=CARTESIAN_POINT('Ctrl Pts',(137.791734821713,-5.363428724454,332.496803513422));
#11693=CARTESIAN_POINT('Ctrl Pts',(137.784403321626,-5.42770402531529,332.639411756516));
#11694=CARTESIAN_POINT('Ctrl Pts',(137.777071821538,-5.4862202114806,332.78430183607));
#11695=CARTESIAN_POINT('Ctrl Pts',(137.769738837051,-5.54474824534539,332.929221251338));
#11696=CARTESIAN_POINT('Ctrl Pts',(137.762405852564,-5.5975147017393,333.076423069507));
#11697=CARTESIAN_POINT('Ctrl Pts',(137.755072868076,-5.64435388013823,333.225401499418));
#11698=CARTESIAN_POINT('Ctrl Pts',(137.747732768696,-5.69123850466704,333.374524476977));
#11699=CARTESIAN_POINT('Ctrl Pts',(137.740392669315,-5.7321842498568,333.525427145767));
#11700=CARTESIAN_POINT('Ctrl Pts',(137.733052569934,-5.76707562313242,333.677589579755));
#11701=CARTESIAN_POINT('Ctrl Pts',(137.725708798612,-5.80198445108681,333.829828134175));
#11702=CARTESIAN_POINT('Ctrl Pts',(137.71836502729,-5.83083280290243,333.983327335639));
#11703=CARTESIAN_POINT('Ctrl Pts',(137.711021255968,-5.85355676798457,334.137559435971));
#11704=CARTESIAN_POINT('Ctrl Pts',(137.703666819554,-5.87631373425489,334.292015521975));
#11705=CARTESIAN_POINT('Ctrl Pts',(137.696312383139,-5.89292850420375,334.447206255056));
#11706=CARTESIAN_POINT('Ctrl Pts',(137.688957946725,-5.9033891956881,334.602600243164));
#11707=CARTESIAN_POINT('Ctrl Pts',(137.682655966051,-5.91235291117344,334.735756593261));
#11708=CARTESIAN_POINT('Ctrl Pts',(137.676353985377,-5.91679874913726,334.869062031968));
#11709=CARTESIAN_POINT('Ctrl Pts',(137.670052004703,-5.9167495966891,335.002184623396));
#11710=CARTESIAN_POINT('',(135.920052004703,-5.91701510194892,334.994566743858));
#11711=CARTESIAN_POINT('Ctrl Pts',(137.670052004703,-5.92552048316578,335.002187861844));
#11712=CARTESIAN_POINT('Ctrl Pts',(137.664358987021,-5.92609142514278,335.122625259287));
#11713=CARTESIAN_POINT('Ctrl Pts',(137.658665969338,-5.92273849818748,335.243030259708));
#11714=CARTESIAN_POINT('Ctrl Pts',(137.560226940231,-5.79517465950716,337.320703036502));
#11715=CARTESIAN_POINT('Ctrl Pts',(137.374734917381,-3.4185942150446,341.10457504779));
#11716=CARTESIAN_POINT('Ctrl Pts',(137.096496883108,3.28346990442389,341.178304646741));
#11717=CARTESIAN_POINT('Ctrl Pts',(136.818258848833,6.9723421565426,335.58229526301));
#11718=CARTESIAN_POINT('Ctrl Pts',(136.540020814561,4.26279892320134,329.451922111074));
#11719=CARTESIAN_POINT('Ctrl Pts',(136.261782780286,-2.35865196315249,328.412938148315));
#11720=CARTESIAN_POINT('Ctrl Pts',(136.055126510334,-5.66897159192276,332.13095423252));
#11721=CARTESIAN_POINT('Ctrl Pts',(135.941216251806,-5.92117244379854,334.545155774113));
#11722=CARTESIAN_POINT('Ctrl Pts',(135.920052004703,-5.91701510194892,334.994566743858));
#11723=CARTESIAN_POINT('',(134.170052004703,-5.90701886447581,335.000579480333));
#11724=CARTESIAN_POINT('Ctrl Pts',(135.920052004703,-5.91701510194892,334.994566743858));
#11725=CARTESIAN_POINT('Ctrl Pts',(135.848470240382,-5.90295413096146,336.514565540108));
#11726=CARTESIAN_POINT('Ctrl Pts',(135.684142464635,-4.53096395093087,340.026512027423));
#11727=CARTESIAN_POINT('Ctrl Pts',(135.427068677465,1.38457380943765,341.858248922823));
#11728=CARTESIAN_POINT('Ctrl Pts',(135.14883064319,6.51652016864368,337.547074363439));
#11729=CARTESIAN_POINT('Ctrl Pts',(134.870592608916,5.66835215276419,330.898487255479));
#11730=CARTESIAN_POINT('Ctrl Pts',(134.592354574642,-0.381578968966501,
328.013797854939));
#11731=CARTESIAN_POINT('Ctrl Pts',(134.358841039905,-5.16515039241891,330.973395682556));
#11732=CARTESIAN_POINT('Ctrl Pts',(134.218073516592,-5.9061263129331,333.97650851601));
#11733=CARTESIAN_POINT('Ctrl Pts',(134.170052004703,-5.90701886447581,335.000579480333));
#11734=CARTESIAN_POINT('',(132.42005275816,-5.91838694893146,335.005182949526));
#11735=CARTESIAN_POINT('Ctrl Pts',(134.170052004703,-5.90701886447581,335.000579480333));
#11736=CARTESIAN_POINT('Ctrl Pts',(134.125327505167,-5.90785013611822,335.954340817035));
#11737=CARTESIAN_POINT('Ctrl Pts',(133.987856994207,-5.23884552278572,338.884834317021));
#11738=CARTESIAN_POINT('Ctrl Pts',(133.75764047182,-0.629385110448728,341.96824922803));
#11739=CARTESIAN_POINT('Ctrl Pts',(133.479402437547,5.51915303955582,339.300182862063));
#11740=CARTESIAN_POINT('Ctrl Pts',(133.201164403272,6.60284590772511,332.685902154172));
#11741=CARTESIAN_POINT('Ctrl Pts',(132.922926368998,1.62720454421991,328.195234883371));
#11742=CARTESIAN_POINT('Ctrl Pts',(132.662555937229,-4.42628508806817,329.836565795096));
#11743=CARTESIAN_POINT('Ctrl Pts',(132.494931516886,-5.90453803129754,333.416645424348));
#11744=CARTESIAN_POINT('Ctrl Pts',(132.420053107966,-5.91914799116607,335.005176197054));
#11745=CARTESIAN_POINT('',(130.670050602533,-5.92092256589507,334.996739404803));
#11746=CARTESIAN_POINT('Ctrl Pts',(132.420052004703,-5.91674771716332,335.005197493878));
#11747=CARTESIAN_POINT('Ctrl Pts',(132.409195503532,-5.91654548053808,335.23542058194));
#11748=CARTESIAN_POINT('Ctrl Pts',(132.39833900236,-5.90290294749101,335.465076387483));
#11749=CARTESIAN_POINT('Ctrl Pts',(132.387482501188,-5.87603693698799,335.692907264829));
#11750=CARTESIAN_POINT('Ctrl Pts',(132.380471767609,-5.85868784458893,335.840032158642));
#11751=CARTESIAN_POINT('Ctrl Pts',(132.37346103403,-5.8358253124178,335.9863969032));
#11752=CARTESIAN_POINT('Ctrl Pts',(132.366450300451,-5.80751716224808,336.13166910919));
#11753=CARTESIAN_POINT('Ctrl Pts',(132.359026323013,-5.77754040363806,336.285504305964));
#11754=CARTESIAN_POINT('Ctrl Pts',(132.351602345575,-5.74140179668153,336.438379667599));
#11755=CARTESIAN_POINT('Ctrl Pts',(132.344178368137,-5.69917399358948,336.589762986515));
#11756=CARTESIAN_POINT('Ctrl Pts',(132.336763152109,-5.65699602565854,336.740967650338));
#11757=CARTESIAN_POINT('Ctrl Pts',(132.329347936081,-5.6087432650755,336.890683420422));
#11758=CARTESIAN_POINT('Ctrl Pts',(132.321932720054,-5.55453965787506,337.038386555978));
#11759=CARTESIAN_POINT('Ctrl Pts',(132.31452463891,-5.50038820511271,337.185947572321));
#11760=CARTESIAN_POINT('Ctrl Pts',(132.307116557766,-5.44029743259817,337.331499461419));
#11761=CARTESIAN_POINT('Ctrl Pts',(132.299708476621,-5.3744415119523,337.474532076394));
#11762=CARTESIAN_POINT('Ctrl Pts',(132.292305909447,-5.30863460907078,337.617458229582));
#11763=CARTESIAN_POINT('Ctrl Pts',(132.284903342273,-5.23707125769066,337.757868504776));
#11764=CARTESIAN_POINT('Ctrl Pts',(132.277500775099,-5.15997426631245,337.895271340219));
#11765=CARTESIAN_POINT('Ctrl Pts',(132.270102105345,-5.08291786616336,338.032601833669));
#11766=CARTESIAN_POINT('Ctrl Pts',(132.26270343559,-5.00033381046468,338.166927716154));
#11767=CARTESIAN_POINT('Ctrl Pts',(132.255304765835,-4.9124914523721,338.297780813346));
#11768=CARTESIAN_POINT('Ctrl Pts',(132.247907316631,-4.82466358554092,338.42861232384));
#11769=CARTESIAN_POINT('Ctrl Pts',(132.240509867427,-4.73157934574908,338.555971876501));
#11770=CARTESIAN_POINT('Ctrl Pts',(132.233112418223,-4.63355219558828,338.679419059207));
#11771=CARTESIAN_POINT('Ctrl Pts',(132.22571528976,-4.53552929571385,338.802860889459));
#11772=CARTESIAN_POINT('Ctrl Pts',(132.218318161296,-4.43256414368824,338.922390394772));
#11773=CARTESIAN_POINT('Ctrl Pts',(132.210921032833,-4.32501122064948,339.037599349088));
#11774=CARTESIAN_POINT('Ctrl Pts',(132.203522765396,-4.21744173714538,339.152826042707));
#11775=CARTESIAN_POINT('Ctrl Pts',(132.196124497959,-4.10528333078379,339.26373058789));
#11776=CARTESIAN_POINT('Ctrl Pts',(132.188726230523,-3.9889280375635,339.369940923358));
#11777=CARTESIAN_POINT('Ctrl Pts',(132.181325363997,-3.8725318675053,339.476188571634));
#11778=CARTESIAN_POINT('Ctrl Pts',(132.173924497471,-3.75193615050908,339.577738475338));
#11779=CARTESIAN_POINT('Ctrl Pts',(132.166523630946,-3.62756661948799,339.674258335145));
#11780=CARTESIAN_POINT('Ctrl Pts',(132.159114637561,-3.50306051883133,339.770884182987));
#11781=CARTESIAN_POINT('Ctrl Pts',(132.151705644176,-3.3747726233577,339.862468727317));
#11782=CARTESIAN_POINT('Ctrl Pts',(132.144296650791,-3.24315891061265,339.948722142434));
#11783=CARTESIAN_POINT('Ctrl Pts',(132.136883093211,-3.11146411928061,340.035028692629));
#11784=CARTESIAN_POINT('Ctrl Pts',(132.129469535631,-2.97643974746237,340.115997378002));
#11785=CARTESIAN_POINT('Ctrl Pts',(132.122055978051,-2.83856660751528,340.191384225541));
#11786=CARTESIAN_POINT('Ctrl Pts',(132.114631865914,-2.70049717991261,340.266878400059));
#11787=CARTESIAN_POINT('Ctrl Pts',(132.107207753777,-2.55957121749573,340.336774700076));
#11788=CARTESIAN_POINT('Ctrl Pts',(132.09978364164,-2.41629048756569,340.400876858641));
#11789=CARTESIAN_POINT('Ctrl Pts',(132.095926516486,-2.34185037979742,340.434180510807));
#11790=CARTESIAN_POINT('Ctrl Pts',(132.092069391332,-2.2667749461058,340.465921009197));
#11791=CARTESIAN_POINT('Ctrl Pts',(132.088212266178,-2.19113607473682,340.496076169822));
#11792=CARTESIAN_POINT('Ctrl Pts',(132.08078828874,-2.0455506316899,340.554117126017));
#11793=CARTESIAN_POINT('Ctrl Pts',(132.073364311302,-1.8974378047827,340.60645703061));
#11794=CARTESIAN_POINT('Ctrl Pts',(132.065940333864,-1.74728445500175,340.652868970338));
#11795=CARTESIAN_POINT('Ctrl Pts',(132.058525117836,-1.59730830876518,340.699226136994));
#11796=CARTESIAN_POINT('Ctrl Pts',(132.051109901808,-1.44529678616297,340.739669155073));
#11797=CARTESIAN_POINT('Ctrl Pts',(132.043694685781,-1.29175738630769,340.774018827248));
#11798=CARTESIAN_POINT('Ctrl Pts',(132.036286604637,-1.13836572128988,340.808335448343));
#11799=CARTESIAN_POINT('Ctrl Pts',(132.028878523493,-0.983449467519565,
340.836570314711));
#11800=CARTESIAN_POINT('Ctrl Pts',(132.021470442348,-0.827531872647,340.858593821238));
#11801=CARTESIAN_POINT('Ctrl Pts',(132.014067875174,-0.671730330088032,
340.880600935268));
#11802=CARTESIAN_POINT('Ctrl Pts',(132.006665308,-0.514929298420526,340.896405843003));
#11803=CARTESIAN_POINT('Ctrl Pts',(131.999262740826,-0.35766271687783,340.905929896592));
#11804=CARTESIAN_POINT('Ctrl Pts',(131.991864071072,-0.200478935502596,
340.915448935808));
#11805=CARTESIAN_POINT('Ctrl Pts',(131.984465401317,-0.042830463993784,
340.918693684148));
#11806=CARTESIAN_POINT('Ctrl Pts',(131.977066731562,0.11474323742012,340.915637290433));
#11807=CARTESIAN_POINT('Ctrl Pts',(131.969669282358,0.272290944065933,340.912581400929));
#11808=CARTESIAN_POINT('Ctrl Pts',(131.962271833154,0.429763532319038,340.903226439658));
#11809=CARTESIAN_POINT('Ctrl Pts',(131.95487438395,0.586621017634842,340.887597671731));
#11810=CARTESIAN_POINT('Ctrl Pts',(131.947477255487,0.743471701883489,340.87196958144));
#11811=CARTESIAN_POINT('Ctrl Pts',(131.940080127023,0.899706964850715,340.850068262363));
#11812=CARTESIAN_POINT('Ctrl Pts',(131.93268299856,1.05479169045151,340.821970890708));
#11813=CARTESIAN_POINT('Ctrl Pts',(131.925284731123,1.20990029522872,340.79386919276));
#11814=CARTESIAN_POINT('Ctrl Pts',(131.917886463687,1.36385764264725,340.759569609156));
#11815=CARTESIAN_POINT('Ctrl Pts',(131.91048819625,1.51613870526667,340.719200467626));
#11816=CARTESIAN_POINT('Ctrl Pts',(131.903087329724,1.66847326582496,340.678817143992));
#11817=CARTESIAN_POINT('Ctrl Pts',(131.895686463198,1.81913000856909,340.6323601126));
#11818=CARTESIAN_POINT('Ctrl Pts',(131.888285596673,1.96759910739992,340.580007555108));
#11819=CARTESIAN_POINT('Ctrl Pts',(131.880876603288,2.11623123949537,340.527597509502));
#11820=CARTESIAN_POINT('Ctrl Pts',(131.873467609903,2.26267057809113,340.469279133354));
#11821=CARTESIAN_POINT('Ctrl Pts',(131.866058616518,2.40642664695764,340.405279026592));
#11822=CARTESIAN_POINT('Ctrl Pts',(131.858645058938,2.5502712745213,340.341239493556));
#11823=CARTESIAN_POINT('Ctrl Pts',(131.851231501358,2.69142900472983,340.271511420314));
#11824=CARTESIAN_POINT('Ctrl Pts',(131.843817943777,2.82943448031721,340.196367104439));
#11825=CARTESIAN_POINT('Ctrl Pts',(131.836393831641,2.96763643196422,340.121115806873));
#11826=CARTESIAN_POINT('Ctrl Pts',(131.828969719504,3.10267684641389,340.040433057142));
#11827=CARTESIAN_POINT('Ctrl Pts',(131.821545607367,3.23411914352195,339.954634590765));
#11828=CARTESIAN_POINT('Ctrl Pts',(131.817688482213,3.30240870882434,339.910058833179));
#11829=CARTESIAN_POINT('Ctrl Pts',(131.813831357058,3.3697275960796,339.864102904267));
#11830=CARTESIAN_POINT('Ctrl Pts',(131.809974231903,3.43601824744375,339.81681525136));
#11831=CARTESIAN_POINT('Ctrl Pts',(131.802550254465,3.56361076268136,339.725798638159));
#11832=CARTESIAN_POINT('Ctrl Pts',(131.795126277027,3.68777685442863,339.629571527803));
#11833=CARTESIAN_POINT('Ctrl Pts',(131.787702299589,3.80806223806477,339.528420536294));
#11834=CARTESIAN_POINT('Ctrl Pts',(131.780287083562,3.92820566685031,339.427388918174));
#11835=CARTESIAN_POINT('Ctrl Pts',(131.772871867534,4.04447722086647,339.321445223496));
#11836=CARTESIAN_POINT('Ctrl Pts',(131.765456651506,4.15645157236773,339.210919245137));
#11837=CARTESIAN_POINT('Ctrl Pts',(131.758048570362,4.26831818271177,339.100499614317));
#11838=CARTESIAN_POINT('Ctrl Pts',(131.750640489218,4.37589555821339,338.985506737836));
#11839=CARTESIAN_POINT('Ctrl Pts',(131.743232408074,4.47879155183845,338.866310489043));
#11840=CARTESIAN_POINT('Ctrl Pts',(131.7358298409,4.58161095809617,338.747202960194));
#11841=CARTESIAN_POINT('Ctrl Pts',(131.728427273726,4.67975567766997,338.623898569922));
#11842=CARTESIAN_POINT('Ctrl Pts',(131.721024706552,4.77287062874716,338.496803758254));
#11843=CARTESIAN_POINT('Ctrl Pts',(131.713626036797,4.86593655520969,338.36977586145));
#11844=CARTESIAN_POINT('Ctrl Pts',(131.706227367043,4.95397776711305,338.238961817986));
#11845=CARTESIAN_POINT('Ctrl Pts',(131.698828697288,5.03667975184522,338.104800740765));
#11846=CARTESIAN_POINT('Ctrl Pts',(131.691431248084,5.11936809331791,337.970661795955));
#11847=CARTESIAN_POINT('Ctrl Pts',(131.68403379888,5.1967187600848,337.833177230632));
#11848=CARTESIAN_POINT('Ctrl Pts',(131.676636349676,5.26846078149481,337.692814801718));
#11849=CARTESIAN_POINT('Ctrl Pts',(131.669239221213,5.34019969229583,337.552458458674));
#11850=CARTESIAN_POINT('Ctrl Pts',(131.661842092749,5.40633027140921,337.409224832462));
#11851=CARTESIAN_POINT('Ctrl Pts',(131.654444964286,5.46662783593587,337.263605678088));
#11852=CARTESIAN_POINT('Ctrl Pts',(131.647046696849,5.52693468478226,337.117964101998));
#11853=CARTESIAN_POINT('Ctrl Pts',(131.639648429412,5.58140658793936,336.969936611221));
#11854=CARTESIAN_POINT('Ctrl Pts',(131.632250161976,5.62986733645778,336.820034158027));
#11855=CARTESIAN_POINT('Ctrl Pts',(131.62484929545,5.67834510974678,336.670079042526));
#11856=CARTESIAN_POINT('Ctrl Pts',(131.617448428924,5.72080740911297,336.518248008041));
#11857=CARTESIAN_POINT('Ctrl Pts',(131.610047562399,5.75712817515735,336.365066202537));
#11858=CARTESIAN_POINT('Ctrl Pts',(131.602638569014,5.79348882487528,336.211716188766));
#11859=CARTESIAN_POINT('Ctrl Pts',(131.595229575629,5.82369438700597,336.057012805153));
#11860=CARTESIAN_POINT('Ctrl Pts',(131.587820582244,5.84766998943229,335.901491129847));
#11861=CARTESIAN_POINT('Ctrl Pts',(131.580407024664,5.87166036165672,335.745873647825));
#11862=CARTESIAN_POINT('Ctrl Pts',(131.572993467084,5.88941308472895,335.589437239597));
#11863=CARTESIAN_POINT('Ctrl Pts',(131.565579909504,5.90090530796868,335.432720589858));
#11864=CARTESIAN_POINT('Ctrl Pts',(131.558155797367,5.91241389249212,335.275780825277));
#11865=CARTESIAN_POINT('Ctrl Pts',(131.55073168523,5.91764416382847,335.118560394351));
#11866=CARTESIAN_POINT('Ctrl Pts',(131.543307573094,5.91662537214471,334.961597289243));
#11867=CARTESIAN_POINT('Ctrl Pts',(131.539450447939,5.91609606884776,334.880048636699));
#11868=CARTESIAN_POINT('Ctrl Pts',(131.535593322784,5.91388086044975,334.798569358136));
#11869=CARTESIAN_POINT('Ctrl Pts',(131.531736197629,5.90998933949256,334.717234072802));
#11870=CARTESIAN_POINT('Ctrl Pts',(131.524312220191,5.90249915894961,334.560684492736));
#11871=CARTESIAN_POINT('Ctrl Pts',(131.516888242753,5.88877312582884,334.404196566294));
#11872=CARTESIAN_POINT('Ctrl Pts',(131.509464265315,5.86880642216648,334.24830741547));
#11873=CARTESIAN_POINT('Ctrl Pts',(131.502049049288,5.8488632822186,334.092602237299));
#11874=CARTESIAN_POINT('Ctrl Pts',(131.49463383326,5.82269417869338,333.937494794744));
#11875=CARTESIAN_POINT('Ctrl Pts',(131.487218617233,5.79034627220662,333.783521224828));
#11876=CARTESIAN_POINT('Ctrl Pts',(131.479810536088,5.7580294907126,333.629695807507));
#11877=CARTESIAN_POINT('Ctrl Pts',(131.472402454944,5.71954581828712,333.477002453631));
#11878=CARTESIAN_POINT('Ctrl Pts',(131.4649943738,5.67499407605729,333.325971087701));
#11879=CARTESIAN_POINT('Ctrl Pts',(131.457591806626,5.63047549450289,333.175052137174));
#11880=CARTESIAN_POINT('Ctrl Pts',(131.450189239452,5.57989794144367,333.025793067878));
#11881=CARTESIAN_POINT('Ctrl Pts',(131.442786672278,5.5234110458261,332.878712423704));
#11882=CARTESIAN_POINT('Ctrl Pts',(131.435388002523,5.46695389031218,332.731709216847));
#11883=CARTESIAN_POINT('Ctrl Pts',(131.427989332769,5.40459372193263,332.586882498454));
#11884=CARTESIAN_POINT('Ctrl Pts',(131.420590663014,5.33652959927374,332.444734378078));
#11885=CARTESIAN_POINT('Ctrl Pts',(131.41319321381,5.26847670508156,332.302609707728));
#11886=CARTESIAN_POINT('Ctrl Pts',(131.405795764606,5.19472188516404,332.16316309468));
#11887=CARTESIAN_POINT('Ctrl Pts',(131.398398315402,5.1155118485306,332.026875534048));
#11888=CARTESIAN_POINT('Ctrl Pts',(131.391001186939,5.03630524630629,331.890593882607));
#11889=CARTESIAN_POINT('Ctrl Pts',(131.383604058475,4.95164408519902,331.757471333909));
#11890=CARTESIAN_POINT('Ctrl Pts',(131.376206930012,4.86182030367583,331.627962945449));
#11891=CARTESIAN_POINT('Ctrl Pts',(131.368808662575,4.77198269153254,331.49843461593));
#11892=CARTESIAN_POINT('Ctrl Pts',(131.361410395138,4.67698108890476,331.372521861382));
#11893=CARTESIAN_POINT('Ctrl Pts',(131.354012127702,4.57714980968615,331.250649365265));
#11894=CARTESIAN_POINT('Ctrl Pts',(131.346611261176,4.4772834586893,331.128734054057));
#11895=CARTESIAN_POINT('Ctrl Pts',(131.33921039465,4.3725842892917,331.010862115805));
#11896=CARTESIAN_POINT('Ctrl Pts',(131.331809528124,4.26342569164432,330.89742374424));
#11897=CARTESIAN_POINT('Ctrl Pts',(131.32440053474,4.15414722742063,330.783860806498));
#11898=CARTESIAN_POINT('Ctrl Pts',(131.316991541355,4.04039981455201,330.674741427143));
#11899=CARTESIAN_POINT('Ctrl Pts',(131.30958254797,3.92259289407055,330.570418129226));
#11900=CARTESIAN_POINT('Ctrl Pts',(131.30216899039,3.80471340046252,330.466030564559));
#11901=CARTESIAN_POINT('Ctrl Pts',(131.29475543281,3.68276970446464,330.366445204179));
#11902=CARTESIAN_POINT('Ctrl Pts',(131.287341875229,3.55720243171438,330.271972776907));
#11903=CARTESIAN_POINT('Ctrl Pts',(131.279917763093,3.43145639096328,330.17736585084));
#11904=CARTESIAN_POINT('Ctrl Pts',(131.272493650956,3.30207677637937,330.08788660761));
#11905=CARTESIAN_POINT('Ctrl Pts',(131.265069538819,3.1695318259944,330.003801588557));
#11906=CARTESIAN_POINT('Ctrl Pts',(131.261212413665,3.10066938792222,329.96011603584));
#11907=CARTESIAN_POINT('Ctrl Pts',(131.25735528851,3.03095294792238,329.917885738931));
#11908=CARTESIAN_POINT('Ctrl Pts',(131.253498163355,2.96045044598856,329.877143012015));
#11909=CARTESIAN_POINT('Ctrl Pts',(131.246074185917,2.82475119779435,329.798723704043));
#11910=CARTESIAN_POINT('Ctrl Pts',(131.238650208479,2.6857292178045,329.725581621853));
#11911=CARTESIAN_POINT('Ctrl Pts',(131.231226231041,2.54383357608647,329.658011484505));
#11912=CARTESIAN_POINT('Ctrl Pts',(131.223811015014,2.40210539257502,329.590521090086));
#11913=CARTESIAN_POINT('Ctrl Pts',(131.216395798986,2.25751063155815,329.528589710304));
#11914=CARTESIAN_POINT('Ctrl Pts',(131.208980582958,2.11052566341192,329.472467821299));
#11915=CARTESIAN_POINT('Ctrl Pts',(131.201572501814,1.96368212346207,329.416399932492));
#11916=CARTESIAN_POINT('Ctrl Pts',(131.19416442067,1.81445330127638,329.366130538323));
#11917=CARTESIAN_POINT('Ctrl Pts',(131.186756339526,1.66333829945345,329.321863310551));
#11918=CARTESIAN_POINT('Ctrl Pts',(131.179353772352,1.51233577528602,329.277629031684));
#11919=CARTESIAN_POINT('Ctrl Pts',(131.171951205178,1.35945022351259,329.239388128197));
#11920=CARTESIAN_POINT('Ctrl Pts',(131.164548638004,1.20519867156313,329.207295387769));
#11921=CARTESIAN_POINT('Ctrl Pts',(131.157149968249,1.05102833238162,329.175219544029));
#11922=CARTESIAN_POINT('Ctrl Pts',(131.149751298495,0.89549378980647,329.149285492537));
#11923=CARTESIAN_POINT('Ctrl Pts',(131.14235262874,0.739125000495771,329.129597560972));
#11924=CARTESIAN_POINT('Ctrl Pts',(131.134955179536,0.582782007179798,329.109912877305));
#11925=CARTESIAN_POINT('Ctrl Pts',(131.127557730332,0.425605410196819,329.096472315099));
#11926=CARTESIAN_POINT('Ctrl Pts',(131.120160281128,0.268133197000217,329.089328705539));
#11927=CARTESIAN_POINT('Ctrl Pts',(131.112763152664,0.110667811524301,329.082185405714));
#11928=CARTESIAN_POINT('Ctrl Pts',(131.105366024201,-0.0470927918521481,
329.081338532585));
#11929=CARTESIAN_POINT('Ctrl Pts',(131.097968895738,-0.204607960918182,
329.086788846589));
#11930=CARTESIAN_POINT('Ctrl Pts',(131.090570628301,-0.362147383388201,
329.092239999805));
#11931=CARTESIAN_POINT('Ctrl Pts',(131.083172360864,-0.519440923290675,
329.103990257867));
#11932=CARTESIAN_POINT('Ctrl Pts',(131.075774093428,-0.675950538814617,
329.121988309677));
#11933=CARTESIAN_POINT('Ctrl Pts',(131.068373226902,-0.832515137812552,
329.139992684392));
#11934=CARTESIAN_POINT('Ctrl Pts',(131.060972360376,-0.988294893575073,
329.164249180318));
#11935=CARTESIAN_POINT('Ctrl Pts',(131.05357149385,-1.14275962103158,329.19465496193));
#11936=CARTESIAN_POINT('Ctrl Pts',(131.046162500466,-1.29739396552618,329.225094131998));
#11937=CARTESIAN_POINT('Ctrl Pts',(131.038753507081,-1.45071003151352,329.261696000736));
#11938=CARTESIAN_POINT('Ctrl Pts',(131.031344513696,-1.6021898028041,329.304307030897));
#11939=CARTESIAN_POINT('Ctrl Pts',(131.023930956116,-1.75376289085883,329.346944310922));
#11940=CARTESIAN_POINT('Ctrl Pts',(131.016517398536,-1.90349707599541,329.395598013733));
#11941=CARTESIAN_POINT('Ctrl Pts',(131.009103840955,-2.0508926119025,329.450065761025));
#11942=CARTESIAN_POINT('Ctrl Pts',(131.001679728819,-2.19849799233933,329.504611053128));
#11943=CARTESIAN_POINT('Ctrl Pts',(130.994255616682,-2.34375773017976,329.564986778395));
#11944=CARTESIAN_POINT('Ctrl Pts',(130.986831504545,-2.48619429465784,329.630943426289));
#11945=CARTESIAN_POINT('Ctrl Pts',(130.982974379391,-2.56019582449433,329.665210560328));
#11946=CARTESIAN_POINT('Ctrl Pts',(130.979117254236,-2.63343574812116,329.700983365228));
#11947=CARTESIAN_POINT('Ctrl Pts',(130.975260129081,-2.70585012562227,329.738222195857));
#11948=CARTESIAN_POINT('Ctrl Pts',(130.967836151643,-2.84522924431737,329.809897401438));
#11949=CARTESIAN_POINT('Ctrl Pts',(130.960412174205,-2.98196875210054,329.88722257275));
#11950=CARTESIAN_POINT('Ctrl Pts',(130.952988196767,-3.1155777958457,329.969979566589));
#11951=CARTESIAN_POINT('Ctrl Pts',(130.94557298074,-3.24902916081658,330.052638894723));
#11952=CARTESIAN_POINT('Ctrl Pts',(130.938157764712,-3.37935710135488,330.140717090834));
#11953=CARTESIAN_POINT('Ctrl Pts',(130.930742548685,-3.50609319538716,330.233949111921));
#11954=CARTESIAN_POINT('Ctrl Pts',(130.92333446754,-3.63270734458783,330.327091425626));
#11955=CARTESIAN_POINT('Ctrl Pts',(130.915926386396,-3.75573622902762,330.425377472217));
#11956=CARTESIAN_POINT('Ctrl Pts',(130.908518305252,-3.87473848372444,330.528497764146));
#11957=CARTESIAN_POINT('Ctrl Pts',(130.901115738078,-3.99365216286977,330.631541301759));
#11958=CARTESIAN_POINT('Ctrl Pts',(130.893713170904,-4.10854489908171,330.739411676776));
#11959=CARTESIAN_POINT('Ctrl Pts',(130.88631060373,-4.21900673488797,330.851757874295));
#11960=CARTESIAN_POINT('Ctrl Pts',(130.878911933976,-4.32941041302072,330.964044922034));
#11961=CARTESIAN_POINT('Ctrl Pts',(130.871513264221,-4.43538757575636,331.080802833711));
#11962=CARTESIAN_POINT('Ctrl Pts',(130.864114594466,-4.53656370176803,331.201642415161));
#11963=CARTESIAN_POINT('Ctrl Pts',(130.856717145262,-4.63772313686048,331.322462061833));
#11964=CARTESIAN_POINT('Ctrl Pts',(130.849319696058,-4.73408286778036,331.447361756022));
#11965=CARTESIAN_POINT('Ctrl Pts',(130.841922246854,-4.82530733177565,331.575917682588));
#11966=CARTESIAN_POINT('Ctrl Pts',(130.834525118391,-4.91652784043711,331.704468035193));
#11967=CARTESIAN_POINT('Ctrl Pts',(130.827127989927,-5.0026133089068,331.836674000604));
#11968=CARTESIAN_POINT('Ctrl Pts',(130.819730861464,-5.08327051978381,331.972081344356));
#11969=CARTESIAN_POINT('Ctrl Pts',(130.812332594027,-5.16394014985785,332.107509537459));
#11970=CARTESIAN_POINT('Ctrl Pts',(130.804934326591,-5.23917966711533,332.24613976974));
#11971=CARTESIAN_POINT('Ctrl Pts',(130.797536059154,-5.30874105485643,332.387491822983));
#11972=CARTESIAN_POINT('Ctrl Pts',(130.790135192628,-5.37832688024466,332.528893534688));
#11973=CARTESIAN_POINT('Ctrl Pts',(130.782734326102,-5.4422304398142,332.673018636507));
#11974=CARTESIAN_POINT('Ctrl Pts',(130.775333459577,-5.50025129658857,332.819365634299));
#11975=CARTESIAN_POINT('Ctrl Pts',(130.767924466192,-5.5583358658107,332.965873335086));
#11976=CARTESIAN_POINT('Ctrl Pts',(130.760515472807,-5.61052469410175,333.114607457219));
#11977=CARTESIAN_POINT('Ctrl Pts',(130.753106479422,-5.656666565926,333.265049302016));
#11978=CARTESIAN_POINT('Ctrl Pts',(130.745692921842,-5.70283686273494,333.415583824179));
#11979=CARTESIAN_POINT('Ctrl Pts',(130.738279364262,-5.74295268538358,333.567827805239));
#11980=CARTESIAN_POINT('Ctrl Pts',(130.730865806682,-5.77691377670035,333.721251479348));
#11981=CARTESIAN_POINT('Ctrl Pts',(130.723441694545,-5.81092321784797,333.874893580145));
#11982=CARTESIAN_POINT('Ctrl Pts',(130.716017582408,-5.83876036155908,334.029718361975));
#11983=CARTESIAN_POINT('Ctrl Pts',(130.708593470272,-5.86037660726913,334.185189234563));
#11984=CARTESIAN_POINT('Ctrl Pts',(130.704736345117,-5.87160711720014,334.265962612234));
#11985=CARTESIAN_POINT('Ctrl Pts',(130.700879219962,-5.88115932756141,334.346910343893));
#11986=CARTESIAN_POINT('Ctrl Pts',(130.697022094807,-5.88903197523169,334.427957206847));
#11987=CARTESIAN_POINT('Ctrl Pts',(130.688032064773,-5.90738122141063,334.616857930293));
#11988=CARTESIAN_POINT('Ctrl Pts',(130.679042034738,-5.91664347140671,334.806655501886));
#11989=CARTESIAN_POINT('Ctrl Pts',(130.670052004703,-5.91674908643611,334.996712043568));
#11990=CARTESIAN_POINT('',(128.920053149077,-5.91243296764551,334.996538828883));
#11991=CARTESIAN_POINT('Ctrl Pts',(130.670049495371,-5.92421797011413,334.996761009397));
#11992=CARTESIAN_POINT('Ctrl Pts',(130.586294350425,-5.9123736713581,336.769655413876));
#11993=CARTESIAN_POINT('Ctrl Pts',(130.409793194054,-4.12388091182169,340.526437395856));
#11994=CARTESIAN_POINT('Ctrl Pts',(130.14054602626,2.26943811269259,341.618328608785));
#11995=CARTESIAN_POINT('Ctrl Pts',(129.862307991985,6.79361690608675,336.673138444528));
#11996=CARTESIAN_POINT('Ctrl Pts',(129.584069957711,5.08339373838535,330.192533825209));
#11997=CARTESIAN_POINT('Ctrl Pts',(129.305831923437,-1.29178483226323,328.123669956412));
#11998=CARTESIAN_POINT('Ctrl Pts',(129.084493291078,-5.42021756930977,331.497741847142));
#11999=CARTESIAN_POINT('Ctrl Pts',(128.955900670143,-5.91301563696258,334.232721977575));
#12000=CARTESIAN_POINT('Ctrl Pts',(128.920054060632,-5.90899501774148,334.996521404454));
#12001=CARTESIAN_POINT('',(127.170050856975,-5.91375951636249,335.004785277391));
#12002=CARTESIAN_POINT('Ctrl Pts',(128.920052004703,-5.91674900040053,334.996560703666));
#12003=CARTESIAN_POINT('Ctrl Pts',(128.912579712844,-5.91684167049648,335.155984505595));
#12004=CARTESIAN_POINT('Ctrl Pts',(128.905107420984,-5.91048660953891,335.315420720306));
#12005=CARTESIAN_POINT('Ctrl Pts',(128.897635129125,-5.89770744149063,335.474317928278));
#12006=CARTESIAN_POINT('Ctrl Pts',(128.890161693573,-5.88492631749113,335.633239456705));
#12007=CARTESIAN_POINT('Ctrl Pts',(128.882688258021,-5.8657191558017,335.791621452473));
#12008=CARTESIAN_POINT('Ctrl Pts',(128.875214822469,-5.84016151511452,335.948917298754));
#12009=CARTESIAN_POINT('Ctrl Pts',(128.867738883119,-5.81459531194363,336.106265843293));
#12010=CARTESIAN_POINT('Ctrl Pts',(128.860262943769,-5.78267444888914,336.262527155498));
#12011=CARTESIAN_POINT('Ctrl Pts',(128.852787004419,-5.74452568383359,336.417164503604));
#12012=CARTESIAN_POINT('Ctrl Pts',(128.845307199907,-5.70635719535002,336.571881801314));
#12013=CARTESIAN_POINT('Ctrl Pts',(128.837827395396,-5.6619544764055,336.724973110494));
#12014=CARTESIAN_POINT('Ctrl Pts',(128.830347590884,-5.61149423945202,336.875916566134));
#12015=CARTESIAN_POINT('Ctrl Pts',(128.822857867366,-5.56096708692768,337.027060188641));
#12016=CARTESIAN_POINT('Ctrl Pts',(128.815368143848,-5.50436648500666,337.176049923871));
#12017=CARTESIAN_POINT('Ctrl Pts',(128.80787842033,-5.44191779758709,337.322382665885));
#12018=CARTESIAN_POINT('Ctrl Pts',(128.800383220738,-5.37942345111426,337.46882239837));
#12019=CARTESIAN_POINT('Ctrl Pts',(128.792888021145,-5.31107265074541,337.612600938451));
#12020=CARTESIAN_POINT('Ctrl Pts',(128.785392821553,-5.23713674329087,337.753239781525));
#12021=CARTESIAN_POINT('Ctrl Pts',(128.777885565949,-5.16308191010289,337.894104841848));
#12022=CARTESIAN_POINT('Ctrl Pts',(128.770378310346,-5.08342420267718,338.031819802281));
#12023=CARTESIAN_POINT('Ctrl Pts',(128.762871054742,-4.9984788934223,338.165934193017));
#12024=CARTESIAN_POINT('Ctrl Pts',(128.758365988124,-4.94750363731544,338.246415569509));
#12025=CARTESIAN_POINT('Ctrl Pts',(128.753860921507,-4.8946250466006,338.32560093499));
#12026=CARTESIAN_POINT('Ctrl Pts',(128.749355854889,-4.83991808089027,338.403398820704));
#12027=CARTESIAN_POINT('Ctrl Pts',(128.741931877451,-4.74976552298043,338.531603306294));
#12028=CARTESIAN_POINT('Ctrl Pts',(128.734507900013,-4.65437943888897,338.656416647204));
#12029=CARTESIAN_POINT('Ctrl Pts',(128.727083922575,-4.55404336906196,338.777382632883));
#12030=CARTESIAN_POINT('Ctrl Pts',(128.719668706548,-4.45382571089371,338.898205860498));
#12031=CARTESIAN_POINT('Ctrl Pts',(128.71225349052,-4.34866993099153,339.015190486275));
#12032=CARTESIAN_POINT('Ctrl Pts',(128.704838274492,-4.23890294131249,339.127908964189));
#12033=CARTESIAN_POINT('Ctrl Pts',(128.697430193348,-4.129241568878,339.240518984951));
#12034=CARTESIAN_POINT('Ctrl Pts',(128.690022112204,-4.01497807830944,339.348870764282));
#12035=CARTESIAN_POINT('Ctrl Pts',(128.68261403106,-3.89647968528122,339.452569665338));
#12036=CARTESIAN_POINT('Ctrl Pts',(128.675211463886,-3.77806949277126,339.556191381409));
#12037=CARTESIAN_POINT('Ctrl Pts',(128.667808896712,-3.65543095377422,339.655166870259));
#12038=CARTESIAN_POINT('Ctrl Pts',(128.660406329538,-3.52896810021188,339.749138312388));
#12039=CARTESIAN_POINT('Ctrl Pts',(128.653007659783,-3.40257182878891,339.843060278963));
#12040=CARTESIAN_POINT('Ctrl Pts',(128.645608990029,-3.27235555158258,339.93198322376));
#12041=CARTESIAN_POINT('Ctrl Pts',(128.638210320274,-3.13875624671768,340.015589674823));
#12042=CARTESIAN_POINT('Ctrl Pts',(128.63081287107,-3.00517898158994,340.099182333418));
#12043=CARTESIAN_POINT('Ctrl Pts',(128.623415421866,-2.86822011250208,340.177460041162));
#12044=CARTESIAN_POINT('Ctrl Pts',(128.616017972662,-2.72834555510473,340.250148673556));
#12045=CARTESIAN_POINT('Ctrl Pts',(128.608620844199,-2.58847706242438,340.322834154298));
#12046=CARTESIAN_POINT('Ctrl Pts',(128.601223715735,-2.44569346396151,340.389930869431));
#12047=CARTESIAN_POINT('Ctrl Pts',(128.593826587272,-2.30048498560767,340.451210819029));
#12048=CARTESIAN_POINT('Ctrl Pts',(128.586428319835,-2.15525414877301,340.512500204209));
#12049=CARTESIAN_POINT('Ctrl Pts',(128.579030052399,-2.00759803248398,340.567970895406));
#12050=CARTESIAN_POINT('Ctrl Pts',(128.571631784962,-1.85802638693673,340.617443235846));
#12051=CARTESIAN_POINT('Ctrl Pts',(128.564230918436,-1.70840219529709,340.666932956439));
#12052=CARTESIAN_POINT('Ctrl Pts',(128.556830051911,-1.55686148867438,340.710420013551));
#12053=CARTESIAN_POINT('Ctrl Pts',(128.549429185385,-1.403928551426,340.747774802912));
#12054=CARTESIAN_POINT('Ctrl Pts',(128.542020192,-1.25082767919194,340.785170611403));
#12055=CARTESIAN_POINT('Ctrl Pts',(128.534611198615,-1.09633188600138,340.816420615743));
#12056=CARTESIAN_POINT('Ctrl Pts',(128.527202205231,-0.940975731978278,
340.84144633069));
#12057=CARTESIAN_POINT('Ctrl Pts',(128.51978864765,-0.78552387320538,340.86648746234));
#12058=CARTESIAN_POINT('Ctrl Pts',(128.51237509007,-0.629210967153669,340.885296619612));
#12059=CARTESIAN_POINT('Ctrl Pts',(128.50496153249,-0.47257553185195,340.897847313147));
#12060=CARTESIAN_POINT('Ctrl Pts',(128.497537420353,-0.315717097332351,
340.910415874892));
#12061=CARTESIAN_POINT('Ctrl Pts',(128.490113308217,-0.158535588396375,
340.916708162823));
#12062=CARTESIAN_POINT('Ctrl Pts',(128.48268919608,-0.00156918253640919,
340.916749791918));
#12063=CARTESIAN_POINT('Ctrl Pts',(128.478832070925,0.0799811848830685,
340.91677141991));
#12064=CARTESIAN_POINT('Ctrl Pts',(128.47497494577,0.161473569395059,340.915106712601));
#12065=CARTESIAN_POINT('Ctrl Pts',(128.471117820615,0.242833288648434,340.911764758211));
#12066=CARTESIAN_POINT('Ctrl Pts',(128.463693843177,0.399429897742017,340.905332352469));
#12067=CARTESIAN_POINT('Ctrl Pts',(128.456269865739,0.556006982243015,340.892663819937));
#12068=CARTESIAN_POINT('Ctrl Pts',(128.448845888301,0.712027464962904,340.873750714121));
#12069=CARTESIAN_POINT('Ctrl Pts',(128.441430672274,0.867863820038581,340.854859928616));
#12070=CARTESIAN_POINT('Ctrl Pts',(128.434015456246,1.02314451395496,340.82973928348));
#12071=CARTESIAN_POINT('Ctrl Pts',(128.426600240219,1.17733310332001,340.798432316267));
#12072=CARTESIAN_POINT('Ctrl Pts',(128.419192159074,1.33137333320056,340.76715547246));
#12073=CARTESIAN_POINT('Ctrl Pts',(128.41178407793,1.48432318720783,340.729704230556));
#12074=CARTESIAN_POINT('Ctrl Pts',(128.404375996786,1.63565208532899,340.686173829409));
#12075=CARTESIAN_POINT('Ctrl Pts',(128.396973429612,1.78686834658715,340.642675828736));
#12076=CARTESIAN_POINT('Ctrl Pts',(128.389570862438,1.93646569715959,340.593107781144));
#12077=CARTESIAN_POINT('Ctrl Pts',(128.382168295264,2.08392459413759,340.537615809033));
#12078=CARTESIAN_POINT('Ctrl Pts',(128.37476962551,2.23130585465174,340.482153053202));
#12079=CARTESIAN_POINT('Ctrl Pts',(128.367370955755,2.37655055542424,340.420772715484));
#12080=CARTESIAN_POINT('Ctrl Pts',(128.359972286,2.51915525357791,340.353670457814));
#12081=CARTESIAN_POINT('Ctrl Pts',(128.352574836796,2.66173642638404,340.286579269933));
#12082=CARTESIAN_POINT('Ctrl Pts',(128.345177387592,2.80167812356927,340.213768194262));
#12083=CARTESIAN_POINT('Ctrl Pts',(128.337779938388,2.93849769430178,340.135480684715));
#12084=CARTESIAN_POINT('Ctrl Pts',(128.330382809925,3.07531133277629,340.057196569578));
#12085=CARTESIAN_POINT('Ctrl Pts',(128.322985681461,3.20900279002705,339.973436678043));
#12086=CARTESIAN_POINT('Ctrl Pts',(128.315588552998,3.33911504669222,339.884489867678));
#12087=CARTESIAN_POINT('Ctrl Pts',(128.308190285561,3.46924733739688,339.795529361725));
#12088=CARTESIAN_POINT('Ctrl Pts',(128.300792018125,3.59579902207019,339.701380557347));
#12089=CARTESIAN_POINT('Ctrl Pts',(128.293393750688,3.71834316841695,339.602374891769));
#12090=CARTESIAN_POINT('Ctrl Pts',(128.285992884162,3.84093036581098,339.50333444446));
#12091=CARTESIAN_POINT('Ctrl Pts',(128.278592017636,3.9595069316497,339.399433973172));
#12092=CARTESIAN_POINT('Ctrl Pts',(128.271191151111,4.0736801585877,339.2910442235));
#12093=CARTESIAN_POINT('Ctrl Pts',(128.263782157726,4.18797875864438,339.182535451519));
#12094=CARTESIAN_POINT('Ctrl Pts',(128.256373164341,4.29786409264582,339.069527813475));
#12095=CARTESIAN_POINT('Ctrl Pts',(128.248964170956,4.40298087952114,338.952428359512));
#12096=CARTESIAN_POINT('Ctrl Pts',(128.241550613376,4.50816242196326,338.835256768245));
#12097=CARTESIAN_POINT('Ctrl Pts',(128.234137055796,4.60856932628622,338.713988625025));
#12098=CARTESIAN_POINT('Ctrl Pts',(128.226723498216,4.70388789401863,338.589062446239));
#12099=CARTESIAN_POINT('Ctrl Pts',(128.219299386079,4.7993421651824,338.463958412168));
#12100=CARTESIAN_POINT('Ctrl Pts',(128.211875273942,4.88969341790184,338.335186246033));
#12101=CARTESIAN_POINT('Ctrl Pts',(128.204451161806,4.97467195363788,338.203212374506));
#12102=CARTESIAN_POINT('Ctrl Pts',(128.200594036651,5.01882172424593,338.134646634891));
#12103=CARTESIAN_POINT('Ctrl Pts',(128.196736911496,5.06152204164618,338.065217081547));
#12104=CARTESIAN_POINT('Ctrl Pts',(128.192879786341,5.10274013340856,337.994991434612));
#12105=CARTESIAN_POINT('Ctrl Pts',(128.185455808903,5.18207439688276,337.859825061345));
#12106=CARTESIAN_POINT('Ctrl Pts',(128.178031831465,5.25615400242056,337.721300380689));
#12107=CARTESIAN_POINT('Ctrl Pts',(128.170607854027,5.32468120389963,337.579864461428));
#12108=CARTESIAN_POINT('Ctrl Pts',(128.163192638,5.39312753297071,337.438595457831));
#12109=CARTESIAN_POINT('Ctrl Pts',(128.155777421972,5.45603434003352,337.294422387042));
#12110=CARTESIAN_POINT('Ctrl Pts',(128.148362205944,5.51314793644405,337.147819916423));
#12111=CARTESIAN_POINT('Ctrl Pts',(128.1409541248,5.5702065784394,337.001358505963));
#12112=CARTESIAN_POINT('Ctrl Pts',(128.133546043656,5.62148297239911,336.85247269474));
#12113=CARTESIAN_POINT('Ctrl Pts',(128.126137962512,5.66677007941836,336.701660198015));
#12114=CARTESIAN_POINT('Ctrl Pts',(128.118735395338,5.71202347841697,336.550959953785));
#12115=CARTESIAN_POINT('Ctrl Pts',(128.111332828164,5.7512963599982,336.398336235402));
#12116=CARTESIAN_POINT('Ctrl Pts',(128.10393026099,5.78443044712525,336.244305012796));
#12117=CARTESIAN_POINT('Ctrl Pts',(128.096531591235,5.81754708929998,336.090354886958));
#12118=CARTESIAN_POINT('Ctrl Pts',(128.089132921481,5.84453129554744,335.934999096677));
#12119=CARTESIAN_POINT('Ctrl Pts',(128.081734251726,5.86527516033568,335.778766881711));
#12120=CARTESIAN_POINT('Ctrl Pts',(128.074336802522,5.88601560303051,335.622560440208));
#12121=CARTESIAN_POINT('Ctrl Pts',(128.066939353318,5.90051769834206,335.465478230574));
#12122=CARTESIAN_POINT('Ctrl Pts',(128.059541904114,5.90872498180179,335.308057871075));
#12123=CARTESIAN_POINT('Ctrl Pts',(128.05214477565,5.916931909408,335.150644337049));
#12124=CARTESIAN_POINT('Ctrl Pts',(128.044747647187,5.9188445484099,334.992893055013));
#12125=CARTESIAN_POINT('Ctrl Pts',(128.037350518723,5.91445848589812,334.835344659705));
#12126=CARTESIAN_POINT('Ctrl Pts',(128.029952251287,5.91007174804219,334.677772005876));
#12127=CARTESIAN_POINT('Ctrl Pts',(128.02255398385,5.89938438797449,334.520402674066));
#12128=CARTESIAN_POINT('Ctrl Pts',(128.015155716414,5.88244408076651,334.36377504045));
#12129=CARTESIAN_POINT('Ctrl Pts',(128.007754849888,5.86549782225043,334.207092381898));
#12130=CARTESIAN_POINT('Ctrl Pts',(128.000353983362,5.84229428302207,334.051152311142));
#12131=CARTESIAN_POINT('Ctrl Pts',(127.992953116836,5.81293271448255,333.89648569588));
#12132=CARTESIAN_POINT('Ctrl Pts',(127.985544123452,5.78353890413376,333.741649241887));
#12133=CARTESIAN_POINT('Ctrl Pts',(127.978135130067,5.74797362983715,333.588089402902));
#12134=CARTESIAN_POINT('Ctrl Pts',(127.970726136682,5.70638692576973,333.436325220545));
#12135=CARTESIAN_POINT('Ctrl Pts',(127.963312579102,5.66477460285813,333.284467546217));
#12136=CARTESIAN_POINT('Ctrl Pts',(127.955899021522,5.6171335713578,333.134408087623));
#12137=CARTESIAN_POINT('Ctrl Pts',(127.948485463941,5.56366282881179,332.986647946881));
#12138=CARTESIAN_POINT('Ctrl Pts',(127.941061351805,5.51011596087462,332.838677442528));
#12139=CARTESIAN_POINT('Ctrl Pts',(127.933637239668,5.45072294633833,332.693013138515));
#12140=CARTESIAN_POINT('Ctrl Pts',(127.926213127531,5.3857300639857,332.550134240335));
#12141=CARTESIAN_POINT('Ctrl Pts',(127.922356002377,5.35196364494825,332.475902900333));
#12142=CARTESIAN_POINT('Ctrl Pts',(127.918498877222,5.31668644421776,332.402422977283));
#12143=CARTESIAN_POINT('Ctrl Pts',(127.914641752068,5.27993767406057,332.329758677472));
#12144=CARTESIAN_POINT('Ctrl Pts',(127.90721777463,5.20920570929686,332.189898522375));
#12145=CARTESIAN_POINT('Ctrl Pts',(127.899793797192,5.13280607528259,332.052639748412));
#12146=CARTESIAN_POINT('Ctrl Pts',(127.892369819754,5.05095359418336,331.918474671221));
#12147=CARTESIAN_POINT('Ctrl Pts',(127.884954603726,4.96919771132714,331.784467929008));
#12148=CARTESIAN_POINT('Ctrl Pts',(127.877539387699,4.88200198319752,331.653547931638));
#12149=CARTESIAN_POINT('Ctrl Pts',(127.870124171671,4.78962828222269,331.526184881052));
#12150=CARTESIAN_POINT('Ctrl Pts',(127.862716090527,4.69734346275759,331.398944378551));
#12151=CARTESIAN_POINT('Ctrl Pts',(127.855308009383,4.59989080677096,331.275254309417));
#12152=CARTESIAN_POINT('Ctrl Pts',(127.847899928239,4.497576813013,331.155558119369));
#12153=CARTESIAN_POINT('Ctrl Pts',(127.840497361065,4.39533897342959,331.035951021382));
#12154=CARTESIAN_POINT('Ctrl Pts',(127.833094793891,4.28824724225886,330.920332165847));
#12155=CARTESIAN_POINT('Ctrl Pts',(127.825692226717,4.17664985683644,330.809113872236));
#12156=CARTESIAN_POINT('Ctrl Pts',(127.818293556962,4.06511122695055,330.697954134571));
#12157=CARTESIAN_POINT('Ctrl Pts',(127.810894887207,3.94907193088764,330.591190607421));
#12158=CARTESIAN_POINT('Ctrl Pts',(127.803496217453,3.82891862377498,330.489200432849));
#12159=CARTESIAN_POINT('Ctrl Pts',(127.796098768249,3.70878513822579,330.387227083488));
#12160=CARTESIAN_POINT('Ctrl Pts',(127.788701319045,3.58453927284678,330.290025765144));
#12161=CARTESIAN_POINT('Ctrl Pts',(127.781303869841,3.456602566142,330.197934896085));
#12162=CARTESIAN_POINT('Ctrl Pts',(127.773906741378,3.32867140654993,330.105848019925));
#12163=CARTESIAN_POINT('Ctrl Pts',(127.766509612914,3.1970500267216,330.018871370508));
#12164=CARTESIAN_POINT('Ctrl Pts',(127.759112484451,3.06219066986195,329.93730122722));
#12165=CARTESIAN_POINT('Ctrl Pts',(127.751714217014,2.92731054802768,329.855718524166));
#12166=CARTESIAN_POINT('Ctrl Pts',(127.744315949578,2.78919177580796,329.779544177959));
#12167=CARTESIAN_POINT('Ctrl Pts',(127.736917682141,2.64831288493154,329.709029443854));
#12168=CARTESIAN_POINT('Ctrl Pts',(127.729516815615,2.50738450182041,329.638489937182));
#12169=CARTESIAN_POINT('Ctrl Pts',(127.72211594909,2.36369440299247,329.57361416822));
#12170=CARTESIAN_POINT('Ctrl Pts',(127.714715082564,2.21774271704954,329.51460595732));
#12171=CARTESIAN_POINT('Ctrl Pts',(127.707306089179,2.07163076220076,329.455532949762));
#12172=CARTESIAN_POINT('Ctrl Pts',(127.699897095794,1.92325260688589,329.402340507533));
#12173=CARTESIAN_POINT('Ctrl Pts',(127.69248810241,1.77312591638003,329.355183346896));
#12174=CARTESIAN_POINT('Ctrl Pts',(127.685074544829,1.62290674265451,329.307997135821));
#12175=CARTESIAN_POINT('Ctrl Pts',(127.677660987249,1.47093724675896,329.266853712132));
#12176=CARTESIAN_POINT('Ctrl Pts',(127.670247429669,1.31774650514284,329.231856909656));
#12177=CARTESIAN_POINT('Ctrl Pts',(127.662823317532,1.16433766846065,329.196810282825));
#12178=CARTESIAN_POINT('Ctrl Pts',(127.655399205396,1.00970447946961,329.167927822725));
#12179=CARTESIAN_POINT('Ctrl Pts',(127.647975093259,0.854383187870459,329.145261753863));
#12180=CARTESIAN_POINT('Ctrl Pts',(127.644117968104,0.77368752354308,329.133485818537));
#12181=CARTESIAN_POINT('Ctrl Pts',(127.640260842949,0.692806171097826,329.123386966597));
#12182=CARTESIAN_POINT('Ctrl Pts',(127.636403717794,0.611814342979406,329.114966969317));
#12183=CARTESIAN_POINT('Ctrl Pts',(127.628979740356,0.455925830039553,329.09876063239));
#12184=CARTESIAN_POINT('Ctrl Pts',(127.621555762919,0.299157772951509,329.08872811605));
#12185=CARTESIAN_POINT('Ctrl Pts',(127.614131785481,0.142040423038221,329.084955191994));
#12186=CARTESIAN_POINT('Ctrl Pts',(127.606716569453,-0.0148915047626448,
329.081186720556));
#12187=CARTESIAN_POINT('Ctrl Pts',(127.599301353425,-0.172171535386678,
329.083663145815));
#12188=CARTESIAN_POINT('Ctrl Pts',(127.591886137398,-0.329262551795625,
329.092418706908));
#12189=CARTESIAN_POINT('Ctrl Pts',(127.584478056254,-0.486202416019711,
329.101165843445));
#12190=CARTESIAN_POINT('Ctrl Pts',(127.577069975109,-0.642953257952551,
329.116180067183));
#12191=CARTESIAN_POINT('Ctrl Pts',(127.569661893965,-0.79897631056802,329.137443610706));
#12192=CARTESIAN_POINT('Ctrl Pts',(127.562259326791,-0.954883232375269,
329.158691327386));
#12193=CARTESIAN_POINT('Ctrl Pts',(127.554856759617,-1.1100630752735,329.18617905189));
#12194=CARTESIAN_POINT('Ctrl Pts',(127.547454192443,-1.26398065981757,329.21983707374));
#12195=CARTESIAN_POINT('Ctrl Pts',(127.540055522689,-1.41781720742727,329.253477374789));
#12196=CARTESIAN_POINT('Ctrl Pts',(127.532656852934,-1.57039245654284,329.293281423808));
#12197=CARTESIAN_POINT('Ctrl Pts',(127.525258183179,-1.72118001908107,329.339128167463));
#12198=CARTESIAN_POINT('Ctrl Pts',(127.517860733975,-1.87194270635315,329.384967347828));
#12199=CARTESIAN_POINT('Ctrl Pts',(127.510463284771,-2.02091793563043,329.436847135928));
#12200=CARTESIAN_POINT('Ctrl Pts',(127.503065835567,-2.1675930050995,329.494596188585));
#12201=CARTESIAN_POINT('Ctrl Pts',(127.495668707104,-2.3142617149929,329.552342737344));
#12202=CARTESIAN_POINT('Ctrl Pts',(127.48827157864,-2.45863011611126,329.615957907941));
#12203=CARTESIAN_POINT('Ctrl Pts',(127.480874450177,-2.60020432604942,329.685221733196));
#12204=CARTESIAN_POINT('Ctrl Pts',(127.47347618274,-2.74180033488235,329.754496223351));
#12205=CARTESIAN_POINT('Ctrl Pts',(127.466077915304,-2.8806009606181,329.829420935929));
#12206=CARTESIAN_POINT('Ctrl Pts',(127.458679647867,-3.016135956375,329.909729432028));
#12207=CARTESIAN_POINT('Ctrl Pts',(127.451278781341,-3.15171856700074,329.990066141346));
#12208=CARTESIAN_POINT('Ctrl Pts',(127.443877914815,-3.28403294259744,330.075790209788));
#12209=CARTESIAN_POINT('Ctrl Pts',(127.43647704829,-3.41263703799864,330.166591367432));
#12210=CARTESIAN_POINT('Ctrl Pts',(127.429068054905,-3.54138235299166,330.257492233429));
#12211=CARTESIAN_POINT('Ctrl Pts',(127.42165906152,-3.66640894625044,330.35348110707));
#12212=CARTESIAN_POINT('Ctrl Pts',(127.414250068135,-3.78730657518395,330.454206398431));
#12213=CARTESIAN_POINT('Ctrl Pts',(127.406836510555,-3.90827868122739,330.554993740046));
#12214=CARTESIAN_POINT('Ctrl Pts',(127.399422952975,-4.02511647820144,330.660523063904));
#12215=CARTESIAN_POINT('Ctrl Pts',(127.392009395395,-4.13744633639875,330.770405648774));
#12216=CARTESIAN_POINT('Ctrl Pts',(127.384585283258,-4.24993611671397,330.880444671621));
#12217=CARTESIAN_POINT('Ctrl Pts',(127.377161171121,-4.35790488500537,330.994849062763));
#12218=CARTESIAN_POINT('Ctrl Pts',(127.369737058985,-4.46101852908957,331.113196140063));
#12219=CARTESIAN_POINT('Ctrl Pts',(127.36587993383,-4.51459021861594,331.174682211453));
#12220=CARTESIAN_POINT('Ctrl Pts',(127.362022808675,-4.56685209943981,331.237231997994));
#12221=CARTESIAN_POINT('Ctrl Pts',(127.35816568352,-4.61776198028851,331.300783210475));
#12222=CARTESIAN_POINT('Ctrl Pts',(127.350755590316,-4.71556719711442,331.422874246884));
#12223=CARTESIAN_POINT('Ctrl Pts',(127.343345497113,-4.80868200190314,331.549040297182));
#12224=CARTESIAN_POINT('Ctrl Pts',(127.335935403909,-4.8967462828363,331.678884765018));
#12225=CARTESIAN_POINT('Ctrl Pts',(127.328537236175,-4.98466883708833,331.808520267025));
#12226=CARTESIAN_POINT('Ctrl Pts',(127.32113906844,-5.06755685277397,331.941822085217));
#12227=CARTESIAN_POINT('Ctrl Pts',(127.313740900706,-5.14509003449473,332.07836020368));
#12228=CARTESIAN_POINT('Ctrl Pts',(127.306349693167,-5.22255027301627,332.214769867112));
#12229=CARTESIAN_POINT('Ctrl Pts',(127.298958485627,-5.29466551950669,332.354409448406));
#12230=CARTESIAN_POINT('Ctrl Pts',(127.291567278087,-5.3611580764368,332.49681909524));
#12231=CARTESIAN_POINT('Ctrl Pts',(127.284181551165,-5.42760132880623,332.639123144615));
#12232=CARTESIAN_POINT('Ctrl Pts',(127.276795824242,-5.48843003260356,332.78419283324));
#12233=CARTESIAN_POINT('Ctrl Pts',(127.269410097319,-5.54341193738866,332.931542928916));
#12234=CARTESIAN_POINT('Ctrl Pts',(127.26202837521,-5.59836402896301,333.078813125951));
#12235=CARTESIAN_POINT('Ctrl Pts',(127.2546466531,-5.64747550312645,333.228360918027));
#12236=CARTESIAN_POINT('Ctrl Pts',(127.24726493099,-5.69056192600681,333.379680423873));
#12237=CARTESIAN_POINT('Ctrl Pts',(127.239885009437,-5.73363783920222,333.530963019707));
#12238=CARTESIAN_POINT('Ctrl Pts',(127.232505087885,-5.77069152085042,333.684016110063));
#12239=CARTESIAN_POINT('Ctrl Pts',(127.225125166332,-5.80158817946097,333.838317961558));
#12240=CARTESIAN_POINT('Ctrl Pts',(127.217746325309,-5.83248031434543,333.992597220988));
#12241=CARTESIAN_POINT('Ctrl Pts',(127.210367484285,-5.85721715124729,334.148124509523));
#12242=CARTESIAN_POINT('Ctrl Pts',(127.202988643262,-5.87571493624477,334.304367517657));
#12243=CARTESIAN_POINT('Ctrl Pts',(127.19560781495,-5.894217703114,334.460652605567));
#12244=CARTESIAN_POINT('Ctrl Pts',(127.188226986638,-5.90647801889204,334.617653425809));
#12245=CARTESIAN_POINT('Ctrl Pts',(127.180846158326,-5.91246394690351,334.774831975924));
#12246=CARTESIAN_POINT('Ctrl Pts',(127.177248107118,-5.91538200360392,334.851454334303));
#12247=CARTESIAN_POINT('Ctrl Pts',(127.173650055911,-5.91680978494413,334.928118884487));
#12248=CARTESIAN_POINT('Ctrl Pts',(127.170052004703,-5.91674808267963,335.00476325591));
#12249=CARTESIAN_POINT('',(125.420052711425,-5.92190284584293,335.001236346159));
#12250=CARTESIAN_POINT('Ctrl Pts',(127.170050046356,-5.91164874592261,335.004800830766));
#12251=CARTESIAN_POINT('Ctrl Pts',(127.140009247319,-5.91645495858893,335.644171629641));
#12252=CARTESIAN_POINT('Ctrl Pts',(127.017222436859,-5.5259482387815,338.251773747601));
#12253=CARTESIAN_POINT('Ctrl Pts',(126.801689614972,-1.71899598251946,341.782158633747));
#12254=CARTESIAN_POINT('Ctrl Pts',(126.523451580698,4.77301452401663,340.115755591771));
#12255=CARTESIAN_POINT('Ctrl Pts',(126.245213546424,6.88490005144117,333.754699151657));
#12256=CARTESIAN_POINT('Ctrl Pts',(125.96697551215,2.67861442261645,328.536436919456));
#12257=CARTESIAN_POINT('Ctrl Pts',(125.691922095927,-3.90951754564736,329.241527458829));
#12258=CARTESIAN_POINT('Ctrl Pts',(125.509614691129,-5.92071945294146,333.107089038917));
#12259=CARTESIAN_POINT('Ctrl Pts',(125.420053297756,-5.92617800717982,335.001224849182));
#12260=CARTESIAN_POINT('',(123.670052008058,-5.91563694601309,334.994569125369));
#12261=CARTESIAN_POINT('Ctrl Pts',(125.420052004703,-5.91674986791655,335.001250203804));
#12262=CARTESIAN_POINT('Ctrl Pts',(125.41686781767,-5.91673566116889,335.068485459398));
#12263=CARTESIAN_POINT('Ctrl Pts',(125.413683630636,-5.91557544751366,335.135707266568));
#12264=CARTESIAN_POINT('Ctrl Pts',(125.410499443602,-5.91327036300921,335.202889567147));
#12265=CARTESIAN_POINT('Ctrl Pts',(125.403075466164,-5.90789602564378,335.359526058174));
#12266=CARTESIAN_POINT('Ctrl Pts',(125.395651488726,-5.89628557189547,335.51618515453));
#12267=CARTESIAN_POINT('Ctrl Pts',(125.388227511288,-5.87842692712291,335.672329848345));
#12268=CARTESIAN_POINT('Ctrl Pts',(125.380812295261,-5.86058935823815,335.828290267929));
#12269=CARTESIAN_POINT('Ctrl Pts',(125.373397079233,-5.83651831800253,335.983737126171));
#12270=CARTESIAN_POINT('Ctrl Pts',(125.365981863205,-5.80625371891772,336.138133697794));
#12271=CARTESIAN_POINT('Ctrl Pts',(125.358573782061,-5.77601824027782,336.292381709813));
#12272=CARTESIAN_POINT('Ctrl Pts',(125.351165700917,-5.73960113817575,336.445581083296));
#12273=CARTESIAN_POINT('Ctrl Pts',(125.343757619773,-5.69709406484713,336.597200606932));
#12274=CARTESIAN_POINT('Ctrl Pts',(125.336355052599,-5.65461863030943,336.748707277388));
#12275=CARTESIAN_POINT('Ctrl Pts',(125.328952485425,-5.60606235047825,336.89863608159));
#12276=CARTESIAN_POINT('Ctrl Pts',(125.321549918251,-5.55156783453554,337.046466501326));
#12277=CARTESIAN_POINT('Ctrl Pts',(125.314151248496,-5.49710200971745,337.194219088992));
#12278=CARTESIAN_POINT('Ctrl Pts',(125.306752578742,-5.43670430406923,337.339875143151));
#12279=CARTESIAN_POINT('Ctrl Pts',(125.299353908987,-5.37056697394703,337.482929910579));
#12280=CARTESIAN_POINT('Ctrl Pts',(125.291956459783,-5.30444055443047,337.625961078414));
#12281=CARTESIAN_POINT('Ctrl Pts',(125.284559010579,-5.2325765461144,337.766391472775));
#12282=CARTESIAN_POINT('Ctrl Pts',(125.277161561375,-5.15521513670821,337.90373680914));
#12283=CARTESIAN_POINT('Ctrl Pts',(125.269764432911,-5.07785708155784,338.041076190451));
#12284=CARTESIAN_POINT('Ctrl Pts',(125.262367304448,-4.99500228241028,338.175330454555));
#12285=CARTESIAN_POINT('Ctrl Pts',(125.254970175984,-4.90693650275019,338.306040641081));
#12286=CARTESIAN_POINT('Ctrl Pts',(125.247571908548,-4.81885716315839,338.436770953712));
#12287=CARTESIAN_POINT('Ctrl Pts',(125.240173641111,-4.72556545399591,338.563955792672));
#12288=CARTESIAN_POINT('Ctrl Pts',(125.232775373675,-4.62738992069319,338.687165996313));
#12289=CARTESIAN_POINT('Ctrl Pts',(125.225374507149,-4.52917989729312,338.810419484994));
#12290=CARTESIAN_POINT('Ctrl Pts',(125.217973640623,-4.42608286614893,338.929695266565));
#12291=CARTESIAN_POINT('Ctrl Pts',(125.210572774097,-4.31846691137618,339.044598137992));
#12292=CARTESIAN_POINT('Ctrl Pts',(125.203163780712,-4.21073278399664,339.159627183757));
#12293=CARTESIAN_POINT('Ctrl Pts',(125.195754787328,-4.09847007846341,339.270273457221));
#12294=CARTESIAN_POINT('Ctrl Pts',(125.188345793943,-3.98208343545538,339.376178935507));
#12295=CARTESIAN_POINT('Ctrl Pts',(125.180932236363,-3.86562509426086,339.48214965522));
#12296=CARTESIAN_POINT('Ctrl Pts',(125.173518678782,-3.74503803851658,339.583373520898));
#12297=CARTESIAN_POINT('Ctrl Pts',(125.166105121202,-3.62075865534695,339.679533878735));
#12298=CARTESIAN_POINT('Ctrl Pts',(125.158681009065,-3.4963023377229,339.775831138447));
#12299=CARTESIAN_POINT('Ctrl Pts',(125.151256896929,-3.3681434972203,339.867050277009));
#12300=CARTESIAN_POINT('Ctrl Pts',(125.143832784792,-3.23674672785962,339.952918450993));
#12301=CARTESIAN_POINT('Ctrl Pts',(125.139975659637,-3.16848081605814,339.997530424486));
#12302=CARTESIAN_POINT('Ctrl Pts',(125.136118534483,-3.09934131815225,340.040698813525));
#12303=CARTESIAN_POINT('Ctrl Pts',(125.132261409328,-3.0293957313334,340.082390388929));
#12304=CARTESIAN_POINT('Ctrl Pts',(125.12483743189,-2.89476840200828,340.162635987077));
#12305=CARTESIAN_POINT('Ctrl Pts',(125.117413454452,-2.75674734297633,340.237649734957));
#12306=CARTESIAN_POINT('Ctrl Pts',(125.109989477014,-2.61577760133092,340.307130872974));
#12307=CARTESIAN_POINT('Ctrl Pts',(125.102574260987,-2.4749742251906,340.376530012795));
#12308=CARTESIAN_POINT('Ctrl Pts',(125.095159044959,-2.33122942471442,340.440409376061));
#12309=CARTESIAN_POINT('Ctrl Pts',(125.087743828931,-2.18501614258361,340.498512073202));
#12310=CARTESIAN_POINT('Ctrl Pts',(125.080335747787,-2.03894354613673,340.556558864221));
#12311=CARTESIAN_POINT('Ctrl Pts',(125.072927666643,-1.89040754104931,340.608839917708));
#12312=CARTESIAN_POINT('Ctrl Pts',(125.065519585499,-1.73990443252952,340.655144837063));
#12313=CARTESIAN_POINT('Ctrl Pts',(125.058117018325,-1.58951334622209,340.701415290822));
#12314=CARTESIAN_POINT('Ctrl Pts',(125.050714451151,-1.43715842700227,340.741718358076));
#12315=CARTESIAN_POINT('Ctrl Pts',(125.043311883977,-1.2833545637519,340.775892279657));
#12316=CARTESIAN_POINT('Ctrl Pts',(125.035913214222,-1.12963167756334,340.810048208817));
#12317=CARTESIAN_POINT('Ctrl Pts',(125.028514544468,-0.974461730039377,
340.838081338257));
#12318=CARTESIAN_POINT('Ctrl Pts',(125.021115874713,-0.818373219880692,
340.859880189516));
#12319=CARTESIAN_POINT('Ctrl Pts',(125.013718425509,-0.662310459479376,
340.881675444641));
#12320=CARTESIAN_POINT('Ctrl Pts',(125.006320976305,-0.505329806454695,
340.89723841118));
#12321=CARTESIAN_POINT('Ctrl Pts',(124.998923527101,-0.347968485344661,
340.906508993958));
#12322=CARTESIAN_POINT('Ctrl Pts',(124.991526398637,-0.190613987147168,
340.91577917478));
#12323=CARTESIAN_POINT('Ctrl Pts',(124.984129270174,-0.0328792262472288,
340.918757492362));
#12324=CARTESIAN_POINT('Ctrl Pts',(124.976732141711,0.1246952047689,340.915435881523));
#12325=CARTESIAN_POINT('Ctrl Pts',(124.969333874274,0.282293898313986,340.912113759239));
#12326=CARTESIAN_POINT('Ctrl Pts',(124.961935606837,0.439731839669498,340.902489784938));
#12327=CARTESIAN_POINT('Ctrl Pts',(124.954537339401,0.596470342866343,340.886607995491));
#12328=CARTESIAN_POINT('Ctrl Pts',(124.947136472875,0.753263909947715,340.870720626604));
#12329=CARTESIAN_POINT('Ctrl Pts',(124.939735606349,0.909357178566269,340.848571103088));
#12330=CARTESIAN_POINT('Ctrl Pts',(124.932334739823,1.06421862262364,340.820255087688));
#12331=CARTESIAN_POINT('Ctrl Pts',(124.924925746439,1.21925011935187,340.791907978597));
#12332=CARTESIAN_POINT('Ctrl Pts',(124.917516753054,1.37304672283874,340.757380921947));
#12333=CARTESIAN_POINT('Ctrl Pts',(124.910107759669,1.52508838971938,340.716820441998));
#12334=CARTESIAN_POINT('Ctrl Pts',(124.902694202089,1.67722371951129,340.676234975393));
#12335=CARTESIAN_POINT('Ctrl Pts',(124.895280644509,1.82760160282278,340.629608789548));
#12336=CARTESIAN_POINT('Ctrl Pts',(124.887867086929,1.97571960460233,340.577137492163));
#12337=CARTESIAN_POINT('Ctrl Pts',(124.880442974792,2.124048479474,340.52459149228));
#12338=CARTESIAN_POINT('Ctrl Pts',(124.873018862655,2.27011070151455,340.466183899181));
#12339=CARTESIAN_POINT('Ctrl Pts',(124.865594750518,2.413425412381,340.402157748657));
#12340=CARTESIAN_POINT('Ctrl Pts',(124.861737625364,2.48788317462133,340.368893585724));
#12341=CARTESIAN_POINT('Ctrl Pts',(124.857880500209,2.56159974346398,340.334113599218));
#12342=CARTESIAN_POINT('Ctrl Pts',(124.854023375054,2.63451064917932,340.29785656675));
#12343=CARTESIAN_POINT('Ctrl Pts',(124.846599397616,2.77484545743852,340.228071071022));
#12344=CARTESIAN_POINT('Ctrl Pts',(124.839175420178,2.91261723306796,340.152600461198));
#12345=CARTESIAN_POINT('Ctrl Pts',(124.83175144274,3.04733222038819,340.071656228599));
#12346=CARTESIAN_POINT('Ctrl Pts',(124.824336226713,3.18188822375451,339.990807522373));
#12347=CARTESIAN_POINT('Ctrl Pts',(124.816921010685,3.31339430274406,339.904498241852));
#12348=CARTESIAN_POINT('Ctrl Pts',(124.809505794658,3.44137849701398,339.81298707694));
#12349=CARTESIAN_POINT('Ctrl Pts',(124.802097713513,3.56923954553658,339.72156396361));
#12350=CARTESIAN_POINT('Ctrl Pts',(124.794689632369,3.69358515412853,339.624949145983));
#12351=CARTESIAN_POINT('Ctrl Pts',(124.787281551225,3.81396981657318,339.523446120025));
#12352=CARTESIAN_POINT('Ctrl Pts',(124.779878984051,3.93426487451491,339.422018644623));
#12353=CARTESIAN_POINT('Ctrl Pts',(124.772476416877,4.05060457251039,339.315710444982));
#12354=CARTESIAN_POINT('Ctrl Pts',(124.765073849703,4.16257424790502,339.20486696498));
#12355=CARTESIAN_POINT('Ctrl Pts',(124.757675179949,4.27448497175487,339.094081843586));
#12356=CARTESIAN_POINT('Ctrl Pts',(124.750276510194,4.38202999061649,338.978766459188));
#12357=CARTESIAN_POINT('Ctrl Pts',(124.742877840439,4.48482955890165,338.859304910227));
#12358=CARTESIAN_POINT('Ctrl Pts',(124.735480391235,4.58761216845022,338.739863068712));
#12359=CARTESIAN_POINT('Ctrl Pts',(124.728082942031,4.68565063793362,338.616276702745));
#12360=CARTESIAN_POINT('Ctrl Pts',(124.720685492827,4.77860370901436,338.488965054955));
#12361=CARTESIAN_POINT('Ctrl Pts',(124.713288364364,4.87155274981196,338.361658927175));
#12362=CARTESIAN_POINT('Ctrl Pts',(124.7058912359,4.95941661054792,338.23062814015));
#12363=CARTESIAN_POINT('Ctrl Pts',(124.698494107437,5.04189596337167,338.096322925187));
#12364=CARTESIAN_POINT('Ctrl Pts',(124.69109584,5.12438801595684,337.961997030573));
#12365=CARTESIAN_POINT('Ctrl Pts',(124.683697572563,5.20149371450388,337.824396022178));
#12366=CARTESIAN_POINT('Ctrl Pts',(124.676299305127,5.2729585766679,337.683996723404));
#12367=CARTESIAN_POINT('Ctrl Pts',(124.668898438601,5.34444854518958,337.54354810088));
#12368=CARTESIAN_POINT('Ctrl Pts',(124.661497572075,5.41029356260449,337.40029956308));
#12369=CARTESIAN_POINT('Ctrl Pts',(124.65409670555,5.47028643448658,337.254749850243));
#12370=CARTESIAN_POINT('Ctrl Pts',(124.646687712165,5.53034518427751,337.109040309906));
#12371=CARTESIAN_POINT('Ctrl Pts',(124.63927871878,5.58453881273266,336.961024893413));
#12372=CARTESIAN_POINT('Ctrl Pts',(124.631869725395,5.63270910992128,336.811220209005));
#12373=CARTESIAN_POINT('Ctrl Pts',(124.624456167815,5.68090908167455,336.661323239745));
#12374=CARTESIAN_POINT('Ctrl Pts',(124.617042610235,5.72307822861242,336.509635164927));
#12375=CARTESIAN_POINT('Ctrl Pts',(124.609629052655,5.75910914498714,336.356684347454));
#12376=CARTESIAN_POINT('Ctrl Pts',(124.602204940518,5.79519135796764,336.203515776491));
#12377=CARTESIAN_POINT('Ctrl Pts',(124.594780828381,5.82511781625476,336.049081237823));
#12378=CARTESIAN_POINT('Ctrl Pts',(124.587356716244,5.84883267378686,335.893916616102));
#12379=CARTESIAN_POINT('Ctrl Pts',(124.58349959109,5.86115349705078,335.813302348087));
#12380=CARTESIAN_POINT('Ctrl Pts',(124.579642465935,5.87179852965587,335.732491066298));
#12381=CARTESIAN_POINT('Ctrl Pts',(124.57578534078,5.88076549225369,335.651557969499));
#12382=CARTESIAN_POINT('Ctrl Pts',(124.568361363342,5.89802459724597,335.495782499293));
#12383=CARTESIAN_POINT('Ctrl Pts',(124.560937385904,5.90911596448591,335.339085796455));
#12384=CARTESIAN_POINT('Ctrl Pts',(124.553513408466,5.9139502420072,335.181997520761));
#12385=CARTESIAN_POINT('Ctrl Pts',(124.546098192439,5.91877881435365,335.025094632867));
#12386=CARTESIAN_POINT('Ctrl Pts',(124.538682976411,5.91736498419445,334.86780146137));
#12387=CARTESIAN_POINT('Ctrl Pts',(124.531267760383,5.90967088456563,334.710654879742));
#12388=CARTESIAN_POINT('Ctrl Pts',(124.523859679239,5.90198418816074,334.553659503763));
#12389=CARTESIAN_POINT('Ctrl Pts',(124.516451598095,5.88802927059053,334.396810807126));
#12390=CARTESIAN_POINT('Ctrl Pts',(124.509043516951,5.86782025910927,334.240647664594));
#12391=CARTESIAN_POINT('Ctrl Pts',(124.501640949777,5.84762628956434,334.08460075714));
#12392=CARTESIAN_POINT('Ctrl Pts',(124.494238382603,5.82118754265617,333.929238756309));
#12393=CARTESIAN_POINT('Ctrl Pts',(124.486835815429,5.78857011175512,333.775097300274));
#12394=CARTESIAN_POINT('Ctrl Pts',(124.479437145674,5.75596985378888,333.621036999043));
#12395=CARTESIAN_POINT('Ctrl Pts',(124.47203847592,5.71719746754077,333.468196327017));
#12396=CARTESIAN_POINT('Ctrl Pts',(124.464639806165,5.67237044745629,333.317102478068));
#12397=CARTESIAN_POINT('Ctrl Pts',(124.457242356961,5.62755082243814,333.166033554913));
#12398=CARTESIAN_POINT('Ctrl Pts',(124.449844907757,5.57667865198069,333.016711240356));
#12399=CARTESIAN_POINT('Ctrl Pts',(124.442447458553,5.51992181168633,332.869649382057));
#12400=CARTESIAN_POINT('Ctrl Pts',(124.435050330089,5.46316743226963,332.722593900104));
#12401=CARTESIAN_POINT('Ctrl Pts',(124.427653201626,5.40052902471263,332.577799027714));
#12402=CARTESIAN_POINT('Ctrl Pts',(124.420256073163,5.33222321465083,332.435760122056));
#12403=CARTESIAN_POINT('Ctrl Pts',(124.412857805726,5.2639068871994,332.293699345952));
#12404=CARTESIAN_POINT('Ctrl Pts',(124.405459538289,5.18992158145961,332.15439571788));
#12405=CARTESIAN_POINT('Ctrl Pts',(124.398061270853,5.11053055340252,332.018321273973));
#12406=CARTESIAN_POINT('Ctrl Pts',(124.390660404327,5.03111163444238,331.882199025684));
#12407=CARTESIAN_POINT('Ctrl Pts',(124.383259537801,4.94628340004286,331.749308542395));
#12408=CARTESIAN_POINT('Ctrl Pts',(124.375858671275,4.85635312671682,331.620093955281));
#12409=CARTESIAN_POINT('Ctrl Pts',(124.368449677891,4.76632410135291,331.490737478197));
#12410=CARTESIAN_POINT('Ctrl Pts',(124.361040684506,4.67118206183956,331.365065264871));
#12411=CARTESIAN_POINT('Ctrl Pts',(124.353631691121,4.57127581859846,331.243489923773));
#12412=CARTESIAN_POINT('Ctrl Pts',(124.346218133541,4.47130802966539,331.121839688071));
#12413=CARTESIAN_POINT('Ctrl Pts',(124.338804575961,4.36657043650021,331.004291631627));
#12414=CARTESIAN_POINT('Ctrl Pts',(124.33139101838,4.2574492273283,330.891222001711));
#12415=CARTESIAN_POINT('Ctrl Pts',(124.323966906244,4.14817266413791,330.777991396477));
#12416=CARTESIAN_POINT('Ctrl Pts',(124.316542794107,4.03450028961519,330.669252208925));
#12417=CARTESIAN_POINT('Ctrl Pts',(124.30911868197,3.91685251908634,330.565341399135));
#12418=CARTESIAN_POINT('Ctrl Pts',(124.305261556816,3.85572976571972,330.511355549931));
#12419=CARTESIAN_POINT('Ctrl Pts',(124.301404431661,3.79353447278618,330.458672293386));
#12420=CARTESIAN_POINT('Ctrl Pts',(124.297547306506,3.73032864304282,330.407334240619));
#12421=CARTESIAN_POINT('Ctrl Pts',(124.290123329068,3.60867361886075,330.3085216457));
#12422=CARTESIAN_POINT('Ctrl Pts',(124.28269935163,3.48290619370343,330.214397101204));
#12423=CARTESIAN_POINT('Ctrl Pts',(124.275275374192,3.35342341629837,330.1253223744));
#12424=CARTESIAN_POINT('Ctrl Pts',(124.267860158165,3.22409344805238,330.036352769176));
#12425=CARTESIAN_POINT('Ctrl Pts',(124.260444942137,3.0910571598136,329.952421328543));
#12426=CARTESIAN_POINT('Ctrl Pts',(124.25302972611,2.95474552795087,329.873850428679));
#12427=CARTESIAN_POINT('Ctrl Pts',(124.245621644965,2.81856505445383,329.79535512934));
#12428=CARTESIAN_POINT('Ctrl Pts',(124.238213563821,2.67911583260145,329.722210287513));
#12429=CARTESIAN_POINT('Ctrl Pts',(124.230805482677,2.53685865874616,329.654695639344));
#12430=CARTESIAN_POINT('Ctrl Pts',(124.223402915503,2.39470736950351,329.587231243561));
#12431=CARTESIAN_POINT('Ctrl Pts',(124.216000348329,2.24975262549413,329.525388856563));
#12432=CARTESIAN_POINT('Ctrl Pts',(124.208597781155,2.10248062320287,329.469402763575));
#12433=CARTESIAN_POINT('Ctrl Pts',(124.201199111401,1.95528615897728,329.41344614702));
#12434=CARTESIAN_POINT('Ctrl Pts',(124.193800441646,1.8057772142,329.363339816159));
#12435=CARTESIAN_POINT('Ctrl Pts',(124.186401771891,1.65446070043183,329.319270262262));
#12436=CARTESIAN_POINT('Ctrl Pts',(124.179004322687,1.5031691491897,329.275207978472));
#12437=CARTESIAN_POINT('Ctrl Pts',(124.171606873483,1.35007097874838,329.2371805994));
#12438=CARTESIAN_POINT('Ctrl Pts',(124.164209424279,1.19568914168764,329.205325027325));
#12439=CARTESIAN_POINT('Ctrl Pts',(124.156812295816,1.04131399835427,329.173470836451));
#12440=CARTESIAN_POINT('Ctrl Pts',(124.149415167352,0.885655664578183,329.147787995919));
#12441=CARTESIAN_POINT('Ctrl Pts',(124.142018038889,0.729247925332657,329.128362406798));
#12442=CARTESIAN_POINT('Ctrl Pts',(124.134619771452,0.572816103199749,329.108933826622));
#12443=CARTESIAN_POINT('Ctrl Pts',(124.127221504016,0.415635016229508,329.095764462235));
#12444=CARTESIAN_POINT('Ctrl Pts',(124.119823236579,0.258244072589957,329.088888381914));
#12445=CARTESIAN_POINT('Ctrl Pts',(124.112422370053,0.100797835856634,329.082009885953));
#12446=CARTESIAN_POINT('Ctrl Pts',(124.105021503527,-0.0568580317113297,
329.081429092229));
#12447=CARTESIAN_POINT('Ctrl Pts',(124.097620637002,-0.214183765782614,
329.087127950228));
#12448=CARTESIAN_POINT('Ctrl Pts',(124.090211643617,-0.371682258550953,
329.092833066118));
#12449=CARTESIAN_POINT('Ctrl Pts',(124.082802650232,-0.528849520665383,
329.10483159121));
#12450=CARTESIAN_POINT('Ctrl Pts',(124.075393656847,-0.685149819527369,
329.123053489498));
#12451=CARTESIAN_POINT('Ctrl Pts',(124.067980099267,-0.841546404764826,
329.141286613104));
#12452=CARTESIAN_POINT('Ctrl Pts',(124.060566541687,-0.997074594709493,
329.165750691427));
#12453=CARTESIAN_POINT('Ctrl Pts',(124.053152984107,-1.15120900639713,329.196324579537));
#12454=CARTESIAN_POINT('Ctrl Pts',(124.04572887197,-1.30556285663778,329.226941995173));
#12455=CARTESIAN_POINT('Ctrl Pts',(124.038304759833,-1.45851860367209,329.263686506166));
#12456=CARTESIAN_POINT('Ctrl Pts',(124.030880647697,-1.60956537972557,329.30638692473));
#12457=CARTESIAN_POINT('Ctrl Pts',(124.027023522542,-1.6880402611301,329.328571511321));
#12458=CARTESIAN_POINT('Ctrl Pts',(124.023166397387,-1.76600017727977,329.352362926947));
#12459=CARTESIAN_POINT('Ctrl Pts',(124.019309272232,-1.84337574232694,329.377732091487));
#12460=CARTESIAN_POINT('Ctrl Pts',(124.011885294794,-1.99230387561708,329.426561231742));
#12461=CARTESIAN_POINT('Ctrl Pts',(124.004461317356,-2.13951518342932,329.481385550795));
#12462=CARTESIAN_POINT('Ctrl Pts',(123.997037339918,-2.28449058209917,329.542066934929));
#12463=CARTESIAN_POINT('Ctrl Pts',(123.989622123891,-2.42929488798597,329.602676705899));
#12464=CARTESIAN_POINT('Ctrl Pts',(123.982206907863,-2.5718681962005,329.669129640372));
#12465=CARTESIAN_POINT('Ctrl Pts',(123.974791691835,-2.71170618769361,329.741237777373));
#12466=CARTESIAN_POINT('Ctrl Pts',(123.967383610691,-2.8514096277751,329.813276532288));
#12467=CARTESIAN_POINT('Ctrl Pts',(123.959975529547,-2.98838266128292,329.890959487));
#12468=CARTESIAN_POINT('Ctrl Pts',(123.952567448403,-3.12214068877773,329.974050529305));
#12469=CARTESIAN_POINT('Ctrl Pts',(123.945164881229,-3.2557991577301,330.05707972543));
#12470=CARTESIAN_POINT('Ctrl Pts',(123.937762314055,-3.38624706979218,330.145508798021));
#12471=CARTESIAN_POINT('Ctrl Pts',(123.930359746881,-3.5130243007025,330.239055679261));
#12472=CARTESIAN_POINT('Ctrl Pts',(123.922961077126,-3.63973478395483,330.332553308477));
#12473=CARTESIAN_POINT('Ctrl Pts',(123.915562407372,-3.76277813538804,330.431163159045));
#12474=CARTESIAN_POINT('Ctrl Pts',(123.908163737617,-3.88172321158337,330.534559879345));
#12475=CARTESIAN_POINT('Ctrl Pts',(123.900766288413,-4.00064866553452,330.637939542397));
#12476=CARTESIAN_POINT('Ctrl Pts',(123.893368839209,-4.11547690467132,330.746104263301));
#12477=CARTESIAN_POINT('Ctrl Pts',(123.885971390005,-4.22580980530027,330.858688365756));
#12478=CARTESIAN_POINT('Ctrl Pts',(123.878574261541,-4.33613792208701,330.971267586759));
#12479=CARTESIAN_POINT('Ctrl Pts',(123.871177133078,-4.44197082668943,331.088265541764));
#12480=CARTESIAN_POINT('Ctrl Pts',(123.863780004614,-4.54294742138782,331.209279845596));
#12481=CARTESIAN_POINT('Ctrl Pts',(123.856381737178,-4.64393956396104,331.330312782609));
#12482=CARTESIAN_POINT('Ctrl Pts',(123.848983469741,-4.74007366863847,331.455363013227));
#12483=CARTESIAN_POINT('Ctrl Pts',(123.841585202305,-4.83102918196927,331.583995373911));
#12484=CARTESIAN_POINT('Ctrl Pts',(123.834184335779,-4.92201664892828,331.712672924496));
#12485=CARTESIAN_POINT('Ctrl Pts',(123.826783469253,-5.00782168699438,331.844934806164));
#12486=CARTESIAN_POINT('Ctrl Pts',(123.819382602727,-5.08816737777776,331.980317351406));
#12487=CARTESIAN_POINT('Ctrl Pts',(123.811973609343,-5.16860129581119,332.115848559626));
#12488=CARTESIAN_POINT('Ctrl Pts',(123.804564615958,-5.2435637038695,332.254506953758));
#12489=CARTESIAN_POINT('Ctrl Pts',(123.797155622573,-5.31282358107555,332.395804124328));
#12490=CARTESIAN_POINT('Ctrl Pts',(123.789742064993,-5.38212612475491,332.537188338829));
#12491=CARTESIAN_POINT('Ctrl Pts',(123.782328507413,-5.44571898715927,332.681214228331));
#12492=CARTESIAN_POINT('Ctrl Pts',(123.774914949832,-5.50341972677719,332.827374428619));
#12493=CARTESIAN_POINT('Ctrl Pts',(123.767490837696,-5.5612026139615,332.97374271471));
#12494=CARTESIAN_POINT('Ctrl Pts',(123.760066725559,-5.61307650207728,333.122251028857));
#12495=CARTESIAN_POINT('Ctrl Pts',(123.752642613422,-5.65890888671798,333.272377131917));
#12496=CARTESIAN_POINT('Ctrl Pts',(123.748785488268,-5.68272065578047,333.350373686631));
#12497=CARTESIAN_POINT('Ctrl Pts',(123.744928363113,-5.70490253077992,333.428806743467));
#12498=CARTESIAN_POINT('Ctrl Pts',(123.741071237958,-5.72544141714638,333.507602217462));
#12499=CARTESIAN_POINT('Ctrl Pts',(123.731427427444,-5.77679394535045,333.704611282535));
#12500=CARTESIAN_POINT('Ctrl Pts',(123.72178361693,-5.81799862666432,333.904366729355));
#12501=CARTESIAN_POINT('Ctrl Pts',(123.712139806416,-5.84881392545219,334.105960723493));
#12502=CARTESIAN_POINT('Ctrl Pts',(123.702686240882,-5.87902132595345,334.303577840936));
#12503=CARTESIAN_POINT('Ctrl Pts',(123.693232675347,-5.89924525418592,334.502961900108));
#12504=CARTESIAN_POINT('Ctrl Pts',(123.683779109812,-5.90930297922068,334.703236015875));
#12505=CARTESIAN_POINT('Ctrl Pts',(123.67920341457,-5.91417109849555,334.80017227928));
#12506=CARTESIAN_POINT('Ctrl Pts',(123.674627719327,-5.91665821897587,334.897316710721));
#12507=CARTESIAN_POINT('Ctrl Pts',(123.670052024084,-5.91674750630152,334.994567765212));
#12508=CARTESIAN_POINT('',(121.920052004703,-5.90729175175101,335.001447065376));
#12509=CARTESIAN_POINT('Ctrl Pts',(123.670052004703,-5.91540447174683,334.994569410092));
#12510=CARTESIAN_POINT('Ctrl Pts',(123.600979071031,-5.90216581006969,336.462314046667));
#12511=CARTESIAN_POINT('Ctrl Pts',(123.439160125933,-4.60789812849357,339.921680871558));
#12512=CARTESIAN_POINT('Ctrl Pts',(123.18459516941,1.19876002868579,341.893155831318));
#12513=CARTESIAN_POINT('Ctrl Pts',(122.906357135138,6.44531963394435,337.722219266979));
#12514=CARTESIAN_POINT('Ctrl Pts',(122.628119100863,5.77710454389356,331.053142261224));
#12515=CARTESIAN_POINT('Ctrl Pts',(122.34988106659,-0.192674116164957,328.006038346818));
#12516=CARTESIAN_POINT('Ctrl Pts',(122.113858701203,-5.10670098453427,330.865701816946));
#12517=CARTESIAN_POINT('Ctrl Pts',(121.970582347241,-5.90494040890748,333.923998790854));
#12518=CARTESIAN_POINT('Ctrl Pts',(121.920052004703,-5.90729175175101,335.001447065376));
#12519=CARTESIAN_POINT('',(120.170052004703,-5.92072775613925,335.004842343689));
#12520=CARTESIAN_POINT('Ctrl Pts',(121.920052004703,-5.90729175175101,335.001447065376));
#12521=CARTESIAN_POINT('Ctrl Pts',(121.877836335816,-5.90925618551375,335.901603235247));
#12522=CARTESIAN_POINT('Ctrl Pts',(121.742874655505,-5.29259387067636,338.776810722794));
#12523=CARTESIAN_POINT('Ctrl Pts',(121.515166963767,-0.817435776173097,
341.948699279223));
#12524=CARTESIAN_POINT('Ctrl Pts',(121.236928929494,5.40094806495304,339.447739079677));
#12525=CARTESIAN_POINT('Ctrl Pts',(120.958690895219,6.66296158473417,332.865154375237));
#12526=CARTESIAN_POINT('Ctrl Pts',(120.680452860945,1.81047360335528,328.241685990367));
#12527=CARTESIAN_POINT('Ctrl Pts',(120.417573230773,-4.34389803797753,329.733089300436));
#12528=CARTESIAN_POINT('Ctrl Pts',(120.247439612026,-5.90621016686413,333.364210861679));
#12529=CARTESIAN_POINT('Ctrl Pts',(120.170052004703,-5.92072775613925,335.004842343689));
#12530=CARTESIAN_POINT('',(118.420052004704,-5.92029571450889,334.995996540637));
#12531=CARTESIAN_POINT('Ctrl Pts',(120.170052004703,-5.92072775613925,335.004842343689));
#12532=CARTESIAN_POINT('Ctrl Pts',(120.154693600602,-5.92360892807864,335.330443330137));
#12533=CARTESIAN_POINT('Ctrl Pts',(120.046589185076,-5.75090023104754,337.619217809614));
#12534=CARTESIAN_POINT('Ctrl Pts',(119.845738758123,-2.76569986880471,341.426782021898));
#12535=CARTESIAN_POINT('Ctrl Pts',(119.56750072385,3.90773921675531,340.803636544015));
#12536=CARTESIAN_POINT('Ctrl Pts',(119.289262689575,6.99510370123495,334.854579471234));
#12537=CARTESIAN_POINT('Ctrl Pts',(119.011024655301,3.66316476665284,329.038972671294));
#12538=CARTESIAN_POINT('Ctrl Pts',(118.732786621027,-3.03040640606552,328.69371266629));
#12539=CARTESIAN_POINT('Ctrl Pts',(118.535795737496,-5.80051253301409,332.546564672477));
#12540=CARTESIAN_POINT('Ctrl Pts',(118.431550865387,-5.92485583227999,334.752456411305));
#12541=CARTESIAN_POINT('Ctrl Pts',(118.420052004704,-5.92296503915713,334.99599473557));
#12542=CARTESIAN_POINT('',(116.670052030361,-5.91201473463796,334.997295449063));
#12543=CARTESIAN_POINT('Ctrl Pts',(118.420052004704,-5.91674864718901,334.995998939257));
#12544=CARTESIAN_POINT('Ctrl Pts',(118.412737522599,-5.91685329486301,335.150751397025));
#12545=CARTESIAN_POINT('Ctrl Pts',(118.405423040495,-5.9108824720153,335.305741900391));
#12546=CARTESIAN_POINT('Ctrl Pts',(118.39810855839,-5.89880667231961,335.460445876404));
#12547=CARTESIAN_POINT('Ctrl Pts',(118.390801550831,-5.88674321268076,335.614991763023));
#12548=CARTESIAN_POINT('Ctrl Pts',(118.383494543273,-5.86858721879641,335.769251324649));
#12549=CARTESIAN_POINT('Ctrl Pts',(118.376187535715,-5.8443611934897,335.92269865207));
#12550=CARTESIAN_POINT('Ctrl Pts',(118.368886296861,-5.82015429403843,336.076024836573));
#12551=CARTESIAN_POINT('Ctrl Pts',(118.361585058006,-5.7898869595669,336.228539685085));
#12552=CARTESIAN_POINT('Ctrl Pts',(118.354283819152,-5.75363359786507,336.379721342887));
#12553=CARTESIAN_POINT('Ctrl Pts',(118.346868266374,-5.7168126250895,336.533270019335));
#12554=CARTESIAN_POINT('Ctrl Pts',(118.339452713596,-5.67381663270208,336.685443005712));
#12555=CARTESIAN_POINT('Ctrl Pts',(118.332037160818,-5.62477790671428,336.835702607352));
#12556=CARTESIAN_POINT('Ctrl Pts',(118.3247414092,-5.57653142055384,336.983534706269));
#12557=CARTESIAN_POINT('Ctrl Pts',(118.317445657582,-5.52243611057192,337.129514403159));
#12558=CARTESIAN_POINT('Ctrl Pts',(118.310149905963,-5.4626684853699,337.273143986079));
#12559=CARTESIAN_POINT('Ctrl Pts',(118.302854458138,-5.40290334887101,337.416767588312));
#12560=CARTESIAN_POINT('Ctrl Pts',(118.295559010312,-5.33746651456023,337.558040916098));
#12561=CARTESIAN_POINT('Ctrl Pts',(118.288263562487,-5.26658273076751,337.696486028609));
#12562=CARTESIAN_POINT('Ctrl Pts',(118.280966884809,-5.19568699752291,337.83495447993));
#12563=CARTESIAN_POINT('Ctrl Pts',(118.273670207131,-5.11934266325419,337.970593425154));
#12564=CARTESIAN_POINT('Ctrl Pts',(118.266373529452,-5.0378203929602,338.102949604936));
#12565=CARTESIAN_POINT('Ctrl Pts',(118.258868281371,-4.95396786586801,338.239089093091));
#12566=CARTESIAN_POINT('Ctrl Pts',(118.25136303329,-4.8646371873369,338.371754966557));
#12567=CARTESIAN_POINT('Ctrl Pts',(118.243857785209,-4.77017002033784,338.500486900357));
#12568=CARTESIAN_POINT('Ctrl Pts',(118.236550322751,-4.67819234432372,338.625826364595));
#12569=CARTESIAN_POINT('Ctrl Pts',(118.229242860292,-4.58134578891141,338.747436362512));
#12570=CARTESIAN_POINT('Ctrl Pts',(118.221935397834,-4.47998546807229,338.864927006861));
#12571=CARTESIAN_POINT('Ctrl Pts',(118.214331256942,-4.37450998120765,338.987187698344));
#12572=CARTESIAN_POINT('Ctrl Pts',(118.206727116049,-4.26414685358599,339.104987186631));
#12573=CARTESIAN_POINT('Ctrl Pts',(118.199122975157,-4.1493364253379,339.217930510554));
#12574=CARTESIAN_POINT('Ctrl Pts',(118.191518834265,-4.03452599708985,339.330873834477));
#12575=CARTESIAN_POINT('Ctrl Pts',(118.183914693372,-3.91526865943968,339.438960739679));
#12576=CARTESIAN_POINT('Ctrl Pts',(118.17631055248,-3.79204017945385,339.541845642457));
#12577=CARTESIAN_POINT('Ctrl Pts',(118.168886575042,-3.6717313282521,339.642292912932));
#12578=CARTESIAN_POINT('Ctrl Pts',(118.161462597604,-3.54724711066077,339.738108124031));
#12579=CARTESIAN_POINT('Ctrl Pts',(118.154038620166,-3.41897965128562,339.828924176936));
#12580=CARTESIAN_POINT('Ctrl Pts',(118.146623404138,-3.29086356681131,339.919633053234));
#12581=CARTESIAN_POINT('Ctrl Pts',(118.139208188111,-3.15897342943008,340.00535430134));
#12582=CARTESIAN_POINT('Ctrl Pts',(118.131792972083,-3.0237358205097,340.085759751528));
#12583=CARTESIAN_POINT('Ctrl Pts',(118.124384890939,-2.88862833653579,340.166087835998));
#12584=CARTESIAN_POINT('Ctrl Pts',(118.116976809795,-2.7501801119254,340.241110115777));
#12585=CARTESIAN_POINT('Ctrl Pts',(118.109568728651,-2.60884812142239,340.310540654383));
#12586=CARTESIAN_POINT('Ctrl Pts',(118.102166161477,-2.46762132690085,340.37991951457));
#12587=CARTESIAN_POINT('Ctrl Pts',(118.094763594303,-2.32351537389913,340.443714756949));
#12588=CARTESIAN_POINT('Ctrl Pts',(118.087361027129,-2.17701324906763,340.501685548619));
#12589=CARTESIAN_POINT('Ctrl Pts',(118.079962357374,-2.03058825696489,340.559625818921));
#12590=CARTESIAN_POINT('Ctrl Pts',(118.072563687619,-1.88176995168808,340.611747608753));
#12591=CARTESIAN_POINT('Ctrl Pts',(118.065165017865,-1.73106267882237,340.657857594928));
#12592=CARTESIAN_POINT('Ctrl Pts',(118.057767568661,-1.58038026797693,340.703959974388));
#12593=CARTESIAN_POINT('Ctrl Pts',(118.050370119457,-1.42780986454369,340.744052409432));
#12594=CARTESIAN_POINT('Ctrl Pts',(118.042972670253,-1.27387252366521,340.777990944606));
#12595=CARTESIAN_POINT('Ctrl Pts',(118.035575541789,-1.1199418572414,340.811928008265));
#12596=CARTESIAN_POINT('Ctrl Pts',(118.028178413326,-0.964644735675487,
340.839711622233));
#12597=CARTESIAN_POINT('Ctrl Pts',(118.020781284862,-0.808513734597942,
340.861248681251));
#12598=CARTESIAN_POINT('Ctrl Pts',(118.013383017426,-0.652358693243784,
340.882789056439));
#12599=CARTESIAN_POINT('Ctrl Pts',(118.005984749989,-0.495369886456328,
340.898080910577));
#12600=CARTESIAN_POINT('Ctrl Pts',(117.998586482553,-0.338086212866381,
340.907082890494));
#12601=CARTESIAN_POINT('Ctrl Pts',(117.991185616027,-0.180747283867814,
340.916088032902));
#12602=CARTESIAN_POINT('Ctrl Pts',(117.983784749501,-0.0231136541863968,
340.918798880269));
#12603=CARTESIAN_POINT('Ctrl Pts',(117.976383882975,0.134274717233284,340.915226188643));
#12604=CARTESIAN_POINT('Ctrl Pts',(117.968974889591,0.29183591613176,340.911649573861));
#12605=CARTESIAN_POINT('Ctrl Pts',(117.961565896206,0.44915094559031,340.901775649038));
#12606=CARTESIAN_POINT('Ctrl Pts',(117.954156902821,0.6056831756471,340.885667205444));
#12607=CARTESIAN_POINT('Ctrl Pts',(117.946743345241,0.762311834956978,340.869548838493));
#12608=CARTESIAN_POINT('Ctrl Pts',(117.939329787661,0.918156365390284,340.847188352593));
#12609=CARTESIAN_POINT('Ctrl Pts',(117.931916230081,1.0726897951362,340.818699783105));
#12610=CARTESIAN_POINT('Ctrl Pts',(117.924492117944,1.22744323151049,340.790170654924));
#12611=CARTESIAN_POINT('Ctrl Pts',(117.917068005807,1.38088147619017,340.75549610073));
#12612=CARTESIAN_POINT('Ctrl Pts',(117.90964389367,1.53249139509446,340.714840390288));
#12613=CARTESIAN_POINT('Ctrl Pts',(117.905786768516,1.61125885188146,340.693718111887));
#12614=CARTESIAN_POINT('Ctrl Pts',(117.901929643361,1.68953310047218,340.670982193367));
#12615=CARTESIAN_POINT('Ctrl Pts',(117.898072518206,1.76724436844757,340.646660774714));
#12616=CARTESIAN_POINT('Ctrl Pts',(117.890648540768,1.9168186438438,340.599848276778));
#12617=CARTESIAN_POINT('Ctrl Pts',(117.88322456333,2.06475725202675,340.547017951053));
#12618=CARTESIAN_POINT('Ctrl Pts',(117.875800585892,2.21053929064311,340.488300885249));
#12619=CARTESIAN_POINT('Ctrl Pts',(117.868385369865,2.35614928451976,340.429653114417));
#12620=CARTESIAN_POINT('Ctrl Pts',(117.860970153837,2.49960743202581,340.365132570175));
#12621=CARTESIAN_POINT('Ctrl Pts',(117.85355493781,2.64040692058352,340.294920382426));
#12622=CARTESIAN_POINT('Ctrl Pts',(117.846146856665,2.78107093258252,340.224775752492));
#12623=CARTESIAN_POINT('Ctrl Pts',(117.838738775521,2.91908104667356,340.148950547119));
#12624=CARTESIAN_POINT('Ctrl Pts',(117.831330694377,3.05394951751189,340.067674309482));
#12625=CARTESIAN_POINT('Ctrl Pts',(117.823928127203,3.18871760328419,339.986458567234));
#12626=CARTESIAN_POINT('Ctrl Pts',(117.816525560029,3.32034838357892,339.89980006321));
#12627=CARTESIAN_POINT('Ctrl Pts',(117.809122992855,3.44837796508353,339.80797462269));
#12628=CARTESIAN_POINT('Ctrl Pts',(117.8017243231,3.57634013957339,339.716197527862));
#12629=CARTESIAN_POINT('Ctrl Pts',(117.794325653346,3.70070458879116,339.619259131281));
#12630=CARTESIAN_POINT('Ctrl Pts',(117.786926983591,3.82103581280916,339.517478929639));
#12631=CARTESIAN_POINT('Ctrl Pts',(117.779529534387,3.94134718591134,339.41571551857));
#12632=CARTESIAN_POINT('Ctrl Pts',(117.772132085183,4.05762636966001,339.309112128482));
#12633=CARTESIAN_POINT('Ctrl Pts',(117.764734635979,4.1694703360073,339.198029023203));
#12634=CARTESIAN_POINT('Ctrl Pts',(117.757337507515,4.28130945299508,339.086950734295));
#12635=CARTESIAN_POINT('Ctrl Pts',(117.749940379052,4.38871347014439,338.971393379392));
#12636=CARTESIAN_POINT('Ctrl Pts',(117.742543250588,4.49131588602363,338.851754428108));
#12637=CARTESIAN_POINT('Ctrl Pts',(117.735144983152,4.59393410011392,338.732097055412));
#12638=CARTESIAN_POINT('Ctrl Pts',(117.727746715715,4.69174899786508,338.608357118295));
#12639=CARTESIAN_POINT('Ctrl Pts',(117.720348448279,4.78443417554128,338.48096540954));
#12640=CARTESIAN_POINT('Ctrl Pts',(117.712947581753,4.87715191449527,338.353528946737));
#12641=CARTESIAN_POINT('Ctrl Pts',(117.705546715227,4.96473612591647,338.22243845963));
#12642=CARTESIAN_POINT('Ctrl Pts',(117.698145848701,5.04690365202663,338.088153831929));
#12643=CARTESIAN_POINT('Ctrl Pts',(117.690736855316,5.12916140593576,337.95372174687));
#12644=CARTESIAN_POINT('Ctrl Pts',(117.683327861932,5.20599040107577,337.816088835141));
#12645=CARTESIAN_POINT('Ctrl Pts',(117.675918868547,5.27715303870011,337.675740340287));
#12646=CARTESIAN_POINT('Ctrl Pts',(117.668505310967,5.34835951496366,337.535305385919));
#12647=CARTESIAN_POINT('Ctrl Pts',(117.661091753386,5.41389252310431,337.392151853515));
#12648=CARTESIAN_POINT('Ctrl Pts',(117.653678195806,5.47356278320716,337.246784595993));
#12649=CARTESIAN_POINT('Ctrl Pts',(117.64625408367,5.53331799484952,337.101210381566));
#12650=CARTESIAN_POINT('Ctrl Pts',(117.638829971533,5.58719366095912,336.953416497253));
#12651=CARTESIAN_POINT('Ctrl Pts',(117.631405859396,5.63505023319088,336.803923344246));
#12652=CARTESIAN_POINT('Ctrl Pts',(117.627548734242,5.65991364920208,336.726255632567));
#12653=CARTESIAN_POINT('Ctrl Pts',(117.623691609087,5.68315321755644,336.648129436923));
#12654=CARTESIAN_POINT('Ctrl Pts',(117.619834483932,5.70475484390881,336.569618658592));
#12655=CARTESIAN_POINT('Ctrl Pts',(117.612410506494,5.74633243868109,336.41850553065));
#12656=CARTESIAN_POINT('Ctrl Pts',(117.604986529056,5.78196436029644,336.265511278244));
#12657=CARTESIAN_POINT('Ctrl Pts',(117.597562551618,5.81147895305511,336.111144878356));
#12658=CARTESIAN_POINT('Ctrl Pts',(117.590147335591,5.84095871415357,335.956960654047));
#12659=CARTESIAN_POINT('Ctrl Pts',(117.582732119563,5.864335447257,335.801407868586));
#12660=CARTESIAN_POINT('Ctrl Pts',(117.575316903535,5.88148720299975,335.645010731267));
#12661=CARTESIAN_POINT('Ctrl Pts',(117.567908822391,5.89862245540953,335.488764078487));
#12662=CARTESIAN_POINT('Ctrl Pts',(117.560500741247,5.90954461430555,335.331675059754));
#12663=CARTESIAN_POINT('Ctrl Pts',(117.553092660103,5.91418276044594,335.174278049519));
#12664=CARTESIAN_POINT('Ctrl Pts',(117.545690092929,5.91881745432944,335.016998192753));
#12665=CARTESIAN_POINT('Ctrl Pts',(117.538287525755,5.91717743770786,334.859411172393));
#12666=CARTESIAN_POINT('Ctrl Pts',(117.530884958581,5.90924361865239,334.702056351106));
#12667=CARTESIAN_POINT('Ctrl Pts',(117.523486288826,5.90131397671794,334.544784376445));
#12668=CARTESIAN_POINT('Ctrl Pts',(117.516087619072,5.88709715044508,334.387744729184));
#12669=CARTESIAN_POINT('Ctrl Pts',(117.508688949317,5.8666261374193,334.231476528498));
#12670=CARTESIAN_POINT('Ctrl Pts',(117.501291500113,5.84615850147507,334.075234107214));
#12671=CARTESIAN_POINT('Ctrl Pts',(117.493894050909,5.81943877489074,333.919763249614));
#12672=CARTESIAN_POINT('Ctrl Pts',(117.486496601705,5.78655180960394,333.765597830013));
#12673=CARTESIAN_POINT('Ctrl Pts',(117.479099473241,5.75366627023858,333.611439094755));
#12674=CARTESIAN_POINT('Ctrl Pts',(117.471702344778,5.71461410171396,333.458586049953));
#12675=CARTESIAN_POINT('Ctrl Pts',(117.464305216314,5.66953120975157,333.307561988091));
#12676=CARTESIAN_POINT('Ctrl Pts',(117.456906948878,5.62444137614927,333.156514672295));
#12677=CARTESIAN_POINT('Ctrl Pts',(117.449508681441,5.57331907694302,333.007297257817));
#12678=CARTESIAN_POINT('Ctrl Pts',(117.442110414005,5.51634993918263,332.860417351215));
#12679=CARTESIAN_POINT('Ctrl Pts',(117.434709547479,5.45936078756483,332.713485844158));
#12680=CARTESIAN_POINT('Ctrl Pts',(117.427308680953,5.39652084264469,332.568893827702));
#12681=CARTESIAN_POINT('Ctrl Pts',(117.419907814427,5.32806359752402,332.427128284729));
#12682=CARTESIAN_POINT('Ctrl Pts',(117.412498821042,5.2595311798037,332.285207069638));
#12683=CARTESIAN_POINT('Ctrl Pts',(117.405089827658,5.18536930577916,332.146118862639));
#12684=CARTESIAN_POINT('Ctrl Pts',(117.397680834273,5.10585744878188,332.010326058712));
#12685=CARTESIAN_POINT('Ctrl Pts',(117.390267276693,5.02629660973784,331.874449601733));
#12686=CARTESIAN_POINT('Ctrl Pts',(117.382853719112,4.94137942128065,331.74187290657));
#12687=CARTESIAN_POINT('Ctrl Pts',(117.375440161532,4.85142799477547,331.613028347623));
#12688=CARTESIAN_POINT('Ctrl Pts',(117.368016049395,4.76134850594714,331.484000354858));
#12689=CARTESIAN_POINT('Ctrl Pts',(117.360591937259,4.66622068990136,331.358715406627));
#12690=CARTESIAN_POINT('Ctrl Pts',(117.353167825122,4.56640664548534,331.237572471054));
#12691=CARTESIAN_POINT('Ctrl Pts',(117.349310699967,4.51454923083325,331.174633838732));
#12692=CARTESIAN_POINT('Ctrl Pts',(117.345453574813,4.46142751009049,331.112812622566));
#12693=CARTESIAN_POINT('Ctrl Pts',(117.341596449658,4.4070960011583,331.052160667014));
#12694=CARTESIAN_POINT('Ctrl Pts',(117.33417247222,4.30252177026849,330.935421196152));
#12695=CARTESIAN_POINT('Ctrl Pts',(117.326748494782,4.19314811677626,330.822663584307));
#12696=CARTESIAN_POINT('Ctrl Pts',(117.319324517344,4.07931015753743,330.714307617069));
#12697=CARTESIAN_POINT('Ctrl Pts',(117.311909301317,3.96560654421835,330.606079526176));
#12698=CARTESIAN_POINT('Ctrl Pts',(117.304494085289,3.84744937999032,330.502242994759));
#12699=CARTESIAN_POINT('Ctrl Pts',(117.297078869262,3.72521348983267,330.403184252369));
#12700=CARTESIAN_POINT('Ctrl Pts',(117.289670788117,3.60309521443302,330.304220823803));
#12701=CARTESIAN_POINT('Ctrl Pts',(117.282262706973,3.4769063141263,330.210026265571));
#12702=CARTESIAN_POINT('Ctrl Pts',(117.274854625829,3.34705777731504,330.120949395854));
#12703=CARTESIAN_POINT('Ctrl Pts',(117.267452058655,3.21730588914142,330.031938827679));
#12704=CARTESIAN_POINT('Ctrl Pts',(117.260049491481,3.08390009465115,329.948038573586));
#12705=CARTESIAN_POINT('Ctrl Pts',(117.252646924307,2.94728362368041,329.869556568474));
#12706=CARTESIAN_POINT('Ctrl Pts',(117.245248254553,2.81073908068388,329.791115883795));
#12707=CARTESIAN_POINT('Ctrl Pts',(117.237849584798,2.67098755055128,329.718087952245));
#12708=CARTESIAN_POINT('Ctrl Pts',(117.230450915043,2.52850024698414,329.65073677377));
#12709=CARTESIAN_POINT('Ctrl Pts',(117.223053465839,2.38603644939812,329.583396706147));
#12710=CARTESIAN_POINT('Ctrl Pts',(117.215656016635,2.24083811118513,329.521731692309));
#12711=CARTESIAN_POINT('Ctrl Pts',(117.208258567431,2.09340009689756,329.465959288476));
#12712=CARTESIAN_POINT('Ctrl Pts',(117.200861438968,1.94596847526519,329.410189302836));
#12713=CARTESIAN_POINT('Ctrl Pts',(117.193464310504,1.79629771971294,329.360311551241));
#12714=CARTESIAN_POINT('Ctrl Pts',(117.186067182041,1.64490142444076,329.316494931262));
#12715=CARTESIAN_POINT('Ctrl Pts',(117.178668914604,1.49348181791837,329.272671564617));
#12716=CARTESIAN_POINT('Ctrl Pts',(117.171270647168,1.34033650117289,329.234911291598));
#12717=CARTESIAN_POINT('Ctrl Pts',(117.163872379731,1.18599278483601,329.203332709494));
#12718=CARTESIAN_POINT('Ctrl Pts',(117.156471513205,1.03159484592813,329.171743033503));
#12719=CARTESIAN_POINT('Ctrl Pts',(117.149070646679,0.875998034604377,329.146339447025));
#12720=CARTESIAN_POINT('Ctrl Pts',(117.141669780154,0.719738221673399,329.127189135111));
#12721=CARTESIAN_POINT('Ctrl Pts',(117.134260786769,0.563306820529132,329.108017794323));
#12722=CARTESIAN_POINT('Ctrl Pts',(117.126851793384,0.406211334505276,329.095113486677));
#12723=CARTESIAN_POINT('Ctrl Pts',(117.119442799999,0.248991840460065,329.088491425543));
#12724=CARTESIAN_POINT('Ctrl Pts',(117.112029242419,0.0916754937840028,
329.08186528499));
#12725=CARTESIAN_POINT('Ctrl Pts',(117.104615684839,-0.0657646407985479,
329.08152910339));
#12726=CARTESIAN_POINT('Ctrl Pts',(117.097202127259,-0.222790657487817,
329.087445993022));
#12727=CARTESIAN_POINT('Ctrl Pts',(117.089778015122,-0.380040229459693,
329.093371306429));
#12728=CARTESIAN_POINT('Ctrl Pts',(117.082353902985,-0.536874134959452,
329.105567442068));
#12729=CARTESIAN_POINT('Ctrl Pts',(117.074929790849,-0.692760920715127,
329.123945807838));
#12730=CARTESIAN_POINT('Ctrl Pts',(117.071072665694,-0.773750382023262,
329.133494108781));
#12731=CARTESIAN_POINT('Ctrl Pts',(117.067215540539,-0.854484372817623,
329.144710289688));
#12732=CARTESIAN_POINT('Ctrl Pts',(117.063358415384,-0.934889793223836,
329.157576561304));
#12733=CARTESIAN_POINT('Ctrl Pts',(117.055934437946,-1.08964962160184,329.18234083686));
#12734=CARTESIAN_POINT('Ctrl Pts',(117.048510460508,-1.24365826274491,329.213295861666));
#12735=CARTESIAN_POINT('Ctrl Pts',(117.04108648307,-1.3963813590339,329.25038699888));
#12736=CARTESIAN_POINT('Ctrl Pts',(117.033671267043,-1.54892421909094,329.287434362972));
#12737=CARTESIAN_POINT('Ctrl Pts',(117.026256051015,-1.70018419503602,329.330603337855));
#12738=CARTESIAN_POINT('Ctrl Pts',(117.018840834987,-1.84963365889594,329.379787736181));
#12739=CARTESIAN_POINT('Ctrl Pts',(117.011432753843,-1.99893932323336,329.428924809526));
#12740=CARTESIAN_POINT('Ctrl Pts',(117.004024672699,-2.14643759147631,329.484065667575));
#12741=CARTESIAN_POINT('Ctrl Pts',(116.996616591555,-2.29161272556869,329.545053466943));
#12742=CARTESIAN_POINT('Ctrl Pts',(116.989214024381,-2.43667980315796,329.605995871978));
#12743=CARTESIAN_POINT('Ctrl Pts',(116.981811457207,-2.57942684698023,329.672776408968));
#12744=CARTESIAN_POINT('Ctrl Pts',(116.974408890033,-2.71935505091292,329.74518899773));
#12745=CARTESIAN_POINT('Ctrl Pts',(116.967010220278,-2.85920958325803,329.817563461581));
#12746=CARTESIAN_POINT('Ctrl Pts',(116.959611550524,-2.99624790077714,329.895563900634));
#12747=CARTESIAN_POINT('Ctrl Pts',(116.952212880769,-3.12999299951152,329.978936926755));
#12748=CARTESIAN_POINT('Ctrl Pts',(116.944815431565,-3.26371603445751,330.062296198914));
#12749=CARTESIAN_POINT('Ctrl Pts',(116.937417982361,-3.39414661244574,330.151026101863));
#12750=CARTESIAN_POINT('Ctrl Pts',(116.930020533157,-3.52083398620457,330.244828225596));
#12751=CARTESIAN_POINT('Ctrl Pts',(116.922623404693,-3.64751586702006,330.338626282233));
#12752=CARTESIAN_POINT('Ctrl Pts',(116.91522627623,-3.77045456636731,330.43749590029));
#12753=CARTESIAN_POINT('Ctrl Pts',(116.907829147766,-3.8892301193846,330.541096587616));
#12754=CARTESIAN_POINT('Ctrl Pts',(116.90043088033,-4.0080239608718,330.644713226861));
#12755=CARTESIAN_POINT('Ctrl Pts',(116.893032612893,-4.12265309840092,330.75306214051));
#12756=CARTESIAN_POINT('Ctrl Pts',(116.885634345456,-4.23273244294201,330.865764081603));
#12757=CARTESIAN_POINT('Ctrl Pts',(116.87823347893,-4.34285045951512,330.978505616073));
#12758=CARTESIAN_POINT('Ctrl Pts',(116.870832612405,-4.44841524009691,331.095602955928));
#12759=CARTESIAN_POINT('Ctrl Pts',(116.863431745879,-4.54908029690349,331.216641833658));
#12760=CARTESIAN_POINT('Ctrl Pts',(116.856022752494,-4.64985589356604,331.337813623648));
#12761=CARTESIAN_POINT('Ctrl Pts',(116.848613759109,-4.74572078279138,331.462935308015));
#12762=CARTESIAN_POINT('Ctrl Pts',(116.841204765724,-4.83636990475578,331.591560957436));
#12763=CARTESIAN_POINT('Ctrl Pts',(116.833791208144,-4.92707486970636,331.720265844694));
#12764=CARTESIAN_POINT('Ctrl Pts',(116.826377650564,-5.01255746272204,331.852478685551));
#12765=CARTESIAN_POINT('Ctrl Pts',(116.818964092983,-5.09255761178139,331.987727181481));
#12766=CARTESIAN_POINT('Ctrl Pts',(116.811539980847,-5.17267165569857,332.123168228405));
#12767=CARTESIAN_POINT('Ctrl Pts',(116.80411586871,-5.24728749044024,332.261653234254));
#12768=CARTESIAN_POINT('Ctrl Pts',(116.796691756573,-5.31619201513312,332.402687346365));
#12769=CARTESIAN_POINT('Ctrl Pts',(116.792834631419,-5.35199068984995,332.475960245727));
#12770=CARTESIAN_POINT('Ctrl Pts',(116.788977506264,-5.38624855896848,332.549920900035));
#12771=CARTESIAN_POINT('Ctrl Pts',(116.78512038111,-5.41894102331701,332.624498211259));
#12772=CARTESIAN_POINT('Ctrl Pts',(116.776934824929,-5.488320676014,332.782765507863));
#12773=CARTESIAN_POINT('Ctrl Pts',(116.768749268748,-5.55082719148128,332.944220960742));
#12774=CARTESIAN_POINT('Ctrl Pts',(116.760563712567,-5.60618584572961,333.108278343508));
#12775=CARTESIAN_POINT('Ctrl Pts',(116.752409291884,-5.6613339315994,333.271711699235));
#12776=CARTESIAN_POINT('Ctrl Pts',(116.744254871202,-5.70938830934361,333.437727012654));
#12777=CARTESIAN_POINT('Ctrl Pts',(116.736100450519,-5.75012310339411,333.605720667042));
#12778=CARTESIAN_POINT('Ctrl Pts',(116.727965705022,-5.79075961153875,333.773308982239));
#12779=CARTESIAN_POINT('Ctrl Pts',(116.719830959525,-5.82411169567996,333.942865884475));
#12780=CARTESIAN_POINT('Ctrl Pts',(116.711696214028,-5.85000251100064,334.113771370477));
#12781=CARTESIAN_POINT('Ctrl Pts',(116.703593916848,-5.87579005161965,334.28399513932));
#12782=CARTESIAN_POINT('Ctrl Pts',(116.695491619669,-5.89417563440154,334.455556524049));
#12783=CARTESIAN_POINT('Ctrl Pts',(116.68738932249,-5.90503317782377,334.62782567082));
#12784=CARTESIAN_POINT('Ctrl Pts',(116.681610235614,-5.91277748605137,334.750699263752));
#12785=CARTESIAN_POINT('Ctrl Pts',(116.675831148737,-5.91669293342916,334.873932560887));
#12786=CARTESIAN_POINT('Ctrl Pts',(116.67005206186,-5.91674938057594,334.997292611182));
#12787=CARTESIAN_POINT('',(114.920051985967,-5.91445891360904,335.005133702733));
#12788=CARTESIAN_POINT('Ctrl Pts',(116.670052004703,-5.90815805324423,334.997297760704));
#12789=CARTESIAN_POINT('Ctrl Pts',(116.615662118748,-5.90339216544283,336.156617696109));
#12790=CARTESIAN_POINT('Ctrl Pts',(116.468526221367,-5.01269847614412,339.29957741469));
#12791=CARTESIAN_POINT('Ctrl Pts',(116.228644312563,0.0981603043517565,
341.995926491601));
#12792=CARTESIAN_POINT('Ctrl Pts',(115.950406278288,5.93614401145467,338.703352156694));
#12793=CARTESIAN_POINT('Ctrl Pts',(115.672168244014,6.32661597658701,332.012266208978));
#12794=CARTESIAN_POINT('Ctrl Pts',(115.39393020974,0.911245840702667,328.062979462403));
#12795=CARTESIAN_POINT('Ctrl Pts',(115.143224796637,-4.72174289882804,330.240551757169));
#12796=CARTESIAN_POINT('Ctrl Pts',(114.985265394958,-5.9015978468786,333.617997724062));
#12797=CARTESIAN_POINT('Ctrl Pts',(114.920052004703,-5.91304802076869,335.005132079402));
#12798=CARTESIAN_POINT('',(113.170052004703,-5.92205629387471,335.000268163494));
#12799=CARTESIAN_POINT('Ctrl Pts',(114.920051955571,-5.91674777057043,335.005136336223));
#12800=CARTESIAN_POINT('Ctrl Pts',(114.911108166502,-5.91658252040811,335.19549449953));
#12801=CARTESIAN_POINT('Ctrl Pts',(114.902164377432,-5.90722704884812,335.385450638901));
#12802=CARTESIAN_POINT('Ctrl Pts',(114.893220588363,-5.88881999184248,335.574220921054));
#12803=CARTESIAN_POINT('Ctrl Pts',(114.883926180501,-5.86969133238817,335.770391468106));
#12804=CARTESIAN_POINT('Ctrl Pts',(114.874631772639,-5.8407873268764,335.965281261497));
#12805=CARTESIAN_POINT('Ctrl Pts',(114.865337364778,-5.80231725333009,336.15803499697));
#12806=CARTESIAN_POINT('Ctrl Pts',(114.856042956916,-5.76384717978377,336.350788732443));
#12807=CARTESIAN_POINT('Ctrl Pts',(114.846748549055,-5.71581115839886,336.541406475282));
#12808=CARTESIAN_POINT('Ctrl Pts',(114.837454141193,-5.65847091140766,336.729056825918));
#12809=CARTESIAN_POINT('Ctrl Pts',(114.830030163755,-5.61266996246214,336.87894393977));
#12810=CARTESIAN_POINT('Ctrl Pts',(114.822606186317,-5.56084027295747,337.027236078446));
#12811=CARTESIAN_POINT('Ctrl Pts',(114.815182208879,-5.50310940854717,337.173411465889));
#12812=CARTESIAN_POINT('Ctrl Pts',(114.807766992851,-5.44544667524294,337.319414344382));
#12813=CARTESIAN_POINT('Ctrl Pts',(114.800351776824,-5.38189676529112,337.463305100375));
#12814=CARTESIAN_POINT('Ctrl Pts',(114.792936560796,-5.31263738058319,337.604575709195));
#12815=CARTESIAN_POINT('Ctrl Pts',(114.785528479652,-5.24344463690651,337.745710388147));
#12816=CARTESIAN_POINT('Ctrl Pts',(114.778120398508,-5.1685535184537,337.884229606084));
#12817=CARTESIAN_POINT('Ctrl Pts',(114.770712317364,-5.08819026809218,338.019644078065));
#12818=CARTESIAN_POINT('Ctrl Pts',(114.76330975019,-5.00788683356546,338.154957758582));
#12819=CARTESIAN_POINT('Ctrl Pts',(114.755907183016,-4.92211956673602,338.287170974945));
#12820=CARTESIAN_POINT('Ctrl Pts',(114.748504615842,-4.83116115265796,338.415817981033));
#12821=CARTESIAN_POINT('Ctrl Pts',(114.741105946087,-4.74025062778728,338.544397255035));
#12822=CARTESIAN_POINT('Ctrl Pts',(114.733707276332,-4.64415461374849,338.669413754133));
#12823=CARTESIAN_POINT('Ctrl Pts',(114.726308606577,-4.5431896578316,338.79042982991));
#12824=CARTESIAN_POINT('Ctrl Pts',(114.718911157373,-4.44224135799756,338.911425941792));
#12825=CARTESIAN_POINT('Ctrl Pts',(114.71151370817,-4.33642594928277,339.02842265384));
#12826=CARTESIAN_POINT('Ctrl Pts',(114.704116258965,-4.22610096455406,339.141014513364));
#12827=CARTESIAN_POINT('Ctrl Pts',(114.696719130502,-4.11578076332436,339.253601491102));
#12828=CARTESIAN_POINT('Ctrl Pts',(114.689322002038,-4.00095163605661,339.36178372949));
#12829=CARTESIAN_POINT('Ctrl Pts',(114.681924873575,-3.88200856731397,339.465192050271));
#12830=CARTESIAN_POINT('Ctrl Pts',(114.674526606138,-3.76304718430788,339.568616293351));
#12831=CARTESIAN_POINT('Ctrl Pts',(114.667128338702,-3.6399708802243,339.667264910334));
#12832=CARTESIAN_POINT('Ctrl Pts',(114.659730071265,-3.51320823292414,339.760808594621));
#12833=CARTESIAN_POINT('Ctrl Pts',(114.652329204739,-3.38640105257265,339.854385141787));
#12834=CARTESIAN_POINT('Ctrl Pts',(114.644928338213,-3.25590525066864,339.942852964104));
#12835=CARTESIAN_POINT('Ctrl Pts',(114.637527471688,-3.12217878749545,340.025925803413));
#12836=CARTESIAN_POINT('Ctrl Pts',(114.630118478303,-2.98830547988117,340.109089864642));
#12837=CARTESIAN_POINT('Ctrl Pts',(114.622709484918,-2.8511947435109,340.186846914849));
#12838=CARTESIAN_POINT('Ctrl Pts',(114.615300491533,-2.7113302057046,340.258956082545));
#12839=CARTESIAN_POINT('Ctrl Pts',(114.607886933953,-2.57137950651857,340.331109671975));
#12840=CARTESIAN_POINT('Ctrl Pts',(114.600473376373,-2.42867196301874,340.397608288682));
#12841=CARTESIAN_POINT('Ctrl Pts',(114.593059818792,-2.28371113788016,340.458259246428));
#12842=CARTESIAN_POINT('Ctrl Pts',(114.585635706656,-2.13854393446848,340.518996551917));
#12843=CARTESIAN_POINT('Ctrl Pts',(114.578211594519,-1.99111739130797,340.573869441495));
#12844=CARTESIAN_POINT('Ctrl Pts',(114.570787482382,-1.84195095496589,340.622734854321));
#12845=CARTESIAN_POINT('Ctrl Pts',(114.566930357228,-1.76445298574589,340.648122403639));
#12846=CARTESIAN_POINT('Ctrl Pts',(114.563073232073,-1.68648557277676,340.671889239741));
#12847=CARTESIAN_POINT('Ctrl Pts',(114.559216106918,-1.60812252043137,340.694020769349));
#12848=CARTESIAN_POINT('Ctrl Pts',(114.55179212948,-1.45729372715926,340.736618292087));
#12849=CARTESIAN_POINT('Ctrl Pts',(114.544368152042,-1.30454368509424,340.773282985683));
#12850=CARTESIAN_POINT('Ctrl Pts',(114.536944174604,-1.15038019994917,340.803839759854));
#12851=CARTESIAN_POINT('Ctrl Pts',(114.529528958576,-0.996398650911766,
340.834360472434));
#12852=CARTESIAN_POINT('Ctrl Pts',(114.522113742549,-0.841007341654273,
340.858787541895));
#12853=CARTESIAN_POINT('Ctrl Pts',(114.514698526521,-0.684729645653049,
340.876995480249));
#12854=CARTESIAN_POINT('Ctrl Pts',(114.507290445377,-0.528602319264051,
340.895185899015));
#12855=CARTESIAN_POINT('Ctrl Pts',(114.499882364233,-0.371590672276281,
340.907169056833));
#12856=CARTESIAN_POINT('Ctrl Pts',(114.492474283089,-0.214228587833211,
340.912870425999));
#12857=CARTESIAN_POINT('Ctrl Pts',(114.485071715915,-0.0569836308636502,
340.918567551532));
#12858=CARTESIAN_POINT('Ctrl Pts',(114.477669148741,0.100610872827737,340.917992184858));
#12859=CARTESIAN_POINT('Ctrl Pts',(114.470266581567,0.258015701860771,340.911121590705));
#12860=CARTESIAN_POINT('Ctrl Pts',(114.462867911812,0.415337657939364,340.904254613889));
#12861=CARTESIAN_POINT('Ctrl Pts',(114.455469242057,0.572469766325245,340.891099026673));
#12862=CARTESIAN_POINT('Ctrl Pts',(114.448070572303,0.728872697225493,340.871684183753));
#12863=CARTESIAN_POINT('Ctrl Pts',(114.440673123099,0.885249826498768,340.85227254368));
#12864=CARTESIAN_POINT('Ctrl Pts',(114.433275673895,1.04089764701791,340.826603743178));
#12865=CARTESIAN_POINT('Ctrl Pts',(114.425878224691,1.19528172341699,340.794759025548));
#12866=CARTESIAN_POINT('Ctrl Pts',(114.418481096227,1.34965910599172,340.762915688648));
#12867=CARTESIAN_POINT('Ctrl Pts',(114.411083967764,1.50277248787793,340.724897042444));
#12868=CARTESIAN_POINT('Ctrl Pts',(114.4036868393,1.65409767039088,340.680835454342));
#12869=CARTESIAN_POINT('Ctrl Pts',(114.396288571864,1.8054461532044,340.636767081855));
#12870=CARTESIAN_POINT('Ctrl Pts',(114.388890304427,1.95500553005805,340.586654019139));
#12871=CARTESIAN_POINT('Ctrl Pts',(114.381492036991,2.10226695193475,340.530678459764));
#12872=CARTESIAN_POINT('Ctrl Pts',(114.374091170465,2.2495801082977,340.474683235587));
#12873=CARTESIAN_POINT('Ctrl Pts',(114.366690303939,2.39459335372001,340.412821546699));
#12874=CARTESIAN_POINT('Ctrl Pts',(114.359289437413,2.53681813902212,340.345323590956));
#12875=CARTESIAN_POINT('Ctrl Pts',(114.351880444029,2.67919910073561,340.277751516005));
#12876=CARTESIAN_POINT('Ctrl Pts',(114.344471450644,2.81878514999127,340.204530974227));
#12877=CARTESIAN_POINT('Ctrl Pts',(114.337062457259,2.9551120143209,340.12593830877));
#12878=CARTESIAN_POINT('Ctrl Pts',(114.329648899679,3.09152286070137,340.04729722752));
#12879=CARTESIAN_POINT('Ctrl Pts',(114.322235342099,3.22467020652081,339.963277626849));
#12880=CARTESIAN_POINT('Ctrl Pts',(114.314821784519,3.35411951115436,339.874198689774));
#12881=CARTESIAN_POINT('Ctrl Pts',(114.307397672382,3.48375311057188,339.784992932524));
#12882=CARTESIAN_POINT('Ctrl Pts',(114.299973560245,3.60967785591732,339.690713676329));
#12883=CARTESIAN_POINT('Ctrl Pts',(114.292549448109,3.73149234193394,339.59172031646));
#12884=CARTESIAN_POINT('Ctrl Pts',(114.288692322954,3.79477987175087,339.54028928047));
#12885=CARTESIAN_POINT('Ctrl Pts',(114.284835197799,3.85695855219829,339.487586418299));
#12886=CARTESIAN_POINT('Ctrl Pts',(114.280978072645,3.91797617169529,339.433665896358));
#12887=CARTESIAN_POINT('Ctrl Pts',(114.273554095207,4.03541945193731,339.329882710103));
#12888=CARTESIAN_POINT('Ctrl Pts',(114.266130117769,4.14891338754633,339.221273310476));
#12889=CARTESIAN_POINT('Ctrl Pts',(114.258706140331,4.25803593855763,339.108169970735));
#12890=CARTESIAN_POINT('Ctrl Pts',(114.251290924303,4.36702970854041,338.995200109953));
#12891=CARTESIAN_POINT('Ctrl Pts',(114.243875708276,4.47166210616983,338.87774713178));
#12892=CARTESIAN_POINT('Ctrl Pts',(114.236460492248,4.5715443784989,338.756183243389));
#12893=CARTESIAN_POINT('Ctrl Pts',(114.229052411104,4.67133054460841,338.634736323159));
#12894=CARTESIAN_POINT('Ctrl Pts',(114.22164432996,4.76637544917839,338.509186653799));
#12895=CARTESIAN_POINT('Ctrl Pts',(114.214236248816,4.85632750546997,338.379942857818));
#12896=CARTESIAN_POINT('Ctrl Pts',(114.206833681642,4.9462126088032,338.250795260355));
#12897=CARTESIAN_POINT('Ctrl Pts',(114.199431114468,5.03101219941007,338.117959316148));
#12898=CARTESIAN_POINT('Ctrl Pts',(114.192028547294,5.11041535508601,337.981876164599));
#12899=CARTESIAN_POINT('Ctrl Pts',(114.184629877539,5.18977670534751,337.845864660234));
#12900=CARTESIAN_POINT('Ctrl Pts',(114.177231207785,5.26374709148096,337.706609674915));
#12901=CARTESIAN_POINT('Ctrl Pts',(114.16983253803,5.332059336181,337.564580628084));
#12902=CARTESIAN_POINT('Ctrl Pts',(114.162435088826,5.40036031148194,337.422575011636));
#12903=CARTESIAN_POINT('Ctrl Pts',(114.155037639622,5.46300483627296,337.277796577933));
#12904=CARTESIAN_POINT('Ctrl Pts',(114.147640190418,5.51977201613607,337.13073871049));
#12905=CARTESIAN_POINT('Ctrl Pts',(114.140243061954,5.5765367346732,336.98368721922));
#12906=CARTESIAN_POINT('Ctrl Pts',(114.132845933491,5.62742448057049,336.834356838891));
#12907=CARTESIAN_POINT('Ctrl Pts',(114.125448805028,5.67226289041743,336.683260010959));
#12908=CARTESIAN_POINT('Ctrl Pts',(114.118050537591,5.71710820426018,336.532139917888));
#12909=CARTESIAN_POINT('Ctrl Pts',(114.110652270154,5.75590222123792,336.37925319346));
#12910=CARTESIAN_POINT('Ctrl Pts',(114.103254002718,5.78852278440978,336.225126335065));
#12911=CARTESIAN_POINT('Ctrl Pts',(114.095853136192,5.82115480752854,336.070945330283));
#12912=CARTESIAN_POINT('Ctrl Pts',(114.088452269666,5.84760898153712,335.915523689005));
#12913=CARTESIAN_POINT('Ctrl Pts',(114.081051403141,5.86781450273083,335.759396815928));
#12914=CARTESIAN_POINT('Ctrl Pts',(114.073642409756,5.88804221151854,335.603098500618));
#12915=CARTESIAN_POINT('Ctrl Pts',(114.066233416371,5.90200751654431,335.446093777312));
#12916=CARTESIAN_POINT('Ctrl Pts',(114.058824422986,5.9096915561831,335.288922607766));
#12917=CARTESIAN_POINT('Ctrl Pts',(114.051410865406,5.91738032945537,335.131654615358));
#12918=CARTESIAN_POINT('Ctrl Pts',(114.043997307826,5.91878012358746,334.974220344718));
#12919=CARTESIAN_POINT('Ctrl Pts',(114.036583750246,5.91392419152231,334.817157938572));
#12920=CARTESIAN_POINT('Ctrl Pts',(114.029159638109,5.90906134614886,334.659871925337));
#12921=CARTESIAN_POINT('Ctrl Pts',(114.021735525972,5.89792501352182,334.50295920522));
#12922=CARTESIAN_POINT('Ctrl Pts',(114.014311413836,5.88060019337428,334.346951817868));
#12923=CARTESIAN_POINT('Ctrl Pts',(114.010454288681,5.87159925179876,334.265899699176));
#12924=CARTESIAN_POINT('Ctrl Pts',(114.006597163526,5.86092874243482,334.185091777452));
#12925=CARTESIAN_POINT('Ctrl Pts',(114.002740038371,5.84860596029069,334.10460127108));
#12926=CARTESIAN_POINT('Ctrl Pts',(113.995316060933,5.82488776268465,333.949677674021));
#12927=CARTESIAN_POINT('Ctrl Pts',(113.987892083495,5.79497388229717,333.795463424136));
#12928=CARTESIAN_POINT('Ctrl Pts',(113.980468106057,5.75891534475801,333.642493235961));
#12929=CARTESIAN_POINT('Ctrl Pts',(113.97305289003,5.72289936171842,333.489703575624));
#12930=CARTESIAN_POINT('Ctrl Pts',(113.965637674002,5.68075324078695,333.338155414284));
#12931=CARTESIAN_POINT('Ctrl Pts',(113.958222457975,5.63257960238745,333.188377085244));
#12932=CARTESIAN_POINT('Ctrl Pts',(113.95081437683,5.58445231642026,333.038742872159));
#12933=CARTESIAN_POINT('Ctrl Pts',(113.943406295686,5.53030917250915,332.890875454082));
#12934=CARTESIAN_POINT('Ctrl Pts',(113.935998214542,5.4703035262807,332.745291616891));
#12935=CARTESIAN_POINT('Ctrl Pts',(113.928595647368,5.41034254335067,332.599816140409));
#12936=CARTESIAN_POINT('Ctrl Pts',(113.921193080194,5.34452788821302,332.456621204012));
#12937=CARTESIAN_POINT('Ctrl Pts',(113.91379051302,5.27306226655672,332.316206994659));
#12938=CARTESIAN_POINT('Ctrl Pts',(113.906391843265,5.20163427123788,332.175866712774));
#12939=CARTESIAN_POINT('Ctrl Pts',(113.898993173511,5.12456140356545,332.03830457398));
#12940=CARTESIAN_POINT('Ctrl Pts',(113.891594503756,5.04209382339125,331.903999283169));
#12941=CARTESIAN_POINT('Ctrl Pts',(113.884197054552,4.95963984780696,331.76971614856));
#12942=CARTESIAN_POINT('Ctrl Pts',(113.876799605348,4.87179312110084,331.63868911334));
#12943=CARTESIAN_POINT('Ctrl Pts',(113.869402156144,4.77884900134984,331.511370930466));
#12944=CARTESIAN_POINT('Ctrl Pts',(113.862005027681,4.68590891149383,331.384058267887));
#12945=CARTESIAN_POINT('Ctrl Pts',(113.854607899217,4.58787208809426,331.260454439348));
#12946=CARTESIAN_POINT('Ctrl Pts',(113.847210770754,4.4850761783726,331.140981700394));
#12947=CARTESIAN_POINT('Ctrl Pts',(113.839812503317,4.38226444064697,331.021490565621));
#12948=CARTESIAN_POINT('Ctrl Pts',(113.83241423588,4.27469240096722,330.906132069884));
#12949=CARTESIAN_POINT('Ctrl Pts',(113.825015968444,4.16273669609027,330.795293855509));
#12950=CARTESIAN_POINT('Ctrl Pts',(113.817615101918,4.05074165999677,330.684416702503));
#12951=CARTESIAN_POINT('Ctrl Pts',(113.810214235392,3.93436015756705,330.578063255017));
#12952=CARTESIAN_POINT('Ctrl Pts',(113.802813368867,3.81400410608604,330.476582791599));
#12953=CARTESIAN_POINT('Ctrl Pts',(113.795404375482,3.69351589215392,330.37499089293));
#12954=CARTESIAN_POINT('Ctrl Pts',(113.787995382097,3.56904469865514,330.278282905287));
#12955=CARTESIAN_POINT('Ctrl Pts',(113.780586388712,3.44103438384275,330.186766894102));
#12956=CARTESIAN_POINT('Ctrl Pts',(113.773172831132,3.31294521026089,330.095194505897));
#12957=CARTESIAN_POINT('Ctrl Pts',(113.765759273552,3.18131288229146,330.008820671728));
#12958=CARTESIAN_POINT('Ctrl Pts',(113.758345715972,3.04660793071028,329.927908648394));
#12959=CARTESIAN_POINT('Ctrl Pts',(113.750921603835,2.91171120196967,329.846881431982));
#12960=CARTESIAN_POINT('Ctrl Pts',(113.743497491698,2.77373343945004,329.771331735166));
#12961=CARTESIAN_POINT('Ctrl Pts',(113.736073379561,2.63316804487387,329.701475997039));
#12962=CARTESIAN_POINT('Ctrl Pts',(113.732216254407,2.5601386631356,329.665183128643));
#12963=CARTESIAN_POINT('Ctrl Pts',(113.728359129252,2.48641113290674,329.630426384411));
#12964=CARTESIAN_POINT('Ctrl Pts',(113.724502004097,2.41205638441086,329.597230843269));
#12965=CARTESIAN_POINT('Ctrl Pts',(113.717078026659,2.26894254881944,329.533337933759));
#12966=CARTESIAN_POINT('Ctrl Pts',(113.709654049221,2.12307237893853,329.475038974537));
#12967=CARTESIAN_POINT('Ctrl Pts',(113.702230071783,1.97492314052506,329.422580421779));
#12968=CARTESIAN_POINT('Ctrl Pts',(113.694814855756,1.82694874050307,329.370183778007));
#12969=CARTESIAN_POINT('Ctrl Pts',(113.687399639728,1.67670097411336,329.323613944313));
#12970=CARTESIAN_POINT('Ctrl Pts',(113.6799844237,1.52467966190233,329.283070536461));
#12971=CARTESIAN_POINT('Ctrl Pts',(113.672576342556,1.37280462383236,329.242566139271));
#12972=CARTESIAN_POINT('Ctrl Pts',(113.665168261412,1.21915979545529,329.208076719528));
#12973=CARTESIAN_POINT('Ctrl Pts',(113.657760180268,1.06426274256818,329.179752979703));
#12974=CARTESIAN_POINT('Ctrl Pts',(113.650357613094,0.909480982386633,329.151450321754));
#12975=CARTESIAN_POINT('Ctrl Pts',(113.64295504592,0.753449219101078,329.129304272746));
#12976=CARTESIAN_POINT('Ctrl Pts',(113.635552478746,0.596697766275196,329.113415053002));
#12977=CARTESIAN_POINT('Ctrl Pts',(113.628153808991,0.440028842404039,329.097534198863));
#12978=CARTESIAN_POINT('Ctrl Pts',(113.620755139236,0.282641353994469,329.087903650952));
#12979=CARTESIAN_POINT('Ctrl Pts',(113.613356469482,0.125073230051813,329.084572099195));
#12980=CARTESIAN_POINT('Ctrl Pts',(113.605959020278,-0.0324689000430316,
329.081241097041));
#12981=CARTESIAN_POINT('Ctrl Pts',(113.598561571074,-0.190191233763988,
329.084207036568));
#12982=CARTESIAN_POINT('Ctrl Pts',(113.59116412187,-0.347553206286898,329.093466555474));
#12983=CARTESIAN_POINT('Ctrl Pts',(113.583766993406,-0.504908355869133,
329.102725672904));
#12984=CARTESIAN_POINT('Ctrl Pts',(113.576369864943,-0.661902802753377,
329.118277805216));
#12985=CARTESIAN_POINT('Ctrl Pts',(113.568972736479,-0.817998742957661,
329.140067524363));
#12986=CARTESIAN_POINT('Ctrl Pts',(113.561574469043,-0.974118718040169,
329.161860598584));
#12987=CARTESIAN_POINT('Ctrl Pts',(113.554176201606,-1.12933954132454,329.189893120387));
#12988=CARTESIAN_POINT('Ctrl Pts',(113.546777934169,-1.28313141634874,329.224058143395));
#12989=CARTESIAN_POINT('Ctrl Pts',(113.539377067643,-1.43697732007584,329.258235168935));
#12990=CARTESIAN_POINT('Ctrl Pts',(113.531976201118,-1.58939291195257,329.298548904225));
#12991=CARTESIAN_POINT('Ctrl Pts',(113.524575334592,-1.73986156411689,329.344841973896));
#12992=CARTESIAN_POINT('Ctrl Pts',(113.517166341207,-1.89049544524665,329.391185877784));
#12993=CARTESIAN_POINT('Ctrl Pts',(113.509757347822,-2.03917776018813,329.443522118657));
#12994=CARTESIAN_POINT('Ctrl Pts',(113.502348354438,-2.18540925297769,329.501644158523));
#12995=CARTESIAN_POINT('Ctrl Pts',(113.494934796857,-2.33173082941097,329.559802003571));
#12996=CARTESIAN_POINT('Ctrl Pts',(113.487521239277,-2.4755982349946,329.623752598616));
#12997=CARTESIAN_POINT('Ctrl Pts',(113.480107681697,-2.61653546026782,329.693242727648));
#12998=CARTESIAN_POINT('Ctrl Pts',(113.47268356956,-2.75767333548291,329.762831788601));
#12999=CARTESIAN_POINT('Ctrl Pts',(113.465259457423,-2.89587237177943,329.837975956743));
#13000=CARTESIAN_POINT('Ctrl Pts',(113.457835345287,-3.03068355292361,329.918377447651));
#13001=CARTESIAN_POINT('Ctrl Pts',(113.453978220132,-3.10072338911183,329.960149259194));
#13002=CARTESIAN_POINT('Ctrl Pts',(113.450121094978,-3.16984927392779,330.003339443623));
#13003=CARTESIAN_POINT('Ctrl Pts',(113.446263969823,-3.23800173355183,330.047901925848));
#13004=CARTESIAN_POINT('Ctrl Pts',(113.438849585982,-3.36900824102305,330.133562446288));
#13005=CARTESIAN_POINT('Ctrl Pts',(113.431435202141,-3.4968133837742,330.224556072094));
#13006=CARTESIAN_POINT('Ctrl Pts',(113.4240208183,-3.62095233686414,330.320615987477));
#13007=CARTESIAN_POINT('Ctrl Pts',(113.416615191289,-3.74494467442623,330.416562450355));
#13008=CARTESIAN_POINT('Ctrl Pts',(113.409209564279,-3.86527914771921,330.517563066122));
#13009=CARTESIAN_POINT('Ctrl Pts',(113.401803937269,-3.98151805738212,330.623306668129));
#13010=CARTESIAN_POINT('Ctrl Pts',(113.39440543116,-4.09764519719585,330.72894859208));
#13011=CARTESIAN_POINT('Ctrl Pts',(113.387006925051,-4.2096843380371,330.83932417313));
#13012=CARTESIAN_POINT('Ctrl Pts',(113.379608418942,-4.31722926740279,330.954080819495));
#13013=CARTESIAN_POINT('Ctrl Pts',(113.372215403487,-4.42469438442869,331.068752301487));
#13014=CARTESIAN_POINT('Ctrl Pts',(113.364822388033,-4.52767167589312,331.187798103269));
#13015=CARTESIAN_POINT('Ctrl Pts',(113.357429372579,-4.62579045397227,331.310827567267));
#13016=CARTESIAN_POINT('Ctrl Pts',(113.350040221933,-4.72385793900427,331.433792715787));
#13017=CARTESIAN_POINT('Ctrl Pts',(113.342651071288,-4.81707173594637,331.56073708731));
#13018=CARTESIAN_POINT('Ctrl Pts',(113.335261920642,-4.90510035289923,331.691235715484));
#13019=CARTESIAN_POINT('Ctrl Pts',(113.327873945515,-4.9931149656312,331.821713583005));
#13020=CARTESIAN_POINT('Ctrl Pts',(113.320485970388,-5.07594582606789,331.955744275184));
#13021=CARTESIAN_POINT('Ctrl Pts',(113.313097995262,-5.15330378174896,332.092872432192));
#13022=CARTESIAN_POINT('Ctrl Pts',(113.305710294204,-5.23065886770477,332.229995502196));
#13023=CARTESIAN_POINT('Ctrl Pts',(113.298322593147,-5.30254126861194,332.370215482582));
#13024=CARTESIAN_POINT('Ctrl Pts',(113.29093489209,-5.36870711185131,332.513051164648));
#13025=CARTESIAN_POINT('Ctrl Pts',(113.283545996999,-5.43488364910755,332.65590993245));
#13026=CARTESIAN_POINT('Ctrl Pts',(113.276157101909,-5.49534163183526,332.801384903988));
#13027=CARTESIAN_POINT('Ctrl Pts',(113.268768206819,-5.54988485107399,332.948973744117));
#13028=CARTESIAN_POINT('Ctrl Pts',(113.261376649147,-5.60444772491199,333.096615767751));
#13029=CARTESIAN_POINT('Ctrl Pts',(113.253985091475,-5.653091462294,333.246372825637));
#13030=CARTESIAN_POINT('Ctrl Pts',(113.246593533803,-5.69566939665332,333.397726400852));
#13031=CARTESIAN_POINT('Ctrl Pts',(113.239193853586,-5.73829411968817,333.549246297741));
#13032=CARTESIAN_POINT('Ctrl Pts',(113.231794173369,-5.7748396276477,333.702365854845));
#13033=CARTESIAN_POINT('Ctrl Pts',(113.224394493152,-5.80521000822408,333.856554626178));
#13034=CARTESIAN_POINT('Ctrl Pts',(113.216990175569,-5.835599421864,334.01084002734));
#13035=CARTESIAN_POINT('Ctrl Pts',(113.209585857985,-5.8598059399352,334.16619560897));
#13036=CARTESIAN_POINT('Ctrl Pts',(113.202181540402,-5.87778548397389,334.322085280521));
#13037=CARTESIAN_POINT('Ctrl Pts',(113.194766836303,-5.89579024908249,334.478193628603));
#13038=CARTESIAN_POINT('Ctrl Pts',(113.187352132204,-5.90755056919457,334.634837190683));
#13039=CARTESIAN_POINT('Ctrl Pts',(113.179937428105,-5.91307444445758,334.791478593898));
#13040=CARTESIAN_POINT('Ctrl Pts',(113.176642286971,-5.91552928936512,334.861091018633));
#13041=CARTESIAN_POINT('Ctrl Pts',(113.173347145837,-5.91675314398094,334.930703063999));
#13042=CARTESIAN_POINT('Ctrl Pts',(113.170052004703,-5.91674999393393,335.000267923214));
#13043=CARTESIAN_POINT('',(111.420052816644,-5.91485974286145,334.994705964346));
#13044=CARTESIAN_POINT('Ctrl Pts',(113.170052004703,-5.92648485094407,335.000268364029));
#13045=CARTESIAN_POINT('Ctrl Pts',(113.169376648319,-5.92649426041998,335.014549503925));
#13046=CARTESIAN_POINT('Ctrl Pts',(113.168701291934,-5.92644711627134,335.028830579886));
#13047=CARTESIAN_POINT('Ctrl Pts',(113.168025935549,-5.92634323144412,335.043111243086));
#13048=CARTESIAN_POINT('Ctrl Pts',(113.075279924124,-5.91207683285968,337.00426032246));
#13049=CARTESIAN_POINT('Ctrl Pts',(112.889787901276,-3.74337052513098,340.910989767612));
#13050=CARTESIAN_POINT('Ctrl Pts',(112.611549867001,2.94492481531614,341.346655871666));
#13051=CARTESIAN_POINT('Ctrl Pts',(112.333311832728,6.93070611976698,335.95808955878));
#13052=CARTESIAN_POINT('Ctrl Pts',(112.055073798453,4.55628071516118,329.690298599179));
#13053=CARTESIAN_POINT('Ctrl Pts',(111.776835764179,-1.99937625115185,328.29514224405));
#13054=CARTESIAN_POINT('Ctrl Pts',(111.565162248396,-5.59083635352281,331.914700220535));
#13055=CARTESIAN_POINT('Ctrl Pts',(111.446234744037,-5.91862083319085,334.437990101302));
#13056=CARTESIAN_POINT('Ctrl Pts',(111.420053251102,-5.91384955313574,334.994697627575));
#13057=CARTESIAN_POINT('',(109.670051150406,-5.91183323294406,335.00229756853));
#13058=CARTESIAN_POINT('Ctrl Pts',(111.420052004703,-5.91674764548976,334.994721544598));
#13059=CARTESIAN_POINT('Ctrl Pts',(111.412711157276,-5.91688696497021,335.150888101892));
#13060=CARTESIAN_POINT('Ctrl Pts',(111.40537030985,-5.91083926829776,335.307182781746));
#13061=CARTESIAN_POINT('Ctrl Pts',(111.398029462423,-5.8986010122119,335.463073062521));
#13062=CARTESIAN_POINT('Ctrl Pts',(111.390626555473,-5.88625929391097,335.620281239706));
#13063=CARTESIAN_POINT('Ctrl Pts',(111.383223648524,-5.86762182953684,335.777077758205));
#13064=CARTESIAN_POINT('Ctrl Pts',(111.375820741574,-5.84273868919298,335.932917559223));
#13065=CARTESIAN_POINT('Ctrl Pts',(111.368484115834,-5.81807833763348,336.087362063694));
#13066=CARTESIAN_POINT('Ctrl Pts',(111.361147490094,-5.7872837741526,336.240866533846));
#13067=CARTESIAN_POINT('Ctrl Pts',(111.353810864354,-5.75045564278118,336.392907198239));
#13068=CARTESIAN_POINT('Ctrl Pts',(111.346474105685,-5.71362684413768,336.544950617387));
#13069=CARTESIAN_POINT('Ctrl Pts',(111.339137347016,-5.67076434911301,336.695529808621));
#13070=CARTESIAN_POINT('Ctrl Pts',(111.331800588347,-5.62201945940217,336.844133335907));
#13071=CARTESIAN_POINT('Ctrl Pts',(111.324462190267,-5.57326367756963,336.992770068883));
#13072=CARTESIAN_POINT('Ctrl Pts',(111.317123792188,-5.51862300344348,337.139429898357));
#13073=CARTESIAN_POINT('Ctrl Pts',(111.309785394109,-5.45829785252835,337.283618863905));
#13074=CARTESIAN_POINT('Ctrl Pts',(111.302333252569,-5.39703767582811,337.430042724828));
#13075=CARTESIAN_POINT('Ctrl Pts',(111.294881111029,-5.32991549936494,337.573918115048));
#13076=CARTESIAN_POINT('Ctrl Pts',(111.287428969489,-5.25719048201953,337.714752069391));
#13077=CARTESIAN_POINT('Ctrl Pts',(111.280079056957,-5.18546311163429,337.853654053532));
#13078=CARTESIAN_POINT('Ctrl Pts',(111.272729144425,-5.10828588806572,337.989597218341));
#13079=CARTESIAN_POINT('Ctrl Pts',(111.265379231893,-5.02595180002468,338.122136939074));
#13080=CARTESIAN_POINT('Ctrl Pts',(111.257875975849,-4.94189995029351,338.257441877228));
#13081=CARTESIAN_POINT('Ctrl Pts',(111.250372719806,-4.85247393290783,338.389199448089));
#13082=CARTESIAN_POINT('Ctrl Pts',(111.242869463762,-4.75802902184952,338.516971764137));
#13083=CARTESIAN_POINT('Ctrl Pts',(111.235366207718,-4.66358411079121,338.644744080186));
#13084=CARTESIAN_POINT('Ctrl Pts',(111.227862951675,-4.56412061731915,338.768530860917));
#13085=CARTESIAN_POINT('Ctrl Pts',(111.220359695631,-4.46003343831345,338.887934193325));
#13086=CARTESIAN_POINT('Ctrl Pts',(111.212935718193,-4.35704603337513,339.006075922817));
#13087=CARTESIAN_POINT('Ctrl Pts',(111.205511740755,-4.24920584456463,339.120301002308));
#13088=CARTESIAN_POINT('Ctrl Pts',(111.198087763317,-4.1368422863769,339.230185156721));
#13089=CARTESIAN_POINT('Ctrl Pts',(111.190672547289,-4.02461133409392,339.339939631299));
#13090=CARTESIAN_POINT('Ctrl Pts',(111.183257331262,-3.90786790255102,339.445363119701));
#13091=CARTESIAN_POINT('Ctrl Pts',(111.175842115234,-3.78698156412167,339.546064363326));
#13092=CARTESIAN_POINT('Ctrl Pts',(111.16843403409,-3.66621154191839,339.646668712722));
#13093=CARTESIAN_POINT('Ctrl Pts',(111.161025952946,-3.54130683361324,339.742559625765));
#13094=CARTESIAN_POINT('Ctrl Pts',(111.153617871802,-3.41267367717123,339.833382763204));
#13095=CARTESIAN_POINT('Ctrl Pts',(111.146215304628,-3.28413626473679,339.924138299324));
#13096=CARTESIAN_POINT('Ctrl Pts',(111.138812737454,-3.15187623346712,340.009833356178));
#13097=CARTESIAN_POINT('Ctrl Pts',(111.13141017028,-3.0163326121967,340.090154038445));
#13098=CARTESIAN_POINT('Ctrl Pts',(111.124011500525,-2.88086035405,340.170432432224));
#13099=CARTESIAN_POINT('Ctrl Pts',(111.11661283077,-2.7421082691653,340.245341896921));
#13100=CARTESIAN_POINT('Ctrl Pts',(111.109214161016,-2.60054396129825,340.314612090064));
#13101=CARTESIAN_POINT('Ctrl Pts',(111.101816711812,-2.4590030071468,340.383870855776));
#13102=CARTESIAN_POINT('Ctrl Pts',(111.094419262608,-2.31465108566736,340.447492032413));
#13103=CARTESIAN_POINT('Ctrl Pts',(111.087021813404,-2.16798007681421,340.505251397442));
#13104=CARTESIAN_POINT('Ctrl Pts',(111.07962468494,-2.0213154273601,340.563008258125));
#13105=CARTESIAN_POINT('Ctrl Pts',(111.072227556477,-1.87233223771711,340.6149036758));
#13106=CARTESIAN_POINT('Ctrl Pts',(111.064830428013,-1.72154177321008,340.660761829082));
#13107=CARTESIAN_POINT('Ctrl Pts',(111.057432160577,-1.57072809073576,340.706627043375));
#13108=CARTESIAN_POINT('Ctrl Pts',(111.05003389314,-1.41810693640083,340.746453033746));
#13109=CARTESIAN_POINT('Ctrl Pts',(111.042635625704,-1.26420397032278,340.780114089179));
#13110=CARTESIAN_POINT('Ctrl Pts',(111.035234759178,-1.11024693651417,340.813786970094));
#13111=CARTESIAN_POINT('Ctrl Pts',(111.027833892652,-0.955007558751131,
340.84129052426));
#13112=CARTESIAN_POINT('Ctrl Pts',(111.020433026126,-0.79902075118346,340.86255033255));
#13113=CARTESIAN_POINT('Ctrl Pts',(111.013024032742,-0.642862655188266,
340.883833486141));
#13114=CARTESIAN_POINT('Ctrl Pts',(111.005615039357,-0.485955860321188,
340.898859151168));
#13115=CARTESIAN_POINT('Ctrl Pts',(110.998206045972,-0.328840188593058,
340.90760481861));
#13116=CARTESIAN_POINT('Ctrl Pts',(110.990792488392,-0.171627728191757,
340.916355873685));
#13117=CARTESIAN_POINT('Ctrl Pts',(110.983378930812,-0.0142065068204832,
340.918819216462));
#13118=CARTESIAN_POINT('Ctrl Pts',(110.975965373231,0.142885120426389,340.915024463589));
#13119=CARTESIAN_POINT('Ctrl Pts',(110.968541261095,0.300200396364228,340.911224308191));
#13120=CARTESIAN_POINT('Ctrl Pts',(110.961117148958,0.457184769575989,340.90114828684));
#13121=CARTESIAN_POINT('Ctrl Pts',(110.953693036821,0.61330563832227,340.884877803022));
#13122=CARTESIAN_POINT('Ctrl Pts',(110.949835911667,0.694416715164889,340.876424631619));
#13123=CARTESIAN_POINT('Ctrl Pts',(110.945978786512,0.775294879731979,340.866300280802));
#13124=CARTESIAN_POINT('Ctrl Pts',(110.942121661357,0.855866798469,340.854521550543));
#13125=CARTESIAN_POINT('Ctrl Pts',(110.934697683919,1.01094709347015,340.83185051339));
#13126=CARTESIAN_POINT('Ctrl Pts',(110.927273706481,1.16535991373322,340.802979142696));
#13127=CARTESIAN_POINT('Ctrl Pts',(110.919849729043,1.31857021221013,340.767954850549));
#13128=CARTESIAN_POINT('Ctrl Pts',(110.912434513016,1.47159969948322,340.732971892337));
#13129=CARTESIAN_POINT('Ctrl Pts',(110.905019296988,1.62342912953639,340.691850548913));
#13130=CARTESIAN_POINT('Ctrl Pts',(110.897604080961,1.77352948784842,340.644689869092));
#13131=CARTESIAN_POINT('Ctrl Pts',(110.890195999816,1.92348542035144,340.59757456704));
#13132=CARTESIAN_POINT('Ctrl Pts',(110.882787918672,2.07171523956719,340.544431608368));
#13133=CARTESIAN_POINT('Ctrl Pts',(110.875379837528,2.2177011353867,340.485410853947));
#13134=CARTESIAN_POINT('Ctrl Pts',(110.867977270354,2.36357837123802,340.426434029752));
#13135=CARTESIAN_POINT('Ctrl Pts',(110.86057470318,2.50721466476932,340.361588260258));
#13136=CARTESIAN_POINT('Ctrl Pts',(110.853172136006,2.6481084710155,340.291072867409));
#13137=CARTESIAN_POINT('Ctrl Pts',(110.845773466251,2.78892809728785,340.220594600608));
#13138=CARTESIAN_POINT('Ctrl Pts',(110.838374796497,2.92700777899786,340.144452821934));
#13139=CARTESIAN_POINT('Ctrl Pts',(110.830976126742,3.06186713217097,340.06289445154));
#13140=CARTESIAN_POINT('Ctrl Pts',(110.823578677538,3.19670423773869,339.981349535744));
#13141=CARTESIAN_POINT('Ctrl Pts',(110.816181228334,3.32832175009543,339.894389994619));
#13142=CARTESIAN_POINT('Ctrl Pts',(110.80878377913,3.45626493126137,339.802308120834));
#13143=CARTESIAN_POINT('Ctrl Pts',(110.801386650667,3.58420256503402,339.710230239559));
#13144=CARTESIAN_POINT('Ctrl Pts',(110.793989522203,3.70846588146624,339.613030685234));
#13145=CARTESIAN_POINT('Ctrl Pts',(110.78659239374,3.82863035360154,339.511044244738));
#13146=CARTESIAN_POINT('Ctrl Pts',(110.779194126303,3.94881332806575,339.409042100876));
#13147=CARTESIAN_POINT('Ctrl Pts',(110.771795858866,4.06489591702984,339.302251844771));
#13148=CARTESIAN_POINT('Ctrl Pts',(110.76439759143,4.17648794256494,339.191047485786));
#13149=CARTESIAN_POINT('Ctrl Pts',(110.756996724904,4.28811917155207,339.07980405954));
#13150=CARTESIAN_POINT('Ctrl Pts',(110.749595858378,4.39525643195436,338.964143706205));
#13151=CARTESIAN_POINT('Ctrl Pts',(110.742194991853,4.49754767039888,338.844475974042));
#13152=CARTESIAN_POINT('Ctrl Pts',(110.734785998468,4.59995123440293,338.724676835269));
#13153=CARTESIAN_POINT('Ctrl Pts',(110.727377005083,4.69749790669539,338.600861813524));
#13154=CARTESIAN_POINT('Ctrl Pts',(110.719968011698,4.78987663029553,338.473472675731));
#13155=CARTESIAN_POINT('Ctrl Pts',(110.712554454118,4.88231226237568,338.346005061835));
#13156=CARTESIAN_POINT('Ctrl Pts',(110.705140896538,4.96957339558215,338.214959254473));
#13157=CARTESIAN_POINT('Ctrl Pts',(110.697727338957,5.0513936003527,338.080803995196));
#13158=CARTESIAN_POINT('Ctrl Pts',(110.690303226821,5.13333029116406,337.946457741347));
#13159=CARTESIAN_POINT('Ctrl Pts',(110.682879114684,5.20981040195362,337.808993519483));
#13160=CARTESIAN_POINT('Ctrl Pts',(110.675455002547,5.28061416528821,337.668903257868));
#13161=CARTESIAN_POINT('Ctrl Pts',(110.671597877393,5.31739957094704,337.596120726832));
#13162=CARTESIAN_POINT('Ctrl Pts',(110.667740752238,5.35265360398758,337.522629685625));
#13163=CARTESIAN_POINT('Ctrl Pts',(110.663883627083,5.38635070686979,337.448500893425));
#13164=CARTESIAN_POINT('Ctrl Pts',(110.656459649645,5.45120899419265,337.305821965798));
#13165=CARTESIAN_POINT('Ctrl Pts',(110.649035672207,5.51049207988238,337.160348975664));
#13166=CARTESIAN_POINT('Ctrl Pts',(110.641611694769,5.56395028911653,337.012557512902));
#13167=CARTESIAN_POINT('Ctrl Pts',(110.634196478742,5.61734540962053,336.864940466303));
#13168=CARTESIAN_POINT('Ctrl Pts',(110.626781262714,5.66492921122269,336.715010740964));
#13169=CARTESIAN_POINT('Ctrl Pts',(110.619366046686,5.70649870607189,336.563266797479));
#13170=CARTESIAN_POINT('Ctrl Pts',(110.611957965542,5.74802820296249,336.411668861252));
#13171=CARTESIAN_POINT('Ctrl Pts',(110.604549884398,5.78355481586299,336.258260539649));
#13172=CARTESIAN_POINT('Ctrl Pts',(110.597141803254,5.81292434921464,336.103558368555));
#13173=CARTESIAN_POINT('Ctrl Pts',(110.58973923608,5.84227202228622,335.948971345112));
#13174=CARTESIAN_POINT('Ctrl Pts',(110.582336668906,5.86547167157338,335.793092754813));
#13175=CARTESIAN_POINT('Ctrl Pts',(110.574934101732,5.88241949639207,335.636452222061));
#13176=CARTESIAN_POINT('Ctrl Pts',(110.567535431977,5.89935839825507,335.479894159865));
#13177=CARTESIAN_POINT('Ctrl Pts',(110.560136762223,5.91005199093873,335.322575324259));
#13178=CARTESIAN_POINT('Ctrl Pts',(110.552738092468,5.9144479515326,335.165033303039));
#13179=CARTESIAN_POINT('Ctrl Pts',(110.545340643264,5.91884318692946,335.00751727136));
#13180=CARTESIAN_POINT('Ctrl Pts',(110.53794319406,5.91694284174497,334.849778499843));
#13181=CARTESIAN_POINT('Ctrl Pts',(110.530545744856,5.90874662630595,334.692357563691));
#13182=CARTESIAN_POINT('Ctrl Pts',(110.523148616393,5.90055076624054,334.534943453037));
#13183=CARTESIAN_POINT('Ctrl Pts',(110.515751487929,5.88605959809588,334.377847523053));
#13184=CARTESIAN_POINT('Ctrl Pts',(110.508354359466,5.8653249154058,334.221607939904));
#13185=CARTESIAN_POINT('Ctrl Pts',(110.500956092029,5.84458704009223,334.065344299761));
#13186=CARTESIAN_POINT('Ctrl Pts',(110.493557824592,5.81760378516971,333.909937638986));
#13187=CARTESIAN_POINT('Ctrl Pts',(110.486159557156,5.7844785154243,333.755918464451));
#13188=CARTESIAN_POINT('Ctrl Pts',(110.47875869063,5.75134160842319,333.601845181359));
#13189=CARTESIAN_POINT('Ctrl Pts',(110.471357824104,5.71205846893741,333.449160719635));
#13190=CARTESIAN_POINT('Ctrl Pts',(110.463956957579,5.66678297855492,333.298382758532));
#13191=CARTESIAN_POINT('Ctrl Pts',(110.456547964194,5.62145777135548,333.147439228814));
#13192=CARTESIAN_POINT('Ctrl Pts',(110.449138970809,5.57012717969713,332.998406738246));
#13193=CARTESIAN_POINT('Ctrl Pts',(110.441729977424,5.51299436402923,332.85178592671));
#13194=CARTESIAN_POINT('Ctrl Pts',(110.434316419844,5.45582635257627,332.705074791697));
#13195=CARTESIAN_POINT('Ctrl Pts',(110.426902862264,5.39284914364688,332.560778637379));
#13196=CARTESIAN_POINT('Ctrl Pts',(110.419489304684,5.32431273168775,332.419375173008));
#13197=CARTESIAN_POINT('Ctrl Pts',(110.412065192547,5.25567874559884,332.277770394918));
#13198=CARTESIAN_POINT('Ctrl Pts',(110.40464108041,5.18146992513943,332.139066859978));
#13199=CARTESIAN_POINT('Ctrl Pts',(110.397216968274,5.10198101451226,332.00371558592));
#13200=CARTESIAN_POINT('Ctrl Pts',(110.393359843119,5.06068332516423,331.933395149714));
#13201=CARTESIAN_POINT('Ctrl Pts',(110.389502717964,5.01796112090388,331.863979061905));
#13202=CARTESIAN_POINT('Ctrl Pts',(110.385645592809,4.97386007398293,331.795527106225));
#13203=CARTESIAN_POINT('Ctrl Pts',(110.378221615371,4.88897686065786,331.66377463407));
#13204=CARTESIAN_POINT('Ctrl Pts',(110.370797637933,4.79872699905348,331.535198440364));
#13205=CARTESIAN_POINT('Ctrl Pts',(110.363373660495,4.70337530947232,331.410265850965));
#13206=CARTESIAN_POINT('Ctrl Pts',(110.355958444468,4.60813614923138,331.285480700819));
#13207=CARTESIAN_POINT('Ctrl Pts',(110.34854322844,4.50780736998794,331.164330889549));
#13208=CARTESIAN_POINT('Ctrl Pts',(110.341128012412,4.40269828951588,331.047256859598));
#13209=CARTESIAN_POINT('Ctrl Pts',(110.333719931268,4.2976903444719,330.93029547769));
#13210=CARTESIAN_POINT('Ctrl Pts',(110.326311850124,4.18791150277028,330.817402345588));
#13211=CARTESIAN_POINT('Ctrl Pts',(110.31890376898,4.07371268639084,330.708986656833));
#13212=CARTESIAN_POINT('Ctrl Pts',(110.311501201806,3.95959887027595,330.600651663855));
#13213=CARTESIAN_POINT('Ctrl Pts',(110.304098634632,3.8410718995945,330.496787734304));
#13214=CARTESIAN_POINT('Ctrl Pts',(110.296696067458,3.71852097429914,330.397768766544));
#13215=CARTESIAN_POINT('Ctrl Pts',(110.289297397703,3.59603457153095,330.298801931838));
#13216=CARTESIAN_POINT('Ctrl Pts',(110.281898727949,3.46952872301975,330.204675212714));
#13217=CARTESIAN_POINT('Ctrl Pts',(110.274500058194,3.33942718288179,330.115723528225));
#13218=CARTESIAN_POINT('Ctrl Pts',(110.26710260899,3.20934710545753,330.026786518003));
#13219=CARTESIAN_POINT('Ctrl Pts',(110.259705159786,3.07567282145844,329.943023058494));
#13220=CARTESIAN_POINT('Ctrl Pts',(110.252307710582,2.93885875534673,329.864725929551));
#13221=CARTESIAN_POINT('Ctrl Pts',(110.244910582118,2.80205062125432,329.786432195436));
#13222=CARTESIAN_POINT('Ctrl Pts',(110.237513453655,2.66210329964956,329.713604506008));
#13223=CARTESIAN_POINT('Ctrl Pts',(110.230116325192,2.51949737439505,329.64649053957));
#13224=CARTESIAN_POINT('Ctrl Pts',(110.222718057755,2.37686949138777,329.579366239256));
#13225=CARTESIAN_POINT('Ctrl Pts',(110.215319790318,2.23158252734815,329.517957572605));
#13226=CARTESIAN_POINT('Ctrl Pts',(110.207921522882,2.08413853343867,329.462464705671));
#13227=CARTESIAN_POINT('Ctrl Pts',(110.200520656356,1.93664274090411,329.40695234351));
#13228=CARTESIAN_POINT('Ctrl Pts',(110.19311978983,1.78698875881798,329.357360050301));
#13229=CARTESIAN_POINT('Ctrl Pts',(110.185718923304,1.63569518886718,329.313838569684));
#13230=CARTESIAN_POINT('Ctrl Pts',(110.17830992992,1.48423548411169,329.27026929832));
#13231=CARTESIAN_POINT('Ctrl Pts',(110.170900936535,1.33113295482855,329.232784255807));
#13232=CARTESIAN_POINT('Ctrl Pts',(110.16349194315,1.17691854155148,329.201483525155));
#13233=CARTESIAN_POINT('Ctrl Pts',(110.15607838557,1.02260912687707,329.170163512173));
#13234=CARTESIAN_POINT('Ctrl Pts',(110.14866482799,0.867186830903961,329.145035461909));
#13235=CARTESIAN_POINT('Ctrl Pts',(110.141251270409,0.711188655873953,329.126147664585));
#13236=CARTESIAN_POINT('Ctrl Pts',(110.133827158273,0.55496838888195,329.107232977025));
#13237=CARTESIAN_POINT('Ctrl Pts',(110.126403046136,0.398170976388124,329.094576315762));
#13238=CARTESIAN_POINT('Ctrl Pts',(110.118978933999,0.241335191826657,329.088173895683));
#13239=CARTESIAN_POINT('Ctrl Pts',(110.115121808845,0.159852687435522,329.084847580686));
#13240=CARTESIAN_POINT('Ctrl Pts',(110.11126468369,0.0783597821473199,329.083208565479));
#13241=CARTESIAN_POINT('Ctrl Pts',(110.107407558535,-0.00306853474573501,
329.083250795699));
#13242=CARTESIAN_POINT('Ctrl Pts',(110.099983581097,-0.159797176724483,
329.08333207805));
#13243=CARTESIAN_POINT('Ctrl Pts',(110.092559603659,-0.316759019714356,
329.089645155955));
#13244=CARTESIAN_POINT('Ctrl Pts',(110.085135626221,-0.473417769970754,
329.102220233208));
#13245=CARTESIAN_POINT('Ctrl Pts',(110.077720410194,-0.629891639330824,
329.114780469979));
#13246=CARTESIAN_POINT('Ctrl Pts',(110.070305194166,-0.7860627595581,329.133587966412));
#13247=CARTESIAN_POINT('Ctrl Pts',(110.062889978138,-0.941393363609252,
329.158620959272));
#13248=CARTESIAN_POINT('Ctrl Pts',(110.055481896994,-1.09657450933539,329.183629865513));
#13249=CARTESIAN_POINT('Ctrl Pts',(110.04807381585,-1.2509163829423,329.214852283941));
#13250=CARTESIAN_POINT('Ctrl Pts',(110.040665734706,-1.4038849808329,329.252214554884));
#13251=CARTESIAN_POINT('Ctrl Pts',(110.033263167532,-1.55673972140211,329.289549016405));
#13252=CARTESIAN_POINT('Ctrl Pts',(110.025860600358,-1.70822286051232,329.333014142722));
#13253=CARTESIAN_POINT('Ctrl Pts',(110.018458033184,-1.85780936062617,329.38248498515));
#13254=CARTESIAN_POINT('Ctrl Pts',(110.011059363429,-2.00731710410265,329.431929781395));
#13255=CARTESIAN_POINT('Ctrl Pts',(110.003660693675,-2.1549298438544,329.487373879585));
#13256=CARTESIAN_POINT('Ctrl Pts',(109.99626202392,-2.3001366216363,329.548642179759));
#13257=CARTESIAN_POINT('Ctrl Pts',(109.988864574716,-2.44531944480805,329.609900372565));
#13258=CARTESIAN_POINT('Ctrl Pts',(109.981467125512,-2.58809675022478,329.676980715509));
#13259=CARTESIAN_POINT('Ctrl Pts',(109.974069676308,-2.72797641791053,329.749659513344));
#13260=CARTESIAN_POINT('Ctrl Pts',(109.966672547844,-2.86785002065765,329.822335159952));
#13261=CARTESIAN_POINT('Ctrl Pts',(109.959275419381,-3.00482590430447,329.900608606733));
#13262=CARTESIAN_POINT('Ctrl Pts',(109.951878290918,-3.13843571937687,329.984209753405));
#13263=CARTESIAN_POINT('Ctrl Pts',(109.944480023481,-3.27206610702601,330.067823772567));
#13264=CARTESIAN_POINT('Ctrl Pts',(109.937081756044,-3.4023290777154,330.156766927036));
#13265=CARTESIAN_POINT('Ctrl Pts',(109.929683488608,-3.52878461884769,330.250725352616));
#13266=CARTESIAN_POINT('Ctrl Pts',(109.922282622082,-3.65528458514079,330.344716786779));
#13267=CARTESIAN_POINT('Ctrl Pts',(109.914881755556,-3.7779741593557,330.443726777582));
#13268=CARTESIAN_POINT('Ctrl Pts',(109.907480889031,-3.89644593282013,330.547400797836));
#13269=CARTESIAN_POINT('Ctrl Pts',(109.900071895646,-4.01504779961826,330.651188662076));
#13270=CARTESIAN_POINT('Ctrl Pts',(109.892662902261,-4.12942233519182,330.759650537854));
#13271=CARTESIAN_POINT('Ctrl Pts',(109.885253908876,-4.2391980552138,330.872394106607));
#13272=CARTESIAN_POINT('Ctrl Pts',(109.877840351296,-4.34904140086573,330.985207129287));
#13273=CARTESIAN_POINT('Ctrl Pts',(109.870426793716,-4.45428003689691,331.102306823915));
#13274=CARTESIAN_POINT('Ctrl Pts',(109.863013236136,-4.55458275230158,331.223267746459));
#13275=CARTESIAN_POINT('Ctrl Pts',(109.855589123999,-4.65502826698499,331.344400879022));
#13276=CARTESIAN_POINT('Ctrl Pts',(109.848165011862,-4.75052360039316,331.469405922665));
#13277=CARTESIAN_POINT('Ctrl Pts',(109.840740899726,-4.84078037428869,331.597827762972));
#13278=CARTESIAN_POINT('Ctrl Pts',(109.836883774571,-4.88767240212476,331.66454807936));
#13279=CARTESIAN_POINT('Ctrl Pts',(109.833026649416,-4.93315117209298,331.732190236817));
#13280=CARTESIAN_POINT('Ctrl Pts',(109.829169524262,-4.97718119442729,331.800687898885));
#13281=CARTESIAN_POINT('Ctrl Pts',(109.821573460546,-5.06389211036479,331.935584378665));
#13282=CARTESIAN_POINT('Ctrl Pts',(109.813977396831,-5.14523351640621,332.074192335918));
#13283=CARTESIAN_POINT('Ctrl Pts',(109.806381333115,-5.2208801338831,332.216056539704));
#13284=CARTESIAN_POINT('Ctrl Pts',(109.798795450889,-5.29642535736611,332.357730593835));
#13285=CARTESIAN_POINT('Ctrl Pts',(109.791209568663,-5.36629083199038,332.502651895537));
#13286=CARTESIAN_POINT('Ctrl Pts',(109.783623686437,-5.43019430910244,332.650336124487));
#13287=CARTESIAN_POINT('Ctrl Pts',(109.776046747252,-5.49402245002688,332.797846247624));
#13288=CARTESIAN_POINT('Ctrl Pts',(109.768469808068,-5.55190245623123,332.948112490534));
#13289=CARTESIAN_POINT('Ctrl Pts',(109.760892868883,-5.60359774706154,333.100625668377));
#13290=CARTESIAN_POINT('Ctrl Pts',(109.753322796868,-5.6552461851559,333.253000619711));
#13291=CARTESIAN_POINT('Ctrl Pts',(109.745752724853,-5.70072095848832,333.407618120489));
#13292=CARTESIAN_POINT('Ctrl Pts',(109.738182652838,-5.73983330636068,333.563948407023));
#13293=CARTESIAN_POINT('Ctrl Pts',(109.730621362071,-5.77890028409332,333.720097351159));
#13294=CARTESIAN_POINT('Ctrl Pts',(109.723060071304,-5.81161947080259,333.877954779919));
#13295=CARTESIAN_POINT('Ctrl Pts',(109.715498780537,-5.83785189284057,334.036975680599));
#13296=CARTESIAN_POINT('Ctrl Pts',(109.707924317898,-5.86413001211656,334.196273597863));
#13297=CARTESIAN_POINT('Ctrl Pts',(109.700349855259,-5.88389864039625,334.356738706662));
#13298=CARTESIAN_POINT('Ctrl Pts',(109.69277539262,-5.89706912905482,334.51781098141));
#13299=CARTESIAN_POINT('Ctrl Pts',(109.685200929981,-5.91023961771339,334.678883256159));
#13300=CARTESIAN_POINT('Ctrl Pts',(109.677626467342,-5.9168119122902,334.840562346074));
#13301=CARTESIAN_POINT('Ctrl Pts',(109.670052004703,-5.91674956022219,335.00228125196));
#13302=CARTESIAN_POINT('',(107.920052004703,-5.92221754830578,335.00433605404));
#13303=CARTESIAN_POINT('Ctrl Pts',(109.670050448713,-5.90779511345791,335.002310970458));
#13304=CARTESIAN_POINT('Ctrl Pts',(109.630344129138,-5.91071301687524,335.848780750068));
#13305=CARTESIAN_POINT('Ctrl Pts',(109.497891798137,-5.34435609359717,338.668701282137));
#13306=CARTESIAN_POINT('Ctrl Pts',(109.272693455716,-1.00488954949076,341.924075383365));
#13307=CARTESIAN_POINT('Ctrl Pts',(108.99445542144,5.27879931276318,339.592047553848));
#13308=CARTESIAN_POINT('Ctrl Pts',(108.716217387167,6.71821196064523,333.045965462669));
#13309=CARTESIAN_POINT('Ctrl Pts',(108.437979352892,1.99242065288906,328.293072024904));
#13310=CARTESIAN_POINT('Ctrl Pts',(108.172590892072,-4.2590996869207,329.630282370671));
#13311=CARTESIAN_POINT('Ctrl Pts',(107.999948442675,-5.90829782333765,333.311624078754));
#13312=CARTESIAN_POINT('Ctrl Pts',(107.920052004703,-5.92221754830578,335.00433605404));
#13313=CARTESIAN_POINT('',(106.170052004703,-5.92154411674314,334.995412275155));
#13314=CARTESIAN_POINT('Ctrl Pts',(107.920052004703,-5.92221754830578,335.00433605404));
#13315=CARTESIAN_POINT('Ctrl Pts',(107.90720243125,-5.92445622793863,335.276571305242));
#13316=CARTESIAN_POINT('Ctrl Pts',(107.801606846373,-5.78358165308998,337.511424151982));
#13317=CARTESIAN_POINT('Ctrl Pts',(107.60326525007,-2.93834024845692,341.349707040925));
#13318=CARTESIAN_POINT('Ctrl Pts',(107.325027215796,3.74949960540118,340.907103827622));
#13319=CARTESIAN_POINT('Ctrl Pts',(107.046789181522,6.996479013907,335.043638620423));
#13320=CARTESIAN_POINT('Ctrl Pts',(106.768551147248,3.82289289921021,329.14012689537));
#13321=CARTESIAN_POINT('Ctrl Pts',(106.490313112974,-2.85890560328287,328.614134226846));
#13322=CARTESIAN_POINT('Ctrl Pts',(106.290813398793,-5.76869590651112,332.438829820194));
#13323=CARTESIAN_POINT('Ctrl Pts',(106.184059696036,-5.92408171522026,334.698552889316));
#13324=CARTESIAN_POINT('Ctrl Pts',(106.170052004703,-5.92154411674314,334.995412275155));
#13325=CARTESIAN_POINT('',(104.42005273448,-5.91170307006019,334.998082814567));
#13326=CARTESIAN_POINT('Ctrl Pts',(106.170052004703,-5.92154411674314,334.995412275155));
#13327=CARTESIAN_POINT('Ctrl Pts',(106.091313684611,-5.90728007876455,336.664081921709));
#13328=CARTESIAN_POINT('Ctrl Pts',(105.919829353095,-4.29854415330596,340.322347225061));
#13329=CARTESIAN_POINT('Ctrl Pts',(105.655599010152,1.90860364104225,341.731259545033));
#13330=CARTESIAN_POINT('Ctrl Pts',(105.377360975878,6.69331470236746,337.037685259384));
#13331=CARTESIAN_POINT('Ctrl Pts',(105.099122941604,5.33566965449091,330.474157287383));
#13332=CARTESIAN_POINT('Ctrl Pts',(104.820884907332,-0.918440680953387,
328.06392837142));
#13333=CARTESIAN_POINT('Ctrl Pts',(104.594528372549,-5.32070196082337,331.281381489484));
#13334=CARTESIAN_POINT('Ctrl Pts',(104.46091784919,-5.91003360597982,334.126814980488));
#13335=CARTESIAN_POINT('Ctrl Pts',(104.420053337258,-5.90753467241241,334.998071303833));
#13336=CARTESIAN_POINT('',(102.670051327749,-5.91521396419827,335.005380775613));
#13337=CARTESIAN_POINT('Ctrl Pts',(104.420052004704,-5.91674969388947,334.99809675046));
#13338=CARTESIAN_POINT('Ctrl Pts',(104.412468296942,-5.91680178579455,335.160038081326));
#13339=CARTESIAN_POINT('Ctrl Pts',(104.404884589181,-5.9102010264601,335.321923755964));
#13340=CARTESIAN_POINT('Ctrl Pts',(104.397300881419,-5.8969874206776,335.483187254458));
#13341=CARTESIAN_POINT('Ctrl Pts',(104.389712803173,-5.8837661999047,335.644543688975));
#13342=CARTESIAN_POINT('Ctrl Pts',(104.382124724926,-5.86392456237403,335.805276887542));
#13343=CARTESIAN_POINT('Ctrl Pts',(104.37453664668,-5.83755426134891,335.964826828144));
#13344=CARTESIAN_POINT('Ctrl Pts',(104.366943043201,-5.81116475888245,336.124492944471));
#13345=CARTESIAN_POINT('Ctrl Pts',(104.359349439722,-5.77823717070347,336.282973743893));
#13346=CARTESIAN_POINT('Ctrl Pts',(104.351755836244,-5.73891412015043,336.439720557622));
#13347=CARTESIAN_POINT('Ctrl Pts',(104.344149881205,-5.69952710773525,336.596722331683));
#13348=CARTESIAN_POINT('Ctrl Pts',(104.336543926166,-5.6537239278541,336.751984147316));
#13349=CARTESIAN_POINT('Ctrl Pts',(104.328937971128,-5.60169717914256,336.904972250634));
#13350=CARTESIAN_POINT('Ctrl Pts',(104.321325502156,-5.54962587340528,337.05809137684));
#13351=CARTESIAN_POINT('Ctrl Pts',(104.313713033185,-5.49132049193872,337.208932584453));
#13352=CARTESIAN_POINT('Ctrl Pts',(104.306100564214,-5.42702137540082,337.356983146618));
#13353=CARTESIAN_POINT('Ctrl Pts',(104.298473877911,-5.36260217142819,337.50531021355));
#13354=CARTESIAN_POINT('Ctrl Pts',(104.290847191608,-5.29216700613838,337.650835904882));
#13355=CARTESIAN_POINT('Ctrl Pts',(104.283220505305,-5.21600242325113,337.793071657358));
#13356=CARTESIAN_POINT('Ctrl Pts',(104.276949949798,-5.15338096149142,337.91001591671));
#13357=CARTESIAN_POINT('Ctrl Pts',(104.27067939429,-5.0868873502845,338.02473664031));
#13358=CARTESIAN_POINT('Ctrl Pts',(104.264408838783,-5.01670206739496,338.136977993148));
#13359=CARTESIAN_POINT('Ctrl Pts',(104.256984861345,-4.93360672503615,338.269865305942));
#13360=CARTESIAN_POINT('Ctrl Pts',(104.249560883907,-4.84510230919647,338.39964913962));
#13361=CARTESIAN_POINT('Ctrl Pts',(104.242136906469,-4.75144730191213,338.525858632965));
#13362=CARTESIAN_POINT('Ctrl Pts',(104.234721690441,-4.65790282162755,338.651919180118));
#13363=CARTESIAN_POINT('Ctrl Pts',(104.227306474414,-4.55922006943336,338.774413486658));
#13364=CARTESIAN_POINT('Ctrl Pts',(104.219891258386,-4.45570238400033,338.892896971115));
#13365=CARTESIAN_POINT('Ctrl Pts',(104.212483177242,-4.35228430276294,339.01126645136));
#13366=CARTESIAN_POINT('Ctrl Pts',(104.205075096098,-4.2440407937584,339.125632513281));
#13367=CARTESIAN_POINT('Ctrl Pts',(104.197667014954,-4.13131721827334,339.235581259343));
#13368=CARTESIAN_POINT('Ctrl Pts',(104.19026444778,-4.01867754500458,339.345448168545));
#13369=CARTESIAN_POINT('Ctrl Pts',(104.182861880606,-3.90156471094392,339.450904049076));
#13370=CARTESIAN_POINT('Ctrl Pts',(104.175459313432,-3.78036282873408,339.551569778178));
#13371=CARTESIAN_POINT('Ctrl Pts',(104.168060643677,-3.65922475878535,339.652182507214));
#13372=CARTESIAN_POINT('Ctrl Pts',(104.160661973923,-3.53400221462441,339.748009869666));
#13373=CARTESIAN_POINT('Ctrl Pts',(104.153263304168,-3.40511438655748,339.838711251662));
#13374=CARTESIAN_POINT('Ctrl Pts',(104.145865854964,-3.27624782097983,339.929397670746));
#13375=CARTESIAN_POINT('Ctrl Pts',(104.13846840576,-3.143717476462,340.014959573095));
#13376=CARTESIAN_POINT('Ctrl Pts',(104.131070956556,-3.00797378020425,340.095098065799));
#13377=CARTESIAN_POINT('Ctrl Pts',(104.123673828092,-2.87223596955661,340.175233083837));
#13378=CARTESIAN_POINT('Ctrl Pts',(104.116276699629,-2.7332854055776,340.249944970051));
#13379=CARTESIAN_POINT('Ctrl Pts',(104.108879571166,-2.59159928185225,340.31897957552));
#13380=CARTESIAN_POINT('Ctrl Pts',(104.101481303729,-2.44989134200062,340.388024810596));
#13381=CARTESIAN_POINT('Ctrl Pts',(104.094083036292,-2.30544733924833,340.451390860879));
#13382=CARTESIAN_POINT('Ctrl Pts',(104.086684768856,-2.15876657446428,340.508870795315));
#13383=CARTESIAN_POINT('Ctrl Pts',(104.07928390233,-2.01203427918534,340.566370923057));
#13384=CARTESIAN_POINT('Ctrl Pts',(104.071883035804,-1.86306400461667,340.617980681774));
#13385=CARTESIAN_POINT('Ctrl Pts',(104.064482169279,-1.71237226839279,340.6635423347));
#13386=CARTESIAN_POINT('Ctrl Pts',(104.057073175894,-1.56151505823562,340.709154018677));
#13387=CARTESIAN_POINT('Ctrl Pts',(104.049664182509,-1.4089329687871,340.74870422556));
#13388=CARTESIAN_POINT('Ctrl Pts',(104.042255189124,-1.25515553988395,340.782085707874));
#13389=CARTESIAN_POINT('Ctrl Pts',(104.034841631544,-1.10128337878004,340.815487754333));
#13390=CARTESIAN_POINT('Ctrl Pts',(104.027428073964,-0.946214777636154,
340.84271343954));
#13391=CARTESIAN_POINT('Ctrl Pts',(104.020014516384,-0.790486037222097,
340.863707222181));
#13392=CARTESIAN_POINT('Ctrl Pts',(104.012590404247,-0.634535588436436,
340.884730893315));
#13393=CARTESIAN_POINT('Ctrl Pts',(104.00516629211,-0.477923493913411,340.899504907259));
#13394=CARTESIAN_POINT('Ctrl Pts',(103.997742179974,-0.321188529049471,
340.90802576935));
#13395=CARTESIAN_POINT('Ctrl Pts',(103.993885054819,-0.239758404548028,
340.912452700263));
#13396=CARTESIAN_POINT('Ctrl Pts',(103.990027929664,-0.158295082796337,
340.915192625928));
#13397=CARTESIAN_POINT('Ctrl Pts',(103.986170804509,-0.0768736280428343,
340.916250586969));
#13398=CARTESIAN_POINT('Ctrl Pts',(103.978746827071,0.0798418060718854,
340.918286890843));
#13399=CARTESIAN_POINT('Ctrl Pts',(103.971322849633,0.236874618421677,340.914095118803));
#13400=CARTESIAN_POINT('Ctrl Pts',(103.963898872195,0.393688972301404,340.903637823884));
#13401=CARTESIAN_POINT('Ctrl Pts',(103.956483656168,0.550318261649561,340.893192870146));
#13402=CARTESIAN_POINT('Ctrl Pts',(103.94906844014,0.706729236947371,340.876497136512));
#13403=CARTESIAN_POINT('Ctrl Pts',(103.941653224113,0.862383886192894,340.853565118399));
#13404=CARTESIAN_POINT('Ctrl Pts',(103.934245142968,1.01788876531853,340.830655165358));
#13405=CARTESIAN_POINT('Ctrl Pts',(103.926837061824,1.1726384004148,340.801520927792));
#13406=CARTESIAN_POINT('Ctrl Pts',(103.91942898068,1.32609784140368,340.766228843666));
#13407=CARTESIAN_POINT('Ctrl Pts',(103.912026413506,1.47944305972823,340.730963028083));
#13408=CARTESIAN_POINT('Ctrl Pts',(103.904623846332,1.63149963391357,340.689548575441));
#13409=CARTESIAN_POINT('Ctrl Pts',(103.897221279158,1.78174088615125,340.642103329178));
#13410=CARTESIAN_POINT('Ctrl Pts',(103.889822609404,1.93190303702625,340.594683062629));
#13411=CARTESIAN_POINT('Ctrl Pts',(103.882423939649,2.08025141441344,340.541238438134));
#13412=CARTESIAN_POINT('Ctrl Pts',(103.875025269894,2.22627274091179,340.481937636053));
#13413=CARTESIAN_POINT('Ctrl Pts',(103.86762782069,2.37226997842538,340.422646616763));
#13414=CARTESIAN_POINT('Ctrl Pts',(103.860230371486,2.51594058150165,340.357501477549));
#13415=CARTESIAN_POINT('Ctrl Pts',(103.852832922282,2.65678945271268,340.286719244149));
#13416=CARTESIAN_POINT('Ctrl Pts',(103.845435793819,2.797632216962,340.215940079743));
#13417=CARTESIAN_POINT('Ctrl Pts',(103.838038665355,2.93565315913819,340.139524474711));
#13418=CARTESIAN_POINT('Ctrl Pts',(103.830641536892,3.07038032316165,340.057736176754));
#13419=CARTESIAN_POINT('Ctrl Pts',(103.823243269455,3.20512823180502,339.97593528544));
#13420=CARTESIAN_POINT('Ctrl Pts',(103.815845002019,3.33658103342749,339.8887602477));
#13421=CARTESIAN_POINT('Ctrl Pts',(103.808446734582,3.4642945149403,339.796518954018));
#13422=CARTESIAN_POINT('Ctrl Pts',(103.801045868056,3.59205286354241,339.704245254999));
#13423=CARTESIAN_POINT('Ctrl Pts',(103.79364500153,3.71606897417532,339.606901974782));
#13424=CARTESIAN_POINT('Ctrl Pts',(103.786244135005,3.83593068529685,339.50483810365));
#13425=CARTESIAN_POINT('Ctrl Pts',(103.77883514162,3.95592401603667,339.402662156629));
#13426=CARTESIAN_POINT('Ctrl Pts',(103.771426148235,4.07175355253006,339.295755508751));
#13427=CARTESIAN_POINT('Ctrl Pts',(103.76401715485,4.18304254369739,339.184505423598));
#13428=CARTESIAN_POINT('Ctrl Pts',(103.75660359727,4.29440009272229,339.073186804555));
#13429=CARTESIAN_POINT('Ctrl Pts',(103.74919003969,4.40121127016137,338.957519690084));
#13430=CARTESIAN_POINT('Ctrl Pts',(103.74177648211,4.50313914701812,338.837925010353));
#13431=CARTESIAN_POINT('Ctrl Pts',(103.734352369973,4.60521213686767,338.718160065701));
#13432=CARTESIAN_POINT('Ctrl Pts',(103.726928257836,4.70238771112937,338.594456680921));
#13433=CARTESIAN_POINT('Ctrl Pts',(103.7195041457,4.79437136878528,338.467266032578));
#13434=CARTESIAN_POINT('Ctrl Pts',(103.715647020545,4.84216058226133,338.401185369983));
#13435=CARTESIAN_POINT('Ctrl Pts',(103.71178989539,4.88854912197195,338.334163855773));
#13436=CARTESIAN_POINT('Ctrl Pts',(103.707932770235,4.93350060511098,338.266267340845));
#13437=CARTESIAN_POINT('Ctrl Pts',(103.700508792797,5.02002069021073,338.13558394979));
#13438=CARTESIAN_POINT('Ctrl Pts',(103.693084815359,5.10147520497793,338.001263299362));
#13439=CARTESIAN_POINT('Ctrl Pts',(103.685660837921,5.17754268747386,337.863735721376));
#13440=CARTESIAN_POINT('Ctrl Pts',(103.678245621894,5.2535203988957,337.726370446625));
#13441=CARTESIAN_POINT('Ctrl Pts',(103.670830405866,5.32412355388886,337.585806101144));
#13442=CARTESIAN_POINT('Ctrl Pts',(103.663415189838,5.38907319279343,337.442502955006));
#13443=CARTESIAN_POINT('Ctrl Pts',(103.656007108694,5.45396033748232,337.299337694435));
#13444=CARTESIAN_POINT('Ctrl Pts',(103.64859902755,5.51320464264368,337.153439217174));
#13445=CARTESIAN_POINT('Ctrl Pts',(103.641190946406,5.56657248519886,337.005293327553));
#13446=CARTESIAN_POINT('Ctrl Pts',(103.633788379232,5.61990060509416,336.857257705622));
#13447=CARTESIAN_POINT('Ctrl Pts',(103.626385812058,5.6673608456253,336.70697835172));
#13448=CARTESIAN_POINT('Ctrl Pts',(103.618983244884,5.70876728826917,336.554961932295));
#13449=CARTESIAN_POINT('Ctrl Pts',(103.611584575129,5.75015193060182,336.403025548852));
#13450=CARTESIAN_POINT('Ctrl Pts',(103.604185905375,5.78548902490515,336.249354280467));
#13451=CARTESIAN_POINT('Ctrl Pts',(103.59678723562,5.81464223377832,336.094470765101));
#13452=CARTESIAN_POINT('Ctrl Pts',(103.589389786416,5.84379063327737,335.939612800706));
#13453=CARTESIAN_POINT('Ctrl Pts',(103.581992337212,5.86675710304366,335.783543352644));
#13454=CARTESIAN_POINT('Ctrl Pts',(103.574594888008,5.88345621902356,335.626796203987));
#13455=CARTESIAN_POINT('Ctrl Pts',(103.567197759544,5.90015461095892,335.470055851613));
#13456=CARTESIAN_POINT('Ctrl Pts',(103.559800631081,5.91058614988309,335.312638228179));
#13457=CARTESIAN_POINT('Ctrl Pts',(103.552403502617,5.91471722435007,335.155082940637));
#13458=CARTESIAN_POINT('Ctrl Pts',(103.545005235181,5.91884893489939,334.997503393514));
#13459=CARTESIAN_POINT('Ctrl Pts',(103.537606967744,5.91667823958361,334.839786513182));
#13460=CARTESIAN_POINT('Ctrl Pts',(103.530208700308,5.90822366088908,334.682472465114));
#13461=CARTESIAN_POINT('Ctrl Pts',(103.522807833782,5.89976611201213,334.525103150967));
#13462=CARTESIAN_POINT('Ctrl Pts',(103.515406967256,5.885020304456,334.368137323286));
#13463=CARTESIAN_POINT('Ctrl Pts',(103.50800610073,5.86405666733463,334.212110436172));
#13464=CARTESIAN_POINT('Ctrl Pts',(103.500597107345,5.84307001013544,334.05591221662));
#13465=CARTESIAN_POINT('Ctrl Pts',(103.493188113961,5.81585193767445,333.900655366798));
#13466=CARTESIAN_POINT('Ctrl Pts',(103.485779120576,5.78252422653407,333.746866275274));
#13467=CARTESIAN_POINT('Ctrl Pts',(103.478365562996,5.74917598437415,333.592982444365));
#13468=CARTESIAN_POINT('Ctrl Pts',(103.470952005415,5.70971069710263,333.440568533923));
#13469=CARTESIAN_POINT('Ctrl Pts',(103.463538447835,5.66430000226331,333.290135664194));
#13470=CARTESIAN_POINT('Ctrl Pts',(103.456114335698,5.61882465698615,333.139488625735));
#13471=CARTESIAN_POINT('Ctrl Pts',(103.448690223562,5.56738712079512,332.990828612585));
#13472=CARTESIAN_POINT('Ctrl Pts',(103.441266111425,5.5102074262881,332.84464743446));
#13473=CARTESIAN_POINT('Ctrl Pts',(103.43740898627,5.48050027290022,332.768700427075));
#13474=CARTESIAN_POINT('Ctrl Pts',(103.433551861116,5.44924395237199,332.693422127347));
#13475=CARTESIAN_POINT('Ctrl Pts',(103.429694735961,5.41647415130372,332.618878766052));
#13476=CARTESIAN_POINT('Ctrl Pts',(103.422270758523,5.35340068232637,332.475401899155));
#13477=CARTESIAN_POINT('Ctrl Pts',(103.414846781085,5.2845272935753,332.334216448667));
#13478=CARTESIAN_POINT('Ctrl Pts',(103.407422803647,5.21004189875463,332.195825616029));
#13479=CARTESIAN_POINT('Ctrl Pts',(103.40000758762,5.13564440790693,332.057598105395));
#13480=CARTESIAN_POINT('Ctrl Pts',(103.392592371592,5.05564826935856,331.922158973189));
#13481=CARTESIAN_POINT('Ctrl Pts',(103.385177155564,4.97028957295405,331.789991881087));
#13482=CARTESIAN_POINT('Ctrl Pts',(103.37776907442,4.88501300825737,331.657951959496));
#13483=CARTESIAN_POINT('Ctrl Pts',(103.370360993276,4.79438435908125,331.529178121665));
#13484=CARTESIAN_POINT('Ctrl Pts',(103.362952912132,4.6986857217974,331.404129722824));
#13485=CARTESIAN_POINT('Ctrl Pts',(103.355550344958,4.60305831475735,331.27917439979));
#13486=CARTESIAN_POINT('Ctrl Pts',(103.348147777784,4.50236865941098,331.157939289584));
#13487=CARTESIAN_POINT('Ctrl Pts',(103.34074521061,4.39694221120499,331.040854921347));
#13488=CARTESIAN_POINT('Ctrl Pts',(103.333346540855,4.29157126956261,330.923832197517));
#13489=CARTESIAN_POINT('Ctrl Pts',(103.3259478711,4.18146875091419,330.810956140054));
#13490=CARTESIAN_POINT('Ctrl Pts',(103.318549201346,4.0670003726795,330.702624227377));
#13491=CARTESIAN_POINT('Ctrl Pts',(103.311151752142,3.95255087817319,330.594310186102));
#13492=CARTESIAN_POINT('Ctrl Pts',(103.303754302938,3.83373722430933,330.490539058099));
#13493=CARTESIAN_POINT('Ctrl Pts',(103.296356853734,3.71096205280173,330.391671538924));
#13494=CARTESIAN_POINT('Ctrl Pts',(103.28895972527,3.58819220461152,330.292808306472));
#13495=CARTESIAN_POINT('Ctrl Pts',(103.281562596807,3.46146147098186,330.198848494182));
#13496=CARTESIAN_POINT('Ctrl Pts',(103.274165468343,3.33120542982831,330.110112378921));
#13497=CARTESIAN_POINT('Ctrl Pts',(103.266767200907,3.20092933249567,330.021362600513));
#13498=CARTESIAN_POINT('Ctrl Pts',(103.25936893347,3.06712715529281,329.937838330774));
#13499=CARTESIAN_POINT('Ctrl Pts',(103.251970666033,2.93026315846882,329.85981630828));
#13500=CARTESIAN_POINT('Ctrl Pts',(103.244569799508,2.79335107988414,329.781766875831));
#13501=CARTESIAN_POINT('Ctrl Pts',(103.237168932982,2.65337536408568,329.709223723937));
#13502=CARTESIAN_POINT('Ctrl Pts',(103.229768066456,2.51082439908517,329.642417392195));
#13503=CARTESIAN_POINT('Ctrl Pts',(103.222359073071,2.36811689949608,329.575537700712));
#13504=CARTESIAN_POINT('Ctrl Pts',(103.214950079687,2.22282884144005,329.514407568442));
#13505=CARTESIAN_POINT('Ctrl Pts',(103.207541086302,2.0754687765893,329.459209449916));
#13506=CARTESIAN_POINT('Ctrl Pts',(103.200127528722,1.92801793285562,329.403977327444));
#13507=CARTESIAN_POINT('Ctrl Pts',(103.192713971141,1.77849289249599,329.354684617017));
#13508=CARTESIAN_POINT('Ctrl Pts',(103.185300413561,1.62741635035397,329.311463581456));
#13509=CARTESIAN_POINT('Ctrl Pts',(103.177876301424,1.47612472309606,329.268181012838));
#13510=CARTESIAN_POINT('Ctrl Pts',(103.170452189288,1.32327754419817,329.230987471168));
#13511=CARTESIAN_POINT('Ctrl Pts',(103.163028077151,1.16940745920663,329.199964072796));
#13512=CARTESIAN_POINT('Ctrl Pts',(103.159170951996,1.08946575514504,329.183846168321));
#13513=CARTESIAN_POINT('Ctrl Pts',(103.155313826842,1.0092480383871,329.169392867626));
#13514=CARTESIAN_POINT('Ctrl Pts',(103.151456701687,0.928829315873215,329.156610002364));
#13515=CARTESIAN_POINT('Ctrl Pts',(103.144032724249,0.774043884336897,329.132006262661));
#13516=CARTESIAN_POINT('Ctrl Pts',(103.136608746811,0.61804668435539,329.113519816133));
#13517=CARTESIAN_POINT('Ctrl Pts',(103.129184769373,0.46136255964295,329.101264953309));
#13518=CARTESIAN_POINT('Ctrl Pts',(103.121769553346,0.304863345772179,329.089024553067));
#13519=CARTESIAN_POINT('Ctrl Pts',(103.114354337318,0.147679189287689,329.083001126683));
#13520=CARTESIAN_POINT('Ctrl Pts',(103.106939121291,-0.00965542662716032,
329.083257878255));
#13521=CARTESIAN_POINT('Ctrl Pts',(103.099531040146,-0.166838655966651,
329.083514382781));
#13522=CARTESIAN_POINT('Ctrl Pts',(103.092122959002,-0.32417168580736,329.090039034659));
#13523=CARTESIAN_POINT('Ctrl Pts',(103.084714877858,-0.481115576003788,
329.102843196503));
#13524=CARTESIAN_POINT('Ctrl Pts',(103.077312310684,-0.637942649997047,
329.115637827976));
#13525=CARTESIAN_POINT('Ctrl Pts',(103.06990974351,-0.794380790686796,329.134702632675));
#13526=CARTESIAN_POINT('Ctrl Pts',(103.062507176336,-0.94989183431622,329.159996912193));
#13527=CARTESIAN_POINT('Ctrl Pts',(103.055108506582,-1.1053210020595,329.185277874383));
#13528=CARTESIAN_POINT('Ctrl Pts',(103.047709836827,-1.25982367740501,329.216781719728));
#13529=CARTESIAN_POINT('Ctrl Pts',(103.040311167072,-1.41286770159056,329.254416007027));
#13530=CARTESIAN_POINT('Ctrl Pts',(103.032913717868,-1.56588647826504,329.292044085838));
#13531=CARTESIAN_POINT('Ctrl Pts',(103.025516268664,-1.71744671929437,329.335800510401));
#13532=CARTESIAN_POINT('Ctrl Pts',(103.01811881946,-1.86702721555507,329.385541883772));
#13533=CARTESIAN_POINT('Ctrl Pts',(103.010721690997,-2.01660122626601,329.435281100444));
#13534=CARTESIAN_POINT('Ctrl Pts',(103.003324562533,-2.1641953087395,329.491004632191));
#13535=CARTESIAN_POINT('Ctrl Pts',(102.99592743407,-2.30930441912245,329.552519512442));
#13536=CARTESIAN_POINT('Ctrl Pts',(102.988529166633,-2.45443587268598,329.614043864449));
#13537=CARTESIAN_POINT('Ctrl Pts',(102.981130899197,-2.59708124867286,329.681361194825));
#13538=CARTESIAN_POINT('Ctrl Pts',(102.97373263176,-2.73675659384932,329.754230856345));
#13539=CARTESIAN_POINT('Ctrl Pts',(102.966331765235,-2.87648100844369,329.827126117744));
#13540=CARTESIAN_POINT('Ctrl Pts',(102.958930898709,-3.01323298413462,329.905577421394));
#13541=CARTESIAN_POINT('Ctrl Pts',(102.951530032183,-3.14655436048236,329.989298829602));
#13542=CARTESIAN_POINT('Ctrl Pts',(102.944121038798,-3.28002213644734,330.07311217192));
#13543=CARTESIAN_POINT('Ctrl Pts',(102.936712045414,-3.41005147366832,330.162206977305));
#13544=CARTESIAN_POINT('Ctrl Pts',(102.929303052029,-3.53621373574666,330.256254330424));
#13545=CARTESIAN_POINT('Ctrl Pts',(102.921889494449,-3.66245371813079,330.350359619958));
#13546=CARTESIAN_POINT('Ctrl Pts',(102.914475936868,-3.78482158902665,330.449423302345));
#13547=CARTESIAN_POINT('Ctrl Pts',(102.907062379288,-3.9029232656339,330.553077407344));
#13548=CARTESIAN_POINT('Ctrl Pts',(102.899638267151,-4.02119308159887,330.656879082938));
#13549=CARTESIAN_POINT('Ctrl Pts',(102.892214155015,-4.13518430314986,330.765283976961));
#13550=CARTESIAN_POINT('Ctrl Pts',(102.884790042878,-4.24454047274818,330.877888073123));
#13551=CARTESIAN_POINT('Ctrl Pts',(102.880932917723,-4.30135540560929,330.936390434598));
#13552=CARTESIAN_POINT('Ctrl Pts',(102.877075792568,-4.35691990394507,330.996025713659));
#13553=CARTESIAN_POINT('Ctrl Pts',(102.873218667413,-4.41118847323711,331.05673399121));
#13554=CARTESIAN_POINT('Ctrl Pts',(102.865865035668,-4.51465181909997,331.172474678664));
#13555=CARTESIAN_POINT('Ctrl Pts',(102.858511403922,-4.61372889142071,331.292482793505));
#13556=CARTESIAN_POINT('Ctrl Pts',(102.851157772177,-4.70804192368787,331.416388440791));
#13557=CARTESIAN_POINT('Ctrl Pts',(102.843611698532,-4.80482309410307,331.543536654321));
#13558=CARTESIAN_POINT('Ctrl Pts',(102.836065624887,-4.89658713161454,331.674788962405));
#13559=CARTESIAN_POINT('Ctrl Pts',(102.828519551243,-4.98296549190882,331.80970448564));
#13560=CARTESIAN_POINT('Ctrl Pts',(102.821183857563,-5.06693567581008,331.940858645763));
#13561=CARTESIAN_POINT('Ctrl Pts',(102.813848163883,-5.14581622420385,332.075474155608));
#13562=CARTESIAN_POINT('Ctrl Pts',(102.806512470203,-5.2193091077421,332.213112309342));
#13563=CARTESIAN_POINT('Ctrl Pts',(102.799181707702,-5.29275258811072,332.350657940362));
#13564=CARTESIAN_POINT('Ctrl Pts',(102.791850945201,-5.3608154310141,332.491221837879));
#13565=CARTESIAN_POINT('Ctrl Pts',(102.784520182699,-5.42324365377972,332.634337548542));
#13566=CARTESIAN_POINT('Ctrl Pts',(102.777192833119,-5.48564281236084,332.777386630024));
#13567=CARTESIAN_POINT('Ctrl Pts',(102.76986548354,-5.54241241982301,332.922984811724));
#13568=CARTESIAN_POINT('Ctrl Pts',(102.76253813396,-5.59334519502373,333.070642570231));
#13569=CARTESIAN_POINT('Ctrl Pts',(102.754830956522,-5.64691817275784,333.225954464735));
#13570=CARTESIAN_POINT('Ctrl Pts',(102.747123779084,-5.69403286319964,333.383544751446));
#13571=CARTESIAN_POINT('Ctrl Pts',(102.739416601646,-5.73450626313315,333.542821740285));
#13572=CARTESIAN_POINT('Ctrl Pts',(102.73208993929,-5.77298142970359,333.694234981734));
#13573=CARTESIAN_POINT('Ctrl Pts',(102.724763276934,-5.80545524539736,333.84717197329));
#13574=CARTESIAN_POINT('Ctrl Pts',(102.717436614578,-5.83182233017694,334.001111181487));
#13575=CARTESIAN_POINT('Ctrl Pts',(102.710109070923,-5.85819258656002,334.155068906489));
#13576=CARTESIAN_POINT('Ctrl Pts',(102.702781527269,-5.87845459279923,334.310028711433));
#13577=CARTESIAN_POINT('Ctrl Pts',(102.695453983615,-5.89255456859799,334.46546167715));
#13578=CARTESIAN_POINT('Ctrl Pts',(102.688122269657,-5.90666256907455,334.620983103975));
#13579=CARTESIAN_POINT('Ctrl Pts',(102.680790555699,-5.91460151443724,334.77697784916));
#13580=CARTESIAN_POINT('Ctrl Pts',(102.673458841741,-5.91636967316463,334.932914584612));
#13581=CARTESIAN_POINT('Ctrl Pts',(102.672323229395,-5.91664354403461,334.957067693005));
#13582=CARTESIAN_POINT('Ctrl Pts',(102.67118761705,-5.91676947294849,334.981219413314));
#13583=CARTESIAN_POINT('Ctrl Pts',(102.670052004704,-5.91674756512981,335.005367777056));
#13584=CARTESIAN_POINT('',(100.920052004704,-5.92200910417624,334.999274282758));
#13585=CARTESIAN_POINT('Ctrl Pts',(102.67005103823,-5.91455807452654,335.005386334829));
#13586=CARTESIAN_POINT('Ctrl Pts',(102.645027569866,-5.91924007014113,335.537308585578));
#13587=CARTESIAN_POINT('Ctrl Pts',(102.52725809008,-5.60948765469108,338.03536527471));
#13588=CARTESIAN_POINT('Ctrl Pts',(102.316742598864,-2.08285686558825,341.679395945644));
#13589=CARTESIAN_POINT('Ctrl Pts',(102.038504564592,4.48969318508649,340.366123183922));
#13590=CARTESIAN_POINT('Ctrl Pts',(101.760266530317,6.94211806756556,334.128438380165));
#13591=CARTESIAN_POINT('Ctrl Pts',(101.482028496044,3.02386366494078,328.690572810701));
#13592=CARTESIAN_POINT('Ctrl Pts',(101.203790461769,-3.66934579084986,329.042775445864));
#13593=CARTESIAN_POINT('Ctrl Pts',(101.016464964656,-5.90853212608389,332.960493776982));
#13594=CARTESIAN_POINT('Ctrl Pts',(100.921885478968,-5.92645748560412,334.960501290448));
#13595=CARTESIAN_POINT('Ctrl Pts',(100.920052004704,-5.92639050991422,334.999273745835));
#13596=CARTESIAN_POINT('',(99.1700520270116,-5.9141281310151,334.995021507455));
#13597=CARTESIAN_POINT('Ctrl Pts',(100.920052004704,-5.9167499555727,334.999274927244));
#13598=CARTESIAN_POINT('Ctrl Pts',(100.912653210428,-5.91676909816112,335.155482574443));
#13599=CARTESIAN_POINT('Ctrl Pts',(100.905254416151,-5.91059793288327,335.311933625634));
#13600=CARTESIAN_POINT('Ctrl Pts',(100.897855621875,-5.89820461626513,335.468094933928));
#13601=CARTESIAN_POINT('Ctrl Pts',(100.890465537159,-5.88582588855612,335.62407241547));
#13602=CARTESIAN_POINT('Ctrl Pts',(100.883075452442,-5.86723961667127,335.779760461813));
#13603=CARTESIAN_POINT('Ctrl Pts',(100.875685367726,-5.8424659210364,335.934624268906));
#13604=CARTESIAN_POINT('Ctrl Pts',(100.868302342465,-5.8177158907311,336.089340140743));
#13605=CARTESIAN_POINT('Ctrl Pts',(100.860919317204,-5.78679026122925,336.243232971833));
#13606=CARTESIAN_POINT('Ctrl Pts',(100.853536291943,-5.74976106211383,336.395771575545));
#13607=CARTESIAN_POINT('Ctrl Pts',(100.84615868182,-5.71275902235735,336.548198298612));
#13608=CARTESIAN_POINT('Ctrl Pts',(100.838781071697,-5.66966241415348,336.699272407962));
#13609=CARTESIAN_POINT('Ctrl Pts',(100.831403461574,-5.62059457665737,336.848471576019));
#13610=CARTESIAN_POINT('Ctrl Pts',(100.823733083726,-5.56957956671361,337.003591455566));
#13611=CARTESIAN_POINT('Ctrl Pts',(100.816062705878,-5.51210974251225,337.156684117268));
#13612=CARTESIAN_POINT('Ctrl Pts',(100.80839232803,-5.44838152063113,337.30717779292));
#13613=CARTESIAN_POINT('Ctrl Pts',(100.801019583112,-5.3871261387845,337.451831877021));
#13614=CARTESIAN_POINT('Ctrl Pts',(100.793646838194,-5.32008909750129,337.594084513008));
#13615=CARTESIAN_POINT('Ctrl Pts',(100.786274093277,-5.24749442809488,337.733447052645));
#13616=CARTESIAN_POINT('Ctrl Pts',(100.778901455742,-5.17490081601893,337.872807562487));
#13617=CARTESIAN_POINT('Ctrl Pts',(100.771528818207,-5.09674991022246,338.009277726004));
#13618=CARTESIAN_POINT('Ctrl Pts',(100.764156180672,-5.01331204470294,338.142392862921));
#13619=CARTESIAN_POINT('Ctrl Pts',(100.756782169677,-4.92985863541142,338.275532798067));
#13620=CARTESIAN_POINT('Ctrl Pts',(100.749408158682,-4.84111650543503,338.405316143782));
#13621=CARTESIAN_POINT('Ctrl Pts',(100.742034147687,-4.74739960743119,338.531306773683));
#13622=CARTESIAN_POINT('Ctrl Pts',(100.734657281808,-4.65364642647555,338.657346181469));
#13623=CARTESIAN_POINT('Ctrl Pts',(100.727280415929,-4.5549148676611,338.779589648939));
#13624=CARTESIAN_POINT('Ctrl Pts',(100.719903550049,-4.4515593534164,338.897633882949));
#13625=CARTESIAN_POINT('Ctrl Pts',(100.712518519967,-4.34808945246633,339.015808760119));
#13626=CARTESIAN_POINT('Ctrl Pts',(100.705133489885,-4.23998562652681,339.129774842121));
#13627=CARTESIAN_POINT('Ctrl Pts',(100.697748459803,-4.12763980697507,339.239165034105));
#13628=CARTESIAN_POINT('Ctrl Pts',(100.690358595546,-4.01522044684805,339.348626831935));
#13629=CARTESIAN_POINT('Ctrl Pts',(100.682968731289,-3.89855384004281,339.453506522037));
#13630=CARTESIAN_POINT('Ctrl Pts',(100.675578867032,-3.77806473386628,339.553477509466));
#13631=CARTESIAN_POINT('Ctrl Pts',(100.668178963507,-3.65741194100149,339.653584309339));
#13632=CARTESIAN_POINT('Ctrl Pts',(100.660779059982,-3.53292657951394,339.748768866886));
#13633=CARTESIAN_POINT('Ctrl Pts',(100.653379156457,-3.40506255255605,339.838747728047));
#13634=CARTESIAN_POINT('Ctrl Pts',(100.651357568712,-3.3701312390514,339.863329151633));
#13635=CARTESIAN_POINT('Ctrl Pts',(100.649335980967,-3.33494790616683,339.887522321181));
#13636=CARTESIAN_POINT('Ctrl Pts',(100.647314393222,-3.2995221135164,339.911322060802));
#13637=CARTESIAN_POINT('Ctrl Pts',(100.639890415784,-3.16942620944326,339.998723030857));
#13638=CARTESIAN_POINT('Ctrl Pts',(100.632466438346,-3.03565890746535,340.081083118453));
#13639=CARTESIAN_POINT('Ctrl Pts',(100.625042460908,-2.89864835787401,340.158077961789));
#13640=CARTESIAN_POINT('Ctrl Pts',(100.61762724488,-2.76179950134534,340.234981939626));
#13641=CARTESIAN_POINT('Ctrl Pts',(100.610212028852,-2.62171533813551,340.306533095682));
#13642=CARTESIAN_POINT('Ctrl Pts',(100.602796812825,-2.47885424324229,340.372449367212));
#13643=CARTESIAN_POINT('Ctrl Pts',(100.595388731681,-2.33613060857546,340.438302214438));
#13644=CARTESIAN_POINT('Ctrl Pts',(100.587980650537,-2.1906356981925,340.49853081573));
#13645=CARTESIAN_POINT('Ctrl Pts',(100.580572569393,-2.04285372704659,340.552898271389));
#13646=CARTESIAN_POINT('Ctrl Pts',(100.573170002219,-1.89518175272074,340.607225260357));
#13647=CARTESIAN_POINT('Ctrl Pts',(100.565767435045,-1.74522645592163,340.655699661874));
#13648=CARTESIAN_POINT('Ctrl Pts',(100.558364867871,-1.59349323552573,340.698132138766));
#13649=CARTESIAN_POINT('Ctrl Pts',(100.550966198116,-1.44183990200765,340.740542275144));
#13650=CARTESIAN_POINT('Ctrl Pts',(100.543567528361,-1.28841086764603,340.776916721881));
#13651=CARTESIAN_POINT('Ctrl Pts',(100.536168858607,-1.13372783741781,340.807115613897));
#13652=CARTESIAN_POINT('Ctrl Pts',(100.528771409403,-0.979070325085853,
340.837309524033));
#13653=CARTESIAN_POINT('Ctrl Pts',(100.521373960199,-0.823159593397856,
340.861329829943));
#13654=CARTESIAN_POINT('Ctrl Pts',(100.513976510995,-0.666528836142006,
340.879087503439));
#13655=CARTESIAN_POINT('Ctrl Pts',(100.506579382531,-0.509904870122723,
340.896844406993));
#13656=CARTESIAN_POINT('Ctrl Pts',(100.499182254068,-0.352561311445007,
340.908339175994));
#13657=CARTESIAN_POINT('Ctrl Pts',(100.491785125605,-0.195037527677288,
340.913534554334));
#13658=CARTESIAN_POINT('Ctrl Pts',(100.484386858168,-0.0374894891794162,
340.918730732632));
#13659=CARTESIAN_POINT('Ctrl Pts',(100.476988590731,0.120238456631527,340.917625576671));
#13660=CARTESIAN_POINT('Ctrl Pts',(100.469590323295,0.277606031478055,340.910233959311));
#13661=CARTESIAN_POINT('Ctrl Pts',(100.462189456769,0.435028891208541,340.902839745197));
#13662=CARTESIAN_POINT('Ctrl Pts',(100.454788590243,0.592090755344619,340.889154690065));
#13663=CARTESIAN_POINT('Ctrl Pts',(100.447387723718,0.748255706205567,340.869245604047));
#13664=CARTESIAN_POINT('Ctrl Pts',(100.439978730333,0.904592141112852,340.84931465595));
#13665=CARTESIAN_POINT('Ctrl Pts',(100.432569736948,1.06002932541838,340.823146075169));
#13666=CARTESIAN_POINT('Ctrl Pts',(100.425160743564,1.21404005987996,340.790858079379));
#13667=CARTESIAN_POINT('Ctrl Pts',(100.417747185983,1.36814567026627,340.75855019307));
#13668=CARTESIAN_POINT('Ctrl Pts',(100.410333628403,1.52082271872443,340.720115470881));
#13669=CARTESIAN_POINT('Ctrl Pts',(100.402920070823,1.67155893713738,340.675722093459));
#13670=CARTESIAN_POINT('Ctrl Pts',(100.395495958686,1.8225097561533,340.631265513937));
#13671=CARTESIAN_POINT('Ctrl Pts',(100.38807184655,1.97151387404858,340.580833455787));
#13672=CARTESIAN_POINT('Ctrl Pts',(100.380647734413,2.11807800585394,340.524642624063));
#13673=CARTESIAN_POINT('Ctrl Pts',(100.376790609258,2.19422397309841,340.495449224702));
#13674=CARTESIAN_POINT('Ctrl Pts',(100.372933484103,2.26971171367343,340.464702175955));
#13675=CARTESIAN_POINT('Ctrl Pts',(100.369076358949,2.34447475722508,340.432436716174));
#13676=CARTESIAN_POINT('Ctrl Pts',(100.361652381511,2.4883744561581,340.370333974928));
#13677=CARTESIAN_POINT('Ctrl Pts',(100.354228404073,2.63002197355981,340.302415966113));
#13678=CARTESIAN_POINT('Ctrl Pts',(100.346804426635,2.76891284998212,340.228867199662));
#13679=CARTESIAN_POINT('Ctrl Pts',(100.339389210607,2.9076398142731,340.155405231822));
#13680=CARTESIAN_POINT('Ctrl Pts',(100.331973994579,3.04361628661856,340.07632590656));
#13681=CARTESIAN_POINT('Ctrl Pts',(100.324558778552,3.17635702142493,339.991862040857));
#13682=CARTESIAN_POINT('Ctrl Pts',(100.317150697408,3.30897003376444,339.907479445859));
#13683=CARTESIAN_POINT('Ctrl Pts',(100.309742616264,3.43835319401689,339.817722823796));
#13684=CARTESIAN_POINT('Ctrl Pts',(100.302334535119,3.56404525167383,339.72287116133));
#13685=CARTESIAN_POINT('Ctrl Pts',(100.294931967945,3.68964375443676,339.628090098688));
#13686=CARTESIAN_POINT('Ctrl Pts',(100.287529400771,3.81155632835938,339.528221770575));
#13687=CARTESIAN_POINT('Ctrl Pts',(100.280126833597,3.92935025544174,339.423588716479));
#13688=CARTESIAN_POINT('Ctrl Pts',(100.272728163843,4.04708216453596,339.319010751229));
#13689=CARTESIAN_POINT('Ctrl Pts',(100.265329494088,4.16069946706159,339.209673303264));
#13690=CARTESIAN_POINT('Ctrl Pts',(100.257930824333,4.26980222298958,339.095939396409));
#13691=CARTESIAN_POINT('Ctrl Pts',(100.250533375129,4.37888698035122,338.982224252116));
#13692=CARTESIAN_POINT('Ctrl Pts',(100.243135925925,4.4834584111145,338.864114357442));
#13693=CARTESIAN_POINT('Ctrl Pts',(100.235738476721,4.58315310782257,338.742009908158));
#13694=CARTESIAN_POINT('Ctrl Pts',(100.228341348258,4.68284348194232,338.619910753111));
#13695=CARTESIAN_POINT('Ctrl Pts',(100.220944219794,4.77765730639749,338.493817676917));
#13696=CARTESIAN_POINT('Ctrl Pts',(100.213547091331,4.86727136899175,338.364164083854));
#13697=CARTESIAN_POINT('Ctrl Pts',(100.206148823894,4.95689922991459,338.234490527375));
#13698=CARTESIAN_POINT('Ctrl Pts',(100.198750556457,5.04132552259523,338.101255669459));
#13699=CARTESIAN_POINT('Ctrl Pts',(100.191352289021,5.12027037836295,337.964921890195));
#13700=CARTESIAN_POINT('Ctrl Pts',(100.183951422495,5.19924296828892,337.828540215441));
#13701=CARTESIAN_POINT('Ctrl Pts',(100.176550555969,5.27273010036275,337.68905777454));
#13702=CARTESIAN_POINT('Ctrl Pts',(100.169149689443,5.34049794084267,337.546961386899));
#13703=CARTESIAN_POINT('Ctrl Pts',(100.161740696059,5.40834019689005,337.404708963841));
#13704=CARTESIAN_POINT('Ctrl Pts',(100.154331702674,5.47045045844053,337.259837198837));
#13705=CARTESIAN_POINT('Ctrl Pts',(100.146922709289,5.52664283949753,337.112853399347));
#13706=CARTESIAN_POINT('Ctrl Pts',(100.139509151709,5.58286983699978,336.965779052765));
#13707=CARTESIAN_POINT('Ctrl Pts',(100.132095594128,5.63317157067045,336.816590431933));
#13708=CARTESIAN_POINT('Ctrl Pts',(100.124682036548,5.67741224953052,336.665809326238));
#13709=CARTESIAN_POINT('Ctrl Pts',(100.117257924411,5.72171591309616,336.514813556035));
#13710=CARTESIAN_POINT('Ctrl Pts',(100.109833812275,5.75994119752516,336.362221133977));
#13711=CARTESIAN_POINT('Ctrl Pts',(100.102409700138,5.79200338991732,336.208564145458));
#13712=CARTESIAN_POINT('Ctrl Pts',(100.098552574983,5.80866098970979,336.128733153592));
#13713=CARTESIAN_POINT('Ctrl Pts',(100.094695449829,5.82365588836928,336.048614909744));
#13714=CARTESIAN_POINT('Ctrl Pts',(100.090838324674,5.8369817476534,335.968284379747));
#13715=CARTESIAN_POINT('Ctrl Pts',(100.083414347236,5.86263061169119,335.813668696206));
#13716=CARTESIAN_POINT('Ctrl Pts',(100.075990369798,5.88217050851072,335.657799945201));
#13717=CARTESIAN_POINT('Ctrl Pts',(100.06856639236,5.89548360449685,335.501202186357));
#13718=CARTESIAN_POINT('Ctrl Pts',(100.061151176332,5.90878098902664,335.34478923643));
#13719=CARTESIAN_POINT('Ctrl Pts',(100.053735960305,5.91586616884547,335.187649359434));
#13720=CARTESIAN_POINT('Ctrl Pts',(100.046320744277,5.91667233048297,335.030316599369));
#13721=CARTESIAN_POINT('Ctrl Pts',(100.038912663133,5.91747771643579,334.873135224092));
#13722=CARTESIAN_POINT('Ctrl Pts',(100.031504581989,5.91201611008612,334.715761705935));
#13723=CARTESIAN_POINT('Ctrl Pts',(100.024096500845,5.90027250815382,334.558734895982));
#13724=CARTESIAN_POINT('Ctrl Pts',(100.016693933671,5.88853764719892,334.401824963951));
#13725=CARTESIAN_POINT('Ctrl Pts',(100.009291366497,5.87053012858272,334.245261596863));
#13726=CARTESIAN_POINT('Ctrl Pts',(100.001888799323,5.84628701410339,334.089583221142));
#13727=CARTESIAN_POINT('Ctrl Pts',(99.9944901295682,5.82205666351787,333.933986809405));
#13728=CARTESIAN_POINT('Ctrl Pts',(99.9870914598135,5.79159731266814,333.779274828917));
#13729=CARTESIAN_POINT('Ctrl Pts',(99.9796927900588,5.75499780553456,333.625980050803));
#13730=CARTESIAN_POINT('Ctrl Pts',(99.9722953408548,5.71840433618311,333.472710561566));
#13731=CARTESIAN_POINT('Ctrl Pts',(99.9648978916508,5.67567280748164,333.320858173352));
#13732=CARTESIAN_POINT('Ctrl Pts',(99.9575004424468,5.62694309196391,333.170945052138));
#13733=CARTESIAN_POINT('Ctrl Pts',(99.9501033139833,5.57821548928169,333.021038430895));
#13734=CARTESIAN_POINT('Ctrl Pts',(99.9427061855198,5.52349033226132,332.873071264399));
#13735=CARTESIAN_POINT('Ctrl Pts',(99.9353090570564,5.46295717114055,332.727549888604));
#13736=CARTESIAN_POINT('Ctrl Pts',(99.9279107896197,5.40241468942382,332.582006106149));
#13737=CARTESIAN_POINT('Ctrl Pts',(99.9205125221831,5.33606256631044,332.438909208845));
#13738=CARTESIAN_POINT('Ctrl Pts',(99.9131142547465,5.2641381740847,332.298744764624));
#13739=CARTESIAN_POINT('Ctrl Pts',(99.9057133882207,5.19218851406397,332.158531079162));
#13740=CARTESIAN_POINT('Ctrl Pts',(99.898312521695,5.11466285763911,332.02125222975));
#13741=CARTESIAN_POINT('Ctrl Pts',(99.8909116551692,5.03184404078075,331.887368298086));
#13742=CARTESIAN_POINT('Ctrl Pts',(99.8835026617844,4.94893428094351,331.753337349065));
#13743=CARTESIAN_POINT('Ctrl Pts',(99.8760936683997,4.86071994945993,331.62270908028));
#13744=CARTESIAN_POINT('Ctrl Pts',(99.8686846750149,4.76752705841442,331.495914340404));
#13745=CARTESIAN_POINT('Ctrl Pts',(99.8612711174347,4.67427675733347,331.369041490595));
#13746=CARTESIAN_POINT('Ctrl Pts',(99.8538575598544,4.57604201767905,331.246007166438));
#13747=CARTESIAN_POINT('Ctrl Pts',(99.8464440022742,4.47318813898736,331.127207927642));
#13748=CARTESIAN_POINT('Ctrl Pts',(99.8390198901375,4.37018782896944,331.00823955638));
#13749=CARTESIAN_POINT('Ctrl Pts',(99.8315957780008,4.26255550061586,330.893518583876));
#13750=CARTESIAN_POINT('Ctrl Pts',(99.8241716658641,4.15069275287367,330.783404188953));
#13751=CARTESIAN_POINT('Ctrl Pts',(99.8203145407094,4.0925755517534,330.726195327512));
#13752=CARTESIAN_POINT('Ctrl Pts',(99.8164574155547,4.03331701132481,330.670229218396));
#13753=CARTESIAN_POINT('Ctrl Pts',(99.8126002904001,3.97297674196854,330.615551759882));
#13754=CARTESIAN_POINT('Ctrl Pts',(99.8051763129621,3.85683718716056,330.510311664708));
#13755=CARTESIAN_POINT('Ctrl Pts',(99.7977523355241,3.73633798849539,330.409530623692));
#13756=CARTESIAN_POINT('Ctrl Pts',(99.7903283580861,3.6118560723602,330.313591324366));
#13757=CARTESIAN_POINT('Ctrl Pts',(99.7829131420584,3.48752106361527,330.217765247849));
#13758=CARTESIAN_POINT('Ctrl Pts',(99.7754979260309,3.35921298596517,330.126769764857));
#13759=CARTESIAN_POINT('Ctrl Pts',(99.7680827100032,3.22734477179831,330.040950062114));
#13760=CARTESIAN_POINT('Ctrl Pts',(99.7606746288591,3.09560344056336,329.955212934657));
#13761=CARTESIAN_POINT('Ctrl Pts',(99.7532665477151,2.96030910314582,329.874641875189));
#13762=CARTESIAN_POINT('Ctrl Pts',(99.745858466571,2.82190677178258,329.799541103531));
#13763=CARTESIAN_POINT('Ctrl Pts',(99.738455899397,2.68360745580221,329.724496230748));
#13764=CARTESIAN_POINT('Ctrl Pts',(99.731053332223,2.54220507869098,329.65491371579));
#13765=CARTESIAN_POINT('Ctrl Pts',(99.723650765049,2.39817247098011,329.591053766034));
#13766=CARTESIAN_POINT('Ctrl Pts',(99.7162520952942,2.25421569580709,329.527227438262));
#13767=CARTESIAN_POINT('Ctrl Pts',(99.7088534255395,2.10763178827678,329.469117826199));
#13768=CARTESIAN_POINT('Ctrl Pts',(99.7014547557847,1.95891684556952,329.416938532074));
#13769=CARTESIAN_POINT('Ctrl Pts',(99.6940573065807,1.8102264362106,329.364767845911));
#13770=CARTESIAN_POINT('Ctrl Pts',(99.6866598573768,1.65940604121787,329.318525659483));
#13771=CARTESIAN_POINT('Ctrl Pts',(99.6792624081728,1.50697045415601,329.278376924963));
#13772=CARTESIAN_POINT('Ctrl Pts',(99.6718652797094,1.35454147643524,329.238229931221));
#13773=CARTESIAN_POINT('Ctrl Pts',(99.6644681512459,1.20049780679511,329.204175959125));
#13774=CARTESIAN_POINT('Ctrl Pts',(99.6570710227824,1.04536781045199,329.176329619272));
#13775=CARTESIAN_POINT('Ctrl Pts',(99.6496727553458,0.890213927962546,329.148478991778));
#13776=CARTESIAN_POINT('Ctrl Pts',(99.6422744879093,0.73397375308156,329.126837965635));
#13777=CARTESIAN_POINT('Ctrl Pts',(99.6348762204727,0.5771840660067,329.111469698095));
#13778=CARTESIAN_POINT('Ctrl Pts',(99.6274753539469,0.420339297065263,329.096096031522));
#13779=CARTESIAN_POINT('Ctrl Pts',(99.6200744874212,0.262945002766155,329.086999547471));
#13780=CARTESIAN_POINT('Ctrl Pts',(99.6126736208954,0.105541134396792,329.084191379748));
#13781=CARTESIAN_POINT('Ctrl Pts',(99.6052646275107,-0.0520355784683301,
329.081380128388));
#13782=CARTESIAN_POINT('Ctrl Pts',(99.597855634126,-0.20962151302473,329.084870990014));
#13783=CARTESIAN_POINT('Ctrl Pts',(99.5904466407412,-0.366677935584943,
329.09462297105));
#13784=CARTESIAN_POINT('Ctrl Pts',(99.583033083161,-0.523831110318572,329.104380959642));
#13785=CARTESIAN_POINT('Ctrl Pts',(99.5756195255808,-0.680453752658934,
329.120407715454));
#13786=CARTESIAN_POINT('Ctrl Pts',(99.5682059680006,-0.836014702547161,
329.142610651525));
#13787=CARTESIAN_POINT('Ctrl Pts',(99.5607818558639,-0.991797121927017,
329.164845197541));
#13788=CARTESIAN_POINT('Ctrl Pts',(99.5533577437272,-1.14651446398342,329.193273417778));
#13789=CARTESIAN_POINT('Ctrl Pts',(99.5459336315905,-1.29964735934819,329.227751971386));
#13790=CARTESIAN_POINT('Ctrl Pts',(99.5420765064357,-1.37920606372499,329.245664968115));
#13791=CARTESIAN_POINT('Ctrl Pts',(99.5382193812809,-1.45833735534825,329.26521026601));
#13792=CARTESIAN_POINT('Ctrl Pts',(99.5343622561261,-1.53697037878076,329.286362575622));
#13793=CARTESIAN_POINT('Ctrl Pts',(99.5269382786881,-1.68831879720438,329.327075350815));
#13794=CARTESIAN_POINT('Ctrl Pts',(99.5195143012501,-1.83827675530462,329.373867293602));
#13795=CARTESIAN_POINT('Ctrl Pts',(99.5120903238121,-1.9863184664741,329.426628532724));
#13796=CARTESIAN_POINT('Ctrl Pts',(99.5046751077845,-2.13418546615065,329.479327505646));
#13797=CARTESIAN_POINT('Ctrl Pts',(99.4972598917568,-2.28014037223469,329.537981628309));
#13798=CARTESIAN_POINT('Ctrl Pts',(99.4898446757292,-2.42366944843697,329.602430457399));
#13799=CARTESIAN_POINT('Ctrl Pts',(99.4824365945851,-2.56706042168449,329.66681727415));
#13800=CARTESIAN_POINT('Ctrl Pts',(99.475028513441,-2.70802987366323,329.736987545419));
#13801=CARTESIAN_POINT('Ctrl Pts',(99.4676204322969,-2.84608115778066,329.812731681721));
#13802=CARTESIAN_POINT('Ctrl Pts',(99.4602178651229,-2.98402968780591,329.888419440278));
#13803=CARTESIAN_POINT('Ctrl Pts',(99.4528152979489,-3.11906404903283,329.969672624391));
#13804=CARTESIAN_POINT('Ctrl Pts',(99.4454127307749,-3.25070955179678,330.05623443392));
#13805=CARTESIAN_POINT('Ctrl Pts',(99.4380140610203,-3.3822857437771,330.142750669033));
#13806=CARTESIAN_POINT('Ctrl Pts',(99.4306153912657,-3.51047631961996,330.234569758688));
#13807=CARTESIAN_POINT('Ctrl Pts',(99.4232167215111,-3.63483319000509,330.331390116605));
#13808=CARTESIAN_POINT('Ctrl Pts',(99.4158192723071,-3.75916954537005,330.42819450217));
#13809=CARTESIAN_POINT('Ctrl Pts',(99.4084218231031,-3.879673156275,330.529998289478));
#13810=CARTESIAN_POINT('Ctrl Pts',(99.4010243738991,-3.99592672658031,330.636457842727));
#13811=CARTESIAN_POINT('Ctrl Pts',(99.3936272454357,-4.11217525633365,330.742912780075));
#13812=CARTESIAN_POINT('Ctrl Pts',(99.3862301169722,-4.22417383664596,330.854022829934));
#13813=CARTESIAN_POINT('Ctrl Pts',(99.3788329885087,-4.33154016028266,330.969405701096));
#13814=CARTESIAN_POINT('Ctrl Pts',(99.3714347210721,-4.43892301565267,331.084806338339));
#13815=CARTESIAN_POINT('Ctrl Pts',(99.3640364536355,-4.5416719399151,331.204480833627));
#13816=CARTESIAN_POINT('Ctrl Pts',(99.3566381861989,-4.63944334022348,331.328011975053));
#13817=CARTESIAN_POINT('Ctrl Pts',(99.3492373196732,-4.73724908865262,331.451586514268));
#13818=CARTESIAN_POINT('Ctrl Pts',(99.3418364531475,-4.83007360008329,331.579020104727));
#13819=CARTESIAN_POINT('Ctrl Pts',(99.3344355866218,-4.91761531323803,331.709864715014));
#13820=CARTESIAN_POINT('Ctrl Pts',(99.327026593237,-5.00525315556376,331.840853005194));
#13821=CARTESIAN_POINT('Ctrl Pts',(99.3196175998523,-5.0875964070157,331.975259485043));
#13822=CARTESIAN_POINT('Ctrl Pts',(99.3122086064675,-5.16438800025667,332.112608937933));
#13823=CARTESIAN_POINT('Ctrl Pts',(99.3047950488872,-5.24122689976794,332.250043002824));
#13824=CARTESIAN_POINT('Ctrl Pts',(99.297381491307,-5.31250715766586,332.390423321351));
#13825=CARTESIAN_POINT('Ctrl Pts',(99.2899679337267,-5.37801919111498,332.533253125572));
#13826=CARTESIAN_POINT('Ctrl Pts',(99.28254382159,-5.44362449293725,332.676286274168));
#13827=CARTESIAN_POINT('Ctrl Pts',(99.2751197094533,-5.50344502751617,332.821775529035));
#13828=CARTESIAN_POINT('Ctrl Pts',(99.2676955973166,-5.5573202726657,332.969206571431));
#13829=CARTESIAN_POINT('Ctrl Pts',(99.2638384721618,-5.58531063157485,333.04580293363));
#13830=CARTESIAN_POINT('Ctrl Pts',(99.259981347007,-5.61169705604384,333.122923207148));
#13831=CARTESIAN_POINT('Ctrl Pts',(99.2561242218521,-5.63646246856781,333.200494122564));
#13832=CARTESIAN_POINT('Ctrl Pts',(99.2471743973967,-5.69392653461697,333.380484671991));
#13833=CARTESIAN_POINT('Ctrl Pts',(99.2382245729412,-5.74280101829535,333.563341817107));
#13834=CARTESIAN_POINT('Ctrl Pts',(99.2292747484858,-5.78283892385022,333.748319312563));
#13835=CARTESIAN_POINT('Ctrl Pts',(99.2203760436108,-5.82264814101625,333.932240254115));
#13836=CARTESIAN_POINT('Ctrl Pts',(99.2114773387359,-5.85372137608482,334.118257381203));
#13837=CARTESIAN_POINT('Ctrl Pts',(99.2025786338609,-5.87586259412093,334.305615857388));
#13838=CARTESIAN_POINT('Ctrl Pts',(99.1937730964491,-5.89777199852301,334.49101273195));
#13839=CARTESIAN_POINT('Ctrl Pts',(99.1849675590373,-5.91093537759809,334.677722982322));
#13840=CARTESIAN_POINT('Ctrl Pts',(99.1761620216254,-5.91520955858939,334.864994665021));
#13841=CARTESIAN_POINT('Ctrl Pts',(99.1741253679381,-5.91619814407475,334.90830917784));
#13842=CARTESIAN_POINT('Ctrl Pts',(99.1720887142508,-5.91671139333383,334.951653638754));
#13843=CARTESIAN_POINT('Ctrl Pts',(99.1700520605635,-5.91674790303204,334.995018587954));
#13844=CARTESIAN_POINT('',(97.4200520047035,-5.90851871549448,335.003050241221));
#13845=CARTESIAN_POINT('Ctrl Pts',(99.1700520047035,-5.91238628844001,334.995023448582));
#13846=CARTESIAN_POINT('Ctrl Pts',(99.1059967323284,-5.90156737437933,336.357909306957));
#13847=CARTESIAN_POINT('Ctrl Pts',(98.9491954485287,-4.75485099692124,339.710562044037));
#13848=CARTESIAN_POINT('Ctrl Pts',(98.6996481533043,0.824642780502851,341.947847667141));
#13849=CARTESIAN_POINT('Ctrl Pts',(98.4214101190303,6.28885485565189,338.066419332996));
#13850=CARTESIAN_POINT('Ctrl Pts',(98.1431720847566,5.9818776531124,331.37098323724));
#13851=CARTESIAN_POINT('Ctrl Pts',(97.8649340504824,0.185419620684727,328.005842260465));
#13852=CARTESIAN_POINT('Ctrl Pts',(97.6238940237982,-4.98351069473949,330.650937683327));
#13853=CARTESIAN_POINT('Ctrl Pts',(97.4756000085385,-5.90300490085091,333.819225757616));
#13854=CARTESIAN_POINT('Ctrl Pts',(97.4200520047035,-5.90851871549448,335.003050241221));
#13855=CARTESIAN_POINT('',(95.6700520047035,-5.92356759530611,335.003691307709));
#13856=CARTESIAN_POINT('Ctrl Pts',(97.4200520047035,-5.90851871549448,335.003050241221));
#13857=CARTESIAN_POINT('Ctrl Pts',(97.3828539971138,-5.91221106994108,335.795804419332));
#13858=CARTESIAN_POINT('Ctrl Pts',(97.2529099780996,-5.39419567492929,338.560510449033));
#13859=CARTESIAN_POINT('Ctrl Pts',(97.0302199476606,-1.19160955147132,341.894395520859));
#13860=CARTESIAN_POINT('Ctrl Pts',(96.7519819133865,5.15279597612825,339.733002910377));
#13861=CARTESIAN_POINT('Ctrl Pts',(96.4737438791129,6.76855669157607,333.228203388051));
#13862=CARTESIAN_POINT('Ctrl Pts',(96.1955058448389,2.17291283490253,328.349355464833));
#13863=CARTESIAN_POINT('Ctrl Pts',(95.927608553369,-4.17187446274379,329.528202769892));
#13864=CARTESIAN_POINT('Ctrl Pts',(95.752457273324,-5.91083243971606,333.258866916678));
#13865=CARTESIAN_POINT('Ctrl Pts',(95.6700520047035,-5.92356759530611,335.003691307709));
#13866=CARTESIAN_POINT('',(93.9200520047036,-5.91881622079639,334.9949747712));
#13867=CARTESIAN_POINT('Ctrl Pts',(95.6700520047035,-5.92356759530611,335.003691307709));
#13868=CARTESIAN_POINT('Ctrl Pts',(95.6597112618994,-5.92516568449061,335.222643087955));
#13869=CARTESIAN_POINT('Ctrl Pts',(95.5566245076704,-5.8146635492223,337.403741509423));
#13870=CARTESIAN_POINT('Ctrl Pts',(95.3607917420169,-3.10883504916976,341.267995497622));
#13871=CARTESIAN_POINT('Ctrl Pts',(95.0825537077432,3.58852210574754,341.006257738209));
#13872=CARTESIAN_POINT('Ctrl Pts',(94.8043156734692,6.99274549072358,335.232665904654));
#13873=CARTESIAN_POINT('Ctrl Pts',(94.5260776391951,3.97982955161444,329.245560004544));
#13874=CARTESIAN_POINT('Ctrl Pts',(94.2478396049213,-2.68531722482238,328.539218752868));
#13875=CARTESIAN_POINT('Ctrl Pts',(94.0458310600907,-5.73526615944503,332.330987701425));
#13876=CARTESIAN_POINT('Ctrl Pts',(93.9365685266848,-5.92317375626255,334.644710114703));
#13877=CARTESIAN_POINT('Ctrl Pts',(93.9200520047036,-5.92000683156533,334.994973760341));
#13878=CARTESIAN_POINT('',(92.1700520270473,-5.91150425643539,334.998948922259));
#13879=CARTESIAN_POINT('Ctrl Pts',(93.9200520047036,-5.91674786747094,334.994976527286));
#13880=CARTESIAN_POINT('Ctrl Pts',(93.9127497712506,-5.91687927201086,335.149747454818));
#13881=CARTESIAN_POINT('Ctrl Pts',(93.9054475377976,-5.91093376253086,335.304730384447));
#13882=CARTESIAN_POINT('Ctrl Pts',(93.8981453043445,-5.89888816629507,335.459400657427));
#13883=CARTESIAN_POINT('Ctrl Pts',(93.8908494566086,-5.88685310379126,335.613935673075));
#13884=CARTESIAN_POINT('Ctrl Pts',(93.8835536088727,-5.8687285990787,335.76815819435));
#13885=CARTESIAN_POINT('Ctrl Pts',(93.8762577611368,-5.84454352770003,335.921543007851));
#13886=CARTESIAN_POINT('Ctrl Pts',(93.8689665925407,-5.82037396724416,336.074829449099));
#13887=CARTESIAN_POINT('Ctrl Pts',(93.8616754239446,-5.79015163599576,336.227278872607));
#13888=CARTESIAN_POINT('Ctrl Pts',(93.8543842553485,-5.75395726397602,336.378370910473));
#13889=CARTESIAN_POINT('Ctrl Pts',(93.8470952608465,-5.71777368446038,336.529417895438));
#13890=CARTESIAN_POINT('Ctrl Pts',(93.8398062663444,-5.6756216927509,336.679107924966));
#13891=CARTESIAN_POINT('Ctrl Pts',(93.8325172718423,-5.6276331552403,336.826930658931));
#13892=CARTESIAN_POINT('Ctrl Pts',(93.8252291497028,-5.57965036110126,336.974735701151));
#13893=CARTESIAN_POINT('Ctrl Pts',(93.8179410275632,-5.52583252932446,337.120673525813));
#13894=CARTESIAN_POINT('Ctrl Pts',(93.8106529054237,-5.46636134326529,337.264249153109));
#13895=CARTESIAN_POINT('Ctrl Pts',(93.8033641179255,-5.40688472786907,337.407837887937));
#13896=CARTESIAN_POINT('Ctrl Pts',(93.7960753304273,-5.34175387893055,337.549063640338));
#13897=CARTESIAN_POINT('Ctrl Pts',(93.788786542929,-5.27119842506811,337.687451902092));
#13898=CARTESIAN_POINT('Ctrl Pts',(93.7814955519873,-5.20062164187481,337.825881999437));
#13899=CARTESIAN_POINT('Ctrl Pts',(93.7742045610455,-5.12461716627325,337.961472556544));
#13900=CARTESIAN_POINT('Ctrl Pts',(93.7669135701037,-5.04346016314264,338.093774417325));
#13901=CARTESIAN_POINT('Ctrl Pts',(93.7596149443138,-4.96221817548822,338.226214819577));
#13902=CARTESIAN_POINT('Ctrl Pts',(93.7523163185239,-4.87581309023246,338.355359321746));
#13903=CARTESIAN_POINT('Ctrl Pts',(93.745017692734,-4.78456321040497,338.480788049873));
#13904=CARTESIAN_POINT('Ctrl Pts',(93.7377147095408,-4.69325885285226,338.606291661078));
#13905=CARTESIAN_POINT('Ctrl Pts',(93.7304117263475,-4.59710417957538,338.728074779704));
#13906=CARTESIAN_POINT('Ctrl Pts',(93.7231087431543,-4.49645666286742,338.845751947468));
#13907=CARTESIAN_POINT('Ctrl Pts',(93.7157956129763,-4.39566930346896,338.963592619433));
#13908=CARTESIAN_POINT('Ctrl Pts',(93.7084824827983,-4.29037689992064,339.07731567077));
#13909=CARTESIAN_POINT('Ctrl Pts',(93.7011693526203,-4.18097292138371,339.186573299628));
#13910=CARTESIAN_POINT('Ctrl Pts',(93.6979007472047,-4.13207478501374,339.235406024971));
#13911=CARTESIAN_POINT('Ctrl Pts',(93.6946321417891,-4.08235573426027,339.283347262807));
#13912=CARTESIAN_POINT('Ctrl Pts',(93.6913635363735,-4.03185287865414,339.330368682617));
#13913=CARTESIAN_POINT('Ctrl Pts',(93.6839395589355,-3.91714583607711,339.437168346505));
#13914=CARTESIAN_POINT('Ctrl Pts',(93.6765155814975,-3.7980193007917,339.539568266908));
#13915=CARTESIAN_POINT('Ctrl Pts',(93.6690916040594,-3.67484499424399,339.637180698526));
#13916=CARTESIAN_POINT('Ctrl Pts',(93.6616763880318,-3.55181605191058,339.734677932788));
#13917=CARTESIAN_POINT('Ctrl Pts',(93.6542611720041,-3.42474913662316,339.827398695052));
#13918=CARTESIAN_POINT('Ctrl Pts',(93.6468459559765,-3.29405247922026,339.914992250924));
#13919=CARTESIAN_POINT('Ctrl Pts',(93.6394378748324,-3.16348157748305,340.002501524718));
#13920=CARTESIAN_POINT('Ctrl Pts',(93.6320297936882,-3.02928819453711,340.084893207155));
#13921=CARTESIAN_POINT('Ctrl Pts',(93.6246217125441,-2.89191319164979,340.161857093572));
#13922=CARTESIAN_POINT('Ctrl Pts',(93.6172191453701,-2.75464043948608,340.238763694363));
#13923=CARTESIAN_POINT('Ctrl Pts',(93.6098165781961,-2.61419110688851,340.310250361747));
#13924=CARTESIAN_POINT('Ctrl Pts',(93.602414011022,-2.47103446553667,340.376050523631));
#13925=CARTESIAN_POINT('Ctrl Pts',(93.5950153412673,-2.32795319553085,340.441816042017));
#13926=CARTESIAN_POINT('Ctrl Pts',(93.5876166715125,-2.18216779376351,340.501900862));
#13927=CARTESIAN_POINT('Ctrl Pts',(93.5802180017578,-2.0341714261272,340.556084698025));
#13928=CARTESIAN_POINT('Ctrl Pts',(93.5728205525538,-1.88619947329581,340.610259595399));
#13929=CARTESIAN_POINT('Ctrl Pts',(93.5654231033498,-1.73601762860874,340.658535312671));
#13930=CARTESIAN_POINT('Ctrl Pts',(93.5580256541458,-1.58413840995274,340.700739957287));
#13931=CARTESIAN_POINT('Ctrl Pts',(93.5506285256823,-1.4322657765151,340.742942771984));
#13932=CARTESIAN_POINT('Ctrl Pts',(93.5432313972188,-1.278696275026,340.779074937492));
#13933=CARTESIAN_POINT('Ctrl Pts',(93.5358342687553,-1.12395667395598,340.809014714869));
#13934=CARTESIAN_POINT('Ctrl Pts',(93.5284360013186,-0.969193246849669,
340.838959102226));
#13935=CARTESIAN_POINT('Ctrl Pts',(93.521037733882,-0.813259727865903,340.862709132061));
#13936=CARTESIAN_POINT('Ctrl Pts',(93.5136394664454,-0.656691994880478,
340.880194400388));
#13937=CARTESIAN_POINT('Ctrl Pts',(93.5062385999196,-0.500069258004175,
340.897685811475));
#13938=CARTESIAN_POINT('Ctrl Pts',(93.4988377333938,-0.342812234191548,
340.908908037715));
#13939=CARTESIAN_POINT('Ctrl Pts',(93.491436866868,-0.185460675013545,340.913842650978));
#13940=CARTESIAN_POINT('Ctrl Pts',(93.4840278734832,-0.0279363287802752,
340.918782682918));
#13941=CARTESIAN_POINT('Ctrl Pts',(93.4766188800984,0.129682386879827,340.917421301719));
#13942=CARTESIAN_POINT('Ctrl Pts',(93.4692098867137,0.286856233585559,340.909792218323));
#13943=CARTESIAN_POINT('Ctrl Pts',(93.4617963291334,0.444126904802365,340.902158435149));
#13944=CARTESIAN_POINT('Ctrl Pts',(93.4543827715531,0.60095179009131,340.888249288879));
#13945=CARTESIAN_POINT('Ctrl Pts',(93.4469692139729,0.756798526924307,340.868150181458));
#13946=CARTESIAN_POINT('Ctrl Pts',(93.4395451018362,0.912867140118635,340.848022459278));
#13947=CARTESIAN_POINT('Ctrl Pts',(93.4321209896994,1.06795445665763,340.821687237847));
#13948=CARTESIAN_POINT('Ctrl Pts',(93.4246968775627,1.22153921788592,340.789280827673));
#13949=CARTESIAN_POINT('Ctrl Pts',(93.4208397524083,1.3013326847631,340.772444392886));
#13950=CARTESIAN_POINT('Ctrl Pts',(93.4169826272538,1.38072083211056,340.753970031105));
#13951=CARTESIAN_POINT('Ctrl Pts',(93.4131255020994,1.45963246927007,340.733882072135));
#13952=CARTESIAN_POINT('Ctrl Pts',(93.4057015246614,1.61151714773126,340.695217899158));
#13953=CARTESIAN_POINT('Ctrl Pts',(93.3982775472234,1.76209362912566,340.650456326819));
#13954=CARTESIAN_POINT('Ctrl Pts',(93.3908535697854,1.910834690356,340.599700112384));
#13955=CARTESIAN_POINT('Ctrl Pts',(93.3834383537578,2.05940021475512,340.549003797918));
#13956=CARTESIAN_POINT('Ctrl Pts',(93.3760231377301,2.20613428081304,340.492327042776));
#13957=CARTESIAN_POINT('Ctrl Pts',(93.3686079217025,2.35052103136587,340.429823334475));
#13958=CARTESIAN_POINT('Ctrl Pts',(93.3611998405584,2.49476885371421,340.367379766927));
#13959=CARTESIAN_POINT('Ctrl Pts',(93.3537917594143,2.63667351675123,340.299120555318));
#13960=CARTESIAN_POINT('Ctrl Pts',(93.3463836782702,2.77573558743026,340.22524855975));
#13961=CARTESIAN_POINT('Ctrl Pts',(93.3389811110962,2.9146941516701,340.151431548458));
#13962=CARTESIAN_POINT('Ctrl Pts',(93.3315785439222,3.05081400822313,340.072010245948));
#13963=CARTESIAN_POINT('Ctrl Pts',(93.3241759767482,3.18361704109762,339.98723501533));
#13964=CARTESIAN_POINT('Ctrl Pts',(93.3167773069935,3.31635015375534,339.902504418501));
#13965=CARTESIAN_POINT('Ctrl Pts',(93.3093786372387,3.44576960679308,339.81242570772));
#13966=CARTESIAN_POINT('Ctrl Pts',(93.301979967484,3.57142327702471,339.717294387552));
#13967=CARTESIAN_POINT('Ctrl Pts',(93.29458251828,3.69705621830304,339.622178761097));
#13968=CARTESIAN_POINT('Ctrl Pts',(93.287185069076,3.81892431246661,339.522012404587));
#13969=CARTESIAN_POINT('Ctrl Pts',(93.2797876198721,3.93660565856321,339.417133284322));
#13970=CARTESIAN_POINT('Ctrl Pts',(93.2723904914086,4.05428190220172,339.312258711434));
#13971=CARTESIAN_POINT('Ctrl Pts',(93.2649933629451,4.16777148009504,339.20267202939));
#13972=CARTESIAN_POINT('Ctrl Pts',(93.2575962344817,4.27668695472454,339.088750329109));
#13973=CARTESIAN_POINT('Ctrl Pts',(93.2501979670451,4.38561919961824,338.97481108773));
#13974=CARTESIAN_POINT('Ctrl Pts',(93.2427996996084,4.48997568097655,338.856535768842));
#13975=CARTESIAN_POINT('Ctrl Pts',(93.2354014321718,4.58940720031757,338.734336903946));
#13976=CARTESIAN_POINT('Ctrl Pts',(93.2280005656461,4.68887365099706,338.612095109303));
#13977=CARTESIAN_POINT('Ctrl Pts',(93.2205996991203,4.78341145944938,338.485927313598));
#13978=CARTESIAN_POINT('Ctrl Pts',(93.2131988325946,4.87271303851913,338.356277432923));
#13979=CARTESIAN_POINT('Ctrl Pts',(93.2057898392098,4.96211267926027,338.226485184283));
#13980=CARTESIAN_POINT('Ctrl Pts',(93.1983808458251,5.04626439597001,338.093203522154));
#13981=CARTESIAN_POINT('Ctrl Pts',(93.1909718524403,5.12490472406927,337.956904146521));
#13982=CARTESIAN_POINT('Ctrl Pts',(93.1835582948601,5.20359349732318,337.820520805771));
#13983=CARTESIAN_POINT('Ctrl Pts',(93.1761447372798,5.27676394352619,337.681116376867));
#13984=CARTESIAN_POINT('Ctrl Pts',(93.1687311796996,5.34419978708432,337.539184750708));
#13985=CARTESIAN_POINT('Ctrl Pts',(93.1613070675629,5.41173163791164,337.397051058895));
#13986=CARTESIAN_POINT('Ctrl Pts',(93.1538829554262,5.47351243426087,337.252383326344));
#13987=CARTESIAN_POINT('Ctrl Pts',(93.1464588432895,5.52937471957837,337.105693656016));
#13988=CARTESIAN_POINT('Ctrl Pts',(93.1426017181348,5.55839742585336,337.029482466458));
#13989=CARTESIAN_POINT('Ctrl Pts',(93.1387445929801,5.58582342272072,336.952725742459));
#13990=CARTESIAN_POINT('Ctrl Pts',(93.1348874678255,5.61163464428278,336.875496516015));
#13991=CARTESIAN_POINT('Ctrl Pts',(93.1274634903875,5.66131463101879,336.726850047032));
#13992=CARTESIAN_POINT('Ctrl Pts',(93.1200395129495,5.7051592440521,336.576004016209));
#13993=CARTESIAN_POINT('Ctrl Pts',(93.1126155355115,5.74296958348887,336.423457384547));
#13994=CARTESIAN_POINT('Ctrl Pts',(93.1052003194839,5.78073530103625,336.271090780862));
#13995=CARTESIAN_POINT('Ctrl Pts',(93.0977851034563,5.81248083123473,336.117027929962));
#13996=CARTESIAN_POINT('Ctrl Pts',(93.0903698874287,5.83805608510027,335.961785688043));
#13997=CARTESIAN_POINT('Ctrl Pts',(93.0829618062846,5.86360673058536,335.806692819427));
#13998=CARTESIAN_POINT('Ctrl Pts',(93.0755537251405,5.88299885895413,335.650423184761));
#13999=CARTESIAN_POINT('Ctrl Pts',(93.0681456439964,5.89613278771588,335.493506547192));
#14000=CARTESIAN_POINT('Ctrl Pts',(93.0607430768224,5.90925694065456,335.336706705543));
#14001=CARTESIAN_POINT('Ctrl Pts',(93.0533405096484,5.9161321379307,335.179261190196));
#14002=CARTESIAN_POINT('Ctrl Pts',(93.0459379424744,5.91671017922907,335.021707544934));
#14003=CARTESIAN_POINT('Ctrl Pts',(93.0385392727197,5.91728791619122,334.86423685098));
#14004=CARTESIAN_POINT('Ctrl Pts',(93.0311406029651,5.9115750986757,334.706658512759));
#14005=CARTESIAN_POINT('Ctrl Pts',(93.0237419332104,5.89957555297738,334.549512644782));
#14006=CARTESIAN_POINT('Ctrl Pts',(93.0163444840064,5.88757798683141,334.392392700992));
#14007=CARTESIAN_POINT('Ctrl Pts',(93.0089470348025,5.86929577922842,334.235705457616));
#14008=CARTESIAN_POINT('Ctrl Pts',(93.0015495855985,5.84478481842733,334.079988593124));
#14009=CARTESIAN_POINT('Ctrl Pts',(92.9941524571351,5.8202749203788,333.924278480245));
#14010=CARTESIAN_POINT('Ctrl Pts',(92.9867553286716,5.78953686414773,333.769539031264));
#14011=CARTESIAN_POINT('Ctrl Pts',(92.9793582002081,5.75267808885966,333.616300116191));
#14012=CARTESIAN_POINT('Ctrl Pts',(92.9719599327716,5.7158136382404,333.46303760615));
#14013=CARTESIAN_POINT('Ctrl Pts',(92.964561665335,5.6728266793312,333.311276452942));
#14014=CARTESIAN_POINT('Ctrl Pts',(92.9571633978984,5.62387514733678,333.161533549485));
#14015=CARTESIAN_POINT('Ctrl Pts',(92.9497625313727,5.57490641815424,333.011738039772));
#14016=CARTESIAN_POINT('Ctrl Pts',(92.9423616648469,5.51996905980628,332.863962546006));
#14017=CARTESIAN_POINT('Ctrl Pts',(92.9349607983212,5.45926991774558,332.718705953259));
#14018=CARTESIAN_POINT('Ctrl Pts',(92.9275518049365,5.39850412222383,332.573289854885));
#14019=CARTESIAN_POINT('Ctrl Pts',(92.9201428115517,5.33196405163685,332.430398525928));
#14020=CARTESIAN_POINT('Ctrl Pts',(92.912733818167,5.25990379276315,332.2905087833));
#14021=CARTESIAN_POINT('Ctrl Pts',(92.9053202605868,5.18779914228446,332.150532863765));
#14022=CARTESIAN_POINT('Ctrl Pts',(92.8979067030065,5.11016771091606,332.013562539026));
#14023=CARTESIAN_POINT('Ctrl Pts',(92.8904931454263,5.02730778291849,331.880046952548));
#14024=CARTESIAN_POINT('Ctrl Pts',(92.8830690332896,4.94432988864364,331.746341282189));
#14025=CARTESIAN_POINT('Ctrl Pts',(92.875644921153,4.85610883987707,331.616100481387));
#14026=CARTESIAN_POINT('Ctrl Pts',(92.8682208090163,4.76298465457447,331.489742496228));
#14027=CARTESIAN_POINT('Ctrl Pts',(92.8643636838614,4.71460289106556,331.424094435678));
#14028=CARTESIAN_POINT('Ctrl Pts',(92.8605065587065,4.66489830492699,331.359493862144));
#14029=CARTESIAN_POINT('Ctrl Pts',(92.8566494335516,4.61392253382932,331.29599548943));
#14030=CARTESIAN_POINT('Ctrl Pts',(92.8492254561136,4.51580723828781,331.173777395008));
#14031=CARTESIAN_POINT('Ctrl Pts',(92.8418014786756,4.41268442872467,331.055276081702));
#14032=CARTESIAN_POINT('Ctrl Pts',(92.8343775012376,4.30486605594624,330.940928825105));
#14033=CARTESIAN_POINT('Ctrl Pts',(92.8269622852099,4.19717492507007,330.826716515476));
#14034=CARTESIAN_POINT('Ctrl Pts',(92.8195470691823,4.08479951490953,330.716648773124));
#14035=CARTESIAN_POINT('Ctrl Pts',(92.8121318531547,3.9680932391058,330.611131511624));
#14036=CARTESIAN_POINT('Ctrl Pts',(92.8047237720106,3.85149925749286,330.505715778301));
#14037=CARTESIAN_POINT('Ctrl Pts',(92.7973156908665,3.73058298121668,330.404842057776));
#14038=CARTESIAN_POINT('Ctrl Pts',(92.7899076097224,3.60573595549293,330.308880860417));
#14039=CARTESIAN_POINT('Ctrl Pts',(92.7825050425484,3.48098185569005,330.212991088729));
#14040=CARTESIAN_POINT('Ctrl Pts',(92.7751024753743,3.35230312662593,330.122006786087));
#14041=CARTESIAN_POINT('Ctrl Pts',(92.7676999082003,3.2201257163797,330.03625938095));
#14042=CARTESIAN_POINT('Ctrl Pts',(92.7603012384455,3.08801789696211,329.950557121446));
#14043=CARTESIAN_POINT('Ctrl Pts',(92.7529025686907,2.95241537720475,329.870086470917));
#14044=CARTESIAN_POINT('Ctrl Pts',(92.7455038989359,2.81377442154918,329.795136498703));
#14045=CARTESIAN_POINT('Ctrl Pts',(92.7381064497319,2.67515633734705,329.720198890907));
#14046=CARTESIAN_POINT('Ctrl Pts',(92.7307090005279,2.53350114004959,329.650780331211));
#14047=CARTESIAN_POINT('Ctrl Pts',(92.723311551324,2.38929121929656,329.58712479066));
#14048=CARTESIAN_POINT('Ctrl Pts',(92.7159144228605,2.24508755123427,329.523472010101));
#14049=CARTESIAN_POINT('Ctrl Pts',(92.708517294397,2.09832972138873,329.465581902562));
#14050=CARTESIAN_POINT('Ctrl Pts',(92.7011201659335,1.94952145022995,329.413650863257));
#14051=CARTESIAN_POINT('Ctrl Pts',(92.6937218984969,1.80069026631196,329.361711827867));
#14052=CARTESIAN_POINT('Ctrl Pts',(92.6863236310603,1.64980836483906,329.315733810647));
#14053=CARTESIAN_POINT('Ctrl Pts',(92.6789253636237,1.49739587989629,329.27586372093));
#14054=CARTESIAN_POINT('Ctrl Pts',(92.6715244970979,1.34492985084431,329.235979624431));
#14055=CARTESIAN_POINT('Ctrl Pts',(92.6641236305721,1.19093252857694,329.20220782207));
#14056=CARTESIAN_POINT('Ctrl Pts',(92.6567227640463,1.03593537213602,329.174644348432));
#14057=CARTESIAN_POINT('Ctrl Pts',(92.6493137706616,0.880768013999356,329.147050607464));
#14058=CARTESIAN_POINT('Ctrl Pts',(92.6419047772768,0.724598996762802,329.12567887519));
#14059=CARTESIAN_POINT('Ctrl Pts',(92.634495783892,0.567966786876173,329.110573517608));
#14060=CARTESIAN_POINT('Ctrl Pts',(92.6270822263118,0.411238086145321,329.095458854604));
#14061=CARTESIAN_POINT('Ctrl Pts',(92.6196686687315,0.254045995933292,329.086618279364));
#14062=CARTESIAN_POINT('Ctrl Pts',(92.6122551111513,0.096929629291864,329.084044015591));
#14063=CARTESIAN_POINT('Ctrl Pts',(92.6048309990146,-0.0604104212611402,
329.081466086882));
#14064=CARTESIAN_POINT('Ctrl Pts',(92.5974068868779,-0.217674160831285,
329.085172278375));
#14065=CARTESIAN_POINT('Ctrl Pts',(92.5899827747412,-0.374326126412815,
329.095102836324));
#14066=CARTESIAN_POINT('Ctrl Pts',(92.5861256495867,-0.455713129441094,
329.10026216099));
#14067=CARTESIAN_POINT('Ctrl Pts',(92.5822685244321,-0.536935133518491,
329.107100730755));
#14068=CARTESIAN_POINT('Ctrl Pts',(92.5784113992776,-0.617918184534345,
329.115604731179));
#14069=CARTESIAN_POINT('Ctrl Pts',(92.5709874218396,-0.773789803814569,
329.131972752633));
#14070=CARTESIAN_POINT('Ctrl Pts',(92.5635634444016,-0.929245755728457,
329.15456306299));
#14071=CARTESIAN_POINT('Ctrl Pts',(92.5561394669636,-1.08374951142005,329.183349971075));
#14072=CARTESIAN_POINT('Ctrl Pts',(92.5487242509359,-1.23807092943315,329.212102906276));
#14073=CARTESIAN_POINT('Ctrl Pts',(92.5413090349083,-1.39144202470665,329.247037815032));
#14074=CARTESIAN_POINT('Ctrl Pts',(92.5338938188807,-1.54333020345631,329.288077167398));
#14075=CARTESIAN_POINT('Ctrl Pts',(92.5264857377366,-1.69507223616481,329.329077031905));
#14076=CARTESIAN_POINT('Ctrl Pts',(92.5190776565926,-1.845333835068,329.376169549952));
#14077=CARTESIAN_POINT('Ctrl Pts',(92.5116695754485,-1.99359154250904,329.429225967234));
#14078=CARTESIAN_POINT('Ctrl Pts',(92.5042670082745,-2.14173889903071,329.482242893656));
#14079=CARTESIAN_POINT('Ctrl Pts',(92.4968644411006,-2.28788498406668,329.541214755328));
#14080=CARTESIAN_POINT('Ctrl Pts',(92.4894618739266,-2.43152058740869,329.60596271838));
#14081=CARTESIAN_POINT('Ctrl Pts',(92.4820632041719,-2.57508056723278,329.670676591912));
#14082=CARTESIAN_POINT('Ctrl Pts',(92.4746645344172,-2.71613235833852,329.741160357322));
#14083=CARTESIAN_POINT('Ctrl Pts',(92.4672658646625,-2.85418596528124,329.817186764112));
#14084=CARTESIAN_POINT('Ctrl Pts',(92.4598684154585,-2.99221679766649,329.893200628907));
#14085=CARTESIAN_POINT('Ctrl Pts',(92.4524709662546,-3.12725010092552,329.974755140508));
#14086=CARTESIAN_POINT('Ctrl Pts',(92.4450735170506,-3.25881966589009,330.061576673906));
#14087=CARTESIAN_POINT('Ctrl Pts',(92.4376763885871,-3.39038352622762,330.148394442874));
#14088=CARTESIAN_POINT('Ctrl Pts',(92.4302792601237,-3.51848363537998,330.240478574009));
#14089=CARTESIAN_POINT('Ctrl Pts',(92.4228821316602,-3.64268224837314,330.33751175874));
#14090=CARTESIAN_POINT('Ctrl Pts',(92.4154838642236,-3.76689998485228,330.43455988416));
#14091=CARTESIAN_POINT('Ctrl Pts',(92.408085596787,-3.8872147349197,330.536558350696));
#14092=CARTESIAN_POINT('Ctrl Pts',(92.4006873293505,-4.00322148498267,330.64314926757));
#14093=CARTESIAN_POINT('Ctrl Pts',(92.3932864628247,-4.11926898943731,330.749777630955));
#14094=CARTESIAN_POINT('Ctrl Pts',(92.385885596299,-4.23100520597538,330.861001404555));
#14095=CARTESIAN_POINT('Ctrl Pts',(92.3784847297732,-4.33806177408423,330.976425642948));
#14096=CARTESIAN_POINT('Ctrl Pts',(92.3710757363884,-4.44523590053988,331.091976628189));
#14097=CARTESIAN_POINT('Ctrl Pts',(92.3636667430036,-4.54771986235856,331.211737015859));
#14098=CARTESIAN_POINT('Ctrl Pts',(92.3562577496189,-4.64518495613238,331.335278007021));
#14099=CARTESIAN_POINT('Ctrl Pts',(92.3488441920386,-4.74271009176625,331.458895103696));
#14100=CARTESIAN_POINT('Ctrl Pts',(92.3414306344583,-4.83520997978545,331.586297143367));
#14101=CARTESIAN_POINT('Ctrl Pts',(92.334017076878,-4.92239941443725,331.717026566168));
#14102=CARTESIAN_POINT('Ctrl Pts',(92.3265929647413,-5.00971297921125,331.847942106235));
#14103=CARTESIAN_POINT('Ctrl Pts',(92.3191688526046,-5.0917007969904,331.982194172792));
#14104=CARTESIAN_POINT('Ctrl Pts',(92.3117447404679,-5.16812334621587,332.119300147395));
#14105=CARTESIAN_POINT('Ctrl Pts',(92.3078876153132,-5.20782793736116,332.190532221179));
#14106=CARTESIAN_POINT('Ctrl Pts',(92.3040304901585,-5.24603112507699,332.262534279703));
#14107=CARTESIAN_POINT('Ctrl Pts',(92.3001733650038,-5.28270450540837,332.335236657593));
#14108=CARTESIAN_POINT('Ctrl Pts',(92.2922446478177,-5.3580904079244,332.484683867605));
#14109=CARTESIAN_POINT('Ctrl Pts',(92.2843159306316,-5.42721247029743,332.637494118537));
#14110=CARTESIAN_POINT('Ctrl Pts',(92.2763872134455,-5.48977933379852,332.793134931923));
#14111=CARTESIAN_POINT('Ctrl Pts',(92.2684733496026,-5.5522289870276,332.948484174004));
#14112=CARTESIAN_POINT('Ctrl Pts',(92.2605594857598,-5.60814781624935,333.106653132832));
#14113=CARTESIAN_POINT('Ctrl Pts',(92.2526456219169,-5.65729082478846,333.267085955316));
#14114=CARTESIAN_POINT('Ctrl Pts',(92.2447527932948,-5.70630321015079,333.427092343897));
#14115=CARTESIAN_POINT('Ctrl Pts',(92.2368599646728,-5.74857561356557,333.58935031139));
#14116=CARTESIAN_POINT('Ctrl Pts',(92.2289671360507,-5.78391172835668,333.75328604681));
#14117=CARTESIAN_POINT('Ctrl Pts',(92.22108714372,-5.81919037519964,333.916955169718));
#14118=CARTESIAN_POINT('Ctrl Pts',(92.2132071513893,-5.84755515751885,334.08229633424));
#14119=CARTESIAN_POINT('Ctrl Pts',(92.2053271590587,-5.86885928070626,334.248720221377));
#14120=CARTESIAN_POINT('Ctrl Pts',(92.1974651758119,-5.89011471504646,334.414763760206));
#14121=CARTESIAN_POINT('Ctrl Pts',(92.1896031925652,-5.90434163731046,334.581884794039));
#14122=CARTESIAN_POINT('Ctrl Pts',(92.1817412093184,-5.91144417937927,334.749483979389));
#14123=CARTESIAN_POINT('Ctrl Pts',(92.1778448241734,-5.91496418680491,334.832545842486));
#14124=CARTESIAN_POINT('Ctrl Pts',(92.1739484390285,-5.91673510119079,334.915724957293));
#14125=CARTESIAN_POINT('Ctrl Pts',(92.1700520538834,-5.91674990637331,334.998947416805));
#14126=CARTESIAN_POINT('',(90.4200520047035,-5.91614342231082,335.00545103649));
#14127=CARTESIAN_POINT('Ctrl Pts',(92.1700520047035,-5.90713672806163,334.9989501757));
#14128=CARTESIAN_POINT('Ctrl Pts',(92.1206797800456,-5.90547239974453,336.051773050695));
#14129=CARTESIAN_POINT('Ctrl Pts',(91.9785615439628,-5.13393945780749,339.08460722529));
#14130=CARTESIAN_POINT('Ctrl Pts',(91.7436972964561,-0.279901569715299,
341.991014091852));
#14131=CARTESIAN_POINT('Ctrl Pts',(91.4654592621819,5.72742209646294,339.018614070817));
#14132=CARTESIAN_POINT('Ctrl Pts',(91.187221227908,6.47877504132782,332.358391231638));
#14133=CARTESIAN_POINT('Ctrl Pts',(90.9089831936341,1.28465175732854,328.122333769104));
#14134=CARTESIAN_POINT('Ctrl Pts',(90.6532601192325,-4.57267337374315,330.029862090751));
#14135=CARTESIAN_POINT('Ctrl Pts',(90.4902830562557,-5.90248644698631,333.513572395831));
#14136=CARTESIAN_POINT('Ctrl Pts',(90.4200520047035,-5.91614342231082,335.00545103649));
#14137=CARTESIAN_POINT('',(88.6700510690619,-5.92177106793959,334.998328828675));
#14138=CARTESIAN_POINT('Ctrl Pts',(90.420051987023,-5.91674748815069,335.005451968678));
#14139=CARTESIAN_POINT('Ctrl Pts',(90.4104409465018,-5.91655934632297,335.209632834768));
#14140=CARTESIAN_POINT('Ctrl Pts',(90.4008299059805,-5.90579871717187,335.413343160755));
#14141=CARTESIAN_POINT('Ctrl Pts',(90.3912188654592,-5.88463187011856,335.615660877176));
#14142=CARTESIAN_POINT('Ctrl Pts',(90.3813759739492,-5.86295440671688,335.822859185085));
#14143=CARTESIAN_POINT('Ctrl Pts',(90.3715330824393,-5.83036257602901,336.028597195015));
#14144=CARTESIAN_POINT('Ctrl Pts',(90.3616901909294,-5.78708280121524,336.231910392187));
#14145=CARTESIAN_POINT('Ctrl Pts',(90.3586291689817,-5.7736233070752,336.295138373333));
#14146=CARTESIAN_POINT('Ctrl Pts',(90.3555681470339,-5.75913048755993,336.35813200794));
#14147=CARTESIAN_POINT('Ctrl Pts',(90.3525071250861,-5.74361208103852,336.420862704503));
#14148=CARTESIAN_POINT('Ctrl Pts',(90.3450831476481,-5.70597487952363,336.573005120961));
#14149=CARTESIAN_POINT('Ctrl Pts',(90.3376591702101,-5.66223157998761,336.723880562478));
#14150=CARTESIAN_POINT('Ctrl Pts',(90.3302351927721,-5.61248137558281,336.872961123792));
#14151=CARTESIAN_POINT('Ctrl Pts',(90.3228199767445,-5.56278988390454,337.021865747613));
#14152=CARTESIAN_POINT('Ctrl Pts',(90.3154047607168,-5.50710571521944,337.168979357021));
#14153=CARTESIAN_POINT('Ctrl Pts',(90.3079895446892,-5.44557886855915,337.313785069708));
#14154=CARTESIAN_POINT('Ctrl Pts',(90.3005814635451,-5.38411122272096,337.458451451066));
#14155=CARTESIAN_POINT('Ctrl Pts',(90.293173382401,-5.31681223582546,337.600814015401));
#14156=CARTESIAN_POINT('Ctrl Pts',(90.2857653012568,-5.24388138932037,337.740371970598));
#14157=CARTESIAN_POINT('Ctrl Pts',(90.2783627340828,-5.17100482657627,337.87982605026));
#14158=CARTESIAN_POINT('Ctrl Pts',(90.2709601669088,-5.0925049230122,338.016479347992));
#14159=CARTESIAN_POINT('Ctrl Pts',(90.2635575997348,-5.00862880601297,338.149852067332));
#14160=CARTESIAN_POINT('Ctrl Pts',(90.2561589299801,-4.92479684942301,338.283154566518));
#14161=CARTESIAN_POINT('Ctrl Pts',(90.2487602602254,-4.83559451479498,338.413179612019));
#14162=CARTESIAN_POINT('Ctrl Pts',(90.2413615904706,-4.74131424553725,338.539473094624));
#14163=CARTESIAN_POINT('Ctrl Pts',(90.2339641412667,-4.64704952959606,338.665745742726));
#14164=CARTESIAN_POINT('Ctrl Pts',(90.2265666920627,-4.54770876463457,338.788287750904));
#14165=CARTESIAN_POINT('Ctrl Pts',(90.2191692428587,-4.4436270590002,338.906674944633));
#14166=CARTESIAN_POINT('Ctrl Pts',(90.2117721143952,-4.33954986616713,339.025057005299));
#14167=CARTESIAN_POINT('Ctrl Pts',(90.2043749859318,-4.23073238780169,339.139284329412));
#14168=CARTESIAN_POINT('Ctrl Pts',(90.1969778574683,-4.11754908880057,339.248966940777));
#14169=CARTESIAN_POINT('Ctrl Pts',(90.1895795900317,-4.00434836239684,339.358666440527));
#14170=CARTESIAN_POINT('Ctrl Pts',(90.1821813225951,-3.88678074489291,339.463819574451));
#14171=CARTESIAN_POINT('Ctrl Pts',(90.1747830551585,-3.76525639929152,339.564074365092));
#14172=CARTESIAN_POINT('Ctrl Pts',(90.1673821886327,-3.6436893609092,339.664364376297));
#14173=CARTESIAN_POINT('Ctrl Pts',(90.1599813221069,-3.51816311456883,339.759752380678));
#14174=CARTESIAN_POINT('Ctrl Pts',(90.1525804555812,-3.3891194882614,339.849927799131));
#14175=CARTESIAN_POINT('Ctrl Pts',(90.1451714621964,-3.25993415971541,339.940202238815));
#14176=CARTESIAN_POINT('Ctrl Pts',(90.1377624688116,-3.12722404384612,340.025252447698));
#14177=CARTESIAN_POINT('Ctrl Pts',(90.1303534754269,-2.99145904998252,340.104811780544));
#14178=CARTESIAN_POINT('Ctrl Pts',(90.1229399178466,-2.85561042019957,340.184420124683));
#14179=CARTESIAN_POINT('Ctrl Pts',(90.1155263602664,-2.71670349097573,340.258530677302));
#14180=CARTESIAN_POINT('Ctrl Pts',(90.1081128026861,-2.57523068084449,340.326923831156));
#14181=CARTESIAN_POINT('Ctrl Pts',(90.1006886905494,-2.43355645826807,340.395414355186));
#14182=CARTESIAN_POINT('Ctrl Pts',(90.0932645784127,-2.28930940031275,340.458171075227));
#14183=CARTESIAN_POINT('Ctrl Pts',(90.085840466276,-2.14300046696549,340.515023078926));
#14184=CARTESIAN_POINT('Ctrl Pts',(90.0819833411215,-2.06698708559968,340.544559983746));
#14185=CARTESIAN_POINT('Ctrl Pts',(90.0781262159669,-1.9904173953332,340.572503901069));
#14186=CARTESIAN_POINT('Ctrl Pts',(90.0742690908124,-1.91336430444853,340.598836272027));
#14187=CARTESIAN_POINT('Ctrl Pts',(90.0668451133744,-1.7650568512715,340.649519337794));
#14188=CARTESIAN_POINT('Ctrl Pts',(90.0594211359363,-1.61451046434392,340.694382022628));
#14189=CARTESIAN_POINT('Ctrl Pts',(90.0519971584983,-1.46222274957149,340.733222060337));
#14190=CARTESIAN_POINT('Ctrl Pts',(90.0445819424707,-1.3101147572153,340.772016260958));
#14191=CARTESIAN_POINT('Ctrl Pts',(90.037166726443,-1.1562698857,340.804801870969));
#14192=CARTESIAN_POINT('Ctrl Pts',(90.0297515104154,-1.00120396546976,340.83142531308));
#14193=CARTESIAN_POINT('Ctrl Pts',(90.0223434292713,-0.846287248887313,
340.858023138248));
#14194=CARTESIAN_POINT('Ctrl Pts',(90.0149353481272,-0.690152187941684,
340.878470536731));
#14195=CARTESIAN_POINT('Ctrl Pts',(90.007527266983,-0.533327860263088,340.892664249384));
#14196=CARTESIAN_POINT('Ctrl Pts',(90.000124699809,-0.376620259795989,340.906847397398));
#14197=CARTESIAN_POINT('Ctrl Pts',(89.992722132635,-0.219224784220909,340.914786094336));
#14198=CARTESIAN_POINT('Ctrl Pts',(89.985319565461,-0.0616786394269871,
340.916428509493));
#14199=CARTESIAN_POINT('Ctrl Pts',(89.9779208957063,0.0957845580107002,
340.918070059925));
#14200=CARTESIAN_POINT('Ctrl Pts',(89.9705222259515,0.253397894432321,340.913421926644));
#14201=CARTESIAN_POINT('Ctrl Pts',(89.9631235561967,0.410621241804524,340.902484287));
#14202=CARTESIAN_POINT('Ctrl Pts',(89.9557261069927,0.567818652206232,340.891548451726));
#14203=CARTESIAN_POINT('Ctrl Pts',(89.9483286577887,0.724625829295427,340.874325195212));
#14204=CARTESIAN_POINT('Ctrl Pts',(89.9409312085847,0.880504729307353,340.85086677204));
#14205=CARTESIAN_POINT('Ctrl Pts',(89.9335340801212,1.03637687068193,340.827409365985));
#14206=CARTESIAN_POINT('Ctrl Pts',(89.9261369516578,1.1913204459509,340.797717386349));
#14207=CARTESIAN_POINT('Ctrl Pts',(89.9187398231943,1.34480487136977,340.761894690155));
#14208=CARTESIAN_POINT('Ctrl Pts',(89.9113415557576,1.49831292955868,340.726066478161));
#14209=CARTESIAN_POINT('Ctrl Pts',(89.903943288321,1.65036102707908,340.684105754859));
#14210=CARTESIAN_POINT('Ctrl Pts',(89.8965450208844,1.80043121584224,340.636166959869));
#14211=CARTESIAN_POINT('Ctrl Pts',(89.8891441543587,1.95055412584089,340.588211323477));
#14212=CARTESIAN_POINT('Ctrl Pts',(89.8817432878329,2.09869738832798,340.534273547477));
#14213=CARTESIAN_POINT('Ctrl Pts',(89.8743424213071,2.24436073222976,340.47455710228));
#14214=CARTESIAN_POINT('Ctrl Pts',(89.8669334279223,2.39018402840932,340.414775082717));
#14215=CARTESIAN_POINT('Ctrl Pts',(89.8595244345375,2.53352162212728,340.349201863242));
#14216=CARTESIAN_POINT('Ctrl Pts',(89.8521154411528,2.67389499081471,340.2780883036));
#14217=CARTESIAN_POINT('Ctrl Pts',(89.8447018835725,2.81435483433905,340.206930935551));
#14218=CARTESIAN_POINT('Ctrl Pts',(89.8372883259923,2.95184648899596,340.130226607802));
#14219=CARTESIAN_POINT('Ctrl Pts',(89.8298747684121,3.08591880644607,340.048270563522));
#14220=CARTESIAN_POINT('Ctrl Pts',(89.8224506562754,3.22018200038529,339.966197839809));
#14221=CARTESIAN_POINT('Ctrl Pts',(89.8150265441386,3.35101582507747,339.878858673592));
#14222=CARTESIAN_POINT('Ctrl Pts',(89.8076024320019,3.4780000469114,339.786590251545));
#14223=CARTESIAN_POINT('Ctrl Pts',(89.8037453068474,3.54397346262093,339.738653091505));
#14224=CARTESIAN_POINT('Ctrl Pts',(89.7998881816928,3.60890835182653,339.689386062502));
#14225=CARTESIAN_POINT('Ctrl Pts',(89.7960310565382,3.67274965312461,339.638840431398));
#14226=CARTESIAN_POINT('Ctrl Pts',(89.7886070791002,3.79562779719748,339.541553045101));
#14227=CARTESIAN_POINT('Ctrl Pts',(89.7811831016622,3.91482307429404,339.439233149551));
#14228=CARTESIAN_POINT('Ctrl Pts',(89.7737591242242,4.02989611135027,339.332189734329));
#14229=CARTESIAN_POINT('Ctrl Pts',(89.7663439081966,4.14483334490911,339.225272646442));
#14230=CARTESIAN_POINT('Ctrl Pts',(89.7589286921689,4.25565775141133,339.113643386663));
#14231=CARTESIAN_POINT('Ctrl Pts',(89.7515134761413,4.36196103898518,338.997652618334));
#14232=CARTESIAN_POINT('Ctrl Pts',(89.7441053949972,4.46816204207088,338.881773455739));
#14233=CARTESIAN_POINT('Ctrl Pts',(89.7366973138531,4.56985033618628,338.761541412585));
#14234=CARTESIAN_POINT('Ctrl Pts',(89.729289232709,4.66665277425075,338.637345522091));
#14235=CARTESIAN_POINT('Ctrl Pts',(89.721886665535,4.76338316049274,338.513242072867));
#14236=CARTESIAN_POINT('Ctrl Pts',(89.714484098361,4.85523470329714,338.385180944007));
#14237=CARTESIAN_POINT('Ctrl Pts',(89.707081531187,4.94187310418581,338.253585834833));
#14238=CARTESIAN_POINT('Ctrl Pts',(89.6996828614322,5.02846589033494,338.122060009909));
#14239=CARTESIAN_POINT('Ctrl Pts',(89.6922841916775,5.10985079608434,337.987004221151));
#14240=CARTESIAN_POINT('Ctrl Pts',(89.6848855219227,5.18573567629961,337.84887276972));
#14241=CARTESIAN_POINT('Ctrl Pts',(89.6774880727187,5.26160803786605,337.710764105689));
#14242=CARTESIAN_POINT('Ctrl Pts',(89.6700906235148,5.33198199513823,337.569581112771));
#14243=CARTESIAN_POINT('Ctrl Pts',(89.6626931743108,5.39661032375546,337.425804521398));
#14244=CARTESIAN_POINT('Ctrl Pts',(89.6552960458473,5.46123585020104,337.282034163928));
#14245=CARTESIAN_POINT('Ctrl Pts',(89.6478989173839,5.52011609031253,337.135670772002));
#14246=CARTESIAN_POINT('Ctrl Pts',(89.6405017889204,5.57305125036858,336.987216727804));
#14247=CARTESIAN_POINT('Ctrl Pts',(89.6331035214838,5.62599456111788,336.83873982539));
#14248=CARTESIAN_POINT('Ctrl Pts',(89.6257052540472,5.67299084378648,336.688171981297));
#14249=CARTESIAN_POINT('Ctrl Pts',(89.6183069866105,5.71388967851577,336.536032325262));
#14250=CARTESIAN_POINT('Ctrl Pts',(89.6109061200848,5.7548028814358,336.383839220967));
#14251=CARTESIAN_POINT('Ctrl Pts',(89.603505253559,5.78961427467648,336.230073565502));
#14252=CARTESIAN_POINT('Ctrl Pts',(89.5961043870333,5.81822423546171,336.075266156998));
#14253=CARTESIAN_POINT('Ctrl Pts',(89.5886953936485,5.84686561271912,335.92028875516));
#14254=CARTESIAN_POINT('Ctrl Pts',(89.5812864002637,5.86929189019015,335.764267682981));
#14255=CARTESIAN_POINT('Ctrl Pts',(89.573877406879,5.88545506516443,335.6077410949));
#14256=CARTESIAN_POINT('Ctrl Pts',(89.5664638492987,5.90162819721203,335.451118081041));
#14257=CARTESIAN_POINT('Ctrl Pts',(89.5590502917185,5.91153051519712,335.293989302346));
#14258=CARTESIAN_POINT('Ctrl Pts',(89.5516367341382,5.91516615314655,335.136893912098));
#14259=CARTESIAN_POINT('Ctrl Pts',(89.5442126220015,5.9188069670922,334.979574867801));
#14260=CARTESIAN_POINT('Ctrl Pts',(89.5367885098648,5.91616328870546,334.822289679041));
#14261=CARTESIAN_POINT('Ctrl Pts',(89.5293643977281,5.90729125293326,334.66557420028));
#14262=CARTESIAN_POINT('Ctrl Pts',(89.5255072725736,5.90268187315569,334.584154199597));
#14263=CARTESIAN_POINT('Ctrl Pts',(89.521650147419,5.89639217191359,334.502887849604));
#14264=CARTESIAN_POINT('Ctrl Pts',(89.5177930222644,5.88843546371964,334.421849196049));
#14265=CARTESIAN_POINT('Ctrl Pts',(89.5103690448264,5.87312083955135,334.265870556134));
#14266=CARTESIAN_POINT('Ctrl Pts',(89.5029450673884,5.85158126034507,334.110265538108));
#14267=CARTESIAN_POINT('Ctrl Pts',(89.4955210899504,5.82383879205416,333.955570832146));
#14268=CARTESIAN_POINT('Ctrl Pts',(89.4881058739228,5.79612906404991,333.801058689211));
#14269=CARTESIAN_POINT('Ctrl Pts',(89.4806906578952,5.76223108345799,333.647455083697));
#14270=CARTESIAN_POINT('Ctrl Pts',(89.4732754418676,5.72221878040337,333.495293121004));
#14271=CARTESIAN_POINT('Ctrl Pts',(89.4658673607235,5.68224497698528,333.343277567785));
#14272=CARTESIAN_POINT('Ctrl Pts',(89.4584592795794,5.636168657678,333.192701254375));
#14273=CARTESIAN_POINT('Ctrl Pts',(89.4510511984353,5.58411503751873,333.044088496312));
#14274=CARTESIAN_POINT('Ctrl Pts',(89.4436486312613,5.53210016181966,332.89558635344));
#14275=CARTESIAN_POINT('Ctrl Pts',(89.4362460640873,5.47411696674855,332.749045206557));
#14276=CARTESIAN_POINT('Ctrl Pts',(89.4288434969133,5.41034084201738,332.604975462402));
#14277=CARTESIAN_POINT('Ctrl Pts',(89.4214448271586,5.34659829513706,332.460981570336));
#14278=CARTESIAN_POINT('Ctrl Pts',(89.4140461574039,5.277069043448,332.319456830024));
#14279=CARTESIAN_POINT('Ctrl Pts',(89.4066474876491,5.20197702199252,332.180892760968));
#14280=CARTESIAN_POINT('Ctrl Pts',(89.3992500384452,5.12689738838885,332.042351550681));
#14281=CARTESIAN_POINT('Ctrl Pts',(89.3918525892412,5.04625698397372,331.906770370101));
#14282=CARTESIAN_POINT('Ctrl Pts',(89.3844551400372,4.96032627793727,331.774617266292));
#14283=CARTESIAN_POINT('Ctrl Pts',(89.3770580115738,4.87439929770649,331.64246989241));
#14284=CARTESIAN_POINT('Ctrl Pts',(89.3696608831103,4.78318267538167,331.513750612644));
#14285=CARTESIAN_POINT('Ctrl Pts',(89.3622637546468,4.6869907550137,331.388899305625));
#14286=CARTESIAN_POINT('Ctrl Pts',(89.3548654872102,4.59078402349128,331.264028774621));
#14287=CARTESIAN_POINT('Ctrl Pts',(89.3474672197737,4.48960069636764,331.143027697883));
#14288=CARTESIAN_POINT('Ctrl Pts',(89.3400689523371,4.38379592009836,331.026303497569));
#14289=CARTESIAN_POINT('Ctrl Pts',(89.3326680858113,4.27795397349836,330.909538290816));
#14290=CARTESIAN_POINT('Ctrl Pts',(89.3252672192856,4.16748759573141,330.797053228328));
#14291=CARTESIAN_POINT('Ctrl Pts',(89.3178663527598,4.05278923467022,330.689219330348));
#14292=CARTESIAN_POINT('Ctrl Pts',(89.3104573593751,3.937964923843,330.58126702044));
#14293=CARTESIAN_POINT('Ctrl Pts',(89.3030483659903,3.81889962124384,330.477976330628));
#14294=CARTESIAN_POINT('Ctrl Pts',(89.2956393726056,3.69601989539976,330.379678853661));
#14295=CARTESIAN_POINT('Ctrl Pts',(89.2882258150254,3.57306447140599,330.281320822058));
#14296=CARTESIAN_POINT('Ctrl Pts',(89.2808122574451,3.44629024166273,330.187962353408));
#14297=CARTESIAN_POINT('Ctrl Pts',(89.2733986998649,3.31615282882766,330.099891738098));
#14298=CARTESIAN_POINT('Ctrl Pts',(89.2659745877282,3.18583014156066,330.011695738144));
#14299=CARTESIAN_POINT('Ctrl Pts',(89.2585504755915,3.05213502473042,329.928802823039));
#14300=CARTESIAN_POINT('Ctrl Pts',(89.2511263634548,2.91554846762974,329.851455769307));
#14301=CARTESIAN_POINT('Ctrl Pts',(89.2472692383,2.8445862521478,329.811270860848));
#14302=CARTESIAN_POINT('Ctrl Pts',(89.2434121131452,2.77284392644715,329.772582119761));
#14303=CARTESIAN_POINT('Ctrl Pts',(89.2395549879904,2.70039096242497,329.735418419993));
#14304=CARTESIAN_POINT('Ctrl Pts',(89.2321310105524,2.56093757457113,329.663887822068));
#14305=CARTESIAN_POINT('Ctrl Pts',(89.2247070331144,2.41842969297576,329.597794109881));
#14306=CARTESIAN_POINT('Ctrl Pts',(89.2172830556764,2.27333057300988,329.53740916155));
#14307=CARTESIAN_POINT('Ctrl Pts',(89.2098678396487,2.12840269183701,329.477095476543));
#14308=CARTESIAN_POINT('Ctrl Pts',(89.2024526236211,1.98089000060662,329.422477286888));
#14309=CARTESIAN_POINT('Ctrl Pts',(89.1950374075934,1.83128080685596,329.373780917086));
#14310=CARTESIAN_POINT('Ctrl Pts',(89.1876293264493,1.68181556631823,329.325131402687));
#14311=CARTESIAN_POINT('Ctrl Pts',(89.1802212453053,1.53025819173092,329.282392479334));
#14312=CARTESIAN_POINT('Ctrl Pts',(89.1728131641612,1.3771173522576,329.245742588256));
#14313=CARTESIAN_POINT('Ctrl Pts',(89.1654105969871,1.22409049830801,329.209119976361));
#14314=CARTESIAN_POINT('Ctrl Pts',(89.1580080298131,1.06948288764735,329.178577459006));
#14315=CARTESIAN_POINT('Ctrl Pts',(89.1506054626391,0.913818645627798,329.154243757613));
#14316=CARTESIAN_POINT('Ctrl Pts',(89.1432067928844,0.758236360151347,329.129922867808));
#14317=CARTESIAN_POINT('Ctrl Pts',(89.1358081231296,0.60159891904849,329.111804341225));
#14318=CARTESIAN_POINT('Ctrl Pts',(89.1284094533749,0.444440835655226,329.099965855514));
#14319=CARTESIAN_POINT('Ctrl Pts',(89.1210120041709,0.287308678465478,329.088129322786));
#14320=CARTESIAN_POINT('Ctrl Pts',(89.1136145549669,0.129656421243884,329.082570802788));
#14321=CARTESIAN_POINT('Ctrl Pts',(89.106217105763,-0.0279759788522484,
329.08331613933));
#14322=CARTESIAN_POINT('Ctrl Pts',(89.0988199772995,-0.185601544282214,
329.084061443556));
#14323=CARTESIAN_POINT('Ctrl Pts',(89.091422848836,-0.343206881091485,329.091110059099));
#14324=CARTESIAN_POINT('Ctrl Pts',(89.0840257203725,-0.500251976352694,
329.104435690907));
#14325=CARTESIAN_POINT('Ctrl Pts',(89.0766274529359,-0.657321252638202,
329.117763374529));
#14326=CARTESIAN_POINT('Ctrl Pts',(89.0692291854993,-0.813829743716658,
329.137369967296));
#14327=CARTESIAN_POINT('Ctrl Pts',(89.0618309180627,-0.969242649478629,
329.163177298484));
#14328=CARTESIAN_POINT('Ctrl Pts',(89.0544300515369,-1.12471015342897,329.188993696059));
#14329=CARTESIAN_POINT('Ctrl Pts',(89.0470291850112,-1.27908093780846,329.221015108116));
#14330=CARTESIAN_POINT('Ctrl Pts',(89.0396283184854,-1.43183062771581,329.259112297211));
#14331=CARTESIAN_POINT('Ctrl Pts',(89.0322193251006,-1.58474805138602,329.297251320661));
#14332=CARTESIAN_POINT('Ctrl Pts',(89.0248103317159,-1.73604046326154,329.341479354688));
#14333=CARTESIAN_POINT('Ctrl Pts',(89.0174013383311,-1.88519817921912,329.39161713258));
#14334=CARTESIAN_POINT('Ctrl Pts',(89.0099877807509,-2.03444778147482,329.441785797073));
#14335=CARTESIAN_POINT('Ctrl Pts',(89.0025742231706,-2.18155971949618,329.49787132718));
#14336=CARTESIAN_POINT('Ctrl Pts',(88.9951606655904,-2.32604500018266,329.559646590558));
#14337=CARTESIAN_POINT('Ctrl Pts',(88.9877365534537,-2.47073598211767,329.621509802334));
#14338=CARTESIAN_POINT('Ctrl Pts',(88.980312441317,-2.61279250201358,329.689078765579));
#14339=CARTESIAN_POINT('Ctrl Pts',(88.9728883291803,-2.75175011300632,329.762080386444));
#14340=CARTESIAN_POINT('Ctrl Pts',(88.9690312040257,-2.82394418644098,329.800007667577));
#14341=CARTESIAN_POINT('Ctrl Pts',(88.9651740788711,-2.89530226321513,329.83940062205));
#14342=CARTESIAN_POINT('Ctrl Pts',(88.9613169537165,-2.96576246738171,329.880216454813));
#14343=CARTESIAN_POINT('Ctrl Pts',(88.9538929762785,-3.10138030321598,329.958776472805));
#14344=CARTESIAN_POINT('Ctrl Pts',(88.9464689988405,-3.23407910767295,330.04284729059));
#14345=CARTESIAN_POINT('Ctrl Pts',(88.9390450214025,-3.36337955858028,330.132186475693));
#14346=CARTESIAN_POINT('Ctrl Pts',(88.9316298053749,-3.49252741550123,330.221420227116));
#14347=CARTESIAN_POINT('Ctrl Pts',(88.9242145893472,-3.61828459791148,330.315909759804));
#14348=CARTESIAN_POINT('Ctrl Pts',(88.9167993733196,-3.74019653348104,330.415366922704));
#14349=CARTESIAN_POINT('Ctrl Pts',(88.9093912921755,-3.86199116600011,330.514728388423));
#14350=CARTESIAN_POINT('Ctrl Pts',(88.9019832110314,-3.97994763019167,330.619047734263));
#14351=CARTESIAN_POINT('Ctrl Pts',(88.8945751298873,-4.09364060094926,330.72799377426));
#14352=CARTESIAN_POINT('Ctrl Pts',(88.8871725627133,-4.20724894795202,330.836858723729));
#14353=CARTESIAN_POINT('Ctrl Pts',(88.8797699955393,-4.31659985190306,330.950343253272));
#14354=CARTESIAN_POINT('Ctrl Pts',(88.8723674283653,-4.4213014339096,331.068076273246));
#14355=CARTESIAN_POINT('Ctrl Pts',(88.8649687586106,-4.52594789099111,331.1857473073));
#14356=CARTESIAN_POINT('Ctrl Pts',(88.8575700888559,-4.6259496537724,331.307662098862));
#14357=CARTESIAN_POINT('Ctrl Pts',(88.8501714191011,-4.72095214562284,331.433413200097));
#14358=CARTESIAN_POINT('Ctrl Pts',(88.8427739698971,-4.81593896501203,331.559143556306));
#14359=CARTESIAN_POINT('Ctrl Pts',(88.8353765206932,-4.90592792553089,331.688708668649));
#14360=CARTESIAN_POINT('Ctrl Pts',(88.8279790714892,-4.99060509276845,331.8216684612));
#14361=CARTESIAN_POINT('Ctrl Pts',(88.8205819430257,-5.07527858855166,331.954622488846));
#14362=CARTESIAN_POINT('Ctrl Pts',(88.8131848145622,-5.15464054850606,332.09097058925));
#14363=CARTESIAN_POINT('Ctrl Pts',(88.8057876860988,-5.2284208527207,332.230244424261));
#14364=CARTESIAN_POINT('Ctrl Pts',(88.7983894186622,-5.30221251726033,332.369539703966));
#14365=CARTESIAN_POINT('Ctrl Pts',(88.7909911512256,-5.37042064009199,332.511761285448));
#14366=CARTESIAN_POINT('Ctrl Pts',(88.783592883789,-5.43282154561915,332.656417141222));
#14367=CARTESIAN_POINT('Ctrl Pts',(88.7761920172632,-5.49524437324065,332.80112381612));
#14368=CARTESIAN_POINT('Ctrl Pts',(88.7687911507375,-5.55185577391612,332.948266125513));
#14369=CARTESIAN_POINT('Ctrl Pts',(88.7613902842117,-5.60248065682288,333.097333173563));
#14370=CARTESIAN_POINT('Ctrl Pts',(88.753981290827,-5.65316113069103,333.246563911482));
#14371=CARTESIAN_POINT('Ctrl Pts',(88.7465722974422,-5.69784183853674,333.397723255326));
#14372=CARTESIAN_POINT('Ctrl Pts',(88.7391633040575,-5.73639771023748,333.550285589338));
#14373=CARTESIAN_POINT('Ctrl Pts',(88.7317497464772,-5.7749773336851,333.702941907009));
#14374=CARTESIAN_POINT('Ctrl Pts',(88.724336188897,-5.80742452583055,333.857002572714));
#14375=CARTESIAN_POINT('Ctrl Pts',(88.7169226313168,-5.83366566488127,334.011933467379));
#14376=CARTESIAN_POINT('Ctrl Pts',(88.7094985191801,-5.85994416299754,334.167084934537));
#14377=CARTESIAN_POINT('Ctrl Pts',(88.7020744070434,-5.87999891440106,334.323108735878));
#14378=CARTESIAN_POINT('Ctrl Pts',(88.6946502949067,-5.89380823068842,334.479466521375));
#14379=CARTESIAN_POINT('Ctrl Pts',(88.690793169752,-5.900982726472,334.560700686009));
#14380=CARTESIAN_POINT('Ctrl Pts',(88.6869360445973,-5.9064723005119,334.642025003162));
#14381=CARTESIAN_POINT('Ctrl Pts',(88.6830789194426,-5.9102794554545,334.72336428117));
#14382=CARTESIAN_POINT('Ctrl Pts',(88.6787366145296,-5.91456550450621,334.81493505794));
#14383=CARTESIAN_POINT('Ctrl Pts',(88.6743943096166,-5.91672357262935,334.906606214109));
#14384=CARTESIAN_POINT('Ctrl Pts',(88.6700520047036,-5.91674975877771,334.998310472272));
#14385=CARTESIAN_POINT('',(86.9200532024049,-5.91345947321307,334.995429316743));
#14386=CARTESIAN_POINT('Ctrl Pts',(88.6700502969966,-5.92591451127428,334.998343975863));
#14387=CARTESIAN_POINT('Ctrl Pts',(88.5816471597205,-5.91883322604964,336.868206066303));
#14388=CARTESIAN_POINT('Ctrl Pts',(88.4004980110199,-3.95334079215119,340.712572307138));
#14389=CARTESIAN_POINT('Ctrl Pts',(88.1266028508947,2.5977797484408,341.496473143162));
#14390=CARTESIAN_POINT('Ctrl Pts',(87.8483648166207,6.86883054471249,336.331085973649));
#14391=CARTESIAN_POINT('Ctrl Pts',(87.5701267823467,4.83645693387304,329.944180852918));
#14392=CARTESIAN_POINT('Ctrl Pts',(87.2918887480729,-1.63426181919367,328.196926339695));
#14393=CARTESIAN_POINT('Ctrl Pts',(87.075197847428,-5.50564593875477,331.698261224195));
#14394=CARTESIAN_POINT('Ctrl Pts',(86.9512529582079,-5.91578097000932,334.331223968412));
#14395=CARTESIAN_POINT('Ctrl Pts',(86.9200540804124,-5.91104854439068,334.995412478147));
#14396=CARTESIAN_POINT('',(85.1700508174281,-5.91265977156438,335.003771382507));
#14397=CARTESIAN_POINT('Ctrl Pts',(86.9200520047035,-5.91674825227522,334.995452286488));
#14398=CARTESIAN_POINT('Ctrl Pts',(86.9123586994878,-5.9168742583105,335.15939093106));
#14399=CARTESIAN_POINT('Ctrl Pts',(86.904665394272,-5.91018172402343,335.323406540034));
#14400=CARTESIAN_POINT('Ctrl Pts',(86.8969720890562,-5.89668281031374,335.486890539085));
#14401=CARTESIAN_POINT('Ctrl Pts',(86.8895765307271,-5.88370633259449,335.644047367906));
#14402=CARTESIAN_POINT('Ctrl Pts',(86.882180972398,-5.8644404998989,335.800712565962));
#14403=CARTESIAN_POINT('Ctrl Pts',(86.8747854140689,-5.83894918947698,335.956348746643));
#14404=CARTESIAN_POINT('Ctrl Pts',(86.8673893946862,-5.81345628987677,336.111994629989));
#14405=CARTESIAN_POINT('Ctrl Pts',(86.8599933753034,-5.78173719942712,336.266611000192));
#14406=CARTESIAN_POINT('Ctrl Pts',(86.8525973559207,-5.74390721152469,336.419669154379));
#14407=CARTESIAN_POINT('Ctrl Pts',(86.8451994203594,-5.70606742253748,336.572766963242));
#14408=CARTESIAN_POINT('Ctrl Pts',(86.837801484798,-5.66211367295776,336.724305390377));
#14409=CARTESIAN_POINT('Ctrl Pts',(86.8304035492367,-5.61221152486639,336.873769559646));
#14410=CARTESIAN_POINT('Ctrl Pts',(86.8230022415009,-5.56228663005751,337.023301858632));
#14411=CARTESIAN_POINT('Ctrl Pts',(86.8156009337651,-5.50640805566121,337.170757663903));
#14412=CARTESIAN_POINT('Ctrl Pts',(86.8081996260293,-5.44478995781093,337.315640921607));
#14413=CARTESIAN_POINT('Ctrl Pts',(86.8007894619212,-5.38309812801616,337.460697545979));
#14414=CARTESIAN_POINT('Ctrl Pts',(86.7933792978132,-5.31565320750368,337.603175133357));
#14415=CARTESIAN_POINT('Ctrl Pts',(86.7859691337051,-5.24271620041503,337.742600482098));
#14416=CARTESIAN_POINT('Ctrl Pts',(86.7785537337463,-5.16972765772175,337.88212434557));
#14417=CARTESIAN_POINT('Ctrl Pts',(86.7711383337874,-5.0912394818629,338.018591351566));
#14418=CARTESIAN_POINT('Ctrl Pts',(86.7637229338285,-5.00755637960994,338.151556705428));
#14419=CARTESIAN_POINT('Ctrl Pts',(86.7562969808181,-4.92375418572361,338.284711285797));
#14420=CARTESIAN_POINT('Ctrl Pts',(86.7488710278077,-4.83474251551918,338.414353959321));
#14421=CARTESIAN_POINT('Ctrl Pts',(86.7414450747972,-4.74086715485042,338.54007191771));
#14422=CARTESIAN_POINT('Ctrl Pts',(86.7394342763732,-4.71544759899988,338.574113807317));
#14423=CARTESIAN_POINT('Ctrl Pts',(86.7374234779491,-4.68967164190016,338.60786813478));
#14424=CARTESIAN_POINT('Ctrl Pts',(86.7354126795251,-4.663546611525,338.641327170776));
#14425=CARTESIAN_POINT('Ctrl Pts',(86.727988702087,-4.5670915746845,338.764859756322));
#14426=CARTESIAN_POINT('Ctrl Pts',(86.720564724649,-4.4655792630452,338.884743557117));
#14427=CARTESIAN_POINT('Ctrl Pts',(86.713140747211,-4.35931569085774,339.00053712268));
#14428=CARTESIAN_POINT('Ctrl Pts',(86.7057255311833,-4.25317752567361,339.116194034414));
#14429=CARTESIAN_POINT('Ctrl Pts',(86.6983103151557,-4.14229951105499,339.227770047022));
#14430=CARTESIAN_POINT('Ctrl Pts',(86.6908950991281,-4.02702954403851,339.33485450897));
#14431=CARTESIAN_POINT('Ctrl Pts',(86.6834870179839,-3.91187048920382,339.441835934788));
#14432=CARTESIAN_POINT('Ctrl Pts',(86.6760789368398,-3.79232816658171,339.544334161424));
#14433=CARTESIAN_POINT('Ctrl Pts',(86.6686708556957,-3.66878907963946,339.641973422115));
#14434=CARTESIAN_POINT('Ctrl Pts',(86.6612682885216,-3.54534194509598,339.739540008121));
#14435=CARTESIAN_POINT('Ctrl Pts',(86.6538657213476,-3.41790426116913,339.832254598968));
#14436=CARTESIAN_POINT('Ctrl Pts',(86.6464631541736,-3.28689745908954,339.919780041418));
#14437=CARTESIAN_POINT('Ctrl Pts',(86.6390644844188,-3.15595963151851,340.007259402104));
#14438=CARTESIAN_POINT('Ctrl Pts',(86.6316658146641,-3.02145673772766,340.089554848654));
#14439=CARTESIAN_POINT('Ctrl Pts',(86.6242671449093,-2.88384109486179,340.166371173472));
#14440=CARTESIAN_POINT('Ctrl Pts',(86.6168696957053,-2.74624815430399,340.243174825982));
#14441=CARTESIAN_POINT('Ctrl Pts',(86.6094722465013,-2.60554380937926,340.314500968952));
#14442=CARTESIAN_POINT('Ctrl Pts',(86.6020747972973,-2.46220710937423,340.380099135987));
#14443=CARTESIAN_POINT('Ctrl Pts',(86.5946776688338,-2.31887662419832,340.4456944588));
#14444=CARTESIAN_POINT('Ctrl Pts',(86.5872805403703,-2.17291435023966,340.50556214418));
#14445=CARTESIAN_POINT('Ctrl Pts',(86.5798834119068,-2.02482130847057,340.559499009017));
#14446=CARTESIAN_POINT('Ctrl Pts',(86.5724851444701,-1.87670546406953,340.613444178785));
#14447=CARTESIAN_POINT('Ctrl Pts',(86.5650868770335,-1.72645854929582,340.661456581983));
#14448=CARTESIAN_POINT('Ctrl Pts',(86.5576886095969,-1.57459866584797,340.703382295096));
#14449=CARTESIAN_POINT('Ctrl Pts',(86.5502877430711,-1.42268543242737,340.745322737151));
#14450=CARTESIAN_POINT('Ctrl Pts',(86.5428868765454,-1.26915846165383,340.781172132474));
#14451=CARTESIAN_POINT('Ctrl Pts',(86.5354860100196,-1.11454786652365,340.810827274642));
#14452=CARTESIAN_POINT('Ctrl Pts',(86.5280770166348,-0.959767494177773,
340.840514980992));
#14453=CARTESIAN_POINT('Ctrl Pts',(86.5206680232501,-0.803901487883792,
340.86399478012));
#14454=CARTESIAN_POINT('Ctrl Pts',(86.5132590298653,-0.647487665506531,
340.881215034797));
#14455=CARTESIAN_POINT('Ctrl Pts',(86.505845472285,-0.490977486819397,340.898445897743));
#14456=CARTESIAN_POINT('Ctrl Pts',(86.4984319147047,-0.333919191023641,
340.90940950653));
#14457=CARTESIAN_POINT('Ctrl Pts',(86.4910183571245,-0.176851947027658,
340.914106352724));
#14458=CARTESIAN_POINT('Ctrl Pts',(86.4835942449878,-0.0195610890550666,
340.918809885739));
#14459=CARTESIAN_POINT('Ctrl Pts',(86.4761701328511,0.137738370374983,340.917228841115));
#14460=CARTESIAN_POINT('Ctrl Pts',(86.4687460207144,0.294510209793697,340.909415732442));
#14461=CARTESIAN_POINT('Ctrl Pts',(86.4648888955599,0.375959492104575,340.905356507925));
#14462=CARTESIAN_POINT('Ctrl Pts',(86.4610317704055,0.457266479000304,340.899615962269));
#14463=CARTESIAN_POINT('Ctrl Pts',(86.457174645251,0.538357036472173,340.892206909451));
#14464=CARTESIAN_POINT('Ctrl Pts',(86.449750667813,0.69443557813221,340.877946381531));
#14465=CARTESIAN_POINT('Ctrl Pts',(86.4423266903751,0.850182560432624,340.857458516544));
#14466=CARTESIAN_POINT('Ctrl Pts',(86.4349027129371,1.00506115637499,340.830761754218));
#14467=CARTESIAN_POINT('Ctrl Pts',(86.4274874969094,1.15975697227141,340.804096498087));
#14468=CARTESIAN_POINT('Ctrl Pts',(86.4200722808818,1.31358607753257,340.771236992768));
#14469=CARTESIAN_POINT('Ctrl Pts',(86.4126570648542,1.46601487947295,340.732253565193));
#14470=CARTESIAN_POINT('Ctrl Pts',(86.4052489837101,1.6182970151876,340.693307647275));
#14471=CARTESIAN_POINT('Ctrl Pts',(86.397840902566,1.76918117077637,340.648249629638));
#14472=CARTESIAN_POINT('Ctrl Pts',(86.3904328214219,1.91814219674899,340.597201182337));
#14473=CARTESIAN_POINT('Ctrl Pts',(86.3830302542479,2.06699234830908,340.546190731328));
#14474=CARTESIAN_POINT('Ctrl Pts',(86.3756276870739,2.21392186887688,340.48919884922));
#14475=CARTESIAN_POINT('Ctrl Pts',(86.3682251198999,2.35841917847937,340.426397473562));
#14476=CARTESIAN_POINT('Ctrl Pts',(86.3608264501452,2.50284041088029,340.363629162554));
#14477=CARTESIAN_POINT('Ctrl Pts',(86.3534277803904,2.64483164118487,340.295057597912));
#14478=CARTESIAN_POINT('Ctrl Pts',(86.3460291106357,2.78389984826712,340.220903389004));
#14479=CARTESIAN_POINT('Ctrl Pts',(86.3386316614317,2.92294511341351,340.146761413239));
#14480=CARTESIAN_POINT('Ctrl Pts',(86.3312342122277,3.0590679833657,340.06703879645));
#14481=CARTESIAN_POINT('Ctrl Pts',(86.3238367630237,3.19179859453153,339.982002839667));
#14482=CARTESIAN_POINT('Ctrl Pts',(86.3164396345602,3.32452345072947,339.896970569894));
#14483=CARTESIAN_POINT('Ctrl Pts',(86.3090425060968,3.45385602633921,339.80662561952));
#14484=CARTESIAN_POINT('Ctrl Pts',(86.3016453776333,3.57935432915095,339.711279353731));
#14485=CARTESIAN_POINT('Ctrl Pts',(86.2942471101967,3.70487195556828,339.615918406996));
#14486=CARTESIAN_POINT('Ctrl Pts',(86.2868488427601,3.82655383646696,339.515554837309));
#14487=CARTESIAN_POINT('Ctrl Pts',(86.2794505753235,3.94399015971994,339.410541030592));
#14488=CARTESIAN_POINT('Ctrl Pts',(86.2720497087978,4.0614677395886,339.30549033142));
#14489=CARTESIAN_POINT('Ctrl Pts',(86.264648842272,4.17469651419082,339.195786391189));
#14490=CARTESIAN_POINT('Ctrl Pts',(86.2572479757462,4.28330282048432,339.08181914231));
#14491=CARTESIAN_POINT('Ctrl Pts',(86.2498389823614,4.39202838688538,338.967726746497));
#14492=CARTESIAN_POINT('Ctrl Pts',(86.2424299889767,4.49612109048732,338.849361963128));
#14493=CARTESIAN_POINT('Ctrl Pts',(86.2350209955919,4.59524646433407,338.727149110852));
#14494=CARTESIAN_POINT('Ctrl Pts',(86.2276074380116,4.6944329028301,338.604860971244));
#14495=CARTESIAN_POINT('Ctrl Pts',(86.2201938804314,4.78864569121504,338.478720337424));
#14496=CARTESIAN_POINT('Ctrl Pts',(86.2127803228512,4.87759346762527,338.349180874047));
#14497=CARTESIAN_POINT('Ctrl Pts',(86.2053562107145,4.96666787747923,338.219456987528));
#14498=CARTESIAN_POINT('Ctrl Pts',(86.1979320985778,5.05046210666401,338.086324922291));
#14499=CARTESIAN_POINT('Ctrl Pts',(86.1905079864411,5.12873013477052,337.950264016524));
#14500=CARTESIAN_POINT('Ctrl Pts',(86.1866508612864,5.16939352649414,337.879574898077));
#14501=CARTESIAN_POINT('Ctrl Pts',(86.1827937361318,5.20856605518826,337.808095579537));
#14502=CARTESIAN_POINT('Ctrl Pts',(86.1789366109771,5.24621837823364,337.735895336153));
#14503=CARTESIAN_POINT('Ctrl Pts',(86.1715126335392,5.31868945074736,337.596928370755));
#14504=CARTESIAN_POINT('Ctrl Pts',(86.1640886561012,5.3857443968736,337.454870251285));
#14505=CARTESIAN_POINT('Ctrl Pts',(86.1566646786632,5.44710821507903,337.310182385813));
#14506=CARTESIAN_POINT('Ctrl Pts',(86.1492494626356,5.50839961474629,337.165665273791));
#14507=CARTESIAN_POINT('Ctrl Pts',(86.1418342466079,5.56401311126594,337.018524933571));
#14508=CARTESIAN_POINT('Ctrl Pts',(86.1344190305803,5.61371908643525,336.869248132564));
#14509=CARTESIAN_POINT('Ctrl Pts',(86.1270109494362,5.66337723476544,336.720114964943));
#14510=CARTESIAN_POINT('Ctrl Pts',(86.1196028682921,5.70713906078391,336.568849780765));
#14511=CARTESIAN_POINT('Ctrl Pts',(86.112194787148,5.74482269091336,336.415960032087));
#14512=CARTESIAN_POINT('Ctrl Pts',(86.1047922199741,5.78247827242856,336.263184082042));
#14513=CARTESIAN_POINT('Ctrl Pts',(86.0973896528001,5.81406457728902,336.108786335991));
#14514=CARTESIAN_POINT('Ctrl Pts',(86.0899870856261,5.83944934616971,335.953290037721));
#14515=CARTESIAN_POINT('Ctrl Pts',(86.0825884158713,5.86482075008083,335.797875607571));
#14516=CARTESIAN_POINT('Ctrl Pts',(86.0751897461165,5.88399706063643,335.641364144494));
#14517=CARTESIAN_POINT('Ctrl Pts',(86.0677910763617,5.89689699093968,335.48428962486));
#14518=CARTESIAN_POINT('Ctrl Pts',(86.0603936271578,5.90979479315489,335.327241017645));
#14519=CARTESIAN_POINT('Ctrl Pts',(86.0529961779538,5.91641823955004,335.169629909822));
#14520=CARTESIAN_POINT('Ctrl Pts',(86.0455987287498,5.91673783911079,335.011996071631));
#14521=CARTESIAN_POINT('Ctrl Pts',(86.0382016002864,5.91705742481426,334.854369068169));
#14522=CARTESIAN_POINT('Ctrl Pts',(86.0308044718229,5.91107370638444,334.696719709511));
#14523=CARTESIAN_POINT('Ctrl Pts',(86.0234073433595,5.8988093301012,334.539588173902));
#14524=CARTESIAN_POINT('Ctrl Pts',(86.0160090759229,5.88654306541016,334.382432443959));
#14525=CARTESIAN_POINT('Ctrl Pts',(86.0086108084863,5.86799424635611,334.225795067923));
#14526=CARTESIAN_POINT('Ctrl Pts',(86.0012125410497,5.8432374289237,334.0702113618));
#14527=CARTESIAN_POINT('Ctrl Pts',(85.9938116745239,5.81847191416096,333.914572997485));
#14528=CARTESIAN_POINT('Ctrl Pts',(85.9864108079982,5.78749411739314,333.759989408423));
#14529=CARTESIAN_POINT('Ctrl Pts',(85.9790099414724,5.75042973059065,333.60698583064));
#14530=CARTESIAN_POINT('Ctrl Pts',(85.9716009480876,5.71332464354791,333.4538142403));
#14531=CARTESIAN_POINT('Ctrl Pts',(85.9641919547029,5.67011970676866,333.30222648907));
#14532=CARTESIAN_POINT('Ctrl Pts',(85.9567829613181,5.62099073959442,333.152733460517));
#14533=CARTESIAN_POINT('Ctrl Pts',(85.9493694037379,5.57183150728205,333.003148339102));
#14534=CARTESIAN_POINT('Ctrl Pts',(85.9419558461577,5.51674110293494,332.855660860501));
#14535=CARTESIAN_POINT('Ctrl Pts',(85.9345422885775,5.45594335021597,332.710761541094));
#14536=CARTESIAN_POINT('Ctrl Pts',(85.9271181764409,5.39505904076532,332.565655930978));
#14537=CARTESIAN_POINT('Ctrl Pts',(85.9196940643042,5.32845131238363,332.42314617637));
#14538=CARTESIAN_POINT('Ctrl Pts',(85.9122699521675,5.25639011501967,332.283698558476));
#14539=CARTESIAN_POINT('Ctrl Pts',(85.9084128270127,5.21895142175617,332.211249906725));
#14540=CARTESIAN_POINT('Ctrl Pts',(85.9045557018579,5.18004144084578,332.139627330889));
#14541=CARTESIAN_POINT('Ctrl Pts',(85.900698576703,5.1397025483473,332.068892994616));
#14542=CARTESIAN_POINT('Ctrl Pts',(85.893274599265,5.06206051814006,331.932747524736));
#14543=CARTESIAN_POINT('Ctrl Pts',(85.885850621827,4.97888809376132,331.799483790245));
#14544=CARTESIAN_POINT('Ctrl Pts',(85.878426644389,4.89042446399098,331.669582740181));
#14545=CARTESIAN_POINT('Ctrl Pts',(85.8710114283614,4.80206523461385,331.539834992901));
#14546=CARTESIAN_POINT('Ctrl Pts',(85.8635962123337,4.70842743748956,331.413442336211));
#14547=CARTESIAN_POINT('Ctrl Pts',(85.8561809963061,4.60979614613365,331.290861278734));
#14548=CARTESIAN_POINT('Ctrl Pts',(85.848772915162,4.51125975731002,331.168398168134));
#14549=CARTESIAN_POINT('Ctrl Pts',(85.8413648340179,4.40773967194467,331.049739644264));
#14550=CARTESIAN_POINT('Ctrl Pts',(85.8339567528738,4.29956419507076,330.935313259922));
#14551=CARTESIAN_POINT('Ctrl Pts',(85.8265541856997,4.19146923517896,330.820972045226));
#14552=CARTESIAN_POINT('Ctrl Pts',(85.8191516185257,4.07872603857352,330.710856967875));
#14553=CARTESIAN_POINT('Ctrl Pts',(85.8117490513516,3.96170303900783,330.605362404792));
#14554=CARTESIAN_POINT('Ctrl Pts',(85.8043503815968,3.84474165154055,330.499923384136));
#14555=CARTESIAN_POINT('Ctrl Pts',(85.7969517118421,3.72350522519156,330.399100282185));
#14556=CARTESIAN_POINT('Ctrl Pts',(85.7895530420873,3.59839880307863,330.303250420078));
#14557=CARTESIAN_POINT('Ctrl Pts',(85.7821555928833,3.47331301964068,330.207416370221));
#14558=CARTESIAN_POINT('Ctrl Pts',(85.7747581436793,3.34435880348351,330.116554158676));
#14559=CARTESIAN_POINT('Ctrl Pts',(85.7673606944754,3.21197409963915,330.030980685714));
#14560=CARTESIAN_POINT('Ctrl Pts',(85.7599635660119,3.07959513576494,329.945410923069));
#14561=CARTESIAN_POINT('Ctrl Pts',(85.7525664375484,2.94378629337883,329.865129645665));
#14562=CARTESIAN_POINT('Ctrl Pts',(85.7451693090849,2.80501407509356,329.790410131207));
#14563=CARTESIAN_POINT('Ctrl Pts',(85.7377710416483,2.6662204893507,329.715679111809));
#14564=CARTESIAN_POINT('Ctrl Pts',(85.7303727742117,2.52446294780906,329.64651173745));
#14565=CARTESIAN_POINT('Ctrl Pts',(85.7229745067751,2.38023195563828,329.583135002618));
#14566=CARTESIAN_POINT('Ctrl Pts',(85.7155736402494,2.23595029360381,329.519736002873));
#14567=CARTESIAN_POINT('Ctrl Pts',(85.7081727737236,2.08919379232855,329.462131843012));
#14568=CARTESIAN_POINT('Ctrl Pts',(85.7007719071979,1.94047215312956,329.410501061327));
#14569=CARTESIAN_POINT('Ctrl Pts',(85.6933629138131,1.79158720335175,329.358813584107));
#14570=CARTESIAN_POINT('Ctrl Pts',(85.6859539204284,1.64073315896957,329.313112706888));
#14571=CARTESIAN_POINT('Ctrl Pts',(85.6785449270436,1.48843477880754,329.273527047847));
#14572=CARTESIAN_POINT('Ctrl Pts',(85.6711313694633,1.33604257758979,329.233917002675));
#14573=CARTESIAN_POINT('Ctrl Pts',(85.663717811883,1.18220463144588,329.200429761492));
#14574=CARTESIAN_POINT('Ctrl Pts',(85.6563042543028,1.02745454989345,329.173142552765));
#14575=CARTESIAN_POINT('Ctrl Pts',(85.6488801421661,0.872484153269253,329.1458164957));
#14576=CARTESIAN_POINT('Ctrl Pts',(85.6414560300294,0.71659939652762,329.124708150083));
#14577=CARTESIAN_POINT('Ctrl Pts',(85.6340319178927,0.560338470891678,329.109842840761));
#14578=CARTESIAN_POINT('Ctrl Pts',(85.6301747927382,0.479154628859491,329.102119714081));
#14579=CARTESIAN_POINT('Ctrl Pts',(85.6263176675837,0.397869253520564,329.09608086165));
#14580=CARTESIAN_POINT('Ctrl Pts',(85.6224605424292,0.316557551728029,329.091724288852));
#14581=CARTESIAN_POINT('Ctrl Pts',(85.6150365649912,0.160053363926919,329.083339002696));
#14582=CARTESIAN_POINT('Ctrl Pts',(85.6076125875532,0.00297967527304754,
329.081163815357));
#14583=CARTESIAN_POINT('Ctrl Pts',(85.6001886101152,-0.154129635153365,
329.08525785701));
#14584=CARTESIAN_POINT('Ctrl Pts',(85.5927733940876,-0.311053532954991,
329.089347067077));
#14585=CARTESIAN_POINT('Ctrl Pts',(85.58535817806,-0.468012599393245,329.099690769409));
#14586=CARTESIAN_POINT('Ctrl Pts',(85.5779429620324,-0.624468676991852,
329.116296282616));
#14587=CARTESIAN_POINT('Ctrl Pts',(85.5705348808883,-0.780774213340468,
329.132885818082));
#14588=CARTESIAN_POINT('Ctrl Pts',(85.5631267997443,-0.936577355703673,
329.155725130479));
#14589=CARTESIAN_POINT('Ctrl Pts',(85.5557187186002,-1.09134090112104,329.184769514453));
#14590=CARTESIAN_POINT('Ctrl Pts',(85.5483161514262,-1.2459892532048,329.213792280161));
#14591=CARTESIAN_POINT('Ctrl Pts',(85.5409135842522,-1.39959918383672,329.249010852699));
#14592=CARTESIAN_POINT('Ctrl Pts',(85.5335110170782,-1.5516396724024,329.290328828249));
#14593=CARTESIAN_POINT('Ctrl Pts',(85.5261123473235,-1.70360011231513,329.331625050065));
#14594=CARTESIAN_POINT('Ctrl Pts',(85.5187136775688,-1.85399239655353,329.379014181752));
#14595=CARTESIAN_POINT('Ctrl Pts',(85.5113150078141,-2.00229685407605,329.432348980885));
#14596=CARTESIAN_POINT('Ctrl Pts',(85.5039175586101,-2.15057684596881,329.485674981431));
#14597=CARTESIAN_POINT('Ctrl Pts',(85.4965201094061,-2.29676934387149,329.544944576575));
#14598=CARTESIAN_POINT('Ctrl Pts',(85.4891226602022,-2.44037086239749,329.609960981917));
#14599=CARTESIAN_POINT('Ctrl Pts',(85.4817255317387,-2.583966154612,329.67497456826));
#14600=CARTESIAN_POINT('Ctrl Pts',(85.4743284032753,-2.72497035083156,329.745734315435));
#14601=CARTESIAN_POINT('Ctrl Pts',(85.4669312748118,-2.86290119467269,329.821995817688));
#14602=CARTESIAN_POINT('Ctrl Pts',(85.4595330073752,-3.00085327642105,329.898269062309));
#14603=CARTESIAN_POINT('Ctrl Pts',(85.4521347399386,-3.13573073691531,329.980045568166));
#14604=CARTESIAN_POINT('Ctrl Pts',(85.4447364725019,-3.26707725115514,330.067035698742));
#14605=CARTESIAN_POINT('Ctrl Pts',(85.4373356059762,-3.39846990880614,330.154056389865));
#14606=CARTESIAN_POINT('Ctrl Pts',(85.4299347394505,-3.52632883949095,330.246294146473));
#14607=CARTESIAN_POINT('Ctrl Pts',(85.4225338729247,-3.65022807792137,330.343416967168));
#14608=CARTESIAN_POINT('Ctrl Pts',(85.41512487954,-3.7742633695609,330.440646438007));
#14609=CARTESIAN_POINT('Ctrl Pts',(85.4077158861552,-3.89432999161803,330.542771455278));
#14610=CARTESIAN_POINT('Ctrl Pts',(85.4003068927705,-4.0100358092131,330.649420340767));
#14611=CARTESIAN_POINT('Ctrl Pts',(85.3928933351902,-4.12581290558276,330.756134925649));
#14612=CARTESIAN_POINT('Ctrl Pts',(85.3854797776101,-4.23722358099036,330.867378668847));
#14613=CARTESIAN_POINT('Ctrl Pts',(85.3780662200298,-4.34391412564184,330.98274463949));
#14614=CARTESIAN_POINT('Ctrl Pts',(85.3706421078932,-4.45075656381594,331.098274854712));
#14615=CARTESIAN_POINT('Ctrl Pts',(85.3632179957565,-4.55286520851005,331.217938735301));
#14616=CARTESIAN_POINT('Ctrl Pts',(85.3557938836198,-4.64992751736846,331.341297409502));
#14617=CARTESIAN_POINT('Ctrl Pts',(85.351936758465,-4.7003552946154,331.405387207254));
#14618=CARTESIAN_POINT('Ctrl Pts',(85.3480796333101,-4.74942167521198,331.47047384397));
#14619=CARTESIAN_POINT('Ctrl Pts',(85.3442225081553,-4.79708763772977,331.536492997201));
#14620=CARTESIAN_POINT('Ctrl Pts',(85.3367393826128,-4.88956334627111,331.66457533625));
#14621=CARTESIAN_POINT('Ctrl Pts',(85.3292562570703,-4.97704343511309,331.796554376371));
#14622=CARTESIAN_POINT('Ctrl Pts',(85.3217731315277,-5.05918476797303,331.932007163305));
#14623=CARTESIAN_POINT('Ctrl Pts',(85.3142990850663,-5.14122644089619,332.067295608906));
#14624=CARTESIAN_POINT('Ctrl Pts',(85.3068250386048,-5.21794206427955,332.206049102698));
#14625=CARTESIAN_POINT('Ctrl Pts',(85.2993509921433,-5.28902964290597,332.347812978133));
#14626=CARTESIAN_POINT('Ctrl Pts',(85.2918846182601,-5.3600442456667,332.489431324043));
#14627=CARTESIAN_POINT('Ctrl Pts',(85.2844182443769,-5.4254421437923,332.63405357482));
#14628=CARTESIAN_POINT('Ctrl Pts',(85.2769518704937,-5.48496547831313,332.781197560797));
#14629=CARTESIAN_POINT('Ctrl Pts',(85.2694917677292,-5.54443881829795,332.928217958347));
#14630=CARTESIAN_POINT('Ctrl Pts',(85.2620316649647,-5.59804728371563,333.077755536417));
#14631=CARTESIAN_POINT('Ctrl Pts',(85.2545715622002,-5.64557970362559,333.229305115919));
#14632=CARTESIAN_POINT('Ctrl Pts',(85.2471167580928,-5.6930783628758,333.380747054913));
#14633=CARTESIAN_POINT('Ctrl Pts',(85.2396619539853,-5.73450946622863,333.534197800506));
#14634=CARTESIAN_POINT('Ctrl Pts',(85.2322071498779,-5.76971063860679,333.689133985013));
#14635=CARTESIAN_POINT('Ctrl Pts',(85.2247555166807,-5.80489683812204,333.844004267219));
#14636=CARTESIAN_POINT('Ctrl Pts',(85.2173038834836,-5.83385830372132,334.000358374298));
#14637=CARTESIAN_POINT('Ctrl Pts',(85.2098522502864,-5.85648299479626,334.157659514114));
#14638=CARTESIAN_POINT('Ctrl Pts',(85.2024015160298,-5.87910495650304,334.314941677639));
#14639=CARTESIAN_POINT('Ctrl Pts',(85.1949507817731,-5.89539160873179,334.473170285755));
#14640=CARTESIAN_POINT('Ctrl Pts',(85.1875000475164,-5.90528232234687,334.631799978439));
#14641=CARTESIAN_POINT('Ctrl Pts',(85.1816840332455,-5.91300297504414,334.755625701471));
#14642=CARTESIAN_POINT('Ctrl Pts',(85.1758680189745,-5.91682740891254,334.87969558763));
#14643=CARTESIAN_POINT('Ctrl Pts',(85.1700520047035,-5.91674881247257,335.003748680365));
#14644=CARTESIAN_POINT('',(83.4200520047036,-5.92472559629233,335.002923715034));
#14645=CARTESIAN_POINT('Ctrl Pts',(85.1700498850932,-5.90944875995897,335.003789209877));
#14646=CARTESIAN_POINT('Ctrl Pts',(85.1353614146893,-5.91370990462514,335.742769459017));
#14647=CARTESIAN_POINT('Ctrl Pts',(85.0079269328602,-5.44210307607092,338.452296737771));
#14648=CARTESIAN_POINT('Ctrl Pts',(84.7877464396077,-1.37745943898813,341.859681363963));
#14649=CARTESIAN_POINT('Ctrl Pts',(84.5095084053333,5.02303006280172,339.870502223532));
#14650=CARTESIAN_POINT('Ctrl Pts',(84.2312703710595,6.81395901576062,333.411735081052));
#14651=CARTESIAN_POINT('Ctrl Pts',(83.9530323367856,2.35181835382513,328.410495211943));
#14652=CARTESIAN_POINT('Ctrl Pts',(83.6826262146669,-4.08219951646664,329.426907744826));
#14653=CARTESIAN_POINT('Ctrl Pts',(83.5049661039729,-5.91383814749851,333.205903189172));
#14654=CARTESIAN_POINT('Ctrl Pts',(83.4200520047036,-5.92472559629233,335.002923715034));
#14655=CARTESIAN_POINT('',(81.6700520047036,-5.91801367655859,334.994687890905));
#14656=CARTESIAN_POINT('Ctrl Pts',(83.4200520047036,-5.92472559629233,335.002923715034));
#14657=CARTESIAN_POINT('Ctrl Pts',(83.4122200925483,-5.92572978220824,335.168668944872));
#14658=CARTESIAN_POINT('Ctrl Pts',(83.404388180393,-5.91937917051338,335.334336070522));
#14659=CARTESIAN_POINT('Ctrl Pts',(83.303810256813,-5.74017621052549,337.453586964006));
#14660=CARTESIAN_POINT('Ctrl Pts',(83.1183182339638,-3.27705977547671,341.181707057858));
#14661=CARTESIAN_POINT('Ctrl Pts',(82.8400801996897,3.42492426372844,341.101025873486));
#14662=CARTESIAN_POINT('Ctrl Pts',(82.5618421654159,6.98390585790928,335.42152329601));
#14663=CARTESIAN_POINT('Ctrl Pts',(82.2836041311419,4.13386012856826,329.35519501146));
#14664=CARTESIAN_POINT('Ctrl Pts',(82.0053660968678,-2.50976802508626,328.469020947708));
#14665=CARTESIAN_POINT('Ctrl Pts',(81.8008487213886,-5.70019332344303,332.223047555137));
#14666=CARTESIAN_POINT('Ctrl Pts',(81.6890773573338,-5.92214175837517,334.590937491054));
#14667=CARTESIAN_POINT('Ctrl Pts',(81.6700520047036,-5.9184019942076,334.994687542344));
#14668=CARTESIAN_POINT('',(79.9200520047356,-5.91674999747214,334.99982704509));
#14669=CARTESIAN_POINT('Ctrl Pts',(81.6700520047036,-5.91674761639107,334.994689027342));
#14670=CARTESIAN_POINT('Ctrl Pts',(81.662747770902,-5.91688671416704,335.149652437497));
#14671=CARTESIAN_POINT('Ctrl Pts',(81.6554435371003,-5.91093377111608,335.304809948067));
#14672=CARTESIAN_POINT('Ctrl Pts',(81.6481393032986,-5.89886984741152,335.459635818664));
#14673=CARTESIAN_POINT('Ctrl Pts',(81.6408408138345,-5.88681541125234,335.614339928091));
#14674=CARTESIAN_POINT('Ctrl Pts',(81.6335423243703,-5.86865958823044,335.768712534865));
#14675=CARTESIAN_POINT('Ctrl Pts',(81.6262438349062,-5.84443550203431,335.922227859621));
#14676=CARTESIAN_POINT('Ctrl Pts',(81.6188540929651,-5.81990854387023,336.077662575191));
#14677=CARTESIAN_POINT('Ctrl Pts',(81.6114643510241,-5.7891605465858,336.232218026418));
#14678=CARTESIAN_POINT('Ctrl Pts',(81.604074609083,-5.75228016881055,336.385353175912));
#14679=CARTESIAN_POINT('Ctrl Pts',(81.5967815438203,-5.71588228047122,336.536484926949));
#14680=CARTESIAN_POINT('Ctrl Pts',(81.5894884785576,-5.67351160277635,336.686232932781));
#14681=CARTESIAN_POINT('Ctrl Pts',(81.5821954132949,-5.62530478166383,336.834087423186));
#14682=CARTESIAN_POINT('Ctrl Pts',(81.5749026303751,-5.57709982682531,336.981936189567));
#14683=CARTESIAN_POINT('Ctrl Pts',(81.5676098474554,-5.52305929713086,337.127891220378));
#14684=CARTESIAN_POINT('Ctrl Pts',(81.5603170645357,-5.46336948475028,337.271458658131));
#14685=CARTESIAN_POINT('Ctrl Pts',(81.5530230288349,-5.40366941863425,337.415050758427));
#14686=CARTESIAN_POINT('Ctrl Pts',(81.5457289931341,-5.33831828692846,337.556254094363));
#14687=CARTESIAN_POINT('Ctrl Pts',(81.5384349574334,-5.26755009681816,337.694595802715));
#14688=CARTESIAN_POINT('Ctrl Pts',(81.5309728800073,-5.19515153235098,337.836124660173));
#14689=CARTESIAN_POINT('Ctrl Pts',(81.5235108025811,-5.11708346993486,337.974658054906));
#14690=CARTESIAN_POINT('Ctrl Pts',(81.516048725155,-5.03364509571469,338.109718252975));
#14691=CARTESIAN_POINT('Ctrl Pts',(81.5087438989445,-4.95196505031146,338.241932275763));
#14692=CARTESIAN_POINT('Ctrl Pts',(81.501439072734,-4.86513904868359,338.370817744346));
#14693=CARTESIAN_POINT('Ctrl Pts',(81.4941342465235,-4.77349003294312,338.495958161634));
#14694=CARTESIAN_POINT('Ctrl Pts',(81.4865935434896,-4.67888162048663,338.625139431264));
#14695=CARTESIAN_POINT('Ctrl Pts',(81.4790528404557,-4.57913377475567,338.750329374966));
#14696=CARTESIAN_POINT('Ctrl Pts',(81.4715121374218,-4.47464411467867,338.871109738753));
#14697=CARTESIAN_POINT('Ctrl Pts',(81.4639714343879,-4.37015445460175,338.991890102541));
#14698=CARTESIAN_POINT('Ctrl Pts',(81.4564307313539,-4.2609233356176,339.108260612671));
#14699=CARTESIAN_POINT('Ctrl Pts',(81.44889002832,-4.14738639006992,339.219847946782));
#14700=CARTESIAN_POINT('Ctrl Pts',(81.441466050882,-4.03560692887947,339.329707975361));
#14701=CARTESIAN_POINT('Ctrl Pts',(81.434042073444,-3.91929070850586,339.435289280455));
#14702=CARTESIAN_POINT('Ctrl Pts',(81.426618096006,-3.79879883789278,339.536194214507));
#14703=CARTESIAN_POINT('Ctrl Pts',(81.4192028799784,-3.67844916581601,339.636980065554));
#14704=CARTESIAN_POINT('Ctrl Pts',(81.4117876639508,-3.55393393590162,339.733100293574));
#14705=CARTESIAN_POINT('Ctrl Pts',(81.4043724479231,-3.42565175318212,339.824193261927));
#14706=CARTESIAN_POINT('Ctrl Pts',(81.396964366779,-3.29749300293311,339.915198581084));
#14707=CARTESIAN_POINT('Ctrl Pts',(81.3895562856349,-3.16557481793074,340.001186055908));
#14708=CARTESIAN_POINT('Ctrl Pts',(81.3821482044908,-3.0303295168267,340.081833683027));
#14709=CARTESIAN_POINT('Ctrl Pts',(81.3747456373168,-2.89518488126986,340.162421282644));
#14710=CARTESIAN_POINT('Ctrl Pts',(81.3673430701428,-2.75671837972484,340.23767675813));
#14711=CARTESIAN_POINT('Ctrl Pts',(81.3599405029688,-2.61539190982473,340.307320955108));
#14712=CARTESIAN_POINT('Ctrl Pts',(81.3525418332141,-2.47413984769425,340.376928484719));
#14713=CARTESIAN_POINT('Ctrl Pts',(81.3451431634593,-2.33003114994793,340.440930454958));
#14714=CARTESIAN_POINT('Ctrl Pts',(81.3377444937046,-2.1835528503593,340.499093335468));
#14715=CARTESIAN_POINT('Ctrl Pts',(81.3303470445007,-2.03709871514119,340.557246620909));
#14716=CARTESIAN_POINT('Ctrl Pts',(81.3229495952967,-1.88827610044171,340.609562590799));
#14717=CARTESIAN_POINT('Ctrl Pts',(81.3155521460927,-1.73759269253072,340.65585556723));
#14718=CARTESIAN_POINT('Ctrl Pts',(81.3081550176293,-1.58691581798949,340.702146536478));
#14719=CARTESIAN_POINT('Ctrl Pts',(81.3007578891658,-1.43437866741149,340.742414921911));
#14720=CARTESIAN_POINT('Ctrl Pts',(81.2933607607023,-1.28050452758628,340.776524795873));
#14721=CARTESIAN_POINT('Ctrl Pts',(81.2859624932657,-1.12660669498486,340.810639921903));
#14722=CARTESIAN_POINT('Ctrl Pts',(81.2785642258291,-0.971371827624401,
340.838594567584));
#14723=CARTESIAN_POINT('Ctrl Pts',(81.2711659583925,-0.815333705432265,
340.860303875337));
#14724=CARTESIAN_POINT('Ctrl Pts',(81.2637650918667,-0.659240765406648,
340.882020809798));
#14725=CARTESIAN_POINT('Ctrl Pts',(81.256364225341,-0.50234437812377,340.89748798658));
#14726=CARTESIAN_POINT('Ctrl Pts',(81.2489633588152,-0.345183600167206,
340.906672400318));
#14727=CARTESIAN_POINT('Ctrl Pts',(81.2415543654305,-0.187850244651283,
340.91586689942));
#14728=CARTESIAN_POINT('Ctrl Pts',(81.2341453720458,-0.0302522914625299,
340.918764835873));
#14729=CARTESIAN_POINT('Ctrl Pts',(81.226736378661,0.127070307032321,340.915385338215));
#14730=CARTESIAN_POINT('Ctrl Pts',(81.2193228210808,0.284489821674369,340.91200375867));
#14731=CARTESIAN_POINT('Ctrl Pts',(81.2119092635005,0.441633271979515,340.902337062137));
#14732=CARTESIAN_POINT('Ctrl Pts',(81.2044957059203,0.597966182245034,340.88645623507));
#14733=CARTESIAN_POINT('Ctrl Pts',(81.1970715937836,0.754521661028995,340.870552798737));
#14734=CARTESIAN_POINT('Ctrl Pts',(81.189647481647,0.910263926598655,340.848417615111));
#14735=CARTESIAN_POINT('Ctrl Pts',(81.1822233695103,1.06466822753262,340.820172860645));
#14736=CARTESIAN_POINT('Ctrl Pts',(81.1783662443556,1.14488747828769,340.805498573547));
#14737=CARTESIAN_POINT('Ctrl Pts',(81.1745091192008,1.22474581389733,340.789176005825));
#14738=CARTESIAN_POINT('Ctrl Pts',(81.1706519940461,1.3041714123094,340.771227554846));
#14739=CARTESIAN_POINT('Ctrl Pts',(81.1632280166081,1.45704533445618,340.736681386452));
#14740=CARTESIAN_POINT('Ctrl Pts',(81.1558040391702,1.6087762874556,340.696004697682));
#14741=CARTESIAN_POINT('Ctrl Pts',(81.1483800617322,1.75883446422273,340.649285962842));
#14742=CARTESIAN_POINT('Ctrl Pts',(81.1409648457046,1.9087155497638,340.602622363138));
#14743=CARTESIAN_POINT('Ctrl Pts',(81.133549629677,2.05692743572992,340.549931020646));
#14744=CARTESIAN_POINT('Ctrl Pts',(81.1261344136493,2.2029503061003,340.491351428506));
#14745=CARTESIAN_POINT('Ctrl Pts',(81.1187263325052,2.34883267400025,340.432828201354));
#14746=CARTESIAN_POINT('Ctrl Pts',(81.1113182513611,2.49252987541165,340.368428141822));
#14747=CARTESIAN_POINT('Ctrl Pts',(81.103910170217,2.63353717839881,340.298340541386));
#14748=CARTESIAN_POINT('Ctrl Pts',(81.0965076030431,2.77443952707464,340.22830510843));
#14749=CARTESIAN_POINT('Ctrl Pts',(81.089105035869,2.91265563110731,340.152590729172));
#14750=CARTESIAN_POINT('Ctrl Pts',(81.081702468695,3.04770078431308,340.071434756733));
#14751=CARTESIAN_POINT('Ctrl Pts',(81.0743037989403,3.18267483683686,339.990321512558));
#14752=CARTESIAN_POINT('Ctrl Pts',(81.0669051291855,3.31448094433997,339.903772572727));
#14753=CARTESIAN_POINT('Ctrl Pts',(81.0595064594307,3.44265916424283,339.812071117653));
#14754=CARTESIAN_POINT('Ctrl Pts',(81.0521090102268,3.570816238719,339.720384790473));
#14755=CARTESIAN_POINT('Ctrl Pts',(81.0447115610228,3.69534631016562,339.623547851978));
#14756=CARTESIAN_POINT('Ctrl Pts',(81.0373141118188,3.81581849989679,339.521886745413));
#14757=CARTESIAN_POINT('Ctrl Pts',(81.0299169833553,3.93628546616384,339.420230046697));
#14758=CARTESIAN_POINT('Ctrl Pts',(81.0225198548918,4.05269461532006,339.313749836495));
#14759=CARTESIAN_POINT('Ctrl Pts',(81.0151227264284,4.16464846239253,339.20281259958));
#14760=CARTESIAN_POINT('Ctrl Pts',(81.0077244589917,4.27661954756302,339.0918582811));
#14761=CARTESIAN_POINT('Ctrl Pts',(81.0003261915551,4.38413369960563,338.97644583216));
#14762=CARTESIAN_POINT('Ctrl Pts',(80.9929279241185,4.48683070102693,338.856978198386));
#14763=CARTESIAN_POINT('Ctrl Pts',(80.9855270575927,4.58956378098481,338.737468594375));
#14764=CARTESIAN_POINT('Ctrl Pts',(80.978126191067,4.68747609779013,338.613901251934));
#14765=CARTESIAN_POINT('Ctrl Pts',(80.9707253245412,4.78024818207935,338.486711614147));
#14766=CARTESIAN_POINT('Ctrl Pts',(80.9633163311564,4.87312213898621,338.359382309978));
#14767=CARTESIAN_POINT('Ctrl Pts',(80.9559073377717,4.96084437101275,338.228423068635));
#14768=CARTESIAN_POINT('Ctrl Pts',(80.9484983443869,5.04313876454832,338.094298299132));
#14769=CARTESIAN_POINT('Ctrl Pts',(80.9410847868067,5.12548385426883,337.960090904145));
#14770=CARTESIAN_POINT('Ctrl Pts',(80.9336712292265,5.20239426077343,337.822714420106));
#14771=CARTESIAN_POINT('Ctrl Pts',(80.9262576716462,5.27364044261458,337.682656713879));
#14772=CARTESIAN_POINT('Ctrl Pts',(80.9188335595096,5.34498805643899,337.542399609866));
#14773=CARTESIAN_POINT('Ctrl Pts',(80.9114094473729,5.41065518468264,337.399453998156));
#14774=CARTESIAN_POINT('Ctrl Pts',(80.9039853352362,5.47046059502883,337.254327270105));
#14775=CARTESIAN_POINT('Ctrl Pts',(80.9001282100816,5.5015319135085,337.178928091985));
#14776=CARTESIAN_POINT('Ctrl Pts',(80.896271084927,5.53102184575222,337.102940435887));
#14777=CARTESIAN_POINT('Ctrl Pts',(80.8924139597724,5.55891035915082,337.026436819007));
#14778=CARTESIAN_POINT('Ctrl Pts',(80.8849899823343,5.61258860031539,336.879186962474));
#14779=CARTESIAN_POINT('Ctrl Pts',(80.8775660048964,5.66049302991841,336.729580676738));
#14780=CARTESIAN_POINT('Ctrl Pts',(80.8701420274583,5.7024113388756,336.578111366401));
#14781=CARTESIAN_POINT('Ctrl Pts',(80.8627268114307,5.74428017792118,336.42682081264));
#14782=CARTESIAN_POINT('Ctrl Pts',(80.8553115954031,5.78017685979185,336.273671966918));
#14783=CARTESIAN_POINT('Ctrl Pts',(80.8478963793755,5.80993738496833,336.119177441359));
#14784=CARTESIAN_POINT('Ctrl Pts',(80.8404882982314,5.83966927471737,335.964831569655));
#14785=CARTESIAN_POINT('Ctrl Pts',(80.8330802170873,5.86327669176948,335.809142959855));
#14786=CARTESIAN_POINT('Ctrl Pts',(80.8256721359432,5.88064567595252,335.652638488293));
#14787=CARTESIAN_POINT('Ctrl Pts',(80.8182695687692,5.89800173208338,335.496250505867));
#14788=CARTESIAN_POINT('Ctrl Pts',(80.8108670015952,5.90912855999987,335.339048240168));
#14789=CARTESIAN_POINT('Ctrl Pts',(80.8034644344212,5.91396345267819,335.181567736359));
#14790=CARTESIAN_POINT('Ctrl Pts',(80.7960657646664,5.91879579980669,335.024170145347));
#14791=CARTESIAN_POINT('Ctrl Pts',(80.7886670949116,5.91734279766458,334.866494980067));
#14792=CARTESIAN_POINT('Ctrl Pts',(80.7812684251568,5.9095936773828,334.709082261219));
#14793=CARTESIAN_POINT('Ctrl Pts',(80.7738709759528,5.9018458354653,334.551695510584));
#14794=CARTESIAN_POINT('Ctrl Pts',(80.7664735267488,5.88780395515307,334.39457149285));
#14795=CARTESIAN_POINT('Ctrl Pts',(80.7590760775448,5.86750937635446,334.238249200268));
#14796=CARTESIAN_POINT('Ctrl Pts',(80.7516789490813,5.8472156774934,334.081933685548));
#14797=CARTESIAN_POINT('Ctrl Pts',(80.7442818206178,5.82066986724324,333.926420196969));
#14798=CARTESIAN_POINT('Ctrl Pts',(80.7368846921543,5.78796502854048,333.772241314064));
#14799=CARTESIAN_POINT('Ctrl Pts',(80.7294864247177,5.75525515410893,333.618038691458));
#14800=CARTESIAN_POINT('Ctrl Pts',(80.7220881572811,5.71638444040983,333.465171448806));
#14801=CARTESIAN_POINT('Ctrl Pts',(80.7146898898445,5.67149679866059,333.31416055768));
#14802=CARTESIAN_POINT('Ctrl Pts',(80.7072890233187,5.62659338741082,333.16309661484));
#14803=CARTESIAN_POINT('Ctrl Pts',(80.6998881567929,5.57566894578945,333.013890679483));
#14804=CARTESIAN_POINT('Ctrl Pts',(80.6924872902672,5.51891676397256,332.867047043453));
#14805=CARTESIAN_POINT('Ctrl Pts',(80.6850782968824,5.46210226283423,332.720042159071));
#14806=CARTESIAN_POINT('Ctrl Pts',(80.6776693034977,5.39944737614575,332.575405102757));
#14807=CARTESIAN_POINT('Ctrl Pts',(80.6702603101129,5.33119321443762,332.433619382704));
#14808=CARTESIAN_POINT('Ctrl Pts',(80.6628467525326,5.26289700581145,332.291746317755));
#14809=CARTESIAN_POINT('Ctrl Pts',(80.6554331949523,5.18899482366178,332.152728417939));
#14810=CARTESIAN_POINT('Ctrl Pts',(80.6480196373721,5.10977270759461,332.017022722309));
#14811=CARTESIAN_POINT('Ctrl Pts',(80.6405955252354,5.03043780434191,331.881123824777));
#14812=CARTESIAN_POINT('Ctrl Pts',(80.6331714130987,4.94576804091561,331.748546862977));
#14813=CARTESIAN_POINT('Ctrl Pts',(80.625747300962,4.85609201832578,331.619718817605));
#14814=CARTESIAN_POINT('Ctrl Pts',(80.6218901758074,4.80950171417569,331.552787461334));
#14815=CARTESIAN_POINT('Ctrl Pts',(80.6180330506528,4.76156076750666,331.486867467286));
#14816=CARTESIAN_POINT('Ctrl Pts',(80.6141759254982,4.71231931878221,331.422014924524));
#14817=CARTESIAN_POINT('Ctrl Pts',(80.6067519480602,4.61754214933732,331.297190399789));
#14818=CARTESIAN_POINT('Ctrl Pts',(80.5993279706223,4.51765886756541,331.175945997321));
#14819=CARTESIAN_POINT('Ctrl Pts',(80.5919039931843,4.41296949529584,331.0587272619));
#14820=CARTESIAN_POINT('Ctrl Pts',(80.5844887771566,4.30840367223699,330.941646862224));
#14821=CARTESIAN_POINT('Ctrl Pts',(80.577073561129,4.19904329489378,330.828582948518));
#14822=CARTESIAN_POINT('Ctrl Pts',(80.5696583451014,4.08523068018667,330.71995083531));
#14823=CARTESIAN_POINT('Ctrl Pts',(80.5622502639573,3.97152757540421,330.611423247375));
#14824=CARTESIAN_POINT('Ctrl Pts',(80.5548421828132,3.85338102991335,330.50731922656));
#14825=CARTESIAN_POINT('Ctrl Pts',(80.5474341016691,3.73117243487341,330.408019727423));
#14826=CARTESIAN_POINT('Ctrl Pts',(80.5400315344951,3.60905480192282,330.308794138716));
#14827=CARTESIAN_POINT('Ctrl Pts',(80.5326289673211,3.48288142797572,330.214366185506));
#14828=CARTESIAN_POINT('Ctrl Pts',(80.5252264001471,3.35306915047842,330.125078684265));
#14829=CARTESIAN_POINT('Ctrl Pts',(80.5178277303924,3.22332521857768,330.035838192503));
#14830=CARTESIAN_POINT('Ctrl Pts',(80.5104290606376,3.08994650541052,329.951732973671));
#14831=CARTESIAN_POINT('Ctrl Pts',(80.5030303908828,2.95338129825054,329.873064319728));
#14832=CARTESIAN_POINT('Ctrl Pts',(80.4956329416788,2.81683862010928,329.794408643671));
#14833=CARTESIAN_POINT('Ctrl Pts',(80.4882354924749,2.67711081434308,329.721187938625));
#14834=CARTESIAN_POINT('Ctrl Pts',(80.4808380432709,2.53467350243085,329.653659120616));
#14835=CARTESIAN_POINT('Ctrl Pts',(80.4734409148075,2.39224236635234,329.586133230538));
#14836=CARTESIAN_POINT('Ctrl Pts',(80.466043786344,2.24710229494725,329.524298896675));
#14837=CARTESIAN_POINT('Ctrl Pts',(80.4586466578805,2.09975151822453,329.468366052945));
#14838=CARTESIAN_POINT('Ctrl Pts',(80.4512483904439,1.95237805316047,329.412424596953));
#14839=CARTESIAN_POINT('Ctrl Pts',(80.4438501230074,1.80279355395116,329.362386572853));
#14840=CARTESIAN_POINT('Ctrl Pts',(80.4364518555708,1.65151399532478,329.318412890244));
#14841=CARTESIAN_POINT('Ctrl Pts',(80.429050989045,1.50018129059802,329.274423759218));
#14842=CARTESIAN_POINT('Ctrl Pts',(80.4216501225192,1.34715269898234,329.236503315546));
#14843=CARTESIAN_POINT('Ctrl Pts',(80.4142492559935,1.1929568906518,329.204761918649));
#14844=CARTESIAN_POINT('Ctrl Pts',(80.4068402626087,1.03859176058234,329.172985666662));
#14845=CARTESIAN_POINT('Ctrl Pts',(80.399431269224,0.883057219908353,329.147402087118));
#14846=CARTESIAN_POINT('Ctrl Pts',(80.3920222758392,0.726890339726405,329.128070079053));
#14847=CARTESIAN_POINT('Ctrl Pts',(80.384608718259,0.570627255359718,329.108726161804));
#14848=CARTESIAN_POINT('Ctrl Pts',(80.3771951606788,0.413731426320462,329.095641520972));
#14849=CARTESIAN_POINT('Ctrl Pts',(80.3697816030985,0.256741978943702,329.088822949805));
#14850=CARTESIAN_POINT('Ctrl Pts',(80.3623574909619,0.099529028347838,329.081994671155));
#14851=CARTESIAN_POINT('Ctrl Pts',(80.3549333788252,-0.0577774345755615,
329.081450280275));
#14852=CARTESIAN_POINT('Ctrl Pts',(80.3475092666885,-0.21464052778645,329.087144513323));
#14853=CARTESIAN_POINT('Ctrl Pts',(80.3436521415338,-0.296137220121997,
329.090102896644));
#14854=CARTESIAN_POINT('Ctrl Pts',(80.3397950163791,-0.377514346555329,
329.094744370205));
#14855=CARTESIAN_POINT('Ctrl Pts',(80.3359378912244,-0.458697606713513,
329.101057122832));
#14856=CARTESIAN_POINT('Ctrl Pts',(80.3285139137864,-0.614954577276633,
329.113207553836));
#14857=CARTESIAN_POINT('Ctrl Pts',(80.3210899363484,-0.770964157015842,
329.131589233217));
#14858=CARTESIAN_POINT('Ctrl Pts',(80.3136659589105,-0.926189318792645,
329.156190976062));
#14859=CARTESIAN_POINT('Ctrl Pts',(80.3062507428828,-1.08123129152422,329.18076368515));
#14860=CARTESIAN_POINT('Ctrl Pts',(80.2988355268552,-1.23549032395035,329.211541788247));
#14861=CARTESIAN_POINT('Ctrl Pts',(80.2914203108275,-1.38843192189614,329.248462174274));
#14862=CARTESIAN_POINT('Ctrl Pts',(80.2840122296834,-1.54122636020646,329.285347035691));
#14863=CARTESIAN_POINT('Ctrl Pts',(80.2766041485393,-1.69270552728362,329.32836232719));
#14864=CARTESIAN_POINT('Ctrl Pts',(80.2691960673952,-1.84234267767444,329.377393485178));
#14865=CARTESIAN_POINT('Ctrl Pts',(80.2617935002212,-1.99186845040183,329.426388148379));
#14866=CARTESIAN_POINT('Ctrl Pts',(80.2543909330472,-2.13955458325798,329.481389646566));
#14867=CARTESIAN_POINT('Ctrl Pts',(80.2469883658731,-2.28488721989842,329.5422329699));
#14868=CARTESIAN_POINT('Ctrl Pts',(80.2395896961184,-2.43014333954022,329.60304425949));
#14869=CARTESIAN_POINT('Ctrl Pts',(80.2321910263636,-2.57304808732545,329.669691105036));
#14870=CARTESIAN_POINT('Ctrl Pts',(80.2247923566089,-2.71310550645209,329.741959578573));
#14871=CARTESIAN_POINT('Ctrl Pts',(80.2173949074049,-2.85313982045348,329.814216130056));
#14872=CARTESIAN_POINT('Ctrl Pts',(80.2099974582009,-2.99032740670102,329.892092297984));
#14873=CARTESIAN_POINT('Ctrl Pts',(80.202600008997,-3.12419483295627,329.975327154109));
#14874=CARTESIAN_POINT('Ctrl Pts',(80.1952028805335,-3.25805645495331,330.058558401317));
#14875=CARTESIAN_POINT('Ctrl Pts',(80.18780575207,-3.38859788624905,330.147147677683));
#14876=CARTESIAN_POINT('Ctrl Pts',(80.1804086236066,-3.51537296808742,330.240789618252));
#14877=CARTESIAN_POINT('Ctrl Pts',(80.17301035617,-3.64216757012357,330.334445977342));
#14878=CARTESIAN_POINT('Ctrl Pts',(80.1656120887334,-3.76519436778241,330.43315632795));
#14879=CARTESIAN_POINT('Ctrl Pts',(80.1582138212968,-3.88403882521727,330.536573853338));
#14880=CARTESIAN_POINT('Ctrl Pts',(80.150812954771,-4.00292503396033,330.640027710391));
#14881=CARTESIAN_POINT('Ctrl Pts',(80.1434120882452,-4.11762569574288,330.748191789857));
#14882=CARTESIAN_POINT('Ctrl Pts',(80.1360112217195,-4.22776191320848,330.860681243523));
#14883=CARTESIAN_POINT('Ctrl Pts',(80.1286022283347,-4.33801907077005,330.973294221363));
#14884=CARTESIAN_POINT('Ctrl Pts',(80.12119323495,-4.44370151313924,331.090241791923));
#14885=CARTESIAN_POINT('Ctrl Pts',(80.1137842415652,-4.54446907087158,331.211104194308));
#14886=CARTESIAN_POINT('Ctrl Pts',(80.106370683985,-4.64529870489561,331.332041052102));
#14887=CARTESIAN_POINT('Ctrl Pts',(80.0989571264047,-4.74120719429455,331.456897252016));
#14888=CARTESIAN_POINT('Ctrl Pts',(80.0915435688244,-4.83189707428448,331.585223107431));
#14889=CARTESIAN_POINT('Ctrl Pts',(80.0841194566878,-4.9227160679212,331.713731658194));
#14890=CARTESIAN_POINT('Ctrl Pts',(80.0766953445511,-5.00830141115666,331.845719417711));
#14891=CARTESIAN_POINT('Ctrl Pts',(80.0692712324144,-5.08840062964462,331.980710415556));
#14892=CARTESIAN_POINT('Ctrl Pts',(80.0654141072598,-5.13001539849632,332.050843673763));
#14893=CARTESIAN_POINT('Ctrl Pts',(80.0615569821051,-5.17015011688825,332.121787203156));
#14894=CARTESIAN_POINT('Ctrl Pts',(80.0576998569504,-5.20877450889368,332.193472131263));
#14895=CARTESIAN_POINT('Ctrl Pts',(80.049875041618,-5.28713046641486,332.338896845801));
#14896=CARTESIAN_POINT('Ctrl Pts',(80.0420502262856,-5.35948338707886,332.487773869415));
#14897=CARTESIAN_POINT('Ctrl Pts',(80.0342254109531,-5.42553325429316,332.639593367858));
#14898=CARTESIAN_POINT('Ctrl Pts',(80.0264137334295,-5.49147222425392,332.791157962452));
#14899=CARTESIAN_POINT('Ctrl Pts',(80.0186020559058,-5.55112911112713,332.945654897665));
#14900=CARTESIAN_POINT('Ctrl Pts',(80.0107903783822,-5.60424943125671,333.102549374882));
#14901=CARTESIAN_POINT('Ctrl Pts',(80.0029966038673,-5.65724800883473,333.259084277197));
#14902=CARTESIAN_POINT('Ctrl Pts',(79.9952028293525,-5.70373979997366,333.418005465413));
#14903=CARTESIAN_POINT('Ctrl Pts',(79.9874090548376,-5.74351834540505,333.578758437669));
#14904=CARTESIAN_POINT('Ctrl Pts',(79.9796258163115,-5.78324311633875,333.739294096541));
#14905=CARTESIAN_POINT('Ctrl Pts',(79.9718425777854,-5.81627265272573,333.901656301376));
#14906=CARTESIAN_POINT('Ctrl Pts',(79.9640593392593,-5.84244959957532,334.065273709088));
#14907=CARTESIAN_POINT('Ctrl Pts',(79.9562906289864,-5.86857768433349,334.228585707282));
#14908=CARTESIAN_POINT('Ctrl Pts',(79.9485219187135,-5.88787864306747,334.393147926222));
#14909=CARTESIAN_POINT('Ctrl Pts',(79.9407532084407,-5.90024577640127,334.558377604102));
#14910=CARTESIAN_POINT('Ctrl Pts',(79.9338528072056,-5.91123063477968,334.705139554704));
#14911=CARTESIAN_POINT('Ctrl Pts',(79.9269524059706,-5.9167456887839,334.852427753432));
#14912=CARTESIAN_POINT('Ctrl Pts',(79.9200520047356,-5.91674999747214,334.99982704509));
#14913=CARTESIAN_POINT('',(78.1700520047036,-5.91674755306803,335.00538105598));
#14914=CARTESIAN_POINT('Ctrl Pts',(79.9200520047036,-5.91674999747216,334.999827045773));
#14915=CARTESIAN_POINT('Ctrl Pts',(79.9123202372434,-5.91675482525579,335.164985129787));
#14916=CARTESIAN_POINT('Ctrl Pts',(79.9045884697832,-5.90984009020886,335.3300164581));
#14917=CARTESIAN_POINT('Ctrl Pts',(79.8968567023231,-5.89606343540053,335.494334429544));
#14918=CARTESIAN_POINT('Ctrl Pts',(79.889115815794,-5.88227053200939,335.658846202328));
#14919=CARTESIAN_POINT('Ctrl Pts',(79.881374929265,-5.8615995840751,335.822642619378));
#14920=CARTESIAN_POINT('Ctrl Pts',(79.8736340427359,-5.83415972547376,335.985145095993));
#14921=CARTESIAN_POINT('Ctrl Pts',(79.865786357731,-5.80634128813123,336.149889566051));
#14922=CARTESIAN_POINT('Ctrl Pts',(79.857938672726,-5.77156587241067,336.313303792882));
#14923=CARTESIAN_POINT('Ctrl Pts',(79.8500909877211,-5.72999951188898,336.474800378442));
#14924=CARTESIAN_POINT('Ctrl Pts',(79.8423239099273,-5.68886009872801,336.634638157695));
#14925=CARTESIAN_POINT('Ctrl Pts',(79.8345568321335,-5.64106875826645,336.792597223523));
#14926=CARTESIAN_POINT('Ctrl Pts',(79.8267897543398,-5.58683534686467,336.948127657399));
#14927=CARTESIAN_POINT('Ctrl Pts',(79.8189017657292,-5.53175767894282,337.106079247892));
#14928=CARTESIAN_POINT('Ctrl Pts',(79.8110137771187,-5.47003586305808,337.261525649259));
#14929=CARTESIAN_POINT('Ctrl Pts',(79.8031257885081,-5.40193857534993,337.413915945232));
#14930=CARTESIAN_POINT('Ctrl Pts',(79.7952377998976,-5.33384128764181,337.566306241205));
#14931=CARTESIAN_POINT('Ctrl Pts',(79.787349811287,-5.25936873664166,337.715640155412));
#14932=CARTESIAN_POINT('Ctrl Pts',(79.7794618226765,-5.17883592564806,337.861396340551));
#14933=CARTESIAN_POINT('Ctrl Pts',(79.7720378452385,-5.10304045973776,337.998578413616));
#14934=CARTESIAN_POINT('Ctrl Pts',(79.7646138678006,-5.02167616900644,338.13295373613));
#14935=CARTESIAN_POINT('Ctrl Pts',(79.7571898903626,-4.93497572224292,338.264038171249));
#14936=CARTESIAN_POINT('Ctrl Pts',(79.749774674335,-4.84837759505124,338.394967907013));
#14937=CARTESIAN_POINT('Ctrl Pts',(79.7423594583074,-4.75645605091942,338.522614177775));
#14938=CARTESIAN_POINT('Ctrl Pts',(79.7349442422799,-4.65948996940092,338.646516664922));
#14939=CARTESIAN_POINT('Ctrl Pts',(79.7275361611358,-4.56261718815782,338.77029993372));
#14940=CARTESIAN_POINT('Ctrl Pts',(79.7201280799917,-4.46070976107004,338.890346298368));
#14941=CARTESIAN_POINT('Ctrl Pts',(79.7127199988477,-4.35409018648798,339.006223809328));
#14942=CARTESIAN_POINT('Ctrl Pts',(79.7053174316737,-4.24754997080285,339.122015070541));
#14943=CARTESIAN_POINT('Ctrl Pts',(79.6979148644997,-4.13630484286159,339.233643383032));
#14944=CARTESIAN_POINT('Ctrl Pts',(79.6905122973258,-4.02071787431496,339.340709427924));
#14945=CARTESIAN_POINT('Ctrl Pts',(79.683113627571,-3.90519176180136,339.447719103012));
#14946=CARTESIAN_POINT('Ctrl Pts',(79.6757149578163,-3.78532863441719,339.550171041278));
#14947=CARTESIAN_POINT('Ctrl Pts',(79.6683162880615,-3.66152867050092,339.647702481614));
#14948=CARTESIAN_POINT('Ctrl Pts',(79.6609188388576,-3.53774912973494,339.745217832291));
#14949=CARTESIAN_POINT('Ctrl Pts',(79.6535213896537,-3.41003433427522,339.837814065324));
#14950=CARTESIAN_POINT('Ctrl Pts',(79.6461239404497,-3.27881790750221,339.925168392242));
#14951=CARTESIAN_POINT('Ctrl Pts',(79.6387268119863,-3.14760717004481,340.012518931629));
#14952=CARTESIAN_POINT('Ctrl Pts',(79.6313296835228,-3.01289541381673,340.094627809989));
#14953=CARTESIAN_POINT('Ctrl Pts',(79.6239325550594,-2.87514540656207,340.171215471591));
#14954=CARTESIAN_POINT('Ctrl Pts',(79.6165342876228,-2.7373741892447,340.247814925782));
#14955=CARTESIAN_POINT('Ctrl Pts',(79.6091360201863,-2.59656411562483,340.318891289129));
#14956=CARTESIAN_POINT('Ctrl Pts',(79.6017377527497,-2.45320257915038,340.384210960591));
#14957=CARTESIAN_POINT('Ctrl Pts',(79.5943368862239,-2.30979067826044,340.449553579541));
#14958=CARTESIAN_POINT('Ctrl Pts',(79.5869360196982,-2.1638258692795,340.509135325395));
#14959=CARTESIAN_POINT('Ctrl Pts',(79.5795351531724,-2.01581539474792,340.562770789525));
#14960=CARTESIAN_POINT('Ctrl Pts',(79.5721261597877,-1.86764239056515,340.616465150523));
#14961=CARTESIAN_POINT('Ctrl Pts',(79.564717166403,-1.71741958587069,340.664200062636));
#14962=CARTESIAN_POINT('Ctrl Pts',(79.5573081730183,-1.56566995381436,340.705839829352));
#14963=CARTESIAN_POINT('Ctrl Pts',(79.549894615438,-1.41382683875039,340.747505247601));
#14964=CARTESIAN_POINT('Ctrl Pts',(79.5424810578578,-1.26045538481414,340.783067954373));
#14965=CARTESIAN_POINT('Ctrl Pts',(79.5350675002776,-1.10608810937295,340.81244351859));
#14966=CARTESIAN_POINT('Ctrl Pts',(79.527643388141,-0.951501063854682,340.841860904302));
#14967=CARTESIAN_POINT('Ctrl Pts',(79.5202192760043,-0.795915733462748,
340.865073500139));
#14968=CARTESIAN_POINT('Ctrl Pts',(79.5127951638677,-0.639869918127623,
340.882048712003));
#14969=CARTESIAN_POINT('Ctrl Pts',(79.5089380387126,-0.55879783454485,340.890868018001));
#14970=CARTESIAN_POINT('Ctrl Pts',(79.5050809135576,-0.477601470499032,
340.898004575316));
#14971=CARTESIAN_POINT('Ctrl Pts',(79.5012237884025,-0.396356052928012,
340.903459362256));
#14972=CARTESIAN_POINT('Ctrl Pts',(79.4937998109645,-0.239979445288353,
340.913958429188));
#14973=CARTESIAN_POINT('Ctrl Pts',(79.4863758335265,-0.0829494834163334,
340.918255658748));
#14974=CARTESIAN_POINT('Ctrl Pts',(79.4789518560885,0.0742008012545575,
340.916284712858));
#14975=CARTESIAN_POINT('Ctrl Pts',(79.4715366400609,0.23116562494422,340.91431609298));
#14976=CARTESIAN_POINT('Ctrl Pts',(79.4641214240333,0.388250119228613,340.90609402691));
#14977=CARTESIAN_POINT('Ctrl Pts',(79.4567062080057,0.544916274636628,340.891603925599));
#14978=CARTESIAN_POINT('Ctrl Pts',(79.4492981268616,0.701431686659512,340.877127766591));
#14979=CARTESIAN_POINT('Ctrl Pts',(79.4418900457175,0.857529192013971,340.856395613223));
#14980=CARTESIAN_POINT('Ctrl Pts',(79.4344819645734,1.01267103275587,340.829444908558));
#14981=CARTESIAN_POINT('Ctrl Pts',(79.4270793973994,1.16769739859159,340.802514263796));
#14982=CARTESIAN_POINT('Ctrl Pts',(79.4196768302254,1.3217691500244,340.769374347519));
#14983=CARTESIAN_POINT('Ctrl Pts',(79.4122742630514,1.47435401238794,340.730114380067));
#14984=CARTESIAN_POINT('Ctrl Pts',(79.4048755932967,1.62685853948896,340.690875082817));
#14985=CARTESIAN_POINT('Ctrl Pts',(79.3974769235419,1.77787737606564,340.645522244318));
#14986=CARTESIAN_POINT('Ctrl Pts',(79.3900782537872,1.92688890910211,340.594196072223));
#14987=CARTESIAN_POINT('Ctrl Pts',(79.3826808045832,2.0758758598628,340.542878367353));
#14988=CARTESIAN_POINT('Ctrl Pts',(79.3752833553792,2.22285581177223,340.48558940604));
#14989=CARTESIAN_POINT('Ctrl Pts',(79.3678859061752,2.36732266662489,340.422519152072));
#14990=CARTESIAN_POINT('Ctrl Pts',(79.3604887777118,2.51178325764637,340.35945163272));
#14991=CARTESIAN_POINT('Ctrl Pts',(79.3530916492483,2.65373062622977,340.290603468445));
#14992=CARTESIAN_POINT('Ctrl Pts',(79.3456945207848,2.79267925781721,340.216212526868));
#14993=CARTESIAN_POINT('Ctrl Pts',(79.3382962533482,2.93164928402549,340.141810130944));
#14994=CARTESIAN_POINT('Ctrl Pts',(79.3308979859116,3.06761932482788,340.061863434553));
#14995=CARTESIAN_POINT('Ctrl Pts',(79.3234997184749,3.20012918356456,339.976655882317));
#14996=CARTESIAN_POINT('Ctrl Pts',(79.3160988519492,3.33268559440775,339.891418395772));
#14997=CARTESIAN_POINT('Ctrl Pts',(79.3086979854235,3.46177908921587,339.800916575358));
#14998=CARTESIAN_POINT('Ctrl Pts',(79.3012971188977,3.58697925587329,339.705476636902));
#14999=CARTESIAN_POINT('Ctrl Pts',(79.293888125513,3.71231690428348,339.609931896269));
#15000=CARTESIAN_POINT('Ctrl Pts',(79.2864791321282,3.83375238966257,339.509438434912));
#15001=CARTESIAN_POINT('Ctrl Pts',(79.2790701387435,3.95088859113733,339.404362598938));
#15002=CARTESIAN_POINT('Ctrl Pts',(79.2716565811632,4.06809695255291,339.299222032624));
#15003=CARTESIAN_POINT('Ctrl Pts',(79.264243023583,4.18100048555196,339.189493726194));
#15004=CARTESIAN_POINT('Ctrl Pts',(79.2568294660027,4.28924001453668,339.07557979436));
#15005=CARTESIAN_POINT('Ctrl Pts',(79.249405353866,4.39763364230674,338.96150368519));
#15006=CARTESIAN_POINT('Ctrl Pts',(79.2419812417293,4.50134975912482,338.843230329141));
#15007=CARTESIAN_POINT('Ctrl Pts',(79.2345571295926,4.60006992151687,338.72119433511));
#15008=CARTESIAN_POINT('Ctrl Pts',(79.230700004438,4.6513590204187,338.657791722961));
#15009=CARTESIAN_POINT('Ctrl Pts',(79.2268428792833,4.70130031534411,338.593373968852));
#15010=CARTESIAN_POINT('Ctrl Pts',(79.2229857541286,4.74985391935847,338.528004862136));
#15011=CARTESIAN_POINT('Ctrl Pts',(79.2155617766906,4.84330716401107,338.402186084176));
#15012=CARTESIAN_POINT('Ctrl Pts',(79.2081377992526,4.93189871877175,338.27246171664));
#15013=CARTESIAN_POINT('Ctrl Pts',(79.2007138218146,5.01528434464131,338.139244097692));
#15014=CARTESIAN_POINT('Ctrl Pts',(79.1932986057869,5.09857156292619,338.006183695578));
#15015=CARTESIAN_POINT('Ctrl Pts',(79.1858833897593,5.17666488552189,337.869638561351));
#15016=CARTESIAN_POINT('Ctrl Pts',(79.1784681737317,5.2492608963903,337.73005322368));
#15017=CARTESIAN_POINT('Ctrl Pts',(79.1710600925876,5.32178705574251,337.590602194319));
#15018=CARTESIAN_POINT('Ctrl Pts',(79.1636520114435,5.38882626269449,337.448117114075));
#15019=CARTESIAN_POINT('Ctrl Pts',(79.1562439302994,5.45011899223641,337.303070457664));
#15020=CARTESIAN_POINT('Ctrl Pts',(79.1488413631254,5.51136610048038,337.158131762128));
#15021=CARTESIAN_POINT('Ctrl Pts',(79.1414387959514,5.56687510320979,337.010635629106));
#15022=CARTESIAN_POINT('Ctrl Pts',(79.1340362287774,5.61643298334764,336.861077941964));
#15023=CARTESIAN_POINT('Ctrl Pts',(79.1266375590227,5.66596477147812,336.711598996291));
#15024=CARTESIAN_POINT('Ctrl Pts',(79.1192388892679,5.70955155995479,336.560061011511));
#15025=CARTESIAN_POINT('Ctrl Pts',(79.1118402195132,5.74702897765007,336.406978497544));
#15026=CARTESIAN_POINT('Ctrl Pts',(79.1044427703092,5.78450021273525,336.253921237437));
#15027=CARTESIAN_POINT('Ctrl Pts',(79.0970453211052,5.81586398864669,336.09932031599));
#15028=CARTESIAN_POINT('Ctrl Pts',(79.0896478719012,5.84100617120702,335.943704122287));
#15029=CARTESIAN_POINT('Ctrl Pts',(79.0822507434378,5.86614726364613,335.788094675831));
#15030=CARTESIAN_POINT('Ctrl Pts',(79.0748536149743,5.8850672395747,335.631470413078));
#15031=CARTESIAN_POINT('Ctrl Pts',(79.0674564865108,5.89770338716464,335.474368337399));
#15032=CARTESIAN_POINT('Ctrl Pts',(79.0600582190742,5.91034148040587,335.317242071922));
#15033=CARTESIAN_POINT('Ctrl Pts',(79.0526599516376,5.9166937888601,335.15963821906));
#15034=CARTESIAN_POINT('Ctrl Pts',(79.045261684201,5.91674962833785,335.002097156152));
#15035=CARTESIAN_POINT('Ctrl Pts',(79.0378608176752,5.9168054874326,334.84450074741));
#15036=CARTESIAN_POINT('Ctrl Pts',(79.0304599511494,5.91056047329898,334.686967545517));
#15037=CARTESIAN_POINT('Ctrl Pts',(79.0230590846236,5.89805598709171,334.530036027305));
#15038=CARTESIAN_POINT('Ctrl Pts',(79.0156500912388,5.88553776976313,334.372932183282));
#15039=CARTESIAN_POINT('Ctrl Pts',(79.0082410978541,5.86674638327842,334.21643171466));
#15040=CARTESIAN_POINT('Ctrl Pts',(79.0008321044693,5.84177499100484,334.061066819752));
#15041=CARTESIAN_POINT('Ctrl Pts',(78.993418546889,5.81678821549222,333.90560621471));
#15042=CARTESIAN_POINT('Ctrl Pts',(78.9860049893088,5.78561392177289,333.751282942301));
#15043=CARTESIAN_POINT('Ctrl Pts',(78.9785914317285,5.74839588616332,333.598616648293));
#15044=CARTESIAN_POINT('Ctrl Pts',(78.9711673195918,5.71112486386649,333.445733005867));
#15045=CARTESIAN_POINT('Ctrl Pts',(78.9637432074551,5.66779301755273,333.294511411067));
#15046=CARTESIAN_POINT('Ctrl Pts',(78.9563190953184,5.61859349108032,333.145454841615));
#15047=CARTESIAN_POINT('Ctrl Pts',(78.9524619701639,5.59303235627328,333.068013952671));
#15048=CARTESIAN_POINT('Ctrl Pts',(78.9486048450093,5.56588819286609,332.991157109282));
#15049=CARTESIAN_POINT('Ctrl Pts',(78.9447477198548,5.53719305757851,332.914952373301));
#15050=CARTESIAN_POINT('Ctrl Pts',(78.9373237424168,5.48196227599398,332.768277785901));
#15051=CARTESIAN_POINT('Ctrl Pts',(78.9298997649788,5.42081626144866,332.623577958629));
#15052=CARTESIAN_POINT('Ctrl Pts',(78.9224757875408,5.35391547042627,332.481365509243));
#15053=CARTESIAN_POINT('Ctrl Pts',(78.9150605715132,5.2870936324032,332.339320891945));
#15054=CARTESIAN_POINT('Ctrl Pts',(78.9076453554855,5.21453069381927,332.199758143838));
#15055=CARTESIAN_POINT('Ctrl Pts',(78.9002301394579,5.13643627248911,332.063172973912));
#15056=CARTESIAN_POINT('Ctrl Pts',(78.8928220583138,5.05841699321783,331.92671922555));
#15057=CARTESIAN_POINT('Ctrl Pts',(78.8854139771697,4.97487701104492,331.793237673493));
#15058=CARTESIAN_POINT('Ctrl Pts',(78.8780058960257,4.8860731961658,331.663202241039));
#15059=CARTESIAN_POINT('Ctrl Pts',(78.8706033288516,4.79733547958791,331.533263596332));
#15060=CARTESIAN_POINT('Ctrl Pts',(78.8632007616777,4.70334194112026,331.406766270799));
#15061=CARTESIAN_POINT('Ctrl Pts',(78.8557981945036,4.60439430390263,331.28415774599));
#15062=CARTESIAN_POINT('Ctrl Pts',(78.8483995247489,4.50549876218306,331.161613774032));
#15063=CARTESIAN_POINT('Ctrl Pts',(78.8410008549941,4.40165455011443,331.042954814906));
#15064=CARTESIAN_POINT('Ctrl Pts',(78.8336021852393,4.29320537941507,330.928597522639));
#15065=CARTESIAN_POINT('Ctrl Pts',(78.8262047360354,4.18477409946197,330.814259095775));
#15066=CARTESIAN_POINT('Ctrl Pts',(78.8188072868314,4.07173962515045,330.704221197901));
#15067=CARTESIAN_POINT('Ctrl Pts',(78.8114098376274,3.95448452558128,330.598865748533));
#15068=CARTESIAN_POINT('Ctrl Pts',(78.8040127091639,3.83723450998864,330.493514867193));
#15069=CARTESIAN_POINT('Ctrl Pts',(78.7966155807005,3.71576451061122,330.392846280121));
#15070=CARTESIAN_POINT('Ctrl Pts',(78.789218452237,3.59049216806972,330.297203326367));
#15071=CARTESIAN_POINT('Ctrl Pts',(78.7818201848004,3.46520053671504,330.201545645986));
#15072=CARTESIAN_POINT('Ctrl Pts',(78.7744219173638,3.33610569311327,330.110915366196));
#15073=CARTESIAN_POINT('Ctrl Pts',(78.7670236499272,3.20365627026824,330.025613900744));
#15074=CARTESIAN_POINT('Ctrl Pts',(78.7596227834015,3.07116031654838,329.94028246799));
#15075=CARTESIAN_POINT('Ctrl Pts',(78.7522219168758,2.9353077507679,329.86028377881));
#15076=CARTESIAN_POINT('Ctrl Pts',(78.7448210503501,2.79657379412326,329.7858744188));
#15077=CARTESIAN_POINT('Ctrl Pts',(78.7374120569653,2.65768749433004,329.711383350199));
#15078=CARTESIAN_POINT('Ctrl Pts',(78.7300030635806,2.51591381399847,329.642494044424));
#15079=CARTESIAN_POINT('Ctrl Pts',(78.7225940701958,2.37175070608923,329.579416161458));
#15080=CARTESIAN_POINT('Ctrl Pts',(78.7151805126156,2.22749878873341,329.51629942034));
#15081=CARTESIAN_POINT('Ctrl Pts',(78.7077669550354,2.08085485751147,329.459001371235));
#15082=CARTESIAN_POINT('Ctrl Pts',(78.7003533974552,1.93233369925061,329.407682319714));
#15083=CARTESIAN_POINT('Ctrl Pts',(78.6929292853185,1.7836010939302,329.356290206127));
#15084=CARTESIAN_POINT('Ctrl Pts',(78.6855051731819,1.63298628027064,329.310894198097));
#15085=CARTESIAN_POINT('Ctrl Pts',(78.6780810610452,1.48101674419461,329.271604066939));
#15086=CARTESIAN_POINT('Ctrl Pts',(78.6742239358904,1.4020624518061,329.251191261954));
#15087=CARTESIAN_POINT('Ctrl Pts',(78.6703668107356,1.32274262817448,329.232425720055));
#15088=CARTESIAN_POINT('Ctrl Pts',(78.6665096855808,1.24313185569531,329.215317316235));
#15089=CARTESIAN_POINT('Ctrl Pts',(78.6590857081428,1.08990152092884,329.182388023338));
#15090=CARTESIAN_POINT('Ctrl Pts',(78.6516617307048,0.935130732112104,329.155501632051));
#15091=CARTESIAN_POINT('Ctrl Pts',(78.6442377532668,0.779337392664969,329.134800617976));
#15092=CARTESIAN_POINT('Ctrl Pts',(78.6368225372391,0.623727912798643,329.114124034212));
#15093=CARTESIAN_POINT('Ctrl Pts',(78.6294073212115,0.467098650745942,329.09961834622));
#15094=CARTESIAN_POINT('Ctrl Pts',(78.6219921051838,0.309979894999703,329.091375538486));
#15095=CARTESIAN_POINT('Ctrl Pts',(78.6145840240398,0.153012318129479,329.083140661941));
#15096=CARTESIAN_POINT('Ctrl Pts',(78.6071759428957,-0.00444344457639809,
329.081156688209));
#15097=CARTESIAN_POINT('Ctrl Pts',(78.5997678617516,-0.16184985370418,329.085464076755));
#15098=CARTESIAN_POINT('Ctrl Pts',(78.5923652945775,-0.31913910236706,329.089768259233));
#15099=CARTESIAN_POINT('Ctrl Pts',(78.5849627274035,-0.47637869912249,329.100354469734));
#15100=CARTESIAN_POINT('Ctrl Pts',(78.5775601602295,-0.633029067485845,
329.117211140775));
#15101=CARTESIAN_POINT('Ctrl Pts',(78.5701614904748,-0.78959696011467,329.134058936853));
#15102=CARTESIAN_POINT('Ctrl Pts',(78.5627628207201,-0.9455758720507,329.157170578768));
#15103=CARTESIAN_POINT('Ctrl Pts',(78.5553641509653,-1.10042942790038,329.186482507405));
#15104=CARTESIAN_POINT('Ctrl Pts',(78.5479667017613,-1.25525743772258,329.215789600484));
#15105=CARTESIAN_POINT('Ctrl Pts',(78.5405692525574,-1.40896009356819,329.251294880904));
#15106=CARTESIAN_POINT('Ctrl Pts',(78.5331718033534,-1.56100920107542,329.292883316713));
#15107=CARTESIAN_POINT('Ctrl Pts',(78.5257746748899,-1.71305171599789,329.334469949319));
#15108=CARTESIAN_POINT('Ctrl Pts',(78.5183775464264,-1.86344046514696,329.382139114417));
#15109=CARTESIAN_POINT('Ctrl Pts',(78.5109804179629,-2.0116607180864,329.435725409561));
#15110=CARTESIAN_POINT('Ctrl Pts',(78.5035821505263,-2.15990379324502,329.489319955656));
#15111=CARTESIAN_POINT('Ctrl Pts',(78.4961838830897,-2.30597735636702,329.548833319));
#15112=CARTESIAN_POINT('Ctrl Pts',(78.4887856156531,-2.44938516114103,329.614051346802));
#15113=CARTESIAN_POINT('Ctrl Pts',(78.4813847491273,-2.59284334658487,329.679292286383));
#15114=CARTESIAN_POINT('Ctrl Pts',(78.4739838826015,-2.73363356957718,329.750241726197));
#15115=CARTESIAN_POINT('Ctrl Pts',(78.4665830160758,-2.87128289235744,329.82663889579));
#15116=CARTESIAN_POINT('Ctrl Pts',(78.459174022691,-3.0090833672544,329.903119956779));
#15117=CARTESIAN_POINT('Ctrl Pts',(78.4517650293062,-3.14373572756957,329.985060512957));
#15118=CARTESIAN_POINT('Ctrl Pts',(78.4443560359214,-3.27479419483106,330.072155284102));
#15119=CARTESIAN_POINT('Ctrl Pts',(78.4369424783412,-3.4059333986289,330.159303708631));
#15120=CARTESIAN_POINT('Ctrl Pts',(78.4295289207609,-3.53347399613346,330.251612456776));
#15121=CARTESIAN_POINT('Ctrl Pts',(78.4221153631806,-3.65700260227987,330.348735383853));
#15122=CARTESIAN_POINT('Ctrl Pts',(78.4146912510439,-3.78070707401207,330.445996583199));
#15123=CARTESIAN_POINT('Ctrl Pts',(78.4072671389072,-3.90038786359415,330.548085408464));
#15124=CARTESIAN_POINT('Ctrl Pts',(78.3998430267705,-4.0156672090846,330.654617689042));
#15125=CARTESIAN_POINT('Ctrl Pts',(78.3959859016159,-4.07555947028801,330.709965497862));
#15126=CARTESIAN_POINT('Ctrl Pts',(78.3921287764613,-4.13426432275085,330.766512118276));
#15127=CARTESIAN_POINT('Ctrl Pts',(78.3882716513067,-4.19173310156535,330.824200176285));
#15128=CARTESIAN_POINT('Ctrl Pts',(78.3809497166853,-4.30082539813059,330.933708727926));
#15129=CARTESIAN_POINT('Ctrl Pts',(78.3736277820639,-4.40581013785178,331.04768289274));
#15130=CARTESIAN_POINT('Ctrl Pts',(78.3663058474424,-4.50629201713378,331.165777416631));
#15131=CARTESIAN_POINT('Ctrl Pts',(78.3589927243679,-4.60665297198342,331.283729820238));
#15132=CARTESIAN_POINT('Ctrl Pts',(78.3516796012933,-4.7025216017473,331.405792427091));
#15133=CARTESIAN_POINT('Ctrl Pts',(78.3443664782187,-4.79353790424402,331.531581783712));
#15134=CARTESIAN_POINT('Ctrl Pts',(78.3370616527893,-4.88445093745738,331.657228416708));
#15135=CARTESIAN_POINT('Ctrl Pts',(78.3297568273599,-4.97052238337176,331.78659306962));
#15136=CARTESIAN_POINT('Ctrl Pts',(78.3224520019304,-5.05143148884183,331.919258128951));
#15137=CARTESIAN_POINT('Ctrl Pts',(78.3151518665795,-5.13228864645006,332.0518380104));
#15138=CARTESIAN_POINT('Ctrl Pts',(78.3078517312287,-5.20798985723673,332.187713756579));
#15139=CARTESIAN_POINT('Ctrl Pts',(78.3005515958778,-5.27825672391012,332.326437485489));
#15140=CARTESIAN_POINT('Ctrl Pts',(78.2932546132463,-5.3484932443361,332.465101303593));
#15141=CARTESIAN_POINT('Ctrl Pts',(78.2859576306148,-5.41329991681757,332.606610315089));
#15142=CARTESIAN_POINT('Ctrl Pts',(78.2786606479834,-5.47244364816107,332.750490924623));
#15143=CARTESIAN_POINT('Ctrl Pts',(78.2713652833192,-5.53157426550559,332.894339631366));
#15144=CARTESIAN_POINT('Ctrl Pts',(78.264069918655,-5.58504429525359,333.040558534064));
#15145=CARTESIAN_POINT('Ctrl Pts',(78.2567745539908,-5.63266839287065,333.188653170026));
#15146=CARTESIAN_POINT('Ctrl Pts',(78.2494767028018,-5.68030872250736,333.336798282012));
#15147=CARTESIAN_POINT('Ctrl Pts',(78.2421788516127,-5.72209901513291,333.486820040269));
#15148=CARTESIAN_POINT('Ctrl Pts',(78.2348810004237,-5.75790345231781,333.638207653022));
#15149=CARTESIAN_POINT('Ctrl Pts',(78.2275821132039,-5.79371297243669,333.789616757337));
#15150=CARTESIAN_POINT('Ctrl Pts',(78.2202832259842,-5.82353486460667,333.942391726058));
#15151=CARTESIAN_POINT('Ctrl Pts',(78.2129843387645,-5.84728441350013,334.096011310835));
#15152=CARTESIAN_POINT('Ctrl Pts',(78.2056786537645,-5.87105608141101,334.249773968404));
#15153=CARTESIAN_POINT('Ctrl Pts',(78.1983729687645,-5.88874405596246,334.404382432076));
#15154=CARTESIAN_POINT('Ctrl Pts',(78.1910672837646,-5.90031545013051,334.559309460674));
#15155=CARTESIAN_POINT('Ctrl Pts',(78.1840621907443,-5.9114107399661,334.707862025793));
#15156=CARTESIAN_POINT('Ctrl Pts',(78.177057097724,-5.91688276630358,334.856707155613));
#15157=CARTESIAN_POINT('Ctrl Pts',(78.1700520047036,-5.91674755306803,335.00538105598));
#15158=CARTESIAN_POINT('',(76.4200520047036,-5.92511437741598,334.99740540478));
#15159=CARTESIAN_POINT('Ctrl Pts',(78.1700520047036,-5.91776632301522,335.005381982512));
#15160=CARTESIAN_POINT('Ctrl Pts',(78.15004587548,-5.92170700115339,335.430062848705));
#15161=CARTESIAN_POINT('Ctrl Pts',(78.0372937348318,-5.68602897212947,337.819173824506));
#15162=CARTESIAN_POINT('Ctrl Pts',(77.831795582759,-2.44063524270045,341.557127613012));
#15163=CARTESIAN_POINT('Ctrl Pts',(77.5535575484851,4.19326072651748,340.600820243559));
#15164=CARTESIAN_POINT('Ctrl Pts',(77.275319514211,6.97906321943746,334.504722804564));
#15165=CARTESIAN_POINT('Ctrl Pts',(76.997081479937,3.36028240668291,328.863133937542));
#15166=CARTESIAN_POINT('Ctrl Pts',(76.7188434456631,-3.34217997299833,328.853256476042));
#15167=CARTESIAN_POINT('Ctrl Pts',(76.5265002872521,-5.85529074220202,332.745839943748));
#15168=CARTESIAN_POINT('Ctrl Pts',(76.4269031402655,-5.92590944952505,334.852441329886));
#15169=CARTESIAN_POINT('Ctrl Pts',(76.4200520047036,-5.92511437741598,334.99740540478));
#15170=CARTESIAN_POINT('',(74.6700520047036,-5.9098640687304,334.996010226465));
#15171=CARTESIAN_POINT('Ctrl Pts',(76.4200520047036,-5.92511437741598,334.99740540478));
#15172=CARTESIAN_POINT('Ctrl Pts',(76.3341571288408,-5.91514630431429,336.81486633591));
#15173=CARTESIAN_POINT('Ctrl Pts',(76.1555162415536,-4.04647218064248,340.612465457021));
#15174=CARTESIAN_POINT('Ctrl Pts',(75.8841293428413,2.42129812204568,341.564292675178));
#15175=CARTESIAN_POINT('Ctrl Pts',(75.6058913085675,6.83035710149624,336.516194178614));
#15176=CARTESIAN_POINT('Ctrl Pts',(75.3276532742934,4.97129818480821,330.076706663327));
#15177=CARTESIAN_POINT('Ctrl Pts',(75.0494152400195,-1.44984769983852,328.155252775411));
#15178=CARTESIAN_POINT('Ctrl Pts',(74.8302148168229,-5.4603378352444,331.590028565428));
#15179=CARTESIAN_POINT('Ctrl Pts',(74.7037604050509,-5.91430140141107,334.278035342772));
#15180=CARTESIAN_POINT('Ctrl Pts',(74.6700520047036,-5.9098640687304,334.996010226465));
#15181=CARTESIAN_POINT('',(72.9200519871268,-5.91377486651518,335.004343153495));
#15182=CARTESIAN_POINT('Ctrl Pts',(74.6700520047036,-5.9098640687304,334.996010226465));
#15183=CARTESIAN_POINT('Ctrl Pts',(74.6110143936263,-5.90209242966351,336.253486745966));
#15184=CARTESIAN_POINT('Ctrl Pts',(74.4592307711244,-4.89277859890401,339.497807759121));
#15185=CARTESIAN_POINT('Ctrl Pts',(74.2147011371977,0.448117352137371,341.982249906723));
#15186=CARTESIAN_POINT('Ctrl Pts',(73.9364631029237,6.11402491854263,338.401664624365));
#15187=CARTESIAN_POINT('Ctrl Pts',(73.6582250686499,6.16918206006022,331.699421924716));
#15188=CARTESIAN_POINT('Ctrl Pts',(73.3799870343759,0.562971882037213,328.026071008301));
#15189=CARTESIAN_POINT('Ctrl Pts',(73.1339293463939,-4.8517161019475,330.437248912705));
#15190=CARTESIAN_POINT('Ctrl Pts',(72.9806176698364,-5.90182657715511,333.714701501588));
#15191=CARTESIAN_POINT('Ctrl Pts',(72.9200520047036,-5.91056552183396,335.004340422057));
#15192=CARTESIAN_POINT('',(71.1700520047036,-5.9210755085991,335.002052628764));
#15193=CARTESIAN_POINT('Ctrl Pts',(72.9200519708414,-5.91674840410918,335.00434568424));
#15194=CARTESIAN_POINT('Ctrl Pts',(72.9115360439865,-5.91661508257688,335.185865997231));
#15195=CARTESIAN_POINT('Ctrl Pts',(72.9030201171316,-5.90812453106049,335.367048315781));
#15196=CARTESIAN_POINT('Ctrl Pts',(72.8945041902767,-5.89139359093756,335.547185635009));
#15197=CARTESIAN_POINT('Ctrl Pts',(72.8859464929619,-5.87458058587037,335.728206524374));
#15198=CARTESIAN_POINT('Ctrl Pts',(72.8773887956471,-5.84944626172956,335.908172011056));
#15199=CARTESIAN_POINT('Ctrl Pts',(72.8688310983323,-5.81615864682976,336.086383522246));
#15200=CARTESIAN_POINT('Ctrl Pts',(72.8602189075065,-5.78265906381012,336.265729844659));
#15201=CARTESIAN_POINT('Ctrl Pts',(72.8516067166807,-5.74090210412475,336.443299656695));
#15202=CARTESIAN_POINT('Ctrl Pts',(72.8429945258548,-5.69110759812134,336.618401949179));
#15203=CARTESIAN_POINT('Ctrl Pts',(72.8365000058459,-5.65355717429603,336.750447948291));
#15204=CARTESIAN_POINT('Ctrl Pts',(72.8300054858369,-5.61143697585951,336.881091143479));
#15205=CARTESIAN_POINT('Ctrl Pts',(72.823510965828,-5.56485894612647,337.010043649331));
#15206=CARTESIAN_POINT('Ctrl Pts',(72.81608698839,-5.51161494328004,337.157451077854));
#15207=CARTESIAN_POINT('Ctrl Pts',(72.8086630109521,-5.4524295661987,337.302963847902));
#15208=CARTESIAN_POINT('Ctrl Pts',(72.8012390335141,-5.38745633068201,337.446067220559));
#15209=CARTESIAN_POINT('Ctrl Pts',(72.7938238174865,-5.32255977335893,337.589001709706));
#15210=CARTESIAN_POINT('Ctrl Pts',(72.7864086014589,-5.25188910669696,337.729532124879));
#15211=CARTESIAN_POINT('Ctrl Pts',(72.7789933854313,-5.17564723179545,337.867159970164));
#15212=CARTESIAN_POINT('Ctrl Pts',(72.7715853042873,-5.09947871644215,338.004655390629));
#15213=CARTESIAN_POINT('Ctrl Pts',(72.7641772231432,-5.0177498444251,338.139253476944));
#15214=CARTESIAN_POINT('Ctrl Pts',(72.7567691419992,-4.93071105926034,338.270476878467));
#15215=CARTESIAN_POINT('Ctrl Pts',(72.7493665748252,-4.84373705865302,338.401602608016));
#15216=CARTESIAN_POINT('Ctrl Pts',(72.7419640076512,-4.75146121984235,338.52935834453));
#15217=CARTESIAN_POINT('Ctrl Pts',(72.7345614404773,-4.6541791924521,338.653292570688));
#15218=CARTESIAN_POINT('Ctrl Pts',(72.7271627707225,-4.55694838362404,338.777161546018));
#15219=CARTESIAN_POINT('Ctrl Pts',(72.7197641009678,-4.45471686530048,338.897212725196));
#15220=CARTESIAN_POINT('Ctrl Pts',(72.7123654312131,-4.34782268836525,339.013024848295));
#15221=CARTESIAN_POINT('Ctrl Pts',(72.7049679820092,-4.24094614565005,339.128817865991));
#15222=CARTESIAN_POINT('Ctrl Pts',(72.6975705328052,-4.1294087238083,339.240372941537));
#15223=CARTESIAN_POINT('Ctrl Pts',(72.6901730836013,-4.01358779686133,339.347303021344));
#15224=CARTESIAN_POINT('Ctrl Pts',(72.6827759551379,-3.89777189170792,339.454228464849));
#15225=CARTESIAN_POINT('Ctrl Pts',(72.6753788266745,-3.77767312494759,339.556529058171));
#15226=CARTESIAN_POINT('Ctrl Pts',(72.667981698211,-3.65370446018548,339.65385585081));
#15227=CARTESIAN_POINT('Ctrl Pts',(72.6605834307745,-3.5297167073434,339.751197629346));
#15228=CARTESIAN_POINT('Ctrl Pts',(72.6531851633379,-3.40185816361799,339.843563851829));
#15229=CARTESIAN_POINT('Ctrl Pts',(72.6457868959013,-3.27057334862619,339.930647070492));
#15230=CARTESIAN_POINT('Ctrl Pts',(72.6383860293756,-3.13924241189826,340.017760882406));
#15231=CARTESIAN_POINT('Ctrl Pts',(72.6309851628499,-3.00448311818376,340.09958778909));
#15232=CARTESIAN_POINT('Ctrl Pts',(72.6235842963241,-2.86676717854363,340.175864807597));
#15233=CARTESIAN_POINT('Ctrl Pts',(72.6161753029394,-2.7289000136356,340.252225585564));
#15234=CARTESIAN_POINT('Ctrl Pts',(72.6087663095547,-2.58807004568195,340.323024123761));
#15235=CARTESIAN_POINT('Ctrl Pts',(72.60135731617,-2.4447723494503,340.388044053445));
#15236=CARTESIAN_POINT('Ctrl Pts',(72.5939437585897,-2.301386376895,340.453104037648));
#15237=CARTESIAN_POINT('Ctrl Pts',(72.5865302010096,-2.15552999179425,340.51237817974));
#15238=CARTESIAN_POINT('Ctrl Pts',(72.5791166434294,-2.00771576807876,340.565699233439));
#15239=CARTESIAN_POINT('Ctrl Pts',(72.5716925312927,-1.8596911037548,340.61909619942));
#15240=CARTESIAN_POINT('Ctrl Pts',(72.5642684191561,-1.70970338882277,340.6665230379));
#15241=CARTESIAN_POINT('Ctrl Pts',(72.5568443070194,-1.55827857792387,340.707862860658));
#15242=CARTESIAN_POINT('Ctrl Pts',(72.5529871818643,-1.47960729218889,340.729340562953));
#15243=CARTESIAN_POINT('Ctrl Pts',(72.5491300567091,-1.40054825221413,340.749176091258));
#15244=CARTESIAN_POINT('Ctrl Pts',(72.545272931554,-1.32117590016515,340.76735856379));
#15245=CARTESIAN_POINT('Ctrl Pts',(72.537848954116,-1.16840446363898,340.802355163696));
#15246=CARTESIAN_POINT('Ctrl Pts',(72.530424976678,-1.01401106733166,340.831330226838));
#15247=CARTESIAN_POINT('Ctrl Pts',(72.52300099924,-0.858511642384867,340.854134293163));
#15248=CARTESIAN_POINT('Ctrl Pts',(72.5155857832123,-0.703195730155659,
340.87691144726));
#15249=CARTESIAN_POINT('Ctrl Pts',(72.5081705671848,-0.546776753138711,
340.893532047254));
#15250=CARTESIAN_POINT('Ctrl Pts',(72.5007553511572,-0.389783708609473,
340.903896952268));
#15251=CARTESIAN_POINT('Ctrl Pts',(72.493347270013,-0.232941721997103,340.914251884223));
#15252=CARTESIAN_POINT('Ctrl Pts',(72.4859391888689,-0.0755271374395719,
340.918363079876));
#15253=CARTESIAN_POINT('Ctrl Pts',(72.4785311077248,0.0819231013680721,
340.916182820701));
#15254=CARTESIAN_POINT('Ctrl Pts',(72.4711285405508,0.239256147087246,340.914004184333));
#15255=CARTESIAN_POINT('Ctrl Pts',(72.4637259733768,0.39662442263823,340.905543422509));
#15256=CARTESIAN_POINT('Ctrl Pts',(72.4563234062028,0.553488244498939,340.890804811374));
#15257=CARTESIAN_POINT('Ctrl Pts',(72.4489247364481,0.710269478243119,340.876073960053));
#15258=CARTESIAN_POINT('Ctrl Pts',(72.4415260666933,0.86654641660166,340.855071876868));
#15259=CARTESIAN_POINT('Ctrl Pts',(72.4341273969386,1.02178187438646,340.827854868103));
#15260=CARTESIAN_POINT('Ctrl Pts',(72.4267299477346,1.17699172314103,340.8006423493));
#15261=CARTESIAN_POINT('Ctrl Pts',(72.4193324985307,1.33116006506648,340.767217004133));
#15262=CARTESIAN_POINT('Ctrl Pts',(72.4119350493267,1.48375719980413,340.727686717561));
#15263=CARTESIAN_POINT('Ctrl Pts',(72.4045379208632,1.63634771819606,340.688158144954));
#15264=CARTESIAN_POINT('Ctrl Pts',(72.3971407923998,1.78736680356902,340.642525250844));
#15265=CARTESIAN_POINT('Ctrl Pts',(72.3897436639363,1.93629753769941,340.590946467996));
#15266=CARTESIAN_POINT('Ctrl Pts',(72.3823453964997,2.08525120344516,340.539359743304));
#15267=CARTESIAN_POINT('Ctrl Pts',(72.3749471290631,2.23211552501007,340.4818254291));
#15268=CARTESIAN_POINT('Ctrl Pts',(72.3675488616265,2.3763914079367,340.418550953787));
#15269=CARTESIAN_POINT('Ctrl Pts',(72.3601479951008,2.52071797649814,340.355254249485));
#15270=CARTESIAN_POINT('Ctrl Pts',(72.352747128575,2.66245395434451,340.28621351887));
#15271=CARTESIAN_POINT('Ctrl Pts',(72.3453462620492,2.801122923585,340.211683118674));
#15272=CARTESIAN_POINT('Ctrl Pts',(72.3379372686645,2.93994416461109,340.137070876973));
#15273=CARTESIAN_POINT('Ctrl Pts',(72.3305282752798,3.07569134228388,340.056957103882));
#15274=CARTESIAN_POINT('Ctrl Pts',(72.323119281895,3.20791459414548,339.971641028792));
#15275=CARTESIAN_POINT('Ctrl Pts',(72.3157057243148,3.3402193000911,339.886272396057));
#15276=CARTESIAN_POINT('Ctrl Pts',(72.3082921667346,3.46899544995079,339.795695289551));
#15277=CARTESIAN_POINT('Ctrl Pts',(72.3008786091543,3.59382501959234,339.700250237067));
#15278=CARTESIAN_POINT('Ctrl Pts',(72.2934544970176,3.71883230697929,339.604669301078));
#15279=CARTESIAN_POINT('Ctrl Pts',(72.2860303848809,3.83988150610707,339.504206815396));
#15280=CARTESIAN_POINT('Ctrl Pts',(72.2786062727442,3.95658969894248,339.399241811576));
#15281=CARTESIAN_POINT('Ctrl Pts',(72.2747491475896,4.01722430386967,339.344708266132));
#15282=CARTESIAN_POINT('Ctrl Pts',(72.2708920224349,4.07668780572416,339.288959975301));
#15283=CARTESIAN_POINT('Ctrl Pts',(72.2670348972802,4.13493076885349,339.232053650332));
#15284=CARTESIAN_POINT('Ctrl Pts',(72.2596109198422,4.24703354666201,339.122523558435));
#15285=CARTESIAN_POINT('Ctrl Pts',(72.2521869424042,4.35495042124674,339.008370926896));
#15286=CARTESIAN_POINT('Ctrl Pts',(72.2447629649662,4.45827650851751,338.889948731809));
#15287=CARTESIAN_POINT('Ctrl Pts',(72.2373477489385,4.56148065545912,338.77166629273));
#15288=CARTESIAN_POINT('Ctrl Pts',(72.2299325329109,4.66010455636274,338.64912459825));
#15289=CARTESIAN_POINT('Ctrl Pts',(72.2225173168832,4.75377857076852,338.522714842647));
#15290=CARTESIAN_POINT('Ctrl Pts',(72.2151092357391,4.84736245250915,338.396426717873));
#15291=CARTESIAN_POINT('Ctrl Pts',(72.207701154595,4.93600570879356,338.266278239294));
#15292=CARTESIAN_POINT('Ctrl Pts',(72.2002930734509,5.01937764105134,338.132695111085));
#15293=CARTESIAN_POINT('Ctrl Pts',(72.1928905062769,5.10268751805733,337.999211411237));
#15294=CARTESIAN_POINT('Ctrl Pts',(72.1854879391029,5.18073368662685,337.862298467319));
#15295=CARTESIAN_POINT('Ctrl Pts',(72.1780853719288,5.25322768894203,337.722412424787));
#15296=CARTESIAN_POINT('Ctrl Pts',(72.1706867021741,5.32568352348182,337.582600031644));
#15297=CARTESIAN_POINT('Ctrl Pts',(72.1632880324193,5.3925928421868,337.439817987846));
#15298=CARTESIAN_POINT('Ctrl Pts',(72.1558893626645,5.45371229248286,337.294548494437));
#15299=CARTESIAN_POINT('Ctrl Pts',(72.1484919134605,5.51482165996753,337.149302965983));
#15300=CARTESIAN_POINT('Ctrl Pts',(72.1410944642566,5.57014291011179,337.001571146005));
#15301=CARTESIAN_POINT('Ctrl Pts',(72.1336970150526,5.61948011442046,336.851856853575));
#15302=CARTESIAN_POINT('Ctrl Pts',(72.1262998865891,5.66881517955393,336.702149052496));
#15303=CARTESIAN_POINT('Ctrl Pts',(72.1189027581256,5.71216659792967,336.550459304337));
#15304=CARTESIAN_POINT('Ctrl Pts',(72.1115056296621,5.74938786492976,336.39730803372));
#15305=CARTESIAN_POINT('Ctrl Pts',(72.1041073622255,5.78661486307582,336.24413318163));
#15306=CARTESIAN_POINT('Ctrl Pts',(72.0967090947889,5.81770974229293,336.08949672168));
#15307=CARTESIAN_POINT('Ctrl Pts',(72.0893108273523,5.84257684490011,335.933930604455));
#15308=CARTESIAN_POINT('Ctrl Pts',(72.0819099608265,5.86745268358196,335.778309835217));
#15309=CARTESIAN_POINT('Ctrl Pts',(72.0745090943007,5.88609633070922,335.621759126749));
#15310=CARTESIAN_POINT('Ctrl Pts',(72.0671082277749,5.89846386322769,335.464816756042));
#15311=CARTESIAN_POINT('Ctrl Pts',(72.0596992343901,5.91084497647925,335.307702047607));
#15312=CARTESIAN_POINT('Ctrl Pts',(72.0522902410054,5.91693618254478,335.150195190316));
#15313=CARTESIAN_POINT('Ctrl Pts',(72.0448812476206,5.91674566341376,334.9928364133));
#15314=CARTESIAN_POINT('Ctrl Pts',(72.0374676900403,5.9165550269164,334.835380697849));
#15315=CARTESIAN_POINT('Ctrl Pts',(72.0300541324601,5.91007496954033,334.678073616469));
#15316=CARTESIAN_POINT('Ctrl Pts',(72.0226405748798,5.89736563152799,334.5214509737));
#15317=CARTESIAN_POINT('Ctrl Pts',(72.0152164627431,5.88463819944623,334.364605349926));
#15318=CARTESIAN_POINT('Ctrl Pts',(72.0077923506064,5.8656638194122,334.208446480369));
#15319=CARTESIAN_POINT('Ctrl Pts',(72.0003682384697,5.84055400822791,334.053501484696));
#15320=CARTESIAN_POINT('Ctrl Pts',(71.9965111133152,5.82750845038064,333.973001321259));
#15321=CARTESIAN_POINT('Ctrl Pts',(71.9926539881607,5.8128076361528,333.892828594951));
#15322=CARTESIAN_POINT('Ctrl Pts',(71.9887968630062,5.7964725027736,333.813055566975));
#15323=CARTESIAN_POINT('Ctrl Pts',(71.9813728855682,5.76503155730365,333.659512931947));
#15324=CARTESIAN_POINT('Ctrl Pts',(71.9739489081302,5.72743818720968,333.506988790802));
#15325=CARTESIAN_POINT('Ctrl Pts',(71.9665249306922,5.68377011160646,333.356014634825));
#15326=CARTESIAN_POINT('Ctrl Pts',(71.9591097146646,5.64015357090266,333.205218651068));
#15327=CARTESIAN_POINT('Ctrl Pts',(71.951694498637,5.59047669751993,333.055969366426));
#15328=CARTESIAN_POINT('Ctrl Pts',(71.9442792826093,5.53486842140816,332.908789317118));
#15329=CARTESIAN_POINT('Ctrl Pts',(71.9368712014653,5.47931365129966,332.761750883713));
#15330=CARTESIAN_POINT('Ctrl Pts',(71.9294631203212,5.41783897139126,332.616778068705));
#15331=CARTESIAN_POINT('Ctrl Pts',(71.9220550391771,5.35062340543414,332.474379336535));
#15332=CARTESIAN_POINT('Ctrl Pts',(71.9146524720031,5.28345786925032,332.332086594342));
#15333=CARTESIAN_POINT('Ctrl Pts',(71.9072499048291,5.21056011390173,332.192364456133));
#15334=CARTESIAN_POINT('Ctrl Pts',(71.8998473376551,5.13215762075654,332.055702338721));
#15335=CARTESIAN_POINT('Ctrl Pts',(71.8924486679004,5.05379640618144,331.919112173317));
#15336=CARTESIAN_POINT('Ctrl Pts',(71.8850499981457,4.96993641103757,331.78557914304));
#15337=CARTESIAN_POINT('Ctrl Pts',(71.877651328391,4.88085143643022,331.655568834914));
#15338=CARTESIAN_POINT('Ctrl Pts',(71.870253879187,4.79178115807731,331.525579974453));
#15339=CARTESIAN_POINT('Ctrl Pts',(71.862856429983,4.69748782172357,331.399112990339));
#15340=CARTESIAN_POINT('Ctrl Pts',(71.8554589807791,4.59828907142544,331.276605288435));
#15341=CARTESIAN_POINT('Ctrl Pts',(71.8480618523156,4.49909462221226,331.154102898252));
#15342=CARTESIAN_POINT('Ctrl Pts',(71.8406647238522,4.39499541681371,331.035559738993));
#15343=CARTESIAN_POINT('Ctrl Pts',(71.8332675953887,4.286349809343,330.921380641143));
#15344=CARTESIAN_POINT('Ctrl Pts',(71.8258693279521,4.17768747316082,330.807183962562));
#15345=CARTESIAN_POINT('Ctrl Pts',(71.8184710605155,4.06447759833277,330.697352953731));
#15346=CARTESIAN_POINT('Ctrl Pts',(71.8110727930789,3.94711574759629,330.59225592422));
#15347=CARTESIAN_POINT('Ctrl Pts',(71.8036719265532,3.82971266640744,330.487121973017));
#15348=CARTESIAN_POINT('Ctrl Pts',(71.7962710600275,3.70815498302717,330.386725561173));
#15349=CARTESIAN_POINT('Ctrl Pts',(71.7888701935017,3.58287157677643,330.291394917088));
#15350=CARTESIAN_POINT('Ctrl Pts',(71.781461200117,3.45745059736798,330.195959590841));
#15351=CARTESIAN_POINT('Ctrl Pts',(71.7740522067323,3.32829602192653,330.105601367489));
#15352=CARTESIAN_POINT('Ctrl Pts',(71.7666432133475,3.19586656839799,330.020605715602));
#15353=CARTESIAN_POINT('Ctrl Pts',(71.7592296557673,3.06335553375799,329.935557703462));
#15354=CARTESIAN_POINT('Ctrl Pts',(71.7518160981871,2.92756592215524,329.855879033942));
#15355=CARTESIAN_POINT('Ctrl Pts',(71.7444025406068,2.78898084839398,329.781809088411));
#15356=CARTESIAN_POINT('Ctrl Pts',(71.7369784284702,2.65019847340903,329.707633690752));
#15357=CARTESIAN_POINT('Ctrl Pts',(71.7295543163335,2.50861302270973,329.639083127011));
#15358=CARTESIAN_POINT('Ctrl Pts',(71.7221302041968,2.36472811061008,329.57634887503));
#15359=CARTESIAN_POINT('Ctrl Pts',(71.718273079042,2.28997410586941,329.543755905401));
#15360=CARTESIAN_POINT('Ctrl Pts',(71.7144159538872,2.21459969578901,329.512732071195));
#15361=CARTESIAN_POINT('Ctrl Pts',(71.7105588287323,2.13867697669353,329.483298870533));
#15362=CARTESIAN_POINT('Ctrl Pts',(71.7031348512943,1.99254519953525,329.426647502254));
#15363=CARTESIAN_POINT('Ctrl Pts',(71.6957108738563,1.84394046562048,329.375721004578));
#15364=CARTESIAN_POINT('Ctrl Pts',(71.6882868964183,1.69335177558446,329.330741642276));
#15365=CARTESIAN_POINT('Ctrl Pts',(71.6808716803907,1.54294080285997,329.285815362389));
#15366=CARTESIAN_POINT('Ctrl Pts',(71.673456464363,1.39055088866465,329.246822353184));
#15367=CARTESIAN_POINT('Ctrl Pts',(71.6660412483354,1.23669121624611,329.213936969047));
#15368=CARTESIAN_POINT('Ctrl Pts',(71.6586331671913,1.08297958682957,329.181083227061));
#15369=CARTESIAN_POINT('Ctrl Pts',(71.6512250860472,0.927801377115052,329.154325488162));
#15370=CARTESIAN_POINT('Ctrl Pts',(71.6438170049031,0.771681045721263,329.133788366742));
#15371=CARTESIAN_POINT('Ctrl Pts',(71.6364144377291,0.615676917541566,329.113266531476));
#15372=CARTESIAN_POINT('Ctrl Pts',(71.629011870555,0.458732432388857,329.098956142915));
#15373=CARTESIAN_POINT('Ctrl Pts',(71.621609303381,0.301382254523396,329.090930758642));
#15374=CARTESIAN_POINT('Ctrl Pts',(71.6142106336263,0.144114920838886,329.0829095997));
#15375=CARTESIAN_POINT('Ctrl Pts',(71.6068119638716,-0.0135573083823089,
329.081166873884));
#15376=CARTESIAN_POINT('Ctrl Pts',(71.5994132941168,-0.17109474158854,329.085724291859));
#15377=CARTESIAN_POINT('Ctrl Pts',(71.5920158449128,-0.328606186010314,
329.090280958003));
#15378=CARTESIAN_POINT('Ctrl Pts',(71.5846183957088,-0.485982505858217,
329.101135694425));
#15379=CARTESIAN_POINT('Ctrl Pts',(71.5772209465048,-0.642683981786378,
329.118258092873));
#15380=CARTESIAN_POINT('Ctrl Pts',(71.5698238180413,-0.799378663411509,
329.135379748923));
#15381=CARTESIAN_POINT('Ctrl Pts',(71.5624266895779,-0.955398188292443,
329.158768486122));
#15382=CARTESIAN_POINT('Ctrl Pts',(71.5550295611144,-1.11020819986524,329.188342033855));
#15383=CARTESIAN_POINT('Ctrl Pts',(71.5476312936778,-1.26504204831536,329.217920135176));
#15384=CARTESIAN_POINT('Ctrl Pts',(71.5402330262411,-1.41866564603453,329.253684873166));
#15385=CARTESIAN_POINT('Ctrl Pts',(71.5328347588045,-1.57055521195258,329.295502924121));
#15386=CARTESIAN_POINT('Ctrl Pts',(71.5254338922787,-1.72249813827276,329.337335666198));
#15387=CARTESIAN_POINT('Ctrl Pts',(71.518033025753,-1.87270546031198,329.385225856279));
#15388=CARTESIAN_POINT('Ctrl Pts',(71.5106321592272,-2.02066907259672,329.438990463814));
#15389=CARTESIAN_POINT('Ctrl Pts',(71.5032231658424,-2.16879516307341,329.492814110029));
#15390=CARTESIAN_POINT('Ctrl Pts',(71.4958141724577,-2.31467227245839,329.5525249285));
#15391=CARTESIAN_POINT('Ctrl Pts',(71.4884051790729,-2.45781210553765,329.617891656946));
#15392=CARTESIAN_POINT('Ctrl Pts',(71.4809916214926,-2.60104011769161,329.683298653551));
#15393=CARTESIAN_POINT('Ctrl Pts',(71.4735780639124,-2.74152716120539,329.754368334855));
#15394=CARTESIAN_POINT('Ctrl Pts',(71.4661645063321,-2.87881049403801,329.830823982305));
#15395=CARTESIAN_POINT('Ctrl Pts',(71.4587403941954,-3.01628927482789,329.907388478366));
#15396=CARTESIAN_POINT('Ctrl Pts',(71.4513162820587,-3.15055491788447,329.989354060982));
#15397=CARTESIAN_POINT('Ctrl Pts',(71.443892169922,-3.2811738708044,330.07640084978));
#15398=CARTESIAN_POINT('Ctrl Pts',(71.4400350447674,-3.34903567564968,330.12162516112));
#15399=CARTESIAN_POINT('Ctrl Pts',(71.4361779196129,-3.41591369797062,330.16822033376));
#15400=CARTESIAN_POINT('Ctrl Pts',(71.4323207944583,-3.48175084408011,330.216137374229));
#15401=CARTESIAN_POINT('Ctrl Pts',(71.4249601178028,-3.60738999889424,330.30757901199));
#15402=CARTESIAN_POINT('Ctrl Pts',(71.4175994411473,-3.72962979400118,330.404123189567));
#15403=CARTESIAN_POINT('Ctrl Pts',(71.4102387644918,-3.84802294240781,330.505486678493));
#15404=CARTESIAN_POINT('Ctrl Pts',(71.4028868057498,-3.96627586712788,330.606730113495));
#15405=CARTESIAN_POINT('Ctrl Pts',(71.3955348470077,-4.08069092514987,330.712781256849));
#15406=CARTESIAN_POINT('Ctrl Pts',(71.3881828882656,-4.19084984256576,330.823313734602));
#15407=CARTESIAN_POINT('Ctrl Pts',(71.3808379650751,-4.30090334198744,330.933740436877));
#15408=CARTESIAN_POINT('Ctrl Pts',(71.3734930418846,-4.40670854038181,331.048639671035));
#15409=CARTESIAN_POINT('Ctrl Pts',(71.3661481186941,-4.50788046984098,331.167645080094));
#15410=CARTESIAN_POINT('Ctrl Pts',(71.3588085550214,-4.60897857514308,331.286563652083));
#15411=CARTESIAN_POINT('Ctrl Pts',(71.3514689913487,-4.70544989620773,331.409582146164));
#15412=CARTESIAN_POINT('Ctrl Pts',(71.3441294276761,-4.79694671114355,331.536297816938));
#15413=CARTESIAN_POINT('Ctrl Pts',(71.3367930035454,-4.88840438777385,331.662959284331));
#15414=CARTESIAN_POINT('Ctrl Pts',(71.3294565794146,-4.97489156949275,331.793314474467));
#15415=CARTESIAN_POINT('Ctrl Pts',(71.3221201552839,-5.05610125657842,331.926928141789));
#15416=CARTESIAN_POINT('Ctrl Pts',(71.3147852802572,-5.13729379603809,332.060513596256));
#15417=CARTESIAN_POINT('Ctrl Pts',(71.3074504052306,-5.21321086032108,332.197355834426));
#15418=CARTESIAN_POINT('Ctrl Pts',(71.3001155302039,-5.28358931096442,332.336991446585));
#15419=CARTESIAN_POINT('Ctrl Pts',(71.292780694991,-5.35396737959323,332.476626300801));
#15420=CARTESIAN_POINT('Ctrl Pts',(71.2854458597781,-5.41880672313075,332.619054159305));
#15421=CARTESIAN_POINT('Ctrl Pts',(71.2781110245651,-5.47789073763026,332.763788107293));
#15422=CARTESIAN_POINT('Ctrl Pts',(71.2707747201294,-5.53698658710326,332.908551046582));
#15423=CARTESIAN_POINT('Ctrl Pts',(71.2634384156937,-5.59032466976917,333.055620642552));
#15424=CARTESIAN_POINT('Ctrl Pts',(71.256102111258,-5.63773708135723,333.204491391279));
#15425=CARTESIAN_POINT('Ctrl Pts',(71.248758650777,-5.68519574039464,333.353507352878));
#15426=CARTESIAN_POINT('Ctrl Pts',(71.2414151902958,-5.72671706718547,333.504327613786));
#15427=CARTESIAN_POINT('Ctrl Pts',(71.2340717298148,-5.76218330324322,333.656432308246));
#15428=CARTESIAN_POINT('Ctrl Pts',(71.2267246167017,-5.79766718018159,333.808612659473));
#15429=CARTESIAN_POINT('Ctrl Pts',(71.2193775035886,-5.82708989440807,333.962078343988));
#15430=CARTESIAN_POINT('Ctrl Pts',(71.2120303904755,-5.85038523797935,334.116301448607));
#15431=CARTESIAN_POINT('Ctrl Pts',(71.2046724631652,-5.87371486990786,334.270751553824));
#15432=CARTESIAN_POINT('Ctrl Pts',(71.1973145358549,-5.89089906999728,334.425960928768));
#15433=CARTESIAN_POINT('Ctrl Pts',(71.1899566085446,-5.90192364540613,334.581397746905));
#15434=CARTESIAN_POINT('Ctrl Pts',(71.1833217405976,-5.91186484201282,334.721559876667));
#15435=CARTESIAN_POINT('Ctrl Pts',(71.1766868726506,-5.91679822761007,334.861906730318));
#15436=CARTESIAN_POINT('Ctrl Pts',(71.1700520047036,-5.91674964447282,335.002051129139));
#15437=CARTESIAN_POINT('',(69.4200520047036,-5.91677564200862,334.994557387791));
#15438=CARTESIAN_POINT('Ctrl Pts',(71.1700520047036,-5.92563727779681,335.002054210169));
#15439=CARTESIAN_POINT('Ctrl Pts',(71.1647289231972,-5.92614260361302,335.114659599285));
#15440=CARTESIAN_POINT('Ctrl Pts',(71.1594058416908,-5.92321159438174,335.227238160444));
#15441=CARTESIAN_POINT('Ctrl Pts',(71.0613367487598,-5.80437581181731,337.297592947633));
#15442=CARTESIAN_POINT('Ctrl Pts',(70.8758447259104,-3.44289158951305,341.090904729519));
#15443=CARTESIAN_POINT('Ctrl Pts',(70.5976066916366,3.25882553864336,341.191339033676));
#15444=CARTESIAN_POINT('Ctrl Pts',(70.3193686573626,6.96996657017265,335.610072890641));
#15445=CARTESIAN_POINT('Ctrl Pts',(70.0411306230885,4.28487215679163,329.468951860526));
#15446=CARTESIAN_POINT('Ctrl Pts',(69.7628925888149,-2.33238619026497,328.403592069872));
#15447=CARTESIAN_POINT('Ctrl Pts',(69.5558663826863,-5.66344677170153,332.11502018656));
#15448=CARTESIAN_POINT('Ctrl Pts',(69.4415861879827,-5.92099704865869,334.537243699616));
#15449=CARTESIAN_POINT('Ctrl Pts',(69.4200520047036,-5.91677564200862,334.994557387791));
#15450=CARTESIAN_POINT('',(67.6700520047036,-5.90704436558369,335.000708871167));
#15451=CARTESIAN_POINT('Ctrl Pts',(69.4200520047036,-5.91677564200862,334.994557387791));
#15452=CARTESIAN_POINT('Ctrl Pts',(69.348840176558,-5.90281578660099,336.5068573134));
#15453=CARTESIAN_POINT('Ctrl Pts',(69.1848823369878,-4.54245475610646,340.011087696333));
#15454=CARTESIAN_POINT('Ctrl Pts',(68.9281784859928,1.35723518751296,341.863711500856));
#15455=CARTESIAN_POINT('Ctrl Pts',(68.649940451719,6.50631927003558,337.573020108275));
#15456=CARTESIAN_POINT('Ctrl Pts',(68.371702417445,5.6846501915613,330.92110614004));
#15457=CARTESIAN_POINT('Ctrl Pts',(68.0934643831711,-0.353738462407954,
328.012332862722));
#15458=CARTESIAN_POINT('Ctrl Pts',(67.8595809122574,-5.15666167148477,330.957504813185));
#15459=CARTESIAN_POINT('Ctrl Pts',(67.7184434527681,-5.90594384398274,333.968760031375));
#15460=CARTESIAN_POINT('Ctrl Pts',(67.6700520047036,-5.90704436558369,335.000708871167));
#15461=CARTESIAN_POINT('',(65.9200528093559,-5.91850530180183,335.005138733431));
#15462=CARTESIAN_POINT('Ctrl Pts',(67.6700520047036,-5.90704436558369,335.000708871167));
#15463=CARTESIAN_POINT('Ctrl Pts',(67.6256974413435,-5.90805308007831,335.946571043714));
#15464=CARTESIAN_POINT('Ctrl Pts',(67.4885968665589,-5.24689642131051,338.86891281132));
#15465=CARTESIAN_POINT('Ctrl Pts',(67.2587502803491,-0.657146055416641,
341.965686038222));
#15466=CARTESIAN_POINT('Ctrl Pts',(66.9805122460754,5.5019745583164,339.322140543857));
#15467=CARTESIAN_POINT('Ctrl Pts',(66.7022742118012,6.61201432889349,332.712230467085));
#15468=CARTESIAN_POINT('Ctrl Pts',(66.4240361775276,1.65430614301727,328.201772723248));
#15469=CARTESIAN_POINT('Ctrl Pts',(66.1632958442427,-4.41428479853386,329.82126715782));
#15470=CARTESIAN_POINT('Ctrl Pts',(65.9953015223826,-5.90475744606087,333.408917292735));
#15471=CARTESIAN_POINT('Ctrl Pts',(65.9200532119472,-5.91938465457413,335.005130959516));
#15472=CARTESIAN_POINT('',(64.1700505935735,-5.92083642894063,334.996626893551));
#15473=CARTESIAN_POINT('Ctrl Pts',(65.9200520047037,-5.91674775497404,335.005154271017));
#15474=CARTESIAN_POINT('Ctrl Pts',(65.9090739000334,-5.91654498274101,335.237922813964));
#15475=CARTESIAN_POINT('Ctrl Pts',(65.898095795363,-5.90260318783092,335.470115853266));
#15476=CARTESIAN_POINT('Ctrl Pts',(65.8871176906927,-5.87514389833077,335.700438959801));
#15477=CARTESIAN_POINT('Ctrl Pts',(65.8805984967883,-5.8588375833427,335.837213115016));
#15478=CARTESIAN_POINT('Ctrl Pts',(65.874079302884,-5.83776526405744,335.973328646159));
#15479=CARTESIAN_POINT('Ctrl Pts',(65.8675601089796,-5.81198034837483,336.108519279311));
#15480=CARTESIAN_POINT('Ctrl Pts',(65.8601361315416,-5.78261680510881,336.262472701327));
#15481=CARTESIAN_POINT('Ctrl Pts',(65.8527121541035,-5.74708763781901,336.41549084855));
#15482=CARTESIAN_POINT('Ctrl Pts',(65.8452881766655,-5.70546337748581,336.567041228133));
#15483=CARTESIAN_POINT('Ctrl Pts',(65.8378729606378,-5.66388824004251,336.718412755466));
#15484=CARTESIAN_POINT('Ctrl Pts',(65.8304577446101,-5.61623242547244,336.868319606721));
#15485=CARTESIAN_POINT('Ctrl Pts',(65.8230425285825,-5.5626177919096,337.016237551389));
#15486=CARTESIAN_POINT('Ctrl Pts',(65.8156344474383,-5.50905474607722,337.164013170155));
#15487=CARTESIAN_POINT('Ctrl Pts',(65.8082263662942,-5.44954442200096,337.309803343657));
#15488=CARTESIAN_POINT('Ctrl Pts',(65.80081828515,-5.38425895716904,337.453097235057));
#15489=CARTESIAN_POINT('Ctrl Pts',(65.793415717976,-5.31902208550095,337.596284470197));
#15490=CARTESIAN_POINT('Ctrl Pts',(65.786013150802,-5.24801878617323,337.736978784671));
#15491=CARTESIAN_POINT('Ctrl Pts',(65.7786105836279,-5.17146990722256,337.874687732814));
#15492=CARTESIAN_POINT('Ctrl Pts',(65.7712119138731,-5.09496133092188,338.012324177798));
#15493=CARTESIAN_POINT('Ctrl Pts',(65.7638132441183,-5.0129131706709,338.146978061368));
#15494=CARTESIAN_POINT('Ctrl Pts',(65.7564145743635,-4.92559291198239,338.27818013964));
#15495=CARTESIAN_POINT('Ctrl Pts',(65.7490171251595,-4.83828705842531,338.409360573642));
#15496=CARTESIAN_POINT('Ctrl Pts',(65.7416196759555,-4.74571103914577,338.537090022111));
#15497=CARTESIAN_POINT('Ctrl Pts',(65.7342222267515,-4.64817655936471,338.660926827386));
#15498=CARTESIAN_POINT('Ctrl Pts',(65.7268250982879,-4.55064630850865,338.784758263312));
#15499=CARTESIAN_POINT('Ctrl Pts',(65.7194279698244,-4.44815825554298,338.904697098438));
#15500=CARTESIAN_POINT('Ctrl Pts',(65.7120308413609,-4.3410652521591,339.020333697468));
#15501=CARTESIAN_POINT('Ctrl Pts',(65.7046325739243,-4.23395575912603,339.135988101647));
#15502=CARTESIAN_POINT('Ctrl Pts',(65.6972343064876,-4.12224015747432,339.247338676892));
#15503=CARTESIAN_POINT('Ctrl Pts',(65.689836039051,-4.00630899756151,339.354011802758));
#15504=CARTESIAN_POINT('Ctrl Pts',(65.6824351725252,-3.89033710981307,339.460722404015));
#15505=CARTESIAN_POINT('Ctrl Pts',(65.6750343059994,-3.77014698966021,339.562752031663));
#15506=CARTESIAN_POINT('Ctrl Pts',(65.6676334394736,-3.64616304254419,339.659766692624));
#15507=CARTESIAN_POINT('Ctrl Pts',(65.6602244460888,-3.52204294920091,339.756887884958));
#15508=CARTESIAN_POINT('Ctrl Pts',(65.652815452704,-3.3941210033003,339.848982882879));
#15509=CARTESIAN_POINT('Ctrl Pts',(65.6454064593192,-3.26285202391792,339.935760046084));
#15510=CARTESIAN_POINT('Ctrl Pts',(65.6379929017389,-3.13150217831639,340.022590667013));
#15511=CARTESIAN_POINT('Ctrl Pts',(65.6305793441586,-2.99680150920922,340.104096732665));
#15512=CARTESIAN_POINT('Ctrl Pts',(65.6231657865784,-2.85922985299295,340.180032356101));
#15513=CARTESIAN_POINT('Ctrl Pts',(65.6157416744416,-2.72146233833811,340.256076087799));
#15514=CARTESIAN_POINT('Ctrl Pts',(65.6083175623049,-2.58081600605014,340.326533371689));
#15515=CARTESIAN_POINT('Ctrl Pts',(65.6008934501681,-2.43779183739425,340.391205943018));
#15516=CARTESIAN_POINT('Ctrl Pts',(65.597036325014,-2.36348502354024,340.424805947579));
#15517=CARTESIAN_POINT('Ctrl Pts',(65.5931791998598,-2.28853666020672,340.456845342317));
#15518=CARTESIAN_POINT('Ctrl Pts',(65.5893220747057,-2.21301854667385,340.487301656969));
#15519=CARTESIAN_POINT('Ctrl Pts',(65.5818980972677,-2.0676655315084,340.545922257491));
#15520=CARTESIAN_POINT('Ctrl Pts',(65.5744741198297,-1.91976243592748,340.598851922377));
#15521=CARTESIAN_POINT('Ctrl Pts',(65.5670501423917,-1.76979521288567,340.645861800199));
#15522=CARTESIAN_POINT('Ctrl Pts',(65.5596349263641,-1.62000497373084,340.692816199293));
#15523=CARTESIAN_POINT('Ctrl Pts',(65.5522197103365,-1.46815580863526,340.733864606996));
#15524=CARTESIAN_POINT('Ctrl Pts',(65.5448044943088,-1.31475449864639,340.768825805204));
#15525=CARTESIAN_POINT('Ctrl Pts',(65.5373964131647,-1.1615007906256,340.803753363924));
#15526=CARTESIAN_POINT('Ctrl Pts',(65.5299883320207,-1.00669827237262,340.832605291131));
#15527=CARTESIAN_POINT('Ctrl Pts',(65.5225802508766,-0.850869670954471,
340.855249897788));
#15528=CARTESIAN_POINT('Ctrl Pts',(65.5151776837026,-0.695157055610355,
340.877877649651));
#15529=CARTESIAN_POINT('Ctrl Pts',(65.5077751165286,-0.538420245553648,
340.894307227058));
#15530=CARTESIAN_POINT('Ctrl Pts',(65.5003725493546,-0.381192862395804,
340.904457855228));
#15531=CARTESIAN_POINT('Ctrl Pts',(65.4929738795998,-0.224048258768149,
340.914603139136));
#15532=CARTESIAN_POINT('Ctrl Pts',(65.4855752098451,-0.0664139679263883,
340.918476033599));
#15533=CARTESIAN_POINT('Ctrl Pts',(65.4781765400904,0.0911706611757941,
340.916047538098));
#15534=CARTESIAN_POINT('Ctrl Pts',(65.4707790908864,0.248729293707663,340.913619443224));
#15535=CARTESIAN_POINT('Ctrl Pts',(65.4633816416824,0.406237907955571,340.904892027271));
#15536=CARTESIAN_POINT('Ctrl Pts',(65.4559841924784,0.563156422989418,340.889888403505));
#15537=CARTESIAN_POINT('Ctrl Pts',(65.448587064015,0.720068134310021,340.874885430271));
#15538=CARTESIAN_POINT('Ctrl Pts',(65.4411899355515,0.876389425772367,340.853606825821));
#15539=CARTESIAN_POINT('Ctrl Pts',(65.433792807088,1.03158487802041,340.826127633509));
#15540=CARTESIAN_POINT('Ctrl Pts',(65.4263945396514,1.18680422649391,340.798644210087));
#15541=CARTESIAN_POINT('Ctrl Pts',(65.4189962722148,1.34089702307072,340.764958362871));
#15542=CARTESIAN_POINT('Ctrl Pts',(65.4115980047782,1.49333773313908,340.725196326527));
#15543=CARTESIAN_POINT('Ctrl Pts',(65.4041971382524,1.64583199723209,340.685420321362));
#15544=CARTESIAN_POINT('Ctrl Pts',(65.3967962717267,1.79667265834933,340.639563971162));
#15545=CARTESIAN_POINT('Ctrl Pts',(65.389395405201,1.94534918444987,340.587803424697));
#15546=CARTESIAN_POINT('Ctrl Pts',(65.3819864118162,2.0941889715901,340.535986040205));
#15547=CARTESIAN_POINT('Ctrl Pts',(65.3745774184314,2.24085952518916,340.478251634588));
#15548=CARTESIAN_POINT('Ctrl Pts',(65.3671684250467,2.38486946999285,340.414824851608));
#15549=CARTESIAN_POINT('Ctrl Pts',(65.3597548674665,2.52896812988996,340.351358995542));
#15550=CARTESIAN_POINT('Ctrl Pts',(65.3523413098862,2.67040258052837,340.28219393812));
#15551=CARTESIAN_POINT('Ctrl Pts',(65.344927752306,2.80870638332948,340.207600120472));
#15552=CARTESIAN_POINT('Ctrl Pts',(65.3375036401693,2.94720708691368,340.13290010487));
#15553=CARTESIAN_POINT('Ctrl Pts',(65.3300795280326,3.08256792076255,340.052756082643));
#15554=CARTESIAN_POINT('Ctrl Pts',(65.322655415896,3.21435105010636,339.967482047193));
#15555=CARTESIAN_POINT('Ctrl Pts',(65.3187982907412,3.28281769147805,339.923178752586));
#15556=CARTESIAN_POINT('Ctrl Pts',(65.3149411655864,3.35031916198981,339.877491429811));
#15557=CARTESIAN_POINT('Ctrl Pts',(65.3110840404317,3.41679771120956,339.830468296467));
#15558=CARTESIAN_POINT('Ctrl Pts',(65.3036600629937,3.54475188166431,339.739960815636));
#15559=CARTESIAN_POINT('Ctrl Pts',(65.2962360855557,3.66930041776815,339.644229225961));
#15560=CARTESIAN_POINT('Ctrl Pts',(65.2888121081177,3.78998789644607,339.54355833101));
#15561=CARTESIAN_POINT('Ctrl Pts',(65.2813968920901,3.91053294574074,339.443006242863));
#15562=CARTESIAN_POINT('Ctrl Pts',(65.2739816760624,4.0272257238441,339.337526689139));
#15563=CARTESIAN_POINT('Ctrl Pts',(65.2665664600348,4.13963959228238,339.22744776532));
#15564=CARTESIAN_POINT('Ctrl Pts',(65.2591583788907,4.25194529666245,339.117474758887));
#15565=CARTESIAN_POINT('Ctrl Pts',(65.2517502977467,4.35998002297345,339.002911452056));
#15566=CARTESIAN_POINT('Ctrl Pts',(65.2443422166026,4.46335015348345,338.884126152676));
#15567=CARTESIAN_POINT('Ctrl Pts',(65.2369396494286,4.56664334371741,338.765429267363));
#15568=CARTESIAN_POINT('Ctrl Pts',(65.2295370822546,4.66527860734633,338.642516927017));
#15569=CARTESIAN_POINT('Ctrl Pts',(65.2221345150806,4.75889924586057,338.515794153566));
#15570=CARTESIAN_POINT('Ctrl Pts',(65.2147358453258,4.85247059351786,338.389138099101));
#15571=CARTESIAN_POINT('Ctrl Pts',(65.2073371755711,4.94103235292452,338.258675906373));
#15572=CARTESIAN_POINT('Ctrl Pts',(65.1999385058164,5.02426826425997,338.124845431577));
#15573=CARTESIAN_POINT('Ctrl Pts',(65.1925410566124,5.10749044425467,337.991037034655));
#15574=CARTESIAN_POINT('Ctrl Pts',(65.1851436074084,5.18538832299996,337.853861775083));
#15575=CARTESIAN_POINT('Ctrl Pts',(65.1777461582045,5.25768906815454,337.713786326354));
#15576=CARTESIAN_POINT('Ctrl Pts',(65.170349029741,5.3299866784748,337.573716951053));
#15577=CARTESIAN_POINT('Ctrl Pts',(65.1629519012776,5.39668746655833,337.43074796826));
#15578=CARTESIAN_POINT('Ctrl Pts',(65.1555547728141,5.45756479182469,337.285370233799));
#15579=CARTESIAN_POINT('Ctrl Pts',(65.1481565053775,5.51845149067948,337.139970114796));
#15580=CARTESIAN_POINT('Ctrl Pts',(65.1407582379409,5.57351279717003,336.992160849907));
#15581=CARTESIAN_POINT('Ctrl Pts',(65.1333599705043,5.62257046778665,336.84245268522));
#15582=CARTESIAN_POINT('Ctrl Pts',(65.1259591039786,5.6716453728789,336.69269192648));
#15583=CARTESIAN_POINT('Ctrl Pts',(65.1185582374528,5.71471232665893,336.541031294172));
#15584=CARTESIAN_POINT('Ctrl Pts',(65.1111573709271,5.75164317820467,336.387995429788));
#15585=CARTESIAN_POINT('Ctrl Pts',(65.1037483775423,5.78861458335614,336.234791517394));
#15586=CARTESIAN_POINT('Ctrl Pts',(65.0963393841576,5.81943634247086,336.080209720115));
#15587=CARTESIAN_POINT('Ctrl Pts',(65.0889303907728,5.84403145193407,335.924784813514));
#15588=CARTESIAN_POINT('Ctrl Pts',(65.0815168331926,5.86864171283308,335.769264159809));
#15589=CARTESIAN_POINT('Ctrl Pts',(65.0741032756124,5.8870176372221,335.612899731633));
#15590=CARTESIAN_POINT('Ctrl Pts',(65.0666897180321,5.89913422813944,335.456230118354));
#15591=CARTESIAN_POINT('Ctrl Pts',(65.0592656058954,5.91126806924218,335.299337457199));
#15592=CARTESIAN_POINT('Ctrl Pts',(65.0518414937588,5.91712476535286,335.142139115129));
#15593=CARTESIAN_POINT('Ctrl Pts',(65.0444173816221,5.91673142270296,334.985173196588));
#15594=CARTESIAN_POINT('Ctrl Pts',(65.0405602564673,5.9165270653601,334.903623082353));
#15595=CARTESIAN_POINT('Ctrl Pts',(65.0367031313125,5.91463653986993,334.822135623827));
#15596=CARTESIAN_POINT('Ctrl Pts',(65.0328460061578,5.91106914136758,334.740785477892));
#15597=CARTESIAN_POINT('Ctrl Pts',(65.0254220287198,5.90420281348577,334.584207294977));
#15598=CARTESIAN_POINT('Ctrl Pts',(65.0179980512818,5.8911004368634,334.42766591759));
#15599=CARTESIAN_POINT('Ctrl Pts',(65.0105740738438,5.87175505333894,334.271698444263));
#15600=CARTESIAN_POINT('Ctrl Pts',(65.0031588578162,5.85243250027771,334.115915036021));
#15601=CARTESIAN_POINT('Ctrl Pts',(64.9957436417886,5.82688165130592,333.960704550447));
#15602=CARTESIAN_POINT('Ctrl Pts',(64.988328425761,5.79514753035372,333.806603308227));
#15603=CARTESIAN_POINT('Ctrl Pts',(64.9809203446168,5.76344394381292,333.652650341446));
#15604=CARTESIAN_POINT('Ctrl Pts',(64.9735122634727,5.7255690044362,333.499804856304));
#15605=CARTESIAN_POINT('Ctrl Pts',(64.9661041823286,5.68161942100958,333.348597166859));
#15606=CARTESIAN_POINT('Ctrl Pts',(64.9587016151547,5.63770255006059,333.197502024059));
#15607=CARTESIAN_POINT('Ctrl Pts',(64.9512990479807,5.58772014168348,333.048042606512));
#15608=CARTESIAN_POINT('Ctrl Pts',(64.9438964808067,5.53181975742786,332.900738050211));
#15609=CARTESIAN_POINT('Ctrl Pts',(64.9364978110519,5.47594880448024,332.753511049115));
#15610=CARTESIAN_POINT('Ctrl Pts',(64.9290991412972,5.41416621301346,332.608436997844));
#15611=CARTESIAN_POINT('Ctrl Pts',(64.9217004715424,5.34666903930941,332.466018795139));
#15612=CARTESIAN_POINT('Ctrl Pts',(64.9143030223384,5.27918300054306,332.323624087015));
#15613=CARTESIAN_POINT('Ctrl Pts',(64.9069055731345,5.20598441023189,332.183884694831));
#15614=CARTESIAN_POINT('Ctrl Pts',(64.8995081239305,5.12731805883598,332.047282592927));
#15615=CARTESIAN_POINT('Ctrl Pts',(64.892110995467,5.04865511827599,331.910686413852));
#15616=CARTESIAN_POINT('Ctrl Pts',(64.8847138670035,4.96452507425847,331.777227578006));
#15617=CARTESIAN_POINT('Ctrl Pts',(64.8773167385401,4.87521804969405,331.647362302539));
#15618=CARTESIAN_POINT('Ctrl Pts',(64.8699184711035,4.7858972740772,331.517477031062));
#15619=CARTESIAN_POINT('Ctrl Pts',(64.8625202036669,4.69139814221855,331.391186729227));
#15620=CARTESIAN_POINT('Ctrl Pts',(64.8551219362303,4.59205327314849,331.268917409241));
#15621=CARTESIAN_POINT('Ctrl Pts',(64.8477210697045,4.49267350318119,331.146605134757));
#15622=CARTESIAN_POINT('Ctrl Pts',(64.8403202031788,4.38844484180724,331.028316944103));
#15623=CARTESIAN_POINT('Ctrl Pts',(64.832919336653,4.27973912143312,330.914444515739));
#15624=CARTESIAN_POINT('Ctrl Pts',(64.8255103432683,4.17091403178527,330.800447044562));
#15625=CARTESIAN_POINT('Ctrl Pts',(64.8181013498835,4.05760232300439,330.69087528936));
#15626=CARTESIAN_POINT('Ctrl Pts',(64.8106923564988,3.94021202819587,330.586083401857));
#15627=CARTESIAN_POINT('Ctrl Pts',(64.8032787989186,3.82274941691652,330.481226958937));
#15628=CARTESIAN_POINT('Ctrl Pts',(64.7958652413383,3.70120350047246,330.381156487811));
#15629=CARTESIAN_POINT('Ctrl Pts',(64.7884516837581,3.57601366286169,330.286184470567));
#15630=CARTESIAN_POINT('Ctrl Pts',(64.7810275716214,3.45064559459811,330.191077243269));
#15631=CARTESIAN_POINT('Ctrl Pts',(64.7736034594847,3.32162354939444,330.101083179629));
#15632=CARTESIAN_POINT('Ctrl Pts',(64.766179347348,3.18941469949486,330.016470684631));
#15633=CARTESIAN_POINT('Ctrl Pts',(64.7623222221933,3.12072687915573,329.972511086923));
#15634=CARTESIAN_POINT('Ctrl Pts',(64.7584650970386,3.05117926500293,329.930003330584));
#15635=CARTESIAN_POINT('Ctrl Pts',(64.7546079718839,2.98083966773048,329.888980000256));
#15636=CARTESIAN_POINT('Ctrl Pts',(64.7471839944459,2.84545396926202,329.810020602629));
#15637=CARTESIAN_POINT('Ctrl Pts',(64.7397600170079,2.70672453754865,329.736325149011));
#15638=CARTESIAN_POINT('Ctrl Pts',(64.7323360395698,2.56509926474443,329.668190145503));
#15639=CARTESIAN_POINT('Ctrl Pts',(64.7249208235422,2.42364113107078,329.600135551551));
#15640=CARTESIAN_POINT('Ctrl Pts',(64.7175056075146,2.27929429199498,329.537628505835));
#15641=CARTESIAN_POINT('Ctrl Pts',(64.7100903914869,2.1325341160549,329.480921380669));
#15642=CARTESIAN_POINT('Ctrl Pts',(64.7026823103428,1.98591515201716,329.424268818812));
#15643=CARTESIAN_POINT('Ctrl Pts',(64.6952742291987,1.83688781978518,329.373405201078));
#15644=CARTESIAN_POINT('Ctrl Pts',(64.6878661480546,1.68595040643739,329.328536186351));
#15645=CARTESIAN_POINT('Ctrl Pts',(64.6804635808806,1.53512533856302,329.28370056845));
#15646=CARTESIAN_POINT('Ctrl Pts',(64.6730610137065,1.38239337660806,329.244850775169));
#15647=CARTESIAN_POINT('Ctrl Pts',(64.6656584465325,1.2282709271253,329.212143653123));
#15648=CARTESIAN_POINT('Ctrl Pts',(64.6582597767778,1.07422962243848,329.179453751235));
#15649=CARTESIAN_POINT('Ctrl Pts',(64.650861107023,0.918799652377362,329.152900156983));
#15650=CARTESIAN_POINT('Ctrl Pts',(64.6434624372682,0.762510553684954,329.132589308901));
#15651=CARTESIAN_POINT('Ctrl Pts',(64.6360649880642,0.606247237840906,329.112281811479));
#15652=CARTESIAN_POINT('Ctrl Pts',(64.6286675388603,0.449125444392178,329.09821506434));
#15653=CARTESIAN_POINT('Ctrl Pts',(64.6212700896563,0.291682946008149,329.090444041934));
#15654=CARTESIAN_POINT('Ctrl Pts',(64.6138729611928,0.134247274056367,329.082673356467));
#15655=CARTESIAN_POINT('Ctrl Pts',(64.6064758327293,-0.0235087024250638,
329.081197871375));
#15656=CARTESIAN_POINT('Ctrl Pts',(64.5990787042658,-0.181044338547331,
329.08602050139));
#15657=CARTESIAN_POINT('Ctrl Pts',(64.5916804368292,-0.338604231225055,
329.09084387397));
#15658=CARTESIAN_POINT('Ctrl Pts',(64.5842821693926,-0.495943342931435,
329.101967281142));
#15659=CARTESIAN_POINT('Ctrl Pts',(64.576883901956,-0.652523431670751,329.119341556116));
#15660=CARTESIAN_POINT('Ctrl Pts',(64.5694830354302,-0.809158528641985,
329.136721934856));
#15661=CARTESIAN_POINT('Ctrl Pts',(64.5620821689044,-0.96503370103994,329.160357512489));
#15662=CARTESIAN_POINT('Ctrl Pts',(64.5546813023786,-1.11961835824078,329.190147566901));
#15663=CARTESIAN_POINT('Ctrl Pts',(64.5472723089939,-1.2743727641742,329.21997033364));
#15664=CARTESIAN_POINT('Ctrl Pts',(64.5398633156091,-1.42783345818093,329.255961002987));
#15665=CARTESIAN_POINT('Ctrl Pts',(64.5324543222243,-1.57948181639369,329.29796810302));
#15666=CARTESIAN_POINT('Ctrl Pts',(64.525040764644,-1.73122359522613,329.340001080874));
#15667=CARTESIAN_POINT('Ctrl Pts',(64.5176272070638,-1.8811504589978,329.388057761112));
#15668=CARTESIAN_POINT('Ctrl Pts',(64.5102136494835,-2.02876185896069,329.441937758344));
#15669=CARTESIAN_POINT('Ctrl Pts',(64.5027895373468,-2.17658341077489,329.495894463615));
#15670=CARTESIAN_POINT('Ctrl Pts',(64.4953654252101,-2.32208257077187,329.555690902298));
#15671=CARTESIAN_POINT('Ctrl Pts',(64.4879413130734,-2.46478081776782,329.621079468623));
#15672=CARTESIAN_POINT('Ctrl Pts',(64.4840841879189,-2.53891830220502,329.655051461415));
#15673=CARTESIAN_POINT('Ctrl Pts',(64.4802270627644,-2.61230018603011,329.690532147838));
#15674=CARTESIAN_POINT('Ctrl Pts',(64.4763699376098,-2.68486237186319,329.727482137854));
#15675=CARTESIAN_POINT('Ctrl Pts',(64.4689459601718,-2.82452598372336,329.798601399278));
#15676=CARTESIAN_POINT('Ctrl Pts',(64.4615219827338,-2.96157251868736,329.875381099471));
#15677=CARTESIAN_POINT('Ctrl Pts',(64.4540980052958,-3.0955102583044,329.957605052831));
#15678=CARTESIAN_POINT('Ctrl Pts',(64.4466827892682,-3.22928993123667,330.039731969555));
#15679=CARTESIAN_POINT('Ctrl Pts',(64.4392675732405,-3.35996779675236,330.127290156948));
#15680=CARTESIAN_POINT('Ctrl Pts',(64.4318523572129,-3.48707438039661,330.220016440605));
#15681=CARTESIAN_POINT('Ctrl Pts',(64.4244442760688,-3.61405866272606,330.3126535035));
#15682=CARTESIAN_POINT('Ctrl Pts',(64.4170361949247,-3.73747820466366,330.410448544422));
#15683=CARTESIAN_POINT('Ctrl Pts',(64.4096281137806,-3.85689041153574,330.513093836963));
#15684=CARTESIAN_POINT('Ctrl Pts',(64.4022255466065,-3.97621373772126,330.615662728737));
#15685=CARTESIAN_POINT('Ctrl Pts',(64.3948229794325,-4.09153538608778,330.723074441593));
#15686=CARTESIAN_POINT('Ctrl Pts',(64.3874204122585,-4.20244400375068,330.834979596948));
#15687=CARTESIAN_POINT('Ctrl Pts',(64.3800217425037,-4.31329422851119,330.946825834728));
#15688=CARTESIAN_POINT('Ctrl Pts',(64.372623072749,-4.41973578778379,331.063160539011));
#15689=CARTESIAN_POINT('Ctrl Pts',(64.3652244029943,-4.52139261241745,331.18359601105));
#15690=CARTESIAN_POINT('Ctrl Pts',(64.3578269537903,-4.62303266683173,331.304011614975));
#15691=CARTESIAN_POINT('Ctrl Pts',(64.3504295045863,-4.71988931268382,331.428526359106));
#15692=CARTESIAN_POINT('Ctrl Pts',(64.3430320553823,-4.81162530113623,331.556717768761));
#15693=CARTESIAN_POINT('Ctrl Pts',(64.3356349269188,-4.90335731207604,331.68490362026));
#15694=CARTESIAN_POINT('Ctrl Pts',(64.3282377984553,-4.98996888987844,331.816765516812));
#15695=CARTESIAN_POINT('Ctrl Pts',(64.3208406699918,-5.07116500951098,331.951850395927));
#15696=CARTESIAN_POINT('Ctrl Pts',(64.3134424025552,-5.15237363131895,332.08695607474));
#15697=CARTESIAN_POINT('Ctrl Pts',(64.3060441351186,-5.22816494238112,332.225285404338));
#15698=CARTESIAN_POINT('Ctrl Pts',(64.298645867682,-5.29828901447146,332.366359158573));
#15699=CARTESIAN_POINT('Ctrl Pts',(64.2912450011562,-5.36843772188596,332.507482473502));
#15700=CARTESIAN_POINT('Ctrl Pts',(64.2838441346305,-5.43291506031164,332.651351798689));
#15701=CARTESIAN_POINT('Ctrl Pts',(64.2764432681047,-5.4915185960913,332.797466442643));
#15702=CARTESIAN_POINT('Ctrl Pts',(64.2690342747199,-5.55018648415592,332.943741534445));
#15703=CARTESIAN_POINT('Ctrl Pts',(64.2616252813351,-5.60296754957407,333.092266522304));
#15704=CARTESIAN_POINT('Ctrl Pts',(64.2542162879504,-5.6497085111847,333.242523314195));
#15705=CARTESIAN_POINT('Ctrl Pts',(64.2468027303701,-5.69647826683992,333.392872669453));
#15706=CARTESIAN_POINT('Ctrl Pts',(64.2393891727899,-5.73720040797205,333.544955594916));
#15707=CARTESIAN_POINT('Ctrl Pts',(64.2319756152096,-5.77177256728104,333.698242728431));
#15708=CARTESIAN_POINT('Ctrl Pts',(64.2245515030729,-5.80639394638803,333.851748094244));
#15709=CARTESIAN_POINT('Ctrl Pts',(64.2171273909362,-5.83484778961272,334.006460726064));
#15710=CARTESIAN_POINT('Ctrl Pts',(64.2097032787995,-5.85708335865905,334.16184423153));
#15711=CARTESIAN_POINT('Ctrl Pts',(64.205846153645,-5.86863563199691,334.24257221846));
#15712=CARTESIAN_POINT('Ctrl Pts',(64.2019890284904,-5.87851031382604,334.323481245407));
#15713=CARTESIAN_POINT('Ctrl Pts',(64.1981319033359,-5.88670584130011,334.404496095308));
#15714=CARTESIAN_POINT('Ctrl Pts',(64.1887719371252,-5.90659367411937,334.601092323655));
#15715=CARTESIAN_POINT('Ctrl Pts',(64.1794119709144,-5.91663528152812,334.798701233181));
#15716=CARTESIAN_POINT('Ctrl Pts',(64.1700520047036,-5.91674902275044,334.996599370386));
#15717=CARTESIAN_POINT('',(62.4200520047037,-5.90885860505928,334.996668088724));
#15718=CARTESIAN_POINT('Ctrl Pts',(64.1700494855937,-5.9240457458271,334.996648503969));
#15719=CARTESIAN_POINT('Ctrl Pts',(64.0866642800831,-5.91193315107515,336.761847268243));
#15720=CARTESIAN_POINT('Ctrl Pts',(63.9105330631479,-4.13709079260203,340.511496579727));
#15721=CARTESIAN_POINT('Ctrl Pts',(63.6416558347881,2.24304846138158,341.627318954231));
#15722=CARTESIAN_POINT('Ctrl Pts',(63.3634178005139,6.7868961248111,336.700195257098));
#15723=CARTESIAN_POINT('Ctrl Pts',(63.0851797662404,5.10250938892159,330.212827467371));
#15724=CARTESIAN_POINT('Ctrl Pts',(62.8069417319662,-1.26437490026262,328.118577252282));
#15725=CARTESIAN_POINT('Ctrl Pts',(62.5852324781208,-5.41315464388666,331.481794192749));
#15726=CARTESIAN_POINT('Ctrl Pts',(62.4562692356999,-5.91279898515629,334.22492707629));
#15727=CARTESIAN_POINT('Ctrl Pts',(62.4200520047037,-5.90885860505928,334.996668088724));
#15728=CARTESIAN_POINT('',(60.6700520047037,-5.91184663644443,335.00482244531));
#15729=CARTESIAN_POINT('Ctrl Pts',(62.4200520047037,-5.90885860505928,334.996668088724));
#15730=CARTESIAN_POINT('Ctrl Pts',(62.3635232242752,-5.90270835902497,336.201221198928));
#15731=CARTESIAN_POINT('Ctrl Pts',(62.2142484324222,-4.95843404406749,339.390925102401));
#15732=CARTESIAN_POINT('Ctrl Pts',(61.9722276291445,0.259294994690306,341.991808709264));
#15733=CARTESIAN_POINT('Ctrl Pts',(61.6939895948703,6.0198805072899,338.56562218963));
#15734=CARTESIAN_POINT('Ctrl Pts',(61.4157515605967,6.25611053163765,331.867316815072));
#15735=CARTESIAN_POINT('Ctrl Pts',(61.1375135263227,0.751200261145621,328.043828560992));
#15736=CARTESIAN_POINT('Ctrl Pts',(60.8889470076916,-4.78251313240014,330.330906474057));
#15737=CARTESIAN_POINT('Ctrl Pts',(60.7331265004854,-5.90158848196943,333.662495110449));
#15738=CARTESIAN_POINT('Ctrl Pts',(60.6700520047037,-5.91184663644443,335.00482244531));
#15739=CARTESIAN_POINT('',(58.9200526404505,-5.92193719492645,335.001095068209));
#15740=CARTESIAN_POINT('Ctrl Pts',(60.6700520047037,-5.91184663644443,335.00482244531));
#15741=CARTESIAN_POINT('Ctrl Pts',(60.6403804890607,-5.91667227931642,335.636280311452));
#15742=CARTESIAN_POINT('Ctrl Pts',(60.5179629619931,-5.53236301513891,338.23580376784));
#15743=CARTESIAN_POINT('Ctrl Pts',(60.3027994235009,-1.74600677399053,341.775255217807));
#15744=CARTESIAN_POINT('Ctrl Pts',(60.0245613892267,4.75259220513214,340.134733708085));
#15745=CARTESIAN_POINT('Ctrl Pts',(59.7463233549531,6.8898074657468,333.782142863004));
#15746=CARTESIAN_POINT('Ctrl Pts',(59.4680853206789,2.70434810844245,328.547161536998));
#15747=CARTESIAN_POINT('Ctrl Pts',(59.1926619252332,-3.89540661009425,329.226908277723));
#15748=CARTESIAN_POINT('Ctrl Pts',(59.0099845412119,-5.92134586278168,333.099183268187));
#15749=CARTESIAN_POINT('Ctrl Pts',(58.9200531686153,-5.92624669111755,335.001084705077));
#15750=CARTESIAN_POINT('',(57.1700520097339,-5.91552009762918,334.994582380634));
#15751=CARTESIAN_POINT('Ctrl Pts',(58.9200520047036,-5.91674989634092,335.001107542211));
#15752=CARTESIAN_POINT('Ctrl Pts',(58.9172377538462,-5.9167387733927,335.060528936766));
#15753=CARTESIAN_POINT('Ctrl Pts',(58.9144235029886,-5.91583252987226,335.11994095873));
#15754=CARTESIAN_POINT('Ctrl Pts',(58.9116092521311,-5.91403186056312,335.179325722484));
#15755=CARTESIAN_POINT('Ctrl Pts',(58.9041852746931,-5.90928170537042,335.335982384803));
#15756=CARTESIAN_POINT('Ctrl Pts',(58.8967612972551,-5.89829557337556,335.492686500929));
#15757=CARTESIAN_POINT('Ctrl Pts',(58.8893373198171,-5.88105925025173,335.64890111537));
#15758=CARTESIAN_POINT('Ctrl Pts',(58.8819221037895,-5.86384326858252,335.804931373062));
#15759=CARTESIAN_POINT('Ctrl Pts',(58.8745068877619,-5.84039181869279,335.960472911608));
#15760=CARTESIAN_POINT('Ctrl Pts',(58.8670916717343,-5.81074267411211,336.114988850954));
#15761=CARTESIAN_POINT('Ctrl Pts',(58.8596835905902,-5.78112205778905,336.269356115842));
#15762=CARTESIAN_POINT('Ctrl Pts',(58.8522755094461,-5.74531568863431,336.422699382042));
#15763=CARTESIAN_POINT('Ctrl Pts',(58.844867428302,-5.70341310147181,336.57448707726));
#15764=CARTESIAN_POINT('Ctrl Pts',(58.8374648611281,-5.66154170317029,336.726161794124));
#15765=CARTESIAN_POINT('Ctrl Pts',(58.8300622939541,-5.61358322062559,336.876282887221));
#15766=CARTESIAN_POINT('Ctrl Pts',(58.8226597267801,-5.55967818781155,337.024329274222));
#15767=CARTESIAN_POINT('Ctrl Pts',(58.8152610570254,-5.50580153576148,337.172297715448));
#15768=CARTESIAN_POINT('Ctrl Pts',(58.8078623872706,-5.44598469604835,337.318193276202));
#15769=CARTESIAN_POINT('Ctrl Pts',(58.8004637175159,-5.38041791224381,337.461510441194));
#15770=CARTESIAN_POINT('Ctrl Pts',(58.7930662683119,-5.31486194492279,337.604803963303));
#15771=CARTESIAN_POINT('Ctrl Pts',(58.7856688191079,-5.24355807121388,337.745519594793));
#15772=CARTESIAN_POINT('Ctrl Pts',(58.7782713699039,-5.16674454722182,337.883172097925));
#15773=CARTESIAN_POINT('Ctrl Pts',(58.7708742414405,-5.08993435373031,338.020818632684));
#15774=CARTESIAN_POINT('Ctrl Pts',(58.763477112977,-5.00761516680744,338.155401977256));
#15775=CARTESIAN_POINT('Ctrl Pts',(58.7560799845136,-4.92007091887895,338.286462036248));
#15776=CARTESIAN_POINT('Ctrl Pts',(58.748681717077,-4.83251319132162,338.417542275219));
#15777=CARTESIAN_POINT('Ctrl Pts',(58.7412834496404,-4.73972900814861,338.545097838062));
#15778=CARTESIAN_POINT('Ctrl Pts',(58.7338851822038,-4.64204520212892,338.668698257406));
#15779=CARTESIAN_POINT('Ctrl Pts',(58.7264843156781,-4.54432707876063,338.792342098876));
#15780=CARTESIAN_POINT('Ctrl Pts',(58.7190834491523,-4.44170613672706,338.912027737765));
#15781=CARTESIAN_POINT('Ctrl Pts',(58.7116825826266,-4.33454888248113,339.027358507494));
#15782=CARTESIAN_POINT('Ctrl Pts',(58.7042735892418,-4.22727395932564,339.142815921433));
#15783=CARTESIAN_POINT('Ctrl Pts',(58.6968645958571,-4.11545303021221,339.253908642604));
#15784=CARTESIAN_POINT('Ctrl Pts',(58.6894556024723,-3.99948930601635,339.360277038625));
#15785=CARTESIAN_POINT('Ctrl Pts',(58.6820420448921,-3.88345414416653,339.466710961247));
#15786=CARTESIAN_POINT('Ctrl Pts',(58.6746284873118,-3.76327138605488,339.568414518944));
#15787=CARTESIAN_POINT('Ctrl Pts',(58.6672149297316,-3.63937615359108,339.665069321583));
#15788=CARTESIAN_POINT('Ctrl Pts',(58.659790817595,-3.51530453358173,339.761861730028));
#15789=CARTESIAN_POINT('Ctrl Pts',(58.6523667054583,-3.38751018561926,339.853590810846));
#15790=CARTESIAN_POINT('Ctrl Pts',(58.6449425933216,-3.25645661285392,339.939981871536));
#15791=CARTESIAN_POINT('Ctrl Pts',(58.6410854681668,-3.18836900549629,339.984865505727));
#15792=CARTESIAN_POINT('Ctrl Pts',(58.637228343012,-3.11940206680971,340.028309047847));
#15793=CARTESIAN_POINT('Ctrl Pts',(58.6333712178572,-3.04962316104359,340.070279000028));
#15794=CARTESIAN_POINT('Ctrl Pts',(58.6259472404192,-2.91531665003766,340.151060402125));
#15795=CARTESIAN_POINT('Ctrl Pts',(58.6185232629812,-2.77759558924419,340.226623518268));
#15796=CARTESIAN_POINT('Ctrl Pts',(58.6110992855432,-2.63690382380578,340.296665817899));
#15797=CARTESIAN_POINT('Ctrl Pts',(58.6036840695155,-2.4963780958186,340.366625457078));
#15798=CARTESIAN_POINT('Ctrl Pts',(58.5962688534879,-2.35288897254252,340.43107708403));
#15799=CARTESIAN_POINT('Ctrl Pts',(58.5888536374603,-2.2069083692926,340.489761926718));
#15800=CARTESIAN_POINT('Ctrl Pts',(58.5814455563162,-2.06106822784422,340.548390303147));
#15801=CARTESIAN_POINT('Ctrl Pts',(58.5740374751721,-1.91274172294228,340.601262803605));
#15802=CARTESIAN_POINT('Ctrl Pts',(58.566629394028,-1.76242431750096,340.648167055566));
#15803=CARTESIAN_POINT('Ctrl Pts',(58.559226826854,-1.61221879604985,340.695036395836));
#15804=CARTESIAN_POINT('Ctrl Pts',(58.55182425968,-1.46002567940949,340.735946222136));
#15805=CARTESIAN_POINT('Ctrl Pts',(58.5444216925059,-1.30635920782263,340.770732724935));
#15806=CARTESIAN_POINT('Ctrl Pts',(58.5370230227512,-1.15277364096126,340.805500912793));
#15807=CARTESIAN_POINT('Ctrl Pts',(58.5296243529965,-0.997716627119905,
340.834152115551));
#15808=CARTESIAN_POINT('Ctrl Pts',(58.5222256832417,-0.841716216602509,
340.856572749758));
#15809=CARTESIAN_POINT('Ctrl Pts',(58.5148282340377,-0.685741541308998,
340.878989685257));
#15810=CARTESIAN_POINT('Ctrl Pts',(58.5074307848337,-0.528824147273298,
340.895178039114));
#15811=CARTESIAN_POINT('Ctrl Pts',(58.5000333356298,-0.371501015311117,
340.905075575987));
#15812=CARTESIAN_POINT('Ctrl Pts',(58.4926362071663,-0.214184704605776,
340.914972683721));
#15813=CARTESIAN_POINT('Ctrl Pts',(58.4852390787028,-0.0564630634277288,
340.918579493373));
#15814=CARTESIAN_POINT('Ctrl Pts',(58.4778419502394,0.101123352065179,340.915885785761));
#15815=CARTESIAN_POINT('Ctrl Pts',(58.4704436828028,0.258734031932412,340.913191663385));
#15816=CARTESIAN_POINT('Ctrl Pts',(58.4630454153662,0.416209071476924,340.904195098482));
#15817=CARTESIAN_POINT('Ctrl Pts',(58.4556471479296,0.573009613535163,340.888937981105));
#15818=CARTESIAN_POINT('Ctrl Pts',(58.4482462814038,0.729865241272778,340.873675503741));
#15819=CARTESIAN_POINT('Ctrl Pts',(58.4408454148781,0.886045528518061,340.852148131026));
#15820=CARTESIAN_POINT('Ctrl Pts',(58.4334445483523,1.04101857221098,340.824449407009));
#15821=CARTESIAN_POINT('Ctrl Pts',(58.4260355549675,1.19616179112189,340.796720267145));
#15822=CARTESIAN_POINT('Ctrl Pts',(58.4186265615828,1.35009475144059,340.762806308183));
#15823=CARTESIAN_POINT('Ctrl Pts',(58.411217568198,1.50229683008476,340.722851981033));
#15824=CARTESIAN_POINT('Ctrl Pts',(58.4038040106178,1.65459267045927,340.68287304064));
#15825=CARTESIAN_POINT('Ctrl Pts',(58.3963904530376,1.80515514837665,340.636846426176));
#15826=CARTESIAN_POINT('Ctrl Pts',(58.3889768954573,1.95348105334845,340.584965741767));
#15827=CARTESIAN_POINT('Ctrl Pts',(58.3815527833207,2.10201812740078,340.533011195706));
#15828=CARTESIAN_POINT('Ctrl Pts',(58.374128671184,2.24831192293559,340.475186071175));
#15829=CARTESIAN_POINT('Ctrl Pts',(58.3667045590473,2.39188061701794,340.411731485988));
#15830=CARTESIAN_POINT('Ctrl Pts',(58.3628474338926,2.46647033376405,340.37876427426));
#15831=CARTESIAN_POINT('Ctrl Pts',(58.3589903087379,2.54032490300279,340.344278297606));
#15832=CARTESIAN_POINT('Ctrl Pts',(58.3551331835833,2.61337970100166,340.308312076441));
#15833=CARTESIAN_POINT('Ctrl Pts',(58.3477092061453,2.75399146503163,340.239086317943));
#15834=CARTESIAN_POINT('Ctrl Pts',(58.3402852287073,2.89206286989311,340.164165277727));
#15835=CARTESIAN_POINT('Ctrl Pts',(58.3328612512693,3.02709932111036,340.083758478));
#15836=CARTESIAN_POINT('Ctrl Pts',(58.3254460352417,3.16197640899775,340.003446570393));
#15837=CARTESIAN_POINT('Ctrl Pts',(58.318030819214,3.2938253551254,339.917661979002));
#15838=CARTESIAN_POINT('Ctrl Pts',(58.3106156031864,3.42217317211194,339.826661511084));
#15839=CARTESIAN_POINT('Ctrl Pts',(58.3032075220423,3.55039749347531,339.735748603358));
#15840=CARTESIAN_POINT('Ctrl Pts',(58.2957994408982,3.67512708987139,339.6396300248));
#15841=CARTESIAN_POINT('Ctrl Pts',(58.2883913597541,3.79591524929912,339.538607493785));
#15842=CARTESIAN_POINT('Ctrl Pts',(58.2809887925801,3.91661350389376,339.437660155684));
#15843=CARTESIAN_POINT('Ctrl Pts',(58.2735862254061,4.03337587785536,339.33181637142));
#15844=CARTESIAN_POINT('Ctrl Pts',(58.2661836582321,4.14578633535286,339.221419929846));
#15845=CARTESIAN_POINT('Ctrl Pts',(58.2587849884773,4.25813760923585,339.111081611516));
#15846=CARTESIAN_POINT('Ctrl Pts',(58.2513863187226,4.36614126424074,338.996195670399));
#15847=CARTESIAN_POINT('Ctrl Pts',(58.2439876489678,4.46941602730123,338.877144688737));
#15848=CARTESIAN_POINT('Ctrl Pts',(58.2365901997639,4.57267375323266,338.758113346791));
#15849=CARTESIAN_POINT('Ctrl Pts',(58.2291927505599,4.67120389118536,338.63491860962));
#15850=CARTESIAN_POINT('Ctrl Pts',(58.2217953013559,4.76466351500142,338.507978356734));
#15851=CARTESIAN_POINT('Ctrl Pts',(58.2143981728924,4.85811908657106,338.381043607756));
#15852=CARTESIAN_POINT('Ctrl Pts',(58.207001044429,4.9465043598626,338.250363966507));
#15853=CARTESIAN_POINT('Ctrl Pts',(58.1996039159655,5.02951821539355,338.116388468007));
#15854=CARTESIAN_POINT('Ctrl Pts',(58.1922056485289,5.11254485298595,337.982392340624));
#15855=CARTESIAN_POINT('Ctrl Pts',(58.1848073810922,5.19019822943935,337.845099662797));
#15856=CARTESIAN_POINT('Ctrl Pts',(58.1774091136556,5.26222196446109,337.704986240121));
#15857=CARTESIAN_POINT('Ctrl Pts',(58.1700082471299,5.33427100217847,337.564823594126));
#15858=CARTESIAN_POINT('Ctrl Pts',(58.1626073806042,5.40068629024772,337.421838562005));
#15859=CARTESIAN_POINT('Ctrl Pts',(58.1552065140784,5.46125864858901,337.27652905444));
#15860=CARTESIAN_POINT('Ctrl Pts',(58.1477975206936,5.52189752117071,337.131059983145));
#15861=CARTESIAN_POINT('Ctrl Pts',(58.1403885273089,5.57668050705673,336.98326168362));
#15862=CARTESIAN_POINT('Ctrl Pts',(58.1329795339241,5.62544733907619,336.8336501296));
#15863=CARTESIAN_POINT('Ctrl Pts',(58.1255659763439,5.67424421314632,336.683946409701));
#15864=CARTESIAN_POINT('Ctrl Pts',(58.1181524187636,5.71701744718284,336.532427567818));
#15865=CARTESIAN_POINT('Ctrl Pts',(58.1107388611834,5.75365753095644,336.379621534686));
#15866=CARTESIAN_POINT('Ctrl Pts',(58.1033147490467,5.79034977859712,336.226597954191));
#15867=CARTESIAN_POINT('Ctrl Pts',(58.09589063691,5.82089136483445,336.072283887596));
#15868=CARTESIAN_POINT('Ctrl Pts',(58.0884665247733,5.84522430874448,335.91721499277));
#15869=CARTESIAN_POINT('Ctrl Pts',(58.0846093996187,5.85786625276605,335.836650458733));
#15870=CARTESIAN_POINT('Ctrl Pts',(58.080752274464,5.86883320446076,335.75588223507));
#15871=CARTESIAN_POINT('Ctrl Pts',(58.0768951493094,5.87812258485851,335.674985510864));
#15872=CARTESIAN_POINT('Ctrl Pts',(58.0694711718714,5.89600226148839,335.519280048574));
#15873=CARTESIAN_POINT('Ctrl Pts',(58.0620471944334,5.90771792010705,335.362628784773));
#15874=CARTESIAN_POINT('Ctrl Pts',(58.0546232169954,5.91317809895577,335.205561018994));
#15875=CARTESIAN_POINT('Ctrl Pts',(58.0472080009677,5.91863183397192,335.048678616811));
#15876=CARTESIAN_POINT('Ctrl Pts',(58.0397927849401,5.9178447711773,334.891381060417));
#15877=CARTESIAN_POINT('Ctrl Pts',(58.0323775689125,5.91077690466284,334.734205068136));
#15878=CARTESIAN_POINT('Ctrl Pts',(58.0249694877684,5.90371583881395,334.577180309804));
#15879=CARTESIAN_POINT('Ctrl Pts',(58.0175614066243,5.89038601709737,334.420277253065));
#15880=CARTESIAN_POINT('Ctrl Pts',(58.0101533254802,5.87079941943505,334.264034824695));
#15881=CARTESIAN_POINT('Ctrl Pts',(58.0027507583062,5.85122740043508,334.107908690419));
#15882=CARTESIAN_POINT('Ctrl Pts',(57.9953481911322,5.82540792454322,333.952442574158));
#15883=CARTESIAN_POINT('Ctrl Pts',(57.9879456239582,5.7934049502816,333.798172373195));
#15884=CARTESIAN_POINT('Ctrl Pts',(57.9805469542034,5.76141882544605,333.643983394817));
#15885=CARTESIAN_POINT('Ctrl Pts',(57.9731482844486,5.72325576154802,333.490989442274));
#15886=CARTESIAN_POINT('Ctrl Pts',(57.9657496146939,5.67903115142419,333.339718173425));
#15887=CARTESIAN_POINT('Ctrl Pts',(57.9583521654899,5.63481383698776,333.188471859639));
#15888=CARTESIAN_POINT('Ctrl Pts',(57.9509547162859,5.58453706556066,333.03894802339));
#15889=CARTESIAN_POINT('Ctrl Pts',(57.943557267082,5.52836666391632,332.891661177183));
#15890=CARTESIAN_POINT('Ctrl Pts',(57.9361601386185,5.47219869772271,332.744380717076));
#15891=CARTESIAN_POINT('Ctrl Pts',(57.928763010155,5.41013774239253,332.599337402872));
#15892=CARTESIAN_POINT('Ctrl Pts',(57.9213658816916,5.3423984480232,332.457027450982));
#15893=CARTESIAN_POINT('Ctrl Pts',(57.913967614255,5.27464872349348,332.314695586912));
#15894=CARTESIAN_POINT('Ctrl Pts',(57.9065693468184,5.20121907944653,332.175098260165));
#15895=CARTESIAN_POINT('Ctrl Pts',(57.8991710793817,5.12237088887098,332.03870855211));
#15896=CARTESIAN_POINT('Ctrl Pts',(57.891770212856,5.04349499809679,331.902270928916));
#15897=CARTESIAN_POINT('Ctrl Pts',(57.8843693463302,4.95919695741673,331.76904349091));
#15898=CARTESIAN_POINT('Ctrl Pts',(57.8769684798044,4.86978227120296,331.639471590125));
#15899=CARTESIAN_POINT('Ctrl Pts',(57.8695594864197,4.7802693991154,331.509757407006));
#15900=CARTESIAN_POINT('Ctrl Pts',(57.8621504930349,4.68562887301656,331.383707084893));
#15901=CARTESIAN_POINT('Ctrl Pts',(57.8547414996501,4.58620785646418,331.261734618863));
#15902=CARTESIAN_POINT('Ctrl Pts',(57.8473279420699,4.48672559313621,331.139687013587));
#15903=CARTESIAN_POINT('Ctrl Pts',(57.8399143844896,4.38245721774821,331.021722549066));
#15904=CARTESIAN_POINT('Ctrl Pts',(57.8325008269094,4.27378741625107,330.908219008403));
#15905=CARTESIAN_POINT('Ctrl Pts',(57.8250767147727,4.16496290339691,330.79455387467));
#15906=CARTESIAN_POINT('Ctrl Pts',(57.817652602636,4.05172471743978,330.685362607253));
#15907=CARTESIAN_POINT('Ctrl Pts',(57.8102284904993,3.93449192770485,330.580983838757));
#15908=CARTESIAN_POINT('Ctrl Pts',(57.8063713653446,3.87358477356824,330.526754866166));
#15909=CARTESIAN_POINT('Ctrl Pts',(57.80251424019,3.81159989802079,330.473824202212));
#15910=CARTESIAN_POINT('Ctrl Pts',(57.7986571150353,3.74859913353756,330.422234704734));
#15911=CARTESIAN_POINT('Ctrl Pts',(57.7912331375973,3.62733880742767,330.322938143187));
#15912=CARTESIAN_POINT('Ctrl Pts',(57.7838091601593,3.50194743281196,330.228313208422));
#15913=CARTESIAN_POINT('Ctrl Pts',(57.7763851827213,3.37282061375475,330.138723246931));
#15914=CARTESIAN_POINT('Ctrl Pts',(57.7689699666937,3.2438461837722,330.049239015074));
#15915=CARTESIAN_POINT('Ctrl Pts',(57.7615547506661,3.11114538796478,329.964778139473));
#15916=CARTESIAN_POINT('Ctrl Pts',(57.7541395346385,2.97514791472798,329.885664711031));
#15917=CARTESIAN_POINT('Ctrl Pts',(57.7467314534944,2.83928129757518,329.806627405133));
#15918=CARTESIAN_POINT('Ctrl Pts',(57.7393233723502,2.70012463838737,329.732927489496));
#15919=CARTESIAN_POINT('Ctrl Pts',(57.7319152912061,2.55813761521197,329.664846534153));
#15920=CARTESIAN_POINT('Ctrl Pts',(57.7245127240321,2.41625627557101,329.596816252708));
#15921=CARTESIAN_POINT('Ctrl Pts',(57.7171101568582,2.27154910175669,329.534396764668));
#15922=CARTESIAN_POINT('Ctrl Pts',(57.7097075896842,2.12450135285257,329.477824290714));
#15923=CARTESIAN_POINT('Ctrl Pts',(57.7023089199294,1.9775310239458,329.421281601921));
#15924=CARTESIAN_POINT('Ctrl Pts',(57.6949102501746,1.82822292159833,329.370579930014));
#15925=CARTESIAN_POINT('Ctrl Pts',(57.6875115804199,1.6770832102468,329.32590778464));
#15926=CARTESIAN_POINT('Ctrl Pts',(57.6801141312159,1.5259684322543,329.281243008783));
#15927=CARTESIAN_POINT('Ctrl Pts',(57.672716682012,1.3730230025021,329.242605891014));
#15928=CARTESIAN_POINT('Ctrl Pts',(57.665319232808,1.21876932391259,329.210135416299));
#15929=CARTESIAN_POINT('Ctrl Pts',(57.6579221043445,1.06452233349377,329.177666349448));
#15930=CARTESIAN_POINT('Ctrl Pts',(57.650524975881,0.908967572230166,329.151363470898));
#15931=CARTESIAN_POINT('Ctrl Pts',(57.6431278474176,0.752638478572933,329.131314807977));
#15932=CARTESIAN_POINT('Ctrl Pts',(57.635729579981,0.596285314137554,329.111263058062));
#15933=CARTESIAN_POINT('Ctrl Pts',(57.6283313125444,0.439157950112207,329.097467488698));
#15934=CARTESIAN_POINT('Ctrl Pts',(57.6209330451077,0.281795654633014,329.089964317237));
#15935=CARTESIAN_POINT('Ctrl Pts',(57.613532178582,0.124378076124673,329.082458509833));
#15936=CARTESIAN_POINT('Ctrl Pts',(57.6061313120562,-0.0332742256094407,
329.081249519367));
#15937=CARTESIAN_POINT('Ctrl Pts',(57.5987304455305,-0.190621418598294,
329.086321446234));
#15938=CARTESIAN_POINT('Ctrl Pts',(57.5913214521457,-0.348141393848144,
329.091398942562));
#15939=CARTESIAN_POINT('Ctrl Pts',(57.5839124587609,-0.505355218022771,
329.102771117964));
#15940=CARTESIAN_POINT('Ctrl Pts',(57.5765034653762,-0.661726883708614,
329.12037007169));
#15941=CARTESIAN_POINT('Ctrl Pts',(57.5690899077959,-0.818194879734465,
329.137979866979));
#15942=CARTESIAN_POINT('Ctrl Pts',(57.5616763502157,-0.973819315452161,
329.161824027759));
#15943=CARTESIAN_POINT('Ctrl Pts',(57.5542627926354,-1.12807432934979,329.191783503522));
#15944=CARTESIAN_POINT('Ctrl Pts',(57.5468386804987,-1.28254895349975,329.221785632083));
#15945=CARTESIAN_POINT('Ctrl Pts',(57.539414568362,-1.43564989979138,329.257920378292));
#15946=CARTESIAN_POINT('Ctrl Pts',(57.5319904562253,-1.58686562238468,329.300018591347));
#15947=CARTESIAN_POINT('Ctrl Pts',(57.5281333310707,-1.66542827831582,329.32189030793));
#15948=CARTESIAN_POINT('Ctrl Pts',(57.5242762059161,-1.74348237571021,329.345370892741));
#15949=CARTESIAN_POINT('Ctrl Pts',(57.5204190807615,-1.8209584133973,329.370431542367));
#15950=CARTESIAN_POINT('Ctrl Pts',(57.5129951033235,-1.97007993077494,329.41866687048));
#15951=CARTESIAN_POINT('Ctrl Pts',(57.5055711258855,-2.11750852491339,329.472904170722));
#15952=CARTESIAN_POINT('Ctrl Pts',(57.4981471484475,-2.26272456593604,329.533007398833));
#15953=CARTESIAN_POINT('Ctrl Pts',(57.4907319324199,-2.40776923018144,329.593039696092));
#15954=CARTESIAN_POINT('Ctrl Pts',(57.4833167163922,-2.55060619734944,329.658924000182));
#15955=CARTESIAN_POINT('Ctrl Pts',(57.4759015003646,-2.69073040343831,329.730474361149));
#15956=CARTESIAN_POINT('Ctrl Pts',(57.4684934192206,-2.83071978272151,329.801955876718));
#15957=CARTESIAN_POINT('Ctrl Pts',(57.4610853380765,-2.96800126719247,329.879092426955));
#15958=CARTESIAN_POINT('Ctrl Pts',(57.4536772569324,-3.10208932043758,329.961649832482));
#15959=CARTESIAN_POINT('Ctrl Pts',(57.4462746897584,-3.23607756949592,330.044145789025));
#15960=CARTESIAN_POINT('Ctrl Pts',(57.4388721225844,-3.36687680369746,330.132054372069));
#15961=CARTESIAN_POINT('Ctrl Pts',(57.4314695554104,-3.49402577849576,330.225095349464));
#15962=CARTESIAN_POINT('Ctrl Pts',(57.4240708856557,-3.6211078099147,330.318087341192));
#15963=CARTESIAN_POINT('Ctrl Pts',(57.4166722159009,-3.74454310897152,330.416206125874));
#15964=CARTESIAN_POINT('Ctrl Pts',(57.4092735461462,-3.86389923926214,330.519128072425));
#15965=CARTESIAN_POINT('Ctrl Pts',(57.4018760969422,-3.9832356794973,330.62203304005));
#15966=CARTESIAN_POINT('Ctrl Pts',(57.3944786477382,-4.09849400416171,330.729739353454));
#15967=CARTESIAN_POINT('Ctrl Pts',(57.3870811985343,-4.20927463563525,330.841882925614));
#15968=CARTESIAN_POINT('Ctrl Pts',(57.3796840700708,-4.32005046385366,330.954021635424));
#15969=CARTESIAN_POINT('Ctrl Pts',(57.3722869416074,-4.4263487226235,331.070596955944));
#15970=CARTESIAN_POINT('Ctrl Pts',(57.3648898131439,-4.52780671373297,331.191207944036));
#15971=CARTESIAN_POINT('Ctrl Pts',(57.3574915457073,-4.62928032684041,331.31183750321));
#15972=CARTESIAN_POINT('Ctrl Pts',(57.3500932782707,-4.72591194807402,331.436503681611));
#15973=CARTESIAN_POINT('Ctrl Pts',(57.3426950108341,-4.81737929255915,331.564772596447));
#15974=CARTESIAN_POINT('Ctrl Pts',(57.3352941443084,-4.90887877048416,331.693086573501));
#15975=CARTESIAN_POINT('Ctrl Pts',(57.3278932777826,-4.99521014291513,331.82500550328));
#15976=CARTESIAN_POINT('Ctrl Pts',(57.3204924112569,-5.07609464611404,331.960066825374));
#15977=CARTESIAN_POINT('Ctrl Pts',(57.3130834178722,-5.15706796823044,332.095276457712));
#15978=CARTESIAN_POINT('Ctrl Pts',(57.3056744244875,-5.2325822845081,332.233635053115));
#15979=CARTESIAN_POINT('Ctrl Pts',(57.2982654311027,-5.30240462976961,332.374655126522));
#15980=CARTESIAN_POINT('Ctrl Pts',(57.2908518735225,-5.37226998800428,332.515762073158));
#15981=CARTESIAN_POINT('Ctrl Pts',(57.2834383159423,-5.43643623640651,332.65953342483));
#15982=CARTESIAN_POINT('Ctrl Pts',(57.2760247583621,-5.49471891325114,332.805462548312));
#15983=CARTESIAN_POINT('Ctrl Pts',(57.2686006462254,-5.55308456615629,332.951599428617));
#15984=CARTESIAN_POINT('Ctrl Pts',(57.2611765340887,-5.605549794137,333.099899865204));
#15985=CARTESIAN_POINT('Ctrl Pts',(57.2537524219521,-5.65198001290537,333.249842151057));
#15986=CARTESIAN_POINT('Ctrl Pts',(57.2498952967972,-5.67610238086791,333.327743205336));
#15987=CARTESIAN_POINT('Ctrl Pts',(57.2460381716424,-5.69859660700881,333.406087252807));
#15988=CARTESIAN_POINT('Ctrl Pts',(57.2421810464875,-5.71944930166043,333.484800261274));
#15989=CARTESIAN_POINT('Ctrl Pts',(57.2326002064978,-5.77124599551726,333.680318090994));
#15990=CARTESIAN_POINT('Ctrl Pts',(57.2230193665081,-5.81303845332948,333.878589080625));
#15991=CARTESIAN_POINT('Ctrl Pts',(57.2134385265183,-5.8445851370561,334.078720922737));
#15992=CARTESIAN_POINT('Ctrl Pts',(57.2040376317612,-5.87553931789689,334.275093932541));
#15993=CARTESIAN_POINT('Ctrl Pts',(57.1946367370041,-5.89662901993686,334.473258743316));
#15994=CARTESIAN_POINT('Ctrl Pts',(57.185235842247,-5.90767099538767,334.672350838922));
#15995=CARTESIAN_POINT('Ctrl Pts',(57.1801745706339,-5.91361579514823,334.779538420307));
#15996=CARTESIAN_POINT('Ctrl Pts',(57.1751132990208,-5.91664898040585,334.88699439044));
#15997=CARTESIAN_POINT('Ctrl Pts',(57.1700520274078,-5.9167475183286,334.994580880855));
#15998=CARTESIAN_POINT('',(55.4200520047037,-5.9073516651236,335.001572401572));
#15999=CARTESIAN_POINT('Ctrl Pts',(57.1700520047036,-5.91517075142323,334.994582807498));
#16000=CARTESIAN_POINT('Ctrl Pts',(57.1013490072069,-5.90207856338616,336.454613423218));
#16001=CARTESIAN_POINT('Ctrl Pts',(56.9398999982855,-4.61904585079844,339.906179566562));
#16002=CARTESIAN_POINT('Ctrl Pts',(56.6857049779395,1.1712837905338,341.897877731828));
#16003=CARTESIAN_POINT('Ctrl Pts',(56.4074669436658,6.43442141176684,337.747879913133));
#16004=CARTESIAN_POINT('Ctrl Pts',(56.1292289093918,5.7927854753311,331.076193256795));
#16005=CARTESIAN_POINT('Ctrl Pts',(55.8509908751177,-0.164804190445459,
328.005326133404));
#16006=CARTESIAN_POINT('Ctrl Pts',(55.6145985735551,-5.09790670228151,330.849837736591));
#16007=CARTESIAN_POINT('Ctrl Pts',(55.4709522834171,-5.90477649463899,333.916263515696));
#16008=CARTESIAN_POINT('Ctrl Pts',(55.4200520047037,-5.9073516651236,335.001572401572));
#16009=CARTESIAN_POINT('',(53.6700520047037,-5.92095424708517,335.00477685681));
#16010=CARTESIAN_POINT('Ctrl Pts',(55.4200520047037,-5.9073516651236,335.001572401572));
#16011=CARTESIAN_POINT('Ctrl Pts',(55.3782062719925,-5.90946874382158,335.893817919584));
#16012=CARTESIAN_POINT('Ctrl Pts',(55.2436145278565,-5.30035127753471,338.760873686747));
#16013=CARTESIAN_POINT('Ctrl Pts',(55.0162767722962,-0.845117328821545,
341.945386931031));
#16014=CARTESIAN_POINT('Ctrl Pts',(54.7380387380219,5.38318256419084,339.469224586192));
#16015=CARTESIAN_POINT('Ctrl Pts',(54.4598007037483,6.67141527368653,332.891720804254));
#16016=CARTESIAN_POINT('Ctrl Pts',(54.1815626694741,1.83738865645259,328.248953722098));
#16017=CARTESIAN_POINT('Ctrl Pts',(53.9183131031261,-4.33154583340499,329.717886501529));
#16018=CARTESIAN_POINT('Ctrl Pts',(53.7478095482025,-5.90649086568565,333.356466118773));
#16019=CARTESIAN_POINT('Ctrl Pts',(53.6700520047037,-5.92095424708517,335.00477685681));
#16020=CARTESIAN_POINT('',(51.9200520047037,-5.92019556150583,334.995902038103));
#16021=CARTESIAN_POINT('Ctrl Pts',(53.6700520047037,-5.92095424708517,335.00477685681));
#16022=CARTESIAN_POINT('Ctrl Pts',(53.6550635367779,-5.92374219431769,335.322503620248));
#16023=CARTESIAN_POINT('Ctrl Pts',(53.5473290574271,-5.75582090692233,337.603316580136));
#16024=CARTESIAN_POINT('Ctrl Pts',(53.3468485666526,-2.79128630412854,341.41571069248));
#16025=CARTESIAN_POINT('Ctrl Pts',(53.0686105323781,3.88458281135488,340.819161391726));
#16026=CARTESIAN_POINT('Ctrl Pts',(52.7903724981046,6.99562761720305,334.882453572468));
#16027=CARTESIAN_POINT('Ctrl Pts',(52.5121344638305,3.6868882140429,329.053616374772));
#16028=CARTESIAN_POINT('Ctrl Pts',(52.2338964295567,-3.00525408476659,328.681687661471));
#16029=CARTESIAN_POINT('Ctrl Pts',(52.0365356098476,-5.79592130595738,332.530685836328));
#16030=CARTESIAN_POINT('Ctrl Pts',(51.9319208015634,-5.92475043617385,334.744504705933));
#16031=CARTESIAN_POINT('Ctrl Pts',(51.9200520047037,-5.92276479782944,334.995900259677));
#16032=CARTESIAN_POINT('',(50.1700520295874,-5.91196191274669,334.997409895193));
#16033=CARTESIAN_POINT('Ctrl Pts',(51.9200520047037,-5.91674858252048,334.995904424104));
#16034=CARTESIAN_POINT('Ctrl Pts',(51.9127391591387,-5.91685569133361,335.150641128864));
#16035=CARTESIAN_POINT('Ctrl Pts',(51.9054263135738,-5.91088856752764,335.305614441861));
#16036=CARTESIAN_POINT('Ctrl Pts',(51.8981134680088,-5.89881806647569,335.460299881729));
#16037=CARTESIAN_POINT('Ctrl Pts',(51.8908080257001,-5.88675978515568,335.61482872374));
#16038=CARTESIAN_POINT('Ctrl Pts',(51.8835025833913,-5.86861045034028,335.769069892076));
#16039=CARTESIAN_POINT('Ctrl Pts',(51.8761971410826,-5.84439292948739,335.922497614229));
#16040=CARTESIAN_POINT('Ctrl Pts',(51.8688973956181,-5.82019429365704,336.075805692178));
#16041=CARTESIAN_POINT('Ctrl Pts',(51.8615976501536,-5.7899369485819,336.228301208236));
#16042=CARTESIAN_POINT('Ctrl Pts',(51.8542979046891,-5.75369566429892,336.379462491381));
#16043=CARTESIAN_POINT('Ctrl Pts',(51.8469280070357,-5.71710609315713,336.532076468312));
#16044=CARTESIAN_POINT('Ctrl Pts',(51.8395581093824,-5.67441698959474,336.683330036368));
#16045=CARTESIAN_POINT('Ctrl Pts',(51.832188211729,-5.62575849370094,336.832695264645));
#16046=CARTESIAN_POINT('Ctrl Pts',(51.8248937832169,-5.57759826997733,336.980530964828));
#16047=CARTESIAN_POINT('Ctrl Pts',(51.8175993547047,-5.5235904729516,337.126516449146));
#16048=CARTESIAN_POINT('Ctrl Pts',(51.8103049261926,-5.46391165425848,337.270154179116));
#16049=CARTESIAN_POINT('Ctrl Pts',(51.8030107439393,-5.40423485031395,337.413787059896));
#16050=CARTESIAN_POINT('Ctrl Pts',(51.7957165616861,-5.3388875529823,337.555071988646));
#16051=CARTESIAN_POINT('Ctrl Pts',(51.7884223794329,-5.26809454556195,337.693531217848));
#16052=CARTESIAN_POINT('Ctrl Pts',(51.7811269090558,-5.19728903637546,337.832014898404));
#16053=CARTESIAN_POINT('Ctrl Pts',(51.7738314386787,-5.12103607899454,337.967671544158));
#16054=CARTESIAN_POINT('Ctrl Pts',(51.7665359683016,-5.03960636180203,338.100048109398));
#16055=CARTESIAN_POINT('Ctrl Pts',(51.7591096676938,-4.95671635923634,338.234798593752));
#16056=CARTESIAN_POINT('Ctrl Pts',(51.7516833670861,-4.86846236842017,338.366149874553));
#16057=CARTESIAN_POINT('Ctrl Pts',(51.7442570664783,-4.77517532000896,338.493655853927));
#16058=CARTESIAN_POINT('Ctrl Pts',(51.7369507764448,-4.68339580985058,338.619101309952));
#16059=CARTESIAN_POINT('Ctrl Pts',(51.7296444864112,-4.58674497578895,338.740824547462));
#16060=CARTESIAN_POINT('Ctrl Pts',(51.7223381963777,-4.4855775118768,338.85843555699));
#16061=CARTESIAN_POINT('Ctrl Pts',(51.7148518904828,-4.38191743569982,338.978944322709));
#16062=CARTESIAN_POINT('Ctrl Pts',(51.707365584588,-4.27351558957195,339.095135287745));
#16063=CARTESIAN_POINT('Ctrl Pts',(51.6998792786932,-4.16079164584239,339.206630889725));
#16064=CARTESIAN_POINT('Ctrl Pts',(51.6923929727983,-4.04806770211283,339.318126491705));
#16065=CARTESIAN_POINT('Ctrl Pts',(51.6849066669035,-3.93102202258054,339.424926494386));
#16066=CARTESIAN_POINT('Ctrl Pts',(51.6774203610087,-3.81010768033821,339.526699683735));
#16067=CARTESIAN_POINT('Ctrl Pts',(51.6699963835707,-3.69020003011022,339.627625543851));
#16068=CARTESIAN_POINT('Ctrl Pts',(51.6625724061327,-3.56609858956593,339.723936018681));
#16069=CARTESIAN_POINT('Ctrl Pts',(51.6551484286947,-3.43819401744272,339.815262449848));
#16070=CARTESIAN_POINT('Ctrl Pts',(51.6477332126671,-3.31044039195871,339.906481102086));
#16071=CARTESIAN_POINT('Ctrl Pts',(51.6403179966395,-3.1788928696426,339.992727203956));
#16072=CARTESIAN_POINT('Ctrl Pts',(51.6329027806118,-3.04397672083853,340.073670888567));
#16073=CARTESIAN_POINT('Ctrl Pts',(51.6254946994677,-2.90919038767392,340.154536689572));
#16074=CARTESIAN_POINT('Ctrl Pts',(51.6180866183237,-2.77104219868998,340.230110039646));
#16075=CARTESIAN_POINT('Ctrl Pts',(51.6106785371796,-2.62998798564979,340.300103183697));
#16076=CARTESIAN_POINT('Ctrl Pts',(51.6032759700056,-2.48903876183643,340.370044230573));
#16077=CARTESIAN_POINT('Ctrl Pts',(51.5958734028316,-2.34518815371135,340.434413176366));
#16078=CARTESIAN_POINT('Ctrl Pts',(51.5884708356576,-2.19891818445906,340.492967265564));
#16079=CARTESIAN_POINT('Ctrl Pts',(51.5810721659029,-2.05272522570621,340.55149052629));
#16080=CARTESIAN_POINT('Ctrl Pts',(51.5736734961481,-1.90411578824837,340.604204889221));
#16081=CARTESIAN_POINT('Ctrl Pts',(51.5662748263934,-1.75359344334423,340.65091502307));
#16082=CARTESIAN_POINT('Ctrl Pts',(51.5588773771894,-1.60309592995303,340.697617451198));
#16083=CARTESIAN_POINT('Ctrl Pts',(51.5514799279855,-1.45068649151728,340.738317505586));
#16084=CARTESIAN_POINT('Ctrl Pts',(51.5440824787815,-1.29688560543285,340.772869155708));
#16085=CARTESIAN_POINT('Ctrl Pts',(51.5366853503181,-1.1430913878867,340.80741930773));
#16086=CARTESIAN_POINT('Ctrl Pts',(51.5292882218546,-0.987906206784983,
340.835821503739));
#16087=CARTESIAN_POINT('Ctrl Pts',(51.5218910933911,-0.831862262539577,
340.857980517095));
#16088=CARTESIAN_POINT('Ctrl Pts',(51.5144928259545,-0.675794291421915,
340.880142942385));
#16089=CARTESIAN_POINT('Ctrl Pts',(51.5070945585179,-0.518867663403791,
340.896060218484));
#16090=CARTESIAN_POINT('Ctrl Pts',(51.4996962910813,-0.36162110806051,340.905688845233));
#16091=CARTESIAN_POINT('Ctrl Pts',(51.4922954245555,-0.204319310347798,
340.915320854619));
#16092=CARTESIAN_POINT('Ctrl Pts',(51.4848945580297,-0.0466977338128898,
340.918659793208));
#16093=CARTESIAN_POINT('Ctrl Pts',(51.477493691504,0.110703624027263,340.915714265423));
#16094=CARTESIAN_POINT('Ctrl Pts',(51.4700846981192,0.268277823605588,340.912765503166));
#16095=CARTESIAN_POINT('Ctrl Pts',(51.4626757047345,0.425630948190814,340.903518499966));
#16096=CARTESIAN_POINT('Ctrl Pts',(51.4552667113497,0.582226121880862,340.888033908318));
#16097=CARTESIAN_POINT('Ctrl Pts',(51.4478531537695,0.738917763599223,340.872539777627));
#16098=CARTESIAN_POINT('Ctrl Pts',(51.4404395961892,0.8948501552421,340.850800453072));
#16099=CARTESIAN_POINT('Ctrl Pts',(51.433026038609,1.04949587479265,340.822927869319));
#16100=CARTESIAN_POINT('Ctrl Pts',(51.4256019264723,1.20436176083678,340.795015603841));
#16101=CARTESIAN_POINT('Ctrl Pts',(51.4181778143357,1.35793695291711,340.760952720575));
#16102=CARTESIAN_POINT('Ctrl Pts',(51.410753702199,1.50970766647115,340.72090144333));
#16103=CARTESIAN_POINT('Ctrl Pts',(51.4068965770443,1.58855866255312,340.70009319231));
#16104=CARTESIAN_POINT('Ctrl Pts',(51.4030394518895,1.66692288412385,340.677669348726));
#16105=CARTESIAN_POINT('Ctrl Pts',(51.3991823267348,1.74473044719056,340.653657774322));
#16106=CARTESIAN_POINT('Ctrl Pts',(51.3917583492968,1.89449006595895,340.60744164716));
#16107=CARTESIAN_POINT('Ctrl Pts',(51.3843343718587,2.04263800935645,340.555201222443));
#16108=CARTESIAN_POINT('Ctrl Pts',(51.3769103944207,2.18865285682813,340.497065511234));
#16109=CARTESIAN_POINT('Ctrl Pts',(51.3694951783931,2.33449538481078,340.438998408911));
#16110=CARTESIAN_POINT('Ctrl Pts',(51.3620799623654,2.478209484374,340.375050005474));
#16111=CARTESIAN_POINT('Ctrl Pts',(51.3546647463378,2.61928762522662,340.305399409925));
#16112=CARTESIAN_POINT('Ctrl Pts',(51.3472566651937,2.76023002140195,340.235815831829));
#16113=CARTESIAN_POINT('Ctrl Pts',(51.3398485840496,2.89854117576706,340.160541148573));
#16114=CARTESIAN_POINT('Ctrl Pts',(51.3324405029055,3.0337324322031,340.079802958019));
#16115=CARTESIAN_POINT('Ctrl Pts',(51.3250379357315,3.16882306331819,339.999124862375));
#16116=CARTESIAN_POINT('Ctrl Pts',(51.3176353685574,3.30079810129,339.912991547142));
#16117=CARTESIAN_POINT('Ctrl Pts',(51.3102328013834,3.4291925574252,339.821676986962));
#16118=CARTESIAN_POINT('Ctrl Pts',(51.3028341316286,3.55751941444094,339.730410503499));
#16119=CARTESIAN_POINT('Ctrl Pts',(51.2954354618739,3.68226914065808,339.633968423628));
#16120=CARTESIAN_POINT('Ctrl Pts',(51.2880367921191,3.80300496652803,339.532668506196));
#16121=CARTESIAN_POINT('Ctrl Pts',(51.2806393429151,3.92372087473515,339.431385300106));
#16122=CARTESIAN_POINT('Ctrl Pts',(51.273241893711,4.04042391115701,339.32524608661));
#16123=CARTESIAN_POINT('Ctrl Pts',(51.2658444445071,4.15270961542479,339.214609520757));
#16124=CARTESIAN_POINT('Ctrl Pts',(51.2584473160436,4.26499045118042,339.103977751913));
#16125=CARTESIAN_POINT('Ctrl Pts',(51.2510501875801,4.3728540697571,338.988849280371));
#16126=CARTESIAN_POINT('Ctrl Pts',(51.2436530591166,4.47593238886079,338.869620112213));
#16127=CARTESIAN_POINT('Ctrl Pts',(51.23625479168,4.57902657945222,338.75037258574));
#16128=CARTESIAN_POINT('Ctrl Pts',(51.2288565242434,4.67733375937255,338.627023387787));
#16129=CARTESIAN_POINT('Ctrl Pts',(51.2214582568068,4.77052581092442,338.500002007114));
#16130=CARTESIAN_POINT('Ctrl Pts',(51.214057390281,4.8637506018245,338.372936002494));
#16131=CARTESIAN_POINT('Ctrl Pts',(51.2066565237552,4.95185646590455,338.242195547336));
#16132=CARTESIAN_POINT('Ctrl Pts',(51.1992556572294,5.03455841516474,338.108239393418));
#16133=CARTESIAN_POINT('Ctrl Pts',(51.1918466638446,5.11735117907148,337.974136142837));
#16134=CARTESIAN_POINT('Ctrl Pts',(51.1844376704598,5.19472798143771,337.836810459366));
#16135=CARTESIAN_POINT('Ctrl Pts',(51.177028677075,5.26644929188387,337.696746635952));
#16136=CARTESIAN_POINT('Ctrl Pts',(51.1696151194948,5.33821478513126,337.55659652839));
#16137=CARTESIAN_POINT('Ctrl Pts',(51.1622015619145,5.40431768784139,337.413705257666));
#16138=CARTESIAN_POINT('Ctrl Pts',(51.1547880043343,5.46456670994654,337.268576918476));
#16139=CARTESIAN_POINT('Ctrl Pts',(51.1473638921976,5.52490150756467,337.123241962527));
#16140=CARTESIAN_POINT('Ctrl Pts',(51.1399397800609,5.579365650904,336.97566392646));
#16141=CARTESIAN_POINT('Ctrl Pts',(51.1325156679242,5.62781751911758,336.826362651286));
#16142=CARTESIAN_POINT('Ctrl Pts',(51.1286585427697,5.65299021535728,336.74879462787));
#16143=CARTESIAN_POINT('Ctrl Pts',(51.1248014176153,5.67654090372352,336.670761653686));
#16144=CARTESIAN_POINT('Ctrl Pts',(51.1209442924608,5.69845519551331,336.592337573264));
#16145=CARTESIAN_POINT('Ctrl Pts',(51.1135203150228,5.74063459112599,336.441391316573));
#16146=CARTESIAN_POINT('Ctrl Pts',(51.1060963375848,5.77687585638018,336.288540259003));
#16147=CARTESIAN_POINT('Ctrl Pts',(51.0986723601468,5.80700530885049,336.134292689513));
#16148=CARTESIAN_POINT('Ctrl Pts',(51.0912571441192,5.83709920403371,335.980227155362));
#16149=CARTESIAN_POINT('Ctrl Pts',(51.0838419280915,5.86109557289093,335.824768752575));
#16150=CARTESIAN_POINT('Ctrl Pts',(51.0764267120639,5.87887037824104,335.668441200361));
#16151=CARTESIAN_POINT('Ctrl Pts',(51.0690186309198,5.89662808076293,335.51226406573));
#16152=CARTESIAN_POINT('Ctrl Pts',(51.0616105497757,5.9081760956172,335.355219814915));
#16153=CARTESIAN_POINT('Ctrl Pts',(51.0542024686316,5.91344137483696,335.197842535534));
#16154=CARTESIAN_POINT('Ctrl Pts',(51.0467999014575,5.91870273501325,335.040582394935));
#16155=CARTESIAN_POINT('Ctrl Pts',(51.0393973342835,5.91769065843273,334.882990090739));
#16156=CARTESIAN_POINT('Ctrl Pts',(51.0319947671094,5.91038390415388,334.725604905257));
#16157=CARTESIAN_POINT('Ctrl Pts',(51.0245960973547,5.90308099684926,334.568302582389));
#16158=CARTESIAN_POINT('Ctrl Pts',(51.0171974276,5.88949002937804,334.411207532932));
#16159=CARTESIAN_POINT('Ctrl Pts',(51.0097987578452,5.86964185086974,334.254859003263));
#16160=CARTESIAN_POINT('Ctrl Pts',(51.0024013086412,5.84979694669454,334.098536266246));
#16161=CARTESIAN_POINT('Ctrl Pts',(50.9950038594373,5.82369692711172,333.94296017448));
#16162=CARTESIAN_POINT('Ctrl Pts',(50.9876064102333,5.79142451609014,333.788664936143));
#16163=CARTESIAN_POINT('Ctrl Pts',(50.9802092817698,5.75915350434404,333.634376387778));
#16164=CARTESIAN_POINT('Ctrl Pts',(50.9728121533063,5.72071070969162,333.481368947727));
#16165=CARTESIAN_POINT('Ctrl Pts',(50.9654150248428,5.67622995164501,333.330166445855));
#16166=CARTESIAN_POINT('Ctrl Pts',(50.9580167574062,5.63174234467205,333.178940662573));
#16167=CARTESIAN_POINT('Ctrl Pts',(50.9506184899696,5.58121502849314,333.029520728898));
#16168=CARTESIAN_POINT('Ctrl Pts',(50.943220222533,5.52483160605675,332.882414987016));
#16169=CARTESIAN_POINT('Ctrl Pts',(50.9358193560073,5.46842837553104,332.735257565339));
#16170=CARTESIAN_POINT('Ctrl Pts',(50.9284184894815,5.40616507613066,332.590416302406));
#16171=CARTESIAN_POINT('Ctrl Pts',(50.9210176229557,5.33827325865388,332.448379107618));
#16172=CARTESIAN_POINT('Ctrl Pts',(50.913608629571,5.2703068894709,332.30618594241));
#16173=CARTESIAN_POINT('Ctrl Pts',(50.9061996361862,5.19669982016629,332.166803331467));
#16174=CARTESIAN_POINT('Ctrl Pts',(50.8987906428014,5.11772967937687,332.030694779696));
#16175=CARTESIAN_POINT('Ctrl Pts',(50.8913770852212,5.03871089025671,331.894502380362));
#16176=CARTESIAN_POINT('Ctrl Pts',(50.8839635276409,4.9543226458939,331.761588373541));
#16177=CARTESIAN_POINT('Ctrl Pts',(50.8765499700607,4.86488533224153,331.632386413699));
#16178=CARTESIAN_POINT('Ctrl Pts',(50.869125857924,4.77532068819956,331.503000511213));
#16179=CARTESIAN_POINT('Ctrl Pts',(50.8617017457873,4.68069284234474,331.377337507796));
#16180=CARTESIAN_POINT('Ctrl Pts',(50.8542776336506,4.58136230090664,331.255797811238));
#16181=CARTESIAN_POINT('Ctrl Pts',(50.8504205084961,4.52975608551756,331.192653045609));
#16182=CARTESIAN_POINT('Ctrl Pts',(50.8465633833414,4.47688112157734,331.130620649466));
#16183=CARTESIAN_POINT('Ctrl Pts',(50.8427062581869,4.4227917199731,331.069752684088));
#16184=CARTESIAN_POINT('Ctrl Pts',(50.8352822807489,4.31868348364384,330.952597449669));
#16185=CARTESIAN_POINT('Ctrl Pts',(50.8278583033109,4.2097599965518,330.839404918701));
#16186=CARTESIAN_POINT('Ctrl Pts',(50.8204343258729,4.09635470019938,330.73059620876));
#16187=CARTESIAN_POINT('Ctrl Pts',(50.8130191098453,3.98308323915932,330.621915909468));
#16188=CARTESIAN_POINT('Ctrl Pts',(50.8056038938176,3.86534076379671,330.517609389007));
#16189=CARTESIAN_POINT('Ctrl Pts',(50.79818867779,3.74350055713083,330.418064367403));
#16190=CARTESIAN_POINT('Ctrl Pts',(50.7907805966459,3.62177758449868,330.318615127518));
#16191=CARTESIAN_POINT('Ctrl Pts',(50.7833725155019,3.49596501705927,330.223918500148));
#16192=CARTESIAN_POINT('Ctrl Pts',(50.7759644343578,3.36647245003869,330.134324938343));
#16193=CARTESIAN_POINT('Ctrl Pts',(50.7685618671839,3.23707626670113,330.044798062663));
#16194=CARTESIAN_POINT('Ctrl Pts',(50.7611593000099,3.10400584330925,329.960366901007));
#16195=CARTESIAN_POINT('Ctrl Pts',(50.7537567328359,2.96770317917187,329.881341151939));
#16196=CARTESIAN_POINT('Ctrl Pts',(50.7463580630812,2.83147227778989,329.802357009582));
#16197=CARTESIAN_POINT('Ctrl Pts',(50.7389593933264,2.69201284687648,329.728772798705));
#16198=CARTESIAN_POINT('Ctrl Pts',(50.7315607235716,2.54979504444844,329.660854394774));
#16199=CARTESIAN_POINT('Ctrl Pts',(50.7241632743677,2.40760070354261,329.592947195271));
#16200=CARTESIAN_POINT('Ctrl Pts',(50.7167658251636,2.26264923069101,329.530704108348));
#16201=CARTESIAN_POINT('Ctrl Pts',(50.7093683759597,2.11543461963498,329.474344660355));
#16202=CARTESIAN_POINT('Ctrl Pts',(50.7019712474962,1.96822639154762,329.417987656009));
#16203=CARTESIAN_POINT('Ctrl Pts',(50.6945741190328,1.8187555689043,329.367513916796));
#16204=CARTESIAN_POINT('Ctrl Pts',(50.6871769905693,1.66753506883221,329.323094385432));
#16205=CARTESIAN_POINT('Ctrl Pts',(50.6797787231327,1.51629128457905,329.278668014569));
#16206=CARTESIAN_POINT('Ctrl Pts',(50.6723804556962,1.36329764457743,329.240297812872));
#16207=CARTESIAN_POINT('Ctrl Pts',(50.6649821882596,1.2090809827058,329.208104477828));
#16208=CARTESIAN_POINT('Ctrl Pts',(50.6575813217338,1.0548101428972,329.175899832926));
#16209=CARTESIAN_POINT('Ctrl Pts',(50.650180455208,0.899315790871016,329.149876451358));
#16210=CARTESIAN_POINT('Ctrl Pts',(50.6427795886822,0.743133525473775,329.13010365289));
#16211=CARTESIAN_POINT('Ctrl Pts',(50.6353705952975,0.586779757018519,329.110309141999));
#16212=CARTESIAN_POINT('Ctrl Pts',(50.6279616019127,0.429736937105505,329.096778968361));
#16213=CARTESIAN_POINT('Ctrl Pts',(50.620552608528,0.272545077685719,329.089530497234));
#16214=CARTESIAN_POINT('Ctrl Pts',(50.6131390509477,0.115256382657845,329.082277560799));
#16215=CARTESIAN_POINT('Ctrl Pts',(50.6057254933675,-0.0421811624949565,
329.081314040133));
#16216=CARTESIAN_POINT('Ctrl Pts',(50.5983119357873,-0.199229509259026,
329.086605191166));
#16217=CARTESIAN_POINT('Ctrl Pts',(50.5908878236506,-0.356501443095588,
329.091903875122));
#16218=CARTESIAN_POINT('Ctrl Pts',(50.5834637115139,-0.513382700708155,
329.103474987807));
#16219=CARTESIAN_POINT('Ctrl Pts',(50.5760395993772,-0.669341480036475,
329.121232055473));
#16220=CARTESIAN_POINT('Ctrl Pts',(50.5721824742225,-0.750368344902806,
329.130457567036));
#16221=CARTESIAN_POINT('Ctrl Pts',(50.5683253490677,-0.831146387179152,
329.141351963281));
#16222=CARTESIAN_POINT('Ctrl Pts',(50.564468223913,-0.911602436687748,329.153897746368));
#16223=CARTESIAN_POINT('Ctrl Pts',(50.557044246475,-1.06645971311497,329.178045163639));
#16224=CARTESIAN_POINT('Ctrl Pts',(50.549620269037,-1.22059047615725,329.208386274223));
#16225=CARTESIAN_POINT('Ctrl Pts',(50.542196291599,-1.37346015472957,329.24486857093));
#16226=CARTESIAN_POINT('Ctrl Pts',(50.5347810755714,-1.52614942408015,329.281307813038));
#16227=CARTESIAN_POINT('Ctrl Pts',(50.5273658595438,-1.67758021189812,329.323873729168));
#16228=CARTESIAN_POINT('Ctrl Pts',(50.5199506435162,-1.82722447128094,329.372462235218));
#16229=CARTESIAN_POINT('Ctrl Pts',(50.5125425623721,-1.97672474371095,329.421003989652));
#16230=CARTESIAN_POINT('Ctrl Pts',(50.505134481228,-2.12444155729559,329.475556682944));
#16231=CARTESIAN_POINT('Ctrl Pts',(50.4977264000839,-2.26985855310917,329.535965527984));
#16232=CARTESIAN_POINT('Ctrl Pts',(50.4903238329099,-2.41516731239723,329.596329409618));
#16233=CARTESIAN_POINT('Ctrl Pts',(50.4829212657359,-2.55817931917107,329.662540621351));
#16234=CARTESIAN_POINT('Ctrl Pts',(50.4755186985619,-2.69839495011332,329.734395072197));
#16235=CARTESIAN_POINT('Ctrl Pts',(50.4681200288071,-2.83853675813838,329.806211691989));
#16236=CARTESIAN_POINT('Ctrl Pts',(50.4607213590524,-2.97588479116169,329.883665463913));
#16237=CARTESIAN_POINT('Ctrl Pts',(50.4533226892977,-3.10996103935167,329.966504902534));
#16238=CARTESIAN_POINT('Ctrl Pts',(50.4459252400937,-3.24401516912417,330.049330675219));
#16239=CARTESIAN_POINT('Ctrl Pts',(50.4385277908898,-3.37479826808915,330.137540155303));
#16240=CARTESIAN_POINT('Ctrl Pts',(50.4311303416858,-3.50185840349794,330.230836731213));
#16241=CARTESIAN_POINT('Ctrl Pts',(50.4237332132223,-3.6289130298004,330.324129261945));
#16242=CARTESIAN_POINT('Ctrl Pts',(50.4163360847588,-3.75224471268036,330.422508229055));
#16243=CARTESIAN_POINT('Ctrl Pts',(50.4089389562954,-3.87143213387249,330.5256348165));
#16244=CARTESIAN_POINT('Ctrl Pts',(50.4015406888588,-3.99063790695293,330.628777282865));
#16245=CARTESIAN_POINT('Ctrl Pts',(50.3941424214222,-4.10569786553179,330.7366685809));
#16246=CARTESIAN_POINT('Ctrl Pts',(50.3867441539855,-4.21622541247485,330.848931001091));
#16247=CARTESIAN_POINT('Ctrl Pts',(50.3793432874598,-4.32679178890742,330.961232860252));
#16248=CARTESIAN_POINT('Ctrl Pts',(50.371942420934,-4.43282232179738,331.077908633209));
#16249=CARTESIAN_POINT('Ctrl Pts',(50.3645415544083,-4.53396887540603,331.198545436369));
#16250=CARTESIAN_POINT('Ctrl Pts',(50.3571325610235,-4.63522649760047,331.319314710273));
#16251=CARTESIAN_POINT('Ctrl Pts',(50.3497235676387,-4.73158919023638,331.444053414583));
#16252=CARTESIAN_POINT('Ctrl Pts',(50.342314574254,-4.82275011904547,331.572316839067));
#16253=CARTESIAN_POINT('Ctrl Pts',(50.3349010166737,-4.91396720613118,331.700659278244));
#16254=CARTESIAN_POINT('Ctrl Pts',(50.3274874590935,-4.99997594066146,331.832530452426));
#16255=CARTESIAN_POINT('Ctrl Pts',(50.3200739015133,-5.08051437074151,331.96745910313));
#16256=CARTESIAN_POINT('Ctrl Pts',(50.3126497893766,-5.16116746202119,332.10257984947));
#16257=CARTESIAN_POINT('Ctrl Pts',(50.3052256772399,-5.23633451684443,332.240766438935));
#16258=CARTESIAN_POINT('Ctrl Pts',(50.2978015651032,-5.3058004642216,332.381524871921));
#16259=CARTESIAN_POINT('Ctrl Pts',(50.2939444399485,-5.34189082062931,332.454654544886));
#16260=CARTESIAN_POINT('Ctrl Pts',(50.2900873147938,-5.37644312412405,332.528478106887));
#16261=CARTESIAN_POINT('Ctrl Pts',(50.2862301896391,-5.40943249242955,332.602924558478));
#16262=CARTESIAN_POINT('Ctrl Pts',(50.2780661846716,-5.47925790797001,332.760498185523));
#16263=CARTESIAN_POINT('Ctrl Pts',(50.2699021797042,-5.54225998356434,332.921272647656));
#16264=CARTESIAN_POINT('Ctrl Pts',(50.2617381747368,-5.59816281199632,333.084666166727));
#16265=CARTESIAN_POINT('Ctrl Pts',(50.2536045243065,-5.653857788462,333.247452173348));
#16266=CARTESIAN_POINT('Ctrl Pts',(50.2454708738763,-5.70250608800867,333.412837577739));
#16267=CARTESIAN_POINT('Ctrl Pts',(50.237337223446,-5.74388052029439,333.580222858656));
#16268=CARTESIAN_POINT('Ctrl Pts',(50.2292225881197,-5.78515822613071,333.747216820998));
#16269=CARTESIAN_POINT('Ctrl Pts',(50.2211079527933,-5.81919591411558,333.916201097296));
#16270=CARTESIAN_POINT('Ctrl Pts',(50.2129933174669,-5.84581534515739,334.08655951873));
#16271=CARTESIAN_POINT('Ctrl Pts',(50.2049101411301,-5.87233157742681,334.256257491039));
#16272=CARTESIAN_POINT('Ctrl Pts',(50.1968269647934,-5.8914868647934,334.427318739594));
#16273=CARTESIAN_POINT('Ctrl Pts',(50.1887437884566,-5.90315367809505,334.599116955593));
#16274=CARTESIAN_POINT('Ctrl Pts',(50.1825132123242,-5.91214654989078,334.731540376734));
#16275=CARTESIAN_POINT('Ctrl Pts',(50.1762826361917,-5.91669114572374,334.864401284286));
#16276=CARTESIAN_POINT('Ctrl Pts',(50.1700520600592,-5.91674943187699,334.997407147659));
#16277=CARTESIAN_POINT('',(48.4200519872132,-5.9145671363793,335.005177061859));
#16278=CARTESIAN_POINT('Ctrl Pts',(50.1700520047037,-5.9080523696217,334.99741213886));
#16279=CARTESIAN_POINT('Ctrl Pts',(50.1160320549241,-5.90352393792915,336.148898367647));
#16280=CARTESIAN_POINT('Ctrl Pts',(49.96926609372,-5.02192580754506,339.283759072858));
#16281=CARTESIAN_POINT('Ctrl Pts',(49.729754121091,0.0702832997843916,341.996262086213));
#16282=CARTESIAN_POINT('Ctrl Pts',(49.4515160868174,5.92134037336825,338.726976134069));
#16283=CARTESIAN_POINT('Ctrl Pts',(49.1732780525432,6.33847078515738,332.037499193767));
#16284=CARTESIAN_POINT('Ctrl Pts',(48.8950400182694,0.938880113080063,328.066665516904));
#16285=CARTESIAN_POINT('Ctrl Pts',(48.6439646689894,-4.71106541156814,330.224955150084));
#16286=CARTESIAN_POINT('Ctrl Pts',(48.4856353311342,-5.90162062968873,333.610301631254));
#16287=CARTESIAN_POINT('Ctrl Pts',(48.4200520047037,-5.91326451545619,335.005175549532));
#16288=CARTESIAN_POINT('',(46.6700520047037,-5.92206232538312,335.000121321822));
#16289=CARTESIAN_POINT('Ctrl Pts',(48.4200519579342,-5.91674773286061,335.005179593505));
#16290=CARTESIAN_POINT('Ctrl Pts',(48.4110676566621,-5.91658035782511,335.196375265698));
#16291=CARTESIAN_POINT('Ctrl Pts',(48.40208335539,-5.90714176842452,335.387163876296));
#16292=CARTESIAN_POINT('Ctrl Pts',(48.3930990541179,-5.88857245527102,335.576753848295));
#16293=CARTESIAN_POINT('Ctrl Pts',(48.3839905901862,-5.86974651500326,335.768963945606));
#16294=CARTESIAN_POINT('Ctrl Pts',(48.3748821262545,-5.84153578648773,335.959942063276));
#16295=CARTESIAN_POINT('Ctrl Pts',(48.3657736623228,-5.80413574004996,336.148885927138));
#16296=CARTESIAN_POINT('Ctrl Pts',(48.3567037581224,-5.76689402280502,336.337029916873));
#16297=CARTESIAN_POINT('Ctrl Pts',(48.347633853922,-5.72054076236795,336.523156929097));
#16298=CARTESIAN_POINT('Ctrl Pts',(48.3385639497216,-5.6653156537755,336.706496148717));
#16299=CARTESIAN_POINT('Ctrl Pts',(48.3311399722836,-5.62011231412162,336.856564572802));
#16300=CARTESIAN_POINT('Ctrl Pts',(48.3237159948457,-5.5688739263724,337.005062056713));
#16301=CARTESIAN_POINT('Ctrl Pts',(48.3162920174077,-5.5117259760806,337.151466320233));
#16302=CARTESIAN_POINT('Ctrl Pts',(48.3088768013801,-5.45464546896845,337.297697804695));
#16303=CARTESIAN_POINT('Ctrl Pts',(48.3014615853525,-5.39166941590445,337.441840641686));
#16304=CARTESIAN_POINT('Ctrl Pts',(48.2940463693249,-5.3229734930756,337.583386102485));
#16305=CARTESIAN_POINT('Ctrl Pts',(48.2866382881809,-5.25434366911781,337.724795368956));
#16306=CARTESIAN_POINT('Ctrl Pts',(48.2792302070368,-5.18000509395967,337.863611901128));
#16307=CARTESIAN_POINT('Ctrl Pts',(48.2718221258927,-5.10018205904981,337.99934551645));
#16308=CARTESIAN_POINT('Ctrl Pts',(48.2644195587187,-5.02041843788275,338.134978102762));
#16309=CARTESIAN_POINT('Ctrl Pts',(48.2570169915448,-4.93517867356555,338.267532020922));
#16310=CARTESIAN_POINT('Ctrl Pts',(48.2496144243708,-4.84473359315843,338.396540441953));
#16311=CARTESIAN_POINT('Ctrl Pts',(48.2422157546161,-4.75433613169079,338.525480940614));
#16312=CARTESIAN_POINT('Ctrl Pts',(48.2348170848613,-4.65873902585754,338.650879354946));
#16313=CARTESIAN_POINT('Ctrl Pts',(48.2274184151066,-4.55825707656579,338.77229677868));
#16314=CARTESIAN_POINT('Ctrl Pts',(48.2200209659027,-4.45779170367561,338.893694172309));
#16315=CARTESIAN_POINT('Ctrl Pts',(48.2126235166987,-4.35244332438794,339.011111591514));
#16316=CARTESIAN_POINT('Ctrl Pts',(48.2052260674948,-4.24256785314958,339.124142162186));
#16317=CARTESIAN_POINT('Ctrl Pts',(48.1978289390313,-4.1326971459201,339.23716783205));
#16318=CARTESIAN_POINT('Ctrl Pts',(48.1904318105679,-4.01829999716163,339.345806763964));
#16319=CARTESIAN_POINT('Ctrl Pts',(48.1830346821044,-3.8997699172604,339.449688208732));
#16320=CARTESIAN_POINT('Ctrl Pts',(48.1756364146678,-3.78122158668578,339.553585648649));
#16321=CARTESIAN_POINT('Ctrl Pts',(48.1682381472313,-3.65853933856589,339.652723896846));
#16322=CARTESIAN_POINT('Ctrl Pts',(48.1608398797947,-3.53215043519213,339.746771941612));
#16323=CARTESIAN_POINT('Ctrl Pts',(48.153439013269,-3.40571713006748,339.840853026444));
#16324=CARTESIAN_POINT('Ctrl Pts',(48.1460381467432,-3.27557487626077,339.9298401248));
#16325=CARTESIAN_POINT('Ctrl Pts',(48.1386372802175,-3.14218048978496,340.01344515599));
#16326=CARTESIAN_POINT('Ctrl Pts',(48.1312282868328,-3.00863962351961,340.097141993496));
#16327=CARTESIAN_POINT('Ctrl Pts',(48.123819293448,-2.87183980922479,340.175444762883));
#16328=CARTESIAN_POINT('Ctrl Pts',(48.1164103000633,-2.73226371059572,340.248110667494));
#16329=CARTESIAN_POINT('Ctrl Pts',(48.1089967424831,-2.5926016282755,340.320821336808));
#16330=CARTESIAN_POINT('Ctrl Pts',(48.1015831849028,-2.45016019051551,340.387888063315));
#16331=CARTESIAN_POINT('Ctrl Pts',(48.0941696273226,-2.30544218820852,340.449116155793));
#16332=CARTESIAN_POINT('Ctrl Pts',(48.0867455151859,-2.16051815333116,340.510431417671));
#16333=CARTESIAN_POINT('Ctrl Pts',(48.0793214030493,-2.01331142907448,340.565891312841));
#16334=CARTESIAN_POINT('Ctrl Pts',(48.0718972909127,-1.86434088783647,340.615350711794));
#16335=CARTESIAN_POINT('Ctrl Pts',(48.0680401657576,-1.78694469400318,340.64104686082));
#16336=CARTESIAN_POINT('Ctrl Pts',(48.0641830406026,-1.70907260219412,340.665124180061));
#16337=CARTESIAN_POINT('Ctrl Pts',(48.0603259154475,-1.63079835804735,340.687567782268));
#16338=CARTESIAN_POINT('Ctrl Pts',(48.0529019380095,-1.48014049781042,340.730765964779));
#16339=CARTESIAN_POINT('Ctrl Pts',(48.0454779605715,-1.32753776386418,340.768039020726));
#16340=CARTESIAN_POINT('Ctrl Pts',(48.0380539831335,-1.173497260219,340.799209837793));
#16341=CARTESIAN_POINT('Ctrl Pts',(48.0306387671058,-1.01963854754477,340.830343868607));
#16342=CARTESIAN_POINT('Ctrl Pts',(48.0232235510782,-0.864345804888217,
340.85538992206));
#16343=CARTESIAN_POINT('Ctrl Pts',(48.0158083350505,-0.70814190154676,340.874220425705));
#16344=CARTESIAN_POINT('Ctrl Pts',(48.0084002539064,-0.552088296814716,
340.893032810735));
#16345=CARTESIAN_POINT('Ctrl Pts',(48.0009921727623,-0.395125644824597,
340.90564150779));
#16346=CARTESIAN_POINT('Ctrl Pts',(47.9935840916182,-0.237787527515724,
340.911969862428));
#16347=CARTESIAN_POINT('Ctrl Pts',(47.9861815244442,-0.0805665198410168,
340.918293506756));
#16348=CARTESIAN_POINT('Ctrl Pts',(47.9787789572701,0.0770290253830899,
340.918346101489));
#16349=CARTESIAN_POINT('Ctrl Pts',(47.9713763900961,0.234459981648922,340.912102762935));
#16350=CARTESIAN_POINT('Ctrl Pts',(47.9639777203413,0.391808051204665,340.905862711471));
#16351=CARTESIAN_POINT('Ctrl Pts',(47.9565790505866,0.548991332402498,340.893333343055));
#16352=CARTESIAN_POINT('Ctrl Pts',(47.9491803808318,0.705470382763265,340.87454186312));
#16353=CARTESIAN_POINT('Ctrl Pts',(47.9417829316278,0.861923618939321,340.855753483195));
#16354=CARTESIAN_POINT('Ctrl Pts',(47.9343854824238,1.01767248466195,340.830705086484));
#16355=CARTESIAN_POINT('Ctrl Pts',(47.9269880332198,1.1721822250829,340.799475786112));
#16356=CARTESIAN_POINT('Ctrl Pts',(47.9195909047563,1.32668526623088,340.768247839788));
#16357=CARTESIAN_POINT('Ctrl Pts',(47.9121937762928,1.47994892308881,340.7308395966));
#16358=CARTESIAN_POINT('Ctrl Pts',(47.9047966478293,1.63144847369738,340.687381334162));
#16359=CARTESIAN_POINT('Ctrl Pts',(47.8973983803927,1.7829713514548,340.643916380236));
#16360=CARTESIAN_POINT('Ctrl Pts',(47.8900001129561,1.93272922334991,340.594399655131));
#16361=CARTESIAN_POINT('Ctrl Pts',(47.8826018455195,2.08021251843005,340.539011323392));
#16362=CARTESIAN_POINT('Ctrl Pts',(47.8752009789937,2.22774762594272,340.48360353315));
#16363=CARTESIAN_POINT('Ctrl Pts',(47.867800112468,2.37300621650351,340.422320160459));
#16364=CARTESIAN_POINT('Ctrl Pts',(47.8603992459422,2.51549882755647,340.355389454658));
#16365=CARTESIAN_POINT('Ctrl Pts',(47.8529902525574,2.65814790911929,340.288385252543));
#16366=CARTESIAN_POINT('Ctrl Pts',(47.8455812591727,2.79802460750033,340.215721491733));
#16367=CARTESIAN_POINT('Ctrl Pts',(47.8381722657879,2.93466355279005,340.137672663223));
#16368=CARTESIAN_POINT('Ctrl Pts',(47.8307587082076,3.07138667238326,340.059575753942));
#16369=CARTESIAN_POINT('Ctrl Pts',(47.8233451506274,3.20486774876914,339.976087364074));
#16370=CARTESIAN_POINT('Ctrl Pts',(47.8159315930471,3.33467097294413,339.887524942617));
#16371=CARTESIAN_POINT('Ctrl Pts',(47.8085074809104,3.46465899577239,339.798836436339));
#16372=CARTESIAN_POINT('Ctrl Pts',(47.8010833687737,3.59095841002202,339.705059692958));
#16373=CARTESIAN_POINT('Ctrl Pts',(47.793659256637,3.71316638156332,339.606552505435));
#16374=CARTESIAN_POINT('Ctrl Pts',(47.7898021314825,3.7766583429496,339.555374055555));
#16375=CARTESIAN_POINT('Ctrl Pts',(47.7859450063281,3.83904653153453,339.502919371229));
#16376=CARTESIAN_POINT('Ctrl Pts',(47.7820878811736,3.90027852031823,339.449242410393));
#16377=CARTESIAN_POINT('Ctrl Pts',(47.7746639037356,4.0181344065045,339.345928016844));
#16378=CARTESIAN_POINT('Ctrl Pts',(47.7672399262975,4.13206021011723,339.237771711533));
#16379=CARTESIAN_POINT('Ctrl Pts',(47.7598159488595,4.24163257055394,339.125104083404));
#16380=CARTESIAN_POINT('Ctrl Pts',(47.7524007328319,4.35107561911929,339.012569420028));
#16381=CARTESIAN_POINT('Ctrl Pts',(47.7449855168043,4.45617519354885,338.895534296369));
#16382=CARTESIAN_POINT('Ctrl Pts',(47.7375703007767,4.55654106087152,338.774369367602));
#16383=CARTESIAN_POINT('Ctrl Pts',(47.7301622196326,4.656810356662,338.653321023119));
#16384=CARTESIAN_POINT('Ctrl Pts',(47.7227541384885,4.75235477651703,338.528151069873));
#16385=CARTESIAN_POINT('Ctrl Pts',(47.7153460573444,4.84282110827666,338.399266726182));
#16386=CARTESIAN_POINT('Ctrl Pts',(47.7079434901704,4.93322010429331,338.270478313462));
#16387=CARTESIAN_POINT('Ctrl Pts',(47.7005409229964,5.01854832467766,338.137981319358));
#16388=CARTESIAN_POINT('Ctrl Pts',(47.6931383558224,5.0984930919132,338.002215640858));
#16389=CARTESIAN_POINT('Ctrl Pts',(47.6857396860676,5.17839576857824,337.866521442394));
#16390=CARTESIAN_POINT('Ctrl Pts',(47.6783410163129,5.2529204480056,337.727562307692));
#16391=CARTESIAN_POINT('Ctrl Pts',(47.6709423465581,5.32179808454506,337.585806587862));
#16392=CARTESIAN_POINT('Ctrl Pts',(47.6635448973541,5.39066435841326,337.444074253324));
#16393=CARTESIAN_POINT('Ctrl Pts',(47.6561474481502,5.4538852753457,337.299546584645));
#16394=CARTESIAN_POINT('Ctrl Pts',(47.6487499989462,5.51123797672396,337.152716081237));
#16395=CARTESIAN_POINT('Ctrl Pts',(47.6413528704827,5.56858819138904,337.005891944143));
#16396=CARTESIAN_POINT('Ctrl Pts',(47.6339557420192,5.62007056061471,336.856765518481));
#16397=CARTESIAN_POINT('Ctrl Pts',(47.6265586135557,5.66551068046576,336.705848554834));
#16398=CARTESIAN_POINT('Ctrl Pts',(47.6191603461191,5.71095779696097,336.554908353741));
#16399=CARTESIAN_POINT('Ctrl Pts',(47.6117620786826,5.75036070401466,336.402177423098));
#16400=CARTESIAN_POINT('Ctrl Pts',(47.604363811246,5.78359514775494,336.248181769361));
#16401=CARTESIAN_POINT('Ctrl Pts',(47.5969629447202,5.81684126710482,336.094132015332));
#16402=CARTESIAN_POINT('Ctrl Pts',(47.5895620781944,5.84391452987427,335.938817018171));
#16403=CARTESIAN_POINT('Ctrl Pts',(47.5821612116687,5.8647419995275,335.782771896199));
#16404=CARTESIAN_POINT('Ctrl Pts',(47.5747522182839,5.88559233973358,335.626555421763));
#16405=CARTESIAN_POINT('Ctrl Pts',(47.5673432248992,5.90018314067225,335.469607591536));
#16406=CARTESIAN_POINT('Ctrl Pts',(47.5599342315144,5.90849338931678,335.312468287831));
#16407=CARTESIAN_POINT('Ctrl Pts',(47.5525206739342,5.91680875736113,335.155232180894));
#16408=CARTESIAN_POINT('Ctrl Pts',(47.5451071163539,5.91883585874994,334.997804737747));
#16409=CARTESIAN_POINT('Ctrl Pts',(47.5376935587736,5.9146058018589,334.840724229347));
#16410=CARTESIAN_POINT('Ctrl Pts',(47.530269446637,5.91036972270746,334.683420088086));
#16411=CARTESIAN_POINT('Ctrl Pts',(47.5228453345002,5.89985871866828,334.526464239412));
#16412=CARTESIAN_POINT('Ctrl Pts',(47.5154212223635,5.88315566881497,334.370389057441));
#16413=CARTESIAN_POINT('Ctrl Pts',(47.5115640972089,5.87447776194045,334.289301716718));
#16414=CARTESIAN_POINT('Ctrl Pts',(47.5077069720543,5.86412932749561,334.208451918402));
#16415=CARTESIAN_POINT('Ctrl Pts',(47.5038498468997,5.8521273686027,334.127912949213));
#16416=CARTESIAN_POINT('Ctrl Pts',(47.4964258694617,5.82902667353565,333.972896073645));
#16417=CARTESIAN_POINT('Ctrl Pts',(47.4890018920237,5.79972751838205,333.818563852076));
#16418=CARTESIAN_POINT('Ctrl Pts',(47.4815779145857,5.76427879772342,333.665451198114));
#16419=CARTESIAN_POINT('Ctrl Pts',(47.4741626985581,5.72887191188869,333.51251924012));
#16420=CARTESIAN_POINT('Ctrl Pts',(47.4667474825304,5.68732998990494,333.360804344895));
#16421=CARTESIAN_POINT('Ctrl Pts',(47.4593322665028,5.6397535461651,333.210835250454));
#16422=CARTESIAN_POINT('Ctrl Pts',(47.4519241853587,5.5922228802399,333.06101045552));
#16423=CARTESIAN_POINT('Ctrl Pts',(47.4445161042147,5.53866936409267,332.912928470562));
#16424=CARTESIAN_POINT('Ctrl Pts',(47.4371080230706,5.47924429292858,332.767106688418));
#16425=CARTESIAN_POINT('Ctrl Pts',(47.4297054558966,5.41986345293028,332.621393444089));
#16426=CARTESIAN_POINT('Ctrl Pts',(47.4223028887226,5.35461990007123,332.477937396985));
#16427=CARTESIAN_POINT('Ctrl Pts',(47.4149003215486,5.28371434536787,332.3372395378));
#16428=CARTESIAN_POINT('Ctrl Pts',(47.4075016517939,5.21284612212912,332.196615755424));
#16429=CARTESIAN_POINT('Ctrl Pts',(47.4001029820392,5.13632200145885,332.058747601318));
#16430=CARTESIAN_POINT('Ctrl Pts',(47.3927043122845,5.05439023375785,331.924114773371));
#16431=CARTESIAN_POINT('Ctrl Pts',(47.3853068630805,4.9724719822544,331.78950415566));
#16432=CARTESIAN_POINT('Ctrl Pts',(47.3779094138765,4.88514804806749,331.658128123334));
#16433=CARTESIAN_POINT('Ctrl Pts',(47.3705119646725,4.79271198287325,331.530440602652));
#16434=CARTESIAN_POINT('Ctrl Pts',(47.3631148362091,4.70027992554565,331.402758618279));
#16435=CARTESIAN_POINT('Ctrl Pts',(47.3557177077456,4.60273639677976,331.278765129871));
#16436=CARTESIAN_POINT('Ctrl Pts',(47.3483205792821,4.50041735858163,331.158883735022));
#16437=CARTESIAN_POINT('Ctrl Pts',(47.3409223118455,4.39808256580584,331.038983881432));
#16438=CARTESIAN_POINT('Ctrl Pts',(47.333524044409,4.29097104180144,330.923197665996));
#16439=CARTESIAN_POINT('Ctrl Pts',(47.3261257769724,4.17945787572152,330.811914228723));
#16440=CARTESIAN_POINT('Ctrl Pts',(47.3187249104466,4.06790553389365,330.700591696409));
#16441=CARTESIAN_POINT('Ctrl Pts',(47.3113240439209,3.95194873522945,330.593775355227));
#16442=CARTESIAN_POINT('Ctrl Pts',(47.3039231773951,3.83199800199564,330.491816122295));
#16443=CARTESIAN_POINT('Ctrl Pts',(47.2965141840104,3.71191555138892,330.389744928377));
#16444=CARTESIAN_POINT('Ctrl Pts',(47.2891051906257,3.58783069222419,330.292541735986));
#16445=CARTESIAN_POINT('Ctrl Pts',(47.2816961972409,3.46018605170202,330.200516376723));
#16446=CARTESIAN_POINT('Ctrl Pts',(47.2742826396607,3.33246277767837,330.108434326664));
#16447=CARTESIAN_POINT('Ctrl Pts',(47.2668690820805,3.20117566304607,330.021536671188));
#16448=CARTESIAN_POINT('Ctrl Pts',(47.2594555245003,3.06679418586286,329.940088539899));
#16449=CARTESIAN_POINT('Ctrl Pts',(47.2520314123636,2.93222139204506,329.858524452284));
#16450=CARTESIAN_POINT('Ctrl Pts',(47.2446073002269,2.79454576298211,329.782425563981));
#16451=CARTESIAN_POINT('Ctrl Pts',(47.2371831880902,2.65425983404841,329.71201027839));
#16452=CARTESIAN_POINT('Ctrl Pts',(47.2333260629354,2.58137564596042,329.675426702558));
#16453=CARTESIAN_POINT('Ctrl Pts',(47.2294689377806,2.50778719402751,329.640376456826));
#16454=CARTESIAN_POINT('Ctrl Pts',(47.2256118126258,2.43356530797972,329.606884902554));
#16455=CARTESIAN_POINT('Ctrl Pts',(47.2181878351878,2.29070719855655,329.542422243632));
#16456=CARTESIAN_POINT('Ctrl Pts',(47.2107638577498,2.1450704868661,329.483542507598));
#16457=CARTESIAN_POINT('Ctrl Pts',(47.2033398803118,1.9971314528381,329.430494050404));
#16458=CARTESIAN_POINT('Ctrl Pts',(47.1959246642841,1.84936700912889,329.377508198371));
#16459=CARTESIAN_POINT('Ctrl Pts',(47.1885094482565,1.69930599937836,329.33034005162));
#16460=CARTESIAN_POINT('Ctrl Pts',(47.1810942322289,1.54744744476871,329.289191215933));
#16461=CARTESIAN_POINT('Ctrl Pts',(47.1736861510848,1.3957350076958,329.248081973448));
#16462=CARTESIAN_POINT('Ctrl Pts',(47.1662780699407,1.24222882686587,329.212980608687));
#16463=CARTESIAN_POINT('Ctrl Pts',(47.1588699887966,1.08744586347258,329.184039885237));
#16464=CARTESIAN_POINT('Ctrl Pts',(47.1514674216226,0.932778107865729,329.155120702896));
#16465=CARTESIAN_POINT('Ctrl Pts',(47.1440648544486,0.776835827228476,329.132353099811));
#16466=CARTESIAN_POINT('Ctrl Pts',(47.1366622872746,0.620148931572908,329.115839408618));
#16467=CARTESIAN_POINT('Ctrl Pts',(47.1292636175198,0.463544530882996,329.099334411812));
#16468=CARTESIAN_POINT('Ctrl Pts',(47.1218649477651,0.306196666159692,329.089076808395));
#16469=CARTESIAN_POINT('Ctrl Pts',(47.1144662780104,0.148643068126189,329.08511743136));
#16470=CARTESIAN_POINT('Ctrl Pts',(47.1070688288064,-0.00888453845582626,
329.0811587075));
#16471=CARTESIAN_POINT('Ctrl Pts',(47.0996713796024,-0.166617438258161,
329.083496157286));
#16472=CARTESIAN_POINT('Ctrl Pts',(47.0922739303984,-0.324015057350487,
329.092128572395));
#16473=CARTESIAN_POINT('Ctrl Pts',(47.0848768019349,-0.481405851956453,
329.100760613218));
#16474=CARTESIAN_POINT('Ctrl Pts',(47.0774796734715,-0.638461022105863,
329.115687056235));
#16475=CARTESIAN_POINT('Ctrl Pts',(47.070082545008,-0.794642547225585,329.136854616792));
#16476=CARTESIAN_POINT('Ctrl Pts',(47.0626842775714,-0.95084812040125,329.158025436624));
#16477=CARTESIAN_POINT('Ctrl Pts',(47.0552860101348,-1.10617941084858,329.1854392373));
#16478=CARTESIAN_POINT('Ctrl Pts',(47.0478877426982,-1.26010620016897,329.218991184335));
#16479=CARTESIAN_POINT('Ctrl Pts',(47.0404868761725,-1.41408706558918,329.252554918522));
#16480=CARTESIAN_POINT('Ctrl Pts',(47.0330860096467,-1.56666208307261,329.292261013015));
#16481=CARTESIAN_POINT('Ctrl Pts',(47.0256851431209,-1.7173140017749,329.337954152269));
#16482=CARTESIAN_POINT('Ctrl Pts',(47.0182761497362,-1.86813135068703,329.383697466958));
#16483=CARTESIAN_POINT('Ctrl Pts',(47.0108671563515,-2.01702102618953,329.435440847344));
#16484=CARTESIAN_POINT('Ctrl Pts',(47.0034581629667,-2.16348295330334,329.492979746427));
#16485=CARTESIAN_POINT('Ctrl Pts',(46.9960446053865,-2.31003510601626,329.550554091456));
#16486=CARTESIAN_POINT('Ctrl Pts',(46.9886310478062,-2.45415618936657,329.613930919474));
#16487=CARTESIAN_POINT('Ctrl Pts',(46.981217490226,-2.59536918869862,329.682858913208));
#16488=CARTESIAN_POINT('Ctrl Pts',(46.9737933780893,-2.73678323058761,329.751885038559));
#16489=CARTESIAN_POINT('Ctrl Pts',(46.9663692659526,-2.87528059197245,329.826477937205));
#16490=CARTESIAN_POINT('Ctrl Pts',(46.9589451538159,-3.01041107362125,329.906341616253));
#16491=CARTESIAN_POINT('Ctrl Pts',(46.9550880286612,-3.08061679928056,329.947834012883));
#16492=CARTESIAN_POINT('Ctrl Pts',(46.9512309035065,-3.14991423252374,329.990748412904));
#16493=CARTESIAN_POINT('Ctrl Pts',(46.9473737783518,-3.21824371641076,330.035038978574));
#16494=CARTESIAN_POINT('Ctrl Pts',(46.9399541975366,-3.349682574999,330.120236481418));
#16495=CARTESIAN_POINT('Ctrl Pts',(46.9325346167214,-3.4779353625985,330.210786306678));
#16496=CARTESIAN_POINT('Ctrl Pts',(46.9251150359061,-3.60253581249218,330.306422869259));
#16497=CARTESIAN_POINT('Ctrl Pts',(46.9177042145106,-3.72698916140179,330.401946525086));
#16498=CARTESIAN_POINT('Ctrl Pts',(46.9102933931151,-3.84779846173344,330.502544739512));
#16499=CARTESIAN_POINT('Ctrl Pts',(46.9028825717195,-3.96452442672832,330.607907488181));
#16500=CARTESIAN_POINT('Ctrl Pts',(46.8954788788627,-4.08113811192175,330.713168887434));
#16501=CARTESIAN_POINT('Ctrl Pts',(46.8880751860059,-4.19367600557905,330.823185448392));
#16502=CARTESIAN_POINT('Ctrl Pts',(46.880671493149,-4.30173016544464,330.937605614148));
#16503=CARTESIAN_POINT('Ctrl Pts',(46.8732733035934,-4.40970400666335,331.051940729288));
#16504=CARTESIAN_POINT('Ctrl Pts',(46.8658751140378,-4.51320049464683,331.170672661232));
#16505=CARTESIAN_POINT('Ctrl Pts',(46.8584769244822,-4.61184707517202,331.293411660607));
#16506=CARTESIAN_POINT('Ctrl Pts',(46.8510826173692,-4.7104418876698,331.416086248667));
#16507=CARTESIAN_POINT('Ctrl Pts',(46.8436883102561,-4.80419162790907,331.542763425736));
#16508=CARTESIAN_POINT('Ctrl Pts',(46.836294003143,-4.89276280918619,331.673018987799));
#16509=CARTESIAN_POINT('Ctrl Pts',(46.8289008955166,-4.98131962266,331.80325342012));
#16510=CARTESIAN_POINT('Ctrl Pts',(46.8215077878902,-5.06469933431005,331.937064776745));
#16511=CARTESIAN_POINT('Ctrl Pts',(46.8141146802638,-5.14261067861065,332.073998296183));
#16512=CARTESIAN_POINT('Ctrl Pts',(46.8067218718188,-5.22051887002503,332.210926274248));
#16513=CARTESIAN_POINT('Ctrl Pts',(46.7993290633738,-5.29295894924627,332.350975839106));
#16514=CARTESIAN_POINT('Ctrl Pts',(46.7919362549288,-5.35968482578323,332.493666197258));
#16515=CARTESIAN_POINT('Ctrl Pts',(46.7845422820638,-5.42642121212097,332.636379030158));
#16516=CARTESIAN_POINT('Ctrl Pts',(46.7771483091989,-5.48744144545509,332.781733145974));
#16517=CARTESIAN_POINT('Ctrl Pts',(46.7697543363339,-5.54254701029076,332.929226424445));
#16518=CARTESIAN_POINT('Ctrl Pts',(46.7623577350253,-5.59767216430661,333.076772134507));
#16519=CARTESIAN_POINT('Ctrl Pts',(46.7549611337168,-5.64687833301567,333.226458171368));
#16520=CARTESIAN_POINT('Ctrl Pts',(46.7475645324083,-5.69001647333298,333.377766016969));
#16521=CARTESIAN_POINT('Ctrl Pts',(46.7401598047119,-5.73320200802044,333.529240099224));
#16522=CARTESIAN_POINT('Ctrl Pts',(46.7327550770155,-5.77030609846415,333.68233918891));
#16523=CARTESIAN_POINT('Ctrl Pts',(46.7253503493191,-5.80123040153664,333.836532600033));
#16524=CARTESIAN_POINT('Ctrl Pts',(46.717941023626,-5.83217390718474,333.9908217582));
#16525=CARTESIAN_POINT('Ctrl Pts',(46.7105316979329,-5.85692992065084,334.146206223648));
#16526=CARTESIAN_POINT('Ctrl Pts',(46.7031223722398,-5.87545190896669,334.302149422928));
#16527=CARTESIAN_POINT('Ctrl Pts',(46.6957025664195,-5.89400009572497,334.458313196202));
#16528=CARTESIAN_POINT('Ctrl Pts',(46.6882827605993,-5.90629661854936,334.615036910139));
#16529=CARTESIAN_POINT('Ctrl Pts',(46.6808629547791,-5.91234702142441,334.77178242672));
#16530=CARTESIAN_POINT('Ctrl Pts',(46.677259304754,-5.91528558006071,334.847910562476));
#16531=CARTESIAN_POINT('Ctrl Pts',(46.6736556547288,-5.91675155731,334.924043887191));
#16532=CARTESIAN_POINT('Ctrl Pts',(46.6700520047037,-5.91674999875839,335.000121212992));
#16533=CARTESIAN_POINT('',(44.9200520047037,-5.91362697320443,334.994759399896));
#16534=CARTESIAN_POINT('Ctrl Pts',(46.6700520047037,-5.92649690913588,335.000121412671));
#16535=CARTESIAN_POINT('Ctrl Pts',(46.6697465844951,-5.92649885470028,335.006579817236));
#16536=CARTESIAN_POINT('Ctrl Pts',(46.6694411642864,-5.92648921301328,335.013038215818));
#16537=CARTESIAN_POINT('Ctrl Pts',(46.5763897326532,-5.92001614787365,336.980686933046));
#16538=CARTESIAN_POINT('Ctrl Pts',(46.3908977098039,-3.76689395428887,340.89602687056));
#16539=CARTESIAN_POINT('Ctrl Pts',(46.11265967553,2.91961231867273,341.358339942929));
#16540=CARTESIAN_POINT('Ctrl Pts',(45.8344216412561,6.92683346019826,335.985698298619));
#16541=CARTESIAN_POINT('Ctrl Pts',(45.556183606982,4.57740177519211,329.708495874547));
#16542=CARTESIAN_POINT('Ctrl Pts',(45.2779455727082,-1.972643956568,328.287228683932));
#16543=CARTESIAN_POINT('Ctrl Pts',(45.065901705282,-5.5848071039122,331.898755083066));
#16544=CARTESIAN_POINT('Ctrl Pts',(44.9466038492806,-5.91842218040601,334.430123096533));
#16545=CARTESIAN_POINT('Ctrl Pts',(44.9200520047037,-5.91362697320443,334.994759399896));
#16546=CARTESIAN_POINT('',(43.1700520047037,-5.90788815228446,335.002395865961));
#16547=CARTESIAN_POINT('Ctrl Pts',(44.9200520047037,-5.91362697320443,334.994759399896));
#16548=CARTESIAN_POINT('Ctrl Pts',(44.8538578378559,-5.90167244610358,336.402406599885));
#16549=CARTESIAN_POINT('Ctrl Pts',(44.6949176595833,-4.69332639461075,339.800777237329));
#16550=CARTESIAN_POINT('Ctrl Pts',(44.4432314698865,0.984477120973444,341.927007125697));
#16551=CARTESIAN_POINT('Ctrl Pts',(44.1649934356125,6.35782513266129,337.920733213378));
#16552=CARTESIAN_POINT('Ctrl Pts',(43.8867554013384,5.89669086145038,331.234145541087));
#16553=CARTESIAN_POINT('Ctrl Pts',(43.6085173670646,0.0242504217003248,
328.003426921824));
#16554=CARTESIAN_POINT('Ctrl Pts',(43.3696162348529,-5.03706062467533,330.742371873038));
#16555=CARTESIAN_POINT('Ctrl Pts',(43.223461114066,-5.90374971504265,333.863851207851));
#16556=CARTESIAN_POINT('Ctrl Pts',(43.1700520047037,-5.90788815228446,335.002395865961));
#16557=CARTESIAN_POINT('',(41.4200520047037,-5.92242663459137,335.004249368818));
#16558=CARTESIAN_POINT('Ctrl Pts',(43.1700520047037,-5.90788815228446,335.002395865961));
#16559=CARTESIAN_POINT('Ctrl Pts',(43.1307151026414,-5.91093619600615,335.840957306968));
#16560=CARTESIAN_POINT('Ctrl Pts',(42.9986321891541,-5.35183494074253,338.652745309149));
#16561=CARTESIAN_POINT('Ctrl Pts',(42.773803264243,-1.03247149672339,341.920016295474));
#16562=CARTESIAN_POINT('Ctrl Pts',(42.4955652299687,5.2604597648615,339.613045196343));
#16563=CARTESIAN_POINT('Ctrl Pts',(42.2173271956949,6.72594474449119,333.072750608958));
#16564=CARTESIAN_POINT('Ctrl Pts',(41.939089161421,2.01912950688338,328.30106434158));
#16565=CARTESIAN_POINT('Ctrl Pts',(41.6733307644238,-4.24639111760399,329.615183290383));
#16566=CARTESIAN_POINT('Ctrl Pts',(41.5003183788515,-5.90864287789061,333.303856397318));
#16567=CARTESIAN_POINT('Ctrl Pts',(41.4200520047037,-5.92242663459137,335.004249368818));
#16568=CARTESIAN_POINT('',(39.6700520047037,-5.92132355008389,334.995338312928));
#16569=CARTESIAN_POINT('Ctrl Pts',(41.4200520047037,-5.92242663459137,335.004249368818));
#16570=CARTESIAN_POINT('Ctrl Pts',(41.4075723674268,-5.92456970241727,335.268622685015));
#16571=CARTESIAN_POINT('Ctrl Pts',(41.3023467187248,-5.78826462712125,337.495538792487));
#16572=CARTESIAN_POINT('Ctrl Pts',(41.1043750585995,-2.96361819744428,341.337948414188));
#16573=CARTESIAN_POINT('Ctrl Pts',(40.826137024325,3.72593217667956,340.92199732658));
#16574=CARTESIAN_POINT('Ctrl Pts',(40.5478989900514,6.99624958693683,335.071516700898));
#16575=CARTESIAN_POINT('Ctrl Pts',(40.2696609557772,3.84621201573579,329.155406254391));
#16576=CARTESIAN_POINT('Ctrl Pts',(39.9914229215034,-2.83343755231025,328.602793222165));
#16577=CARTESIAN_POINT('Ctrl Pts',(39.7915532711454,-5.76386867538184,332.422934646081));
#16578=CARTESIAN_POINT('Ctrl Pts',(39.6844296322123,-5.92395602760576,334.690609525211));
#16579=CARTESIAN_POINT('Ctrl Pts',(39.6700520047037,-5.92132355008389,334.995338312928));
#16580=CARTESIAN_POINT('',(37.9200520047037,-5.90746150631063,334.998222585503));
#16581=CARTESIAN_POINT('Ctrl Pts',(39.6700520047037,-5.92132355008389,334.995338312928));
#16582=CARTESIAN_POINT('Ctrl Pts',(39.5916836207876,-5.90697465914474,336.656328807495));
#16583=CARTESIAN_POINT('Ctrl Pts',(39.4205692254472,-4.31103524867919,340.307183998279));
#16584=CARTESIAN_POINT('Ctrl Pts',(39.1567088186815,1.88176686553378,341.738811199685));
#16585=CARTESIAN_POINT('Ctrl Pts',(38.8784707844076,6.685142130748,337.064339510092));
#16586=CARTESIAN_POINT('Ctrl Pts',(38.6002327501337,5.35366113510944,330.495453921688));
#16587=CARTESIAN_POINT('Ctrl Pts',(38.3219947158598,-0.890795664309563,
328.060323782362));
#16588=CARTESIAN_POINT('Ctrl Pts',(38.0952678007163,-5.31306658525543,331.265445823351));
#16589=CARTESIAN_POINT('Ctrl Pts',(37.9612868969977,-5.90982214709327,334.11904235838));
#16590=CARTESIAN_POINT('Ctrl Pts',(37.9200520047037,-5.90746150631063,334.998222585503));
#16591=CARTESIAN_POINT('',(36.1700520047038,-5.9147878109749,335.005387872254));
#16592=CARTESIAN_POINT('Ctrl Pts',(37.9200520047037,-5.90746150631063,334.998222585503));
#16593=CARTESIAN_POINT('Ctrl Pts',(37.8685408855731,-5.90451256569713,336.096505008402));
#16594=CARTESIAN_POINT('Ctrl Pts',(37.724283755018,-5.08328597131374,339.176347489048));
#16595=CARTESIAN_POINT('Ctrl Pts',(37.4872806130378,-0.118779716061436,
341.99560678571));
#16596=CARTESIAN_POINT('Ctrl Pts',(37.209042578764,5.81847647089011,338.885608636871));
#16597=CARTESIAN_POINT('Ctrl Pts',(36.9308045444899,6.4162026810768,332.209844793464));
#16598=CARTESIAN_POINT('Ctrl Pts',(36.6525665102162,1.12587439383617,328.094565200472));
#16599=CARTESIAN_POINT('Ctrl Pts',(36.3989823302873,-4.63734310247643,330.119439702854));
#16600=CARTESIAN_POINT('Ctrl Pts',(36.2381441617832,-5.90195021880725,333.558100165989));
#16601=CARTESIAN_POINT('Ctrl Pts',(36.1700520047038,-5.9147878109749,335.005387872254));
#16602=CARTESIAN_POINT('',(34.4200520047038,-5.92198531706792,334.999129254866));
#16603=CARTESIAN_POINT('Ctrl Pts',(36.1700520047038,-5.9147878109749,335.005387872254));
#16604=CARTESIAN_POINT('Ctrl Pts',(36.1453981503586,-5.91943586650756,335.529401530159));
#16605=CARTESIAN_POINT('Ctrl Pts',(36.027998284589,-5.6153715872659,338.019412061154));
#16606=CARTESIAN_POINT('Ctrl Pts',(35.8178524073941,-2.10945529650313,341.671043492088));
#16607=CARTESIAN_POINT('Ctrl Pts',(35.5396143731204,4.46827549150828,340.383970380044));
#16608=CARTESIAN_POINT('Ctrl Pts',(35.2613763388463,6.94553581259915,334.156107117514));
#16609=CARTESIAN_POINT('Ctrl Pts',(34.9831383045725,3.04898043440978,328.702671897399));
#16610=CARTESIAN_POINT('Ctrl Pts',(34.7049002702983,-3.64557928556341,329.028201728633));
#16611=CARTESIAN_POINT('Ctrl Pts',(34.517204837009,-5.90481133641296,332.944685763767));
#16612=CARTESIAN_POINT('Ctrl Pts',(34.4222554151441,-5.92643859533875,334.952532118383));
#16613=CARTESIAN_POINT('Ctrl Pts',(34.4200520047038,-5.92634295523124,334.999128614136));
#16614=CARTESIAN_POINT('',(32.6700520280108,-5.91402521091767,334.995077176078));
#16615=CARTESIAN_POINT('Ctrl Pts',(34.4200520047038,-5.91674993604115,334.999130024655));
#16616=CARTESIAN_POINT('Ctrl Pts',(34.4126579298141,-5.91677289021799,335.155242637744));
#16617=CARTESIAN_POINT('Ctrl Pts',(34.4052638549244,-5.91061306742824,335.311599720021));
#16618=CARTESIAN_POINT('Ctrl Pts',(34.3978697800347,-5.89823842825458,335.467668692517));
#16619=CARTESIAN_POINT('Ctrl Pts',(34.3904843951807,-5.88587833262526,335.623554241805));
#16620=CARTESIAN_POINT('Ctrl Pts',(34.3830990103266,-5.86731798692203,335.779151983579));
#16621=CARTESIAN_POINT('Ctrl Pts',(34.3757136254726,-5.84257731564632,335.933927659509));
#16622=CARTESIAN_POINT('Ctrl Pts',(34.3683352764739,-5.81786021413507,336.088555884862));
#16623=CARTESIAN_POINT('Ctrl Pts',(34.3609569274751,-5.7869745660705,336.242363233957));
#16624=CARTESIAN_POINT('Ctrl Pts',(34.3535785784763,-5.74999220681904,336.394819050637));
#16625=CARTESIAN_POINT('Ctrl Pts',(34.3462056169747,-5.71303685121784,336.54716354766));
#16626=CARTESIAN_POINT('Ctrl Pts',(34.338832655473,-5.66999373564674,336.698158112603));
#16627=CARTESIAN_POINT('Ctrl Pts',(34.3314596939714,-5.62098600697052,336.847280940177));
#16628=CARTESIAN_POINT('Ctrl Pts',(34.3238332151289,-5.57029316044088,337.001531316933));
#16629=CARTESIAN_POINT('Ctrl Pts',(34.3162067362864,-5.5132182511541,337.153778529582));
#16630=CARTESIAN_POINT('Ctrl Pts',(34.3085802574439,-5.44995434787204,337.303460042764));
#16631=CARTESIAN_POINT('Ctrl Pts',(34.3012120822682,-5.38883315009494,337.448071944594));
#16632=CARTESIAN_POINT('Ctrl Pts',(34.2938439070925,-5.3219355205658,337.590288740651));
#16633=CARTESIAN_POINT('Ctrl Pts',(34.2864757319169,-5.24948504540392,337.729622193744));
#16634=CARTESIAN_POINT('Ctrl Pts',(34.2791076357912,-5.17703534753248,337.868954151988));
#16635=CARTESIAN_POINT('Ctrl Pts',(34.2717395396656,-5.09903309590665,338.005402494501));
#16636=CARTESIAN_POINT('Ctrl Pts',(34.26437144354,-5.0157481858264,338.138502939122));
#16637=CARTESIAN_POINT('Ctrl Pts',(34.2570019419513,-4.93244738916414,338.27162877263));
#16638=CARTESIAN_POINT('Ctrl Pts',(34.2496324403626,-4.84386212789593,338.401405117803));
#16639=CARTESIAN_POINT('Ctrl Pts',(34.2422629387739,-4.75030591952179,338.527396239928));
#16640=CARTESIAN_POINT('Ctrl Pts',(34.2348905465991,-4.65671301500481,338.653436780347));
#16641=CARTESIAN_POINT('Ctrl Pts',(34.2275181544243,-4.55814550637757,338.775688840202));
#16642=CARTESIAN_POINT('Ctrl Pts',(34.2201457622494,-4.45495738023128,338.893749517216));
#16643=CARTESIAN_POINT('Ctrl Pts',(34.2127652038723,-4.3516549553489,339.011940966895));
#16644=CARTESIAN_POINT('Ctrl Pts',(34.2053846454953,-4.24372194256433,339.125931481295));
#16645=CARTESIAN_POINT('Ctrl Pts',(34.1980040871182,-4.13154982505284,339.235354366001));
#16646=CARTESIAN_POINT('Ctrl Pts',(34.1906186555257,-4.01930364283438,339.344849500158));
#16647=CARTESIAN_POINT('Ctrl Pts',(34.1832332239331,-3.90281305889682,339.449770745627));
#16648=CARTESIAN_POINT('Ctrl Pts',(34.1758477923406,-3.78250235883659,339.549791914791));
#16649=CARTESIAN_POINT('Ctrl Pts',(34.1684523991843,-3.66202938217995,339.649947993775));
#16650=CARTESIAN_POINT('Ctrl Pts',(34.1610570060282,-3.53772630150714,339.745190575623));
#16651=CARTESIAN_POINT('Ctrl Pts',(34.1536616128719,-3.41004651512151,339.835236636113));
#16652=CARTESIAN_POINT('Ctrl Pts',(34.1519158091648,-3.37990560987346,339.856493483841));
#16653=CARTESIAN_POINT('Ctrl Pts',(34.1501700054577,-3.34957663745125,339.877460945083));
#16654=CARTESIAN_POINT('Ctrl Pts',(34.1484242017506,-3.31906575364121,339.898135674469));
#16655=CARTESIAN_POINT('Ctrl Pts',(34.1410002243126,-3.18931914347101,339.986054335586));
#16656=CARTESIAN_POINT('Ctrl Pts',(34.1335762468746,-3.05588107845703,340.068946783448));
#16657=CARTESIAN_POINT('Ctrl Pts',(34.1261522694366,-2.91917841302769,340.146486952807));
#16658=CARTESIAN_POINT('Ctrl Pts',(34.118737053409,-2.78263707731139,340.2239356131));
#16659=CARTESIAN_POINT('Ctrl Pts',(34.1113218373814,-2.64283913154804,340.296044385628));
#16660=CARTESIAN_POINT('Ctrl Pts',(34.1039066213538,-2.50024182317893,340.362529383428));
#16661=CARTESIAN_POINT('Ctrl Pts',(34.0964985402097,-2.35778172122227,340.428950409697));
#16662=CARTESIAN_POINT('Ctrl Pts',(34.0890904590657,-2.21252795497314,340.48975827721));
#16663=CARTESIAN_POINT('Ctrl Pts',(34.0816823779216,-2.06496379158148,340.544714158724));
#16664=CARTESIAN_POINT('Ctrl Pts',(34.0742798107476,-1.91750946289127,340.599629135573));
#16665=CARTESIAN_POINT('Ctrl Pts',(34.0668772435735,-1.76774850941976,340.648700669642));
#16666=CARTESIAN_POINT('Ctrl Pts',(34.0594746763995,-1.61618557159137,340.691737411431));
#16667=CARTESIAN_POINT('Ctrl Pts',(34.0520760066447,-1.46470243098648,340.734751494563));
#16668=CARTESIAN_POINT('Ctrl Pts',(34.0446773368899,-1.31141955360445,340.771737011493));
#16669=CARTESIAN_POINT('Ctrl Pts',(34.0372786671352,-1.156858082969,340.802552019445));
#16670=CARTESIAN_POINT('Ctrl Pts',(34.0298812179312,-1.00232211017793,340.833361943877));
#16671=CARTESIAN_POINT('Ctrl Pts',(34.0224837687272,-0.84650832840989,340.858003306718));
#16672=CARTESIAN_POINT('Ctrl Pts',(34.0150863195233,-0.689949572475246,
340.876384955901));
#16673=CARTESIAN_POINT('Ctrl Pts',(34.0076891910598,-0.533397604655317,
340.894765808088));
#16674=CARTESIAN_POINT('Ctrl Pts',(34.0002920625963,-0.376101097558557,
340.90688744275));
#16675=CARTESIAN_POINT('Ctrl Pts',(33.9928949341329,-0.218599266019462,
340.912710454893));
#16676=CARTESIAN_POINT('Ctrl Pts',(33.9854966666963,-0.0610731831300849,
340.918534363633));
#16677=CARTESIAN_POINT('Ctrl Pts',(33.9780983992597,0.0966579141717653,
340.918057705003));
#16678=CARTESIAN_POINT('Ctrl Pts',(33.9707001318231,0.254053692634734,340.911293198934));
#16679=CARTESIAN_POINT('Ctrl Pts',(33.9632992652973,0.411504765890113,340.904526316422));
#16680=CARTESIAN_POINT('Ctrl Pts',(33.9558983987716,0.568619913132773,340.891467204396));
#16681=CARTESIAN_POINT('Ctrl Pts',(33.9484975322458,0.724862954722387,340.872180537021));
#16682=CARTESIAN_POINT('Ctrl Pts',(33.9410885388611,0.881277566109089,340.852872691042));
#16683=CARTESIAN_POINT('Ctrl Pts',(33.9336795454763,1.03681778873289,340.827323678711));
#16684=CARTESIAN_POINT('Ctrl Pts',(33.9262705520916,1.19095595648239,340.795649616067));
#16685=CARTESIAN_POINT('Ctrl Pts',(33.9188569945113,1.34518907866002,340.763956041108));
#16686=CARTESIAN_POINT('Ctrl Pts',(33.9114434369311,1.4980180634654,340.726129986608));
#16687=CARTESIAN_POINT('Ctrl Pts',(33.9040298793509,1.64892997670942,340.682337590676));
#16688=CARTESIAN_POINT('Ctrl Pts',(33.8966057672142,1.80005674068985,340.638482848251));
#16689=CARTESIAN_POINT('Ctrl Pts',(33.8891816550775,1.94926062911523,340.58864491774));
#16690=CARTESIAN_POINT('Ctrl Pts',(33.8817575429408,2.0960474974414,340.533038536913));
#16691=CARTESIAN_POINT('Ctrl Pts',(33.8779004177861,2.17230918527429,340.504148783324));
#16692=CARTESIAN_POINT('Ctrl Pts',(33.8740432926314,2.24791884239155,340.47370276989));
#16693=CARTESIAN_POINT('Ctrl Pts',(33.8701861674767,2.32280985855492,340.44173546982));
#16694=CARTESIAN_POINT('Ctrl Pts',(33.8627621900387,2.46695587197247,340.380206609607));
#16695=CARTESIAN_POINT('Ctrl Pts',(33.8553382126007,2.60887289346655,340.312853553867));
#16696=CARTESIAN_POINT('Ctrl Pts',(33.8479142351627,2.7480557323888,340.239858800978));
#16697=CARTESIAN_POINT('Ctrl Pts',(33.8404990191351,2.88707431461993,340.16695019288));
#16698=CARTESIAN_POINT('Ctrl Pts',(33.8330838031074,3.02336480986931,340.088413312245));
#16699=CARTESIAN_POINT('Ctrl Pts',(33.8256685870798,3.15644104870449,340.004479040675));
#16700=CARTESIAN_POINT('Ctrl Pts',(33.8182605059357,3.2893892422528,339.920625530238));
#16701=CARTESIAN_POINT('Ctrl Pts',(33.8108524247916,3.41912902290022,339.831385165612));
#16702=CARTESIAN_POINT('Ctrl Pts',(33.8034443436475,3.54519803213956,339.737035093327));
#16703=CARTESIAN_POINT('Ctrl Pts',(33.7960417764735,3.67117320591284,339.642755247525));
#16704=CARTESIAN_POINT('Ctrl Pts',(33.7886392092995,3.79348275101191,339.54337348955));
#16705=CARTESIAN_POINT('Ctrl Pts',(33.7812366421255,3.91169266766929,339.439210632106));
#16706=CARTESIAN_POINT('Ctrl Pts',(33.7738379723707,4.02984034732235,339.335102615951));
#16707=CARTESIAN_POINT('Ctrl Pts',(33.766439302616,4.14389241788081,339.226218759654));
#16708=CARTESIAN_POINT('Ctrl Pts',(33.7590406328613,4.25344749597255,339.11292049054));
#16709=CARTESIAN_POINT('Ctrl Pts',(33.7516431836573,4.36298450087812,338.999640912123));
#16710=CARTESIAN_POINT('Ctrl Pts',(33.7442457344533,4.46802572649885,338.881948634247));
#16711=CARTESIAN_POINT('Ctrl Pts',(33.7368482852493,4.56820617362811,338.760242401458));
#16712=CARTESIAN_POINT('Ctrl Pts',(33.7294511567858,4.66838227710783,338.63854144564));
#16713=CARTESIAN_POINT('Ctrl Pts',(33.7220540283224,4.76369778396113,338.512827169104));
#16714=CARTESIAN_POINT('Ctrl Pts',(33.7146568998589,4.85382775759897,338.383531684802));
#16715=CARTESIAN_POINT('Ctrl Pts',(33.7072586324223,4.94397160900281,338.254216292224));
#16716=CARTESIAN_POINT('Ctrl Pts',(33.6998603649857,5.02892812395047,338.121318900122));
#16717=CARTESIAN_POINT('Ctrl Pts',(33.6924620975491,5.10841559357635,337.985300769739));
#16718=CARTESIAN_POINT('Ctrl Pts',(33.6850612310234,5.1879309879861,337.849234854757));
#16719=CARTESIAN_POINT('Ctrl Pts',(33.6776603644977,5.26197332351767,337.710046340687));
#16720=CARTESIAN_POINT('Ctrl Pts',(33.6702594979719,5.33030682848717,337.56822111133));
#16721=CARTESIAN_POINT('Ctrl Pts',(33.6628505045872,5.39871537017816,337.426240144313));
#16722=CARTESIAN_POINT('Ctrl Pts',(33.6554415112023,5.46140240000281,337.281617016229));
#16723=CARTESIAN_POINT('Ctrl Pts',(33.6480325178176,5.51818001200433,337.134858289821));
#16724=CARTESIAN_POINT('Ctrl Pts',(33.6406189602374,5.57499260097331,336.988009154975));
#16725=CARTESIAN_POINT('Ctrl Pts',(33.6332054026572,5.62588839776436,336.83902215264));
#16726=CARTESIAN_POINT('Ctrl Pts',(33.6257918450769,5.67072953333535,336.688418526983));
#16727=CARTESIAN_POINT('Ctrl Pts',(33.6183677329402,5.71563450847209,336.537600489492));
#16728=CARTESIAN_POINT('Ctrl Pts',(33.6109436208036,5.75446751480416,336.385161592691));
#16729=CARTESIAN_POINT('Ctrl Pts',(33.6035195086669,5.78714171993692,336.231633580196));
#16730=CARTESIAN_POINT('Ctrl Pts',(33.5996623835122,5.80411728498861,336.151869596565));
#16731=CARTESIAN_POINT('Ctrl Pts',(33.5958052583575,5.81943130670169,336.071811737973));
#16732=CARTESIAN_POINT('Ctrl Pts',(33.5919481332028,5.8330771481725,335.991534944401));
#16733=CARTESIAN_POINT('Ctrl Pts',(33.5845241557648,5.85934189591565,335.837022689711));
#16734=CARTESIAN_POINT('Ctrl Pts',(33.5771001783268,5.87950271795634,335.681233035491));
#16735=CARTESIAN_POINT('Ctrl Pts',(33.5696762008888,5.89343969342769,335.524689567679));
#16736=CARTESIAN_POINT('Ctrl Pts',(33.5622609848611,5.90736022117104,335.368330844712));
#16737=CARTESIAN_POINT('Ctrl Pts',(33.5548457688335,5.91507149006048,335.21122044707));
#16738=CARTESIAN_POINT('Ctrl Pts',(33.5474305528058,5.91650455918472,335.053892148282));
#16739=CARTESIAN_POINT('Ctrl Pts',(33.5400224716617,5.91793624941707,334.896715229991));
#16740=CARTESIAN_POINT('Ctrl Pts',(33.5326143905177,5.9131017627182,334.739321198657));
#16741=CARTESIAN_POINT('Ctrl Pts',(33.5252063093735,5.90198394880129,334.582248841304));
#16742=CARTESIAN_POINT('Ctrl Pts',(33.5178037421995,5.89087441007637,334.425293395776));
#16743=CARTESIAN_POINT('Ctrl Pts',(33.5104011750255,5.87349088255147,334.268659518178));
#16744=CARTESIAN_POINT('Ctrl Pts',(33.5029986078515,5.84986828229686,334.112885778337));
#16745=CARTESIAN_POINT('Ctrl Pts',(33.4955999380967,5.82625811923782,333.957194052687));
#16746=CARTESIAN_POINT('Ctrl Pts',(33.4882012683419,5.79641548122736,333.802361930962));
#16747=CARTESIAN_POINT('Ctrl Pts',(33.4808025985871,5.76042708864121,333.648922534068));
#16748=CARTESIAN_POINT('Ctrl Pts',(33.4734051493831,5.7244446330226,333.495508449911));
#16749=CARTESIAN_POINT('Ctrl Pts',(33.4660077001791,5.68231852014944,333.34348699759));
#16750=CARTESIAN_POINT('Ctrl Pts',(33.4586102509751,5.63418654080336,333.193380896279));
#16751=CARTESIAN_POINT('Ctrl Pts',(33.4512131225117,5.58605664837599,333.043281303306));
#16752=CARTESIAN_POINT('Ctrl Pts',(33.4438159940482,5.5319215212007,332.895097251609));
#16753=CARTESIAN_POINT('Ctrl Pts',(33.4364188655847,5.47196869044563,332.749335828409));
#16754=CARTESIAN_POINT('Ctrl Pts',(33.4290205981481,5.41200662845135,332.603551961589));
#16755=CARTESIAN_POINT('Ctrl Pts',(33.4216223307115,5.34622522123311,332.460191811185));
#16756=CARTESIAN_POINT('Ctrl Pts',(33.4142240632749,5.27485990437902,332.319741887117));
#16757=CARTESIAN_POINT('Ctrl Pts',(33.4068231967491,5.20346951613872,332.179242621514));
#16758=CARTESIAN_POINT('Ctrl Pts',(33.3994223302234,5.12649148150508,332.041655950343));
#16759=CARTESIAN_POINT('Ctrl Pts',(33.3920214636977,5.04420680094495,331.907443078648));
#16760=CARTESIAN_POINT('Ctrl Pts',(33.3846124703129,4.96183176393849,331.773082828388));
#16761=CARTESIAN_POINT('Ctrl Pts',(33.3772034769281,4.87413863895259,331.64210409456));
#16762=CARTESIAN_POINT('Ctrl Pts',(33.3697944835434,4.78145171870812,331.514939021457));
#16763=CARTESIAN_POINT('Ctrl Pts',(33.3623809259632,4.68870770012433,331.387695610284));
#16764=CARTESIAN_POINT('Ctrl Pts',(33.354967368383,4.59096398740696,331.264270833113));
#16765=CARTESIAN_POINT('Ctrl Pts',(33.3475538108028,4.48858429704586,331.145062702091));
#16766=CARTESIAN_POINT('Ctrl Pts',(33.3401296986661,4.38605885045184,331.025684856469));
#16767=CARTESIAN_POINT('Ctrl Pts',(33.3327055865294,4.27888449795346,330.910535918977));
#16768=CARTESIAN_POINT('Ctrl Pts',(33.3252814743927,4.1674614041125,330.799976665811));
#16769=CARTESIAN_POINT('Ctrl Pts',(33.3214243492381,4.10957262089594,330.742536682604));
#16770=CARTESIAN_POINT('Ctrl Pts',(33.3175672240835,4.05053755551535,330.686334894033));
#16771=CARTESIAN_POINT('Ctrl Pts',(33.3137100989289,3.9904156349902,330.631417435538));
#16772=CARTESIAN_POINT('Ctrl Pts',(33.3062861214909,3.87469634572208,330.525715401903));
#16773=CARTESIAN_POINT('Ctrl Pts',(33.2988621440529,3.75459967949589,330.424455015429));
#16774=CARTESIAN_POINT('Ctrl Pts',(33.2914381666149,3.63050103483573,330.328020462528));
#16775=CARTESIAN_POINT('Ctrl Pts',(33.2840229505872,3.50654884524791,330.231699716908));
#16776=CARTESIAN_POINT('Ctrl Pts',(33.2766077345596,3.37860437013577,330.14019369523));
#16777=CARTESIAN_POINT('Ctrl Pts',(33.269192518532,3.24707916316589,330.05384922686));
#16778=CARTESIAN_POINT('Ctrl Pts',(33.2617844373879,3.11568050908782,329.967587838703));
#16779=CARTESIAN_POINT('Ctrl Pts',(33.2543763562438,2.98070829212938,329.886478320085));
#16780=CARTESIAN_POINT('Ctrl Pts',(33.2469682750997,2.84260630878921,329.810826661622));
#16781=CARTESIAN_POINT('Ctrl Pts',(33.2395657079257,2.70460711727768,329.735231312071));
#16782=CARTESIAN_POINT('Ctrl Pts',(33.2321631407517,2.56348312375822,329.665085912409));
#16783=CARTESIAN_POINT('Ctrl Pts',(33.2247605735777,2.4197061181765,329.600652552006));
#16784=CARTESIAN_POINT('Ctrl Pts',(33.2173619038229,2.27600481055944,329.536253115485));
#16785=CARTESIAN_POINT('Ctrl Pts',(33.2099632340682,2.12965361240599,329.477559881123));
#16786=CARTESIAN_POINT('Ctrl Pts',(33.2025645643134,1.98114776583088,329.424788426217));
#16787=CARTESIAN_POINT('Ctrl Pts',(33.1951671151094,1.83266641810952,329.372025676963));
#16788=CARTESIAN_POINT('Ctrl Pts',(33.1877696659055,1.6820314787462,329.325182893159));
#16789=CARTESIAN_POINT('Ctrl Pts',(33.1803722167015,1.52975707994427,329.284427076936));
#16790=CARTESIAN_POINT('Ctrl Pts',(33.1729750882381,1.3774892834948,329.243673027814));
#16791=CARTESIAN_POINT('Ctrl Pts',(33.1655779597746,1.22358252946698,329.209005518005));
#16792=CARTESIAN_POINT('Ctrl Pts',(33.1581808313111,1.06856472220108,329.180541262543));
#16793=CARTESIAN_POINT('Ctrl Pts',(33.1507825638745,0.913523046062173,329.152072624295));
#16794=CARTESIAN_POINT('Ctrl Pts',(33.1433842964379,0.757370343150165,329.129809209622));
#16795=CARTESIAN_POINT('Ctrl Pts',(33.1359860290013,0.600643137742669,329.113816314149));
#16796=CARTESIAN_POINT('Ctrl Pts',(33.1285851624755,0.443860872419733,329.097817800203));
#16797=CARTESIAN_POINT('Ctrl Pts',(33.1211842959498,0.28650407380993,329.088094229288));
#16798=CARTESIAN_POINT('Ctrl Pts',(33.113783429424,0.129112644549985,329.084658886631));
#16799=CARTESIAN_POINT('Ctrl Pts',(33.1063744360392,-0.0284516155462758,
329.081219771638));
#16800=CARTESIAN_POINT('Ctrl Pts',(33.0989654426544,-0.186050208891175,
329.084082682857));
#16801=CARTESIAN_POINT('Ctrl Pts',(33.0915564492697,-0.343144242729558,
329.093208773693));
#16802=CARTESIAN_POINT('Ctrl Pts',(33.0841428916894,-0.500335051911762,
329.102340486515));
#16803=CARTESIAN_POINT('Ctrl Pts',(33.0767293341092,-0.657020311672226,
329.11774303077));
#16804=CARTESIAN_POINT('Ctrl Pts',(33.069315776529,-0.812668497243394,329.139325936713));
#16805=CARTESIAN_POINT('Ctrl Pts',(33.0618916643923,-0.968538276501934,
329.160939569873));
#16806=CARTESIAN_POINT('Ctrl Pts',(33.0544675522556,-1.12336766643381,329.188751072032));
#16807=CARTESIAN_POINT('Ctrl Pts',(33.0470434401189,-1.27663673063275,329.222619172973));
#16808=CARTESIAN_POINT('Ctrl Pts',(33.0431863149643,-1.35626618019799,329.240215014964));
#16809=CARTESIAN_POINT('Ctrl Pts',(33.0393291898095,-1.43547472452992,329.259444848248));
#16810=CARTESIAN_POINT('Ctrl Pts',(33.0354720646549,-1.51419140798456,329.280283665907));
#16811=CARTESIAN_POINT('Ctrl Pts',(33.0280480872168,-1.66570085051652,329.320393049435));
#16812=CARTESIAN_POINT('Ctrl Pts',(33.0206241097789,-1.81584406703773,329.366587092774));
#16813=CARTESIAN_POINT('Ctrl Pts',(33.0132001323409,-1.96409483731779,329.418758020609));
#16814=CARTESIAN_POINT('Ctrl Pts',(33.0057849163133,-2.11217064938319,329.470867378899));
#16815=CARTESIAN_POINT('Ctrl Pts',(32.9983697002856,-2.25835811214371,329.528939458651));
#16816=CARTESIAN_POINT('Ctrl Pts',(32.990954484258,-2.40214285408021,329.59281586488));
#16817=CARTESIAN_POINT('Ctrl Pts',(32.9835464031139,-2.54578924706228,329.656630809553));
#16818=CARTESIAN_POINT('Ctrl Pts',(32.9761383219698,-2.68703718296428,329.726238811711));
#16819=CARTESIAN_POINT('Ctrl Pts',(32.9687302408257,-2.82538918399848,329.801432262493));
#16820=CARTESIAN_POINT('Ctrl Pts',(32.9613276736517,-2.96363820711171,329.876569745417));
#16821=CARTESIAN_POINT('Ctrl Pts',(32.9539251064777,-3.09899526076012,329.957284221617));
#16822=CARTESIAN_POINT('Ctrl Pts',(32.9465225393037,-3.23098463579218,330.043320784459));
#16823=CARTESIAN_POINT('Ctrl Pts',(32.9391238695489,-3.36290451899495,330.129312049427));
#16824=CARTESIAN_POINT('Ctrl Pts',(32.9317251997942,-3.49145994288626,330.220619617289));
#16825=CARTESIAN_POINT('Ctrl Pts',(32.9243265300394,-3.61620161999129,330.316943689633));
#16826=CARTESIAN_POINT('Ctrl Pts',(32.9169290808355,-3.74092271859286,330.413251871495));
#16827=CARTESIAN_POINT('Ctrl Pts',(32.9095316316315,-3.86183102396098,330.514574687506));
#16828=CARTESIAN_POINT('Ctrl Pts',(32.9021341824276,-3.97850787400498,330.620570167364));
#16829=CARTESIAN_POINT('Ctrl Pts',(32.8947370539641,-4.09517966514451,330.726561051443));
#16830=CARTESIAN_POINT('Ctrl Pts',(32.8873399255006,-4.20762008951414,330.837223945583));
#16831=CARTESIAN_POINT('Ctrl Pts',(32.8799427970371,-4.3154453196227,330.952178084964));
#16832=CARTESIAN_POINT('Ctrl Pts',(32.8725445296005,-4.42328715212455,331.067149924412));
#16833=CARTESIAN_POINT('Ctrl Pts',(32.8651462621639,-4.52651212007774,331.186414052508));
#16834=CARTESIAN_POINT('Ctrl Pts',(32.8577479947274,-4.62477497092559,331.30955462975));
#16835=CARTESIAN_POINT('Ctrl Pts',(32.8503471282016,-4.72307234254658,331.432738467572));
#16836=CARTESIAN_POINT('Ctrl Pts',(32.8429462616758,-4.8164038936307,331.559801174423));
#16837=CARTESIAN_POINT('Ctrl Pts',(32.8355453951501,-4.90446628005209,331.690295924054));
#16838=CARTESIAN_POINT('Ctrl Pts',(32.8281364017653,-4.99262536739299,331.820933969397));
#16839=CARTESIAN_POINT('Ctrl Pts',(32.8207274083806,-5.0755035261362,331.955011274293));
#16840=CARTESIAN_POINT('Ctrl Pts',(32.8133184149958,-5.15284179741967,332.092053650209));
#16841=CARTESIAN_POINT('Ctrl Pts',(32.8059048574156,-5.23022771174594,332.229180448955));
#16842=CARTESIAN_POINT('Ctrl Pts',(32.7984912998354,-5.30206676833751,332.369275627115));
#16843=CARTESIAN_POINT('Ctrl Pts',(32.7910777422551,-5.36814740658304,332.511843255802));
#16844=CARTESIAN_POINT('Ctrl Pts',(32.7836536301184,-5.4343221227146,332.654613855609));
#16845=CARTESIAN_POINT('Ctrl Pts',(32.7762295179817,-5.49472190421748,332.799863592385));
#16846=CARTESIAN_POINT('Ctrl Pts',(32.7688054058451,-5.54918418080667,332.947078791092));
#16847=CARTESIAN_POINT('Ctrl Pts',(32.7649482806904,-5.57747952618227,333.023563013802));
#16848=CARTESIAN_POINT('Ctrl Pts',(32.7610911555357,-5.6041730374472,333.100577534769));
#16849=CARTESIAN_POINT('Ctrl Pts',(32.757234030381,-5.62924734528016,333.1780491532));
#16850=CARTESIAN_POINT('Ctrl Pts',(32.7483245768245,-5.68716570990079,333.35699843762));
#16851=CARTESIAN_POINT('Ctrl Pts',(32.7394151232681,-5.73658396790036,333.53882492236));
#16852=CARTESIAN_POINT('Ctrl Pts',(32.7305056697117,-5.77725438143087,333.722791178101));
#16853=CARTESIAN_POINT('Ctrl Pts',(32.7216448111127,-5.817702965755,333.905754024115));
#16854=CARTESIAN_POINT('Ctrl Pts',(32.7127839525136,-5.84949880810189,334.090833337918));
#16855=CARTESIAN_POINT('Ctrl Pts',(32.7039230939145,-5.8724449569823,334.277282358239));
#16856=CARTESIAN_POINT('Ctrl Pts',(32.6951516005632,-5.89515968491686,334.46185096678));
#16857=CARTESIAN_POINT('Ctrl Pts',(32.6863801072118,-5.90920226207405,334.64776174815));
#16858=CARTESIAN_POINT('Ctrl Pts',(32.6776086138604,-5.91442846696909,334.834269883227));
#16859=CARTESIAN_POINT('Ctrl Pts',(32.6750897633767,-5.91592924091947,334.887828164289));
#16860=CARTESIAN_POINT('Ctrl Pts',(32.672570912893,-5.91670329426,334.941435577252));
#16861=CARTESIAN_POINT('Ctrl Pts',(32.6700520624094,-5.9167479495726,334.995074177391));
#16862=CARTESIAN_POINT('',(30.9200520047038,-5.90864326687124,335.003157960057));
#16863=CARTESIAN_POINT('Ctrl Pts',(32.6700520047037,-5.91218039106208,334.99507920787));
#16864=CARTESIAN_POINT('Ctrl Pts',(32.6063666685048,-5.90157038152927,336.350213184948));
#16865=CARTESIAN_POINT('Ctrl Pts',(32.4499353208814,-4.76532520505771,339.694927843386));
#16866=CARTESIAN_POINT('Ctrl Pts',(32.200757961833,0.796951585255475,341.951078412161));
#16867=CARTESIAN_POINT('Ctrl Pts',(31.9225199275592,6.27658636339294,338.091453791354));
#16868=CARTESIAN_POINT('Ctrl Pts',(31.6442818932852,5.99629047810708,331.39484765601));
#16869=CARTESIAN_POINT('Ctrl Pts',(31.3660438590111,0.213287326162839,328.006636614779));
#16870=CARTESIAN_POINT('Ctrl Pts',(31.1246338961508,-4.97409082752309,330.63514264744));
#16871=CARTESIAN_POINT('Ctrl Pts',(30.975969944715,-5.90288956727121,333.811512346957));
#16872=CARTESIAN_POINT('Ctrl Pts',(30.9200520047038,-5.90864326687124,335.003157960057));
#16873=CARTESIAN_POINT('',(29.1700520047038,-5.92375170242329,335.003585402275));
#16874=CARTESIAN_POINT('Ctrl Pts',(30.9200520047038,-5.90864326687124,335.003157960057));
#16875=CARTESIAN_POINT('Ctrl Pts',(30.8832239332903,-5.91243270653441,335.787986759724));
#16876=CARTESIAN_POINT('Ctrl Pts',(30.7536498504522,-5.40138091405304,338.544554349899));
#16877=CARTESIAN_POINT('Ctrl Pts',(30.5313297561895,-1.2190717529215,341.889592657226));
#16878=CARTESIAN_POINT('Ctrl Pts',(30.2530917219154,5.13389577264302,339.753497356351));
#16879=CARTESIAN_POINT('Ctrl Pts',(29.9748536876416,6.77556292383056,333.255187693066));
#16880=CARTESIAN_POINT('Ctrl Pts',(29.6966156533676,2.19939598696192,328.35806653046));
#16881=CARTESIAN_POINT('Ctrl Pts',(29.4283484257217,-4.158806077555,329.513215736931));
#16882=CARTESIAN_POINT('Ctrl Pts',(29.2528272095004,-5.91124546303899,333.251071106676));
#16883=CARTESIAN_POINT('Ctrl Pts',(29.1700520047038,-5.92375170242329,335.003585402275));
#16884=CARTESIAN_POINT('',(27.4200520047038,-5.91977329940477,334.994921843694));
#16885=CARTESIAN_POINT('Ctrl Pts',(29.1700520047038,-5.92375170242329,335.003585402275));
#16886=CARTESIAN_POINT('Ctrl Pts',(29.1600811980758,-5.92525815951815,335.214687038293));
#16887=CARTESIAN_POINT('Ctrl Pts',(29.0573643800223,-5.81911313062826,337.387873149651));
#16888=CARTESIAN_POINT('Ctrl Pts',(28.8619015505466,-3.13378605384101,341.255558159747));
#16889=CARTESIAN_POINT('Ctrl Pts',(28.5836635162714,3.5645608626718,341.020509013158));
#16890=CARTESIAN_POINT('Ctrl Pts',(28.3054254819982,6.99176288834324,335.260527607764));
#16891=CARTESIAN_POINT('Ctrl Pts',(28.0271874477237,4.00272730963239,329.261463862102));
#16892=CARTESIAN_POINT('Ctrl Pts',(27.7489494134502,-2.6595520409677,328.528570029539));
#16893=CARTESIAN_POINT('Ctrl Pts',(27.5465709324433,-5.73019854909535,332.315077454903));
#16894=CARTESIAN_POINT('Ctrl Pts',(27.4369384628612,-5.92302912543987,334.636776519727));
#16895=CARTESIAN_POINT('Ctrl Pts',(27.4200520047038,-5.91977329940477,334.994921843694));
#16896=CARTESIAN_POINT('',(25.6700520047038,-5.90709767767298,334.999078370416));
#16897=CARTESIAN_POINT('Ctrl Pts',(27.4200520047038,-5.91977329940477,334.994921843694));
#16898=CARTESIAN_POINT('Ctrl Pts',(27.3441924514366,-5.90514705237084,336.603829053699));
#16899=CARTESIAN_POINT('Ctrl Pts',(27.1755868867448,-4.39436720596486,340.203961359681));
#16900=CARTESIAN_POINT('Ctrl Pts',(26.9142353106283,1.69899873852852,341.787195754337));
#16901=CARTESIAN_POINT('Ctrl Pts',(26.6359972763544,6.62692341423896,337.244216786105));
#16902=CARTESIAN_POINT('Ctrl Pts',(26.3577592420802,5.47341828593005,330.641753197846));
#16903=CARTESIAN_POINT('Ctrl Pts',(26.0795212078066,-0.70296201585298,328.038788372311));
#16904=CARTESIAN_POINT('Ctrl Pts',(25.8502854620142,-5.26009475152233,331.157382410602));
#16905=CARTESIAN_POINT('Ctrl Pts',(25.7137957276467,-5.90839173125013,334.066263377539));
#16906=CARTESIAN_POINT('Ctrl Pts',(25.6700520047038,-5.90709767767298,334.999078370416));
#16907=CARTESIAN_POINT('',(23.9200520047038,-5.91638134160122,335.005450646086));
#16908=CARTESIAN_POINT('Ctrl Pts',(25.6700520047038,-5.90709767767298,334.999078370416));
#16909=CARTESIAN_POINT('Ctrl Pts',(25.621049716222,-5.90564806199256,336.044029881305));
#16910=CARTESIAN_POINT('Ctrl Pts',(25.4793014163158,-5.1425470526809,339.068726244074));
#16911=CARTESIAN_POINT('Ctrl Pts',(25.2448071049846,-0.307755998838631,
341.989843286254));
#16912=CARTESIAN_POINT('Ctrl Pts',(24.9665690707106,5.71136391117128,339.041403864425));
#16913=CARTESIAN_POINT('Ctrl Pts',(24.6883310364366,6.48924945949215,332.384227767235));
#16914=CARTESIAN_POINT('Ctrl Pts',(24.4100930021627,1.31204655999919,328.127507239318));
#16915=CARTESIAN_POINT('Ctrl Pts',(24.1539999915853,-4.56131717805019,330.014406803911));
#16916=CARTESIAN_POINT('Ctrl Pts',(23.9906529924321,-5.9026043456772,333.505867600689));
#16917=CARTESIAN_POINT('Ctrl Pts',(23.9200520047038,-5.91638134160122,335.005450646086));
#16918=CARTESIAN_POINT('',(22.1700520047038,-5.92581566588214,334.998170041165));
#16919=CARTESIAN_POINT('Ctrl Pts',(23.9200520047038,-5.91638134160122,335.005450646086));
#16920=CARTESIAN_POINT('Ctrl Pts',(23.8979069810075,-5.92070269617454,335.475816616073));
#16921=CARTESIAN_POINT('Ctrl Pts',(23.7830159458868,-5.654242975896,337.911293734121));
#16922=CARTESIAN_POINT('Ctrl Pts',(23.5753788993408,-2.28893515882164,341.611610905065));
#16923=CARTESIAN_POINT('Ctrl Pts',(23.2971408650671,4.32117050908963,340.502736442224));
#16924=CARTESIAN_POINT('Ctrl Pts',(23.018902830793,6.96580178118044,334.344081966615));
#16925=CARTESIAN_POINT('Ctrl Pts',(22.7406647965191,3.21801957374706,328.787353788907));
#16926=CARTESIAN_POINT('Ctrl Pts',(22.4624267622454,-3.48289169861992,328.931879340613));
#16927=CARTESIAN_POINT('Ctrl Pts',(22.2722224983067,-5.8787228513342,332.837404167105));
#16928=CARTESIAN_POINT('Ctrl Pts',(22.1747642457929,-5.92621969426432,334.898494469636));
#16929=CARTESIAN_POINT('Ctrl Pts',(22.1700520047038,-5.92581566588214,334.998170041165));
#16930=CARTESIAN_POINT('',(20.4200532134703,-5.91336702896276,334.99550345961));
#16931=CARTESIAN_POINT('Ctrl Pts',(22.1700520047038,-5.92581566588214,334.998170041165));
#16932=CARTESIAN_POINT('Ctrl Pts',(22.0820182343683,-5.91826763488531,336.860302348495));
#16933=CARTESIAN_POINT('Ctrl Pts',(21.9012384526082,-3.96724156732265,340.697866670071));
#16934=CARTESIAN_POINT('Ctrl Pts',(21.6277126594233,2.57187304028365,341.506772778104));
#16935=CARTESIAN_POINT('Ctrl Pts',(21.3494746251494,6.86347212116061,336.358445200694));
#16936=CARTESIAN_POINT('Ctrl Pts',(21.0712365908757,4.85656414112844,329.963492513229));
#16937=CARTESIAN_POINT('Ctrl Pts',(20.7929985566017,-1.60714106844329,328.190468407641));
#16938=CARTESIAN_POINT('Ctrl Pts',(20.5759377291129,-5.49907885329114,331.682300406566));
#16939=CARTESIAN_POINT('Ctrl Pts',(20.4516229130488,-5.91556391747135,334.323369558575));
#16940=CARTESIAN_POINT('Ctrl Pts',(20.4200541084095,-5.91086361778023,334.995486298683));
#16941=CARTESIAN_POINT('',(18.6700508084278,-5.91273647904805,335.003866065122));
#16942=CARTESIAN_POINT('Ctrl Pts',(20.4200520047038,-5.91674830895615,334.995526638342));
#16943=CARTESIAN_POINT('Ctrl Pts',(20.4124049415101,-5.91687152346305,335.158497862473));
#16944=CARTESIAN_POINT('Ctrl Pts',(20.4047578783163,-5.91025650452325,335.321540234287));
#16945=CARTESIAN_POINT('Ctrl Pts',(20.3971108151226,-5.89691613023303,335.484056520974));
#16946=CARTESIAN_POINT('Ctrl Pts',(20.3897099568282,-5.88400526272547,335.641340432174));
#16947=CARTESIAN_POINT('Ctrl Pts',(20.3823090985338,-5.86479544317899,335.79813121691));
#16948=CARTESIAN_POINT('Ctrl Pts',(20.3749082402394,-5.83935123385778,335.953890837645));
#16949=CARTESIAN_POINT('Ctrl Pts',(20.3675067820282,-5.81390496201789,336.109663084323));
#16950=CARTESIAN_POINT('Ctrl Pts',(20.3601053238169,-5.78222335353899,336.264403633166));
#16951=CARTESIAN_POINT('Ctrl Pts',(20.3527038656057,-5.74442237470037,336.417583205156));
#16952=CARTESIAN_POINT('Ctrl Pts',(20.345300357778,-5.70661092799109,336.570805195729));
#16953=CARTESIAN_POINT('Ctrl Pts',(20.3378968499505,-5.66267682562992,336.722464987473));
#16954=CARTESIAN_POINT('Ctrl Pts',(20.3304933421228,-5.61278628424508,336.872047192218));
#16955=CARTESIAN_POINT('Ctrl Pts',(20.3230863340341,-5.56287215540371,337.021700117056));
#16956=CARTESIAN_POINT('Ctrl Pts',(20.3156793259455,-5.50699609746431,337.169273146422));
#16957=CARTESIAN_POINT('Ctrl Pts',(20.3082723178568,-5.44537289865636,337.314269767568));
#16958=CARTESIAN_POINT('Ctrl Pts',(20.3008563608104,-5.38367524827593,337.459441569922));
#16959=CARTESIAN_POINT('Ctrl Pts',(20.2934404037638,-5.3162167385794,337.602030406583));
#16960=CARTESIAN_POINT('Ctrl Pts',(20.2860244467174,-5.24325897864871,337.741562664854));
#16961=CARTESIAN_POINT('Ctrl Pts',(20.2786031501137,-5.1702486884591,337.881195387635));
#16962=CARTESIAN_POINT('Ctrl Pts',(20.27118185351,-5.09173144359106,338.017766825795));
#16963=CARTESIAN_POINT('Ctrl Pts',(20.2637605569062,-5.00801252846529,338.150831807195));
#16964=CARTESIAN_POINT('Ctrl Pts',(20.2563287610752,-4.92417517259198,338.284085041344));
#16965=CARTESIAN_POINT('Ctrl Pts',(20.2488969652442,-4.83512166474423,338.413821610219));
#16966=CARTESIAN_POINT('Ctrl Pts',(20.2414651694131,-4.74119832129923,338.53962837606));
#16967=CARTESIAN_POINT('Ctrl Pts',(20.23981760896,-4.72037638407118,338.567518573375));
#16968=CARTESIAN_POINT('Ctrl Pts',(20.2381700485069,-4.69931525608397,338.595215774627));
#16969=CARTESIAN_POINT('Ctrl Pts',(20.2365224880537,-4.67801895485086,338.622715724502));
#16970=CARTESIAN_POINT('Ctrl Pts',(20.2290985106158,-4.58205691620946,338.746631667637));
#16971=CARTESIAN_POINT('Ctrl Pts',(20.2216745331777,-4.48102310383591,338.866919006391));
#16972=CARTESIAN_POINT('Ctrl Pts',(20.2142505557397,-4.37522177053171,338.983135074431));
#16973=CARTESIAN_POINT('Ctrl Pts',(20.2068353397121,-4.26954529871933,339.099213990026));
#16974=CARTESIAN_POINT('Ctrl Pts',(20.1994201236846,-4.15911275420038,339.21123092547));
#16975=CARTESIAN_POINT('Ctrl Pts',(20.192004907657,-4.04427039495244,339.318773846245));
#16976=CARTESIAN_POINT('Ctrl Pts',(20.1845968265129,-3.92953853644458,339.426213289763));
#16977=CARTESIAN_POINT('Ctrl Pts',(20.1771887453688,-3.81040558102687,339.529187035419));
#16978=CARTESIAN_POINT('Ctrl Pts',(20.1697806642247,-3.68725653180423,339.627317779358));
#16979=CARTESIAN_POINT('Ctrl Pts',(20.1623780970507,-3.56419914466789,339.725375482793));
#16980=CARTESIAN_POINT('Ctrl Pts',(20.1549755298767,-3.43713190639008,339.818597130477));
#16981=CARTESIAN_POINT('Ctrl Pts',(20.1475729627027,-3.30647490142266,339.906643892597));
#16982=CARTESIAN_POINT('Ctrl Pts',(20.140174292948,-3.17588668679769,339.994644298482));
#16983=CARTESIAN_POINT('Ctrl Pts',(20.1327756231933,-3.04171277824053,340.077475036877));
#16984=CARTESIAN_POINT('Ctrl Pts',(20.1253769534385,-2.90440431301012,340.154839100211));
#16985=CARTESIAN_POINT('Ctrl Pts',(20.1179795042346,-2.76711849941242,340.232190400878));
#16986=CARTESIAN_POINT('Ctrl Pts',(20.1105820550306,-2.62669948026288,340.304076633305));
#16987=CARTESIAN_POINT('Ctrl Pts',(20.1031846058266,-2.4836253030275,340.370245424248));
#16988=CARTESIAN_POINT('Ctrl Pts',(20.0957874773632,-2.34055732923901,340.436411346228));
#16989=CARTESIAN_POINT('Ctrl Pts',(20.0883903488997,-2.19483476500656,340.496860162968));
#16990=CARTESIAN_POINT('Ctrl Pts',(20.0809932204363,-2.04695781771414,340.551386696583));
#16991=CARTESIAN_POINT('Ctrl Pts',(20.0735949529997,-1.89905810106313,340.605921625923));
#16992=CARTESIAN_POINT('Ctrl Pts',(20.066196685563,-1.74900369103808,340.654532327333));
#16993=CARTESIAN_POINT('Ctrl Pts',(20.0587984181264,-1.59731207189522,340.697062814072));
#16994=CARTESIAN_POINT('Ctrl Pts',(20.0513975516007,-1.44556716189089,340.739608242217));
#16995=CARTESIAN_POINT('Ctrl Pts',(20.0439966850749,-1.29218425673634,340.776069102143));
#16996=CARTESIAN_POINT('Ctrl Pts',(20.0365958185491,-1.13769305397936,340.806340075937));
#16997=CARTESIAN_POINT('Ctrl Pts',(20.0291868251643,-0.983032205112258,
340.836644290154));
#16998=CARTESIAN_POINT('Ctrl Pts',(20.0217778317796,-0.827260994660747,
340.860744972289));
#16999=CARTESIAN_POINT('Ctrl Pts',(20.0143688383948,-0.670917030464474,
340.878588342513));
#17000=CARTESIAN_POINT('Ctrl Pts',(20.0069552808146,-0.514476752992932,
340.896442704869));
#17001=CARTESIAN_POINT('Ctrl Pts',(19.9995417232344,-0.35746339003329,340.908032046865));
#17002=CARTESIAN_POINT('Ctrl Pts',(19.9921281656541,-0.200416108172359,
340.913354711675));
#17003=CARTESIAN_POINT('Ctrl Pts',(19.9847040535174,-0.0431452407550206,
340.918684954272));
#17004=CARTESIAN_POINT('Ctrl Pts',(19.9772799413807,0.114159269810065,340.917730703396));
#17005=CARTESIAN_POINT('Ctrl Pts',(19.969855829244,0.270960997063454,340.91054233557));
#17006=CARTESIAN_POINT('Ctrl Pts',(19.9659987040893,0.352425807314618,340.906807689076));
#17007=CARTESIAN_POINT('Ctrl Pts',(19.9621415789345,0.433755022734136,340.901391167795));
#17008=CARTESIAN_POINT('Ctrl Pts',(19.9582844537797,0.51487445884276,340.894305290204));
#17009=CARTESIAN_POINT('Ctrl Pts',(19.9508604763417,0.671008584465399,340.880666791776));
#17010=CARTESIAN_POINT('Ctrl Pts',(19.9434364989037,0.826835967036266,340.860799684575));
#17011=CARTESIAN_POINT('Ctrl Pts',(19.9360125214657,0.981819710343022,340.83472026912));
#17012=CARTESIAN_POINT('Ctrl Pts',(19.9285973054381,1.1366205495139,340.808671631299));
#17013=CARTESIAN_POINT('Ctrl Pts',(19.9211820894105,1.29057936676259,340.776425339938));
#17014=CARTESIAN_POINT('Ctrl Pts',(19.9137668733829,1.44316229341234,340.738049595235));
#17015=CARTESIAN_POINT('Ctrl Pts',(19.9063587922388,1.59559840553823,340.69971077548));
#17016=CARTESIAN_POINT('Ctrl Pts',(19.8989507110947,1.74666090313312,340.655254334086));
#17017=CARTESIAN_POINT('Ctrl Pts',(19.8915426299506,1.89582415606476,340.604799847611));
#17018=CARTESIAN_POINT('Ctrl Pts',(19.8841400627765,2.04487638406384,340.554382915332));
#17019=CARTESIAN_POINT('Ctrl Pts',(19.8767374956025,2.19203183014765,340.497976946422));
#17020=CARTESIAN_POINT('Ctrl Pts',(19.8693349284285,2.3367782332958,340.435751838605));
#17021=CARTESIAN_POINT('Ctrl Pts',(19.8619362586737,2.4814484280949,340.373559492035));
#17022=CARTESIAN_POINT('Ctrl Pts',(19.854537588919,2.62371176394598,340.305554255226));
#17023=CARTESIAN_POINT('Ctrl Pts',(19.8471389191642,2.76307434458884,340.231954771285));
#17024=CARTESIAN_POINT('Ctrl Pts',(19.8397414699602,2.90241393473314,340.158367428974));
#17025=CARTESIAN_POINT('Ctrl Pts',(19.8323440207563,3.03885338971015,340.07918784526));
#17026=CARTESIAN_POINT('Ctrl Pts',(19.8249465715523,3.17192178456038,339.994681446812));
#17027=CARTESIAN_POINT('Ctrl Pts',(19.8175494430888,3.30498440979718,339.910178712415));
#17028=CARTESIAN_POINT('Ctrl Pts',(19.8101523146254,3.43467595047803,339.820349822587));
#17029=CARTESIAN_POINT('Ctrl Pts',(19.8027551861619,3.56055317722488,339.725504378863));
#17030=CARTESIAN_POINT('Ctrl Pts',(19.7953569187253,3.68644978592178,339.630644331309));
#17031=CARTESIAN_POINT('Ctrl Pts',(19.7879586512887,3.8085306131858,339.530766416463));
#17032=CARTESIAN_POINT('Ctrl Pts',(19.7805603838521,3.92638444601334,339.4262213845));
#17033=CARTESIAN_POINT('Ctrl Pts',(19.7731595173264,4.04427968213241,339.321639624767));
#17034=CARTESIAN_POINT('Ctrl Pts',(19.7657586508006,4.15794468819,339.212387730971));
#17035=CARTESIAN_POINT('Ctrl Pts',(19.7583577842748,4.26700425037125,339.098854143515));
#17036=CARTESIAN_POINT('Ctrl Pts',(19.7509487908901,4.37618357037828,338.985195885326));
#17037=CARTESIAN_POINT('Ctrl Pts',(19.7435397975053,4.48074708827724,338.867246813225));
#17038=CARTESIAN_POINT('Ctrl Pts',(19.7361308041205,4.58035864901165,338.74542990976));
#17039=CARTESIAN_POINT('Ctrl Pts',(19.7287172465403,4.68003157390315,338.623537962881));
#17040=CARTESIAN_POINT('Ctrl Pts',(19.72130368896,4.77474623895761,338.497773734186));
#17041=CARTESIAN_POINT('Ctrl Pts',(19.7138901313798,4.86420947693562,338.368589723755));
#17042=CARTESIAN_POINT('Ctrl Pts',(19.7064660192431,4.95380008221146,338.239221796235));
#17043=CARTESIAN_POINT('Ctrl Pts',(19.6990419071064,5.03812412908979,338.106424677452));
#17044=CARTESIAN_POINT('Ctrl Pts',(19.6916177949697,5.11693368912605,337.970676721487));
#17045=CARTESIAN_POINT('Ctrl Pts',(19.6877606698151,5.15787842848923,337.900150193062));
#17046=CARTESIAN_POINT('Ctrl Pts',(19.6839035446605,5.1973354653187,337.82882753027));
#17047=CARTESIAN_POINT('Ctrl Pts',(19.6800464195059,5.23527518119148,337.75677789089));
#17048=CARTESIAN_POINT('Ctrl Pts',(19.6726224420679,5.30829941124691,337.618100799602));
#17049=CARTESIAN_POINT('Ctrl Pts',(19.6651984646299,5.37591987503774,337.476310997487));
#17050=CARTESIAN_POINT('Ctrl Pts',(19.6577744871919,5.43785973467028,337.331868793168));
#17051=CARTESIAN_POINT('Ctrl Pts',(19.6503592711643,5.4997264959491,337.187597052383));
#17052=CARTESIAN_POINT('Ctrl Pts',(19.6429440551367,5.55592585176677,337.040679479844));
#17053=CARTESIAN_POINT('Ctrl Pts',(19.6355288391091,5.60622624615212,336.891601924152));
#17054=CARTESIAN_POINT('Ctrl Pts',(19.628120757965,5.6564782417513,336.742667810133));
#17055=CARTESIAN_POINT('Ctrl Pts',(19.6207126768209,5.70084245715921,336.59157820178));
#17056=CARTESIAN_POINT('Ctrl Pts',(19.6133045956769,5.73913499823034,336.438839822422));
#17057=CARTESIAN_POINT('Ctrl Pts',(19.6059020285029,5.77739903746373,336.28621512903));
#17058=CARTESIAN_POINT('Ctrl Pts',(19.5984994613288,5.80960031049235,336.131944468644));
#17059=CARTESIAN_POINT('Ctrl Pts',(19.5910968941548,5.83560447410472,335.976550553893));
#17060=CARTESIAN_POINT('Ctrl Pts',(19.5836982244,5.86159494663883,335.821238453358));
#17061=CARTESIAN_POINT('Ctrl Pts',(19.5762995546453,5.88139474627604,335.664804643408));
#17062=CARTESIAN_POINT('Ctrl Pts',(19.5689008848905,5.89492045906299,335.507782772276));
#17063=CARTESIAN_POINT('Ctrl Pts',(19.5615034356866,5.90844394052725,335.350786804879));
#17064=CARTESIAN_POINT('Ctrl Pts',(19.5541059864825,5.91569535734219,335.193203340309));
#17065=CARTESIAN_POINT('Ctrl Pts',(19.5467085372786,5.9166430679393,335.035572027014));
#17066=CARTESIAN_POINT('Ctrl Pts',(19.5393114088151,5.91759073744532,334.877947548338));
#17067=CARTESIAN_POINT('Ctrl Pts',(19.5319142803517,5.9122352419354,334.720275598266));
#17068=CARTESIAN_POINT('Ctrl Pts',(19.5245171518882,5.90059707509556,334.563096440992));
#17069=CARTESIAN_POINT('Ctrl Pts',(19.5171188844516,5.88895711626851,334.405893082052));
#17070=CARTESIAN_POINT('Ctrl Pts',(19.5097206170149,5.87103258750171,334.249183039208));
#17071=CARTESIAN_POINT('Ctrl Pts',(19.5023223495783,5.84689591114812,334.093501921293));
#17072=CARTESIAN_POINT('Ctrl Pts',(19.4949214830525,5.82275075532633,333.937766110965));
#17073=CARTESIAN_POINT('Ctrl Pts',(19.4875206165268,5.79238916392071,333.783060313829));
#17074=CARTESIAN_POINT('Ctrl Pts',(19.480119750001,5.75593473502909,333.629910262579));
#17075=CARTESIAN_POINT('Ctrl Pts',(19.4727107566163,5.71944027568943,333.476592037932));
#17076=CARTESIAN_POINT('Ctrl Pts',(19.4653017632315,5.6768397040147,333.324833334135));
#17077=CARTESIAN_POINT('Ctrl Pts',(19.4578927698468,5.62830680226529,333.175145731278));
#17078=CARTESIAN_POINT('Ctrl Pts',(19.4504792122666,5.57974400257445,333.025365915694));
#17079=CARTESIAN_POINT('Ctrl Pts',(19.4430656546863,5.52524171959014,332.877660092704));
#17080=CARTESIAN_POINT('Ctrl Pts',(19.4356520971061,5.4650218206688,332.732519666653));
#17081=CARTESIAN_POINT('Ctrl Pts',(19.4282279849694,5.40471618769645,332.587172606634));
#17082=CARTESIAN_POINT('Ctrl Pts',(19.4208038728328,5.33867683768847,332.444398575769));
#17083=CARTESIAN_POINT('Ctrl Pts',(19.4133797606961,5.26717186048937,332.304664927218));
#17084=CARTESIAN_POINT('Ctrl Pts',(19.4095226355414,5.2300221459965,332.232067671026));
#17085=CARTESIAN_POINT('Ctrl Pts',(19.4056655103867,5.19139786392455,332.160290621645));
#17086=CARTESIAN_POINT('Ctrl Pts',(19.401808385232,5.15134114229636,332.089396111082));
#17087=CARTESIAN_POINT('Ctrl Pts',(19.394384407794,5.07424221869873,331.952942346739));
#17088=CARTESIAN_POINT('Ctrl Pts',(19.3869604303559,4.99160146216521,331.819348258295));
#17089=CARTESIAN_POINT('Ctrl Pts',(19.3795364529179,4.90365614316965,331.689095744052));
#17090=CARTESIAN_POINT('Ctrl Pts',(19.3721212368903,4.8158146128826,331.558996947373));
#17091=CARTESIAN_POINT('Ctrl Pts',(19.3647060208627,4.72268118793632,331.432232181476));
#17092=CARTESIAN_POINT('Ctrl Pts',(19.357290804835,4.62453912056222,331.309259087271));
#17093=CARTESIAN_POINT('Ctrl Pts',(19.3498827236909,4.52649148499099,331.186404317159));
#17094=CARTESIAN_POINT('Ctrl Pts',(19.3424746425467,4.4234450325462,331.067334245353));
#17095=CARTESIAN_POINT('Ctrl Pts',(19.3350665614026,4.31572636201215,330.952477729433));
#17096=CARTESIAN_POINT('Ctrl Pts',(19.3276639942286,4.20808786845238,330.837706703317));
#17097=CARTESIAN_POINT('Ctrl Pts',(19.3202614270546,4.0957843354581,330.727143259459));
#17098=CARTESIAN_POINT('Ctrl Pts',(19.3128588598806,3.97918262240907,330.62118323973));
#17099=CARTESIAN_POINT('Ctrl Pts',(19.3054601901259,3.86264229965235,330.515279007489));
#17100=CARTESIAN_POINT('Ctrl Pts',(19.2980615203711,3.74180857919321,330.41397362283));
#17101=CARTESIAN_POINT('Ctrl Pts',(19.2906628506164,3.61708507713897,330.317626018008));
#17102=CARTESIAN_POINT('Ctrl Pts',(19.2832654014124,3.49238215058916,330.221294307548));
#17103=CARTESIAN_POINT('Ctrl Pts',(19.2758679522084,3.36379101106114,330.12991898163));
#17104=CARTESIAN_POINT('Ctrl Pts',(19.2684705030044,3.23174833737776,330.043818683063));
#17105=CARTESIAN_POINT('Ctrl Pts',(19.261073374541,3.09971138883507,329.957722117655));
#17106=CARTESIAN_POINT('Ctrl Pts',(19.2536762460775,2.96422351631697,329.876900328686));
#17107=CARTESIAN_POINT('Ctrl Pts',(19.246279117614,2.82575012982042,329.801628450532));
#17108=CARTESIAN_POINT('Ctrl Pts',(19.2388808501774,2.68725542187853,329.726344982388));
#17109=CARTESIAN_POINT('Ctrl Pts',(19.2314825827407,2.54577461256367,329.656613304827));
#17110=CARTESIAN_POINT('Ctrl Pts',(19.2240843153041,2.40179729866099,329.592662365022));
#17111=CARTESIAN_POINT('Ctrl Pts',(19.2166834487783,2.25776940401343,329.52868895858));
#17112=CARTESIAN_POINT('Ctrl Pts',(19.2092825822525,2.11124359944051,329.470500484682));
#17113=CARTESIAN_POINT('Ctrl Pts',(19.2018817157267,1.96272887080264,329.418277511178));
#17114=CARTESIAN_POINT('Ctrl Pts',(19.194472722342,1.8140510587948,329.365997191858));
#17115=CARTESIAN_POINT('Ctrl Pts',(19.1870637289571,1.66338031338868,329.319695578886));
#17116=CARTESIAN_POINT('Ctrl Pts',(19.1796547355724,1.5112408767462,329.279503380392));
#17117=CARTESIAN_POINT('Ctrl Pts',(19.1722411779921,1.35900771696247,329.239286422117));
#17118=CARTESIAN_POINT('Ctrl Pts',(19.1648276204119,1.20530442658057,329.205186458456));
#17119=CARTESIAN_POINT('Ctrl Pts',(19.1574140628316,1.05066430315455,329.177282843502));
#17120=CARTESIAN_POINT('Ctrl Pts',(19.1499899506949,0.895804021202609,329.149339502644));
#17121=CARTESIAN_POINT('Ctrl Pts',(19.1425658385582,0.740004611070968,329.127610180481));
#17122=CARTESIAN_POINT('Ctrl Pts',(19.1351417264215,0.583804158799896,329.112122346153));
#17123=CARTESIAN_POINT('Ctrl Pts',(19.1312846012669,0.502651735115012,329.10407579267));
#17124=CARTESIAN_POINT('Ctrl Pts',(19.1274274761125,0.421391067708476,329.097713095492));
#17125=CARTESIAN_POINT('Ctrl Pts',(19.1235703509579,0.340097370784199,329.09303255969));
#17126=CARTESIAN_POINT('Ctrl Pts',(19.1161463735199,0.183627837740699,329.084023727775));
#17127=CARTESIAN_POINT('Ctrl Pts',(19.1087223960819,0.026564063377994,329.081222676123));
#17128=CARTESIAN_POINT('Ctrl Pts',(19.1012984186439,-0.130560313074239,
329.084690661753));
#17129=CARTESIAN_POINT('Ctrl Pts',(19.0938832026163,-0.287499259121399,
329.088154554638));
#17130=CARTESIAN_POINT('Ctrl Pts',(19.0864679865887,-0.444498295405287,
329.097872750002));
#17131=CARTESIAN_POINT('Ctrl Pts',(19.079052770561,-0.601019297883888,329.113854710758));
#17132=CARTESIAN_POINT('Ctrl Pts',(19.0716446894169,-0.757389696642328,
329.129821293751));
#17133=CARTESIAN_POINT('Ctrl Pts',(19.0642366082728,-0.913282608494122,
329.152039605918));
#17134=CARTESIAN_POINT('Ctrl Pts',(19.0568285271287,-1.0681606566089,329.180467082817));
#17135=CARTESIAN_POINT('Ctrl Pts',(19.0494259599547,-1.22292342616362,329.208873400626));
#17136=CARTESIAN_POINT('Ctrl Pts',(19.0420233927807,-1.37667247054935,329.243479613812));
#17137=CARTESIAN_POINT('Ctrl Pts',(19.0346208256067,-1.52887638923313,329.284191435243));
#17138=CARTESIAN_POINT('Ctrl Pts',(19.0272221558519,-1.68100017321957,329.324881822079));
#17139=CARTESIAN_POINT('Ctrl Pts',(19.0198234860972,-1.83158009201295,329.371671318947));
#17140=CARTESIAN_POINT('Ctrl Pts',(19.0124248163424,-1.9800958919896,329.42441475529));
#17141=CARTESIAN_POINT('Ctrl Pts',(19.0050273671384,-2.12858719147049,329.477149490604));
#17142=CARTESIAN_POINT('Ctrl Pts',(18.9976299179345,-2.2750146965983,329.535836091235));
#17143=CARTESIAN_POINT('Ctrl Pts',(18.9902324687305,-2.41887414186912,329.600279780554));
#17144=CARTESIAN_POINT('Ctrl Pts',(18.982835340267,-2.5627273496452,329.664720675706));
#17145=CARTESIAN_POINT('Ctrl Pts',(18.9754382118034,-2.70401237835945,329.734918010649));
#17146=CARTESIAN_POINT('Ctrl Pts',(18.96804108334,-2.84224600158876,329.810629303186));
#17147=CARTESIAN_POINT('Ctrl Pts',(18.9606428159034,-2.98050090934507,329.886352253372));
#17148=CARTESIAN_POINT('Ctrl Pts',(18.9532445484668,-3.11570314875237,329.967590672354));
#17149=CARTESIAN_POINT('Ctrl Pts',(18.9458462810302,-3.24739524433666,330.054056744203));
#17150=CARTESIAN_POINT('Ctrl Pts',(18.9384454145044,-3.37913360473959,330.140553192493));
#17151=CARTESIAN_POINT('Ctrl Pts',(18.9310445479786,-3.50735905433997,330.232280745469));
#17152=CARTESIAN_POINT('Ctrl Pts',(18.9236436814528,-3.63164430832625,330.328909101687));
#17153=CARTESIAN_POINT('Ctrl Pts',(18.9162346880681,-3.75606603940354,330.425643565078));
#17154=CARTESIAN_POINT('Ctrl Pts',(18.9088256946833,-3.87653863937833,330.527289349745));
#17155=CARTESIAN_POINT('Ctrl Pts',(18.9014167012985,-3.99266849548134,330.633476342937));
#17156=CARTESIAN_POINT('Ctrl Pts',(18.8940031437182,-4.1088698915813,330.73972875098));
#17157=CARTESIAN_POINT('Ctrl Pts',(18.886589586138,-4.22072294843319,330.850527679985));
#17158=CARTESIAN_POINT('Ctrl Pts',(18.8791760285577,-4.32787233757927,330.965467611716));
#17159=CARTESIAN_POINT('Ctrl Pts',(18.871751916421,-4.43517427349696,331.080571181481));
#17160=CARTESIAN_POINT('Ctrl Pts',(18.8643278042844,-4.5377589246694,331.199827246245));
#17161=CARTESIAN_POINT('Ctrl Pts',(18.8569036921477,-4.63531200247758,331.322798183103));
#17162=CARTESIAN_POINT('Ctrl Pts',(18.8530465669932,-4.68599475394827,331.38668653569));
#17163=CARTESIAN_POINT('Ctrl Pts',(18.8491894418386,-4.73532009161764,331.451577143998));
#17164=CARTESIAN_POINT('Ctrl Pts',(18.8453323166841,-4.78324873806546,331.517405841575));
#17165=CARTESIAN_POINT('Ctrl Pts',(18.8378562134419,-4.87614681493517,331.644998833679));
#17166=CARTESIAN_POINT('Ctrl Pts',(18.8303801101998,-4.96407508132413,331.776502304084));
#17167=CARTESIAN_POINT('Ctrl Pts',(18.8229040069576,-5.04668908599542,331.911495534762));
#17168=CARTESIAN_POINT('Ctrl Pts',(18.8154369210783,-5.12920344511252,332.046325942256));
#17169=CARTESIAN_POINT('Ctrl Pts',(18.8079698351989,-5.20641611232975,332.184637422512));
#17170=CARTESIAN_POINT('Ctrl Pts',(18.8005027493195,-5.27802363396329,332.325977359515));
#17171=CARTESIAN_POINT('Ctrl Pts',(18.7930432660791,-5.34955824815441,332.46717339078));
#17172=CARTESIAN_POINT('Ctrl Pts',(18.7855837828386,-5.4154989140809,332.611391415902));
#17173=CARTESIAN_POINT('Ctrl Pts',(18.7781242995982,-5.47558619588623,332.758151125985));
#17174=CARTESIAN_POINT('Ctrl Pts',(18.7706710092691,-5.53562359284104,332.904788995207));
#17175=CARTESIAN_POINT('Ctrl Pts',(18.76321771894,-5.58981714403671,333.053964010386));
#17176=CARTESIAN_POINT('Ctrl Pts',(18.7557644286108,-5.6379540075695,333.205172662613));
#17177=CARTESIAN_POINT('Ctrl Pts',(18.7483162710588,-5.68605772120779,333.356277183609));
#17178=CARTESIAN_POINT('Ctrl Pts',(18.7408681135067,-5.72811294622758,333.50941220359));
#17179=CARTESIAN_POINT('Ctrl Pts',(18.7334199559546,-5.76395556104348,333.664055819723));
#17180=CARTESIAN_POINT('Ctrl Pts',(18.7259748909015,-5.79978329389037,333.818635227329));
#17181=CARTESIAN_POINT('Ctrl Pts',(18.7185298258484,-5.82940347153863,333.974721627405));
#17182=CARTESIAN_POINT('Ctrl Pts',(18.7110847607953,-5.85270226027492,334.131779512409));
#17183=CARTESIAN_POINT('Ctrl Pts',(18.7036403547161,-5.87599898680061,334.288823495985));
#17184=CARTESIAN_POINT('Ctrl Pts',(18.6961959486368,-5.89297537834226,334.446838432158));
#17185=CARTESIAN_POINT('Ctrl Pts',(18.6887515425575,-5.9035689811631,334.605280039586));
#17186=CARTESIAN_POINT('Ctrl Pts',(18.6825183632729,-5.91243897360421,334.737942730836));
#17187=CARTESIAN_POINT('Ctrl Pts',(18.6762851839884,-5.91683510150182,334.870904283113));
#17188=CARTESIAN_POINT('Ctrl Pts',(18.6700520047038,-5.91674875184026,335.003843188353));
#17189=CARTESIAN_POINT('',(16.9200520047038,-5.92487683695815,335.002801334899));
#17190=CARTESIAN_POINT('Ctrl Pts',(18.6700498739345,-5.9096022173903,335.003883935737));
#17191=CARTESIAN_POINT('Ctrl Pts',(18.6357313434263,-5.91393132263513,335.734935624386));
#17192=CARTESIAN_POINT('Ctrl Pts',(18.5086668014939,-5.4490096090293,338.436336667853));
#17193=CARTESIAN_POINT('Ctrl Pts',(18.288856248136,-1.40478184172838,341.854138231637));
#17194=CARTESIAN_POINT('Ctrl Pts',(18.0106182138624,5.00358300468427,339.890478507921));
#17195=CARTESIAN_POINT('Ctrl Pts',(17.7323801795881,6.82023358046314,333.438898840832));
#17196=CARTESIAN_POINT('Ctrl Pts',(17.4541421453145,2.37805646593319,328.419918665697));
#17197=CARTESIAN_POINT('Ctrl Pts',(17.1833660870195,-4.06876805880988,329.412041351052));
#17198=CARTESIAN_POINT('Ctrl Pts',(17.0053360401494,-5.91432262045667,333.198073718685));
#17199=CARTESIAN_POINT('Ctrl Pts',(16.9200520047038,-5.92487683695815,335.002801334899));
#17200=CARTESIAN_POINT('',(15.1700520047038,-5.91816246639694,334.994658507115));
#17201=CARTESIAN_POINT('Ctrl Pts',(16.9200520047038,-5.92487683695815,335.002801334899));
#17202=CARTESIAN_POINT('Ctrl Pts',(16.9125900287247,-5.92580028423173,335.160707020889));
#17203=CARTESIAN_POINT('Ctrl Pts',(16.9051280527456,-5.92003632359302,335.318544233041));
#17204=CARTESIAN_POINT('Ctrl Pts',(16.8049200653418,-5.74990729362354,337.430694969049));
#17205=CARTESIAN_POINT('Ctrl Pts',(16.6194280424926,-3.30166561657978,341.168600090581));
#17206=CARTESIAN_POINT('Ctrl Pts',(16.3411900082185,3.40058670281529,341.114624518141));
#17207=CARTESIAN_POINT('Ctrl Pts',(16.0629519739446,6.98217079761695,335.449348277112));
#17208=CARTESIAN_POINT('Ctrl Pts',(15.7847139396707,4.15631980811429,329.371711754549));
#17209=CARTESIAN_POINT('Ctrl Pts',(15.5064759053968,-2.48372452211122,328.459072281435));
#17210=CARTESIAN_POINT('Ctrl Pts',(15.3015885937412,-5.69488085772441,332.207123730002));
#17211=CARTESIAN_POINT('Ctrl Pts',(15.1894472935101,-5.92197975965578,334.583014993244));
#17212=CARTESIAN_POINT('Ctrl Pts',(15.1700520047038,-5.91816246639694,334.994658507115));
#17213=CARTESIAN_POINT('',(13.4200520047038,-5.90696799723574,334.999957581698));
#17214=CARTESIAN_POINT('Ctrl Pts',(15.1700520047038,-5.91816246639694,334.994658507115));
#17215=CARTESIAN_POINT('Ctrl Pts',(15.0967012820855,-5.90372590802558,336.551446318067));
#17216=CARTESIAN_POINT('Ctrl Pts',(14.9306045480426,-4.47531169421653,340.100099714576));
#17217=CARTESIAN_POINT('Ctrl Pts',(14.671761802575,1.51499000097043,341.830624291977));
#17218=CARTESIAN_POINT('Ctrl Pts',(14.3935237683009,6.56386571174399,337.422455332818));
#17219=CARTESIAN_POINT('Ctrl Pts',(14.115285734027,5.5891787413283,330.791234870104));
#17220=CARTESIAN_POINT('Ctrl Pts',(13.8370476997532,-0.5146150638219,328.022336045841));
#17221=CARTESIAN_POINT('Ctrl Pts',(13.6053031233121,-5.20512640970425,331.049429673258));
#17222=CARTESIAN_POINT('Ctrl Pts',(13.4663045582956,-5.90703089584316,334.013588927452));
#17223=CARTESIAN_POINT('Ctrl Pts',(13.4200520047038,-5.90696799723574,334.999957581698));
#17224=CARTESIAN_POINT('',(11.6700520047038,-5.91800630270739,335.005358570736));
#17225=CARTESIAN_POINT('Ctrl Pts',(13.4200520047038,-5.90696799723574,334.999957581698));
#17226=CARTESIAN_POINT('Ctrl Pts',(13.373558546871,-5.90690477102391,335.991463690498));
#17227=CARTESIAN_POINT('Ctrl Pts',(13.2343190776133,-5.19974192404982,338.960929310428));
#17228=CARTESIAN_POINT('Ctrl Pts',(13.0023335969315,-0.496507558018799,
341.978975796318));
#17229=CARTESIAN_POINT('Ctrl Pts',(12.7240955626572,5.60008090817167,339.194248054982));
#17230=CARTESIAN_POINT('Ctrl Pts',(12.4458575283836,6.55755778108378,332.560520780316));
#17231=CARTESIAN_POINT('Ctrl Pts',(12.1676194941094,1.49726066940123,328.165467579416));
#17232=CARTESIAN_POINT('Ctrl Pts',(11.909017652883,-4.48295950437942,329.909905021892));
#17233=CARTESIAN_POINT('Ctrl Pts',(11.7431618230811,-5.90360988232098,333.453578574384));
#17234=CARTESIAN_POINT('Ctrl Pts',(11.6700520047038,-5.91800630270739,335.005358570736));
#17235=CARTESIAN_POINT('',(9.92005200470384,-5.92497233409181,334.997279528669));
#17236=CARTESIAN_POINT('Ctrl Pts',(11.6700520047038,-5.91800630270739,335.005358570736));
#17237=CARTESIAN_POINT('Ctrl Pts',(11.6504158116564,-5.92187296379579,335.422143241411));
#17238=CARTESIAN_POINT('Ctrl Pts',(11.5380336071844,-5.69140174168275,337.803246946089));
#17239=CARTESIAN_POINT('Ctrl Pts',(11.3329053912876,-2.46674364463169,341.54735051138));
#17240=CARTESIAN_POINT('Ctrl Pts',(11.0546673570137,4.17091021541455,340.617484404395));
#17241=CARTESIAN_POINT('Ctrl Pts',(10.77642932274,6.98098129236843,334.532535761013));
#17242=CARTESIAN_POINT('Ctrl Pts',(10.4981912884658,3.38470895373127,328.876572173443));
#17243=CARTESIAN_POINT('Ctrl Pts',(10.219953254192,-3.31766097947469,328.839987876369));
#17244=CARTESIAN_POINT('Ctrl Pts',(10.0272401596045,-5.85112546410686,332.729993995301));
#17245=CARTESIAN_POINT('Ctrl Pts',(9.92727307644188,-5.92584438465563,334.844478228084));
#17246=CARTESIAN_POINT('Ctrl Pts',(9.92005200470384,-5.92497233409181,334.997279528669));
#17247=CARTESIAN_POINT('',(8.17005320238592,-5.91279716752603,334.996073171796));
#17248=CARTESIAN_POINT('Ctrl Pts',(9.92005200470384,-5.92497233409181,334.997279528669));
#17249=CARTESIAN_POINT('Ctrl Pts',(9.83452706501725,-5.9146439403879,336.807027789136));
#17250=CARTESIAN_POINT('Ctrl Pts',(9.6562561139059,-4.05999276733219,340.597629687215));
#17251=CARTESIAN_POINT('Ctrl Pts',(9.38523915137018,2.39512310876783,341.573888717416));
#17252=CARTESIAN_POINT('Ctrl Pts',(9.10700111709619,6.8242603936016,336.543398329723));
#17253=CARTESIAN_POINT('Ctrl Pts',(8.82876308282223,4.99087814415887,330.096555138453));
#17254=CARTESIAN_POINT('Ctrl Pts',(8.55052504854831,-1.42256592733979,328.149528914564));
#17255=CARTESIAN_POINT('Ctrl Pts',(8.3309554007549,-5.45348075719915,331.574058185186));
#17256=CARTESIAN_POINT('Ctrl Pts',(8.20413176438612,-5.91407537989431,334.270167138421));
#17257=CARTESIAN_POINT('Ctrl Pts',(8.17005413944201,-5.90970551307915,334.996055251526));
#17258=CARTESIAN_POINT('',(6.4200506595843,-5.91295548729207,335.00439982517));
#17259=CARTESIAN_POINT('Ctrl Pts',(8.1700520047039,-5.91674871207825,334.996096076278));
#17260=CARTESIAN_POINT('Ctrl Pts',(8.16261128968737,-5.91685341255526,335.154779097913));
#17261=CARTESIAN_POINT('Ctrl Pts',(8.15517057467084,-5.91057013696326,335.313497435384));
#17262=CARTESIAN_POINT('Ctrl Pts',(8.14772985965431,-5.89791707973895,335.471704020572));
#17263=CARTESIAN_POINT('Ctrl Pts',(8.14028890613604,-5.88526361693856,335.629915676851));
#17264=CARTESIAN_POINT('Ctrl Pts',(8.13284795261774,-5.86623999404314,335.787615182283));
#17265=CARTESIAN_POINT('Ctrl Pts',(8.12540699909948,-5.84091638686498,335.944259669875));
#17266=CARTESIAN_POINT('Ctrl Pts',(8.11796440350357,-5.81558719124586,336.100938725942));
#17267=CARTESIAN_POINT('Ctrl Pts',(8.11052180790766,-5.78395530032008,336.256561938121));
#17268=CARTESIAN_POINT('Ctrl Pts',(8.10307921231174,-5.74614219166644,336.410595787478));
#17269=CARTESIAN_POINT('Ctrl Pts',(8.09563357036449,-5.70831360561479,336.564692684897));
#17270=CARTESIAN_POINT('Ctrl Pts',(8.08818792841724,-5.66429884968457,336.717198567574));
#17271=CARTESIAN_POINT('Ctrl Pts',(8.08074228646998,-5.61426950163742,336.867594315017));
#17272=CARTESIAN_POINT('Ctrl Pts',(8.0732873930601,-5.56417799042865,337.018176934277));
#17273=CARTESIAN_POINT('Ctrl Pts',(8.06583249965017,-5.50805707313053,337.166643831786));
#17274=CARTESIAN_POINT('Ctrl Pts',(8.05837760624027,-5.44612715732812,337.312494226742));
#17275=CARTESIAN_POINT('Ctrl Pts',(8.05091788039282,-5.38415709709514,337.458439165359));
#17276=CARTESIAN_POINT('Ctrl Pts',(8.04345815454545,-5.31637068928892,337.60176388955));
#17277=CARTESIAN_POINT('Ctrl Pts',(8.03599842869801,-5.24303453243653,337.741991877117));
#17278=CARTESIAN_POINT('Ctrl Pts',(8.02852639187366,-5.16957734704341,337.882451286529));
#17279=CARTESIAN_POINT('Ctrl Pts',(8.02105435504934,-5.09055229266335,338.019803428556));
#17280=CARTESIAN_POINT('Ctrl Pts',(8.01358231822499,-5.00627021212153,338.15359939208));
#17281=CARTESIAN_POINT('Ctrl Pts',(8.00707120548348,-4.9328270343914,338.270188833934));
#17282=CARTESIAN_POINT('Ctrl Pts',(8.00056009274194,-4.85539278182729,338.384078304153));
#17283=CARTESIAN_POINT('Ctrl Pts',(7.99404898000043,-4.77419758737321,338.49499183965));
#17284=CARTESIAN_POINT('Ctrl Pts',(7.98662520049577,-4.68162121150709,338.621452195092));
#17285=CARTESIAN_POINT('Ctrl Pts',(7.97920142099114,-4.58387709032002,338.744422551539));
#17286=CARTESIAN_POINT('Ctrl Pts',(7.97177764148648,-4.48125737924786,338.86345219505));
#17287=CARTESIAN_POINT('Ctrl Pts',(7.96436262351687,-4.37875877982704,338.982341359928));
#17288=CARTESIAN_POINT('Ctrl Pts',(7.95694760554722,-4.27139628560484,339.09729878947));
#17289=CARTESIAN_POINT('Ctrl Pts',(7.94953258757761,-4.15950487043829,339.207903254033));
#17290=CARTESIAN_POINT('Ctrl Pts',(7.94212470443006,-4.04772111857621,339.318401293611));
#17291=CARTESIAN_POINT('Ctrl Pts',(7.93471682128259,-3.93141738495927,339.424554446049));
#17292=CARTESIAN_POINT('Ctrl Pts',(7.92730893813504,-3.81096831371177,339.525975151764));
#17293=CARTESIAN_POINT('Ctrl Pts',(7.91990656871137,-3.69060889330077,339.627320369549));
#17294=CARTESIAN_POINT('Ctrl Pts',(7.91250419928765,-3.56611056300302,339.723939914813));
#17295=CARTESIAN_POINT('Ctrl Pts',(7.90510182986398,-3.43788407581089,339.815483739334));
#17296=CARTESIAN_POINT('Ctrl Pts',(7.89770335742933,-3.30972509365438,339.906979370464));
#17297=CARTESIAN_POINT('Ctrl Pts',(7.89030488499471,-3.17784216642058,339.993404386215));
#17298=CARTESIAN_POINT('Ctrl Pts',(7.88290641256006,-3.04267821921571,340.074449705812));
#17299=CARTESIAN_POINT('Ctrl Pts',(7.87550915941151,-2.90753654735533,340.155481668944));
#17300=CARTESIAN_POINT('Ctrl Pts',(7.86811190626295,-2.76911524845875,340.231135503748));
#17301=CARTESIAN_POINT('Ctrl Pts',(7.8607146531144,-2.62788535456432,340.301146020038));
#17302=CARTESIAN_POINT('Ctrl Pts',(7.85331771990311,-2.48666156897862,340.371153508316));
#17303=CARTESIAN_POINT('Ctrl Pts',(7.84592078669181,-2.34262976432439,340.435517997615));
#17304=CARTESIAN_POINT('Ctrl Pts',(7.83852385348052,-2.19628439986807,340.494020877044));
#17305=CARTESIAN_POINT('Ctrl Pts',(7.83112578032705,-2.04991648211161,340.552532772358));
#17306=CARTESIAN_POINT('Ctrl Pts',(7.82372770717357,-1.90123464121756,340.605181120595));
#17307=CARTESIAN_POINT('Ctrl Pts',(7.81632963402009,-1.75075193607407,340.65179601727));
#17308=CARTESIAN_POINT('Ctrl Pts',(7.80892896064176,-1.60021634028417,340.698427297835));
#17309=CARTESIAN_POINT('Ctrl Pts',(7.80152828726342,-1.44787897632691,340.739020794368));
#17310=CARTESIAN_POINT('Ctrl Pts',(7.79412761388508,-1.29426648061765,340.773456922819));
#17311=CARTESIAN_POINT('Ctrl Pts',(7.78671881095491,-1.14048524340577,340.807930878948));
#17312=CARTESIAN_POINT('Ctrl Pts',(7.77931000802474,-0.985426441546715,
340.836233877646));
#17313=CARTESIAN_POINT('Ctrl Pts',(7.77190120509457,-0.829626011028604,
340.858297640469));
#17314=CARTESIAN_POINT('Ctrl Pts',(7.76448783672733,-0.673729573494713,
340.880374999378));
#17315=CARTESIAN_POINT('Ctrl Pts',(7.7570744683601,-0.517090967133179,340.896205423853));
#17316=CARTESIAN_POINT('Ctrl Pts',(7.74966109999286,-0.360249093448792,
340.905772697384));
#17317=CARTESIAN_POINT('Ctrl Pts',(7.74223717350793,-0.203183845600268,
340.915353596625));
#17318=CARTESIAN_POINT('Ctrl Pts',(7.734813247023,-0.0459151243963421,340.918653522137));
#17319=CARTESIAN_POINT('Ctrl Pts',(7.72738932053807,0.111019502717101,340.915708345796));
#17320=CARTESIAN_POINT('Ctrl Pts',(7.72352986226756,0.192604718541949,340.914177244267));
#17321=CARTESIAN_POINT('Ctrl Pts',(7.71967040399709,0.274099735862142,340.910959182106));
#17322=CARTESIAN_POINT('Ctrl Pts',(7.71581094572659,0.355429922037766,340.906064690894));
#17323=CARTESIAN_POINT('Ctrl Pts',(7.70838684006637,0.511877758291882,340.896649581992));
#17324=CARTESIAN_POINT('Ctrl Pts',(7.70096273440614,0.668187230436248,340.880999674986));
#17325=CARTESIAN_POINT('Ctrl Pts',(7.69353862874593,0.823821184575319,340.859116760941));
#17326=CARTESIAN_POINT('Ctrl Pts',(7.68612328556047,0.979271448091348,340.837259674719));
#17327=CARTESIAN_POINT('Ctrl Pts',(7.67870794237503,1.13404741466381,340.809184276456));
#17328=CARTESIAN_POINT('Ctrl Pts',(7.67129259918957,1.28761355480564,340.77494431973));
#17329=CARTESIAN_POINT('Ctrl Pts',(7.66388439205692,1.44103191269953,340.740737313351));
#17330=CARTESIAN_POINT('Ctrl Pts',(7.65647618492427,1.59324240016855,340.700377639446));
#17331=CARTESIAN_POINT('Ctrl Pts',(7.64906797779162,1.74371633521224,340.653970631761));
#17332=CARTESIAN_POINT('Ctrl Pts',(7.64166528590329,1.89407824578052,340.607598173054));
#17333=CARTESIAN_POINT('Ctrl Pts',(7.63426259401497,2.04270582303051,340.555187454431));
#17334=CARTESIAN_POINT('Ctrl Pts',(7.62685990212665,2.18908238948749,340.496894473658));
#17335=CARTESIAN_POINT('Ctrl Pts',(7.61946110903723,2.33538186334032,340.438632194232));
#17336=CARTESIAN_POINT('Ctrl Pts',(7.61206231594777,2.47943234164554,340.374493960295));
#17337=CARTESIAN_POINT('Ctrl Pts',(7.60466352285835,2.62073418769751,340.304684993469));
#17338=CARTESIAN_POINT('Ctrl Pts',(7.59726595275613,2.76201267719003,340.234887565751));
#17339=CARTESIAN_POINT('Ctrl Pts',(7.58986838265393,2.90054310188425,340.159421430637));
#17340=CARTESIAN_POINT('Ctrl Pts',(7.58247081255172,3.03584752374562,340.078539196961));
#17341=CARTESIAN_POINT('Ctrl Pts',(7.57507356471138,3.1711460513126,339.997660486775));
#17342=CARTESIAN_POINT('Ctrl Pts',(7.567676316871,3.30321853515081,339.911366338648));
#17343=CARTESIAN_POINT('Ctrl Pts',(7.56027906903066,3.43161352860415,339.819954268746));
#17344=CARTESIAN_POINT('Ctrl Pts',(7.55288068383599,3.56002826326455,339.728528143898));
#17345=CARTESIAN_POINT('Ctrl Pts',(7.54548229864138,3.68476407766208,339.631982746917));
#17346=CARTESIAN_POINT('Ctrl Pts',(7.53808391344671,3.80540041739779,339.530657593084));
#17347=CARTESIAN_POINT('Ctrl Pts',(7.5306829308802,3.92607910927172,339.429296866745));
#17348=CARTESIAN_POINT('Ctrl Pts',(7.52328194831367,4.04265517541928,339.323153282448));
#17349=CARTESIAN_POINT('Ctrl Pts',(7.51588096574716,4.15474302842909,339.212605005246));
#17350=CARTESIAN_POINT('Ctrl Pts',(7.50847185950113,4.2669539145344,339.101935384861));
#17351=CARTESIAN_POINT('Ctrl Pts',(7.50106275325512,4.37466648318501,338.986851678421));
#17352=CARTESIAN_POINT('Ctrl Pts',(7.4936536470091,4.47753325759919,338.867767636453));
#17353=CARTESIAN_POINT('Ctrl Pts',(7.48623997820027,4.58046337786138,338.748610261967));
#17354=CARTESIAN_POINT('Ctrl Pts',(7.47882630939142,4.67854152580117,338.625447934506));
#17355=CARTESIAN_POINT('Ctrl Pts',(7.4714126405826,4.7714623984152,338.498725073939));
#17356=CARTESIAN_POINT('Ctrl Pts',(7.46398842071034,4.8645155151376,338.371821862594));
#17357=CARTESIAN_POINT('Ctrl Pts',(7.45656420083807,4.95239648958604,338.241348306394));
#17358=CARTESIAN_POINT('Ctrl Pts',(7.44913998096581,5.03484454188067,338.107775893078));
#17359=CARTESIAN_POINT('Ctrl Pts',(7.44528429112804,5.07766306326687,338.0384064771));
#17360=CARTESIAN_POINT('Ctrl Pts',(7.44142860129029,5.11901702152002,337.968201640311));
#17361=CARTESIAN_POINT('Ctrl Pts',(7.43757291145252,5.15887497375226,337.897229636686));
#17362=CARTESIAN_POINT('Ctrl Pts',(7.43014849024341,5.23562446304105,337.760567697803));
#17363=CARTESIAN_POINT('Ctrl Pts',(7.42272406903432,5.30705548352638,337.620647962498));
#17364=CARTESIAN_POINT('Ctrl Pts',(7.41529964782521,5.37287886999374,337.477923164845));
#17365=CARTESIAN_POINT('Ctrl Pts',(7.40788398540425,5.4386246028526,337.335366743451));
#17366=CARTESIAN_POINT('Ctrl Pts',(7.40046832298325,5.49877571517569,337.190012182323));
#17367=CARTESIAN_POINT('Ctrl Pts',(7.39305266056229,5.55308761983282,337.042338965245));
#17368=CARTESIAN_POINT('Ctrl Pts',(7.38564413085279,5.60734728490267,336.894807786786));
#17369=CARTESIAN_POINT('Ctrl Pts',(7.37823560114328,5.65577879560776,336.744962740159));
#17370=CARTESIAN_POINT('Ctrl Pts',(7.37082707143378,5.69818464721681,336.593305459955));
#17371=CARTESIAN_POINT('Ctrl Pts',(7.36342405396734,5.74055894717253,336.441761018846));
#17372=CARTESIAN_POINT('Ctrl Pts',(7.35602103650091,5.77691641496336,336.288407386816));
#17373=CARTESIAN_POINT('Ctrl Pts',(7.34861801903446,5.80710864800857,336.133763517108));
#17374=CARTESIAN_POINT('Ctrl Pts',(7.34121889770174,5.8372849911848,335.979201034915));
#17375=CARTESIAN_POINT('Ctrl Pts',(7.33381977636903,5.86130249032085,335.823350032718));
#17376=CARTESIAN_POINT('Ctrl Pts',(7.32642065503632,5.87906335880463,335.666741768349));
#17377=CARTESIAN_POINT('Ctrl Pts',(7.31902275378596,5.89682129859981,335.510159327989));
#17378=CARTESIAN_POINT('Ctrl Pts',(7.31162485253557,5.90832461331464,335.352820243706));
#17379=CARTESIAN_POINT('Ctrl Pts',(7.30422695128522,5.91352710806851,335.195263167645));
#17380=CARTESIAN_POINT('Ctrl Pts',(7.29682937053205,5.91872937743618,335.037712917385));
#17381=CARTESIAN_POINT('Ctrl Pts',(7.28943178977891,5.9176313572819,334.879945067081));
#17382=CARTESIAN_POINT('Ctrl Pts',(7.28203420902574,5.91023895237013,334.722500291195));
#17383=CARTESIAN_POINT('Ctrl Pts',(7.27463548944905,5.90284540943165,334.56503127741));
#17384=CARTESIAN_POINT('Ctrl Pts',(7.26723676987232,5.88915556984469,334.407885809846));
#17385=CARTESIAN_POINT('Ctrl Pts',(7.25983805029563,5.86922737377835,334.251601311204));
#17386=CARTESIAN_POINT('Ctrl Pts',(7.25243673217286,5.84929217861774,334.095261923001));
#17387=CARTESIAN_POINT('Ctrl Pts',(7.24503541405014,5.8231143118444,333.939784475702));
#17388=CARTESIAN_POINT('Ctrl Pts',(7.23763409592738,5.79080313744415,333.785697901728));
#17389=CARTESIAN_POINT('Ctrl Pts',(7.23022465405535,5.7584564980261,333.63144220103));
#17390=CARTESIAN_POINT('Ctrl Pts',(7.22281521218332,5.7199631834998,333.478580787866));
#17391=CARTESIAN_POINT('Ctrl Pts',(7.21540577031129,5.6754831059991,333.327629802939));
#17392=CARTESIAN_POINT('Ctrl Pts',(7.20799176533832,5.63097563546562,333.176585854926));
#17393=CARTESIAN_POINT('Ctrl Pts',(7.20057776036531,5.58047417462009,333.027455032182));
#17394=CARTESIAN_POINT('Ctrl Pts',(7.19316375539233,5.52418724856345,332.880734607155));
#17395=CARTESIAN_POINT('Ctrl Pts',(7.18573920142785,5.46782023484748,332.733805421476));
#17396=CARTESIAN_POINT('Ctrl Pts',(7.17831464746342,5.40565146237075,332.589293825029));
#17397=CARTESIAN_POINT('Ctrl Pts',(7.17089009349894,5.33793631198391,332.447674297488));
#17398=CARTESIAN_POINT('Ctrl Pts',(7.1670383547255,5.30280678480394,332.374204372168));
#17399=CARTESIAN_POINT('Ctrl Pts',(7.16318661595206,5.26618526045492,332.301512369746));
#17400=CARTESIAN_POINT('Ctrl Pts',(7.15933487717862,5.22811199131594,332.229661470369));
#17401=CARTESIAN_POINT('Ctrl Pts',(7.15191226308202,5.15474170302862,332.091198939563));
#17402=CARTESIAN_POINT('Ctrl Pts',(7.14448964898538,5.0757560925081,331.955443846164));
#17403=CARTESIAN_POINT('Ctrl Pts',(7.13706703488879,4.9913791561326,331.822884219575));
#17404=CARTESIAN_POINT('Ctrl Pts',(7.12965318375392,4.90710183316211,331.69048108973));
#17405=CARTESIAN_POINT('Ctrl Pts',(7.122239332619,4.81744605215242,331.561266229439));
#17406=CARTESIAN_POINT('Ctrl Pts',(7.11482548148413,4.7226824349692,331.435704672599));
#17407=CARTESIAN_POINT('Ctrl Pts',(7.10741876549543,4.6280100190048,331.310263957147));
#17408=CARTESIAN_POINT('Ctrl Pts',(7.1000120495068,4.5282397766885,331.188469841576));
#17409=CARTESIAN_POINT('Ctrl Pts',(7.09260533351809,4.42368644346961,331.070759766524));
#17410=CARTESIAN_POINT('Ctrl Pts',(7.08520413048362,4.31921093120953,330.953137305235));
#17411=CARTESIAN_POINT('Ctrl Pts',(7.07780292744912,4.20995966364025,330.839593109715));
#17412=CARTESIAN_POINT('Ctrl Pts',(7.07040172441464,4.0962885189564,330.730532710985));
#17413=CARTESIAN_POINT('Ctrl Pts',(7.06300441651111,3.98267719751919,330.621529708942));
#17414=CARTESIAN_POINT('Ctrl Pts',(7.05560710860761,3.86465090025415,330.517006061975));
#17415=CARTESIAN_POINT('Ctrl Pts',(7.04820980070409,3.74260324997276,330.41733140236));
#17416=CARTESIAN_POINT('Ctrl Pts',(7.04081370563754,3.62057561020136,330.317673085058));
#17417=CARTESIAN_POINT('Ctrl Pts',(7.033417610571,3.49452821479502,330.222862413263));
#17418=CARTESIAN_POINT('Ctrl Pts',(7.02602151550445,3.36488882944026,330.133229640921));
#17419=CARTESIAN_POINT('Ctrl Pts',(7.01862573626671,3.23525497995955,330.043600696087));
#17420=CARTESIAN_POINT('Ctrl Pts',(7.01122995702894,3.10202975260531,329.959149423422));
#17421=CARTESIAN_POINT('Ctrl Pts',(7.00383417779119,2.96567081092048,329.880163361615));
#17422=CARTESIAN_POINT('Ctrl Pts',(6.9964372535232,2.82929075785482,329.801165071017));
#17423=CARTESIAN_POINT('Ctrl Pts',(6.9890403292552,2.68977634752289,329.72763386319));
#17424=CARTESIAN_POINT('Ctrl Pts',(6.98164340498721,2.54761066928102,329.659811759847));
#17425=CARTESIAN_POINT('Ctrl Pts',(6.9742438744223,2.40539489914216,329.591965759472));
#17426=CARTESIAN_POINT('Ctrl Pts',(6.96684434385742,2.26052633793631,329.5298330293));
#17427=CARTESIAN_POINT('Ctrl Pts',(6.95944481329252,2.11350876220303,329.473607752377));
#17428=CARTESIAN_POINT('Ctrl Pts',(6.95203713822121,1.96632936734119,329.417320589483));
#17429=CARTESIAN_POINT('Ctrl Pts',(6.94462946314989,1.81699658311566,329.366953998521));
#17430=CARTESIAN_POINT('Ctrl Pts',(6.93722178807857,1.66603078181876,329.322652732435));
#17431=CARTESIAN_POINT('Ctrl Pts',(6.92980954078437,1.51497180023448,329.278324122376));
#17432=CARTESIAN_POINT('Ctrl Pts',(6.9223972934902,1.36227815445302,329.240068387432));
#17433=CARTESIAN_POINT('Ctrl Pts',(6.91498504619599,1.20848065000577,329.207979188482));
#17434=CARTESIAN_POINT('Ctrl Pts',(6.90756222056022,1.05446365442841,329.175844193635));
#17435=CARTESIAN_POINT('Ctrl Pts',(6.90013939492441,0.899340021115722,329.149893372611));
#17436=CARTESIAN_POINT('Ctrl Pts',(6.89271656928864,0.74364673873536,329.130168648891));
#17437=CARTESIAN_POINT('Ctrl Pts',(6.88884332716065,0.66240573834677,329.119876256933));
#17438=CARTESIAN_POINT('Ctrl Pts',(6.88497008503266,0.581009665556887,329.111278224026));
#17439=CARTESIAN_POINT('Ctrl Pts',(6.88109684290467,0.499534715108384,329.104374873612));
#17440=CARTESIAN_POINT('Ctrl Pts',(6.87367165959166,0.34334348757668,329.09114083334));
#17441=CARTESIAN_POINT('Ctrl Pts',(6.86624647627868,0.186390603730519,329.084098033159));
#17442=CARTESIAN_POINT('Ctrl Pts',(6.85882129296567,0.0292079906773089,
329.083322092949));
#17443=CARTESIAN_POINT('Ctrl Pts',(6.85140487722359,-0.127789022956951,
329.082547068961));
#17444=CARTESIAN_POINT('Ctrl Pts',(6.84398846148152,-0.285014856387427,
329.088024177195));
#17445=CARTESIAN_POINT('Ctrl Pts',(6.83657204573944,-0.441931705204789,
329.099777382977));
#17446=CARTESIAN_POINT('Ctrl Pts',(6.82916277208321,-0.598697441457273,
329.111519270298));
#17447=CARTESIAN_POINT('Ctrl Pts',(6.82175349842697,-0.755154415918136,
329.129525195049));
#17448=CARTESIAN_POINT('Ctrl Pts',(6.81434422477074,-0.910764169096375,
329.153767094035));
#17449=CARTESIAN_POINT('Ctrl Pts',(6.80694047332627,-1.06625794464312,329.177990925272));
#17450=CARTESIAN_POINT('Ctrl Pts',(6.7995367218818,-1.22090538914842,329.208441419188));
#17451=CARTESIAN_POINT('Ctrl Pts',(6.79213297043734,-1.37417262180029,329.245038647567));
#17452=CARTESIAN_POINT('Ctrl Pts',(6.78473312569383,-1.52735898068852,329.281616564868));
#17453=CARTESIAN_POINT('Ctrl Pts',(6.77733328095034,-1.67916621619237,329.324334670712));
#17454=CARTESIAN_POINT('Ctrl Pts',(6.76993343620683,-1.82907021593176,329.373061870991));
#17455=CARTESIAN_POINT('Ctrl Pts',(6.76253482950683,-1.9789491357295,329.421780918884));
#17456=CARTESIAN_POINT('Ctrl Pts',(6.75513622280677,-2.12692509732166,329.4765069505));
#17457=CARTESIAN_POINT('Ctrl Pts',(6.74773761610678,-2.2724886305767,329.53705885201));
#17458=CARTESIAN_POINT('Ctrl Pts',(6.74033934110337,-2.41804563788316,329.597608038839));
#17459=CARTESIAN_POINT('Ctrl Pts',(6.73294106610005,-2.56119008744361,329.663982432911));
#17460=CARTESIAN_POINT('Ctrl Pts',(6.72554279109664,-2.70143224873621,329.735952662828));
#17461=CARTESIAN_POINT('Ctrl Pts',(6.71814338902837,-2.84169577474058,329.807933856803));
#17462=CARTESIAN_POINT('Ctrl Pts',(6.71074398696007,-2.97905580016819,329.885512413671));
#17463=CARTESIAN_POINT('Ctrl Pts',(6.70334458489179,-3.11304710699253,329.968412946977));
#17464=CARTESIAN_POINT('Ctrl Pts',(6.69594259660327,-3.24708524611863,330.051342455468));
#17465=CARTESIAN_POINT('Ctrl Pts',(6.68854060831471,-3.37775200530665,330.139597447738));
#17466=CARTESIAN_POINT('Ctrl Pts',(6.68113862002619,-3.50461119295173,330.232859248067));
#17467=CARTESIAN_POINT('Ctrl Pts',(6.67372852998265,-3.63160923275648,330.326223126951));
#17468=CARTESIAN_POINT('Ctrl Pts',(6.66631843993913,-3.75479107744746,330.424604536922));
#17469=CARTESIAN_POINT('Ctrl Pts',(6.6589083498956,-3.87375311502474,330.527644092166));
#17470=CARTESIAN_POINT('Ctrl Pts',(6.65149370824658,-3.99278822435404,330.630746938868));
#17471=CARTESIAN_POINT('Ctrl Pts',(6.64407906659752,-4.10759809023561,330.73851337755));
#17472=CARTESIAN_POINT('Ctrl Pts',(6.63666442494849,-4.21781640714295,330.850547588159));
#17473=CARTESIAN_POINT('Ctrl Pts',(6.62923925762629,-4.32819118771191,330.962740840235));
#17474=CARTESIAN_POINT('Ctrl Pts',(6.6218140903041,-4.43396115124822,331.079213688722));
#17475=CARTESIAN_POINT('Ctrl Pts',(6.6143889229819,-4.53480014405338,331.199537105037));
#17476=CARTESIAN_POINT('Ctrl Pts',(6.61054555153154,-4.58699583058992,331.261818204304));
#17477=CARTESIAN_POINT('Ctrl Pts',(6.60670218008119,-4.63787109250377,331.325130477312));
#17478=CARTESIAN_POINT('Ctrl Pts',(6.60285880863083,-4.68738535868419,331.389411535263));
#17479=CARTESIAN_POINT('Ctrl Pts',(6.59524185846718,-4.78551474918296,331.516806355463));
#17480=CARTESIAN_POINT('Ctrl Pts',(6.58762490830355,-4.87860233446218,331.648406409801));
#17481=CARTESIAN_POINT('Ctrl Pts',(6.58000795813993,-4.96626841017571,331.783774162067));
#17482=CARTESIAN_POINT('Ctrl Pts',(6.57258433273256,-5.05170944537365,331.915706164176));
#17483=CARTESIAN_POINT('Ctrl Pts',(6.56516070732519,-5.13200058453951,332.051216610025));
#17484=CARTESIAN_POINT('Ctrl Pts',(6.55773708191782,-5.20682964581119,332.189865554462));
#17485=CARTESIAN_POINT('Ctrl Pts',(6.55032058432585,-5.28158685974334,332.328381374713));
#17486=CARTESIAN_POINT('Ctrl Pts',(6.5429040867338,-5.35089225899854,332.470029371125));
#17487=CARTESIAN_POINT('Ctrl Pts',(6.53548758914184,-5.41447694055085,332.614340757203));
#17488=CARTESIAN_POINT('Ctrl Pts',(6.52807676346715,-5.47801299442558,332.758541778215));
#17489=CARTESIAN_POINT('Ctrl Pts',(6.52066593779253,-5.53583689122712,332.905401795468));
#17490=CARTESIAN_POINT('Ctrl Pts',(6.51325511211783,-5.58772573229615,333.054427666948));
#17491=CARTESIAN_POINT('Ctrl Pts',(6.5054881865,-5.642107900582,333.210614428009));
#17492=CARTESIAN_POINT('Ctrl Pts',(6.49772126088217,-5.68997032163118,333.369179972477));
#17493=CARTESIAN_POINT('Ctrl Pts',(6.48995433526434,-5.73111297915293,333.529532529199));
#17494=CARTESIAN_POINT('Ctrl Pts',(6.48255018059142,-5.77033398047769,333.68239547531));
#17495=CARTESIAN_POINT('Ctrl Pts',(6.4751460259185,-5.80344857707382,333.836881893236));
#17496=CARTESIAN_POINT('Ctrl Pts',(6.46774187124558,-5.83033456700946,333.992463698304));
#17497=CARTESIAN_POINT('Ctrl Pts',(6.46033894185855,-5.85721610768307,334.148019756721));
#17498=CARTESIAN_POINT('Ctrl Pts',(6.45293601247149,-5.87787103452298,334.304670474728));
#17499=CARTESIAN_POINT('Ctrl Pts',(6.44553308308446,-5.89222842132008,334.461878458443));
#17500=CARTESIAN_POINT('Ctrl Pts',(6.43812904123468,-5.90658796564931,334.619110066323));
#17501=CARTESIAN_POINT('Ctrl Pts',(6.43072499938494,-5.9146480485449,334.776898736988));
#17502=CARTESIAN_POINT('Ctrl Pts',(6.42332095753517,-5.91638967914874,334.934702779827));
#17503=CARTESIAN_POINT('Ctrl Pts',(6.4222313065914,-5.91664599447889,334.957926760418));
#17504=CARTESIAN_POINT('Ctrl Pts',(6.42114165564761,-5.91676555092528,334.981151072591));
#17505=CARTESIAN_POINT('Ctrl Pts',(6.42005200470385,-5.9167483832518,335.004373989846));
#17506=CARTESIAN_POINT('',(5.23189948583629,2.55396280645894,329.653827904464));
#17507=CARTESIAN_POINT('Ctrl Pts',(6.42004993338623,-5.91090779291692,335.004413773046));
#17508=CARTESIAN_POINT('Ctrl Pts',(6.38824021370975,-5.91561392752808,335.681685130669));
#17509=CARTESIAN_POINT('Ctrl Pts',(6.26368448260861,-5.49499298147518,338.328028889201));
#17510=CARTESIAN_POINT('Ctrl Pts',(6.04638274008274,-1.58837681372764,341.814009283852));
#17511=CARTESIAN_POINT('Ctrl Pts',(5.76814470580904,4.86755545747182,340.023264886511));
#17512=CARTESIAN_POINT('Ctrl Pts',(5.49665028772668,6.81546684580212,333.780002640514));
#17513=CARTESIAN_POINT('Ctrl Pts',(5.31790188106919,4.18981562870807,330.448172083406));
#17514=CARTESIAN_POINT('Ctrl Pts',(5.23189948583629,2.55396280645894,329.653827904464));
#17515=CARTESIAN_POINT('',(5.23167681249902,5.77251337094751,333.701531692827));
#17516=CARTESIAN_POINT('Origin',(5.23167681249902,0.,335.));
#17517=CARTESIAN_POINT('',(6.1683016202946,-5.91085010084463,335.003787828726));
#17518=CARTESIAN_POINT('Ctrl Pts',(5.23167681249901,5.7725133709475,333.701531692827));
#17519=CARTESIAN_POINT('Ctrl Pts',(5.27804981821134,5.98870477377988,334.662639296794));
#17520=CARTESIAN_POINT('Ctrl Pts',(5.37079582963592,5.92269951237704,336.683589130316));
#17521=CARTESIAN_POINT('Ctrl Pts',(5.55628785248541,3.9027738141709,340.231641120345));
#17522=CARTESIAN_POINT('Ctrl Pts',(5.78815288104678,-1.42257678303753,341.849708232943));
#17523=CARTESIAN_POINT('Ctrl Pts',(6.00761513888745,-5.45702824590155,338.421060314205));
#17524=CARTESIAN_POINT('Ctrl Pts',(6.13433138530335,-5.9154777532734,335.72734314963));
#17525=CARTESIAN_POINT('Ctrl Pts',(6.1683016202946,-5.91085010084463,335.003787828726));
#17526=CARTESIAN_POINT('',(7.91830163717014,-5.91374138950514,334.995600164335));
#17527=CARTESIAN_POINT('Ctrl Pts',(6.1683016202946,-5.91085010084463,335.003787828726));
#17528=CARTESIAN_POINT('Ctrl Pts',(6.227077396728,-5.90284327178869,333.751882277009));
#17529=CARTESIAN_POINT('Ctrl Pts',(6.37859918458608,-4.89799509763915,330.513552613149));
#17530=CARTESIAN_POINT('Ctrl Pts',(6.62286698386865,0.427294553030382,328.016370371526));
#17531=CARTESIAN_POINT('Ctrl Pts',(6.90110501814268,6.10500479148874,331.581181890746));
#17532=CARTESIAN_POINT('Ctrl Pts',(7.17934305241665,6.17814947180328,338.283125900322));
#17533=CARTESIAN_POINT('Ctrl Pts',(7.45758108669047,0.582805599993459,341.972334889221));
#17534=CARTESIAN_POINT('Ctrl Pts',(7.70390060931647,-4.84465710169942,339.573858972125));
#17535=CARTESIAN_POINT('Ctrl Pts',(7.85747412051787,-5.90181156470676,336.290745442971));
#17536=CARTESIAN_POINT('Ctrl Pts',(7.91830162029457,-5.91069881207897,334.995602787516));
#17537=CARTESIAN_POINT('',(9.66830162029456,-5.92110347897511,334.998042942288));
#17538=CARTESIAN_POINT('Ctrl Pts',(7.91830165384826,-5.91674836216028,334.995597571852));
#17539=CARTESIAN_POINT('Ctrl Pts',(7.92683772418695,-5.91661299085589,334.813662077034));
#17540=CARTESIAN_POINT('Ctrl Pts',(7.93537379452558,-5.9080821444984,334.632067955286));
#17541=CARTESIAN_POINT('Ctrl Pts',(7.94390986486428,-5.89127375261271,334.451525630246));
#17542=CARTESIAN_POINT('Ctrl Pts',(7.95248902433919,-5.87438051382923,334.270071947577));
#17543=CARTESIAN_POINT('Ctrl Pts',(7.96106818381414,-5.84912605575822,334.089680827836));
#17544=CARTESIAN_POINT('Ctrl Pts',(7.96964734328904,-5.81567951179891,333.911054464841));
#17545=CARTESIAN_POINT('Ctrl Pts',(7.97828197365068,-5.78201671012143,333.73127314456));
#17546=CARTESIAN_POINT('Ctrl Pts',(7.98691660401228,-5.74005562372791,333.553279595535));
#17547=CARTESIAN_POINT('Ctrl Pts',(7.99555123437392,-5.69001722684064,333.377768659914));
#17548=CARTESIAN_POINT('Ctrl Pts',(8.00171987466208,-5.65426944632587,333.25238242065));
#17549=CARTESIAN_POINT('Ctrl Pts',(8.00788851495028,-5.61440020520827,333.128262813615));
#17550=CARTESIAN_POINT('Ctrl Pts',(8.01405715523845,-5.57050476081265,333.005656180027));
#17551=CARTESIAN_POINT('Ctrl Pts',(8.02148123988807,-5.51767569643178,332.858096590905));
#17552=CARTESIAN_POINT('Ctrl Pts',(8.02890532453766,-5.45889976275216,332.712415060664));
#17553=CARTESIAN_POINT('Ctrl Pts',(8.03632940918729,-5.39432904919198,332.569126767694));
#17554=CARTESIAN_POINT('Ctrl Pts',(8.04374473498362,-5.32983451544838,332.426007524673));
#17555=CARTESIAN_POINT('Ctrl Pts',(8.05116006077994,-5.25955896206744,332.285276235607));
#17556=CARTESIAN_POINT('Ctrl Pts',(8.05857538657628,-5.18370390865521,332.147431972784));
#17557=CARTESIAN_POINT('Ctrl Pts',(8.06598357992732,-5.10792181657112,332.009720295729));
#17558=CARTESIAN_POINT('Ctrl Pts',(8.07339177327832,-5.02657108719275,331.874890441416));
#17559=CARTESIAN_POINT('Ctrl Pts',(8.08079996662937,-4.93990084107574,331.743420468829));
#17560=CARTESIAN_POINT('Ctrl Pts',(8.08820264833253,-4.85329507706065,331.612048309051));
#17561=CARTESIAN_POINT('Ctrl Pts',(8.09560533003574,-4.76137788117132,331.484031363918));
#17562=CARTESIAN_POINT('Ctrl Pts',(8.10300801173889,-4.66444365169039,331.359821984751));
#17563=CARTESIAN_POINT('Ctrl Pts',(8.11040679823126,-4.56756042794927,331.235677963211));
#17564=CARTESIAN_POINT('Ctrl Pts',(8.11780558472363,-4.46566565718142,331.115337811013));
#17565=CARTESIAN_POINT('Ctrl Pts',(8.125204371216,-4.35909622293599,330.999223740112));
#17566=CARTESIAN_POINT('Ctrl Pts',(8.13260194010405,-4.25254432662111,330.883128777884));
#17567=CARTESIAN_POINT('Ctrl Pts',(8.13999950899212,-4.14131954572892,330.771258791351));
#17568=CARTESIAN_POINT('Ctrl Pts',(8.14739707788016,-4.02579818218162,330.66400189589));
#17569=CARTESIAN_POINT('Ctrl Pts',(8.15479432784718,-3.91028179894503,330.556749624446));
#17570=CARTESIAN_POINT('Ctrl Pts',(8.16219157781416,-3.79046947484708,330.454110302568));
#17571=CARTESIAN_POINT('Ctrl Pts',(8.16958882778118,-3.66677320746662,330.35643404187));
#17572=CARTESIAN_POINT('Ctrl Pts',(8.17698721844369,-3.54305786546047,330.25874271897));
#17573=CARTESIAN_POINT('Ctrl Pts',(8.18438560910621,-3.41545768054302,330.166016212421));
#17574=CARTESIAN_POINT('Ctrl Pts',(8.19178399976872,-3.28441632199582,330.078563219312));
#17575=CARTESIAN_POINT('Ctrl Pts',(8.19918499114654,-3.15332889920535,329.991079484336));
#17576=CARTESIAN_POINT('Ctrl Pts',(8.20658598252437,-3.01879820458202,329.908873160688));
#17577=CARTESIAN_POINT('Ctrl Pts',(8.21398697390219,-2.88129522296416,329.832208556779));
#17578=CARTESIAN_POINT('Ctrl Pts',(8.22139609400086,-2.74364121788267,329.75545974994));
#17579=CARTESIAN_POINT('Ctrl Pts',(8.22880521409956,-2.60300873248182,329.68426500001));
#17580=CARTESIAN_POINT('Ctrl Pts',(8.23621433419822,-2.45989224565882,329.618842066781));
#17581=CARTESIAN_POINT('Ctrl Pts',(8.24362801973741,-2.31668757160171,329.553378820463));
#17582=CARTESIAN_POINT('Ctrl Pts',(8.25104170527654,-2.17099619069115,329.493694618884));
#17583=CARTESIAN_POINT('Ctrl Pts',(8.25845539081573,-2.02333021842649,329.439958148566));
#17584=CARTESIAN_POINT('Ctrl Pts',(8.26587963176961,-1.87545400315037,329.386145169644));
#17585=CARTESIAN_POINT('Ctrl Pts',(8.27330387272348,-1.72559793620386,329.338296947935));
#17586=CARTESIAN_POINT('Ctrl Pts',(8.28072811367736,-1.57428765481617,329.296531849621));
#17587=CARTESIAN_POINT('Ctrl Pts',(8.28458380562237,-1.4957064454012,329.274841638573));
#17588=CARTESIAN_POINT('Ctrl Pts',(8.28843949756739,-1.41673316862141,329.254791274787));
#17589=CARTESIAN_POINT('Ctrl Pts',(8.2922951895124,-1.33744215071377,329.236391837053));
#17590=CARTESIAN_POINT('Ctrl Pts',(8.29971898218592,-1.18477433227457,329.20096535252));
#17591=CARTESIAN_POINT('Ctrl Pts',(8.30714277485943,-1.03046754044259,329.171555439486));
#17592=CARTESIAN_POINT('Ctrl Pts',(8.31456656753295,-0.875037250964456,
329.14831303196));
#17593=CARTESIAN_POINT('Ctrl Pts',(8.32198159640168,-0.719790447310228,
329.125098062152));
#17594=CARTESIAN_POINT('Ctrl Pts',(8.32939662527037,-0.563423151547546,
329.108036160072));
#17595=CARTESIAN_POINT('Ctrl Pts',(8.3368116541391,-0.406464050401816,329.097227978464));
#17596=CARTESIAN_POINT('Ctrl Pts',(8.34421954592478,-0.249656024883776,
329.086430199902));
#17597=CARTESIAN_POINT('Ctrl Pts',(8.35162743771053,-0.0922576978533067,
329.081874183981));
#17598=CARTESIAN_POINT('Ctrl Pts',(8.35903532949621,0.0651941497774572,
329.083609184196));
#17599=CARTESIAN_POINT('Ctrl Pts',(8.36643770530399,0.222528757451586,329.085342892515));
#17600=CARTESIAN_POINT('Ctrl Pts',(8.37384008111172,0.379916434764904,329.093358285677));
#17601=CARTESIAN_POINT('Ctrl Pts',(8.38124245691949,0.536817511828146,329.107652630615));
#17602=CARTESIAN_POINT('Ctrl Pts',(8.38864093348939,0.693635940476877,329.121939445937));
#17603=CARTESIAN_POINT('Ctrl Pts',(8.39603941005929,0.849967908592966,329.142498592243));
#17604=CARTESIAN_POINT('Ctrl Pts',(8.40343788662918,1.00527609563477,329.169275299412));
#17605=CARTESIAN_POINT('Ctrl Pts',(8.41083514053918,1.16055861670482,329.196047581507));
#17606=CARTESIAN_POINT('Ctrl Pts',(8.4182323944492,1.3148173250386,329.229035321837));
#17607=CARTESIAN_POINT('Ctrl Pts',(8.42562964835921,1.46752223760303,329.268132150456));
#17608=CARTESIAN_POINT('Ctrl Pts',(8.43302658023806,1.62022050233054,329.307227277038));
#17609=CARTESIAN_POINT('Ctrl Pts',(8.44042351211688,1.77136474421501,329.352430870534));
#17610=CARTESIAN_POINT('Ctrl Pts',(8.44782044399574,1.92043761810329,329.403585976943));
#17611=CARTESIAN_POINT('Ctrl Pts',(8.45521851372274,2.06953342343079,329.454748952389));
#17612=CARTESIAN_POINT('Ctrl Pts',(8.46261658344977,2.21655687327633,329.511865142484));
#17613=CARTESIAN_POINT('Ctrl Pts',(8.47001465317678,2.36100830668288,329.574728547043));
#17614=CARTESIAN_POINT('Ctrl Pts',(8.47741532103311,2.50551047001213,329.63761402861));
#17615=CARTESIAN_POINT('Ctrl Pts',(8.48481598888946,2.6474384764872,329.706250594357));
#17616=CARTESIAN_POINT('Ctrl Pts',(8.4922166567458,2.78631520828013,329.780385251515));
#17617=CARTESIAN_POINT('Ctrl Pts',(8.49962545099421,2.92534443533359,329.854601313121));
#17618=CARTESIAN_POINT('Ctrl Pts',(8.50703424524264,3.06131536714769,329.934327346968));
#17619=CARTESIAN_POINT('Ctrl Pts',(8.51444303949106,3.19377731392234,330.019265412454));
#17620=CARTESIAN_POINT('Ctrl Pts',(8.52185639737291,3.32632085396972,330.104255797682));
#17621=CARTESIAN_POINT('Ctrl Pts',(8.52926975525478,3.45535079683766,330.194464398494));
#17622=CARTESIAN_POINT('Ctrl Pts',(8.53668311313663,3.58044817403435,330.289551885908));
#17623=CARTESIAN_POINT('Ctrl Pts',(8.54410702640874,3.70572366911725,330.384774762109));
#17624=CARTESIAN_POINT('Ctrl Pts',(8.55153093968082,3.82705512846242,330.484890162004));
#17625=CARTESIAN_POINT('Ctrl Pts',(8.55895485295292,3.94405858059623,330.58952015362));
#17626=CARTESIAN_POINT('Ctrl Pts',(8.56281430989739,4.00488496276339,330.643913966282));
#17627=CARTESIAN_POINT('Ctrl Pts',(8.56667376684183,4.06454227385321,330.699527320161));
#17628=CARTESIAN_POINT('Ctrl Pts',(8.5705332237863,4.12298082739577,330.756303538255));
#17629=CARTESIAN_POINT('Ctrl Pts',(8.57795727706771,4.23539325780528,330.865518299376));
#17630=CARTESIAN_POINT('Ctrl Pts',(8.58538133034913,4.34363271208492,330.979367457087));
#17631=CARTESIAN_POINT('Ctrl Pts',(8.59280538363055,4.44729331096703,331.097499164801));
#17632=CARTESIAN_POINT('Ctrl Pts',(8.60022067615752,4.55083158515432,331.215491471188));
#17633=CARTESIAN_POINT('Ctrl Pts',(8.60763596868448,4.64980151550148,331.337755990468));
#17634=CARTESIAN_POINT('Ctrl Pts',(8.61505126121145,4.74383235924362,331.463902559333));
#17635=CARTESIAN_POINT('Ctrl Pts',(8.62245941943236,4.8377727352374,331.58992776168));
#17636=CARTESIAN_POINT('Ctrl Pts',(8.62986757765331,4.92678326328722,331.719827280803));
#17637=CARTESIAN_POINT('Ctrl Pts',(8.63727573587423,5.01053204567707,331.853176334501));
#17638=CARTESIAN_POINT('Ctrl Pts',(8.64467838062512,5.09421849862048,331.986426144098));
#17639=CARTESIAN_POINT('Ctrl Pts',(8.65208102537597,5.17265080563063,332.123120061727));
#17640=CARTESIAN_POINT('Ctrl Pts',(8.65948367012686,5.24553922421881,332.262802745566));
#17641=CARTESIAN_POINT('Ctrl Pts',(8.66688241788194,5.31838927194478,332.402411895843));
#17642=CARTESIAN_POINT('Ctrl Pts',(8.67428116563706,5.38570107137234,332.545006348807));
#17643=CARTESIAN_POINT('Ctrl Pts',(8.68167991339214,5.44722991195677,332.690104580553));
#17644=CARTESIAN_POINT('Ctrl Pts',(8.68907744097947,5.50874860548524,332.835178883359));
#17645=CARTESIAN_POINT('Ctrl Pts',(8.69647496856678,5.56448608739801,332.982755802199));
#17646=CARTESIAN_POINT('Ctrl Pts',(8.7038724961541,5.61424501031915,333.132332062007));
#17647=CARTESIAN_POINT('Ctrl Pts',(8.71126970323063,5.66400177734807,333.281901841163));
#17648=CARTESIAN_POINT('Ctrl Pts',(8.71866691030714,5.70778038262102,333.433470434927));
#17649=CARTESIAN_POINT('Ctrl Pts',(8.72606411738366,5.74543285576739,333.586517823823));
#17650=CARTESIAN_POINT('Ctrl Pts',(8.73346246359525,5.78309112721737,333.739588781298));
#17651=CARTESIAN_POINT('Ctrl Pts',(8.74086080980685,5.81462129895377,333.894138624922));
#17652=CARTESIAN_POINT('Ctrl Pts',(8.74825915601843,5.83992621491512,334.049635666259));
#17653=CARTESIAN_POINT('Ctrl Pts',(8.75566010141336,5.86524002098702,334.205187336739));
#17654=CARTESIAN_POINT('Ctrl Pts',(8.76306104680832,5.88432415695462,334.361686499351));
#17655=CARTESIAN_POINT('Ctrl Pts',(8.77046199220325,5.89713318336375,334.518594993618));
#17656=CARTESIAN_POINT('Ctrl Pts',(8.77787106420263,5.90995627471803,334.675675781179));
#17657=CARTESIAN_POINT('Ctrl Pts',(8.78528013620195,5.91649046567086,334.833166425817));
#17658=CARTESIAN_POINT('Ctrl Pts',(8.79268920820132,5.91674241610059,334.990526668159));
#17659=CARTESIAN_POINT('Ctrl Pts',(8.8001028443691,5.9169945217379,335.147983848234));
#17660=CARTESIAN_POINT('Ctrl Pts',(8.80751648053688,5.91095668961467,335.305310093885));
#17661=CARTESIAN_POINT('Ctrl Pts',(8.81493011670466,5.89868755012404,335.461969423784));
#17662=CARTESIAN_POINT('Ctrl Pts',(8.82235430671008,5.8864009446419,335.618851769367));
#17663=CARTESIAN_POINT('Ctrl Pts',(8.82977849671553,5.86786535906686,335.775064933449));
#17664=CARTESIAN_POINT('Ctrl Pts',(8.83720268672096,5.84319082462592,335.930081474661));
#17665=CARTESIAN_POINT('Ctrl Pts',(8.84105887716739,5.83037465156034,336.010598447533));
#17666=CARTESIAN_POINT('Ctrl Pts',(8.84491506761377,5.81590311068985,336.090792800601));
#17667=CARTESIAN_POINT('Ctrl Pts',(8.8487712580602,5.79979691940674,336.170592267248));
#17668=CARTESIAN_POINT('Ctrl Pts',(8.85619524385121,5.7687890797022,336.324223192573));
#17669=CARTESIAN_POINT('Ctrl Pts',(8.86361922964221,5.73162595104128,336.476852966426));
#17670=CARTESIAN_POINT('Ctrl Pts',(8.87104321543322,5.68838375572378,336.627949879486));
#17671=CARTESIAN_POINT('Ctrl Pts',(8.87845844010974,5.64519259092201,336.778868481677));
#17672=CARTESIAN_POINT('Ctrl Pts',(8.88587366478632,5.59593674103953,336.928257468488));
#17673=CARTESIAN_POINT('Ctrl Pts',(8.89328888946284,5.54074366422659,337.075593941462));
#17674=CARTESIAN_POINT('Ctrl Pts',(8.90069697954199,5.4856036917224,337.222788653874));
#17675=CARTESIAN_POINT('Ctrl Pts',(8.9081050696211,5.42453799492601,337.367934436824));
#17676=CARTESIAN_POINT('Ctrl Pts',(8.91551315970025,5.35772416521539,337.510522322539));
#17677=CARTESIAN_POINT('Ctrl Pts',(8.92291573608602,5.29096006370282,337.653004082941));
#17678=CARTESIAN_POINT('Ctrl Pts',(8.9303183124718,5.21845650551427,337.792931400333));
#17679=CARTESIAN_POINT('Ctrl Pts',(8.93772088885757,5.14043959309047,337.92981421805));
#17680=CARTESIAN_POINT('Ctrl Pts',(8.94511956809161,5.06246375335933,338.066624972599));
#17681=CARTESIAN_POINT('Ctrl Pts',(8.9525182473257,4.97898052434013,338.200394096124));
#17682=CARTESIAN_POINT('Ctrl Pts',(8.95991692655974,4.89026239513531,338.330655231216));
#17683=CARTESIAN_POINT('Ctrl Pts',(8.96731438561524,4.80155889718485,338.460894883846));
#17684=CARTESIAN_POINT('Ctrl Pts',(8.97471184467069,4.70762242236363,338.587627388077));
#17685=CARTESIAN_POINT('Ctrl Pts',(8.98210930372619,4.60876938193421,338.710414444054));
#17686=CARTESIAN_POINT('Ctrl Pts',(8.9895064422716,4.50992062451558,338.833196180031));
#17687=CARTESIAN_POINT('Ctrl Pts',(8.99690358081701,4.40615595908437,338.952032516941));
#17688=CARTESIAN_POINT('Ctrl Pts',(9.00430071936242,4.29783259854894,339.066517615522));
#17689=CARTESIAN_POINT('Ctrl Pts',(9.01169899710373,4.18949255568047,339.181020345374));
#17690=CARTESIAN_POINT('Ctrl Pts',(9.01909727484511,4.07659267632957,339.291170231504));
#17691=CARTESIAN_POINT('Ctrl Pts',(9.02649555258643,3.95952748475246,339.39659785061));
#17692=CARTESIAN_POINT('Ctrl Pts',(9.03389642963216,3.84242116359358,339.502062510564));
#17693=CARTESIAN_POINT('Ctrl Pts',(9.04129730667785,3.72114689365642,339.602801350596));
#17694=CARTESIAN_POINT('Ctrl Pts',(9.04869818372359,3.59613262855752,339.698484934564));
#17695=CARTESIAN_POINT('Ctrl Pts',(9.05610718790516,3.47098108136252,339.794273591684));
#17696=CARTESIAN_POINT('Ctrl Pts',(9.06351619208672,3.34208163363746,339.884995679458));
#17697=CARTESIAN_POINT('Ctrl Pts',(9.07092519626829,3.20989219798347,339.970364437325));
#17698=CARTESIAN_POINT('Ctrl Pts',(9.07833876481848,3.07762132610715,340.05578578721));
#17699=CARTESIAN_POINT('Ctrl Pts',(9.08575233336862,2.94205674819764,340.135847046234));
#17700=CARTESIAN_POINT('Ctrl Pts',(9.09316590191881,2.80368090346349,340.210307472122));
#17701=CARTESIAN_POINT('Ctrl Pts',(9.1005900252035,2.66510805234929,340.28487390769));
#17702=CARTESIAN_POINT('Ctrl Pts',(9.10801414848822,2.5237162753334,340.353823421439));
#17703=CARTESIAN_POINT('Ctrl Pts',(9.11543827177292,2.38000864603019,340.416963116666));
#17704=CARTESIAN_POINT('Ctrl Pts',(9.11929527862669,2.3053491488873,340.449765675015));
#17705=CARTESIAN_POINT('Ctrl Pts',(9.12315228548043,2.23006486464686,340.481000950716));
#17706=CARTESIAN_POINT('Ctrl Pts',(9.12700929233421,2.15422782191943,340.510647244541));
#17707=CARTESIAN_POINT('Ctrl Pts',(9.13443324371234,2.0082569851502,340.567710312417));
#17708=CARTESIAN_POINT('Ctrl Pts',(9.14185719509051,1.85979705777193,340.619055559184));
#17709=CARTESIAN_POINT('Ctrl Pts',(9.14928114646864,1.70933640674325,340.664459339697));
#17710=CARTESIAN_POINT('Ctrl Pts',(9.15669633608286,1.5590533297093,340.709809534568));
#17711=CARTESIAN_POINT('Ctrl Pts',(9.16411152569702,1.40677458297222,340.74923211417));
#17712=CARTESIAN_POINT('Ctrl Pts',(9.17152671531124,1.25300885155084,340.782551286451));
#17713=CARTESIAN_POINT('Ctrl Pts',(9.178934769716,1.09939108002805,340.815838397613));
#17714=CARTESIAN_POINT('Ctrl Pts',(9.18634282412077,0.944289534666818,340.843033714906));
#17715=CARTESIAN_POINT('Ctrl Pts',(9.19375087852552,0.788228316462973,340.864011142863));
#17716=CARTESIAN_POINT('Ctrl Pts',(9.20115341866133,0.632283264188988,340.884972956035));
#17717=CARTESIAN_POINT('Ctrl Pts',(9.20855595879715,0.475380329736878,340.899726046095));
#17718=CARTESIAN_POINT('Ctrl Pts',(9.21595849893296,0.318053964055267,340.908195345319));
#17719=CARTESIAN_POINT('Ctrl Pts',(9.22335714137742,0.160810436102888,340.916660185167));
#17720=CARTESIAN_POINT('Ctrl Pts',(9.23075578382188,0.0031442926772372,
340.918847803503));
#17721=CARTESIAN_POINT('Ctrl Pts',(9.23815442626633,-0.154404841455918,
340.914734965105));
#17722=CARTESIAN_POINT('Ctrl Pts',(9.24555184783926,-0.311927977947833,
340.910622805379));
#17723=CARTESIAN_POINT('Ctrl Pts',(9.25294926941215,-0.469333770743121,
340.900212262033));
#17724=CARTESIAN_POINT('Ctrl Pts',(9.26034669098507,-0.626082420024908,
340.883532218475));
#17725=CARTESIAN_POINT('Ctrl Pts',(9.26774379162101,-0.782824268769665,
340.866852898581));
#17726=CARTESIAN_POINT('Ctrl Pts',(9.27514089225692,-0.938908659569522,
340.843904658796));
#17727=CARTESIAN_POINT('Ctrl Pts',(9.28253799289286,-1.09380100885479,340.81476825983));
#17728=CARTESIAN_POINT('Ctrl Pts',(9.28993623232881,-1.24871720416013,340.785627375251));
#17729=CARTESIAN_POINT('Ctrl Pts',(9.29733447176483,-1.40244062573968,340.750296503577));
#17730=CARTESIAN_POINT('Ctrl Pts',(9.30473271120078,-1.55444712128882,340.708907488269));
#17731=CARTESIAN_POINT('Ctrl Pts',(9.3121335495761,-1.70650701544281,340.667503933348));
#17732=CARTESIAN_POINT('Ctrl Pts',(9.31953438795144,-1.85684842283524,340.62003809559));
#17733=CARTESIAN_POINT('Ctrl Pts',(9.32693522632675,-2.00496272635088,340.566691569365));
#17734=CARTESIAN_POINT('Ctrl Pts',(9.33434419147376,-2.15323967240338,340.513286463962));
#17735=CARTESIAN_POINT('Ctrl Pts',(9.34175315662073,-2.29928427933032,340.453987900637));
#17736=CARTESIAN_POINT('Ctrl Pts',(9.34916212176773,-2.44260760404967,340.389025761224));
#17737=CARTESIAN_POINT('Ctrl Pts',(9.35657565101858,-2.58601921944444,340.324023603544));
#17738=CARTESIAN_POINT('Ctrl Pts',(9.36398918026944,-2.72670587950936,340.25335108482));
#17739=CARTESIAN_POINT('Ctrl Pts',(9.37140270952028,-2.86420406596059,340.177283615086));
#17740=CARTESIAN_POINT('Ctrl Pts',(9.3788267934271,-3.00189800884647,340.101107847947));
#17741=CARTESIAN_POINT('Ctrl Pts',(9.38625087733393,-3.13639409372241,340.019521982744));
#17742=CARTESIAN_POINT('Ctrl Pts',(9.39367496124075,-3.26725787003449,339.932844673532));
#17743=CARTESIAN_POINT('Ctrl Pts',(9.39753241636321,-3.33525294533478,339.887808298053));
#17744=CARTESIAN_POINT('Ctrl Pts',(9.40138987148567,-3.40226794297014,339.84139805386));
#17745=CARTESIAN_POINT('Ctrl Pts',(9.40524732660813,-3.46824561639963,339.793662786098));
#17746=CARTESIAN_POINT('Ctrl Pts',(9.41261048706837,-3.59418465673371,339.702545086739));
#17747=CARTESIAN_POINT('Ctrl Pts',(9.4199736475286,-3.71673576760079,339.606312329512));
#17748=CARTESIAN_POINT('Ctrl Pts',(9.42733680798884,-3.83545069730018,339.505246775825));
#17749=CARTESIAN_POINT('Ctrl Pts',(9.43469124851353,-3.95402503702593,339.404300910568));
#17750=CARTESIAN_POINT('Ctrl Pts',(9.44204568903819,-4.0687719495888,339.298533881596));
#17751=CARTESIAN_POINT('Ctrl Pts',(9.44940012956289,-4.17927208776007,339.188271168271));
#17752=CARTESIAN_POINT('Ctrl Pts',(9.45674753057803,-4.28966645761678,339.078113996003));
#17753=CARTESIAN_POINT('Ctrl Pts',(9.46409493159318,-4.39582187617995,338.963469970323));
#17754=CARTESIAN_POINT('Ctrl Pts',(9.47144233260832,-4.49735219872133,338.844704639261));
#17755=CARTESIAN_POINT('Ctrl Pts',(9.47878436825251,-4.59880837969331,338.726026035472));
#17756=CARTESIAN_POINT('Ctrl Pts',(9.48612640389676,-4.69564594199118,338.603232404785));
#17757=CARTESIAN_POINT('Ctrl Pts',(9.49346843954095,-4.78751589011209,338.476725782173));
#17758=CARTESIAN_POINT('Ctrl Pts',(9.50080733153183,-4.87934650210338,338.35027332614));
#17759=CARTESIAN_POINT('Ctrl Pts',(9.50814622352271,-4.9662135087272,338.220111347855));
#17760=CARTESIAN_POINT('Ctrl Pts',(9.5154851155136,-5.04780854743308,338.086674493846));
#17761=CARTESIAN_POINT('Ctrl Pts',(9.52282245051373,-5.12938627525321,337.953265949281));
#17762=CARTESIAN_POINT('Ctrl Pts',(9.53015978551386,-5.20569406209302,337.816584235143));
#17763=CARTESIAN_POINT('Ctrl Pts',(9.53749712051399,-5.27646732766874,337.677092285026));
#17764=CARTESIAN_POINT('Ctrl Pts',(9.54483440613936,-5.34724011699347,337.537601273584));
#17765=CARTESIAN_POINT('Ctrl Pts',(9.55217169176475,-5.41247828707875,337.395300402612));
#17766=CARTESIAN_POINT('Ctrl Pts',(9.55950897739012,-5.47196372468579,337.250676244648));
#17767=CARTESIAN_POINT('Ctrl Pts',(9.56684772099427,-5.53146098253663,337.106023348678));
#17768=CARTESIAN_POINT('Ctrl Pts',(9.57418646459841,-5.58520308859339,336.959046598407));
#17769=CARTESIAN_POINT('Ctrl Pts',(9.58152520820255,-5.63302057482098,336.810251299169));
#17770=CARTESIAN_POINT('Ctrl Pts',(9.58887113577307,-5.68088487004367,336.661310342788));
#17771=CARTESIAN_POINT('Ctrl Pts',(9.59621706334361,-5.72281284390395,336.510547643699));
#17772=CARTESIAN_POINT('Ctrl Pts',(9.60356299091413,-5.75868512950576,336.358483029599));
#17773=CARTESIAN_POINT('Ctrl Pts',(9.61091255689113,-5.79457518249709,336.206343098547));
#17774=CARTESIAN_POINT('Ctrl Pts',(9.61826212286808,-5.82440349896535,336.052900340431));
#17775=CARTESIAN_POINT('Ctrl Pts',(9.62561168884508,-5.84810223963961,335.8986827901));
#17776=CARTESIAN_POINT('Ctrl Pts',(9.63297217355516,-5.8718361878655,335.744236129605));
#17777=CARTESIAN_POINT('Ctrl Pts',(9.64033265826531,-5.88942232263109,335.589012754514));
#17778=CARTESIAN_POINT('Ctrl Pts',(9.64769314297538,-5.90084480945455,335.433544804182));
#17779=CARTESIAN_POINT('Ctrl Pts',(9.65456263541512,-5.91150534201013,335.288447578729));
#17780=CARTESIAN_POINT('Ctrl Pts',(9.66143212785482,-5.91679763337387,335.143137580778));
#17781=CARTESIAN_POINT('Ctrl Pts',(9.66830162029456,-5.91674967681206,334.998044381317));
#17782=CARTESIAN_POINT('',(11.4183016202945,-5.91660642682179,335.005447186169));
#17783=CARTESIAN_POINT('Ctrl Pts',(9.66830162029456,-5.92571575529067,334.998041417827));
#17784=CARTESIAN_POINT('Ctrl Pts',(9.67336286715706,-5.92617653575604,334.890978712543));
#17785=CARTESIAN_POINT('Ctrl Pts',(9.67842411401957,-5.92352695970669,334.783939278396));
#17786=CARTESIAN_POINT('Ctrl Pts',(9.77623137230671,-5.81083203592888,332.718786120812));
#17787=CARTESIAN_POINT('Ctrl Pts',(9.96172339515596,-3.46005639991333,328.918829283388));
#17788=CARTESIAN_POINT('Ctrl Pts',(10.23996142943,3.24135166517253,328.799494881017));
#17789=CARTESIAN_POINT('Ctrl Pts',(10.5181994637039,6.9682181308629,334.370272377245));
#17790=CARTESIAN_POINT('Ctrl Pts',(10.7964374979778,4.30045420801287,340.518941686844));
#17791=CARTESIAN_POINT('Ctrl Pts',(11.0746755322517,-2.31377335260903,341.602959633473));
#17792=CARTESIAN_POINT('Ctrl Pts',(11.281963573024,-5.65951399291435,337.89625865298));
#17793=CARTESIAN_POINT('Ctrl Pts',(11.3965056023716,-5.92087158251783,335.468355196754));
#17794=CARTESIAN_POINT('Ctrl Pts',(11.4183016202945,-5.91660642682179,335.005447186169));
#17795=CARTESIAN_POINT('',(13.1683016202945,-5.90706551088391,334.999199780965));
#17796=CARTESIAN_POINT('Ctrl Pts',(11.4183016202945,-5.91660642682179,335.005447186169));
#17797=CARTESIAN_POINT('Ctrl Pts',(11.4892516137962,-5.90272257106488,333.498597611211));
#17798=CARTESIAN_POINT('Ctrl Pts',(11.6529476187225,-4.55055703177909,329.999836531847));
#17799=CARTESIAN_POINT('Ctrl Pts',(11.9093896350736,1.3378723248115,328.132488036437));
#17800=CARTESIAN_POINT('Ctrl Pts',(12.1876276693475,6.49903679796859,332.408640592677));
#17801=CARTESIAN_POINT('Ctrl Pts',(12.4658657036214,5.69613113915697,339.062845430127));
#17802=CARTESIAN_POINT('Ctrl Pts',(12.7441037378953,-0.334029997602265,
341.988636983051));
#17803=CARTESIAN_POINT('Ctrl Pts',(12.9782490434532,-5.15062645695485,339.053740283081));
#17804=CARTESIAN_POINT('Ctrl Pts',(13.1196483375861,-5.90581620181614,336.036722990494));
#17805=CARTESIAN_POINT('Ctrl Pts',(13.1683016202945,-5.90706551088391,334.999199780965));
#17806=CARTESIAN_POINT('',(14.9183007632462,-5.91862575758834,334.994894904104));
#17807=CARTESIAN_POINT('Ctrl Pts',(13.1683016202945,-5.90706551088391,334.999199780965));
#17808=CARTESIAN_POINT('Ctrl Pts',(13.2123943490108,-5.90819771497666,334.058929631288));
#17809=CARTESIAN_POINT('Ctrl Pts',(13.3492330891516,-5.25256836435763,331.142357715814));
#17810=CARTESIAN_POINT('Ctrl Pts',(13.5788178407172,-0.676788508317976,
328.036194988672));
#17811=CARTESIAN_POINT('Ctrl Pts',(13.8570558749913,5.48976310418741,330.662359629893));
#17812=CARTESIAN_POINT('Ctrl Pts',(14.1352939092649,6.61844014501037,337.269112815324));
#17813=CARTESIAN_POINT('Ctrl Pts',(14.4135319435389,1.67347235263872,341.793534662167));
#17814=CARTESIAN_POINT('Ctrl Pts',(14.6745340873688,-4.40575991606507,340.189552740701));
#17815=CARTESIAN_POINT('Ctrl Pts',(14.842790219774,-5.90491800172395,336.596553961129));
#17816=CARTESIAN_POINT('Ctrl Pts',(14.9183003407544,-5.91955152666098,334.994903064175));
#17817=CARTESIAN_POINT('',(16.6683030484718,-5.92081106350143,335.003451021425));
#17818=CARTESIAN_POINT('Ctrl Pts',(14.9183016202945,-5.91674778330215,334.994878350942));
#17819=CARTESIAN_POINT('Ctrl Pts',(14.9293698822705,-5.91654466019703,334.760221862702));
#17820=CARTESIAN_POINT('Ctrl Pts',(14.9404381442466,-5.90237883094342,334.526146915353));
#17821=CARTESIAN_POINT('Ctrl Pts',(14.9515064062226,-5.87447532519484,334.293975767996));
#17822=CARTESIAN_POINT('Ctrl Pts',(14.9576736081773,-5.85892757654459,334.164610709875));
#17823=CARTESIAN_POINT('Ctrl Pts',(14.9638408101321,-5.8391154726375,334.035835989689));
#17824=CARTESIAN_POINT('Ctrl Pts',(14.9700080120869,-5.81508355031101,333.907876442246));
#17825=CARTESIAN_POINT('Ctrl Pts',(14.9774319895248,-5.78615431296009,333.753840819584));
#17826=CARTESIAN_POINT('Ctrl Pts',(14.9848559669627,-5.75105683838513,333.600723079315));
#17827=CARTESIAN_POINT('Ctrl Pts',(14.9922799444006,-5.70986015551614,333.449055911082));
#17828=CARTESIAN_POINT('Ctrl Pts',(14.9996951604281,-5.6687120909313,333.297567732928));
#17829=CARTESIAN_POINT('Ctrl Pts',(15.0071103764557,-5.62147924263076,333.147527075918));
#17830=CARTESIAN_POINT('Ctrl Pts',(15.0145255924832,-5.56828198979593,332.999458512149));
#17831=CARTESIAN_POINT('Ctrl Pts',(15.0219336736272,-5.51513592308989,332.851532419206));
#17832=CARTESIAN_POINT('Ctrl Pts',(15.0293417547712,-5.45603700231441,332.705574990743));
#17833=CARTESIAN_POINT('Ctrl Pts',(15.0367498359152,-5.39115592357888,332.562097547038));
#17834=CARTESIAN_POINT('Ctrl Pts',(15.0441524030891,-5.32632313701521,332.418726896214));
#17835=CARTESIAN_POINT('Ctrl Pts',(15.051554970263,-5.25571691503302,332.277832893299));
#17836=CARTESIAN_POINT('Ctrl Pts',(15.058957537437,-5.17955671596436,332.13990860485));
#17837=CARTESIAN_POINT('Ctrl Pts',(15.0663562071916,-5.10343661490798,332.002056932937));
#17838=CARTESIAN_POINT('Ctrl Pts',(15.0737548769462,-5.02176854032462,331.867172187492));
#17839=CARTESIAN_POINT('Ctrl Pts',(15.0811535467008,-4.9348186532721,331.735724364914));
#17840=CARTESIAN_POINT('Ctrl Pts',(15.0885509959047,-4.84788311025075,331.604298227144));
#17841=CARTESIAN_POINT('Ctrl Pts',(15.0959484451085,-4.75566768977953,331.47630819793));
#17842=CARTESIAN_POINT('Ctrl Pts',(15.1033458943124,-4.65848285024896,331.352196812267));
#17843=CARTESIAN_POINT('Ctrl Pts',(15.1107430227758,-4.5613022244836,331.228090807857));
#17844=CARTESIAN_POINT('Ctrl Pts',(15.1181401512391,-4.45915283816774,331.107863406461));
#17845=CARTESIAN_POINT('Ctrl Pts',(15.1255372797025,-4.35238638631023,330.99192523688));
#17846=CARTESIAN_POINT('Ctrl Pts',(15.132935547139,-4.24560349508438,330.875969215715));
#17847=CARTESIAN_POINT('Ctrl Pts',(15.1403338145755,-4.13420237562885,330.76430401593));
#17848=CARTESIAN_POINT('Ctrl Pts',(15.147732082012,-4.01857252304005,330.65730435794));
#17849=CARTESIAN_POINT('Ctrl Pts',(15.1551329485376,-3.90290204846804,330.550267109845));
#17850=CARTESIAN_POINT('Ctrl Pts',(15.1625338150633,-3.7830001566908,330.447898920217));
#17851=CARTESIAN_POINT('Ctrl Pts',(15.169934681589,-3.65929030951345,330.350534977742));
#17852=CARTESIAN_POINT('Ctrl Pts',(15.1773436749736,-3.53544461709659,330.253064120349));
#17853=CARTESIAN_POINT('Ctrl Pts',(15.1847526683583,-3.40778291205219,330.160608715156));
#17854=CARTESIAN_POINT('Ctrl Pts',(15.1921616617429,-3.27675918914466,330.073461684016));
#17855=CARTESIAN_POINT('Ctrl Pts',(15.1995752193231,-3.14565475110432,329.9862609673));
#17856=CARTESIAN_POINT('Ctrl Pts',(15.2069887769032,-3.0111844862383,329.904375334482));
#17857=CARTESIAN_POINT('Ctrl Pts',(15.2144023344834,-2.873827535569,329.828052024787));
#17858=CARTESIAN_POINT('Ctrl Pts',(15.22182644662,-2.73627503213386,329.751620054889));
#17859=CARTESIAN_POINT('Ctrl Pts',(15.2292505587565,-2.5958279672626,329.680766391558));
#17860=CARTESIAN_POINT('Ctrl Pts',(15.2366746708931,-2.45298676106926,329.615690711659));
#17861=CARTESIAN_POINT('Ctrl Pts',(15.240531796049,-2.37877500354578,329.58188127595));
#17862=CARTESIAN_POINT('Ctrl Pts',(15.244388921205,-2.3039172977635,329.549630634522));
#17863=CARTESIAN_POINT('Ctrl Pts',(15.2482460463609,-2.22848537934505,329.518961460038));
#17864=CARTESIAN_POINT('Ctrl Pts',(15.2556700237989,-2.08329826775007,329.459931158919));
#17865=CARTESIAN_POINT('Ctrl Pts',(15.2630940012369,-1.93554503594606,329.406584578907));
#17866=CARTESIAN_POINT('Ctrl Pts',(15.2705179786749,-1.78571098953377,329.359151941032));
#17867=CARTESIAN_POINT('Ctrl Pts',(15.2779331947026,-1.63605376983999,329.311775280807));
#17868=CARTESIAN_POINT('Ctrl Pts',(15.2853484107303,-1.48432097594482,329.270298781773));
#17869=CARTESIAN_POINT('Ctrl Pts',(15.2927636267579,-1.33101887579755,329.234905090567));
#17870=CARTESIAN_POINT('Ctrl Pts',(15.300171707902,-1.17786428215928,329.199545454993));
#17871=CARTESIAN_POINT('Ctrl Pts',(15.3075797890461,-1.0231437495697,329.170257058716));
#17872=CARTESIAN_POINT('Ctrl Pts',(15.3149878701903,-0.867379631619293,
329.14717306448));
#17873=CARTESIAN_POINT('Ctrl Pts',(15.3223904373643,-0.711731451746692,
329.124106252082));
#17874=CARTESIAN_POINT('Ctrl Pts',(15.3297930045383,-0.555041600752708,
329.107234700991));
#17875=CARTESIAN_POINT('Ctrl Pts',(15.3371955717123,-0.397843470320487,
329.096640690622));
#17876=CARTESIAN_POINT('Ctrl Pts',(15.3445942414671,-0.240728104016909,
329.086052257952));
#17877=CARTESIAN_POINT('Ctrl Pts',(15.3519929112219,-0.0831053626589326,
329.081734808737));
#17878=CARTESIAN_POINT('Ctrl Pts',(15.3593915809767,0.07448548873379,329.083718864484));
#17879=CARTESIAN_POINT('Ctrl Pts',(15.3667890301807,0.232050342529715,329.085702592923));
#17880=CARTESIAN_POINT('Ctrl Pts',(15.3741864793847,0.38958294398263,329.093985758454));
#17881=CARTESIAN_POINT('Ctrl Pts',(15.3815839285887,0.546543149124817,329.108546771072));
#17882=CARTESIAN_POINT('Ctrl Pts',(15.3889810570522,0.703496548746151,329.12310715235));
#17883=CARTESIAN_POINT('Ctrl Pts',(15.3963781855157,0.859877229787675,329.143944805024));
#17884=CARTESIAN_POINT('Ctrl Pts',(15.4037753139792,1.0151495633807,329.170986196065));
#17885=CARTESIAN_POINT('Ctrl Pts',(15.4111735814158,1.17044580503697,329.198031750804));
#17886=CARTESIAN_POINT('Ctrl Pts',(15.4185718488525,1.32463299174301,329.231282881844));
#17887=CARTESIAN_POINT('Ctrl Pts',(15.4259701162891,1.47718523496209,329.270614837165));
#17888=CARTESIAN_POINT('Ctrl Pts',(15.4333709828149,1.62979107138849,329.309960610216));
#17889=CARTESIAN_POINT('Ctrl Pts',(15.4407718493406,1.7807604595874,329.355391367716));
#17890=CARTESIAN_POINT('Ctrl Pts',(15.4481727158663,1.92958237276239,329.406732401429));
#17891=CARTESIAN_POINT('Ctrl Pts',(15.4555817092511,2.07856770662599,329.458129812505));
#17892=CARTESIAN_POINT('Ctrl Pts',(15.4629907026359,2.22540050313096,329.515450338983));
#17893=CARTESIAN_POINT('Ctrl Pts',(15.4703996960207,2.36958875542278,329.578470723802));
#17894=CARTESIAN_POINT('Ctrl Pts',(15.477813253601,2.5138658326516,329.641529931352));
#17895=CARTESIAN_POINT('Ctrl Pts',(15.4852268111813,2.65549478446371,329.710295831364));
#17896=CARTESIAN_POINT('Ctrl Pts',(15.4926403687615,2.79400841142042,329.784499299261));
#17897=CARTESIAN_POINT('Ctrl Pts',(15.5000644808982,2.93271923788341,329.858808409379));
#17898=CARTESIAN_POINT('Ctrl Pts',(15.507488593035,3.06830556062849,329.938570359729));
#17899=CARTESIAN_POINT('Ctrl Pts',(15.5149127051717,3.20032866108321,330.023472392968));
#17900=CARTESIAN_POINT('Ctrl Pts',(15.518769830326,3.26891997710075,330.067582417444));
#17901=CARTESIAN_POINT('Ctrl Pts',(15.5226269554804,3.33655002942041,330.11307918662));
#17902=CARTESIAN_POINT('Ctrl Pts',(15.5264840806347,3.40316093185349,330.159914645959));
#17903=CARTESIAN_POINT('Ctrl Pts',(15.5339080580727,3.53136984833921,330.250060902436));
#17904=CARTESIAN_POINT('Ctrl Pts',(15.5413320355107,3.65618787737881,330.345440851766));
#17905=CARTESIAN_POINT('Ctrl Pts',(15.5487560129487,3.77715879448751,330.445770975925));
#17906=CARTESIAN_POINT('Ctrl Pts',(15.5561712289763,3.89798694771296,330.545982695442));
#17907=CARTESIAN_POINT('Ctrl Pts',(15.563586445004,4.01497674181611,330.651132725357));
#17908=CARTESIAN_POINT('Ctrl Pts',(15.5710016610316,4.12770061470438,330.760894174726));
#17909=CARTESIAN_POINT('Ctrl Pts',(15.5784097421757,4.24031602524981,330.870550012182));
#17910=CARTESIAN_POINT('Ctrl Pts',(15.5858178233199,4.34867342056585,330.984808177061));
#17911=CARTESIAN_POINT('Ctrl Pts',(15.593225904464,4.45237814576104,331.103301473087));
#17912=CARTESIAN_POINT('Ctrl Pts',(15.600628471638,4.55600568163524,331.221706572388));
#17913=CARTESIAN_POINT('Ctrl Pts',(15.608031038812,4.65498719812048,331.344340246535));
#17914=CARTESIAN_POINT('Ctrl Pts',(15.6154336059861,4.74896485585733,331.470798481196));
#17915=CARTESIAN_POINT('Ctrl Pts',(15.6228322757408,4.84289303476812,331.597190136148));
#17916=CARTESIAN_POINT('Ctrl Pts',(15.6302309454956,4.93182237966197,331.727402042584));
#17917=CARTESIAN_POINT('Ctrl Pts',(15.6376296152504,5.01543539710643,331.860997237983));
#17918=CARTESIAN_POINT('Ctrl Pts',(15.6450270644544,5.09903462099934,331.994570394323));
#17919=CARTESIAN_POINT('Ctrl Pts',(15.6524245136583,5.17731906025537,332.131525415852));
#17920=CARTESIAN_POINT('Ctrl Pts',(15.6598219628623,5.25001456747629,332.271396400393));
#17921=CARTESIAN_POINT('Ctrl Pts',(15.6672190913258,5.32270692274676,332.411261320373));
#17922=CARTESIAN_POINT('Ctrl Pts',(15.6746162197893,5.3898106556944,332.554041620822));
#17923=CARTESIAN_POINT('Ctrl Pts',(15.6820133482528,5.45109774229761,332.699247087057));
#17924=CARTESIAN_POINT('Ctrl Pts',(15.6894116156894,5.51239426558222,332.844474911308));
#17925=CARTESIAN_POINT('Ctrl Pts',(15.696809883126,5.56787221409481,332.992128301003));
#17926=CARTESIAN_POINT('Ctrl Pts',(15.7042081505626,5.6173519060064,333.141697514777));
#17927=CARTESIAN_POINT('Ctrl Pts',(15.7116090170884,5.66684898065418,333.291319273788));
#17928=CARTESIAN_POINT('Ctrl Pts',(15.7190098836142,5.7103434860261,333.442857842815));
#17929=CARTESIAN_POINT('Ctrl Pts',(15.72641075014,5.74770579208278,333.59578894387));
#17930=CARTESIAN_POINT('Ctrl Pts',(15.7338197435248,5.78510912552349,333.748887977895));
#17931=CARTESIAN_POINT('Ctrl Pts',(15.7412287369095,5.81636672338197,333.903382234944));
#17932=CARTESIAN_POINT('Ctrl Pts',(15.7486377302943,5.84140007414198,334.058737158752));
#17933=CARTESIAN_POINT('Ctrl Pts',(15.7560512878746,5.86644884630955,334.214187786552));
#17934=CARTESIAN_POINT('Ctrl Pts',(15.7634648454549,5.88526568642664,334.370499767935));
#17935=CARTESIAN_POINT('Ctrl Pts',(15.7708784030351,5.8978240786673,334.527134586175));
#17936=CARTESIAN_POINT('Ctrl Pts',(15.7783025151718,5.91040035007842,334.683992402754));
#17937=CARTESIAN_POINT('Ctrl Pts',(15.7857266273085,5.9167003635619,334.841173602231));
#17938=CARTESIAN_POINT('Ctrl Pts',(15.7931507394453,5.91674970764539,334.998140005856));
#17939=CARTESIAN_POINT('Ctrl Pts',(15.7970078645998,5.91677534388339,335.079690372107));
#17940=CARTESIAN_POINT('Ctrl Pts',(15.8008649897542,5.91511464197454,335.161182838334));
#17941=CARTESIAN_POINT('Ctrl Pts',(15.8047221149087,5.91177668646496,335.242542721741));
#17942=CARTESIAN_POINT('Ctrl Pts',(15.8121460923467,5.90535197754329,335.399139646802));
#17943=CARTESIAN_POINT('Ctrl Pts',(15.8195700697847,5.89269114088026,335.555717353779));
#17944=CARTESIAN_POINT('Ctrl Pts',(15.8269940472227,5.87378570358288,335.7117387659));
#17945=CARTESIAN_POINT('Ctrl Pts',(15.8344092632503,5.854902577546,335.867576049281));
#17946=CARTESIAN_POINT('Ctrl Pts',(15.8418244792779,5.8297895645756,336.022857977704));
#17947=CARTESIAN_POINT('Ctrl Pts',(15.8492396953056,5.79849017585737,336.177048105638));
#17948=CARTESIAN_POINT('Ctrl Pts',(15.8566477764496,5.7672209032534,336.331089872607));
#17949=CARTESIAN_POINT('Ctrl Pts',(15.8640558575937,5.72977717896721,336.48404156718));
#17950=CARTESIAN_POINT('Ctrl Pts',(15.8714639387378,5.68625421577511,336.635372604662));
#17951=CARTESIAN_POINT('Ctrl Pts',(15.8788665059118,5.6427636475194,336.78659100369));
#17952=CARTESIAN_POINT('Ctrl Pts',(15.8862690730858,5.59320295278255,336.93619079038));
#17953=CARTESIAN_POINT('Ctrl Pts',(15.8936716402598,5.53771822842728,337.083652414642));
#17954=CARTESIAN_POINT('Ctrl Pts',(15.9010703100146,5.48226271653681,337.231036401004));
#17955=CARTESIAN_POINT('Ctrl Pts',(15.9084689797693,5.42088951775276,337.37628411848));
#17956=CARTESIAN_POINT('Ctrl Pts',(15.915867649524,5.35379426926663,337.518892114575));
#17957=CARTESIAN_POINT('Ctrl Pts',(15.923265098728,5.28671008941308,337.661476584779));
#17958=CARTESIAN_POINT('Ctrl Pts',(15.930662547932,5.21390589204398,337.801421860501));
#17959=CARTESIAN_POINT('Ctrl Pts',(15.938059997136,5.13562510735151,337.938245278945));
#17960=CARTESIAN_POINT('Ctrl Pts',(15.9454571255995,5.0573477167775,338.075062764963));
#17961=CARTESIAN_POINT('Ctrl Pts',(15.9528542540629,4.9735943963554,338.208758338899));
#17962=CARTESIAN_POINT('Ctrl Pts',(15.9602513825264,4.88465398118969,338.338874967193));
#17963=CARTESIAN_POINT('Ctrl Pts',(15.967649649963,4.79569987142016,338.4690116302));
#17964=CARTESIAN_POINT('Ctrl Pts',(15.9750479173995,4.70155728724309,338.595567942188));
#17965=CARTESIAN_POINT('Ctrl Pts',(15.9824461848361,4.60255764489959,338.718116954572));
#17966=CARTESIAN_POINT('Ctrl Pts',(15.9898470513619,4.50352322294063,338.840709019713));
#17967=CARTESIAN_POINT('Ctrl Pts',(15.9972479178877,4.39962857988415,338.959290692176));
#17968=CARTESIAN_POINT('Ctrl Pts',(16.0046487844134,4.2912444420216,339.073469246394));
#17969=CARTESIAN_POINT('Ctrl Pts',(16.0120577777982,4.18274128801374,339.187773179581));
#17970=CARTESIAN_POINT('Ctrl Pts',(16.0194667711829,4.06973905103298,339.297664067839));
#17971=CARTESIAN_POINT('Ctrl Pts',(16.0268757645676,3.95264476376096,339.402786610093));
#17972=CARTESIAN_POINT('Ctrl Pts',(16.0342893221479,3.83547834236897,339.507973911458));
#17973=CARTESIAN_POINT('Ctrl Pts',(16.0417028797281,3.71421513435229,339.608386776058));
#17974=CARTESIAN_POINT('Ctrl Pts',(16.0491164373084,3.58929364067983,339.703711483868));
#17975=CARTESIAN_POINT('Ctrl Pts',(16.0565405494451,3.46419429839136,339.799171903851));
#17976=CARTESIAN_POINT('Ctrl Pts',(16.0639646615817,3.33542657322832,339.889529485687));
#17977=CARTESIAN_POINT('Ctrl Pts',(16.0713887737184,3.20345687860428,339.974514507912));
#17978=CARTESIAN_POINT('Ctrl Pts',(16.0752458988732,3.1348933090586,340.018667648511));
#17979=CARTESIAN_POINT('Ctrl Pts',(16.0791030240279,3.06546585454412,340.061371378362));
#17980=CARTESIAN_POINT('Ctrl Pts',(16.0829601491827,2.99524223358791,340.102592921705));
#17981=CARTESIAN_POINT('Ctrl Pts',(16.0903841266206,2.86007975980807,340.181933828587));
#17982=CARTESIAN_POINT('Ctrl Pts',(16.0978081040587,2.72155872037476,340.256020242603));
#17983=CARTESIAN_POINT('Ctrl Pts',(16.1052320814967,2.58012616943561,340.324554395655));
#17984=CARTESIAN_POINT('Ctrl Pts',(16.1126472975243,2.43886053018624,340.393007668096));
#17985=CARTESIAN_POINT('Ctrl Pts',(16.1200625135519,2.29469055147802,340.455921561271));
#17986=CARTESIAN_POINT('Ctrl Pts',(16.1274777295795,2.14809088820202,340.513042363208));
#17987=CARTESIAN_POINT('Ctrl Pts',(16.1348858107236,2.001632282384,340.570108203796));
#17988=CARTESIAN_POINT('Ctrl Pts',(16.1422938918677,1.85274899160489,340.621391915517));
#17989=CARTESIAN_POINT('Ctrl Pts',(16.1497019730118,1.70193872094931,340.666686435002));
#17990=CARTESIAN_POINT('Ctrl Pts',(16.1571045401858,1.55124070113231,340.711947240949));
#17991=CARTESIAN_POINT('Ctrl Pts',(16.1645071073598,1.39861891321875,340.751227624025));
#17992=CARTESIAN_POINT('Ctrl Pts',(16.1719096745338,1.24458931935898,340.784369281835));
#17993=CARTESIAN_POINT('Ctrl Pts',(16.1793083442885,1.0906408214072,340.817493490707));
#17994=CARTESIAN_POINT('Ctrl Pts',(16.1867070140433,0.935286357602493,340.844485332748));
#17995=CARTESIAN_POINT('Ctrl Pts',(16.194105683798,0.779055162397271,340.865236876414));
#17996=CARTESIAN_POINT('Ctrl Pts',(16.201503133002,0.62284974048802,340.885984996719));
#17997=CARTESIAN_POINT('Ctrl Pts',(16.208900582206,0.465768243831204,340.900494812694));
#17998=CARTESIAN_POINT('Ctrl Pts',(16.2162980314099,0.308348287915098,340.908709833444));
#17999=CARTESIAN_POINT('Ctrl Pts',(16.2236951598734,0.150935157453836,340.916924498006));
#18000=CARTESIAN_POINT('Ctrl Pts',(16.2310922883369,-0.00681603038382703,
340.918844890571));
#18001=CARTESIAN_POINT('Ctrl Pts',(16.2384894168004,-0.164364641079509,
340.914466571658));
#18002=CARTESIAN_POINT('Ctrl Pts',(16.245887684237,-0.321937510328295,340.910087578594));
#18003=CARTESIAN_POINT('Ctrl Pts',(16.2532859516736,-0.479307367238124,
340.899407953332));
#18004=CARTESIAN_POINT('Ctrl Pts',(16.2606842191102,-0.635935833290562,
340.882475344482));
#18005=CARTESIAN_POINT('Ctrl Pts',(16.2680850856359,-0.792619324570043,
340.865536787029));
#18006=CARTESIAN_POINT('Ctrl Pts',(16.2754859521616,-0.948560535604319,
340.842340912372));
#18007=CARTESIAN_POINT('Ctrl Pts',(16.2828868186874,-1.10322859381684,340.812986945821));
#18008=CARTESIAN_POINT('Ctrl Pts',(16.2902958120721,-1.25806649234457,340.783600745808));
#18009=CARTESIAN_POINT('Ctrl Pts',(16.2977048054569,-1.41162807919804,340.748043019108));
#18010=CARTESIAN_POINT('Ctrl Pts',(16.3051137988417,-1.56339430538188,340.706463774388));
#18011=CARTESIAN_POINT('Ctrl Pts',(16.3125273564219,-1.71525402479601,340.664858915418));
#18012=CARTESIAN_POINT('Ctrl Pts',(16.3199409140022,-1.86531582479206,340.617225259484));
#18013=CARTESIAN_POINT('Ctrl Pts',(16.3273544715824,-2.01307859347319,340.563761779498));
#18014=CARTESIAN_POINT('Ctrl Pts',(16.3347785837191,-2.16105172950692,340.51022218446));
#18015=CARTESIAN_POINT('Ctrl Pts',(16.3422026958558,-2.30671895254345,340.45083632948));
#18016=CARTESIAN_POINT('Ctrl Pts',(16.3496268079925,-2.44960104498864,340.385850469786));
#18017=CARTESIAN_POINT('Ctrl Pts',(16.3534839331471,-2.52383404454175,340.352087699301));
#18018=CARTESIAN_POINT('Ctrl Pts',(16.3573410583018,-2.59731570140048,340.316814110192));
#18019=CARTESIAN_POINT('Ctrl Pts',(16.3611981834565,-2.66998180734956,340.280068911569));
#18020=CARTESIAN_POINT('Ctrl Pts',(16.3686221608945,-2.80984543879467,340.209343821098));
#18021=CARTESIAN_POINT('Ctrl Pts',(16.3760461383325,-2.94710796767754,340.132950933523));
#18022=CARTESIAN_POINT('Ctrl Pts',(16.3834701157705,-3.08127706780265,340.051105046812));
#18023=CARTESIAN_POINT('Ctrl Pts',(16.3908853317981,-3.21528782820279,339.969355750563));
#18024=CARTESIAN_POINT('Ctrl Pts',(16.3983005478257,-3.3462121111337,339.882166457331));
#18025=CARTESIAN_POINT('Ctrl Pts',(16.4057157638534,-3.47357970178658,339.789799016434));
#18026=CARTESIAN_POINT('Ctrl Pts',(16.4131238449974,-3.60082473998494,339.697520451024));
#18027=CARTESIAN_POINT('Ctrl Pts',(16.4205319261416,-3.72451959882275,339.600073874593));
#18028=CARTESIAN_POINT('Ctrl Pts',(16.4279400072857,-3.84422081751713,339.497765764095));
#18029=CARTESIAN_POINT('Ctrl Pts',(16.4353425744597,-3.96383294040825,339.395533803393));
#18030=CARTESIAN_POINT('Ctrl Pts',(16.4427451416336,-4.0794570594239,339.288447755084));
#18031=CARTESIAN_POINT('Ctrl Pts',(16.4501477088076,-4.19068083797589,339.176855836239));
#18032=CARTESIAN_POINT('Ctrl Pts',(16.4575463785624,-4.30184605769473,339.065322670051));
#18033=CARTESIAN_POINT('Ctrl Pts',(16.4649450483171,-4.40861528811464,338.949288621615));
#18034=CARTESIAN_POINT('Ctrl Pts',(16.4723437180718,-4.51061136816778,338.829140327522));
#18035=CARTESIAN_POINT('Ctrl Pts',(16.4797411672758,-4.61259062203485,338.709011854166));
#18036=CARTESIAN_POINT('Ctrl Pts',(16.4871386164798,-4.7097980470165,338.584770766438));
#18037=CARTESIAN_POINT('Ctrl Pts',(16.4945360656838,-4.80189520412677,338.456838586206));
#18038=CARTESIAN_POINT('Ctrl Pts',(16.5019331941473,-4.89398836806486,338.328911952891));
#18039=CARTESIAN_POINT('Ctrl Pts',(16.5093303226107,-4.98097148664305,338.197294848174));
#18040=CARTESIAN_POINT('Ctrl Pts',(16.5167274510742,-5.0625482582468,338.062439500696));
#18041=CARTESIAN_POINT('Ctrl Pts',(16.5241257185108,-5.14413759063696,337.927563388861));
#18042=CARTESIAN_POINT('Ctrl Pts',(16.5315239859474,-5.22031872536865,337.789448360821));
#18043=CARTESIAN_POINT('Ctrl Pts',(16.538922253384,-5.29084038366606,337.648572935954));
#18044=CARTESIAN_POINT('Ctrl Pts',(16.5463231199098,-5.36138681696366,337.507648020069));
#18045=CARTESIAN_POINT('Ctrl Pts',(16.5537239864355,-5.4262696482983,337.363961110095));
#18046=CARTESIAN_POINT('Ctrl Pts',(16.5611248529613,-5.48528503273618,337.218012324614));
#18047=CARTESIAN_POINT('Ctrl Pts',(16.568533846346,-5.54436522170827,337.071903273414));
#18048=CARTESIAN_POINT('Ctrl Pts',(16.5759428397308,-5.59756495674408,336.923527732717));
#18049=CARTESIAN_POINT('Ctrl Pts',(16.5833518331155,-5.64472949613641,336.773403360194));
#18050=CARTESIAN_POINT('Ctrl Pts',(16.5907653906957,-5.69192309051188,336.623186505879));
#18051=CARTESIAN_POINT('Ctrl Pts',(16.598178948276,-5.73307398353923,336.47121903239));
#18052=CARTESIAN_POINT('Ctrl Pts',(16.6055925058562,-5.76807831538502,336.318030011071));
#18053=CARTESIAN_POINT('Ctrl Pts',(16.6130166179929,-5.80313248230559,336.164622897136));
#18054=CARTESIAN_POINT('Ctrl Pts',(16.6204407301296,-5.83202254267949,336.009991127921));
#18055=CARTESIAN_POINT('Ctrl Pts',(16.6278648422663,-5.85469624564492,335.85467095056));
#18056=CARTESIAN_POINT('Ctrl Pts',(16.631721967421,-5.86647614719388,335.773975865127));
#18057=CARTESIAN_POINT('Ctrl Pts',(16.6355790925757,-5.87657897448611,335.693095009146));
#18058=CARTESIAN_POINT('Ctrl Pts',(16.6394362177305,-5.88500295254959,335.612103594976));
#18059=CARTESIAN_POINT('Ctrl Pts',(16.6490580185851,-5.906017007339,335.410066267478));
#18060=CARTESIAN_POINT('Ctrl Pts',(16.6586798194398,-5.91662935509008,335.206928493545));
#18061=CARTESIAN_POINT('Ctrl Pts',(16.6683016202945,-5.91674897726595,335.003478867974));
#18062=CARTESIAN_POINT('',(18.4183016202946,-5.90876483699497,335.00325795821));
#18063=CARTESIAN_POINT('Ctrl Pts',(16.6683041419001,-5.92392104138316,335.003429701801));
#18064=CARTESIAN_POINT('Ctrl Pts',(16.7514275119349,-5.91162770464222,333.243676356358));
#18065=CARTESIAN_POINT('Ctrl Pts',(16.9272968933942,-4.14640825180893,329.499088905554));
#18066=CARTESIAN_POINT('Ctrl Pts',(17.1959122862784,2.22434875857224,328.366381415739));
#18067=CARTESIAN_POINT('Ctrl Pts',(17.4741503205522,6.78207413591985,333.280670672585));
#18068=CARTESIAN_POINT('Ctrl Pts',(17.7523883548264,5.11599018198272,339.772763075944));
#18069=CARTESIAN_POINT('Ctrl Pts',(18.0306263891,-1.24496245006616,341.884961250371));
#18070=CARTESIAN_POINT('Ctrl Pts',(18.2525974775897,-5.40812166706467,338.52950027048));
#18071=CARTESIAN_POINT('Ctrl Pts',(18.3818225546544,-5.91264194830766,335.780609200208));
#18072=CARTESIAN_POINT('Ctrl Pts',(18.4183016202946,-5.90876483699497,335.00325795821));
#18073=CARTESIAN_POINT('',(20.1683016202945,-5.91198872894514,334.99513445012));
#18074=CARTESIAN_POINT('Ctrl Pts',(18.4183016202946,-5.90876483699497,335.00325795821));
#18075=CARTESIAN_POINT('Ctrl Pts',(18.474568566079,-5.90278460673951,333.804236562747));
#18076=CARTESIAN_POINT('Ctrl Pts',(18.6235815232882,-4.96516095045598,330.620246725548));
#18077=CARTESIAN_POINT('Ctrl Pts',(18.8653404919221,0.239575224204735,328.007487816731));
#18078=CARTESIAN_POINT('Ctrl Pts',(19.143578526196,6.00980057425877,331.417414344516));
#18079=CARTESIAN_POINT('Ctrl Pts',(19.4218165604697,6.26492064182342,338.115026849459));
#18080=CARTESIAN_POINT('Ctrl Pts',(19.7000545947439,0.77081550646824,341.954025192377));
#18081=CARTESIAN_POINT('Ctrl Pts',(19.9488829480187,-4.77516190733568,339.680170192244));
#18082=CARTESIAN_POINT('Ctrl Pts',(20.1049652898689,-5.90157873863965,336.342952334915));
#18083=CARTESIAN_POINT('Ctrl Pts',(20.1683016202945,-5.91198872894514,334.99513445012));
#18084=CARTESIAN_POINT('',(21.9183016202945,-5.92629064703929,334.99899238386));
#18085=CARTESIAN_POINT('Ctrl Pts',(20.1683016202945,-5.91198872894514,334.99513445012));
#18086=CARTESIAN_POINT('Ctrl Pts',(20.1977113012936,-5.91682251852579,334.369286792539));
#18087=CARTESIAN_POINT('Ctrl Pts',(20.3198669937171,-5.53687134207544,331.775491648162));
#18088=CARTESIAN_POINT('Ctrl Pts',(20.5347686975658,-1.76510783169628,328.229695925316));
#18089=CARTESIAN_POINT('Ctrl Pts',(20.8130067318395,4.7380920049118,329.851883152624));
#18090=CARTESIAN_POINT('Ctrl Pts',(21.0912447661135,6.89321474273118,336.19842122469));
#18091=CARTESIAN_POINT('Ctrl Pts',(21.3694828003874,2.72253605483465,341.445185827526));
#18092=CARTESIAN_POINT('Ctrl Pts',(21.6451684184478,-3.88539471633639,340.783425390433));
#18093=CARTESIAN_POINT('Ctrl Pts',(21.8281080250835,-5.92180424765322,336.906401464071));
#18094=CARTESIAN_POINT('Ctrl Pts',(21.9183016202945,-5.92629064703929,334.99899238386));
#18095=CARTESIAN_POINT('',(23.6683016202945,-5.91500612781905,335.00540571853));
#18096=CARTESIAN_POINT('Ctrl Pts',(21.9183016202945,-5.92629064703929,334.99899238386));
#18097=CARTESIAN_POINT('Ctrl Pts',(21.9208540365081,-5.92641760903151,334.945014029289));
#18098=CARTESIAN_POINT('Ctrl Pts',(21.9234064527217,-5.92574411097084,334.891038923218));
#18099=CARTESIAN_POINT('Ctrl Pts',(22.01870488036,-5.87034887063351,332.876626256431));
#18100=CARTESIAN_POINT('Ctrl Pts',(22.2041969032092,-3.62310438234698,329.014539486737));
#18101=CARTESIAN_POINT('Ctrl Pts',(22.4824349374833,3.07263176483227,328.714178099963));
#18102=CARTESIAN_POINT('Ctrl Pts',(22.7606729717571,6.94865909339069,334.182222692275));
#18103=CARTESIAN_POINT('Ctrl Pts',(23.038911006031,4.44800453399053,340.400729449511));
#18104=CARTESIAN_POINT('Ctrl Pts',(23.3171490403051,-2.13451813381742,341.663066505569));
#18105=CARTESIAN_POINT('Ctrl Pts',(23.5269459117261,-5.62088275218896,338.004367855669));
#18106=CARTESIAN_POINT('Ctrl Pts',(23.6439967717226,-5.91961735110844,335.521952838584));
#18107=CARTESIAN_POINT('Ctrl Pts',(23.6683016202945,-5.91500612781905,335.00540571853));
#18108=CARTESIAN_POINT('',(25.4183016202945,-5.90739708893958,334.998339410743));
#18109=CARTESIAN_POINT('Ctrl Pts',(23.6683016202945,-5.91500612781905,335.00540571853));
#18110=CARTESIAN_POINT('Ctrl Pts',(23.7367427831473,-5.90202116791829,333.550836460046));
#18111=CARTESIAN_POINT('Ctrl Pts',(23.8979299574247,-4.62690565408727,330.104798499186));
#18112=CARTESIAN_POINT('Ctrl Pts',(24.151863143127,1.15182530317369,328.098846372365));
#18113=CARTESIAN_POINT('Ctrl Pts',(24.4301011774006,6.42664607839832,332.233984254528));
#18114=CARTESIAN_POINT('Ctrl Pts',(24.7083392116747,5.80382860462329,338.907453959981));
#18115=CARTESIAN_POINT('Ctrl Pts',(24.9865772459487,-0.14507671524839,341.995110840288));
#18116=CARTESIAN_POINT('Ctrl Pts',(25.2232313821552,-5.09165478374774,339.161387958908));
#18117=CARTESIAN_POINT('Ctrl Pts',(25.3671395069372,-5.90466232056242,336.089210272338));
#18118=CARTESIAN_POINT('Ctrl Pts',(25.4183016202945,-5.90739708893958,334.998339410743));
#18119=CARTESIAN_POINT('',(27.1683016202945,-5.92111329140699,334.99527144238));
#18120=CARTESIAN_POINT('Ctrl Pts',(25.4183016202945,-5.90739708893958,334.998339410743));
#18121=CARTESIAN_POINT('Ctrl Pts',(25.4598855183618,-5.90961987298759,334.111693810387));
#18122=CARTESIAN_POINT('Ctrl Pts',(25.594215427854,-5.30581593151386,331.250407457081));
#18123=CARTESIAN_POINT('Ctrl Pts',(25.8212913487704,-0.864701785489386,
328.057024143541));
#18124=CARTESIAN_POINT('Ctrl Pts',(26.0995293830443,5.3705567668813,330.515611197175));
#18125=CARTESIAN_POINT('Ctrl Pts',(26.3777674173184,6.67733464357878,337.089455665694));
#18126=CARTESIAN_POINT('Ctrl Pts',(26.6560054515924,1.85642107515762,341.745837510118));
#18127=CARTESIAN_POINT('Ctrl Pts',(26.9195168525843,-4.32277153150168,340.292864862948));
#18128=CARTESIAN_POINT('Ctrl Pts',(27.0902822421518,-5.90669512999897,336.649017329653));
#18129=CARTESIAN_POINT('Ctrl Pts',(27.1683016202945,-5.92111329140699,334.99527144238));
#18130=CARTESIAN_POINT('',(28.9183016202945,-5.92262096125729,335.004164858762));
#18131=CARTESIAN_POINT('Ctrl Pts',(27.1683016202945,-5.92111329140699,334.99527144238));
#18132=CARTESIAN_POINT('Ctrl Pts',(27.1830282535764,-5.92383480727534,334.683116823835));
#18133=CARTESIAN_POINT('Ctrl Pts',(27.290500898283,-5.75928232400781,332.407936679943));
#18134=CARTESIAN_POINT('Ctrl Pts',(27.490719554414,-2.809369194695,328.592186983913));
#18135=CARTESIAN_POINT('Ctrl Pts',(27.7689575886882,3.86815579710411,329.169906205681));
#18136=CARTESIAN_POINT('Ctrl Pts',(28.0471956229618,6.99593130778298,335.097816450449));
#18137=CARTESIAN_POINT('Ctrl Pts',(28.3254336572358,3.70364391709208,340.935961982409));
#18138=CARTESIAN_POINT('Ctrl Pts',(28.6036716915099,-2.98742283062345,341.326762817769));
#18139=CARTESIAN_POINT('Ctrl Pts',(28.8012943458627,-5.79265084944902,337.480554438737));
#18140=CARTESIAN_POINT('Ctrl Pts',(28.9061709887909,-5.9246739829894,335.261122693151));
#18141=CARTESIAN_POINT('Ctrl Pts',(28.9183016202945,-5.92262096125729,335.004164858762));
#18142=CARTESIAN_POINT('',(30.6683016202945,-5.90798040082929,335.002506028461));
#18143=CARTESIAN_POINT('Ctrl Pts',(28.9183016202945,-5.92262096125729,335.004164858762));
#18144=CARTESIAN_POINT('Ctrl Pts',(28.9989170002156,-5.90897739069207,333.296524705252));
#18145=CARTESIAN_POINT('Ctrl Pts',(29.1722783915612,-4.23435313665628,329.600953149295));
#18146=CARTESIAN_POINT('Ctrl Pts',(29.4383857943318,2.04429783446821,328.308701973068));
#18147=CARTESIAN_POINT('Ctrl Pts',(29.7166238286054,6.73314212344229,333.098048353212));
#18148=CARTESIAN_POINT('Ctrl Pts',(29.9948618628796,5.24308126675361,339.632787686851));
#18149=CARTESIAN_POINT('Ctrl Pts',(30.2730998971534,-1.05847788068605,341.916086140104));
#18150=CARTESIAN_POINT('Ctrl Pts',(30.4975798162917,-5.35884259352751,338.637697927416));
#18151=CARTESIAN_POINT('Ctrl Pts',(30.6293137240055,-5.91114314230631,335.833595143404));
#18152=CARTESIAN_POINT('Ctrl Pts',(30.6683016202945,-5.90798040082929,335.002506028461));
#18153=CARTESIAN_POINT('',(32.418301636369,-5.91460742755292,334.994794146473));
#18154=CARTESIAN_POINT('Ctrl Pts',(30.6683016202945,-5.90798040082929,335.002506028461));
#18155=CARTESIAN_POINT('Ctrl Pts',(30.7220597354301,-5.90361948278424,333.856566170669));
#18156=CARTESIAN_POINT('Ctrl Pts',(30.8685638619903,-5.02842874153069,330.727440116774));
#18157=CARTESIAN_POINT('Ctrl Pts',(31.1078139999753,0.0505517212931561,
328.003567520179));
#18158=CARTESIAN_POINT('Ctrl Pts',(31.386052034249,5.91080577166923,331.256338950865));
#18159=CARTESIAN_POINT('Ctrl Pts',(31.6642900685232,6.34680060873793,337.944612869997));
#18160=CARTESIAN_POINT('Ctrl Pts',(31.942528102797,0.958430205788535,341.930659020746));
#18161=CARTESIAN_POINT('Ctrl Pts',(32.1938652867209,-4.70347817982554,339.786078150809));
#18162=CARTESIAN_POINT('Ctrl Pts',(32.35245645922,-5.90164065851028,336.395145633034));
#18163=CARTESIAN_POINT('Ctrl Pts',(32.4183016202945,-5.91341914242724,334.994795534346));
#18164=CARTESIAN_POINT('',(34.1683016202624,-5.91674999997471,334.999982700985));
#18165=CARTESIAN_POINT('Ctrl Pts',(32.4183016653215,-5.91674770761404,334.994791646704));
#18166=CARTESIAN_POINT('Ctrl Pts',(32.4273153323639,-5.91657886872254,334.802988774011));
#18167=CARTESIAN_POINT('Ctrl Pts',(32.4363289994064,-5.9070798724418,334.611596525586));
#18168=CARTESIAN_POINT('Ctrl Pts',(32.4453426664488,-5.88839253570148,334.421412143236));
#18169=CARTESIAN_POINT('Ctrl Pts',(32.4544843738112,-5.86943974289714,334.228526166845));
#18170=CARTESIAN_POINT('Ctrl Pts',(32.4636260811736,-5.84103576178567,334.036882586459));
#18171=CARTESIAN_POINT('Ctrl Pts',(32.472767788536,-5.80337755149894,333.847290341301));
#18172=CARTESIAN_POINT('Ctrl Pts',(32.4815132494723,-5.76735163271395,333.665915953769));
#18173=CARTESIAN_POINT('Ctrl Pts',(32.4902587104086,-5.7228567391478,333.486418710041));
#18174=CARTESIAN_POINT('Ctrl Pts',(32.499004171345,-5.67010589101885,333.309488317954));
#18175=CARTESIAN_POINT('Ctrl Pts',(32.506428148783,-5.6253259635575,333.159293005378));
#18176=CARTESIAN_POINT('Ctrl Pts',(32.513852126221,-5.57450658153742,333.010651606305));
#18177=CARTESIAN_POINT('Ctrl Pts',(32.5212761036589,-5.51777175704479,332.864086752778));
#18178=CARTESIAN_POINT('Ctrl Pts',(32.5286913196866,-5.46110388818127,332.71769486783));
#18179=CARTESIAN_POINT('Ctrl Pts',(32.5361065357142,-5.39853460627703,332.573374995057));
#18180=CARTESIAN_POINT('Ctrl Pts',(32.5435217517418,-5.33023815207165,332.431636356608));
#18181=CARTESIAN_POINT('Ctrl Pts',(32.5509298328859,-5.26200741237057,332.290034098363));
#18182=CARTESIAN_POINT('Ctrl Pts',(32.55833791403,-5.18806063197998,332.151008463924));
#18183=CARTESIAN_POINT('Ctrl Pts',(32.5657459951741,-5.1086207190128,332.015050266458));
#18184=CARTESIAN_POINT('Ctrl Pts',(32.5731485623481,-5.0292399346237,331.879193265161));
#18185=CARTESIAN_POINT('Ctrl Pts',(32.5805511295221,-4.94437434620895,331.746399475609));
#18186=CARTESIAN_POINT('Ctrl Pts',(32.5879536966961,-4.85429346317123,331.617136488725));
#18187=CARTESIAN_POINT('Ctrl Pts',(32.5953523664508,-4.76426000732511,331.48794155824));
#18188=CARTESIAN_POINT('Ctrl Pts',(32.6027510362055,-4.66901693818283,331.362274033633));
#18189=CARTESIAN_POINT('Ctrl Pts',(32.6101497059602,-4.56887781756843,331.240573707249));
#18190=CARTESIAN_POINT('Ctrl Pts',(32.6175471551641,-4.46875521679902,331.118893457638));
#18191=CARTESIAN_POINT('Ctrl Pts',(32.6249446043681,-4.36373840447703,331.001179395262));
#18192=CARTESIAN_POINT('Ctrl Pts',(32.632342053572,-4.25418214614182,330.887839396382));
#18193=CARTESIAN_POINT('Ctrl Pts',(32.6397391820355,-4.14463063797514,330.774504311727));
#18194=CARTESIAN_POINT('Ctrl Pts',(32.6471363104989,-4.03054033452622,330.66554318182));
#18195=CARTESIAN_POINT('Ctrl Pts',(32.6545334389624,-3.91230369900613,330.561327864187));
#18196=CARTESIAN_POINT('Ctrl Pts',(32.661931706399,-3.79404885799557,330.457096499996));
#18197=CARTESIAN_POINT('Ctrl Pts',(32.6693299738356,-3.67164669370789,330.357612649864));
#18198=CARTESIAN_POINT('Ctrl Pts',(32.6767282412721,-3.54552353319519,330.263208529177));
#18199=CARTESIAN_POINT('Ctrl Pts',(32.6841291077979,-3.41935606428986,330.16877124333));
#18200=CARTESIAN_POINT('Ctrl Pts',(32.6915299743236,-3.28946529507127,330.07941746349));
#18201=CARTESIAN_POINT('Ctrl Pts',(32.6989308408493,-3.15630722727234,329.995436557544));
#18202=CARTESIAN_POINT('Ctrl Pts',(32.7063398342341,-3.02300293918437,329.911363432534));
#18203=CARTESIAN_POINT('Ctrl Pts',(32.7137488276188,-2.88642450333695,329.832675163101));
#18204=CARTESIAN_POINT('Ctrl Pts',(32.7211578210036,-2.74705389675535,329.759615906174));
#18205=CARTESIAN_POINT('Ctrl Pts',(32.7285713785838,-2.60759743307269,329.686511642226));
#18206=CARTESIAN_POINT('Ctrl Pts',(32.735984936164,-2.46534570760064,329.619043460126));
#18207=CARTESIAN_POINT('Ctrl Pts',(32.7433984937442,-2.32080096015193,329.557407468324));
#18208=CARTESIAN_POINT('Ctrl Pts',(32.7508226058809,-2.17605042679298,329.495683726404));
#18209=CARTESIAN_POINT('Ctrl Pts',(32.7582467180176,-2.02900069945885,329.439808890119));
#18210=CARTESIAN_POINT('Ctrl Pts',(32.7656708301542,-1.88017023918067,329.389929551761));
#18211=CARTESIAN_POINT('Ctrl Pts',(32.7695279553091,-1.80284682304979,329.364015227308));
#18212=CARTESIAN_POINT('Ctrl Pts',(32.7733850804639,-1.72504294531009,329.339718384046));
#18213=CARTESIAN_POINT('Ctrl Pts',(32.7772422056188,-1.64683230932039,329.317054117143));
#18214=CARTESIAN_POINT('Ctrl Pts',(32.7846661830568,-1.49629687847732,329.273431211643));
#18215=CARTESIAN_POINT('Ctrl Pts',(32.7920901604948,-1.3437998712445,329.235727924088));
#18216=CARTESIAN_POINT('Ctrl Pts',(32.7995141379328,-1.18984789011225,329.204122796255));
#18217=CARTESIAN_POINT('Ctrl Pts',(32.8069293539605,-1.03607759548106,329.172554967228));
#18218=CARTESIAN_POINT('Ctrl Pts',(32.8143445699881,-0.880856106873434,
329.147071047008));
#18219=CARTESIAN_POINT('Ctrl Pts',(32.8217597860157,-0.724705931719506,
329.127800082164));
#18220=CARTESIAN_POINT('Ctrl Pts',(32.8291678671598,-0.568706003477776,
329.108547659746));
#18221=CARTESIAN_POINT('Ctrl Pts',(32.836575948304,-0.411779535561657,329.095496336878));
#18222=CARTESIAN_POINT('Ctrl Pts',(32.8439840294481,-0.254459891602752,
329.088724272539));
#18223=CARTESIAN_POINT('Ctrl Pts',(32.8513865966221,-0.0972573435282972,
329.081957248772));
#18224=CARTESIAN_POINT('Ctrl Pts',(32.8587891637962,0.0603374266150702,
329.081460193366));
#18225=CARTESIAN_POINT('Ctrl Pts',(32.8661917309702,0.217785364642319,329.087259510392));
#18226=CARTESIAN_POINT('Ctrl Pts',(32.8735904007249,0.375150407018542,329.093055774104));
#18227=CARTESIAN_POINT('Ctrl Pts',(32.8809890704796,0.532368399219997,329.105141794502));
#18228=CARTESIAN_POINT('Ctrl Pts',(32.8883877402344,0.688899824186392,329.123491887631));
#18229=CARTESIAN_POINT('Ctrl Pts',(32.8957851894384,0.845405426328227,329.141838953565));
#18230=CARTESIAN_POINT('Ctrl Pts',(32.9031826386425,1.0012243157115,329.166447997899));
#18231=CARTESIAN_POINT('Ctrl Pts',(32.9105800878465,1.15582151649482,329.197241415972));
#18232=CARTESIAN_POINT('Ctrl Pts',(32.9179772163099,1.31041201421304,329.228033498896));
#18233=CARTESIAN_POINT('Ctrl Pts',(32.9253743447734,1.46378056263265,329.265009349496));
#18234=CARTESIAN_POINT('Ctrl Pts',(32.9327714732369,1.61540207446399,329.308040170528));
#18235=CARTESIAN_POINT('Ctrl Pts',(32.9401697406735,1.76704693222317,329.351077617233));
#18236=CARTESIAN_POINT('Ctrl Pts',(32.9475680081102,1.91694385872561,329.40017178883));
#18237=CARTESIAN_POINT('Ctrl Pts',(32.9549662755468,2.0645827769338,329.455143958615));
#18238=CARTESIAN_POINT('Ctrl Pts',(32.9623671420726,2.21227356224677,329.510135440701));
#18239=CARTESIAN_POINT('Ctrl Pts',(32.9697680085984,2.35770441034913,329.571008902245));
#18240=CARTESIAN_POINT('Ctrl Pts',(32.9771688751241,2.50038521690832,329.63753747523));
#18241=CARTESIAN_POINT('Ctrl Pts',(32.9845778685089,2.64322270063395,329.704139102948));
#18242=CARTESIAN_POINT('Ctrl Pts',(32.9919868618937,2.78330377364729,329.776408085704));
#18243=CARTESIAN_POINT('Ctrl Pts',(32.9993958552785,2.92016229375279,329.854071246058));
#18244=CARTESIAN_POINT('Ctrl Pts',(33.0068094128587,3.05710512342743,329.931782249599));
#18245=CARTESIAN_POINT('Ctrl Pts',(33.014222970439,3.1908211281813,330.014893855699));
#18246=CARTESIAN_POINT('Ctrl Pts',(33.0216365280193,3.32087360545437,330.103089845719));
#18247=CARTESIAN_POINT('Ctrl Pts',(33.029060640156,3.45111123623795,330.191411398878));
#18248=CARTESIAN_POINT('Ctrl Pts',(33.0364847522927,3.57767462327906,330.284831571752));
#18249=CARTESIAN_POINT('Ctrl Pts',(33.0439088644294,3.7001599249798,330.382993708898));
#18250=CARTESIAN_POINT('Ctrl Pts',(33.0477659895839,3.76379597054971,330.433992891216));
#18251=CARTESIAN_POINT('Ctrl Pts',(33.0516231147384,3.82633184702468,330.486271415834));
#18252=CARTESIAN_POINT('Ctrl Pts',(33.0554802398929,3.88771497543774,330.539775472887));
#18253=CARTESIAN_POINT('Ctrl Pts',(33.0629042173309,4.00586176667684,330.642757070968));
#18254=CARTESIAN_POINT('Ctrl Pts',(33.0703281947689,4.12009214643664,330.75059164542));
#18255=CARTESIAN_POINT('Ctrl Pts',(33.0777521722069,4.22998182345058,330.862949802604));
#18256=CARTESIAN_POINT('Ctrl Pts',(33.0851673882345,4.33974181411186,330.975175360256));
#18257=CARTESIAN_POINT('Ctrl Pts',(33.0925826042622,4.44517104039266,331.091913610034));
#18258=CARTESIAN_POINT('Ctrl Pts',(33.0999978202898,4.54587822552875,331.212794998793));
#18259=CARTESIAN_POINT('Ctrl Pts',(33.1074059014339,4.64648851071844,331.33356007609));
#18260=CARTESIAN_POINT('Ctrl Pts',(33.1148139825781,4.74238556278388,331.458460071151));
#18261=CARTESIAN_POINT('Ctrl Pts',(33.1222220637222,4.83321502250708,331.587088763429));
#18262=CARTESIAN_POINT('Ctrl Pts',(33.1296246308962,4.9239768762044,331.715621715022));
#18263=CARTESIAN_POINT('Ctrl Pts',(33.1370271980702,5.00967843361043,331.847877534171));
#18264=CARTESIAN_POINT('Ctrl Pts',(33.1444297652442,5.09000577782698,331.98341720747));
#18265=CARTESIAN_POINT('Ctrl Pts',(33.1518284349989,5.17029083004798,332.118885519724));
#18266=CARTESIAN_POINT('Ctrl Pts',(33.1592271047537,5.24520711439813,332.257633922598));
#18267=CARTESIAN_POINT('Ctrl Pts',(33.1666257745084,5.31448426542388,332.399194825624));
#18268=CARTESIAN_POINT('Ctrl Pts',(33.1740232237124,5.38374998787089,332.540732375497));
#18269=CARTESIAN_POINT('Ctrl Pts',(33.1814206729164,5.44737825941084,332.685081169785));
#18270=CARTESIAN_POINT('Ctrl Pts',(33.1888181221204,5.50514483333374,332.831749339555));
#18271=CARTESIAN_POINT('Ctrl Pts',(33.1962152505839,5.5629089025987,332.97841115005));
#18272=CARTESIAN_POINT('Ctrl Pts',(33.2036123790473,5.61481164281959,333.127391788823));
#18273=CARTESIAN_POINT('Ctrl Pts',(33.2110095075108,5.66067720748356,333.278179999194));
#18274=CARTESIAN_POINT('Ctrl Pts',(33.2184077749474,5.70654983429954,333.428991427185));
#18275=CARTESIAN_POINT('Ctrl Pts',(33.225806042384,5.74638332603978,333.581610623865));
#18276=CARTESIAN_POINT('Ctrl Pts',(33.2332043098206,5.78005194584998,333.735511935297));
#18277=CARTESIAN_POINT('Ctrl Pts',(33.2406051763464,5.81373239380038,333.889467313878));
#18278=CARTESIAN_POINT('Ctrl Pts',(33.2480060428722,5.84124357803786,334.044705339639));
#18279=CARTESIAN_POINT('Ctrl Pts',(33.2554069093979,5.8625110531423,334.200691102086));
#18280=CARTESIAN_POINT('Ctrl Pts',(33.2628159027827,5.88380188196765,334.356848151814));
#18281=CARTESIAN_POINT('Ctrl Pts',(33.2702248961674,5.89883525903511,334.513754207971));
#18282=CARTESIAN_POINT('Ctrl Pts',(33.2776338895522,5.90758864879145,334.670869449655));
#18283=CARTESIAN_POINT('Ctrl Pts',(33.2850474471324,5.91634743093782,334.828081479747));
#18284=CARTESIAN_POINT('Ctrl Pts',(33.2924610047127,5.91881851105519,334.985502579854));
#18285=CARTESIAN_POINT('Ctrl Pts',(33.2998745622929,5.9150314793299,335.142594393425));
#18286=CARTESIAN_POINT('Ctrl Pts',(33.3072986744296,5.91123905607163,335.299909855953));
#18287=CARTESIAN_POINT('Ctrl Pts',(33.3147227865663,5.90117075060398,335.456894724218));
#18288=CARTESIAN_POINT('Ctrl Pts',(33.322146898703,5.88490794023595,335.613016392479));
#18289=CARTESIAN_POINT('Ctrl Pts',(33.3260040238576,5.87645875549847,335.6941278847));
#18290=CARTESIAN_POINT('Ctrl Pts',(33.3298611490122,5.86633837990226,335.775006546786));
#18291=CARTESIAN_POINT('Ctrl Pts',(33.3337182741668,5.85456360981412,335.855579044355));
#18292=CARTESIAN_POINT('Ctrl Pts',(33.3411422516047,5.83190019497317,336.010660453464));
#18293=CARTESIAN_POINT('Ctrl Pts',(33.3485662290427,5.80303641379231,336.165074692584));
#18294=CARTESIAN_POINT('Ctrl Pts',(33.3559902064807,5.76801965206156,336.31828671234));
#18295=CARTESIAN_POINT('Ctrl Pts',(33.3634054225083,5.7330442153782,336.47131791886));
#18296=CARTESIAN_POINT('Ctrl Pts',(33.370820638536,5.69193033450748,336.623149369867));
#18297=CARTESIAN_POINT('Ctrl Pts',(33.3782358545636,5.64477703226234,336.773252045972));
#18298=CARTESIAN_POINT('Ctrl Pts',(33.3856439357077,5.59766910068724,336.923210294037));
#18299=CARTESIAN_POINT('Ctrl Pts',(33.3930520168517,5.54453342766021,337.071442725081));
#18300=CARTESIAN_POINT('Ctrl Pts',(33.4004600979958,5.48551984860089,337.217431521627));
#18301=CARTESIAN_POINT('Ctrl Pts',(33.4078626651698,5.42655019442619,337.363311656046));
#18302=CARTESIAN_POINT('Ctrl Pts',(33.4152652323438,5.36171148481665,337.50695113661));
#18303=CARTESIAN_POINT('Ctrl Pts',(33.4226677995178,5.29120301706501,337.647848408558));
#18304=CARTESIAN_POINT('Ctrl Pts',(33.4300664692725,5.22073167171348,337.788671498707));
#18305=CARTESIAN_POINT('Ctrl Pts',(33.4374651390273,5.14459667982724,337.926754922663));
#18306=CARTESIAN_POINT('Ctrl Pts',(33.444863808782,5.06304493794562,338.061618284314));
#18307=CARTESIAN_POINT('Ctrl Pts',(33.452261257986,4.98150664956908,338.196459397698));
#18308=CARTESIAN_POINT('Ctrl Pts',(33.4596587071899,4.89455357762578,338.328081184006));
#18309=CARTESIAN_POINT('Ctrl Pts',(33.4670561563939,4.802477992433,338.456028890894));
#18310=CARTESIAN_POINT('Ctrl Pts',(33.4744532848574,4.71040639947719,338.583971050193));
#18311=CARTESIAN_POINT('Ctrl Pts',(33.4818504133209,4.61321295288255,338.708239143888));
#18312=CARTESIAN_POINT('Ctrl Pts',(33.4892475417843,4.51123241866238,338.82840862857));
#18313=CARTESIAN_POINT('Ctrl Pts',(33.4966458092209,4.40923618198558,338.948596616353));
#18314=CARTESIAN_POINT('Ctrl Pts',(33.5040440766575,4.30245163153557,339.064684453979));
#18315=CARTESIAN_POINT('Ctrl Pts',(33.5114423440941,4.19125275749657,339.176281945137));
#18316=CARTESIAN_POINT('Ctrl Pts',(33.5188432106198,4.08001481812373,339.287918641667));
#18317=CARTESIAN_POINT('Ctrl Pts',(33.5262440771455,3.96435973078682,339.395061586713));
#18318=CARTESIAN_POINT('Ctrl Pts',(33.5336449436713,3.84469702644138,339.497358706771));
#18319=CARTESIAN_POINT('Ctrl Pts',(33.541053937056,3.72490292100636,339.599768158848));
#18320=CARTESIAN_POINT('Ctrl Pts',(33.5484629304408,3.60109269388622,339.697320916601));
#18321=CARTESIAN_POINT('Ctrl Pts',(33.5558719238255,3.47370809671462,339.789705901339));
#18322=CARTESIAN_POINT('Ctrl Pts',(33.5632854814058,3.34624502623701,339.882147798414));
#18323=CARTESIAN_POINT('Ctrl Pts',(33.570699038986,3.21520350796785,339.969415372491));
#18324=CARTESIAN_POINT('Ctrl Pts',(33.5781125965663,3.08105227036256,340.051242170971));
#18325=CARTESIAN_POINT('Ctrl Pts',(33.5855367087029,2.94671004391106,340.133185464878));
#18326=CARTESIAN_POINT('Ctrl Pts',(33.5929608208396,2.80924958125493,340.209672332021));
#18327=CARTESIAN_POINT('Ctrl Pts',(33.6003849329763,2.66916279985474,340.280482980786));
#18328=CARTESIAN_POINT('Ctrl Pts',(33.6042420581311,2.59638207692788,340.317271963705));
#18329=CARTESIAN_POINT('Ctrl Pts',(33.6080991832859,2.52289276856279,340.352529608831));
#18330=CARTESIAN_POINT('Ctrl Pts',(33.6119563084408,2.44876563268213,340.386230355146));
#18331=CARTESIAN_POINT('Ctrl Pts',(33.6193802858788,2.30608989304925,340.451095655141));
#18332=CARTESIAN_POINT('Ctrl Pts',(33.6268042633167,2.16061981688871,340.51038589084));
#18333=CARTESIAN_POINT('Ctrl Pts',(33.6342282407547,2.012830981807,340.563851364044));
#18334=CARTESIAN_POINT('Ctrl Pts',(33.6416434567824,1.86521655978671,340.617253739946));
#18335=CARTESIAN_POINT('Ctrl Pts',(33.64905867281,1.7152891733996,340.664844910622));
#18336=CARTESIAN_POINT('Ctrl Pts',(33.6564738888376,1.56354727326193,340.706421863723));
#18337=CARTESIAN_POINT('Ctrl Pts',(33.6638819699817,1.41195137841644,340.747958811689));
#18338=CARTESIAN_POINT('Ctrl Pts',(33.6712900511258,1.25854480315241,340.783492964653));
#18339=CARTESIAN_POINT('Ctrl Pts',(33.6786981322699,1.10384407577409,340.812870101669));
#18340=CARTESIAN_POINT('Ctrl Pts',(33.6861006994439,0.94925849497255,340.842225372746));
#18341=CARTESIAN_POINT('Ctrl Pts',(33.693503266618,0.793381045138071,340.865432683527));
#18342=CARTESIAN_POINT('Ctrl Pts',(33.700905833792,0.636741345570367,340.882388207297));
#18343=CARTESIAN_POINT('Ctrl Pts',(33.7083045035467,0.480184116119897,340.899334804057));
#18344=CARTESIAN_POINT('Ctrl Pts',(33.7157031733014,0.322865806300446,340.910036129039));
#18345=CARTESIAN_POINT('Ctrl Pts',(33.7231018430562,0.165324001334266,340.914439832907));
#18346=CARTESIAN_POINT('Ctrl Pts',(33.7304992922602,0.00780818587397086,
340.918842810302));
#18347=CARTESIAN_POINT('Ctrl Pts',(33.7378967414641,-0.149930678855669,
340.91695021807));
#18348=CARTESIAN_POINT('Ctrl Pts',(33.7452941906681,-0.307352017666371,
340.90876173997));
#18349=CARTESIAN_POINT('Ctrl Pts',(33.7526913191316,-0.464766530962269,
340.900573616908));
#18350=CARTESIAN_POINT('Ctrl Pts',(33.7600884475951,-0.621863173005875,
340.886090170136));
#18351=CARTESIAN_POINT('Ctrl Pts',(33.7674855760585,-0.778103775087002,
340.865363166735));
#18352=CARTESIAN_POINT('Ctrl Pts',(33.7748838434951,-0.934368434320559,
340.844632971894));
#18353=CARTESIAN_POINT('Ctrl Pts',(33.7822821109317,-1.08977642115053,340.81765735533));
#18354=CARTESIAN_POINT('Ctrl Pts',(33.7896803783683,-1.24379722362615,340.784539655755));
#18355=CARTESIAN_POINT('Ctrl Pts',(33.7970812448941,-1.39787213522962,340.751410321583));
#18356=CARTESIAN_POINT('Ctrl Pts',(33.8044821114198,-1.55055852755869,340.712134686673));
#18357=CARTESIAN_POINT('Ctrl Pts',(33.8118829779455,-1.70133871379538,340.666866607168));
#18358=CARTESIAN_POINT('Ctrl Pts',(33.8192919713303,-1.85228447109172,340.621548818984));
#18359=CARTESIAN_POINT('Ctrl Pts',(33.8267009647151,-2.00131948440785,340.57022555242));
#18360=CARTESIAN_POINT('Ctrl Pts',(33.8341099580998,-2.14794310387718,340.513099943317));
#18361=CARTESIAN_POINT('Ctrl Pts',(33.8415235156801,-2.29465704855368,340.455939142869));
#18362=CARTESIAN_POINT('Ctrl Pts',(33.8489370732603,-2.43895629806379,340.392969026254));
#18363=CARTESIAN_POINT('Ctrl Pts',(33.8563506308406,-2.58036313086811,340.324439564438));
#18364=CARTESIAN_POINT('Ctrl Pts',(33.8637747429773,-2.72197128218691,340.255812538388));
#18365=CARTESIAN_POINT('Ctrl Pts',(33.871198855114,-2.86067846436568,340.181610535376));
#18366=CARTESIAN_POINT('Ctrl Pts',(33.8786229672507,-2.99603364518518,340.102128277437));
#18367=CARTESIAN_POINT('Ctrl Pts',(33.8824800924053,-3.06635611110962,340.060834044429));
#18368=CARTESIAN_POINT('Ctrl Pts',(33.88633721756,-3.13577429865372,340.018115252062));
#18369=CARTESIAN_POINT('Ctrl Pts',(33.8901943427146,-3.20422842184017,339.974017569648));
#18370=CARTESIAN_POINT('Ctrl Pts',(33.8976176868341,-3.33597382610674,339.88914807273));
#18371=CARTESIAN_POINT('Ctrl Pts',(33.9050410309535,-3.46454394365831,339.798912566336));
#18372=CARTESIAN_POINT('Ctrl Pts',(33.9124643750729,-3.58947148244047,339.703575771607));
#18373=CARTESIAN_POINT('Ctrl Pts',(33.9198789580572,-3.71425157998444,339.608351494704));
#18374=CARTESIAN_POINT('Ctrl Pts',(33.9272935410415,-3.83539736214807,339.508038137807));
#18375=CARTESIAN_POINT('Ctrl Pts',(33.9347081240258,-3.95246841424756,339.402944923216));
#18376=CARTESIAN_POINT('Ctrl Pts',(33.9421155730338,-4.06942682587704,339.297952824562));
#18377=CARTESIAN_POINT('Ctrl Pts',(33.9495230220418,-4.18231803652413,339.188190271556));
#18378=CARTESIAN_POINT('Ctrl Pts',(33.9569304710498,-4.29073287553002,339.074008094413));
#18379=CARTESIAN_POINT('Ctrl Pts',(33.9643324076227,-4.39906703497138,338.959910888741));
#18380=CARTESIAN_POINT('Ctrl Pts',(33.9717343441956,-4.50293119973579,338.841400877276));
#18381=CARTESIAN_POINT('Ctrl Pts',(33.9791362807685,-4.60195149056355,338.718867171734));
#18382=CARTESIAN_POINT('Ctrl Pts',(33.9865343220827,-4.70091967210267,338.596397949382));
#18383=CARTESIAN_POINT('Ctrl Pts',(33.993932363397,-4.79504882231029,338.4699095396));
#18384=CARTESIAN_POINT('Ctrl Pts',(34.0013304047112,-4.88400403846331,338.339825611432));
#18385=CARTESIAN_POINT('Ctrl Pts',(34.0087272285526,-4.97294461553028,338.209763090774));
#18386=CARTESIAN_POINT('Ctrl Pts',(34.0161240523939,-5.0567127378862,338.076106533883));
#18387=CARTESIAN_POINT('Ctrl Pts',(34.0235208762352,-5.13501564008017,337.93931028281));
#18388=CARTESIAN_POINT('Ctrl Pts',(34.0309173824593,-5.21331517997234,337.802519905724));
#18389=CARTESIAN_POINT('Ctrl Pts',(34.0383138886833,-5.28614978086938,337.66259042648));
#18390=CARTESIAN_POINT('Ctrl Pts',(34.0457103949074,-5.35327177774928,337.520002348422));
#18391=CARTESIAN_POINT('Ctrl Pts',(34.0531080437924,-5.420404144077,337.377392242419));
#18392=CARTESIAN_POINT('Ctrl Pts',(34.0605056926775,-5.48182199018751,337.232123057568));
#18393=CARTESIAN_POINT('Ctrl Pts',(34.0679033415625,-5.53732516275085,337.084696765591));
#18394=CARTESIAN_POINT('Ctrl Pts',(34.0753035937919,-5.59284786771878,336.937218592076));
#18395=CARTESIAN_POINT('Ctrl Pts',(34.0827038460213,-5.6424516235287,336.787582149161));
#18396=CARTESIAN_POINT('Ctrl Pts',(34.0901040982507,-5.68598569908107,336.636305959271));
#18397=CARTESIAN_POINT('Ctrl Pts',(34.0975124774253,-5.72956758368598,336.484863638109));
#18398=CARTESIAN_POINT('Ctrl Pts',(34.1049208565999,-5.76706637302287,336.331778332696));
#18399=CARTESIAN_POINT('Ctrl Pts',(34.1123292357745,-5.79838199679146,336.177580902437));
#18400=CARTESIAN_POINT('Ctrl Pts',(34.1197421840418,-5.82971693436465,336.023288371437));
#18401=CARTESIAN_POINT('Ctrl Pts',(34.1271551323091,-5.85486104813616,335.867882716476));
#18402=CARTESIAN_POINT('Ctrl Pts',(34.1345680805764,-5.87376606042453,335.711900856795));
#18403=CARTESIAN_POINT('Ctrl Pts',(34.1419915729434,-5.89269796300362,335.555697130156));
#18404=CARTESIAN_POINT('Ctrl Pts',(34.1494150653104,-5.90537301024448,335.398915932984));
#18405=CARTESIAN_POINT('Ctrl Pts',(34.1568385576774,-5.91179499930531,335.242095949344));
#18406=CARTESIAN_POINT('Ctrl Pts',(34.1606595785391,-5.91510052626779,335.161377548975));
#18407=CARTESIAN_POINT('Ctrl Pts',(34.1644805994007,-5.91675023582117,335.080648829086));
#18408=CARTESIAN_POINT('Ctrl Pts',(34.1683016202624,-5.91674999997471,334.999982700985));
#18409=CARTESIAN_POINT('',(35.9183016044877,-5.91463655468594,335.005215113745));
#18410=CARTESIAN_POINT('Ctrl Pts',(34.1683016202945,-5.91674999997471,334.999982700307));
#18411=CARTESIAN_POINT('Ctrl Pts',(34.1757262328824,-5.9167495416843,334.843240622263));
#18412=CARTESIAN_POINT('Ctrl Pts',(34.1831508454702,-5.91051634278605,334.686262312169));
#18413=CARTESIAN_POINT('Ctrl Pts',(34.1905754580581,-5.89801996188907,334.529584129033));
#18414=CARTESIAN_POINT('Ctrl Pts',(34.1979913089862,-5.88553832775989,334.373090839171));
#18415=CARTESIAN_POINT('Ctrl Pts',(34.2054071599143,-5.86680825310907,334.216897339617));
#18416=CARTESIAN_POINT('Ctrl Pts',(34.2128230108424,-5.8418512629109,334.06154148492));
#18417=CARTESIAN_POINT('Ctrl Pts',(34.2202317260019,-5.81691828712562,333.906335118587));
#18418=CARTESIAN_POINT('Ctrl Pts',(34.2276404411614,-5.78577038304834,333.751965158449));
#18419=CARTESIAN_POINT('Ctrl Pts',(34.235049156321,-5.74848097373168,333.598965718783));
#18420=CARTESIAN_POINT('Ctrl Pts',(34.2424523559939,-5.7112193248611,333.446080180967));
#18421=CARTESIAN_POINT('Ctrl Pts',(34.2498555556667,-5.66782536247198,333.294563493033));
#18422=CARTESIAN_POINT('Ctrl Pts',(34.2572587553396,-5.61842380275774,333.144940827061));
#18423=CARTESIAN_POINT('Ctrl Pts',(34.2646580554474,-5.56904826484596,332.995396973407));
#18424=CARTESIAN_POINT('Ctrl Pts',(34.2720573555553,-5.5136715484983,332.847745508246));
#18425=CARTESIAN_POINT('Ctrl Pts',(34.2794566556631,-5.45246852796488,332.70249754863));
#18426=CARTESIAN_POINT('Ctrl Pts',(34.286854732152,-5.39127562854728,332.557273608603));
#18427=CARTESIAN_POINT('Ctrl Pts',(34.2942528086408,-5.32425848194353,332.414452728791));
#18428=CARTESIAN_POINT('Ctrl Pts',(34.3016508851297,-5.25164056712346,332.274527212346));
#18429=CARTESIAN_POINT('Ctrl Pts',(34.3090486377602,-5.17902583122722,332.134607821284));
#18430=CARTESIAN_POINT('Ctrl Pts',(34.3164463903907,-5.10081098649808,331.997583872765));
#18431=CARTESIAN_POINT('Ctrl Pts',(34.3238441430212,-5.01726592936693,331.863923923672));
#18432=CARTESIAN_POINT('Ctrl Pts',(34.331243030939,-4.93370805109248,331.730243462614));
#18433=CARTESIAN_POINT('Ctrl Pts',(34.3386419188568,-4.84481852946019,331.599928345348));
#18434=CARTESIAN_POINT('Ctrl Pts',(34.3460408067747,-4.75091104020307,331.473418815541));
#18435=CARTESIAN_POINT('Ctrl Pts',(34.3534422895252,-4.65697061704751,331.346864918113));
#18436=CARTESIAN_POINT('Ctrl Pts',(34.3608437722757,-4.55800894469779,331.224119564853));
#18437=CARTESIAN_POINT('Ctrl Pts',(34.3682452550263,-4.45438038023647,331.105590418219));
#18438=CARTESIAN_POINT('Ctrl Pts',(34.3756548645294,-4.35063803266724,330.986931127791));
#18439=CARTESIAN_POINT('Ctrl Pts',(34.3830644740325,-4.24221880538197,330.872497570185));
#18440=CARTESIAN_POINT('Ctrl Pts',(34.3904740835357,-4.12951486858929,330.762661506016));
#18441=CARTESIAN_POINT('Ctrl Pts',(34.3978882523305,-4.01674158264789,330.652757857361));
#18442=CARTESIAN_POINT('Ctrl Pts',(34.4053024211252,-3.89967861042304,330.547457588168));
#18443=CARTESIAN_POINT('Ctrl Pts',(34.41271658992,-3.7787512719973,330.447092205318));
#18444=CARTESIAN_POINT('Ctrl Pts',(34.4201413236992,-3.65765161547493,330.346583804586));
#18445=CARTESIAN_POINT('Ctrl Pts',(34.4275660574785,-3.53267689047145,330.251024560831));
#18446=CARTESIAN_POINT('Ctrl Pts',(34.4349907912577,-3.40428211726297,330.160703167961));
#18447=CARTESIAN_POINT('Ctrl Pts',(34.438883997926,-3.33695749632928,330.11334256764));
#18448=CARTESIAN_POINT('Ctrl Pts',(34.4427772045943,-3.26869296821449,330.067421359335));
#18449=CARTESIAN_POINT('Ctrl Pts',(34.4466704112625,-3.19955672855037,330.022976059603));
#18450=CARTESIAN_POINT('Ctrl Pts',(34.4540943887005,-3.06772044880581,329.938223070472));
#18451=CARTESIAN_POINT('Ctrl Pts',(34.4615183661385,-2.93231543183702,329.858584157325));
#18452=CARTESIAN_POINT('Ctrl Pts',(34.4689423435766,-2.79377629797551,329.784374959857));
#18453=CARTESIAN_POINT('Ctrl Pts',(34.4763575596042,-2.65540066113629,329.710253340407));
#18454=CARTESIAN_POINT('Ctrl Pts',(34.4837727756319,-2.51389859557135,329.641548856155));
#18455=CARTESIAN_POINT('Ctrl Pts',(34.4911879916595,-2.3697340849914,329.578534245342));
#18456=CARTESIAN_POINT('Ctrl Pts',(34.4985960728037,-2.22570828877776,329.51558026687));
#18457=CARTESIAN_POINT('Ctrl Pts',(34.5060041539477,-2.07902548728249,329.458305411071));
#18458=CARTESIAN_POINT('Ctrl Pts',(34.5134122350919,-1.93017458584001,329.406936739972));
#18459=CARTESIAN_POINT('Ctrl Pts',(34.5208148022659,-1.78143447684204,329.355606303512));
#18460=CARTESIAN_POINT('Ctrl Pts',(34.52821736944,-1.63052983240379,329.310173419742));
#18461=CARTESIAN_POINT('Ctrl Pts',(34.535619936614,-1.4779697758931,329.270817169609));
#18462=CARTESIAN_POINT('Ctrl Pts',(34.5430186063688,-1.32549004158496,329.231481640369));
#18463=CARTESIAN_POINT('Ctrl Pts',(34.5504172761236,-1.17135699145214,329.19821646612));
#18464=CARTESIAN_POINT('Ctrl Pts',(34.5578159458784,-1.01609505146479,329.171150936172));
#18465=CARTESIAN_POINT('Ctrl Pts',(34.5652133950824,-0.860858724876622,
329.144089871196));
#18466=CARTESIAN_POINT('Ctrl Pts',(34.5726108442863,-0.704494245353079,
329.123226484724));
#18467=CARTESIAN_POINT('Ctrl Pts',(34.5800082934903,-0.547536497570136,
329.108639007298));
#18468=CARTESIAN_POINT('Ctrl Pts',(34.5874054219538,-0.3905855552015,329.09405216236));
#18469=CARTESIAN_POINT('Ctrl Pts',(34.5948025504173,-0.23304176732925,329.085740719956));
#18470=CARTESIAN_POINT('Ctrl Pts',(34.6021996788808,-0.0754451444839536,
329.083731024313));
#18471=CARTESIAN_POINT('Ctrl Pts',(34.6095979463175,0.0821757443071198,
329.081721019228));
#18472=CARTESIAN_POINT('Ctrl Pts',(34.6169962137541,0.239849111065977,329.086014697681));
#18473=CARTESIAN_POINT('Ctrl Pts',(34.6243944811907,0.397035088618084,329.096586267175));
#18474=CARTESIAN_POINT('Ctrl Pts',(34.6317953477165,0.55427628725711,329.107161550572));
#18475=CARTESIAN_POINT('Ctrl Pts',(34.6391962142422,0.711029383645316,329.124019091107));
#18476=CARTESIAN_POINT('Ctrl Pts',(34.646597080768,0.866759920317203,329.14708125778));
#18477=CARTESIAN_POINT('Ctrl Pts',(34.6540060741528,1.02266146400678,329.170168748917));
#18478=CARTESIAN_POINT('Ctrl Pts',(34.6614150675375,1.17753783614681,329.199474417956));
#18479=CARTESIAN_POINT('Ctrl Pts',(34.6688240609223,1.33086433522249,329.234869413124));
#18480=CARTESIAN_POINT('Ctrl Pts',(34.6762376185026,1.48428528871039,329.27028621283));
#18481=CARTESIAN_POINT('Ctrl Pts',(34.6836511760828,1.63615410745543,329.311799715318));
#18482=CARTESIAN_POINT('Ctrl Pts',(34.6910647336631,1.78596202810581,329.359231417913));
#18483=CARTESIAN_POINT('Ctrl Pts',(34.6984888457998,1.93598322775725,329.406730648219));
#18484=CARTESIAN_POINT('Ctrl Pts',(34.7059129579365,2.083937319324,329.460164779894));
#18485=CARTESIAN_POINT('Ctrl Pts',(34.7133370700733,2.22933549972864,329.519307179548));
#18486=CARTESIAN_POINT('Ctrl Pts',(34.7171941952277,2.30487570827037,329.550034037279));
#18487=CARTESIAN_POINT('Ctrl Pts',(34.7210513203821,2.37972641491085,329.582300919648));
#18488=CARTESIAN_POINT('Ctrl Pts',(34.7249084455365,2.4538218752867,329.616071251691));
#18489=CARTESIAN_POINT('Ctrl Pts',(34.7323324229745,2.59643664770587,329.681070486388));
#18490=CARTESIAN_POINT('Ctrl Pts',(34.7397564004125,2.73668213301252,329.751838268312));
#18491=CARTESIAN_POINT('Ctrl Pts',(34.7471803778505,2.87405770505323,329.828179926706));
#18492=CARTESIAN_POINT('Ctrl Pts',(34.7545955938781,3.01127115324966,329.904431490457));
#18493=CARTESIAN_POINT('Ctrl Pts',(34.7620108099058,3.14562110686627,329.986243657513));
#18494=CARTESIAN_POINT('Ctrl Pts',(34.7694260259334,3.27662712628925,330.073373848386));
#18495=CARTESIAN_POINT('Ctrl Pts',(34.7768341070775,3.40750709238005,330.160420203028));
#18496=CARTESIAN_POINT('Ctrl Pts',(34.7842421882216,3.53504922107281,330.252774189242));
#18497=CARTESIAN_POINT('Ctrl Pts',(34.7916502693657,3.65879799633629,330.350147552394));
#18498=CARTESIAN_POINT('Ctrl Pts',(34.7990528365397,3.78245466312607,330.447448438773));
#18499=CARTESIAN_POINT('Ctrl Pts',(34.8064554037137,3.90232330636831,330.549761033344));
#18500=CARTESIAN_POINT('Ctrl Pts',(34.8138579708877,4.01797781720591,330.656754114382));
#18501=CARTESIAN_POINT('Ctrl Pts',(34.8212566406425,4.13357143644902,330.763690864029));
#18502=CARTESIAN_POINT('Ctrl Pts',(34.8286553103972,4.2449550687353,330.875302939628));
#18503=CARTESIAN_POINT('Ctrl Pts',(34.8360539801519,4.3517361949416,330.991219306056));
#18504=CARTESIAN_POINT('Ctrl Pts',(34.8434514293559,4.45849970557797,331.107116549883));
#18505=CARTESIAN_POINT('Ctrl Pts',(34.8508488785599,4.56066196442487,331.227316401044));
#18506=CARTESIAN_POINT('Ctrl Pts',(34.8582463277639,4.65786772896121,331.351411398636));
#18507=CARTESIAN_POINT('Ctrl Pts',(34.8656434562274,4.75506927882492,331.475501015686));
#18508=CARTESIAN_POINT('Ctrl Pts',(34.8730405846908,4.84731453153763,331.603485149561));
#18509=CARTESIAN_POINT('Ctrl Pts',(34.8804377131543,4.93428910299219,331.734923950259));
#18510=CARTESIAN_POINT('Ctrl Pts',(34.8878359805909,5.0212770663597,331.866382989251));
#18511=CARTESIAN_POINT('Ctrl Pts',(34.8952342480275,5.10299252659552,332.001297442955));
#18512=CARTESIAN_POINT('Ctrl Pts',(34.9026325154641,5.17916502005664,332.139199367743));
#18513=CARTESIAN_POINT('Ctrl Pts',(34.9100333819899,5.25536427371587,332.277149738928));
#18514=CARTESIAN_POINT('Ctrl Pts',(34.9174342485157,5.32601650318714,332.41808934433));
#18515=CARTESIAN_POINT('Ctrl Pts',(34.9248351150414,5.39089776443169,332.561526736676));
#18516=CARTESIAN_POINT('Ctrl Pts',(34.9322441084262,5.45585027150397,332.705121636992));
#18517=CARTESIAN_POINT('Ctrl Pts',(34.939653101811,5.51501900096914,332.851219461543));
#18518=CARTESIAN_POINT('Ctrl Pts',(34.9470620951958,5.56822836093612,332.999309248543));
#18519=CARTESIAN_POINT('Ctrl Pts',(34.954475652776,5.62147049970415,333.147490263959));
#18520=CARTESIAN_POINT('Ctrl Pts',(34.9618892103563,5.66874584186422,333.297665331861));
#18521=CARTESIAN_POINT('Ctrl Pts',(34.9693027679365,5.70992917308212,333.449310024252));
#18522=CARTESIAN_POINT('Ctrl Pts',(34.9767268800732,5.75117113631163,333.601170610625));
#18523=CARTESIAN_POINT('Ctrl Pts',(34.9841509922099,5.78630368357058,333.754504637383));
#18524=CARTESIAN_POINT('Ctrl Pts',(34.9915751043466,5.81525287631618,333.908778415263));
#18525=CARTESIAN_POINT('Ctrl Pts',(34.9954322295012,5.83029314746079,333.988929854033));
#18526=CARTESIAN_POINT('Ctrl Pts',(34.9992893546558,5.84366524998968,334.069334871644));
#18527=CARTESIAN_POINT('Ctrl Pts',(35.0031464798104,5.85536436252227,334.149918389445));
#18528=CARTESIAN_POINT('Ctrl Pts',(35.0105704572484,5.87788215595793,334.305021009674));
#18529=CARTESIAN_POINT('Ctrl Pts',(35.0179944346864,5.89426689775692,334.461252937728));
#18530=CARTESIAN_POINT('Ctrl Pts',(35.0254184121243,5.90441137317563,334.618087838876));
#18531=CARTESIAN_POINT('Ctrl Pts',(35.032833628152,5.91454387658704,334.774737651244));
#18532=CARTESIAN_POINT('Ctrl Pts',(35.0402488441796,5.91845074882391,334.931988651446));
#18533=CARTESIAN_POINT('Ctrl Pts',(35.0476640602072,5.91607598671165,335.08930555388));
#18534=CARTESIAN_POINT('Ctrl Pts',(35.0550721413513,5.91370350958354,335.246471086782));
#18535=CARTESIAN_POINT('Ctrl Pts',(35.0624802224953,5.90506143649155,335.403702025002));
#18536=CARTESIAN_POINT('Ctrl Pts',(35.0698883036394,5.89014566104608,335.560459324269));
#18537=CARTESIAN_POINT('Ctrl Pts',(35.0772908708134,5.8752409876847,335.717099946215));
#18538=CARTESIAN_POINT('Ctrl Pts',(35.0846934379874,5.85407194508644,335.87326726122));
#18539=CARTESIAN_POINT('Ctrl Pts',(35.0920960051614,5.82668647271372,336.028423702175));
#18540=CARTESIAN_POINT('Ctrl Pts',(35.0994946749162,5.79931541867251,336.183498453942));
#18541=CARTESIAN_POINT('Ctrl Pts',(35.1068933446709,5.76573451778398,336.337563025003));
#18542=CARTESIAN_POINT('Ctrl Pts',(35.1142920144256,5.72604336677771,336.490086549258));
#18543=CARTESIAN_POINT('Ctrl Pts',(35.1216894636295,5.68635876357889,336.642584911869));
#18544=CARTESIAN_POINT('Ctrl Pts',(35.1290869128335,5.64056600471861,336.793542371398));
#18545=CARTESIAN_POINT('Ctrl Pts',(35.1364843620374,5.58881549064892,336.942439696357));
#18546=CARTESIAN_POINT('Ctrl Pts',(35.1438814905009,5.53706722039129,337.091330565387));
#18547=CARTESIAN_POINT('Ctrl Pts',(35.1512786189643,5.47936183106871,337.238161124927));
#18548=CARTESIAN_POINT('Ctrl Pts',(35.1586757474278,5.41589907065227,337.382428974599));
#18549=CARTESIAN_POINT('Ctrl Pts',(35.1660740148644,5.35242653855487,337.526719037918));
#18550=CARTESIAN_POINT('Ctrl Pts',(35.173472282301,5.28319502052826,337.668445264042));
#18551=CARTESIAN_POINT('Ctrl Pts',(35.1808705497376,5.20845165695409,337.807126983176));
#18552=CARTESIAN_POINT('Ctrl Pts',(35.1882714162633,5.13368203525028,337.945857422656));
#18553=CARTESIAN_POINT('Ctrl Pts',(35.1956722827891,5.05339688964474,338.081540897313));
#18554=CARTESIAN_POINT('Ctrl Pts',(35.2030731493149,4.96788829966441,338.213723137509));
#18555=CARTESIAN_POINT('Ctrl Pts',(35.2104821426996,4.88228581307733,338.346050526441));
#18556=CARTESIAN_POINT('Ctrl Pts',(35.2178911360843,4.79144863016722,338.474868689313));
#18557=CARTESIAN_POINT('Ctrl Pts',(35.225300129469,4.69571140675345,338.599753456417));
#18558=CARTESIAN_POINT('Ctrl Pts',(35.2327136870493,4.59991520590759,338.724715156845));
#18559=CARTESIAN_POINT('Ctrl Pts',(35.2401272446295,4.499213187766,338.845738346928));
#18560=CARTESIAN_POINT('Ctrl Pts',(35.2475408022098,4.39397859435842,338.96243393318));
#18561=CARTESIAN_POINT('Ctrl Pts',(35.2549649143464,4.2885941802415,339.079295656964));
#18562=CARTESIAN_POINT('Ctrl Pts',(35.2623890264831,4.1786645631295,339.191817205658));
#18563=CARTESIAN_POINT('Ctrl Pts',(35.2698131386198,4.06459852132363,339.299647592879));
#18564=CARTESIAN_POINT('Ctrl Pts',(35.2736702637746,4.00533662022828,339.355669820367));
#18565=CARTESIAN_POINT('Ctrl Pts',(35.2775273889295,3.94495873751914,339.410426475336));
#18566=CARTESIAN_POINT('Ctrl Pts',(35.2813845140844,3.88352539930828,339.463872874022));
#18567=CARTESIAN_POINT('Ctrl Pts',(35.2888084915224,3.7652819670866,339.566743494511));
#18568=CARTESIAN_POINT('Ctrl Pts',(35.2962324689603,3.64276992966733,339.665067834299));
#18569=CARTESIAN_POINT('Ctrl Pts',(35.3036564463983,3.51637387310443,339.758470904298));
#18570=CARTESIAN_POINT('Ctrl Pts',(35.311071662426,3.39012698290558,339.851763744621));
#18571=CARTESIAN_POINT('Ctrl Pts',(35.3184868784536,3.26000549477615,339.940146656104));
#18572=CARTESIAN_POINT('Ctrl Pts',(35.3259020944813,3.12642923526749,340.02328287073));
#18573=CARTESIAN_POINT('Ctrl Pts',(35.3333101756254,2.99298150216326,340.106339092108));
#18574=CARTESIAN_POINT('Ctrl Pts',(35.3407182567695,2.85608593020623,340.184158471055));
#18575=CARTESIAN_POINT('Ctrl Pts',(35.3481263379136,2.71619359102158,340.256445846634));
#18576=CARTESIAN_POINT('Ctrl Pts',(35.3555289050876,2.57640537625973,340.328679417399));
#18577=CARTESIAN_POINT('Ctrl Pts',(35.3629314722616,2.43362516575836,340.395389012884));
#18578=CARTESIAN_POINT('Ctrl Pts',(35.3703340394356,2.28833095396235,340.456324037998));
#18579=CARTESIAN_POINT('Ctrl Pts',(35.3777327091904,2.14311323893425,340.517226981088));
#18580=CARTESIAN_POINT('Ctrl Pts',(35.3851313789451,1.99538450196292,340.572361264737));
#18581=CARTESIAN_POINT('Ctrl Pts',(35.3925300486998,1.84564505718196,340.621523359855));
#18582=CARTESIAN_POINT('Ctrl Pts',(35.3999274979038,1.69593031475931,340.670677344754));
#18583=CARTESIAN_POINT('Ctrl Pts',(35.4073249471078,1.54420587709747,340.713860980171));
#18584=CARTESIAN_POINT('Ctrl Pts',(35.4147223963118,1.39098976734667,340.750919755103));
#18585=CARTESIAN_POINT('Ctrl Pts',(35.4221195247753,1.23778030077949,340.787976923231));
#18586=CARTESIAN_POINT('Ctrl Pts',(35.4295166532388,1.08307965347235,340.818909671162));
#18587=CARTESIAN_POINT('Ctrl Pts',(35.4369137817022,0.927418399709803,340.843614093554));
#18588=CARTESIAN_POINT('Ctrl Pts',(35.4443120491388,0.771733177999778,340.86832231981));
#18589=CARTESIAN_POINT('Ctrl Pts',(35.4517103165754,0.615087423947733,340.886800252516));
#18590=CARTESIAN_POINT('Ctrl Pts',(35.459108584012,0.458019084879539,340.898995599285));
#18591=CARTESIAN_POINT('Ctrl Pts',(35.4665094505378,0.300895566052063,340.911195230408));
#18592=CARTESIAN_POINT('Ctrl Pts',(35.4739103170636,0.143349538484667,340.917107852313));
#18593=CARTESIAN_POINT('Ctrl Pts',(35.4813111835893,-0.0140789318007903,
340.916733249537));
#18594=CARTESIAN_POINT('Ctrl Pts',(35.4887201769741,-0.1716802735976,340.916358235412));
#18595=CARTESIAN_POINT('Ctrl Pts',(35.4961291703589,-0.329163426881736,
340.909682209891));
#18596=CARTESIAN_POINT('Ctrl Pts',(35.5035381637436,-0.485990596829314,
340.896757049624));
#18597=CARTESIAN_POINT('Ctrl Pts',(35.5109517213239,-0.642914377722902,
340.883823927013));
#18598=CARTESIAN_POINT('Ctrl Pts',(35.5183652789041,-0.799181000477436,
340.864634044037));
#18599=CARTESIAN_POINT('Ctrl Pts',(35.5257788364844,-0.954261285400897,
340.839290707071));
#18600=CARTESIAN_POINT('Ctrl Pts',(35.5332029486211,-1.10956235550119,340.813911289225));
#18601=CARTESIAN_POINT('Ctrl Pts',(35.5406270607577,-1.26367334991961,340.782360995433));
#18602=CARTESIAN_POINT('Ctrl Pts',(35.5480511728944,-1.41607790332439,340.744793637218));
#18603=CARTESIAN_POINT('Ctrl Pts',(35.551908298049,-1.49525820472476,340.725275882138));
#18604=CARTESIAN_POINT('Ctrl Pts',(35.5557654232037,-1.57397818088169,340.704134800404));
#18605=CARTESIAN_POINT('Ctrl Pts',(35.5596225483583,-1.65216750211017,340.681397108764));
#18606=CARTESIAN_POINT('Ctrl Pts',(35.5670465257963,-1.80266190750961,340.637632879457));
#18607=CARTESIAN_POINT('Ctrl Pts',(35.5744705032343,-1.95164323568219,340.587818835621));
#18608=CARTESIAN_POINT('Ctrl Pts',(35.5818944806723,-2.09858802872165,340.532075455759));
#18609=CARTESIAN_POINT('Ctrl Pts',(35.5893096966999,-2.24535940479629,340.476397861472));
#18610=CARTESIAN_POINT('Ctrl Pts',(35.5967249127276,-2.39009868422559,340.414804990898));
#18611=CARTESIAN_POINT('Ctrl Pts',(35.6041401287552,-2.53229547936181,340.347467640641));
#18612=CARTESIAN_POINT('Ctrl Pts',(35.6115482098993,-2.67435545345782,340.280195082044));
#18613=CARTESIAN_POINT('Ctrl Pts',(35.6189562910435,-2.81387747847031,340.207189206269));
#18614=CARTESIAN_POINT('Ctrl Pts',(35.6263643721876,-2.95036924653195,340.128669600551));
#18615=CARTESIAN_POINT('Ctrl Pts',(35.6337669393616,-3.08675942127778,340.05020843841));
#18616=CARTESIAN_POINT('Ctrl Pts',(35.6411695065356,-3.22012350793736,339.96624190323));
#18617=CARTESIAN_POINT('Ctrl Pts',(35.6485720737096,-3.34999210553022,339.877036339355));
#18618=CARTESIAN_POINT('Ctrl Pts',(35.6559707434644,-3.47979232787402,339.787877741819));
#18619=CARTESIAN_POINT('Ctrl Pts',(35.6633694132191,-3.60610041948226,339.693485819732));
#18620=CARTESIAN_POINT('Ctrl Pts',(35.6707680829739,-3.72847447971309,339.594171156654));
#18621=CARTESIAN_POINT('Ctrl Pts',(35.6781655321779,-3.85082835202389,339.49487287741));
#18622=CARTESIAN_POINT('Ctrl Pts',(35.6855629813819,-3.96924919149363,339.390653703882));
#18623=CARTESIAN_POINT('Ctrl Pts',(35.6929604305859,-4.08332673447283,339.281865638018));
#18624=CARTESIAN_POINT('Ctrl Pts',(35.7003575590493,-4.19739933124848,339.173082289015));
#18625=CARTESIAN_POINT('Ctrl Pts',(35.7077546875128,-4.3071287358838,339.059730699127));
#18626=CARTESIAN_POINT('Ctrl Pts',(35.7151518159763,-4.41214044797045,338.942200810446));
#18627=CARTESIAN_POINT('Ctrl Pts',(35.7225500834129,-4.51716832923962,338.824652825096));
#18628=CARTESIAN_POINT('Ctrl Pts',(35.7299483508495,-4.61747682291074,338.702925538274));
#18629=CARTESIAN_POINT('Ctrl Pts',(35.7373466182861,-4.71273084103459,338.577443022951));
#18630=CARTESIAN_POINT('Ctrl Pts',(35.7447474848119,-4.80801832289658,338.451916424301));
#18631=CARTESIAN_POINT('Ctrl Pts',(35.7521483513377,-4.89824756830224,338.322632267601));
#18632=CARTESIAN_POINT('Ctrl Pts',(35.7595492178634,-4.98312613535172,338.190044589293));
#18633=CARTESIAN_POINT('Ctrl Pts',(35.7669582112482,-5.06809790718252,338.057311317037));
#18634=CARTESIAN_POINT('Ctrl Pts',(35.7743672046329,-5.14770706551855,337.921267593205));
#18635=CARTESIAN_POINT('Ctrl Pts',(35.7817761980177,-5.22170620290343,337.78239373437));
#18636=CARTESIAN_POINT('Ctrl Pts',(35.7891897555979,-5.29575092630956,337.643434324447));
#18637=CARTESIAN_POINT('Ctrl Pts',(35.7966033131782,-5.3641785804664,337.501641640776));
#18638=CARTESIAN_POINT('Ctrl Pts',(35.8040168707585,-5.42678966841234,337.357516586859));
#18639=CARTESIAN_POINT('Ctrl Pts',(35.8114409828952,-5.48948989470437,337.213186344541));
#18640=CARTESIAN_POINT('Ctrl Pts',(35.8188650950318,-5.54635688152531,337.066517447194));
#18641=CARTESIAN_POINT('Ctrl Pts',(35.8262892071685,-5.59724053735629,336.918027353683));
#18642=CARTESIAN_POINT('Ctrl Pts',(35.8301463323231,-5.62367664516925,336.840880771797));
#18643=CARTESIAN_POINT('Ctrl Pts',(35.8340034574776,-5.64849855456325,336.763242812029));
#18644=CARTESIAN_POINT('Ctrl Pts',(35.8378605826322,-5.67169067279419,336.685187074078));
#18645=CARTESIAN_POINT('Ctrl Pts',(35.8470348007207,-5.72685340204471,336.499530572323));
#18646=CARTESIAN_POINT('Ctrl Pts',(35.8562090188092,-5.77292764653191,336.311058344617));
#18647=CARTESIAN_POINT('Ctrl Pts',(35.8653832368978,-5.80966959513859,336.120566712794));
#18648=CARTESIAN_POINT('Ctrl Pts',(35.8744336397492,-5.84591567444786,335.932645955822));
#18649=CARTESIAN_POINT('Ctrl Pts',(35.8834840426007,-5.87307965956882,335.742759892796));
#18650=CARTESIAN_POINT('Ctrl Pts',(35.8925344454522,-5.89097312716808,335.551693916482));
#18651=CARTESIAN_POINT('Ctrl Pts',(35.9011234889216,-5.90795444540889,335.370367847023));
#18652=CARTESIAN_POINT('Ctrl Pts',(35.9097125323909,-5.91658653424087,335.187979188446));
#18653=CARTESIAN_POINT('Ctrl Pts',(35.9183015758603,-5.91674769948109,335.005217584232));
#18654=CARTESIAN_POINT('',(37.6683016202945,-5.907956964761,334.997521372297));
#18655=CARTESIAN_POINT('Ctrl Pts',(35.9183016202945,-5.91347087048126,335.005213749647));
#18656=CARTESIAN_POINT('Ctrl Pts',(35.9842339524984,-5.9016480507818,333.603040816822));
#18657=CARTESIAN_POINT('Ctrl Pts',(36.1429122961271,-4.70094670253729,330.210249656623));
#18658=CARTESIAN_POINT('Ctrl Pts',(36.3943366511801,0.96493722398234,328.070243938278));
#18659=CARTESIAN_POINT('Ctrl Pts',(36.672574685454,6.34956261214914,332.061347663363));
#18660=CARTESIAN_POINT('Ctrl Pts',(36.9508127197281,5.90728811053532,338.749209263345));
#18661=CARTESIAN_POINT('Ctrl Pts',(37.2290507540018,0.043982501314167,341.996476860591));
#18662=CARTESIAN_POINT('Ctrl Pts',(37.4682137208575,-5.03058858133461,339.268830814406));
#18663=CARTESIAN_POINT('Ctrl Pts',(37.6146306762883,-5.9036517049508,336.141614378199));
#18664=CARTESIAN_POINT('Ctrl Pts',(37.6683016202945,-5.907956964761,334.997521372297));
#18665=CARTESIAN_POINT('',(39.4183016202944,-5.92257269867875,334.995813786999));
#18666=CARTESIAN_POINT('Ctrl Pts',(37.6683016202945,-5.907956964761,334.997521372297));
#18667=CARTESIAN_POINT('Ctrl Pts',(37.7073766877129,-5.91109140408291,334.164565810094));
#18668=CARTESIAN_POINT('Ctrl Pts',(37.8391977665561,-5.35709580127298,331.358543580458));
#18669=CARTESIAN_POINT('Ctrl Pts',(38.0637648568237,-1.05198365643141,328.082923066223));
#18670=CARTESIAN_POINT('Ctrl Pts',(38.3420028910976,5.24742884367505,330.372137269561));
#18671=CARTESIAN_POINT('Ctrl Pts',(38.6202409253717,6.73135334586379,336.908272793485));
#18672=CARTESIAN_POINT('Ctrl Pts',(38.8984789596455,2.03801423716468,341.693214540886));
#18673=CARTESIAN_POINT('Ctrl Pts',(39.1644991912865,-4.23736427179148,340.395493932002));
#18674=CARTESIAN_POINT('Ctrl Pts',(39.3377734115028,-5.90889301881075,336.701643735705));
#18675=CARTESIAN_POINT('Ctrl Pts',(39.4183016202944,-5.92257269867875,334.995813786999));
#18676=CARTESIAN_POINT('',(41.1683016202944,-5.92116599764251,335.0047121213));
#18677=CARTESIAN_POINT('Ctrl Pts',(39.4183016202944,-5.92257269867875,334.995813786999));
#18678=CARTESIAN_POINT('Ctrl Pts',(39.4305194229274,-5.9246481903756,334.737003936992));
#18679=CARTESIAN_POINT('Ctrl Pts',(39.5354832369853,-5.79155819114906,332.515703125699));
#18680=CARTESIAN_POINT('Ctrl Pts',(39.7331930624671,-2.98148109258298,328.67043497421));
#18681=CARTESIAN_POINT('Ctrl Pts',(40.0114310967413,3.70921576899493,329.067518116311));
#18682=CARTESIAN_POINT('Ctrl Pts',(40.2896691310152,6.99602006730123,334.908752319798));
#18683=CARTESIAN_POINT('Ctrl Pts',(40.5679071652891,3.86268001093083,340.833723172585));
#18684=CARTESIAN_POINT('Ctrl Pts',(40.8461451995632,-2.81538447840677,341.405172375509));
#18685=CARTESIAN_POINT('Ctrl Pts',(41.0462766845649,-5.76043079342616,337.58831708874));
#18686=CARTESIAN_POINT('Ctrl Pts',(41.153662158142,-5.92386532355179,335.315011839286));
#18687=CARTESIAN_POINT('Ctrl Pts',(41.1683016202944,-5.92116599764251,335.0047121213));
#18688=CARTESIAN_POINT('',(42.9183016202944,-5.90741276477635,335.001689847821));
#18689=CARTESIAN_POINT('Ctrl Pts',(41.1683016202944,-5.92116599764251,335.0047121213));
#18690=CARTESIAN_POINT('Ctrl Pts',(41.2464081695666,-5.90676416853575,333.349156749142));
#18691=CARTESIAN_POINT('Ctrl Pts',(41.4172607302634,-4.31984453201313,329.703557399639));
#18692=CARTESIAN_POINT('Ctrl Pts',(41.6808593023849,1.86275416207226,328.255908522793));
#18693=CARTESIAN_POINT('Ctrl Pts',(41.9590973366588,6.67929356397152,332.916814840802));
#18694=CARTESIAN_POINT('Ctrl Pts',(42.2373353709327,5.36634384842577,339.489429431639));
#18695=CARTESIAN_POINT('Ctrl Pts',(42.5155734052068,-0.871220409715002,
341.942160896935));
#18696=CARTESIAN_POINT('Ctrl Pts',(42.742562154994,-5.30763049058483,338.745836565463));
#18697=CARTESIAN_POINT('Ctrl Pts',(42.8768048933565,-5.90967030800872,335.886470939726));
#18698=CARTESIAN_POINT('Ctrl Pts',(42.9183016202944,-5.90741276477635,335.001689847821));
#18699=CARTESIAN_POINT('',(44.6683016202944,-5.91495147643108,334.99459846622));
#18700=CARTESIAN_POINT('Ctrl Pts',(42.9183016202944,-5.90741276477635,335.001689847821));
#18701=CARTESIAN_POINT('Ctrl Pts',(42.9695509047812,-5.90462465390847,333.908967572269));
#18702=CARTESIAN_POINT('Ctrl Pts',(43.1135462006923,-5.08956830760904,330.834875226341));
#18703=CARTESIAN_POINT('Ctrl Pts',(43.3502875080286,-0.138508694537335,
328.004756025501));
#18704=CARTESIAN_POINT('Ctrl Pts',(43.6285255423024,5.80749489289954,331.097997182194));
#18705=CARTESIAN_POINT('Ctrl Pts',(43.9067635765764,6.42404613560693,337.772048731321));
#18706=CARTESIAN_POINT('Ctrl Pts',(44.1850016108504,1.14534505843243,341.902232075086));
#18707=CARTESIAN_POINT('Ctrl Pts',(44.4388476254232,-4.62951679538216,339.891545450806));
#18708=CARTESIAN_POINT('Ctrl Pts',(44.5999476285711,-5.90200285453643,336.447349225365));
#18709=CARTESIAN_POINT('Ctrl Pts',(44.6683016202944,-5.91495147643108,334.99459846622));
#18710=CARTESIAN_POINT('',(46.4183016202944,-5.92630438040088,335.000973658267));
#18711=CARTESIAN_POINT('Ctrl Pts',(44.6683016202944,-5.91495147643108,334.99459846622));
#18712=CARTESIAN_POINT('Ctrl Pts',(44.6926936399957,-5.91957217278538,334.476186530872));
#18713=CARTESIAN_POINT('Ctrl Pts',(44.8098316711211,-5.61950938738174,331.991874660925));
#18714=CARTESIAN_POINT('Ctrl Pts',(45.0197157136725,-2.12826100431989,328.334932257004));
#18715=CARTESIAN_POINT('Ctrl Pts',(45.297953747946,4.45307350904086,329.60344931977));
#18716=CARTESIAN_POINT('Ctrl Pts',(45.5761917822201,6.94788819041166,335.824301288824));
#18717=CARTESIAN_POINT('Ctrl Pts',(45.8544298164939,3.06672843010346,341.288704131791));
#18718=CARTESIAN_POINT('Ctrl Pts',(46.132667850768,-3.62872274567329,340.982056014135));
#18719=CARTESIAN_POINT('Ctrl Pts',(46.3206251187015,-5.90215834541804,337.066504608215));
#18720=CARTESIAN_POINT('Ctrl Pts',(46.4158363752102,-5.92642313844046,335.05310819842));
#18721=CARTESIAN_POINT('Ctrl Pts',(46.4183016202944,-5.92630438040088,335.000973658267));
#18722=CARTESIAN_POINT('',(48.1683016202945,-5.91203636053623,335.004879585725));
#18723=CARTESIAN_POINT('Ctrl Pts',(46.4183016202944,-5.92630438040088,335.000973658267));
#18724=CARTESIAN_POINT('Ctrl Pts',(46.5085823866349,-5.92195529280249,333.091732963305));
#18725=CARTESIAN_POINT('Ctrl Pts',(46.6916091644001,-3.88205234854485,329.213136309643));
#18726=CARTESIAN_POINT('Ctrl Pts',(46.9673819535897,2.72858646747409,328.557373298822));
#18727=CARTESIAN_POINT('Ctrl Pts',(47.2456199878637,6.89433694424205,333.808051586487));
#18728=CARTESIAN_POINT('Ctrl Pts',(47.5238580221377,4.73325616752653,340.152563340105));
#18729=CARTESIAN_POINT('Ctrl Pts',(47.8020960564115,-1.77146393138185,341.768643768218));
#18730=CARTESIAN_POINT('Ctrl Pts',(48.0169105891306,-5.53836790729106,338.220747892415));
#18731=CARTESIAN_POINT('Ctrl Pts',(48.1389791104248,-5.91687241535322,335.628859529147));
#18732=CARTESIAN_POINT('Ctrl Pts',(48.1683016202945,-5.91203636053623,335.004879585725));
#18733=CARTESIAN_POINT('',(49.9183016202945,-5.90873410525529,334.99676686743));
#18734=CARTESIAN_POINT('Ctrl Pts',(48.1683016202945,-5.91203636053623,335.004879585725));
#18735=CARTESIAN_POINT('Ctrl Pts',(48.2317251218495,-5.90157615329038,333.655234105586));
#18736=CARTESIAN_POINT('Ctrl Pts',(48.3878946348288,-4.77270907439321,330.316143069235));
#18737=CARTESIAN_POINT('Ctrl Pts',(48.6368101592334,0.77734454668611,328.046701618874));
#18738=CARTESIAN_POINT('Ctrl Pts',(48.9150481935072,6.26784268903641,331.890856879023));
#18739=CARTESIAN_POINT('Ctrl Pts',(49.1932862277813,6.00643410886364,338.588226890415));
#18740=CARTESIAN_POINT('Ctrl Pts',(49.4715242620551,0.233009601809311,341.992734046616));
#18741=CARTESIAN_POINT('Ctrl Pts',(49.7131960595596,-4.9673952784858,339.376033223979));
#18742=CARTESIAN_POINT('Ctrl Pts',(49.8621218456393,-5.90281046865438,336.193946273827));
#18743=CARTESIAN_POINT('Ctrl Pts',(49.9183016202945,-5.90873410525529,334.99676686743));
#18744=CARTESIAN_POINT('',(51.6683016202944,-5.92387939532596,334.996491143367));
#18745=CARTESIAN_POINT('Ctrl Pts',(49.9183016202945,-5.90873410525529,334.99676686743));
#18746=CARTESIAN_POINT('Ctrl Pts',(49.954867857064,-5.91258967605129,334.217547906538));
#18747=CARTESIAN_POINT('Ctrl Pts',(50.084180105258,-5.40644147763003,331.466739609232));
#18748=CARTESIAN_POINT('Ctrl Pts',(50.306238364877,-1.23849736786919,328.113872845278));
#18749=CARTESIAN_POINT('Ctrl Pts',(50.5844763991509,5.12046924276799,330.232042611864));
#18750=CARTESIAN_POINT('Ctrl Pts',(50.8627144334248,6.78045680731883,336.725696498605));
#18751=CARTESIAN_POINT('Ctrl Pts',(51.140952467699,2.21811923917046,341.635704179819));
#18752=CARTESIAN_POINT('Ctrl Pts',(51.4094815299885,-4.14952426205602,340.497381424821));
#18753=CARTESIAN_POINT('Ctrl Pts',(51.5852645808539,-5.91154402679634,336.754449414842));
#18754=CARTESIAN_POINT('Ctrl Pts',(51.6683016202944,-5.92387939532596,334.996491143367));
#18755=CARTESIAN_POINT('',(53.4183016202944,-5.91960720730597,335.0051128859));
#18756=CARTESIAN_POINT('Ctrl Pts',(51.6683016202944,-5.92387939532596,334.996491143367));
#18757=CARTESIAN_POINT('Ctrl Pts',(51.6780105922785,-5.92532168840715,334.790944706235));
#18758=CARTESIAN_POINT('Ctrl Pts',(51.7804655756869,-5.82224188165806,332.623356646663));
#18759=CARTESIAN_POINT('Ctrl Pts',(51.9756665705209,-3.1514159100441,328.753304819087));
#18760=CARTESIAN_POINT('Ctrl Pts',(52.2539046047944,3.54756726788876,328.969461931057));
#18761=CARTESIAN_POINT('Ctrl Pts',(52.5321426390685,6.99100032608663,334.719754818285));
#18762=CARTESIAN_POINT('Ctrl Pts',(52.8103806733425,4.01889557202994,340.727224572371));
#18763=CARTESIAN_POINT('Ctrl Pts',(53.0886187076162,-2.6412903296749,341.47890487008));
#18764=CARTESIAN_POINT('Ctrl Pts',(53.2912590232671,-5.72659013567874,337.696184823853));
#18765=CARTESIAN_POINT('Ctrl Pts',(53.4011533274931,-5.92292514524674,335.368837807842));
#18766=CARTESIAN_POINT('Ctrl Pts',(53.4183016202944,-5.91960720730597,335.0051128859));
#18767=CARTESIAN_POINT('',(55.1683016202944,-5.90707311933271,335.000830582995));
#18768=CARTESIAN_POINT('Ctrl Pts',(53.4183016202944,-5.91960720730597,335.0051128859));
#18769=CARTESIAN_POINT('Ctrl Pts',(53.4938993389177,-5.90498018047825,333.401642813176));
#18770=CARTESIAN_POINT('Ctrl Pts',(53.6622430689657,-4.40292613845449,329.806849236265));
#18771=CARTESIAN_POINT('Ctrl Pts',(53.9233328104383,1.67985030475698,328.208039614749));
#18772=CARTESIAN_POINT('Ctrl Pts',(54.201570844712,6.62056777777224,332.73710247224));
#18773=CARTESIAN_POINT('Ctrl Pts',(54.4798088789863,5.48568792054639,339.342792990646));
#18774=CARTESIAN_POINT('Ctrl Pts',(54.7580469132599,-0.683326772745727,
341.963166481054));
#18775=CARTESIAN_POINT('Ctrl Pts',(54.9875444936961,-5.25445185386925,338.853889772642));
#18776=CARTESIAN_POINT('Ctrl Pts',(55.1242960627076,-5.90824604487542,335.939238808905));
#18777=CARTESIAN_POINT('Ctrl Pts',(55.1683016202944,-5.90707311933271,335.000830582995));
#18778=CARTESIAN_POINT('',(56.9183016202944,-5.91655016123008,334.994551668503));
#18779=CARTESIAN_POINT('Ctrl Pts',(55.1683016202944,-5.90707311933271,335.000830582995));
#18780=CARTESIAN_POINT('Ctrl Pts',(55.2170420741322,-5.90577398971354,333.961451801674));
#18781=CARTESIAN_POINT('Ctrl Pts',(55.3585285393945,-5.14861220680334,330.942516361876));
#18782=CARTESIAN_POINT('Ctrl Pts',(55.592761016082,-0.32746797118099,328.01105246485));
#18783=CARTESIAN_POINT('Ctrl Pts',(55.8709990503557,5.69994337564951,330.942504659818));
#18784=CARTESIAN_POINT('Ctrl Pts',(56.1492370846297,6.49660081767273,337.597460439936));
#18785=CARTESIAN_POINT('Ctrl Pts',(56.4274751189038,1.33142357898633,341.868765112781));
#18786=CARTESIAN_POINT('Ctrl Pts',(56.6838299641251,-4.55324881616425,339.996525222044));
#18787=CARTESIAN_POINT('Ctrl Pts',(56.8474387979221,-5.90269240546529,336.499586459046));
#18788=CARTESIAN_POINT('Ctrl Pts',(56.9183016202944,-5.91655016123008,334.994551668503));
#18789=CARTESIAN_POINT('',(58.6683016202944,-5.92574144593171,335.001926606557));
#18790=CARTESIAN_POINT('Ctrl Pts',(56.9183016202944,-5.91655016123008,334.994551668503));
#18791=CARTESIAN_POINT('Ctrl Pts',(56.9401848093468,-5.92082958278134,334.529781006691));
#18792=CARTESIAN_POINT('Ctrl Pts',(57.0548140098239,-5.65820055662157,332.099986169156));
#18793=CARTESIAN_POINT('Ctrl Pts',(57.2621892217253,-2.30757253733108,328.394870788079));
#18794=CARTESIAN_POINT('Ctrl Pts',(57.5404272559994,4.30563416012261,329.485098604652));
#18795=CARTESIAN_POINT('Ctrl Pts',(57.8186652902734,6.96762393988721,335.636270031926));
#18796=CARTESIAN_POINT('Ctrl Pts',(58.0969033245473,3.23552807197775,341.203545842231));
#18797=CARTESIAN_POINT('Ctrl Pts',(58.3751413588211,-3.4657641512668,341.077919197307));
#18798=CARTESIAN_POINT('Ctrl Pts',(58.5656074574036,-5.8759136268268,337.173799765407));
#18799=CARTESIAN_POINT('Ctrl Pts',(58.6633275445613,-5.92618778307363,335.107144141683));
#18800=CARTESIAN_POINT('Ctrl Pts',(58.6683016202944,-5.92574144593171,335.001926606557));
#18801=CARTESIAN_POINT('',(60.4183016202944,-5.91073449090133,335.004414681335));
#18802=CARTESIAN_POINT('Ctrl Pts',(58.6683016202944,-5.92574144593171,335.001926606557));
#18803=CARTESIAN_POINT('Ctrl Pts',(58.7560735559859,-5.91786543498634,333.145270772946));
#18804=CARTESIAN_POINT('Ctrl Pts',(58.9365915031022,-3.9770378638174,329.312552672385));
#18805=CARTESIAN_POINT('Ctrl Pts',(59.209855461643,2.55351200167337,328.485999740673));
#18806=CARTESIAN_POINT('Ctrl Pts',(59.4880934959169,6.85961365276339,333.622203405417));
#18807=CARTESIAN_POINT('Ctrl Pts',(59.7663315301909,4.87074910244332,340.022790668771));
#18808=CARTESIAN_POINT('Ctrl Pts',(60.0445695644648,-1.58793000704763,341.814037071656));
#18809=CARTESIAN_POINT('Ctrl Pts',(60.2618929278326,-5.49441940395862,338.328985156489));
#18810=CARTESIAN_POINT('Ctrl Pts',(60.3864702797759,-5.9154146125806,335.682158166079));
#18811=CARTESIAN_POINT('Ctrl Pts',(60.4183016202944,-5.91073449090133,335.004414681335));
#18812=CARTESIAN_POINT('',(62.1683016202944,-5.90971298490255,334.996095888348));
#18813=CARTESIAN_POINT('Ctrl Pts',(60.4183016202944,-5.91073449090133,335.004414681335));
#18814=CARTESIAN_POINT('Ctrl Pts',(60.4792162912005,-5.90177828399176,333.707437530533));
#18815=CARTESIAN_POINT('Ctrl Pts',(60.6328769735312,-4.84222249885208,330.422433708709));
#18816=CARTESIAN_POINT('Ctrl Pts',(60.8792836672866,0.589184251637315,328.028236604786));
#18817=CARTESIAN_POINT('Ctrl Pts',(61.1575217015605,6.18154598103065,331.722636394047));
#18818=CARTESIAN_POINT('Ctrl Pts',(61.4357597358347,6.10119420310092,338.424624390686));
#18819=CARTESIAN_POINT('Ctrl Pts',(61.7139977701083,0.421866558465273,341.98388513136));
#18820=CARTESIAN_POINT('Ctrl Pts',(61.9581783982619,-4.90204272784256,339.482957637104));
#18821=CARTESIAN_POINT('Ctrl Pts',(62.1096130149904,-5.90216516025079,336.246218920781));
#18822=CARTESIAN_POINT('Ctrl Pts',(62.1683016202944,-5.90971298490255,334.996095888348));
#18823=CARTESIAN_POINT('',(63.9183016202944,-5.92498055086206,334.99728658688));
#18824=CARTESIAN_POINT('Ctrl Pts',(62.1683016202944,-5.90971298490255,334.996095888348));
#18825=CARTESIAN_POINT('Ctrl Pts',(62.202359026415,-5.91409304007954,334.270640791982));
#18826=CARTESIAN_POINT('Ctrl Pts',(62.3291624439605,-5.45388643310246,331.574970920775));
#18827=CARTESIAN_POINT('Ctrl Pts',(62.5487118729301,-1.42410672731237,328.149850881153));
#18828=CARTESIAN_POINT('Ctrl Pts',(62.8269499072042,4.98977067018535,330.095429521337));
#18829=CARTESIAN_POINT('Ctrl Pts',(63.1051879414782,6.82460917254905,336.541860098449));
#18830=CARTESIAN_POINT('Ctrl Pts',(63.3834259757519,2.39660456833038,341.57334842103));
#18831=CARTESIAN_POINT('Ctrl Pts',(63.6544638686909,-4.0592289865778,340.598469645657));
#18832=CARTESIAN_POINT('Ctrl Pts',(63.8327557502049,-5.91467205800235,336.807471137171));
#18833=CARTESIAN_POINT('Ctrl Pts',(63.9183016202944,-5.92498055086206,334.99728658688));
#18834=CARTESIAN_POINT('',(65.6683016202944,-5.91799273079897,335.005359985955));
#18835=CARTESIAN_POINT('Ctrl Pts',(63.9183016202944,-5.92498055086206,334.99728658688));
#18836=CARTESIAN_POINT('Ctrl Pts',(63.9255017616296,-5.92584818603211,334.844928739666));
#18837=CARTESIAN_POINT('Ctrl Pts',(63.9327019029648,-5.92048219266218,334.692632997525));
#18838=CARTESIAN_POINT('Ctrl Pts',(64.0326480557246,-5.756739625575,332.585530948395));
#18839=CARTESIAN_POINT('Ctrl Pts',(64.2181400785738,-3.31904956051073,328.840736006949));
#18840=CARTESIAN_POINT('Ctrl Pts',(64.4963781128479,3.38332832967515,328.875809250616));
#18841=CARTESIAN_POINT('Ctrl Pts',(64.7746161471218,6.98087574956347,334.530961952088));
#18842=CARTESIAN_POINT('Ctrl Pts',(65.0528541813957,4.17217653163317,340.616543947135));
#18843=CARTESIAN_POINT('Ctrl Pts',(65.3310922156696,-2.46526750815017,341.547906461952));
#18844=CARTESIAN_POINT('Ctrl Pts',(65.5362413619692,-5.69109873615545,337.804148014749));
#18845=CARTESIAN_POINT('Ctrl Pts',(65.6486444968441,-5.92186363827105,335.422591367118));
#18846=CARTESIAN_POINT('Ctrl Pts',(65.6683016202944,-5.91799273079897,335.005359985955));
#18847=CARTESIAN_POINT('',(67.4183016202943,-5.90696810045156,334.999950211039));
#18848=CARTESIAN_POINT('Ctrl Pts',(65.6683016202944,-5.91799273079897,335.005359985955));
#18849=CARTESIAN_POINT('Ctrl Pts',(65.7413905082688,-5.90359996762069,333.454015113223));
#18850=CARTESIAN_POINT('Ctrl Pts',(65.9072254076679,-4.48362293751429,329.91077451435));
#18851=CARTESIAN_POINT('Ctrl Pts',(66.1658063184914,1.49571981909767,328.165130202852));
#18852=CARTESIAN_POINT('Ctrl Pts',(66.4440443527656,6.55700764647546,332.559042473679));
#18853=CARTESIAN_POINT('Ctrl Pts',(66.7222823870391,5.60102633795406,339.192985437936));
#18854=CARTESIAN_POINT('Ctrl Pts',(67.0005204213133,-0.494934169890714,
341.979087554164));
#18855=CARTESIAN_POINT('Ctrl Pts',(67.2325268323983,-5.19927322096242,338.961829264472));
#18856=CARTESIAN_POINT('Ctrl Pts',(67.3717872320586,-5.90689385452013,335.991902632384));
#18857=CARTESIAN_POINT('Ctrl Pts',(67.4183016202943,-5.90696810045156,334.999950211039));
#18858=CARTESIAN_POINT('',(69.1683016202943,-5.91817602837582,334.994660059035));
#18859=CARTESIAN_POINT('Ctrl Pts',(67.4183016202943,-5.90696810045156,334.999950211039));
#18860=CARTESIAN_POINT('Ctrl Pts',(67.4645332434833,-5.90704189503546,334.014027955488));
#18861=CARTESIAN_POINT('Ctrl Pts',(67.6035108780967,-5.20559334401723,331.050329750945));
#18862=CARTESIAN_POINT('Ctrl Pts',(67.8352345241351,-0.516188130390139,
328.022452240558));
#18863=CARTESIAN_POINT('Ctrl Pts',(68.1134725584092,5.58822975414558,330.789974924528));
#18864=CARTESIAN_POINT('Ctrl Pts',(68.3917105926828,6.56441167543405,337.420975480384));
#18865=CARTESIAN_POINT('Ctrl Pts',(68.6699486269569,1.51652989273906,341.830282571435));
#18866=CARTESIAN_POINT('Ctrl Pts',(68.9288123028274,-4.4746462044703,340.100968698183));
#18867=CARTESIAN_POINT('Ctrl Pts',(69.0949299672732,-5.90373615388174,336.551882931456));
#18868=CARTESIAN_POINT('Ctrl Pts',(69.1683016202943,-5.91817602837582,334.994660059035));
#18869=CARTESIAN_POINT('',(70.9183016202944,-5.92486842591992,335.002808317045));
#18870=CARTESIAN_POINT('Ctrl Pts',(69.1683016202943,-5.91817602837582,334.994660059035));
#18871=CARTESIAN_POINT('Ctrl Pts',(69.1876759786978,-5.92198899008828,334.58346318937));
#18872=CARTESIAN_POINT('Ctrl Pts',(69.2997963485261,-5.69518240152726,332.20802472484));
#18873=CARTESIAN_POINT('Ctrl Pts',(69.5046627297787,-2.48519907860735,328.459632390995));
#18874=CARTESIAN_POINT('Ctrl Pts',(69.7829007640527,4.15505083290677,329.370774875957));
#18875=CARTESIAN_POINT('Ctrl Pts',(70.0611387983268,6.98227192351401,335.447774170024));
#18876=CARTESIAN_POINT('Ctrl Pts',(70.3393768326004,3.4019651280758,341.113857717396));
#18877=CARTESIAN_POINT('Ctrl Pts',(70.6176148668744,-3.300274852473,341.169344277907));
#18878=CARTESIAN_POINT('Ctrl Pts',(70.8105897961057,-5.84815730883804,337.281223184853));
#18879=CARTESIAN_POINT('Ctrl Pts',(70.9108187139124,-5.92579638347857,335.161157513766));
#18880=CARTESIAN_POINT('Ctrl Pts',(70.9183016202944,-5.92486842591992,335.002808317045));
#18881=CARTESIAN_POINT('',(72.6683004134488,-5.91269508019852,335.00386097788));
#18882=CARTESIAN_POINT('Ctrl Pts',(70.9183016202944,-5.92486842591992,335.002808317045));
#18883=CARTESIAN_POINT('Ctrl Pts',(71.003564725337,-5.914294921621,333.198516842018));
#18884=CARTESIAN_POINT('Ctrl Pts',(71.1815738418041,-4.06952942461849,329.412881975299));
#18885=CARTESIAN_POINT('Ctrl Pts',(71.4523289696966,2.37657295890068,328.419382711913));
#18886=CARTESIAN_POINT('Ctrl Pts',(71.7305670039699,6.81988146465013,333.437361292776));
#18887=CARTESIAN_POINT('Ctrl Pts',(72.0088050382442,5.00468541158024,339.889350350746));
#18888=CARTESIAN_POINT('Ctrl Pts',(72.287043072518,-1.40323657466442,341.854454758531));
#18889=CARTESIAN_POINT('Ctrl Pts',(72.5068745564487,-5.44861993418268,338.437239673097));
#18890=CARTESIAN_POINT('Ctrl Pts',(72.6339600289546,-5.91391880206817,335.735378916058));
#18891=CARTESIAN_POINT('Ctrl Pts',(72.6682994900359,-5.90959342734641,335.003878636489));
#18892=CARTESIAN_POINT('',(74.4183028417416,-5.91333520907357,334.995498940171));
#18893=CARTESIAN_POINT('Ctrl Pts',(72.6683016202943,-5.91674875527348,335.003837899133));
#18894=CARTESIAN_POINT('Ctrl Pts',(72.6757466628066,-5.91685175174843,334.845051999899));
#18895=CARTESIAN_POINT('Ctrl Pts',(72.6831917053189,-5.91055848980237,334.686234110631));
#18896=CARTESIAN_POINT('Ctrl Pts',(72.6906367478312,-5.89788795012559,334.52793190082));
#18897=CARTESIAN_POINT('Ctrl Pts',(72.6980821561644,-5.88521678786688,334.369621912643));
#18898=CARTESIAN_POINT('Ctrl Pts',(72.7055275644977,-5.866167751949,334.211828019704));
#18899=CARTESIAN_POINT('Ctrl Pts',(72.7129729728309,-5.84081179818755,334.055093602174));
#18900=CARTESIAN_POINT('Ctrl Pts',(72.7204201449255,-5.81544983779108,333.898322055437));
#18901=CARTESIAN_POINT('Ctrl Pts',(72.7278673170201,-5.7837780416924,333.742610845743));
#18902=CARTESIAN_POINT('Ctrl Pts',(72.7353144891147,-5.74591865285806,333.588493925894));
#18903=CARTESIAN_POINT('Ctrl Pts',(72.7427648236843,-5.70804318686424,333.434311559603));
#18904=CARTESIAN_POINT('Ctrl Pts',(72.7502151582539,-5.66397498144229,333.28172518725));
#18905=CARTESIAN_POINT('Ctrl Pts',(72.7576654928236,-5.61388635854149,333.131254293414));
#18906=CARTESIAN_POINT('Ctrl Pts',(72.7651251739802,-5.563734898507,332.98059463097));
#18907=CARTESIAN_POINT('Ctrl Pts',(72.7725848551368,-5.50754804852549,332.83205609678));
#18908=CARTESIAN_POINT('Ctrl Pts',(72.7800445362934,-5.44554693405786,332.686139772702));
#18909=CARTESIAN_POINT('Ctrl Pts',(72.787509142231,-5.38350488728905,332.540127116631));
#18910=CARTESIAN_POINT('Ctrl Pts',(72.7949737481687,-5.31564108124781,332.396740451863));
#18911=CARTESIAN_POINT('Ctrl Pts',(72.8024383541064,-5.24222280121369,332.256456549472));
#18912=CARTESIAN_POINT('Ctrl Pts',(72.8099152313152,-5.16868382684847,332.115942030513));
#18913=CARTESIAN_POINT('Ctrl Pts',(72.8173921085241,-5.08957231441577,331.978540783871));
#18914=CARTESIAN_POINT('Ctrl Pts',(72.8248689857329,-5.00519974560868,331.844701904881));
#18915=CARTESIAN_POINT('Ctrl Pts',(72.8310857041772,-4.93504739589738,331.733420335805));
#18916=CARTESIAN_POINT('Ctrl Pts',(72.8373024226216,-4.86125878684599,331.624601054125));
#18917=CARTESIAN_POINT('Ctrl Pts',(72.843519141066,-4.78403375003706,331.518484289709));
#18918=CARTESIAN_POINT('Ctrl Pts',(72.850943118504,-4.69181195552443,331.391760122952));
#18919=CARTESIAN_POINT('Ctrl Pts',(72.858367095942,-4.59441237210414,331.268511608734));
#18920=CARTESIAN_POINT('Ctrl Pts',(72.86579107338,-4.4921259084281,331.149190294843));
#18921=CARTESIAN_POINT('Ctrl Pts',(72.8732062894076,-4.38996015816917,331.030009798056));
#18922=CARTESIAN_POINT('Ctrl Pts',(72.8806215054352,-4.28291924800103,330.914747556773));
#18923=CARTESIAN_POINT('Ctrl Pts',(72.8880367214629,-4.17133698706704,330.803825753996));
#18924=CARTESIAN_POINT('Ctrl Pts',(72.895444802607,-4.05986209002254,330.693010679619));
#18925=CARTESIAN_POINT('Ctrl Pts',(72.9028528837511,-3.94385480431372,330.586527990774));
#18926=CARTESIAN_POINT('Ctrl Pts',(72.9102609648952,-3.82368870328334,330.484766311376));
#18927=CARTESIAN_POINT('Ctrl Pts',(72.9176635320692,-3.70361204407653,330.383080375055));
#18928=CARTESIAN_POINT('Ctrl Pts',(72.9250660992432,-3.57938301669183,330.286108691581));
#18929=CARTESIAN_POINT('Ctrl Pts',(72.9324686664172,-3.45141140822068,330.194202474749));
#18930=CARTESIAN_POINT('Ctrl Pts',(72.939867336172,-3.3235071762419,330.102344646139));
#18931=CARTESIAN_POINT('Ctrl Pts',(72.9472660059268,-3.19186458982209,330.015547189946));
#18932=CARTESIAN_POINT('Ctrl Pts',(72.9546646756815,-3.05692572296192,329.934120442925));
#18933=CARTESIAN_POINT('Ctrl Pts',(72.9620621248855,-2.9220091168248,329.852707128789));
#18934=CARTESIAN_POINT('Ctrl Pts',(72.9694595740896,-2.78379762871289,329.776662958035));
#18935=CARTESIAN_POINT('Ctrl Pts',(72.9768570232935,-2.64276156269015,329.706254455939));
#18936=CARTESIAN_POINT('Ctrl Pts',(72.984254151757,-2.50173161174534,329.635849006632));
#18937=CARTESIAN_POINT('Ctrl Pts',(72.9916512802205,-2.35787766031198,329.571078906826));
#18938=CARTESIAN_POINT('Ctrl Pts',(72.999048408684,-2.21169357076184,329.512164168677));
#18939=CARTESIAN_POINT('Ctrl Pts',(73.0064466761206,-2.06548697251136,329.453240359129));
#18940=CARTESIAN_POINT('Ctrl Pts',(73.0138449435572,-1.91694986793742,329.400173845919));
#18941=CARTESIAN_POINT('Ctrl Pts',(73.0212432109939,-1.76659485640011,329.353135987485));
#18942=CARTESIAN_POINT('Ctrl Pts',(73.0286440775196,-1.61618702356597,329.306081604156));
#18943=CARTESIAN_POINT('Ctrl Pts',(73.0360449440454,-1.463960368181,329.265060203762));
#18944=CARTESIAN_POINT('Ctrl Pts',(73.0434458105711,-1.3104412093603,329.230192862902));
#18945=CARTESIAN_POINT('Ctrl Pts',(73.0508548039559,-1.15675347182609,329.195287234368));
#18946=CARTESIAN_POINT('Ctrl Pts',(73.0582637973407,-1.00177076061318,329.166549243657));
#18947=CARTESIAN_POINT('Ctrl Pts',(73.0656727907254,-0.846028839445353,
329.144048688272));
#18948=CARTESIAN_POINT('Ctrl Pts',(73.0730863483057,-0.690190975881867,
329.121534271769));
#18949=CARTESIAN_POINT('Ctrl Pts',(73.0804999058859,-0.533593340756334,
329.10526498571));
#18950=CARTESIAN_POINT('Ctrl Pts',(73.0879134634662,-0.376774811138188,
329.095258574316));
#18951=CARTESIAN_POINT('Ctrl Pts',(73.0953375756029,-0.219733021633884,
329.085237916963));
#18952=CARTESIAN_POINT('Ctrl Pts',(73.1027616877396,-0.0624700816495047,
329.081497950858));
#18953=CARTESIAN_POINT('Ctrl Pts',(73.1101857998763,0.094476318035277,329.084004328278));
#18954=CARTESIAN_POINT('Ctrl Pts',(73.1140429250308,0.176016291434689,329.085306492257));
#18955=CARTESIAN_POINT('Ctrl Pts',(73.1179000501854,0.257470915657662,329.088293828118));
#18956=CARTESIAN_POINT('Ctrl Pts',(73.12175717534,0.338765665720255,329.092956036542));
#18957=CARTESIAN_POINT('Ctrl Pts',(73.1291811527779,0.495237225783612,329.10192959295));
#18958=CARTESIAN_POINT('Ctrl Pts',(73.136605130216,0.651588034156824,329.117138137535));
#18959=CARTESIAN_POINT('Ctrl Pts',(73.1440291076539,0.807280947306682,329.138581397425));
#18960=CARTESIAN_POINT('Ctrl Pts',(73.1514443236816,0.962790119393649,329.159999351041));
#18961=CARTESIAN_POINT('Ctrl Pts',(73.1588595397092,1.11764257559865,329.187637323515));
#18962=CARTESIAN_POINT('Ctrl Pts',(73.1662747557368,1.27130264994705,329.221443075063));
#18963=CARTESIAN_POINT('Ctrl Pts',(73.1736828368809,1.42481487334559,329.255216298887));
#18964=CARTESIAN_POINT('Ctrl Pts',(73.181090918025,1.57713663689715,329.295145407437));
#18965=CARTESIAN_POINT('Ctrl Pts',(73.1884989991691,1.72773897648957,329.341126561619));
#18966=CARTESIAN_POINT('Ctrl Pts',(73.1959015663431,1.8782292200102,329.387073491187));
#18967=CARTESIAN_POINT('Ctrl Pts',(73.2033041335171,2.02700223242095,329.439063388463));
#18968=CARTESIAN_POINT('Ctrl Pts',(73.2107067006911,2.17354091124083,329.496941716676));
#18969=CARTESIAN_POINT('Ctrl Pts',(73.2181053704458,2.32000243808726,329.554789572202));
#18970=CARTESIAN_POINT('Ctrl Pts',(73.2255040402006,2.46423162790464,329.61851954761));
#18971=CARTESIAN_POINT('Ctrl Pts',(73.2329027099554,2.60572828028658,329.687927834468));
#18972=CARTESIAN_POINT('Ctrl Pts',(73.2403001591593,2.74720159011418,329.757324671115));
#18973=CARTESIAN_POINT('Ctrl Pts',(73.2476976083633,2.88594292242243,329.832397795872));
#18974=CARTESIAN_POINT('Ctrl Pts',(73.2550950575673,3.02147364190742,329.912895952139));
#18975=CARTESIAN_POINT('Ctrl Pts',(73.2624921860308,3.15699848501659,329.993390618147));
#18976=CARTESIAN_POINT('Ctrl Pts',(73.2698893144942,3.28931267121137,330.079309657384));
#18977=CARTESIAN_POINT('Ctrl Pts',(73.2772864429577,3.41796393030806,330.170356831648));
#18978=CARTESIAN_POINT('Ctrl Pts',(73.2846847103943,3.54663499848744,330.261418024904));
#18979=CARTESIAN_POINT('Ctrl Pts',(73.2920829778309,3.67164171191348,330.357608709786));
#18980=CARTESIAN_POINT('Ctrl Pts',(73.2994812452675,3.79256257469101,330.458590562441));
#18981=CARTESIAN_POINT('Ctrl Pts',(73.3068821117933,3.91352591823918,330.559607891082));
#18982=CARTESIAN_POINT('Ctrl Pts',(73.3142829783191,4.03040026697695,330.665419499647));
#18983=CARTESIAN_POINT('Ctrl Pts',(73.3216838448448,4.14279898353354,330.77564831666));
#18984=CARTESIAN_POINT('Ctrl Pts',(73.3290928382296,4.25532112462658,330.885998175453));
#18985=CARTESIAN_POINT('Ctrl Pts',(73.3365018316143,4.36335755205725,331.000774667963));
#18986=CARTESIAN_POINT('Ctrl Pts',(73.3439108249991,4.4665596391218,331.119565030481));
#18987=CARTESIAN_POINT('Ctrl Pts',(73.3513243825793,4.56982530223201,331.23842857196));
#18988=CARTESIAN_POINT('Ctrl Pts',(73.3587379401596,4.6682504579066,331.361310619982));
#18989=CARTESIAN_POINT('Ctrl Pts',(73.3661514977398,4.76152856734693,331.487767623741));
#18990=CARTESIAN_POINT('Ctrl Pts',(73.3735756098765,4.85493947525257,331.614404662196));
#18991=CARTESIAN_POINT('Ctrl Pts',(73.3809997220132,4.94318849311046,331.744626513227));
#18992=CARTESIAN_POINT('Ctrl Pts',(73.3884238341499,5.02601352931828,331.877962433665));
#18993=CARTESIAN_POINT('Ctrl Pts',(73.3922809593045,5.06904447021877,331.947235812524));
#18994=CARTESIAN_POINT('Ctrl Pts',(73.3961380844592,5.11061212679421,332.017349362641));
#18995=CARTESIAN_POINT('Ctrl Pts',(73.3999952096138,5.15068483021869,332.088234840813));
#18996=CARTESIAN_POINT('Ctrl Pts',(73.4074191870518,5.22781451467929,332.22467122012));
#18997=CARTESIAN_POINT('Ctrl Pts',(73.4148431644898,5.29963571889571,332.36438016662));
#18998=CARTESIAN_POINT('Ctrl Pts',(73.4222671419278,5.36585799314562,332.506909837191));
#18999=CARTESIAN_POINT('Ctrl Pts',(73.4296823579555,5.43200211514819,332.649271301306));
#19000=CARTESIAN_POINT('Ctrl Pts',(73.4370975739831,5.49256030394941,332.794446528133));
#19001=CARTESIAN_POINT('Ctrl Pts',(73.4445127900107,5.54728660950183,332.941956794783));
#19002=CARTESIAN_POINT('Ctrl Pts',(73.4519208711548,5.60196025767868,333.089325127797));
#19003=CARTESIAN_POINT('Ctrl Pts',(73.4593289522989,5.65081306492765,333.239023680178));
#19004=CARTESIAN_POINT('Ctrl Pts',(73.466737033443,5.69364609892541,333.390551441427));
#19005=CARTESIAN_POINT('Ctrl Pts',(73.474139600617,5.73644725151356,333.541966417796));
#19006=CARTESIAN_POINT('Ctrl Pts',(73.481542167791,5.77323745134734,333.695207534461));
#19007=CARTESIAN_POINT('Ctrl Pts',(73.488944734965,5.80386681787057,333.8497563202));
#19008=CARTESIAN_POINT('Ctrl Pts',(73.4963434047197,5.83448005816613,334.004223736677));
#19009=CARTESIAN_POINT('Ctrl Pts',(73.5037420744744,5.85893885270495,334.159997085907));
#19010=CARTESIAN_POINT('Ctrl Pts',(73.5111407442292,5.87714390120493,334.316545446259));
#19011=CARTESIAN_POINT('Ctrl Pts',(73.5185381934331,5.89534594643729,334.473067980992));
#19012=CARTESIAN_POINT('Ctrl Pts',(73.5259356426371,5.90729625010176,334.630364902748));
#19013=CARTESIAN_POINT('Ctrl Pts',(73.5333330918411,5.91294708220821,334.787897747524));
#19014=CARTESIAN_POINT('Ctrl Pts',(73.5407302203046,5.91859766930443,334.94542376195));
#19015=CARTESIAN_POINT('Ctrl Pts',(73.5481273487681,5.91794931454442,335.103185306085));
#19016=CARTESIAN_POINT('Ctrl Pts',(73.5555244772315,5.91100638160463,335.260641744794));
#19017=CARTESIAN_POINT('Ctrl Pts',(73.5629227446682,5.90406237962649,335.418122427864));
#19018=CARTESIAN_POINT('Ctrl Pts',(73.5703210121048,5.89082188608956,335.575297539095));
#19019=CARTESIAN_POINT('Ctrl Pts',(73.5777192795414,5.87134130912532,335.731629547147));
#19020=CARTESIAN_POINT('Ctrl Pts',(73.5851201460671,5.85185388842959,335.888016476277));
#19021=CARTESIAN_POINT('Ctrl Pts',(73.5925210125928,5.82612206574632,336.043559342399));
#19022=CARTESIAN_POINT('Ctrl Pts',(73.5999218791186,5.79425369685743,336.197728958886));
#19023=CARTESIAN_POINT('Ctrl Pts',(73.6073308725034,5.76235033345261,336.352067868352));
#19024=CARTESIAN_POINT('Ctrl Pts',(73.6147398658881,5.72429704226325,336.505030151006));
#19025=CARTESIAN_POINT('Ctrl Pts',(73.6221488592729,5.68025226318593,336.656099269087));
#19026=CARTESIAN_POINT('Ctrl Pts',(73.6295624168531,5.63618035100563,336.807261450955));
#19027=CARTESIAN_POINT('Ctrl Pts',(73.6369759744334,5.58610971461997,336.956527791325));
#19028=CARTESIAN_POINT('Ctrl Pts',(73.6443895320136,5.53024745963212,337.10340048439));
#19029=CARTESIAN_POINT('Ctrl Pts',(73.6518136441503,5.47430567449726,337.250482277622));
#19030=CARTESIAN_POINT('Ctrl Pts',(73.659237756287,5.41255594909426,337.395163275171));
#19031=CARTESIAN_POINT('Ctrl Pts',(73.6666618684236,5.34525230859312,337.536968332475));
#19032=CARTESIAN_POINT('Ctrl Pts',(73.6705189935784,5.31028535766301,337.610641768911));
#19033=CARTESIAN_POINT('Ctrl Pts',(73.6743761187332,5.27382002168621,337.683539363217));
#19034=CARTESIAN_POINT('Ctrl Pts',(73.6782332438879,5.23589655000898,337.755597554089));
#19035=CARTESIAN_POINT('Ctrl Pts',(73.6856572213259,5.1629035858694,337.894291104803));
#19036=CARTESIAN_POINT('Ctrl Pts',(73.6930811987639,5.08428592689864,338.030291615116));
#19037=CARTESIAN_POINT('Ctrl Pts',(73.7005051762019,5.00026635860841,338.163110321419));
#19038=CARTESIAN_POINT('Ctrl Pts',(73.7079203922295,4.91634594605024,338.295772281666));
#19039=CARTESIAN_POINT('Ctrl Pts',(73.7153356082571,4.82703651142196,338.42525959997));
#19040=CARTESIAN_POINT('Ctrl Pts',(73.7227508242848,4.73260752533167,338.551106387265));
#19041=CARTESIAN_POINT('Ctrl Pts',(73.7301589054289,4.63826939833633,338.676832085415));
#19042=CARTESIAN_POINT('Ctrl Pts',(73.737566986573,4.53882174913629,338.798923929654));
#19043=CARTESIAN_POINT('Ctrl Pts',(73.744975067717,4.43457823445391,338.916943508018));
#19044=CARTESIAN_POINT('Ctrl Pts',(73.7523776348911,4.330412310123,339.034875242256));
#19045=CARTESIAN_POINT('Ctrl Pts',(73.7597802020651,4.22145787401434,339.148740467382));
#19046=CARTESIAN_POINT('Ctrl Pts',(73.7671827692392,4.10806981067076,339.258132571111));
#19047=CARTESIAN_POINT('Ctrl Pts',(73.7745814389939,3.99474144564777,339.367467080375));
#19048=CARTESIAN_POINT('Ctrl Pts',(73.7819801087486,3.87698437017182,339.472332900049));
#19049=CARTESIAN_POINT('Ctrl Pts',(73.7893787785033,3.75519131048829,339.57235921425));
#19050=CARTESIAN_POINT('Ctrl Pts',(73.7967762277073,3.63341834287722,339.672369027215));
#19051=CARTESIAN_POINT('Ctrl Pts',(73.8041736769112,3.50761100061101,339.767540682572));
#19052=CARTESIAN_POINT('Ctrl Pts',(73.8115711261152,3.37819626012077,339.857542649386));
#19053=CARTESIAN_POINT('Ctrl Pts',(73.8189682545787,3.24878713082816,339.947540713872));
#19054=CARTESIAN_POINT('Ctrl Pts',(73.8263653830422,3.11577122070671,340.032369322409));
#19055=CARTESIAN_POINT('Ctrl Pts',(73.8337625115056,2.9796055228116,340.111739575813));
#19056=CARTESIAN_POINT('Ctrl Pts',(73.8411607789423,2.84341885879757,340.191122050254));
#19057=CARTESIAN_POINT('Ctrl Pts',(73.8485590463789,2.70408176378673,340.265044308159));
#19058=CARTESIAN_POINT('Ctrl Pts',(73.8559573138155,2.56207678502752,340.333262895276));
#19059=CARTESIAN_POINT('Ctrl Pts',(73.8633581803413,2.42002191842632,340.401505448299));
#19060=CARTESIAN_POINT('Ctrl Pts',(73.870759046867,2.27529763819714,340.464040179546));
#19061=CARTESIAN_POINT('Ctrl Pts',(73.8781599133928,2.12840731561548,340.520671413998));
#19062=CARTESIAN_POINT('Ctrl Pts',(73.8855689067775,1.98135569341636,340.577364834959));
#19063=CARTESIAN_POINT('Ctrl Pts',(73.8929779001623,1.83213362726564,340.628141678684));
#19064=CARTESIAN_POINT('Ctrl Pts',(73.9003868935471,1.68126122570574,340.672855652442));
#19065=CARTESIAN_POINT('Ctrl Pts',(73.9078004511273,1.53029588154245,340.717597171549));
#19066=CARTESIAN_POINT('Ctrl Pts',(73.9152140087075,1.37767853706626,340.756268286877));
#19067=CARTESIAN_POINT('Ctrl Pts',(73.9226275662878,1.223939884527,340.788773766659));
#19068=CARTESIAN_POINT('Ctrl Pts',(73.9300516784245,1.06998235687021,340.821325523943));
#19069=CARTESIAN_POINT('Ctrl Pts',(73.9374757905612,0.914900699783915,340.847694052046));
#19070=CARTESIAN_POINT('Ctrl Pts',(73.9448999026978,0.75923194006135,340.867835838168));
#19071=CARTESIAN_POINT('Ctrl Pts',(73.9487570278525,0.678355752059643,340.87830030698));
#19072=CARTESIAN_POINT('Ctrl Pts',(73.9526141530071,0.597321124130932,340.887084899145));
#19073=CARTESIAN_POINT('Ctrl Pts',(73.9564712781617,0.516203287562623,340.894189064529));
#19074=CARTESIAN_POINT('Ctrl Pts',(73.9638952555997,0.360072240640283,340.907862762272));
#19075=CARTESIAN_POINT('Ctrl Pts',(73.9713192330376,0.203161983725986,340.915349175448));
#19076=CARTESIAN_POINT('Ctrl Pts',(73.9787432104756,0.0460040905896751,
340.91657115111));
#19077=CARTESIAN_POINT('Ctrl Pts',(73.9861584265032,-0.110968332587724,
340.917791684658));
#19078=CARTESIAN_POINT('Ctrl Pts',(73.9935736425308,-0.268187440692085,
340.912762493661));
#19079=CARTESIAN_POINT('Ctrl Pts',(74.0009888585585,-0.425115631659458,
340.901458062396));
#19080=CARTESIAN_POINT('Ctrl Pts',(74.0083969397025,-0.581892827110618,
340.890164508198));
#19081=CARTESIAN_POINT('Ctrl Pts',(74.0158050208466,-0.738379292932514,
340.87260776091));
#19082=CARTESIAN_POINT('Ctrl Pts',(74.0232131019906,-0.894036621501628,
340.848814331291));
#19083=CARTESIAN_POINT('Ctrl Pts',(74.0306156691646,-1.049578091478,340.825038611556));
#19084=CARTESIAN_POINT('Ctrl Pts',(74.0380182363385,-1.20429128567534,340.795035508693));
#19085=CARTESIAN_POINT('Ctrl Pts',(74.0454208035125,-1.35764222675871,340.758883411445));
#19086=CARTESIAN_POINT('Ctrl Pts',(74.0528194732672,-1.51091242924302,340.722750348119));
#19087=CARTESIAN_POINT('Ctrl Pts',(74.060218143022,-1.66282144466149,340.680474823339));
#19088=CARTESIAN_POINT('Ctrl Pts',(74.0676168127767,-1.81284491932002,340.632186419233));
#19089=CARTESIAN_POINT('Ctrl Pts',(74.0750142619807,-1.96284364476317,340.583905981214));
#19090=CARTESIAN_POINT('Ctrl Pts',(74.0824117111846,-2.11095709187498,340.529614746784));
#19091=CARTESIAN_POINT('Ctrl Pts',(74.0898091603886,-2.25667540777178,340.469492359119));
#19092=CARTESIAN_POINT('Ctrl Pts',(74.097206288852,-2.40238740557655,340.409372578255));
#19093=CARTESIAN_POINT('Ctrl Pts',(74.1046034173155,-2.54570413365216,340.343422289209));
#19094=CARTESIAN_POINT('Ctrl Pts',(74.1120005457789,-2.68613534534628,340.271869447263));
#19095=CARTESIAN_POINT('Ctrl Pts',(74.1193988132155,-2.82658817994117,340.200305587965));
#19096=CARTESIAN_POINT('Ctrl Pts',(74.1267970806521,-2.96415428094545,340.123137627555));
#19097=CARTESIAN_POINT('Ctrl Pts',(74.1341953480886,-3.09836778848121,340.040639603245));
#19098=CARTESIAN_POINT('Ctrl Pts',(74.1415962146144,-3.23262844663473,339.958112596511));
#19099=CARTESIAN_POINT('Ctrl Pts',(74.1489970811402,-3.36353384857073,339.870251993029));
#19100=CARTESIAN_POINT('Ctrl Pts',(74.156397947666,-3.49064704390988,339.777375197464));
#19101=CARTESIAN_POINT('Ctrl Pts',(74.1638069410507,-3.61789982168938,339.684396414298));
#19102=CARTESIAN_POINT('Ctrl Pts',(74.1712159344354,-3.7413517752089,339.586390659074));
#19103=CARTESIAN_POINT('Ctrl Pts',(74.1786249278202,-3.8605984232128,339.483716134769));
#19104=CARTESIAN_POINT('Ctrl Pts',(74.1860384854004,-3.97991853126521,339.380978359415));
#19105=CARTESIAN_POINT('Ctrl Pts',(74.1934520429806,-4.0950278994344,339.273566337949));
#19106=CARTESIAN_POINT('Ctrl Pts',(74.2008656005609,-4.20555925726856,339.161874805434));
#19107=CARTESIAN_POINT('Ctrl Pts',(74.2082897126975,-4.31624797672599,339.050024259573));
#19108=CARTESIAN_POINT('Ctrl Pts',(74.2157138248342,-4.42234541778899,338.933882309191));
#19109=CARTESIAN_POINT('Ctrl Pts',(74.2231379369709,-4.52352437360274,338.813877004299));
#19110=CARTESIAN_POINT('Ctrl Pts',(74.2269950621259,-4.57609091468348,338.751529416911));
#19111=CARTESIAN_POINT('Ctrl Pts',(74.2308521872808,-4.62733055258898,338.688139516362));
#19112=CARTESIAN_POINT('Ctrl Pts',(74.2347093124358,-4.6772021127327,338.623770268539));
#19113=CARTESIAN_POINT('Ctrl Pts',(74.2423589919299,-4.77611035025298,338.496109356502));
#19114=CARTESIAN_POINT('Ctrl Pts',(74.250008671424,-4.86994652241147,338.364191630763));
#19115=CARTESIAN_POINT('Ctrl Pts',(74.2576583509181,-4.95832438822373,338.228459357595));
#19116=CARTESIAN_POINT('Ctrl Pts',(74.265078207762,-5.04404707935131,338.096804948181));
#19117=CARTESIAN_POINT('Ctrl Pts',(74.2724980646059,-5.1246344399638,337.961562210214));
#19118=CARTESIAN_POINT('Ctrl Pts',(74.2799179214499,-5.19977333234696,337.823169823924));
#19119=CARTESIAN_POINT('Ctrl Pts',(74.2873306662723,-5.27484020320359,337.68491008839));
#19120=CARTESIAN_POINT('Ctrl Pts',(74.2947434110947,-5.34446882398607,337.543507037777));
#19121=CARTESIAN_POINT('Ctrl Pts',(74.3021561559172,-5.40838925348953,337.399428316337));
#19122=CARTESIAN_POINT('Ctrl Pts',(74.3095632481942,-5.47226094084134,337.255459461288));
#19123=CARTESIAN_POINT('Ctrl Pts',(74.3169703404712,-5.53043295194006,337.108819335603));
#19124=CARTESIAN_POINT('Ctrl Pts',(74.3243774327482,-5.58268128323765,336.960000064359));
#19125=CARTESIAN_POINT('Ctrl Pts',(74.3317803281464,-5.63490001048733,336.811265114523));
#19126=CARTESIAN_POINT('Ctrl Pts',(74.3391832235446,-5.68120161851954,336.660353827863));
#19127=CARTESIAN_POINT('Ctrl Pts',(74.3465861189427,-5.72141030393377,336.507778066076));
#19128=CARTESIAN_POINT('Ctrl Pts',(74.3539867174594,-5.76160651387961,336.355249643666));
#19129=CARTESIAN_POINT('Ctrl Pts',(74.361387315976,-5.7957134694907,336.20105813341));
#19130=CARTESIAN_POINT('Ctrl Pts',(74.3687879144927,-5.82360530532201,336.045730276087));
#19131=CARTESIAN_POINT('Ctrl Pts',(74.3761872484323,-5.85149237513666,335.890428960407));
#19132=CARTESIAN_POINT('Ctrl Pts',(74.3835865823718,-5.87316637764072,335.733992050929));
#19133=CARTESIAN_POINT('Ctrl Pts',(74.3909859163114,-5.88855265489511,335.576955971481));
#19134=CARTESIAN_POINT('Ctrl Pts',(74.3983864492706,-5.90394142540762,335.419894445236));
#19135=CARTESIAN_POINT('Ctrl Pts',(74.4057869822299,-5.91304040122936,335.262233925485));
#19136=CARTESIAN_POINT('Ctrl Pts',(74.4131875151892,-5.91582682860317,335.104515532238));
#19137=CARTESIAN_POINT('Ctrl Pts',(74.4148922168909,-5.91646867798239,335.068185336178));
#19138=CARTESIAN_POINT('Ctrl Pts',(74.4165969185926,-5.91677579908169,335.031852074546));
#19139=CARTESIAN_POINT('Ctrl Pts',(74.4183016202943,-5.91674830572166,334.995522362246));
#19140=CARTESIAN_POINT('',(76.1683016202944,-5.92582145116702,334.998177799619));
#19141=CARTESIAN_POINT('Ctrl Pts',(74.41830372254,-5.91087398967905,334.995482050269));
#19142=CARTESIAN_POINT('Ctrl Pts',(74.4498515972632,-5.915576218536,334.323813884359));
#19143=CARTESIAN_POINT('Ctrl Pts',(74.574145483411,-5.49945147134948,331.683203449152));
#19144=CARTESIAN_POINT('Ctrl Pts',(74.7911853809838,-1.60867620262318,328.190830902648));
#19145=CARTESIAN_POINT('Ctrl Pts',(75.0694234152574,4.85542856215696,329.962397752996));
#19146=CARTESIAN_POINT('Ctrl Pts',(75.3476614495315,6.86377820144993,336.35689783053));
#19147=CARTESIAN_POINT('Ctrl Pts',(75.6258994838053,2.57333989447748,341.506192796768));
#19148=CARTESIAN_POINT('Ctrl Pts',(75.899446207393,-3.96645730280381,340.698699134842));
#19149=CARTESIAN_POINT('Ctrl Pts',(76.080246919556,-5.91830003067549,336.860747988309));
#19150=CARTESIAN_POINT('Ctrl Pts',(76.1683016202944,-5.92582145116702,334.998177799619));
#19151=CARTESIAN_POINT('',(77.9183016202943,-5.91636786088317,335.005450758099));
#19152=CARTESIAN_POINT('Ctrl Pts',(76.1683016202944,-5.92582145116702,334.998177799619));
#19153=CARTESIAN_POINT('Ctrl Pts',(76.1729929309807,-5.92622217162864,334.898945216272));
#19154=CARTESIAN_POINT('Ctrl Pts',(76.2704302530915,-5.8789467039455,332.838299720819));
#19155=CARTESIAN_POINT('Ctrl Pts',(76.4606135866272,-3.48425963772524,328.932664695425));
#19156=CARTESIAN_POINT('Ctrl Pts',(76.7388516209012,3.21661888179215,328.786628460286));
#19157=CARTESIAN_POINT('Ctrl Pts',(77.0170896551749,6.96565373070174,334.342511577927));
#19158=CARTESIAN_POINT('Ctrl Pts',(77.2953276894491,4.32241096383202,340.501762115993));
#19159=CARTESIAN_POINT('Ctrl Pts',(77.5735657237229,-2.28744454586805,341.612126766086));
#19160=CARTESIAN_POINT('Ctrl Pts',(77.7812237006714,-5.65392581216805,337.912195455118));
#19161=CARTESIAN_POINT('Ctrl Pts',(77.8961356661952,-5.92069250751692,335.476264034432));
#19162=CARTESIAN_POINT('Ctrl Pts',(77.9183016202943,-5.91636786088317,335.005450758099));
#19163=CARTESIAN_POINT('',(79.6683016202943,-5.90709975113901,334.99907110307));
#19164=CARTESIAN_POINT('Ctrl Pts',(77.9183016202943,-5.91636786088317,335.005450758099));
#19165=CARTESIAN_POINT('Ctrl Pts',(77.9888816776198,-5.90259747202661,333.506303557644));
#19166=CARTESIAN_POINT('Ctrl Pts',(78.15220774637,-4.56196104589022,330.015280932936));
#19167=CARTESIAN_POINT('Ctrl Pts',(78.4082798265448,1.31049715735917,328.127211619599));
#19168=CARTESIAN_POINT('Ctrl Pts',(78.6865178608185,6.48865958174404,332.382764864702));
#19169=CARTESIAN_POINT('Ctrl Pts',(78.9647558950927,5.71227488042645,339.040116163141));
#19170=CARTESIAN_POINT('Ctrl Pts',(79.2429939293665,-0.306180165623157,
341.989912490683));
#19171=CARTESIAN_POINT('Ctrl Pts',(79.4775091711004,-5.14206124859087,339.069624867681));
#19172=CARTESIAN_POINT('Ctrl Pts',(79.6192784014097,-5.90563805222993,336.044468030236));
#19173=CARTESIAN_POINT('Ctrl Pts',(79.6683016202943,-5.90709975113901,334.99907110307));
#19174=CARTESIAN_POINT('',(81.4183016202943,-5.91978654872489,334.994924692135));
#19175=CARTESIAN_POINT('Ctrl Pts',(79.6683016202943,-5.90709975113901,334.99907110307));
#19176=CARTESIAN_POINT('Ctrl Pts',(79.7120244128344,-5.90840341009107,334.06670325762));
#19177=CARTESIAN_POINT('Ctrl Pts',(79.848493216799,-5.26054489141,331.158283532971));
#19178=CARTESIAN_POINT('Ctrl Pts',(80.0777080321885,-0.704531368517576,
328.0389470285));
#19179=CARTESIAN_POINT('Ctrl Pts',(80.3559460664623,5.47243560177532,330.640519353683));
#19180=CARTESIAN_POINT('Ctrl Pts',(80.6341841007362,6.62742919334053,337.242722722158));
#19181=CARTESIAN_POINT('Ctrl Pts',(80.9124221350103,1.70052883486869,341.786812551044));
#19182=CARTESIAN_POINT('Ctrl Pts',(81.1737946415294,-4.39368190432037,340.204825231976));
#19183=CARTESIAN_POINT('Ctrl Pts',(81.3424211366242,-5.90516058242414,336.604266515423));
#19184=CARTESIAN_POINT('Ctrl Pts',(81.4183016202943,-5.91978654872489,334.994924692135));
#19185=CARTESIAN_POINT('',(83.1683016202943,-5.92374140024353,335.003591464748));
#19186=CARTESIAN_POINT('Ctrl Pts',(81.4183016202943,-5.91978654872489,334.994924692135));
#19187=CARTESIAN_POINT('Ctrl Pts',(81.4351671480489,-5.92303737988268,334.637225348714));
#19188=CARTESIAN_POINT('Ctrl Pts',(81.5447786872283,-5.73048622156047,332.315977687839));
#19189=CARTESIAN_POINT('Ctrl Pts',(81.7471362378319,-2.66101092507237,328.529169776771));
#19190=CARTESIAN_POINT('Ctrl Pts',(82.025374272106,4.00143348348799,329.260561612978));
#19191=CARTESIAN_POINT('Ctrl Pts',(82.3036123063798,6.99182144531686,335.258951342982));
#19192=CARTESIAN_POINT('Ctrl Pts',(82.5818503406539,3.56591806589121,341.019705247648));
#19193=CARTESIAN_POINT('Ctrl Pts',(82.8600883749277,-3.13237568973752,341.256264497251));
#19194=CARTESIAN_POINT('Ctrl Pts',(83.055572134808,-5.81886229015184,337.388770887391));
#19195=CARTESIAN_POINT('Ctrl Pts',(83.1583098832635,-5.9252530122218,335.21513720506));
#19196=CARTESIAN_POINT('Ctrl Pts',(83.1683016202943,-5.92374140024353,335.003591464748));
#19197=CARTESIAN_POINT('',(84.9183016202943,-5.90863610109609,335.003151912275));
#19198=CARTESIAN_POINT('Ctrl Pts',(83.1683016202943,-5.92374140024353,335.003591464748));
#19199=CARTESIAN_POINT('Ctrl Pts',(83.2510558946881,-5.91122182011041,333.25151230308));
#19200=CARTESIAN_POINT('Ctrl Pts',(83.4265561805065,-4.15954688889828,329.514063221093));
#19201=CARTESIAN_POINT('Ctrl Pts',(83.6948024777495,2.19789854021227,328.35757085637));
#19202=CARTESIAN_POINT('Ctrl Pts',(83.9730405120235,6.77516939239106,333.253660220452));
#19203=CARTESIAN_POINT('Ctrl Pts',(84.2512785462973,5.13496729450675,339.752339824294));
#19204=CARTESIAN_POINT('Ctrl Pts',(84.5295165805716,-1.21751849755278,341.8898673158));
#19205=CARTESIAN_POINT('Ctrl Pts',(84.751857605237,-5.40097549058787,338.545457143259));
#19206=CARTESIAN_POINT('Ctrl Pts',(84.881452618478,-5.91242016185975,335.788429134871));
#19207=CARTESIAN_POINT('Ctrl Pts',(84.9183016202943,-5.90863610109609,335.003151912275));
#19208=CARTESIAN_POINT('',(86.6683016557598,-5.91499694012912,334.995072884561));
#19209=CARTESIAN_POINT('Ctrl Pts',(84.9183016202943,-5.90863610109609,335.003151912275));
#19210=CARTESIAN_POINT('Ctrl Pts',(84.9741986299026,-5.90289598140656,333.811948723774));
#19211=CARTESIAN_POINT('Ctrl Pts',(85.1228416509356,-4.97462503877836,330.636036147798));
#19212=CARTESIAN_POINT('Ctrl Pts',(85.3642306833932,0.211710701760056,328.006588707936));
#19213=CARTESIAN_POINT('Ctrl Pts',(85.642468717667,5.99547756206436,331.393495913769));
#19214=CARTESIAN_POINT('Ctrl Pts',(85.9207067519411,6.27728315676505,338.090038687625));
#19215=CARTESIAN_POINT('Ctrl Pts',(86.1989447862149,0.798518651050066,341.950898566742));
#19216=CARTESIAN_POINT('Ctrl Pts',(86.4481430756662,-4.76473389874006,339.695812636113));
#19217=CARTESIAN_POINT('Ctrl Pts',(86.6045953536925,-5.90157004990948,336.350648623481));
#19218=CARTESIAN_POINT('Ctrl Pts',(86.6683016202943,-5.91219196599268,334.995075975938));
#19219=CARTESIAN_POINT('',(88.4183016202943,-5.92102082817391,334.999137582022));
#19220=CARTESIAN_POINT('Ctrl Pts',(86.6683016778991,-5.91674794688882,334.995070954768));
#19221=CARTESIAN_POINT('Ctrl Pts',(86.6770913492031,-5.91659201877899,334.807897317635));
#19222=CARTESIAN_POINT('Ctrl Pts',(86.6858810205071,-5.90755058647221,334.621105110605));
#19223=CARTESIAN_POINT('Ctrl Pts',(86.6946706918111,-5.88975493954476,334.43544945788));
#19224=CARTESIAN_POINT('Ctrl Pts',(86.7035231249044,-5.87183222453902,334.248468149105));
#19225=CARTESIAN_POINT('Ctrl Pts',(86.7123755579976,-5.84502993007678,334.062639720827));
#19226=CARTESIAN_POINT('Ctrl Pts',(86.7212279910908,-5.80953093661791,333.878714639809));
#19227=CARTESIAN_POINT('Ctrl Pts',(86.7301500921251,-5.77375256891734,333.6933420831));
#19228=CARTESIAN_POINT('Ctrl Pts',(86.7390721931593,-5.72914013624011,333.509902983608));
#19229=CARTESIAN_POINT('Ctrl Pts',(86.7479942941936,-5.67592904703274,333.329143927338));
#19230=CARTESIAN_POINT('Ctrl Pts',(86.7504698143833,-5.6611651337857,333.278990640399));
#19231=CARTESIAN_POINT('Ctrl Pts',(86.7529453345731,-5.64573954508261,333.22904354358));
#19232=CARTESIAN_POINT('Ctrl Pts',(86.7554208547628,-5.62965795197997,333.179318285309));
#19233=CARTESIAN_POINT('Ctrl Pts',(86.762844832201,-5.58142995333242,333.030194397315));
#19234=CARTESIAN_POINT('Ctrl Pts',(86.770268809639,-5.52719989935396,332.882763137558));
#19235=CARTESIAN_POINT('Ctrl Pts',(86.7776927870771,-5.46710380876563,332.737544142601));
#19236=CARTESIAN_POINT('Ctrl Pts',(86.7851080031049,-5.4070786406061,332.592496527906));
#19237=CARTESIAN_POINT('Ctrl Pts',(86.7925232191326,-5.34120135711314,332.449656322658));
#19238=CARTESIAN_POINT('Ctrl Pts',(86.7999384351604,-5.26965788341659,332.309528599995));
#19239=CARTESIAN_POINT('Ctrl Pts',(86.8073465163046,-5.19818324849036,332.169535707522));
#19240=CARTESIAN_POINT('Ctrl Pts',(86.8147545974487,-5.12105344580863,332.032250431909));
#19241=CARTESIAN_POINT('Ctrl Pts',(86.8221626785929,-5.03850263088355,331.898158321081));
#19242=CARTESIAN_POINT('Ctrl Pts',(86.829565245767,-4.95601326003751,331.764166017459));
#19243=CARTESIAN_POINT('Ctrl Pts',(86.8369678129411,-4.86811110595498,331.633362462657));
#19244=CARTESIAN_POINT('Ctrl Pts',(86.8443703801152,-4.77507637811505,331.506208914994));
#19245=CARTESIAN_POINT('Ctrl Pts',(86.8517690498701,-4.68209063265265,331.379122313118));
#19246=CARTESIAN_POINT('Ctrl Pts',(86.8591677196249,-4.58397791500222,331.255682191615));
#19247=CARTESIAN_POINT('Ctrl Pts',(86.8665663893798,-4.48106183499563,331.136321002795));
#19248=CARTESIAN_POINT('Ctrl Pts',(86.8739638385839,-4.37816273294653,331.016979504865));
#19249=CARTESIAN_POINT('Ctrl Pts',(86.8813612877879,-4.27046208468305,330.901715886512));
#19250=CARTESIAN_POINT('Ctrl Pts',(86.888758736992,-4.15832395758744,330.79092974325));
#19251=CARTESIAN_POINT('Ctrl Pts',(86.8961558654556,-4.04619069260545,330.680148403483));
#19252=CARTESIAN_POINT('Ctrl Pts',(86.9035529939192,-3.92962059684443,330.573844415097));
#19253=CARTESIAN_POINT('Ctrl Pts',(86.9109501223827,-3.8090145956135,330.472380496011));
#19254=CARTESIAN_POINT('Ctrl Pts',(86.9183483898194,-3.68839002406911,330.370900954014));
#19255=CARTESIAN_POINT('Ctrl Pts',(86.9257466572562,-3.56372859531484,330.274263205482));
#19256=CARTESIAN_POINT('Ctrl Pts',(86.9331449246929,-3.43546417630343,330.182789556617));
#19257=CARTESIAN_POINT('Ctrl Pts',(86.9405457912187,-3.30715469665277,330.091283772097));
#19258=CARTESIAN_POINT('Ctrl Pts',(86.9479466577446,-3.17524001026643,330.00494591588));
#19259=CARTESIAN_POINT('Ctrl Pts',(86.9553475242704,-3.04018266385231,329.924054774437));
#19260=CARTESIAN_POINT('Ctrl Pts',(86.9627565176553,-2.90497701155974,329.843074806788));
#19261=CARTESIAN_POINT('Ctrl Pts',(86.9701655110401,-2.76662212789234,329.767553690198));
#19262=CARTESIAN_POINT('Ctrl Pts',(86.977574504425,-2.62560548646099,329.697724413804));
#19263=CARTESIAN_POINT('Ctrl Pts',(86.9849880620053,-2.48450197391433,329.627852120168));
#19264=CARTESIAN_POINT('Ctrl Pts',(86.9924016195857,-2.34073377622073,329.5636788054));
#19265=CARTESIAN_POINT('Ctrl Pts',(86.999815177166,-2.19480751753888,329.505388956127));
#19266=CARTESIAN_POINT('Ctrl Pts',(87.0072392893028,-2.04867350611252,329.447016120582));
#19267=CARTESIAN_POINT('Ctrl Pts',(87.0146634014395,-1.90037564839793,329.394543603615));
#19268=CARTESIAN_POINT('Ctrl Pts',(87.0220875135763,-1.75043564479503,329.348106015155));
#19269=CARTESIAN_POINT('Ctrl Pts',(87.0259446387298,-1.67253577626432,329.323979818349));
#19270=CARTESIAN_POINT('Ctrl Pts',(87.0298017638834,-1.5941928345188,329.301481741589));
#19271=CARTESIAN_POINT('Ctrl Pts',(87.0336588890369,-1.51548085109625,329.280625178181));
#19272=CARTESIAN_POINT('Ctrl Pts',(87.0410828664749,-1.36398045487567,329.240481638623));
#19273=CARTESIAN_POINT('Ctrl Pts',(87.0485068439129,-1.21065536931273,329.206301333703));
#19274=CARTESIAN_POINT('Ctrl Pts',(87.0559308213508,-1.0560161754136,329.178251087537));
#19275=CARTESIAN_POINT('Ctrl Pts',(87.0633460373785,-0.901559479029998,
329.150233944882));
#19276=CARTESIAN_POINT('Ctrl Pts',(87.070761253406,-0.745792124940789,329.128332526772));
#19277=CARTESIAN_POINT('Ctrl Pts',(87.0781764694336,-0.589239454681361,
329.112663808857));
#19278=CARTESIAN_POINT('Ctrl Pts',(87.0855845505777,-0.432837418613007,
329.097010167303));
#19279=CARTESIAN_POINT('Ctrl Pts',(87.0929926317218,-0.275651939561479,
329.087577323808));
#19280=CARTESIAN_POINT('Ctrl Pts',(87.1004007128659,-0.118218040117437,
329.08443112985));
#19281=CARTESIAN_POINT('Ctrl Pts',(87.1078032800399,0.0390986783998228,
329.081287277661));
#19282=CARTESIAN_POINT('Ctrl Pts',(87.1152058472139,0.196663077600628,329.084420765329));
#19283=CARTESIAN_POINT('Ctrl Pts',(87.1226084143879,0.353935638096085,329.093845572068));
#19284=CARTESIAN_POINT('Ctrl Pts',(87.1300070841426,0.511125395275907,329.103265416687));
#19285=CARTESIAN_POINT('Ctrl Pts',(87.1374057538974,0.668023248152384,329.118969961363));
#19286=CARTESIAN_POINT('Ctrl Pts',(87.1448044236521,0.824090414503162,329.140921100444));
#19287=CARTESIAN_POINT('Ctrl Pts',(87.1522018728561,0.980131834617748,329.162868618268));
#19288=CARTESIAN_POINT('Ctrl Pts',(87.15959932206,1.13534247096755,329.191060633368));
#19289=CARTESIAN_POINT('Ctrl Pts',(87.166996771264,1.28918927740853,329.225407237777));
#19290=CARTESIAN_POINT('Ctrl Pts',(87.1743938997275,1.44302941332009,329.259752352977));
#19291=CARTESIAN_POINT('Ctrl Pts',(87.1817910281909,1.59550547265486,329.300251445578));
#19292=CARTESIAN_POINT('Ctrl Pts',(87.1891881566544,1.74609547448755,329.346763656411));
#19293=CARTESIAN_POINT('Ctrl Pts',(87.196586424091,1.89670866342128,329.393283028964));
#19294=CARTESIAN_POINT('Ctrl Pts',(87.2039846915276,2.04543486000551,329.445817253133));
#19295=CARTESIAN_POINT('Ctrl Pts',(87.2113829589642,2.19176823977726,329.504175899321));
#19296=CARTESIAN_POINT('Ctrl Pts',(87.21878382549,2.3381530280044,329.562555047515));
#19297=CARTESIAN_POINT('Ctrl Pts',(87.2261846920157,2.48214297930056,329.626762553507));
#19298=CARTESIAN_POINT('Ctrl Pts',(87.2335855585414,2.62325334560855,329.696560319259));
#19299=CARTESIAN_POINT('Ctrl Pts',(87.2409945519262,2.76451866458943,329.766434729631));
#19300=CARTESIAN_POINT('Ctrl Pts',(87.2484035453109,2.90289774905522,329.841911493389));
#19301=CARTESIAN_POINT('Ctrl Pts',(87.2558125386957,3.03793087352768,329.922706767364));
#19302=CARTESIAN_POINT('Ctrl Pts',(87.2632260962759,3.17304718306261,330.003551814015));
#19303=CARTESIAN_POINT('Ctrl Pts',(87.2706396538561,3.3048131137172,330.089721695728));
#19304=CARTESIAN_POINT('Ctrl Pts',(87.2780532114364,3.43279936334925,330.180890217738));
#19305=CARTESIAN_POINT('Ctrl Pts',(87.285477323573,3.56096782483858,330.27218853483));
#19306=CARTESIAN_POINT('Ctrl Pts',(87.2929014357098,3.68534556394649,330.368499477372));
#19307=CARTESIAN_POINT('Ctrl Pts',(87.3003255478464,3.80553706228962,330.469457181524));
#19308=CARTESIAN_POINT('Ctrl Pts',(87.3041826730012,3.86798138466975,330.521908773457));
#19309=CARTESIAN_POINT('Ctrl Pts',(87.308039798156,3.92929635850881,330.575614024287));
#19310=CARTESIAN_POINT('Ctrl Pts',(87.3118969233108,3.98943065837669,330.630517927202));
#19311=CARTESIAN_POINT('Ctrl Pts',(87.3193209007487,4.10517377470132,330.736193869812));
#19312=CARTESIAN_POINT('Ctrl Pts',(87.3267448781867,4.21688972390287,330.846631281051));
#19313=CARTESIAN_POINT('Ctrl Pts',(87.3341688556247,4.32416191534318,330.96149108056));
#19314=CARTESIAN_POINT('Ctrl Pts',(87.3415840716523,4.4313075094577,331.076215328224));
#19315=CARTESIAN_POINT('Ctrl Pts',(87.3489992876799,4.53401953241901,331.195351305386));
#19316=CARTESIAN_POINT('Ctrl Pts',(87.3564145037075,4.63191532445918,331.318520543377));
#19317=CARTESIAN_POINT('Ctrl Pts',(87.3638225848516,4.72971692166116,331.441571268547));
#19318=CARTESIAN_POINT('Ctrl Pts',(87.3712306659957,4.82271128301208,331.568647238415));
#19319=CARTESIAN_POINT('Ctrl Pts',(87.3786387471397,4.91055350117726,331.699334177083));
#19320=CARTESIAN_POINT('Ctrl Pts',(87.3860413143137,4.99833033677514,331.829923843075));
#19321=CARTESIAN_POINT('Ctrl Pts',(87.3934438814877,5.08096245759623,331.964118817828));
#19322=CARTESIAN_POINT('Ctrl Pts',(87.4008464486617,5.15814614332173,332.101472972933));
#19323=CARTESIAN_POINT('Ctrl Pts',(87.4082451184164,5.23528919217407,332.238754811676));
#19324=CARTESIAN_POINT('Ctrl Pts',(87.4156437881712,5.3069893365025,332.37919219368));
#19325=CARTESIAN_POINT('Ctrl Pts',(87.4230424579259,5.3729870541872,332.522311424324));
#19326=CARTESIAN_POINT('Ctrl Pts',(87.4304399071299,5.43897388429783,332.665407044739));
#19327=CARTESIAN_POINT('Ctrl Pts',(87.4378373563338,5.49925999866321,332.811183297147));
#19328=CARTESIAN_POINT('Ctrl Pts',(87.4452348055378,5.55363254095616,332.959143277314));
#19329=CARTESIAN_POINT('Ctrl Pts',(87.4526319340012,5.60800272575043,333.107096842194));
#19330=CARTESIAN_POINT('Ctrl Pts',(87.4600290624647,5.65645971955299,333.257233596266));
#19331=CARTESIAN_POINT('Ctrl Pts',(87.4674261909281,5.69883950001306,333.409038367656));
#19332=CARTESIAN_POINT('Ctrl Pts',(87.4748244583647,5.7412258059014,333.560866513191));
#19333=CARTESIAN_POINT('Ctrl Pts',(87.4822227258013,5.77753293490812,333.714362827944));
#19334=CARTESIAN_POINT('Ctrl Pts',(87.4896209932379,5.8076472927037,333.86899890095));
#19335=CARTESIAN_POINT('Ctrl Pts',(87.4970218597636,5.83777222998987,334.023689299236));
#19336=CARTESIAN_POINT('Ctrl Pts',(87.5044227262893,5.86169999318229,334.179519886889));
#19337=CARTESIAN_POINT('Ctrl Pts',(87.5118235928151,5.8793684790117,334.335954180418));
#19338=CARTESIAN_POINT('Ctrl Pts',(87.5192325861998,5.89705636652772,334.492560253758));
#19339=CARTESIAN_POINT('Ctrl Pts',(87.5266415795845,5.90847120845254,334.649770985798));
#19340=CARTESIAN_POINT('Ctrl Pts',(87.5340505729693,5.9136029107264,334.807046179752));
#19341=CARTESIAN_POINT('Ctrl Pts',(87.5414641305495,5.91873777430587,334.964418260651));
#19342=CARTESIAN_POINT('Ctrl Pts',(87.5488776881297,5.91758178822474,335.121854510262));
#19343=CARTESIAN_POINT('Ctrl Pts',(87.5562912457099,5.91017693659669,335.278817396553));
#19344=CARTESIAN_POINT('Ctrl Pts',(87.5637153578466,5.9027615428067,335.436003748248));
#19345=CARTESIAN_POINT('Ctrl Pts',(87.5711394699833,5.88907954794415,335.592715019877));
#19346=CARTESIAN_POINT('Ctrl Pts',(87.57856358212,5.86922457702474,335.748420621675));
#19347=CARTESIAN_POINT('Ctrl Pts',(87.5824207072749,5.85890912025721,335.829315950625));
#19348=CARTESIAN_POINT('Ctrl Pts',(87.5862778324298,5.84692827967926,335.909940013058));
#19349=CARTESIAN_POINT('Ctrl Pts',(87.5901349575847,5.83330053655822,335.990219880981));
#19350=CARTESIAN_POINT('Ctrl Pts',(87.5975589350227,5.8070706235016,336.144738053001));
#19351=CARTESIAN_POINT('Ctrl Pts',(87.6049829124607,5.77465735868433,336.298446398159));
#19352=CARTESIAN_POINT('Ctrl Pts',(87.6124068898987,5.73612044091608,336.450811100662));
#19353=CARTESIAN_POINT('Ctrl Pts',(87.6198221059263,5.69762900250901,336.602995989892));
#19354=CARTESIAN_POINT('Ctrl Pts',(87.627237321954,5.65302838689777,336.753840034528));
#19355=CARTESIAN_POINT('Ctrl Pts',(87.6346525379816,5.60242977730287,336.902816636697));
#19356=CARTESIAN_POINT('Ctrl Pts',(87.6420606191257,5.55187985343535,337.051649894329));
#19357=CARTESIAN_POINT('Ctrl Pts',(87.6494687002698,5.49534354426832,337.19861893565));
#19358=CARTESIAN_POINT('Ctrl Pts',(87.6568767814139,5.43298257409329,337.343209532265));
#19359=CARTESIAN_POINT('Ctrl Pts',(87.664279348588,5.37066802032726,337.487692507459));
#19360=CARTESIAN_POINT('Ctrl Pts',(87.671681915762,5.30253758513885,337.629800221682));
#19361=CARTESIAN_POINT('Ctrl Pts',(87.679084482936,5.228802066933,337.769035844358));
#19362=CARTESIAN_POINT('Ctrl Pts',(87.6864831526908,5.15510537015528,337.908198160087));
#19363=CARTESIAN_POINT('Ctrl Pts',(87.6938818224455,5.0758096417775,338.044491066806));
#19364=CARTESIAN_POINT('Ctrl Pts',(87.7012804922003,4.99117277940121,338.177439983487));
#19365=CARTESIAN_POINT('Ctrl Pts',(87.7086779414042,4.90654987947903,338.310366967727));
#19366=CARTESIAN_POINT('Ctrl Pts',(87.7160753906082,4.8165877945281,338.439950742262));
#19367=CARTESIAN_POINT('Ctrl Pts',(87.7234728398122,4.72158919314777,338.565743408274));
#19368=CARTESIAN_POINT('Ctrl Pts',(87.7308699682757,4.62659471074119,338.691530620135));
#19369=CARTESIAN_POINT('Ctrl Pts',(87.7382670967392,4.52656437102247,338.813526752482));
#19370=CARTESIAN_POINT('Ctrl Pts',(87.7456642252027,4.42184263110569,338.931315086359));
#19371=CARTESIAN_POINT('Ctrl Pts',(87.7530624926393,4.3171047666551,339.049121556699));
#19372=CARTESIAN_POINT('Ctrl Pts',(87.7604607600759,4.20767431168648,339.162718659589));
#19373=CARTESIAN_POINT('Ctrl Pts',(87.7678590275125,4.09393414584336,339.271724917641));
#19374=CARTESIAN_POINT('Ctrl Pts',(87.7752598940383,3.98015402188385,339.380769470738));
#19375=CARTESIAN_POINT('Ctrl Pts',(87.7826607605641,3.86206144186349,339.48521970982));
#19376=CARTESIAN_POINT('Ctrl Pts',(87.7900616270898,3.74007393855449,339.584733088921));
#19377=CARTESIAN_POINT('Ctrl Pts',(87.7974706204746,3.61795248130439,339.684355743226));
#19378=CARTESIAN_POINT('Ctrl Pts',(87.8048796138594,3.491927848736,339.779030475183));
#19379=CARTESIAN_POINT('Ctrl Pts',(87.8122886072441,3.36244884137766,339.868456465002));
#19380=CARTESIAN_POINT('Ctrl Pts',(87.8197021648244,3.23289007048449,339.957937544316));
#19381=CARTESIAN_POINT('Ctrl Pts',(87.8271157224046,3.09987299903118,340.042163239313));
#19382=CARTESIAN_POINT('Ctrl Pts',(87.8345292799849,2.96387236918584,340.120877965904));
#19383=CARTESIAN_POINT('Ctrl Pts',(87.8419533921216,2.82767811754576,340.199704757318));
#19384=CARTESIAN_POINT('Ctrl Pts',(87.8493775042583,2.68849215345135,340.273004737115));
#19385=CARTESIAN_POINT('Ctrl Pts',(87.856801616395,2.5468113270224,340.340569504));
#19386=CARTESIAN_POINT('Ctrl Pts',(87.8606587415496,2.47320243353146,340.375672120597));
#19387=CARTESIAN_POINT('Ctrl Pts',(87.8645158667041,2.39892041910277,340.409227482542));
#19388=CARTESIAN_POINT('Ctrl Pts',(87.8683729918587,2.32403661171482,340.441211665604));
#19389=CARTESIAN_POINT('Ctrl Pts',(87.8757969692967,2.17990447333581,340.502773021255));
#19390=CARTESIAN_POINT('Ctrl Pts',(87.8832209467346,2.03310716920329,340.558696420712));
#19391=CARTESIAN_POINT('Ctrl Pts',(87.8906449241726,1.88412590285825,340.60874318762));
#19392=CARTESIAN_POINT('Ctrl Pts',(87.8980601402003,1.73532045682294,340.658730891814));
#19393=CARTESIAN_POINT('Ctrl Pts',(87.9054753562279,1.58433652928149,340.702855650617));
#19394=CARTESIAN_POINT('Ctrl Pts',(87.9128905722555,1.43167711524247,340.740925988043));
#19395=CARTESIAN_POINT('Ctrl Pts',(87.9202986533996,1.27916458932299,340.778959694383));
#19396=CARTESIAN_POINT('Ctrl Pts',(87.9277067345437,1.12498014608605,340.810950487196));
#19397=CARTESIAN_POINT('Ctrl Pts',(87.9351148156878,0.96964372945409,340.836756085398));
#19398=CARTESIAN_POINT('Ctrl Pts',(87.9425173828618,0.814422932553928,340.862542476022));
#19399=CARTESIAN_POINT('Ctrl Pts',(87.9499199500358,0.658052236124898,340.882152777878));
#19400=CARTESIAN_POINT('Ctrl Pts',(87.9573225172098,0.501063510710853,340.895495392309));
#19401=CARTESIAN_POINT('Ctrl Pts',(87.9647211869646,0.344157439174849,340.908830981911));
#19402=CARTESIAN_POINT('Ctrl Pts',(87.9721198567193,0.186634357620482,340.915905424529));
#19403=CARTESIAN_POINT('Ctrl Pts',(87.979518526474,0.0290329145482715,340.916678768733));
#19404=CARTESIAN_POINT('Ctrl Pts',(87.986915975678,-0.128542529179842,340.917451985358));
#19405=CARTESIAN_POINT('Ctrl Pts',(87.994313424882,-0.28619593592554,340.911926164783));
#19406=CARTESIAN_POINT('Ctrl Pts',(88.001710874086,-0.443386866669154,340.900113443737));
#19407=CARTESIAN_POINT('Ctrl Pts',(88.0091080025494,-0.600570981888055,
340.88830123487));
#19408=CARTESIAN_POINT('Ctrl Pts',(88.0165051310129,-0.757292288813252,
340.870202695496));
#19409=CARTESIAN_POINT('Ctrl Pts',(88.0239022594764,-0.913013954075224,
340.845881976414));
#19410=CARTESIAN_POINT('Ctrl Pts',(88.031300526913,-1.06875959658631,340.821557512548));
#19411=CARTESIAN_POINT('Ctrl Pts',(88.0386987943496,-1.22350492219589,340.791009018943));
#19412=CARTESIAN_POINT('Ctrl Pts',(88.0460970617862,-1.37672194028502,340.754352027956));
#19413=CARTESIAN_POINT('Ctrl Pts',(88.0534979283119,-1.52999278512387,340.717682158982));
#19414=CARTESIAN_POINT('Ctrl Pts',(88.0608987948377,-1.68173389071534,340.674899606769));
#19415=CARTESIAN_POINT('Ctrl Pts',(88.0682996613634,-1.83143125190803,340.626170112255));
#19416=CARTESIAN_POINT('Ctrl Pts',(88.0757086547482,-1.98129299511505,340.577387108098));
#19417=CARTESIAN_POINT('Ctrl Pts',(88.0831176481329,-2.12910615698859,340.522644235851));
#19418=CARTESIAN_POINT('Ctrl Pts',(88.0905266415177,-2.27437490003277,340.462156110603));
#19419=CARTESIAN_POINT('Ctrl Pts',(88.0979401990979,-2.41973313363353,340.401630722584));
#19420=CARTESIAN_POINT('Ctrl Pts',(88.1053537566782,-2.56254348731432,340.335353185837));
#19421=CARTESIAN_POINT('Ctrl Pts',(88.1127673142584,-2.7023341247331,340.263584409963));
#19422=CARTESIAN_POINT('Ctrl Pts',(88.1201914263951,-2.84232377971634,340.191713458097));
#19423=CARTESIAN_POINT('Ctrl Pts',(88.1276155385318,-2.9792848081739,340.114335836508));
#19424=CARTESIAN_POINT('Ctrl Pts',(88.1350396506685,-3.11277308690336,340.031756579163));
#19425=CARTESIAN_POINT('Ctrl Pts',(88.1388967758232,-3.18212562203004,339.988853330277));
#19426=CARTESIAN_POINT('Ctrl Pts',(88.1427539009779,-3.25054130207272,339.944546731359));
#19427=CARTESIAN_POINT('Ctrl Pts',(88.1466110261326,-3.31796140897478,339.898883816856));
#19428=CARTESIAN_POINT('Ctrl Pts',(88.1540056697473,-3.44721510000488,339.811341679741));
#19429=CARTESIAN_POINT('Ctrl Pts',(88.161400313362,-3.57320442184648,339.718543326015));
#19430=CARTESIAN_POINT('Ctrl Pts',(88.1687949569768,-3.69547034580423,339.620760704233));
#19431=CARTESIAN_POINT('Ctrl Pts',(88.1761808557596,-3.81759167929758,339.523093719206));
#19432=CARTESIAN_POINT('Ctrl Pts',(88.1835667545425,-3.93599808729685,339.420454430029));
#19433=CARTESIAN_POINT('Ctrl Pts',(88.1909526533253,-4.05025826768325,339.313158764475));
#19434=CARTESIAN_POINT('Ctrl Pts',(88.1983314614447,-4.16440875519343,339.205966105673));
#19435=CARTESIAN_POINT('Ctrl Pts',(88.2057102695642,-4.27442066581368,339.094126224688));
#19436=CARTESIAN_POINT('Ctrl Pts',(88.2130890776836,-4.37989476856159,338.977996025492));
#19437=CARTESIAN_POINT('Ctrl Pts',(88.2204624434414,-4.48529107714643,338.861951480037));
#19438=CARTESIAN_POINT('Ctrl Pts',(88.2278358091993,-4.58615598917958,338.741623193864));
#19439=CARTESIAN_POINT('Ctrl Pts',(88.2352091749572,-4.68212635611665,338.617405610083));
#19440=CARTESIAN_POINT('Ctrl Pts',(88.2428380268462,-4.78142208335221,338.488883903741));
#19441=CARTESIAN_POINT('Ctrl Pts',(88.2504668787353,-4.87547766557774,338.356198801304));
#19442=CARTESIAN_POINT('Ctrl Pts',(88.2580957306243,-4.96393512596535,338.219825869159));
#19443=CARTESIAN_POINT('Ctrl Pts',(88.2654641718353,-5.04937309304298,338.088108023816));
#19444=CARTESIAN_POINT('Ctrl Pts',(88.2728326130462,-5.12958862495197,337.952950321232));
#19445=CARTESIAN_POINT('Ctrl Pts',(88.2802010542572,-5.20430267079867,337.814811587517));
#19446=CARTESIAN_POINT('Ctrl Pts',(88.2875693652775,-5.27901539654684,337.676675294531));
#19447=CARTESIAN_POINT('Ctrl Pts',(88.2949376762978,-5.34822665016277,337.535558406234));
#19448=CARTESIAN_POINT('Ctrl Pts',(88.3023059873182,-5.41170317014393,337.391944681792));
#19449=CARTESIAN_POINT('Ctrl Pts',(88.3096756524486,-5.47519135551132,337.248304564763));
#19450=CARTESIAN_POINT('Ctrl Pts',(88.3170453175789,-5.53294255713081,337.102167042566));
#19451=CARTESIAN_POINT('Ctrl Pts',(88.3244149827093,-5.58477160117974,336.954036009176));
#19452=CARTESIAN_POINT('Ctrl Pts',(88.331787486827,-5.63662061112845,336.805847911848));
#19453=CARTESIAN_POINT('Ctrl Pts',(88.3391599909446,-5.68254279796302,336.655665129711));
#19454=CARTESIAN_POINT('Ctrl Pts',(88.3465324950622,-5.72240285811786,336.504006679475));
#19455=CARTESIAN_POINT('Ctrl Pts',(88.3539130925853,-5.76230667594628,336.352181741256));
#19456=CARTESIAN_POINT('Ctrl Pts',(88.3612936901084,-5.79613498510369,336.198878264866));
#19457=CARTESIAN_POINT('Ctrl Pts',(88.3686742876315,-5.82380348353425,336.044626032451));
#19458=CARTESIAN_POINT('Ctrl Pts',(88.3760597134761,-5.85149008245112,335.890272889594));
#19459=CARTESIAN_POINT('Ctrl Pts',(88.3834451393207,-5.87300879162604,335.734970125933));
#19460=CARTESIAN_POINT('Ctrl Pts',(88.3908305651652,-5.88832723993724,335.579251998627));
#19461=CARTESIAN_POINT('Ctrl Pts',(88.3982258965774,-5.90366623383771,335.423325017224));
#19462=CARTESIAN_POINT('Ctrl Pts',(88.4056212279896,-5.91278834517379,335.266981934148));
#19463=CARTESIAN_POINT('Ctrl Pts',(88.4130165594018,-5.91571326754579,335.110756935145));
#19464=CARTESIAN_POINT('Ctrl Pts',(88.4147782463659,-5.91641003112903,335.073541626069));
#19465=CARTESIAN_POINT('Ctrl Pts',(88.4165399333301,-5.91675535479303,335.03633299364));
#19466=CARTESIAN_POINT('Ctrl Pts',(88.4183016202943,-5.91674993723816,334.999138204092));
#19467=CARTESIAN_POINT('',(90.1683016202942,-5.91477476057368,335.005386709628));
#19468=CARTESIAN_POINT('Ctrl Pts',(88.4183016202943,-5.92634586416711,334.999136806411));
#19469=CARTESIAN_POINT('Ctrl Pts',(88.4204841003317,-5.92643975629784,334.952982996016));
#19470=CARTESIAN_POINT('Ctrl Pts',(88.4226665803691,-5.9259473617588,334.906831241244));
#19471=CARTESIAN_POINT('Ctrl Pts',(88.5175950718312,-5.87876314062022,332.900034320683));
#19472=CARTESIAN_POINT('Ctrl Pts',(88.7030870946803,-3.64692550512862,329.029023758107));
#19473=CARTESIAN_POINT('Ctrl Pts',(88.9813251289543,3.0475606556344,328.70198467996));
#19474=CARTESIAN_POINT('Ctrl Pts',(89.2595631632284,6.94534538464283,334.154541302462));
#19475=CARTESIAN_POINT('Ctrl Pts',(89.5378011975022,4.46948916729357,340.382962892745));
#19476=CARTESIAN_POINT('Ctrl Pts',(89.8160392317763,-2.10795128932855,341.671518888756));
#19477=CARTESIAN_POINT('Ctrl Pts',(90.0262060393735,-5.61504000227453,338.020314320455));
#19478=CARTESIAN_POINT('Ctrl Pts',(90.1436268355462,-5.91942493170759,335.529848181018));
#19479=CARTESIAN_POINT('Ctrl Pts',(90.1683016202942,-5.91477476057368,335.005386709628));
#19480=CARTESIAN_POINT('',(91.9183016202943,-5.90746550964324,334.998215606661));
#19481=CARTESIAN_POINT('Ctrl Pts',(90.1683016202942,-5.91477476057368,335.005386709628));
#19482=CARTESIAN_POINT('Ctrl Pts',(90.2363728469709,-5.90194616423239,333.558535761722));
#19483=CARTESIAN_POINT('Ctrl Pts',(90.3971900850721,-4.63796763427977,330.120318055911));
#19484=CARTESIAN_POINT('Ctrl Pts',(90.6507533345981,1.12431756930355,328.094311553177));
#19485=CARTESIAN_POINT('Ctrl Pts',(90.9289913688719,6.4155734914137,332.208398363396));
#19486=CARTESIAN_POINT('Ctrl Pts',(91.2072294031458,5.81935231416251,338.884296791552));
#19487=CARTESIAN_POINT('Ctrl Pts',(91.4854674374199,-0.117202588295501,
341.995633386228));
#19488=CARTESIAN_POINT('Ctrl Pts',(91.7224915098026,-5.08278279076532,339.177244506712));
#19489=CARTESIAN_POINT('Ctrl Pts',(91.8667695707608,-5.90450367428727,336.096942434057));
#19490=CARTESIAN_POINT('Ctrl Pts',(91.9183016202943,-5.90746550964324,334.998215606661));
#19491=CARTESIAN_POINT('',(93.6683016202942,-5.92133609402893,334.995342413241));
#19492=CARTESIAN_POINT('Ctrl Pts',(91.9183016202943,-5.90746550964324,334.998215606661));
#19493=CARTESIAN_POINT('Ctrl Pts',(91.9595155821854,-5.90983430674317,334.119483128464));
#19494=CARTESIAN_POINT('Ctrl Pts',(92.0934755555012,-5.31350020957016,331.266347748298));
#19495=CARTESIAN_POINT('Ctrl Pts',(92.3201815402416,-0.892360157151169,
328.060524784164));
#19496=CARTESIAN_POINT('Ctrl Pts',(92.5984195745155,5.35264547155506,330.494247079894));
#19497=CARTESIAN_POINT('Ctrl Pts',(92.8766576087896,6.68560735593236,337.062832325594));
#19498=CARTESIAN_POINT('Ctrl Pts',(93.1548956430633,1.88328604917356,341.738386793456));
#19499=CARTESIAN_POINT('Ctrl Pts',(93.4187769802319,-4.31032992291039,340.308042313538));
#19500=CARTESIAN_POINT('Ctrl Pts',(93.5899123059753,-5.90699168792046,336.656767378768));
#19501=CARTESIAN_POINT('Ctrl Pts',(93.6683016202942,-5.92133609402893,334.995342413241));
#19502=CARTESIAN_POINT('',(95.4183016202943,-5.92241488864615,335.004254353173));
#19503=CARTESIAN_POINT('Ctrl Pts',(93.6683016202942,-5.92133609402893,334.995342413241));
#19504=CARTESIAN_POINT('Ctrl Pts',(93.6826583173999,-5.9239632160474,334.691058912344));
#19505=CARTESIAN_POINT('Ctrl Pts',(93.7897610259302,-5.76414273014026,332.423834031691));
#19506=CARTESIAN_POINT('Ctrl Pts',(93.9896097458853,-2.83487969874721,328.603432169137));
#19507=CARTESIAN_POINT('Ctrl Pts',(94.2678477801593,3.844894283409,329.15453929355));
#19508=CARTESIAN_POINT('Ctrl Pts',(94.546085814433,6.99626553222726,335.069939429418));
#19509=CARTESIAN_POINT('Ctrl Pts',(94.8243238487073,3.72726716683056,340.921157183209));
#19510=CARTESIAN_POINT('Ctrl Pts',(95.1025618829809,-2.96218926319552,341.338616386109));
#19511=CARTESIAN_POINT('Ctrl Pts',(95.30055447351,-5.78800059838624,337.496437496031));
#19512=CARTESIAN_POINT('Ctrl Pts',(95.4058010526145,-5.92456336273099,335.269072437427));
#19513=CARTESIAN_POINT('Ctrl Pts',(95.4183016202943,-5.92241488864615,335.004254353173));
#19514=CARTESIAN_POINT('',(97.1683016202942,-5.90788275435609,335.002389220978));
#19515=CARTESIAN_POINT('Ctrl Pts',(95.4183016202943,-5.92241488864615,335.004254353173));
#19516=CARTESIAN_POINT('Ctrl Pts',(95.4985470640392,-5.90862309448696,333.304295981126));
#19517=CARTESIAN_POINT('Ctrl Pts',(95.6715385192085,-4.24711155794473,329.616037147329));
#19518=CARTESIAN_POINT('Ctrl Pts',(95.9372759858029,2.01761921385354,328.300609309115));
#19519=CARTESIAN_POINT('Ctrl Pts',(96.2155140200769,6.72551008477971,333.071234327155));
#19520=CARTESIAN_POINT('Ctrl Pts',(96.4937520543506,5.26149961926853,339.611859134628));
#19521=CARTESIAN_POINT('Ctrl Pts',(96.7719900886248,-1.03091138723976,341.920248885184));
#19522=CARTESIAN_POINT('Ctrl Pts',(96.9968399439392,-5.35141349029995,338.653647685618));
#19523=CARTESIAN_POINT('Ctrl Pts',(97.128943787829,-5.91092380235256,335.841398759276));
#19524=CARTESIAN_POINT('Ctrl Pts',(97.1683016202942,-5.90788275435609,335.002389220978));
#19525=CARTESIAN_POINT('',(98.9183016202944,-5.91363949802178,334.994757320841));
#19526=CARTESIAN_POINT('Ctrl Pts',(97.1683016202942,-5.90788275435609,335.002389220978));
#19527=CARTESIAN_POINT('Ctrl Pts',(97.2216897992537,-5.90375762844111,333.864288147476));
#19528=CARTESIAN_POINT('Ctrl Pts',(97.3678239896376,-5.03757698457894,330.743267499416));
#19529=CARTESIAN_POINT('Ctrl Pts',(97.6067041914465,0.0226730784917184,
328.003421632488));
#19530=CARTESIAN_POINT('Ctrl Pts',(97.8849422257205,5.89584171844692,331.23281625717));
#19531=CARTESIAN_POINT('Ctrl Pts',(98.1631802599943,6.35848343586405,337.919299799106));
#19532=CARTESIAN_POINT('Ctrl Pts',(98.4414182942685,0.986038755248901,341.926785004198));
#19533=CARTESIAN_POINT('Ctrl Pts',(98.6931254143681,-4.69271617403346,339.801658490069));
#19534=CARTESIAN_POINT('Ctrl Pts',(98.8520865230436,-5.90167453875089,336.402842058547));
#19535=CARTESIAN_POINT('Ctrl Pts',(98.9183016202944,-5.91363949802178,334.994757320841));
#19536=CARTESIAN_POINT('',(100.668301620294,-5.92209910998399,335.000129634886));
#19537=CARTESIAN_POINT('Ctrl Pts',(98.9183016202944,-5.91363949802178,334.994757320841));
#19538=CARTESIAN_POINT('Ctrl Pts',(98.9448325344683,-5.91843359061835,334.430569139038));
#19539=CARTESIAN_POINT('Ctrl Pts',(99.064109460067,-5.58514965359588,331.89965766233));
#19540=CARTESIAN_POINT('Ctrl Pts',(99.2761323970899,-1.97415726733455,328.287673577286));
#19541=CARTESIAN_POINT('Ctrl Pts',(99.5543704313643,4.57620871558837,329.707464056562));
#19542=CARTESIAN_POINT('Ctrl Pts',(99.8326084656378,6.92705550494563,335.984136653425));
#19543=CARTESIAN_POINT('Ctrl Pts',(100.110846499912,2.92104570058681,341.357681569276));
#19544=CARTESIAN_POINT('Ctrl Pts',(100.389084534186,-3.7655646286397,340.896875948225));
#19545=CARTESIAN_POINT('Ctrl Pts',(100.574902907646,-5.92335917044606,336.975133811572));
#19546=CARTESIAN_POINT('Ctrl Pts',(100.667975269683,-5.92649868725284,335.007030730633));
#19547=CARTESIAN_POINT('Ctrl Pts',(100.668301620294,-5.9264964672619,335.000129731144));
#19548=CARTESIAN_POINT('',(102.418301603228,-5.91452397649362,335.005174647363));
#19549=CARTESIAN_POINT('Ctrl Pts',(100.668301620294,-5.91674999858243,335.000129517794));
#19550=CARTESIAN_POINT('Ctrl Pts',(100.675720896014,-5.91675342721131,334.843499765313));
#19551=CARTESIAN_POINT('Ctrl Pts',(100.683140171735,-5.91053304525965,334.686632128746));
#19552=CARTESIAN_POINT('Ctrl Pts',(100.690559447455,-5.89805807963226,334.530062289463));
#19553=CARTESIAN_POINT('Ctrl Pts',(100.697969965162,-5.88559783996035,334.37367727157));
#19554=CARTESIAN_POINT('Ctrl Pts',(100.705380482868,-5.86689774197576,334.21758972017));
#19555=CARTESIAN_POINT('Ctrl Pts',(100.712791000575,-5.84197897812579,334.062336850657));
#19556=CARTESIAN_POINT('Ctrl Pts',(100.720194391435,-5.81708417915823,333.907233290988));
#19557=CARTESIAN_POINT('Ctrl Pts',(100.727597782296,-5.78598267919092,333.752963181704));
#19558=CARTESIAN_POINT('Ctrl Pts',(100.735001173157,-5.74874757126554,333.600060028298));
#19559=CARTESIAN_POINT('Ctrl Pts',(100.742399062695,-5.71154013205687,333.447270494384));
#19560=CARTESIAN_POINT('Ctrl Pts',(100.749796952234,-5.66820824793961,333.295846255444));
#19561=CARTESIAN_POINT('Ctrl Pts',(100.757194841772,-5.61887630923833,333.146311896791));
#19562=CARTESIAN_POINT('Ctrl Pts',(100.764588851133,-5.56957024503566,332.996855968595));
#19563=CARTESIAN_POINT('Ctrl Pts',(100.771982860494,-5.51427051040527,332.849288300652));
#19564=CARTESIAN_POINT('Ctrl Pts',(100.779376869855,-5.45315165777585,332.704119436949));
#19565=CARTESIAN_POINT('Ctrl Pts',(100.786769683007,-5.39204269301176,332.5589740588));
#19566=CARTESIAN_POINT('Ctrl Pts',(100.794162496158,-5.32511662334934,332.416227058893));
#19567=CARTESIAN_POINT('Ctrl Pts',(100.801555309309,-5.25259660839953,332.276370173476));
#19568=CARTESIAN_POINT('Ctrl Pts',(100.808947825895,-5.1800795026167,332.136518898469));
#19569=CARTESIAN_POINT('Ctrl Pts',(100.816340342481,-5.10196906974435,331.999557839246));
#19570=CARTESIAN_POINT('Ctrl Pts',(100.823732859067,-5.01853488551264,331.865954983509));
#19571=CARTESIAN_POINT('Ctrl Pts',(100.831126542949,-4.93508752681557,331.732331031549));
#19572=CARTESIAN_POINT('Ctrl Pts',(100.838520226832,-4.84631494099473,331.602066655894));
#19573=CARTESIAN_POINT('Ctrl Pts',(100.845913910714,-4.75253047668514,331.475601522149));
#19574=CARTESIAN_POINT('Ctrl Pts',(100.85331022618,-4.6587126323147,331.349091376537));
#19575=CARTESIAN_POINT('Ctrl Pts',(100.860706541646,-4.55987958041388,331.226383465064));
#19576=CARTESIAN_POINT('Ctrl Pts',(100.868102857112,-4.45638533814684,331.10788485776));
#19577=CARTESIAN_POINT('Ctrl Pts',(100.875507300596,-4.35277736315245,330.989256029012));
#19578=CARTESIAN_POINT('Ctrl Pts',(100.88291174408,-4.24449821463794,330.874846023532));
#19579=CARTESIAN_POINT('Ctrl Pts',(100.890316187565,-4.13193969584835,330.765025984451));
#19580=CARTESIAN_POINT('Ctrl Pts',(100.897725232323,-4.01931123086899,330.655137700929));
#19581=CARTESIAN_POINT('Ctrl Pts',(100.905134277082,-3.90239837387915,330.549845316645));
#19582=CARTESIAN_POINT('Ctrl Pts',(100.91254332184,-3.78162604762161,330.449479700249));
#19583=CARTESIAN_POINT('Ctrl Pts',(100.919962843036,-3.66068294852313,330.34897216623));
#19584=CARTESIAN_POINT('Ctrl Pts',(100.927382364231,-3.53586977740861,330.253405539145));
#19585=CARTESIAN_POINT('Ctrl Pts',(100.934801885426,-3.40764109227606,330.163067837076));
#19586=CARTESIAN_POINT('Ctrl Pts',(100.938388124529,-3.34566152343086,330.119402944006));
#19587=CARTESIAN_POINT('Ctrl Pts',(100.941974363632,-3.2828843764741,330.076959000909));
#19588=CARTESIAN_POINT('Ctrl Pts',(100.945560602734,-3.21936296038802,330.035764641782));
#19589=CARTESIAN_POINT('Ctrl Pts',(100.952984580172,-3.0878654371213,329.950487005804));
#19590=CARTESIAN_POINT('Ctrl Pts',(100.96040855761,-2.95277882722675,329.870309185089));
#19591=CARTESIAN_POINT('Ctrl Pts',(100.967832535048,-2.81453648987602,329.795548548631));
#19592=CARTESIAN_POINT('Ctrl Pts',(100.975247751076,-2.67645729928305,329.720876140972));
#19593=CARTESIAN_POINT('Ctrl Pts',(100.982662967104,-2.53523011946853,329.651608367824));
#19594=CARTESIAN_POINT('Ctrl Pts',(100.990078183131,-2.39131784369694,329.588019814068));
#19595=CARTESIAN_POINT('Ctrl Pts',(100.997486264275,-2.24754403959239,329.524492444899));
#19596=CARTESIAN_POINT('Ctrl Pts',(101.004894345419,-2.10109062205886,329.466633566117));
#19597=CARTESIAN_POINT('Ctrl Pts',(101.012302426563,-1.95244558778982,329.414672186056));
#19598=CARTESIAN_POINT('Ctrl Pts',(101.019704993737,-1.8039111927349,329.362749481799));
#19599=CARTESIAN_POINT('Ctrl Pts',(101.027107560911,-1.65318877981853,329.316715658526));
#19600=CARTESIAN_POINT('Ctrl Pts',(101.034510128085,-1.50078675479425,329.276751824433));
#19601=CARTESIAN_POINT('Ctrl Pts',(101.04190879784,-1.34846496877008,329.236809031124));
#19602=CARTESIAN_POINT('Ctrl Pts',(101.049307467595,-1.19446569188727,329.202929956752));
#19603=CARTESIAN_POINT('Ctrl Pts',(101.05670613735,-1.03931283078175,329.175245979248));
#19604=CARTESIAN_POINT('Ctrl Pts',(101.064103586553,-0.884185565080336,
329.14756656874));
#19605=CARTESIAN_POINT('Ctrl Pts',(101.071501035757,-0.727905459902505,
329.126080292255));
#19606=CARTESIAN_POINT('Ctrl Pts',(101.078898484961,-0.571007083957664,
329.110867511036));
#19607=CARTESIAN_POINT('Ctrl Pts',(101.086295613425,-0.414115510852758,
329.095655389416));
#19608=CARTESIAN_POINT('Ctrl Pts',(101.093692741888,-0.256606091751522,
329.086716258238));
#19609=CARTESIAN_POINT('Ctrl Pts',(101.101089870352,-0.0990187279253847,
329.084078613266));
#19610=CARTESIAN_POINT('Ctrl Pts',(101.108488137788,0.0585929004215468,
329.081440562162));
#19611=CARTESIAN_POINT('Ctrl Pts',(101.115886405225,0.216282124208303,329.085105935448));
#19612=CARTESIAN_POINT('Ctrl Pts',(101.123284672662,0.373508977772477,329.095051092006));
#19613=CARTESIAN_POINT('Ctrl Pts',(101.130685539187,0.530791066783069,329.104999742401));
#19614=CARTESIAN_POINT('Ctrl Pts',(101.138086405713,0.687610089929971,329.121232544971));
#19615=CARTESIAN_POINT('Ctrl Pts',(101.145487272239,0.843431284659256,329.143673998951));
#19616=CARTESIAN_POINT('Ctrl Pts',(101.152896265623,0.999423585957447,329.166140095794));
#19617=CARTESIAN_POINT('Ctrl Pts',(101.160305259008,1.15441550102438,329.194828406111));
#19618=CARTESIAN_POINT('Ctrl Pts',(101.167714252393,1.30788181908319,329.229612169896));
#19619=CARTESIAN_POINT('Ctrl Pts',(101.175127809973,1.46144267768766,329.26441736168));
#19620=CARTESIAN_POINT('Ctrl Pts',(101.182541367553,1.61347570701675,329.305325392538));
#19621=CARTESIAN_POINT('Ctrl Pts',(101.189954925134,1.76347143648926,329.352159788451));
#19622=CARTESIAN_POINT('Ctrl Pts',(101.19737903727,1.91368071234296,329.399060861701));
#19623=CARTESIAN_POINT('Ctrl Pts',(101.204803149407,2.06184654494781,329.451905025877));
#19624=CARTESIAN_POINT('Ctrl Pts',(101.212227261544,2.20747923205516,329.510467597095));
#19625=CARTESIAN_POINT('Ctrl Pts',(101.216084386698,2.28314127627484,329.54089321061));
#19626=CARTESIAN_POINT('Ctrl Pts',(101.219941511853,2.35811996050561,329.572861583952));
#19627=CARTESIAN_POINT('Ctrl Pts',(101.223798637008,2.43234939516805,329.606336404416));
#19628=CARTESIAN_POINT('Ctrl Pts',(101.231222614445,2.57522203374634,329.67076685505));
#19629=CARTESIAN_POINT('Ctrl Pts',(101.238646591883,2.71574838958606,329.740975247866));
#19630=CARTESIAN_POINT('Ctrl Pts',(101.246070569321,2.85342706481585,329.816768908463));
#19631=CARTESIAN_POINT('Ctrl Pts',(101.253485785349,2.99094325849408,329.892473121137));
#19632=CARTESIAN_POINT('Ctrl Pts',(101.260901001377,3.12561813730881,329.973749302958));
#19633=CARTESIAN_POINT('Ctrl Pts',(101.268316217404,3.25697029886916,330.06035679074));
#19634=CARTESIAN_POINT('Ctrl Pts',(101.275724298548,3.38819607404093,330.146880945234));
#19635=CARTESIAN_POINT('Ctrl Pts',(101.283132379693,3.51610518729618,330.238725989234));
#19636=CARTESIAN_POINT('Ctrl Pts',(101.290540460837,3.64024097762993,330.335605485459));
#19637=CARTESIAN_POINT('Ctrl Pts',(101.297943028011,3.76428437142794,330.432412872505));
#19638=CARTESIAN_POINT('Ctrl Pts',(101.305345595185,3.88455974158668,330.534247021855));
#19639=CARTESIAN_POINT('Ctrl Pts',(101.312748162359,4.00063966283354,330.640778412301));
#19640=CARTESIAN_POINT('Ctrl Pts',(101.320146832113,4.1166584685091,330.747253714435));
#19641=CARTESIAN_POINT('Ctrl Pts',(101.327545501868,4.22848595012491,330.858421080673));
#19642=CARTESIAN_POINT('Ctrl Pts',(101.334944171623,4.33572811323378,330.973911042884));
#19643=CARTESIAN_POINT('Ctrl Pts',(101.342341620827,4.4429525847157,331.089381952837));
#19644=CARTESIAN_POINT('Ctrl Pts',(101.349739070031,4.54559298526312,331.209173770283));
#19645=CARTESIAN_POINT('Ctrl Pts',(101.357136519235,4.64329245159145,331.332880453068));
#19646=CARTESIAN_POINT('Ctrl Pts',(101.364533647698,4.74098768184118,331.456581772146));
#19647=CARTESIAN_POINT('Ctrl Pts',(101.371930776162,4.83374217252105,331.584197326176));
#19648=CARTESIAN_POINT('Ctrl Pts',(101.379327904625,4.92123978937726,331.715288521354));
#19649=CARTESIAN_POINT('Ctrl Pts',(101.386726172062,5.00875087868236,331.846399901303));
#19650=CARTESIAN_POINT('Ctrl Pts',(101.394124439498,5.0910032752848,331.980987677541));
#19651=CARTESIAN_POINT('Ctrl Pts',(101.401522706935,5.16772465310335,332.118584987856));
#19652=CARTESIAN_POINT('Ctrl Pts',(101.408923573461,5.24447298394842,332.256230637553));
#19653=CARTESIAN_POINT('Ctrl Pts',(101.416324439987,5.31568624565405,332.396887600612));
#19654=CARTESIAN_POINT('Ctrl Pts',(101.423725306512,5.3811385377205,332.540065325998));
#19655=CARTESIAN_POINT('Ctrl Pts',(101.431134299897,5.44666270266144,332.683400274215));
#19656=CARTESIAN_POINT('Ctrl Pts',(101.438543293282,5.50641310915466,332.829261173049));
#19657=CARTESIAN_POINT('Ctrl Pts',(101.445952286667,5.56021213070599,332.977137764441));
#19658=CARTESIAN_POINT('Ctrl Pts',(101.453365844247,5.61404429431039,333.125105452914));
#19659=CARTESIAN_POINT('Ctrl Pts',(101.460779401827,5.66191765425009,333.27509095356));
#19660=CARTESIAN_POINT('Ctrl Pts',(101.468192959407,5.7037049075299,333.426570341477));
#19661=CARTESIAN_POINT('Ctrl Pts',(101.475617071544,5.74555165261478,333.578265388035));
#19662=CARTESIAN_POINT('Ctrl Pts',(101.483041183681,5.78129490135454,333.731458207084));
#19663=CARTESIAN_POINT('Ctrl Pts',(101.490465295817,5.81085858923555,333.885615408215));
#19664=CARTESIAN_POINT('Ctrl Pts',(101.494322420972,5.82621811534386,333.965706280676));
#19665=CARTESIAN_POINT('Ctrl Pts',(101.498179546127,5.83991049649889,334.04605737701));
#19666=CARTESIAN_POINT('Ctrl Pts',(101.502036671282,5.85193061219721,334.126593638374));
#19667=CARTESIAN_POINT('Ctrl Pts',(101.50946064872,5.8750662544607,334.281605302065));
#19668=CARTESIAN_POINT('Ctrl Pts',(101.516884626158,5.89207339365728,334.437770702599));
#19669=CARTESIAN_POINT('Ctrl Pts',(101.524308603596,5.90284271864182,334.594563936635));
#19670=CARTESIAN_POINT('Ctrl Pts',(101.531723819624,5.91359933420257,334.751172131063));
#19671=CARTESIAN_POINT('Ctrl Pts',(101.539139035651,5.91813276352719,334.908406315432));
#19672=CARTESIAN_POINT('Ctrl Pts',(101.546554251679,5.91638487096705,335.06573143154));
#19673=CARTESIAN_POINT('Ctrl Pts',(101.553962332823,5.91463866022033,335.222905170212));
#19674=CARTESIAN_POINT('Ctrl Pts',(101.561370413967,5.90662316389853,335.380169295746));
#19675=CARTESIAN_POINT('Ctrl Pts',(101.568778495111,5.89233212774909,335.536984784511));
#19676=CARTESIAN_POINT('Ctrl Pts',(101.576181062285,5.87805172867886,335.693683552643));
#19677=CARTESIAN_POINT('Ctrl Pts',(101.583583629459,5.85750512414643,335.849933978827));
#19678=CARTESIAN_POINT('Ctrl Pts',(101.590986196633,5.83073811122401,336.005198309201));
#19679=CARTESIAN_POINT('Ctrl Pts',(101.598384866388,5.80398519101701,336.160380893582));
#19680=CARTESIAN_POINT('Ctrl Pts',(101.605783536143,5.77101844805768,336.31457804926));
#19681=CARTESIAN_POINT('Ctrl Pts',(101.613182205897,5.73193536297641,336.467258517495));
#19682=CARTESIAN_POINT('Ctrl Pts',(101.620579655101,5.69285872539041,336.619913798193));
#19683=CARTESIAN_POINT('Ctrl Pts',(101.627977104305,5.64766784069477,336.771052526824));
#19684=CARTESIAN_POINT('Ctrl Pts',(101.635374553509,5.5965110391987,336.920154876729));
#19685=CARTESIAN_POINT('Ctrl Pts',(101.642771681973,5.54535645577246,337.069250761817));
#19686=CARTESIAN_POINT('Ctrl Pts',(101.650168810436,5.48823659098824,337.216310090724));
#19687=CARTESIAN_POINT('Ctrl Pts',(101.6575659389,5.42534918934841,337.36082967114));
#19688=CARTESIAN_POINT('Ctrl Pts',(101.664964206336,5.36245210461861,337.505371503964));
#19689=CARTESIAN_POINT('Ctrl Pts',(101.672362473773,5.29378586371869,337.647372467412));
#19690=CARTESIAN_POINT('Ctrl Pts',(101.67976074121,5.21959568977386,337.786350910742));
#19691=CARTESIAN_POINT('Ctrl Pts',(101.687161607735,5.14537945204099,337.92537817866));
#19692=CARTESIAN_POINT('Ctrl Pts',(101.694562474261,5.06563559314468,338.061380483303));
#19693=CARTESIAN_POINT('Ctrl Pts',(101.701963340787,4.9806543801937,338.193902394808));
#19694=CARTESIAN_POINT('Ctrl Pts',(101.709372334171,4.89557984974584,338.326569828041));
#19695=CARTESIAN_POINT('Ctrl Pts',(101.716781327556,4.80525668154069,338.455748921437));
#19696=CARTESIAN_POINT('Ctrl Pts',(101.724190320941,4.71001783857872,338.58101417517));
#19697=CARTESIAN_POINT('Ctrl Pts',(101.731603878521,4.61472032520421,338.706356596621));
#19698=CARTESIAN_POINT('Ctrl Pts',(101.739017436102,4.51450133994696,338.827780086893));
#19699=CARTESIAN_POINT('Ctrl Pts',(101.746430993682,4.40973257147745,338.944894068356));
#19700=CARTESIAN_POINT('Ctrl Pts',(101.753855105819,4.30481464548585,339.062174783012));
#19701=CARTESIAN_POINT('Ctrl Pts',(101.761279217955,4.19533425856126,339.175133468016));
#19702=CARTESIAN_POINT('Ctrl Pts',(101.768703330092,4.08169878720654,339.283417510939));
#19703=CARTESIAN_POINT('Ctrl Pts',(101.772560455246,4.0226605848,339.339675430823));
#19704=CARTESIAN_POINT('Ctrl Pts',(101.776417580401,3.96250136679259,339.394672235018));
#19705=CARTESIAN_POINT('Ctrl Pts',(101.780274705556,3.90128148076729,339.448362998938));
#19706=CARTESIAN_POINT('Ctrl Pts',(101.787698682994,3.78344888929231,339.551703959885));
#19707=CARTESIAN_POINT('Ctrl Pts',(101.795122660432,3.66132961123008,339.650515685064));
#19708=CARTESIAN_POINT('Ctrl Pts',(101.80254663787,3.53530673538617,339.744421655927));
#19709=CARTESIAN_POINT('Ctrl Pts',(101.809961853897,3.409432585497,339.838216803616));
#19710=CARTESIAN_POINT('Ctrl Pts',(101.817377069925,3.27966430415399,339.927117500308));
#19711=CARTESIAN_POINT('Ctrl Pts',(101.824792285952,3.14642037267739,340.010785307804));
#19712=CARTESIAN_POINT('Ctrl Pts',(101.832200367096,3.01330464784049,340.094372610556));
#19713=CARTESIAN_POINT('Ctrl Pts',(101.839608448241,2.8767202446077,340.172736850836));
#19714=CARTESIAN_POINT('Ctrl Pts',(101.847016529385,2.73711705491418,340.245581072693));
#19715=CARTESIAN_POINT('Ctrl Pts',(101.854419096559,2.59761777442511,340.318371075266));
#19716=CARTESIAN_POINT('Ctrl Pts',(101.861821663733,2.45510451091457,340.385649068427));
#19717=CARTESIAN_POINT('Ctrl Pts',(101.869224230907,2.31005425650241,340.447162554442));
#19718=CARTESIAN_POINT('Ctrl Pts',(101.876622900661,2.16508037041392,340.508643653876));
#19719=CARTESIAN_POINT('Ctrl Pts',(101.884021570416,2.01757249630441,340.564366145176));
#19720=CARTESIAN_POINT('Ctrl Pts',(101.891420240171,1.86803013334616,340.614124507295));
#19721=CARTESIAN_POINT('Ctrl Pts',(101.898817689375,1.718512440235,340.66387466083));
#19722=CARTESIAN_POINT('Ctrl Pts',(101.906215138579,1.56696127816549,340.707662520184));
#19723=CARTESIAN_POINT('Ctrl Pts',(101.913612587783,1.41389405050521,340.745331511449));
#19724=CARTESIAN_POINT('Ctrl Pts',(101.921009716246,1.26083345957339,340.782998869451));
#19725=CARTESIAN_POINT('Ctrl Pts',(101.92840684471,1.10625729615029,340.81454779769));
#19726=CARTESIAN_POINT('Ctrl Pts',(101.935803973173,0.950695716283353,340.839872277502));
#19727=CARTESIAN_POINT('Ctrl Pts',(101.94320224061,0.795110183815789,340.865200656652));
#19728=CARTESIAN_POINT('Ctrl Pts',(101.950600508046,0.638539301175376,340.884302619085));
#19729=CARTESIAN_POINT('Ctrl Pts',(101.957998775483,0.481520803051217,340.897123729305));
#19730=CARTESIAN_POINT('Ctrl Pts',(101.965399642009,0.324447142677535,340.909949343715));
#19731=CARTESIAN_POINT('Ctrl Pts',(101.972800508535,0.166925925470569,340.916489682361));
#19732=CARTESIAN_POINT('Ctrl Pts',(101.98020137506,0.00949721230621073,
340.916742377817));
#19733=CARTESIAN_POINT('Ctrl Pts',(101.987610368445,-0.148104372635867,
340.916995350757));
#19734=CARTESIAN_POINT('Ctrl Pts',(101.99501936183,-0.305612877244675,340.910946891384));
#19735=CARTESIAN_POINT('Ctrl Pts',(102.002428355215,-0.462490304256098,
340.89864673302));
#19736=CARTESIAN_POINT('Ctrl Pts',(102.009841912795,-0.619464373174623,
340.886338997334));
#19737=CARTESIAN_POINT('Ctrl Pts',(102.017255470375,-0.77580622008791,340.867771932418));
#19738=CARTESIAN_POINT('Ctrl Pts',(102.024669027955,-0.930986257866573,
340.843046735237));
#19739=CARTESIAN_POINT('Ctrl Pts',(102.032093140092,-1.08638722283786,340.818286337211));
#19740=CARTESIAN_POINT('Ctrl Pts',(102.039517252229,-1.24062271027355,340.787350370209));
#19741=CARTESIAN_POINT('Ctrl Pts',(102.046941364365,-1.39317574605814,340.750390587003));
#19742=CARTESIAN_POINT('Ctrl Pts',(102.05079848952,-1.47243319003586,340.731188491602));
#19743=CARTESIAN_POINT('Ctrl Pts',(102.054655614675,-1.55123678079143,340.710361248204));
#19744=CARTESIAN_POINT('Ctrl Pts',(102.05851273983,-1.6295160827416,340.687935293108));
#19745=CARTESIAN_POINT('Ctrl Pts',(102.065936717268,-1.78018367796471,340.64477107676));
#19746=CARTESIAN_POINT('Ctrl Pts',(102.073360694706,-1.92936231428572,340.595551064847));
#19747=CARTESIAN_POINT('Ctrl Pts',(102.080784672144,-2.07652805789086,340.540393649127));
#19748=CARTESIAN_POINT('Ctrl Pts',(102.088199888171,-2.22352012377637,340.485301327457));
#19749=CARTESIAN_POINT('Ctrl Pts',(102.095615104199,-2.36850367937562,340.424285679292));
#19750=CARTESIAN_POINT('Ctrl Pts',(102.103030320227,-2.51096766053026,340.357515466172));
#19751=CARTESIAN_POINT('Ctrl Pts',(102.110438401371,-2.65329456355895,340.290809499015));
#19752=CARTESIAN_POINT('Ctrl Pts',(102.117846482515,-2.79310638283807,340.218360147391));
#19753=CARTESIAN_POINT('Ctrl Pts',(102.125254563659,-2.92990993943325,340.140385035122));
#19754=CARTESIAN_POINT('Ctrl Pts',(102.132657130833,-3.06661167064293,340.062467961154));
#19755=CARTESIAN_POINT('Ctrl Pts',(102.140059698007,-3.20030927470092,339.979033499991));
#19756=CARTESIAN_POINT('Ctrl Pts',(102.147462265181,-3.33053229306776,339.890346123469));
#19757=CARTESIAN_POINT('Ctrl Pts',(102.154860934935,-3.46068674958587,339.801705440463));
#19758=CARTESIAN_POINT('Ctrl Pts',(102.16225960469,-3.58736995598831,339.70781755958));
#19759=CARTESIAN_POINT('Ctrl Pts',(102.169658274445,-3.7101387775787,339.608991301099));
#19760=CARTESIAN_POINT('Ctrl Pts',(102.177055723649,-3.83288734612491,339.510181345882));
#19761=CARTESIAN_POINT('Ctrl Pts',(102.184453172853,-3.95172252102909,339.406434863739));
#19762=CARTESIAN_POINT('Ctrl Pts',(102.191850622057,-4.06623263929884,339.298102219073));
#19763=CARTESIAN_POINT('Ctrl Pts',(102.19924775052,-4.18073779260942,339.189774271521));
#19764=CARTESIAN_POINT('Ctrl Pts',(102.206644878984,-4.29091799103915,339.076860813308));
#19765=CARTESIAN_POINT('Ctrl Pts',(102.214042007447,-4.39639718337518,338.959750291181));
#19766=CARTESIAN_POINT('Ctrl Pts',(102.221440274884,-4.5018926168741,338.842621736957));
#19767=CARTESIAN_POINT('Ctrl Pts',(102.228838542321,-4.60268535323869,338.721295109394));
#19768=CARTESIAN_POINT('Ctrl Pts',(102.236236809757,-4.69843861740318,338.596193142894));
#19769=CARTESIAN_POINT('Ctrl Pts',(102.243637676283,-4.79422552069579,338.471047226757));
#19770=CARTESIAN_POINT('Ctrl Pts',(102.251038542809,-4.88496920019156,338.342123627166));
#19771=CARTESIAN_POINT('Ctrl Pts',(102.258439409334,-4.97037540714197,338.209875211683));
#19772=CARTESIAN_POINT('Ctrl Pts',(102.265848402719,-5.05587539827319,338.077481574796));
#19773=CARTESIAN_POINT('Ctrl Pts',(102.273257396104,-5.13602600942856,337.941756144546));
#19774=CARTESIAN_POINT('Ctrl Pts',(102.280666389489,-5.21057792122878,337.803178247865));
#19775=CARTESIAN_POINT('Ctrl Pts',(102.288079947069,-5.28517575957793,337.66451498242));
#19776=CARTESIAN_POINT('Ctrl Pts',(102.295493504649,-5.35416786283656,337.52299608374));
#19777=CARTESIAN_POINT('Ctrl Pts',(102.302907062229,-5.41735273970833,337.379121656426));
#19778=CARTESIAN_POINT('Ctrl Pts',(102.310331174366,-5.48062757181996,337.235042397524));
#19779=CARTESIAN_POINT('Ctrl Pts',(102.317755286502,-5.53807852945946,337.088601258819));
#19780=CARTESIAN_POINT('Ctrl Pts',(102.325179398639,-5.5895534604139,336.940315097007));
#19781=CARTESIAN_POINT('Ctrl Pts',(102.329036523794,-5.61629675946009,336.863274465846));
#19782=CARTESIAN_POINT('Ctrl Pts',(102.332893648949,-5.6414278308641,336.785736028709));
#19783=CARTESIAN_POINT('Ctrl Pts',(102.336750774103,-5.66493078873757,336.707773322579));
#19784=CARTESIAN_POINT('Ctrl Pts',(102.345877968528,-5.72054632037482,336.523288570804));
#19785=CARTESIAN_POINT('Ctrl Pts',(102.355005162953,-5.76717819787763,336.335978502897));
#19786=CARTESIAN_POINT('Ctrl Pts',(102.364132357378,-5.8045820679463,336.146628788657));
#19787=CARTESIAN_POINT('Ctrl Pts',(102.373160560046,-5.84158026299218,335.959332724199));
#19788=CARTESIAN_POINT('Ctrl Pts',(102.382188762715,-5.86954951833401,335.770040982889));
#19789=CARTESIAN_POINT('Ctrl Pts',(102.391216965383,-5.88829939689455,335.57953496446));
#19790=CARTESIAN_POINT('Ctrl Pts',(102.400245168051,-5.9070492754551,335.38902894603));
#19791=CARTESIAN_POINT('Ctrl Pts',(102.409273370719,-5.91657961760549,335.197308583576));
#19792=CARTESIAN_POINT('Ctrl Pts',(102.418301573388,-5.91674773493106,335.005177227848));
#19793=CARTESIAN_POINT('',(104.168301675714,-5.91240382638103,334.997402536992));
#19794=CARTESIAN_POINT('Ctrl Pts',(102.418301620294,-5.91325220417344,335.005173171578));
#19795=CARTESIAN_POINT('Ctrl Pts',(102.483864016322,-5.9016191688865,333.610737067852));
#19796=CARTESIAN_POINT('Ctrl Pts',(102.642172423775,-4.71167084592652,330.225837329939));
#19797=CARTESIAN_POINT('Ctrl Pts',(102.893226842651,0.937317003455184,328.066454027249));
#19798=CARTESIAN_POINT('Ctrl Pts',(103.171464876926,6.3378027430104,332.036070292348));
#19799=CARTESIAN_POINT('Ctrl Pts',(103.4497029112,5.92218045112015,338.725641102628));
#19800=CARTESIAN_POINT('Ctrl Pts',(103.727940945472,0.0718605704745667,
341.996246063401));
#19801=CARTESIAN_POINT('Ctrl Pts',(103.967473848504,-5.02140497767314,339.284654193084));
#19802=CARTESIAN_POINT('Ctrl Pts',(104.114260740112,-5.90351638125909,336.149335155669));
#19803=CARTESIAN_POINT('Ctrl Pts',(104.168301620294,-5.90805822426525,334.99740562831));
#19804=CARTESIAN_POINT('',(105.918301620294,-5.91976240380336,334.995907611496));
#19805=CARTESIAN_POINT('Ctrl Pts',(104.168301675755,-5.91674942901628,334.997400627864));
#19806=CARTESIAN_POINT('Ctrl Pts',(104.176377585023,-5.91667369032755,334.825002517902));
#19807=CARTESIAN_POINT('Ctrl Pts',(104.184453494291,-5.90905900258697,334.652848612642));
#19808=CARTESIAN_POINT('Ctrl Pts',(104.192529403559,-5.89399401348954,334.481574372306));
#19809=CARTESIAN_POINT('Ctrl Pts',(104.200642131212,-5.87886034252009,334.309519286039));
#19810=CARTESIAN_POINT('Ctrl Pts',(104.208754858865,-5.85620836299364,334.138352149417));
#19811=CARTESIAN_POINT('Ctrl Pts',(104.216867586518,-5.82617848403943,333.968702354014));
#19812=CARTESIAN_POINT('Ctrl Pts',(104.224998802207,-5.79608017021225,333.798665944925));
#19813=CARTESIAN_POINT('Ctrl Pts',(104.233130017896,-5.75857040477857,333.630154032497));
#19814=CARTESIAN_POINT('Ctrl Pts',(104.241261233585,-5.71383973478456,333.463781900999));
#19815=CARTESIAN_POINT('Ctrl Pts',(104.249420485457,-5.66895483481357,333.2968361235));
#19816=CARTESIAN_POINT('Ctrl Pts',(104.257579737328,-5.61679926657378,333.132045135939));
#19817=CARTESIAN_POINT('Ctrl Pts',(104.265738989199,-5.5576132958972,332.970008616825));
#19818=CARTESIAN_POINT('Ctrl Pts',(104.271964997473,-5.51245077990218,332.846364841067));
#19819=CARTESIAN_POINT('Ctrl Pts',(104.278191005748,-5.46319571390982,332.724324464125));
#19820=CARTESIAN_POINT('Ctrl Pts',(104.284417014022,-5.40997276369408,332.604144149038));
#19821=CARTESIAN_POINT('Ctrl Pts',(104.29184099146,-5.34650898976519,332.460839497258));
#19822=CARTESIAN_POINT('Ctrl Pts',(104.299264968898,-5.27725155469762,332.319842040562));
#19823=CARTESIAN_POINT('Ctrl Pts',(104.306688946336,-5.20238974119466,332.18165446703));
#19824=CARTESIAN_POINT('Ctrl Pts',(104.314104162363,-5.1276162758952,332.043629975626));
#19825=CARTESIAN_POINT('Ctrl Pts',(104.321519378391,-5.04725177349629,331.908409091629));
#19826=CARTESIAN_POINT('Ctrl Pts',(104.328934594418,-4.96153363947666,331.776474832293));
#19827=CARTESIAN_POINT('Ctrl Pts',(104.336342675563,-4.87589798301393,331.644667519437));
#19828=CARTESIAN_POINT('Ctrl Pts',(104.343750756707,-4.78491915205543,331.516140846414));
#19829=CARTESIAN_POINT('Ctrl Pts',(104.351158837851,-4.68888049227543,331.391353398896));
#19830=CARTESIAN_POINT('Ctrl Pts',(104.358561405025,-4.59291331582377,331.266658832954));
#19831=CARTESIAN_POINT('Ctrl Pts',(104.365963972199,-4.49189403609786,331.145698245306));
#19832=CARTESIAN_POINT('Ctrl Pts',(104.373366539373,-4.38614927922281,331.028901277622));
#19833=CARTESIAN_POINT('Ctrl Pts',(104.380765209127,-4.2804601965004,330.912165803031));
#19834=CARTESIAN_POINT('Ctrl Pts',(104.388163878882,-4.17005084136955,330.799589858619));
#19835=CARTESIAN_POINT('Ctrl Pts',(104.395562548637,-4.05528801181642,330.691569925864));
#19836=CARTESIAN_POINT('Ctrl Pts',(104.40295999784,-3.94054411456643,330.583567813043));
#19837=CARTESIAN_POINT('Ctrl Pts',(104.410357447044,-3.82144843976441,330.480120475742));
#19838=CARTESIAN_POINT('Ctrl Pts',(104.417754896248,-3.69840460943225,330.381587512204));
#19839=CARTESIAN_POINT('Ctrl Pts',(104.425152024712,-3.57536611406615,330.283058820884));
#19840=CARTESIAN_POINT('Ctrl Pts',(104.432549153175,-3.44838009485832,330.189444312941));
#19841=CARTESIAN_POINT('Ctrl Pts',(104.439946281638,-3.31788299989221,330.10106307843));
#19842=CARTESIAN_POINT('Ctrl Pts',(104.447344549075,-3.18736581163103,330.012668235414));
#19843=CARTESIAN_POINT('Ctrl Pts',(104.454742816511,-3.05333678019932,329.929508479565));
#19844=CARTESIAN_POINT('Ctrl Pts',(104.462141083948,-2.91626091739829,329.851859284736));
#19845=CARTESIAN_POINT('Ctrl Pts',(104.469541950474,-2.77913689840513,329.774182810929));
#19846=CARTESIAN_POINT('Ctrl Pts',(104.476942816999,-2.6389642414352,329.702020936384));
#19847=CARTESIAN_POINT('Ctrl Pts',(104.484343683525,-2.49623196021103,329.635602870469));
#19848=CARTESIAN_POINT('Ctrl Pts',(104.49175267691,-2.35334294529623,329.569111871167));
#19849=CARTESIAN_POINT('Ctrl Pts',(104.499161670294,-2.20788903155726,329.508377433961));
#19850=CARTESIAN_POINT('Ctrl Pts',(104.506570663679,-2.06037926541668,329.453580628447));
#19851=CARTESIAN_POINT('Ctrl Pts',(104.513984221259,-1.912778628172,329.39875006621));
#19852=CARTESIAN_POINT('Ctrl Pts',(104.521397778839,-1.76311996884052,329.3498645399));
#19853=CARTESIAN_POINT('Ctrl Pts',(104.528811336419,-1.61192634034383,329.307054889093));
#19854=CARTESIAN_POINT('Ctrl Pts',(104.536235448556,-1.46051746003739,329.264184290909));
#19855=CARTESIAN_POINT('Ctrl Pts',(104.543659560693,-1.30756960795487,329.22740693127));
#19856=CARTESIAN_POINT('Ctrl Pts',(104.551083672829,-1.15361564846502,329.196802476383));
#19857=CARTESIAN_POINT('Ctrl Pts',(104.554940797984,-1.07363036821326,329.180902229912));
#19858=CARTESIAN_POINT('Ctrl Pts',(104.558797923139,-0.993373607276174,
329.166667332352));
#19859=CARTESIAN_POINT('Ctrl Pts',(104.562655048294,-0.912920388189857,
329.154103411167));
#19860=CARTESIAN_POINT('Ctrl Pts',(104.570079025732,-0.758068559613185,
329.129921082707));
#19861=CARTESIAN_POINT('Ctrl Pts',(104.57750300317,-0.602021618121262,329.111859323147));
#19862=CARTESIAN_POINT('Ctrl Pts',(104.584926980608,-0.445304716578557,
329.100030993989));
#19863=CARTESIAN_POINT('Ctrl Pts',(104.592342196636,-0.288772764559113,
329.088216624039));
#19864=CARTESIAN_POINT('Ctrl Pts',(104.599757412663,-0.131572794831305,
329.082621069304));
#19865=CARTESIAN_POINT('Ctrl Pts',(104.607172628691,0.0257605393623651,
329.083306078805));
#19866=CARTESIAN_POINT('Ctrl Pts',(104.614580709835,0.182942488214167,329.083990429193));
#19867=CARTESIAN_POINT('Ctrl Pts',(104.621988790979,0.340257175351975,329.090943311462));
#19868=CARTESIAN_POINT('Ctrl Pts',(104.629396872123,0.497165631698212,329.104174621212));
#19869=CARTESIAN_POINT('Ctrl Pts',(104.636799439297,0.653957298214561,329.117396082657));
#19870=CARTESIAN_POINT('Ctrl Pts',(104.644202006471,0.810342965693608,329.136886635437));
#19871=CARTESIAN_POINT('Ctrl Pts',(104.651604573645,0.965784583151705,329.162604116436));
#19872=CARTESIAN_POINT('Ctrl Pts',(104.6590032434,1.12114436127767,329.188308057294));
#19873=CARTESIAN_POINT('Ctrl Pts',(104.666401913155,1.27556071198526,329.220232336377));
#19874=CARTESIAN_POINT('Ctrl Pts',(104.67380058291,1.42850173010513,329.25828306431));
#19875=CARTESIAN_POINT('Ctrl Pts',(104.681198032114,1.58141751770619,329.296327515055));
#19876=CARTESIAN_POINT('Ctrl Pts',(104.688595481318,1.73285809393971,329.34049631877));
#19877=CARTESIAN_POINT('Ctrl Pts',(104.695992930522,1.8823026419341,329.390644660331));
#19878=CARTESIAN_POINT('Ctrl Pts',(104.703390058985,2.03174071027321,329.440790827548));
#19879=CARTESIAN_POINT('Ctrl Pts',(104.710787187449,2.17918256863004,329.496915898381));
#19880=CARTESIAN_POINT('Ctrl Pts',(104.718184315912,2.3241237002702,329.558825532264));
#19881=CARTESIAN_POINT('Ctrl Pts',(104.725582583349,2.46908714922652,329.620744698685));
#19882=CARTESIAN_POINT('Ctrl Pts',(104.732980850786,2.61154876154769,329.688450055005));
#19883=CARTESIAN_POINT('Ctrl Pts',(104.740379118222,2.75102524082544,329.761699637588));
#19884=CARTESIAN_POINT('Ctrl Pts',(104.747779984748,2.89055071965723,329.834974953521));
#19885=CARTESIAN_POINT('Ctrl Pts',(104.755180851274,3.02708864726,329.913798200257));
#19886=CARTESIAN_POINT('Ctrl Pts',(104.7625817178,3.16018164320287,329.997882194064));
#19887=CARTESIAN_POINT('Ctrl Pts',(104.769990711184,3.29342078797948,330.082058520135));
#19888=CARTESIAN_POINT('Ctrl Pts',(104.777399704569,3.42320713080698,330.171506930408));
#19889=CARTESIAN_POINT('Ctrl Pts',(104.784808697954,3.54911293216977,330.265897344036));
#19890=CARTESIAN_POINT('Ctrl Pts',(104.792222255534,3.67509629584916,330.360345905414));
#19891=CARTESIAN_POINT('Ctrl Pts',(104.799635813114,3.79719406582669,330.459742301537));
#19892=CARTESIAN_POINT('Ctrl Pts',(104.807049370695,3.91501316236303,330.563717490846));
#19893=CARTESIAN_POINT('Ctrl Pts',(104.814473482831,4.03299999595296,330.667840707872));
#19894=CARTESIAN_POINT('Ctrl Pts',(104.821897594968,4.14669572119251,330.776555480103));
#19895=CARTESIAN_POINT('Ctrl Pts',(104.829321707105,4.25574498158056,330.889456822481));
#19896=CARTESIAN_POINT('Ctrl Pts',(104.83317883226,4.31240046274745,330.948113615328));
#19897=CARTESIAN_POINT('Ctrl Pts',(104.837035957414,4.36780243026257,331.007899917929));
#19898=CARTESIAN_POINT('Ctrl Pts',(104.840893082569,4.42190555287358,331.068755687576));
#19899=CARTESIAN_POINT('Ctrl Pts',(104.848317060007,4.52604019862202,331.185887448333));
#19900=CARTESIAN_POINT('Ctrl Pts',(104.855741037445,4.62567467157974,331.307336396068));
#19901=CARTESIAN_POINT('Ctrl Pts',(104.863165014883,4.72042987375358,331.432721994367));
#19902=CARTESIAN_POINT('Ctrl Pts',(104.870580230911,4.81507325053216,331.557959618794));
#19903=CARTESIAN_POINT('Ctrl Pts',(104.877995446938,4.90484859563693,331.687124351313));
#19904=CARTESIAN_POINT('Ctrl Pts',(104.885410662966,4.98941465145081,331.819800006542));
#19905=CARTESIAN_POINT('Ctrl Pts',(104.89281874411,5.07389933823157,331.952348001924));
#19906=CARTESIAN_POINT('Ctrl Pts',(104.900226825254,5.1531845151227,332.088399882053));
#19907=CARTESIAN_POINT('Ctrl Pts',(104.907634906398,5.22697019361061,332.227507771407));
#19908=CARTESIAN_POINT('Ctrl Pts',(104.915037473572,5.30070095207048,332.36651212022));
#19909=CARTESIAN_POINT('Ctrl Pts',(104.922440040746,5.36894018850547,332.508567620822));
#19910=CARTESIAN_POINT('Ctrl Pts',(104.92984260792,5.43143218851948,332.653198997781));
#19911=CARTESIAN_POINT('Ctrl Pts',(104.937241277675,5.4938912867686,332.797754226953));
#19912=CARTESIAN_POINT('Ctrl Pts',(104.94463994743,5.55060902718935,332.944882289818));
#19913=CARTESIAN_POINT('Ctrl Pts',(104.952038617184,5.60137651895223,333.094085087043));
#19914=CARTESIAN_POINT('Ctrl Pts',(104.959436066388,5.65213563565539,333.24326327044));
#19915=CARTESIAN_POINT('Ctrl Pts',(104.966833515592,5.69694633176932,333.394515155934));
#19916=CARTESIAN_POINT('Ctrl Pts',(104.974230964796,5.73564854152856,333.547324409732));
#19917=CARTESIAN_POINT('Ctrl Pts',(104.98162809326,5.77434907322746,333.700127037987));
#19918=CARTESIAN_POINT('Ctrl Pts',(104.989025221723,5.80694155355679,333.854486538497));
#19919=CARTESIAN_POINT('Ctrl Pts',(104.996422350187,5.83331638469168,334.009873483545));
#19920=CARTESIAN_POINT('Ctrl Pts',(105.003820617623,5.85969527689218,334.165284354303));
#19921=CARTESIAN_POINT('Ctrl Pts',(105.01121888506,5.87985455120487,334.321722616627));
#19922=CARTESIAN_POINT('Ctrl Pts',(105.018617152496,5.89373614059483,334.478650915848));
#19923=CARTESIAN_POINT('Ctrl Pts',(105.026018019022,5.90762260673312,334.635634345631));
#19924=CARTESIAN_POINT('Ctrl Pts',(105.033418885548,5.91522696410329,334.793107783546));
#19925=CARTESIAN_POINT('Ctrl Pts',(105.040819752074,5.9165431968366,334.950531197037));
#19926=CARTESIAN_POINT('Ctrl Pts',(105.048228745458,5.91786087491929,335.108127476486));
#19927=CARTESIAN_POINT('Ctrl Pts',(105.055637738843,5.91287663566499,335.265673248387));
#19928=CARTESIAN_POINT('Ctrl Pts',(105.063046732228,5.90163657670515,335.42263019177));
#19929=CARTESIAN_POINT('Ctrl Pts',(105.070460289808,5.89038959348128,335.579683826045));
#19930=CARTESIAN_POINT('Ctrl Pts',(105.077873847388,5.87287915275581,335.736147538967));
#19931=CARTESIAN_POINT('Ctrl Pts',(105.085287404969,5.8492028714466,335.891491071835));
#19932=CARTESIAN_POINT('Ctrl Pts',(105.092711517105,5.82549288261645,336.047055764661));
#19933=CARTESIAN_POINT('Ctrl Pts',(105.100135629242,5.79559959210596,336.201496726913));
#19934=CARTESIAN_POINT('Ctrl Pts',(105.107559741379,5.75967125669765,336.354295971075));
#19935=CARTESIAN_POINT('Ctrl Pts',(105.111416866533,5.74100503995453,336.433681330216));
#19936=CARTESIAN_POINT('Ctrl Pts',(105.115273991688,5.72071064619899,336.512623825523));
#19937=CARTESIAN_POINT('Ctrl Pts',(105.119131116843,5.69881403528363,336.591052844425));
#19938=CARTESIAN_POINT('Ctrl Pts',(105.126555094281,5.65666867082547,336.742008606415));
#19939=CARTESIAN_POINT('Ctrl Pts',(105.133979071719,5.60845759001825,336.891516354692));
#19940=CARTESIAN_POINT('Ctrl Pts',(105.141403049157,5.55429564237294,337.039051367577));
#19941=CARTESIAN_POINT('Ctrl Pts',(105.148818265184,5.50019761397491,337.186412266949));
#19942=CARTESIAN_POINT('Ctrl Pts',(105.156233481212,5.44016282533593,337.331804718157));
#19943=CARTESIAN_POINT('Ctrl Pts',(105.163648697239,5.37435658154257,337.474716528601));
#19944=CARTESIAN_POINT('Ctrl Pts',(105.171056778384,5.30861365618565,337.61749083002));
#19945=CARTESIAN_POINT('Ctrl Pts',(105.178464859528,5.23711048624453,337.757788905736));
#19946=CARTESIAN_POINT('Ctrl Pts',(105.185872940672,5.16006135880073,337.895116117863));
#19947=CARTESIAN_POINT('Ctrl Pts',(105.193275507846,5.08306958042967,338.032341114839));
#19948=CARTESIAN_POINT('Ctrl Pts',(105.20067807502,5.00054024575367,338.166599327096));
#19949=CARTESIAN_POINT('Ctrl Pts',(105.208080642194,4.91273464229113,338.297418520136));
#19950=CARTESIAN_POINT('Ctrl Pts',(105.215479311948,4.82497526809506,338.428168837442));
#19951=CARTESIAN_POINT('Ctrl Pts',(105.222877981703,4.73194536499745,338.555483432404));
#19952=CARTESIAN_POINT('Ctrl Pts',(105.230276651458,4.63395075253962,338.678917094138));
#19953=CARTESIAN_POINT('Ctrl Pts',(105.237674100662,4.53597230614996,338.80233039315));
#19954=CARTESIAN_POINT('Ctrl Pts',(105.245071549866,4.43303100772558,338.921863737578));
#19955=CARTESIAN_POINT('Ctrl Pts',(105.25246899907,4.32547443259754,339.037103106863));
#19956=CARTESIAN_POINT('Ctrl Pts',(105.259866127533,4.21792252093509,339.15233747957));
#19957=CARTESIAN_POINT('Ctrl Pts',(105.267263255997,4.10575598510295,339.263277974482));
#19958=CARTESIAN_POINT('Ctrl Pts',(105.27466038446,3.98936072249202,339.369545924732));
#19959=CARTESIAN_POINT('Ctrl Pts',(105.282058651897,3.87294753791625,339.475830237593));
#19960=CARTESIAN_POINT('Ctrl Pts',(105.289456919334,3.75230460573427,339.57744032161));
#19961=CARTESIAN_POINT('Ctrl Pts',(105.29685518677,3.62785237554537,339.674036553532));
#19962=CARTESIAN_POINT('Ctrl Pts',(105.304256053296,3.50335642397915,339.770666720725));
#19963=CARTESIAN_POINT('Ctrl Pts',(105.311656919822,3.37504880459844,339.86227930015));
#19964=CARTESIAN_POINT('Ctrl Pts',(105.319057786347,3.2433803867706,339.948576990329));
#19965=CARTESIAN_POINT('Ctrl Pts',(105.326466779732,3.11156738443189,340.034969443622));
#19966=CARTESIAN_POINT('Ctrl Pts',(105.333875773117,2.97638652589233,340.11603514765));
#19967=CARTESIAN_POINT('Ctrl Pts',(105.341284766502,2.83831544281442,340.191521550526));
#19968=CARTESIAN_POINT('Ctrl Pts',(105.348698324082,2.70015930318685,340.267054455631));
#19969=CARTESIAN_POINT('Ctrl Pts',(105.356111881662,2.5591097247587,340.337001045404));
#19970=CARTESIAN_POINT('Ctrl Pts',(105.363525439242,2.41566543950032,340.401156454585));
#19971=CARTESIAN_POINT('Ctrl Pts',(105.370949551379,2.27201693504089,340.465403200736));
#19972=CARTESIAN_POINT('Ctrl Pts',(105.378373663516,2.12596726025782,340.523842161495));
#19973=CARTESIAN_POINT('Ctrl Pts',(105.385797775653,1.97803223215624,340.576317696388));
#19974=CARTESIAN_POINT('Ctrl Pts',(105.389654900807,1.90117402909435,340.603580849465));
#19975=CARTESIAN_POINT('Ctrl Pts',(105.393512025962,1.82380713967182,340.629235174725));
#19976=CARTESIAN_POINT('Ctrl Pts',(105.397369151117,1.74600499187263,340.653264289847));
#19977=CARTESIAN_POINT('Ctrl Pts',(105.404793128555,1.59625579610632,340.699514178395));
#19978=CARTESIAN_POINT('Ctrl Pts',(105.412217105993,1.44444175879629,340.739879673351));
#19979=CARTESIAN_POINT('Ctrl Pts',(105.419641083431,1.29106628125662,340.774173397111));
#19980=CARTESIAN_POINT('Ctrl Pts',(105.427056299458,1.13787180985702,340.808426649117));
#19981=CARTESIAN_POINT('Ctrl Pts',(105.434471515486,0.983119926896012,340.83662231253));
#19982=CARTESIAN_POINT('Ctrl Pts',(105.441886731514,0.827330802125772,340.858622219119));
#19983=CARTESIAN_POINT('Ctrl Pts',(105.449294812658,0.67169157686698,340.880600957508));
#19984=CARTESIAN_POINT('Ctrl Pts',(105.456702893802,0.515017463763272,340.896395755523));
#19985=CARTESIAN_POINT('Ctrl Pts',(105.464110974946,0.357840377399421,340.905919134801));
#19986=CARTESIAN_POINT('Ctrl Pts',(105.47151354212,0.20078028081135,340.915435425653));
#19987=CARTESIAN_POINT('Ctrl Pts',(105.478916109294,0.0432183273251074,
340.918689569825));
#19988=CARTESIAN_POINT('Ctrl Pts',(105.486318676468,-0.11430697332543,340.91564573638));
#19989=CARTESIAN_POINT('Ctrl Pts',(105.493717346223,-0.271749337593634,
340.9126035055));
#19990=CARTESIAN_POINT('Ctrl Pts',(105.501116015978,-0.429154715256507,
340.903269907923));
#19991=CARTESIAN_POINT('Ctrl Pts',(105.508514685732,-0.585983222481062,
340.88766118467));
#19992=CARTESIAN_POINT('Ctrl Pts',(105.515912134936,-0.74278585787171,340.872055036372));
#19993=CARTESIAN_POINT('Ctrl Pts',(105.52330958414,-0.899011440681882,340.850175853862));
#19994=CARTESIAN_POINT('Ctrl Pts',(105.530707033344,-1.0541237192351,340.822091870371));
#19995=CARTESIAN_POINT('Ctrl Pts',(105.538104161808,-1.20922927239024,340.794009104554));
#19996=CARTESIAN_POINT('Ctrl Pts',(105.545501290271,-1.3632212500264,340.759722139165));
#19997=CARTESIAN_POINT('Ctrl Pts',(105.552898418735,-1.51557239187673,340.719350565185));
#19998=CARTESIAN_POINT('Ctrl Pts',(105.560296686171,-1.66794699199993,340.67897277499));
#19999=CARTESIAN_POINT('Ctrl Pts',(105.567694953608,-1.8186798925005,340.632508606361));
#20000=CARTESIAN_POINT('Ctrl Pts',(105.575093221045,-1.96725796753637,340.580127834706));
#20001=CARTESIAN_POINT('Ctrl Pts',(105.58249408757,-2.11588823961227,340.527728661135));
#20002=CARTESIAN_POINT('Ctrl Pts',(105.589894954096,-2.2623618272558,340.46940887013));
#20003=CARTESIAN_POINT('Ctrl Pts',(105.597295820622,-2.4061847320271,340.405386720472));
#20004=CARTESIAN_POINT('Ctrl Pts',(105.604704814007,-2.55016556809806,340.341294268373));
#20005=CARTESIAN_POINT('Ctrl Pts',(105.612113807391,-2.69148956730769,340.271487104468));
#20006=CARTESIAN_POINT('Ctrl Pts',(105.619522800776,-2.82968587948925,340.196230209096));
#20007=CARTESIAN_POINT('Ctrl Pts',(105.626936358356,-2.96796732536612,340.12092695288));
#20008=CARTESIAN_POINT('Ctrl Pts',(105.634349915937,-3.10311692526235,340.040167466479));
#20009=CARTESIAN_POINT('Ctrl Pts',(105.641763473517,-3.234692511123,339.954260279899));
#20010=CARTESIAN_POINT('Ctrl Pts',(105.649187585654,-3.36645541891807,339.868230788712));
#20011=CARTESIAN_POINT('Ctrl Pts',(105.65661169779,-3.49463384711528,339.777039176247));
#20012=CARTESIAN_POINT('Ctrl Pts',(105.664035809927,-3.61881777613905,339.681034978036));
#20013=CARTESIAN_POINT('Ctrl Pts',(105.667892935081,-3.68333632699171,339.631156931875));
#20014=CARTESIAN_POINT('Ctrl Pts',(105.671750060236,-3.74677725958832,339.579980491455));
#20015=CARTESIAN_POINT('Ctrl Pts',(105.675607185391,-3.80908706159064,339.52755853852));
#20016=CARTESIAN_POINT('Ctrl Pts',(105.682926719848,-3.92733024129565,339.428079191736));
#20017=CARTESIAN_POINT('Ctrl Pts',(105.690246254305,-4.04187637728178,339.323793849167));
#20018=CARTESIAN_POINT('Ctrl Pts',(105.697565788763,-4.15230161964887,339.215011485389));
#20019=CARTESIAN_POINT('Ctrl Pts',(105.704876630412,-4.26259571905414,339.106358313462));
#20020=CARTESIAN_POINT('Ctrl Pts',(105.712187472062,-4.36877839062624,338.993219013035));
#20021=CARTESIAN_POINT('Ctrl Pts',(105.719498313711,-4.47045756742951,338.875943717382));
#20022=CARTESIAN_POINT('Ctrl Pts',(105.726802174549,-4.57203965511264,338.758780402919));
#20023=CARTESIAN_POINT('Ctrl Pts',(105.734106035387,-4.66912655475497,338.63748924053));
#20024=CARTESIAN_POINT('Ctrl Pts',(105.741409896225,-4.76136210197062,338.512458041944));
#20025=CARTESIAN_POINT('Ctrl Pts',(105.748780384728,-4.85443904516614,338.386286277155));
#20026=CARTESIAN_POINT('Ctrl Pts',(105.756150873231,-4.94257538854965,338.256306165677));
#20027=CARTESIAN_POINT('Ctrl Pts',(105.763521361733,-5.02544536141048,338.122952046058));
#20028=CARTESIAN_POINT('Ctrl Pts',(105.77081673526,-5.10747078020508,337.990956980389));
#20029=CARTESIAN_POINT('Ctrl Pts',(105.778112108787,-5.1843364660858,337.855656693525));
#20030=CARTESIAN_POINT('Ctrl Pts',(105.785407482314,-5.25576921250541,337.717502630611));
#20031=CARTESIAN_POINT('Ctrl Pts',(105.792701419185,-5.32718789189067,337.579375773959));
#20032=CARTESIAN_POINT('Ctrl Pts',(105.799995356055,-5.39317558391413,337.438396600875));
#20033=CARTESIAN_POINT('Ctrl Pts',(105.807289292926,-5.45350483718485,337.295041514505));
#20034=CARTESIAN_POINT('Ctrl Pts',(105.81458332757,-5.51383489914462,337.151684506518));
#20035=CARTESIAN_POINT('Ctrl Pts',(105.821877362213,-5.56850622303597,337.005951876731));
#20036=CARTESIAN_POINT('Ctrl Pts',(105.829171396856,-5.61733946573983,336.858340089742));
#20037=CARTESIAN_POINT('Ctrl Pts',(105.836598915476,-5.66706637782536,336.708026943451));
#20038=CARTESIAN_POINT('Ctrl Pts',(105.844026434096,-5.71073930474988,336.555765579812));
#20039=CARTESIAN_POINT('Ctrl Pts',(105.851453952715,-5.74822216767177,336.402095743374));
#20040=CARTESIAN_POINT('Ctrl Pts',(105.858755885835,-5.78507126522119,336.251024177546));
#20041=CARTESIAN_POINT('Ctrl Pts',(105.866057818954,-5.81593794289666,336.098591782589));
#20042=CARTESIAN_POINT('Ctrl Pts',(105.873359752073,-5.84074480762381,335.945320397916));
#20043=CARTESIAN_POINT('Ctrl Pts',(105.880850063443,-5.86619164997221,335.788094855502));
#20044=CARTESIAN_POINT('Ctrl Pts',(105.888340374813,-5.88526172827391,335.629986881795));
#20045=CARTESIAN_POINT('Ctrl Pts',(105.895830686184,-5.89792834386354,335.471563159239));
#20046=CARTESIAN_POINT('Ctrl Pts',(105.903320997554,-5.91059495945317,335.313139436682));
#20047=CARTESIAN_POINT('Ctrl Pts',(105.910811308924,-5.91685815230932,335.154400398292));
#20048=CARTESIAN_POINT('Ctrl Pts',(105.918301620294,-5.91674858616663,334.995909694977));
#20049=CARTESIAN_POINT('',(107.668301620294,-5.92094148725317,335.004780648189));
#20050=CARTESIAN_POINT('Ctrl Pts',(105.918301620294,-5.92277622144009,334.995905528015));
#20051=CARTESIAN_POINT('Ctrl Pts',(105.930149486751,-5.92475648142696,334.744954570789));
#20052=CARTESIAN_POINT('Ctrl Pts',(106.034743364634,-5.79618199096297,332.531584302122));
#20053=CARTESIAN_POINT('Ctrl Pts',(106.232083253937,-3.00667844047728,328.682365341618));
#20054=CARTESIAN_POINT('Ctrl Pts',(106.510321288213,3.68554753774321,329.052785335281));
#20055=CARTESIAN_POINT('Ctrl Pts',(106.788559322486,6.99560093916926,334.880876446012));
#20056=CARTESIAN_POINT('Ctrl Pts',(107.066797356761,3.88589461361887,340.818285483979));
#20057=CARTESIAN_POINT('Ctrl Pts',(107.345035391035,-2.78983984313537,341.416339811048));
#20058=CARTESIAN_POINT('Ctrl Pts',(107.545536812213,-5.75554344655869,337.60421618645));
#20059=CARTESIAN_POINT('Ctrl Pts',(107.653292221966,-5.92373472965658,335.322952874196));
#20060=CARTESIAN_POINT('Ctrl Pts',(107.668301620294,-5.92094148725317,335.004780648189));
#20061=CARTESIAN_POINT('',(109.418301620294,-5.9073481418614,335.001565332871));
#20062=CARTESIAN_POINT('Ctrl Pts',(107.668301620294,-5.92094148725317,335.004780648189));
#20063=CARTESIAN_POINT('Ctrl Pts',(107.74603823339,-5.90647473787108,333.356904384973));
#20064=CARTESIAN_POINT('Ctrl Pts',(107.916520857911,-4.33224609725952,329.718746258985));
#20065=CARTESIAN_POINT('Ctrl Pts',(108.179749493857,1.83586661996066,328.248539663529));
#20066=CARTESIAN_POINT('Ctrl Pts',(108.457987528129,6.67093980309293,332.890216820446));
#20067=CARTESIAN_POINT('Ctrl Pts',(108.736225562404,5.38418999183579,339.468010860891));
#20068=CARTESIAN_POINT('Ctrl Pts',(109.014463596677,-0.84355150441294,341.945577282027));
#20069=CARTESIAN_POINT('Ctrl Pts',(109.241822282641,-5.29991352060222,338.761775431531));
#20070=CARTESIAN_POINT('Ctrl Pts',(109.37643495718,-5.90945668690147,335.894258462759));
#20071=CARTESIAN_POINT('Ctrl Pts',(109.418301620294,-5.9073481418614,335.001565332871));
#20072=CARTESIAN_POINT('',(111.168301624698,-5.91548968584153,334.994581587743));
#20073=CARTESIAN_POINT('Ctrl Pts',(109.418301620294,-5.9073481418614,335.001565332871));
#20074=CARTESIAN_POINT('Ctrl Pts',(109.469180968605,-5.9047856878815,333.916701116055));
#20075=CARTESIAN_POINT('Ctrl Pts',(109.612806328339,-5.09840548129149,330.850735185492));
#20076=CARTESIAN_POINT('Ctrl Pts',(109.8491776995,-0.166381100682085,328.005363465443));
#20077=CARTESIAN_POINT('Ctrl Pts',(110.127415733773,5.79190072541038,331.074887401844));
#20078=CARTESIAN_POINT('Ctrl Pts',(110.405653768048,6.43504074410829,337.746429235006));
#20079=CARTESIAN_POINT('Ctrl Pts',(110.683891802322,1.17283885298437,341.89761349643));
#20080=CARTESIAN_POINT('Ctrl Pts',(110.938107753071,-4.61841647199816,339.907056893972));
#20081=CARTESIAN_POINT('Ctrl Pts',(111.099577692395,-5.90208330670883,336.455049090138));
#20082=CARTESIAN_POINT('Ctrl Pts',(111.168301620294,-5.91518394046082,334.994581961406));
#20083=CARTESIAN_POINT('',(112.91830226473,-5.92197236043631,335.001102995849));
#20084=CARTESIAN_POINT('Ctrl Pts',(111.168301642816,-5.91674751756803,334.994580050503));
#20085=CARTESIAN_POINT('Ctrl Pts',(111.177681833011,-5.91656486805913,334.79518870395));
#20086=CARTESIAN_POINT('Ctrl Pts',(111.187062023205,-5.90629965081535,334.596247156779));
#20087=CARTESIAN_POINT('Ctrl Pts',(111.1964422134,-5.88610916826479,334.398627052679));
#20088=CARTESIAN_POINT('Ctrl Pts',(111.206007905427,-5.86551940047264,334.197098830444));
#20089=CARTESIAN_POINT('Ctrl Pts',(111.215573597454,-5.83460793238311,333.996944643371));
#20090=CARTESIAN_POINT('Ctrl Pts',(111.225139289481,-5.79358985553926,333.79906405321));
#20091=CARTESIAN_POINT('Ctrl Pts',(111.230215483277,-5.77182292988356,333.694055422232));
#20092=CARTESIAN_POINT('Ctrl Pts',(111.235291677073,-5.74721071566286,333.589686654878));
#20093=CARTESIAN_POINT('Ctrl Pts',(111.240367870869,-5.71979075055661,333.48608972117));
#20094=CARTESIAN_POINT('Ctrl Pts',(111.247791848307,-5.67968881385373,333.334578307422));
#20095=CARTESIAN_POINT('Ctrl Pts',(111.255215825745,-5.63350215019534,333.184432820619));
#20096=CARTESIAN_POINT('Ctrl Pts',(111.262639803183,-5.58133850903378,333.036179486288));
#20097=CARTESIAN_POINT('Ctrl Pts',(111.270055019211,-5.5292364288172,332.888101113197));
#20098=CARTESIAN_POINT('Ctrl Pts',(111.277470235238,-5.47117153433217,332.741910796337));
#20099=CARTESIAN_POINT('Ctrl Pts',(111.284885451266,-5.40730219528288,332.598122915012));
#20100=CARTESIAN_POINT('Ctrl Pts',(111.29229353241,-5.34349431099007,332.454473385663));
#20101=CARTESIAN_POINT('Ctrl Pts',(111.299701613554,-5.2738932513323,332.313222028659));
#20102=CARTESIAN_POINT('Ctrl Pts',(111.307109694698,-5.19870660072143,332.174866331991));
#20103=CARTESIAN_POINT('Ctrl Pts',(111.314512261872,-5.12357591290791,332.036613615996));
#20104=CARTESIAN_POINT('Ctrl Pts',(111.321914829046,-5.04286808968227,331.901252595349));
#20105=CARTESIAN_POINT('Ctrl Pts',(111.32931739622,-4.95683801429786,331.769258991731));
#20106=CARTESIAN_POINT('Ctrl Pts',(111.336716065975,-4.87085323337215,331.637334882168));
#20107=CARTESIAN_POINT('Ctrl Pts',(111.34411473573,-4.77955198419317,331.508774970614));
#20108=CARTESIAN_POINT('Ctrl Pts',(111.351513405484,-4.68323404309151,331.384028559276));
#20109=CARTESIAN_POINT('Ctrl Pts',(111.358910854688,-4.58693199145916,331.259302727223));
#20110=CARTESIAN_POINT('Ctrl Pts',(111.366308303892,-4.48561511828267,331.138389441927));
#20111=CARTESIAN_POINT('Ctrl Pts',(111.373705753096,-4.379625373287,331.021707382286));
#20112=CARTESIAN_POINT('Ctrl Pts',(111.38110288156,-4.27364022382189,330.905030381775));
#20113=CARTESIAN_POINT('Ctrl Pts',(111.388500010023,-4.16298285632729,330.792584518397));
#20114=CARTESIAN_POINT('Ctrl Pts',(111.395897138487,-4.04803401675782,330.684753638357));
#20115=CARTESIAN_POINT('Ctrl Pts',(111.403295405923,-3.93306747793625,330.576906155053));
#20116=CARTESIAN_POINT('Ctrl Pts',(111.41069367336,-3.81380842355036,330.473675325324));
#20117=CARTESIAN_POINT('Ctrl Pts',(111.418091940797,-3.6906726761321,330.375406422165));
#20118=CARTESIAN_POINT('Ctrl Pts',(111.425492807322,-3.56749366983102,330.277102996107));
#20119=CARTESIAN_POINT('Ctrl Pts',(111.432893673848,-3.44043555043321,330.183765199931));
#20120=CARTESIAN_POINT('Ctrl Pts',(111.440294540374,-3.30994512927636,330.095696399724));
#20121=CARTESIAN_POINT('Ctrl Pts',(111.447703533759,-3.17931141716171,330.007530891555));
#20122=CARTESIAN_POINT('Ctrl Pts',(111.455112527144,-3.04523818593642,329.924646142936));
#20123=CARTESIAN_POINT('Ctrl Pts',(111.462521520528,-2.9081996114074,329.847301136035));
#20124=CARTESIAN_POINT('Ctrl Pts',(111.469935078109,-2.77107661638961,329.769908481941));
#20125=CARTESIAN_POINT('Ctrl Pts',(111.477348635689,-2.63098496932983,329.698062539678));
#20126=CARTESIAN_POINT('Ctrl Pts',(111.484762193269,-2.4884205887163,329.631974894232));
#20127=CARTESIAN_POINT('Ctrl Pts',(111.492186305406,-2.34565324160717,329.565793160924));
#20128=CARTESIAN_POINT('Ctrl Pts',(111.499610417542,-2.2004064736915,329.505386240386));
#20129=CARTESIAN_POINT('Ctrl Pts',(111.507034529679,-2.05319395201455,329.450916728151));
#20130=CARTESIAN_POINT('Ctrl Pts',(111.510891654834,-1.97671112012507,329.422617623565));
#20131=CARTESIAN_POINT('Ctrl Pts',(111.514748779989,-1.89969791124875,329.395920327023));
#20132=CARTESIAN_POINT('Ctrl Pts',(111.518605905144,-1.82222752532369,329.370842211445));
#20133=CARTESIAN_POINT('Ctrl Pts',(111.526029882582,-1.67311688614997,329.322573265853));
#20134=CARTESIAN_POINT('Ctrl Pts',(111.53345386002,-1.52186208918751,329.280160278417));
#20135=CARTESIAN_POINT('Ctrl Pts',(111.540877837458,-1.36896395811982,329.243797411151));
#20136=CARTESIAN_POINT('Ctrl Pts',(111.548293053486,-1.21624626985155,329.20747745754));
#20137=CARTESIAN_POINT('Ctrl Pts',(111.555708269513,-1.06188946740132,329.177193497221));
#20138=CARTESIAN_POINT('Ctrl Pts',(111.563123485541,-0.906411806233638,
329.153090713888));
#20139=CARTESIAN_POINT('Ctrl Pts',(111.570531566685,-0.751083744888806,
329.129011122133));
#20140=CARTESIAN_POINT('Ctrl Pts',(111.577939647829,-0.594637338229394,
329.111100923796));
#20141=CARTESIAN_POINT('Ctrl Pts',(111.585347728973,-0.437603270357113,
329.099454776017));
#20142=CARTESIAN_POINT('Ctrl Pts',(111.592750296147,-0.28068608580945,329.087817296678));
#20143=CARTESIAN_POINT('Ctrl Pts',(111.600152863321,-0.123182481584819,
329.082434611768));
#20144=CARTESIAN_POINT('Ctrl Pts',(111.607555430495,0.034369565853609,329.083349824821));
#20145=CARTESIAN_POINT('Ctrl Pts',(111.61495410025,0.191838662827861,329.084264556018));
#20146=CARTESIAN_POINT('Ctrl Pts',(111.622352770005,0.349355779955852,329.091470579372));
#20147=CARTESIAN_POINT('Ctrl Pts',(111.629751439759,0.506380863250504,329.104958949775));
#20148=CARTESIAN_POINT('Ctrl Pts',(111.637148888963,0.66338004228219,329.118445095017));
#20149=CARTESIAN_POINT('Ctrl Pts',(111.644546338167,0.819886977096974,329.138211498495));
#20150=CARTESIAN_POINT('Ctrl Pts',(111.651943787371,0.975364543059989,329.164197178567));
#20151=CARTESIAN_POINT('Ctrl Pts',(111.659340915835,1.13083536778669,329.190181731946));
#20152=CARTESIAN_POINT('Ctrl Pts',(111.666738044298,1.28527654429864,329.222384964228));
#20153=CARTESIAN_POINT('Ctrl Pts',(111.674135172762,1.43815924464937,329.260694419224));
#20154=CARTESIAN_POINT('Ctrl Pts',(111.681533440198,1.5910654851196,329.29900977292));
#20155=CARTESIAN_POINT('Ctrl Pts',(111.688931707635,1.74241240958322,329.343433130683));
#20156=CARTESIAN_POINT('Ctrl Pts',(111.696329975071,1.89168464518075,329.393801665506));
#20157=CARTESIAN_POINT('Ctrl Pts',(111.703730841597,2.04100932168454,329.444187895324));
#20158=CARTESIAN_POINT('Ctrl Pts',(111.711131708123,2.18825750476337,329.50052334136));
#20159=CARTESIAN_POINT('Ctrl Pts',(111.718532574649,2.33293229214959,329.562596439223));
#20160=CARTESIAN_POINT('Ctrl Pts',(111.725941568033,2.47776594628382,329.624737699283));
#20161=CARTESIAN_POINT('Ctrl Pts',(111.733350561418,2.62002021820294,329.692629046344));
#20162=CARTESIAN_POINT('Ctrl Pts',(111.740759554803,2.7592207205391,329.766011885966));
#20163=CARTESIAN_POINT('Ctrl Pts',(111.748173112383,2.89850697518625,329.839439931949));
#20164=CARTESIAN_POINT('Ctrl Pts',(111.755586669963,3.03473538948241,329.918366024808));
#20165=CARTESIAN_POINT('Ctrl Pts',(111.763000227544,3.16745966714886,330.002487636885));
#20166=CARTESIAN_POINT('Ctrl Pts',(111.77042433968,3.3003729021229,330.086729011477));
#20167=CARTESIAN_POINT('Ctrl Pts',(111.777848451817,3.42977173070535,330.176180466471));
#20168=CARTESIAN_POINT('Ctrl Pts',(111.785272563954,3.55524144813195,330.270498038061));
#20169=CARTESIAN_POINT('Ctrl Pts',(111.789129689108,3.62042801782811,330.319499813789));
#20170=CARTESIAN_POINT('Ctrl Pts',(111.792986814263,3.68455461038738,330.369814425085));
#20171=CARTESIAN_POINT('Ctrl Pts',(111.796843939418,3.74756700386472,330.421389718043));
#20172=CARTESIAN_POINT('Ctrl Pts',(111.804267916856,3.86884971280862,330.520658939529));
#20173=CARTESIAN_POINT('Ctrl Pts',(111.811691894294,3.98636834841945,330.624900224016));
#20174=CARTESIAN_POINT('Ctrl Pts',(111.819115871732,4.09968861128476,330.73379749039));
#20175=CARTESIAN_POINT('Ctrl Pts',(111.826531087759,4.21287513918994,330.842566241606));
#20176=CARTESIAN_POINT('Ctrl Pts',(111.833946303787,4.32187289029909,330.955979781222));
#20177=CARTESIAN_POINT('Ctrl Pts',(111.841361519814,4.42627931877771,331.07368086439));
#20178=CARTESIAN_POINT('Ctrl Pts',(111.848769600958,4.53058528791646,331.191268696167));
#20179=CARTESIAN_POINT('Ctrl Pts',(111.856177682103,4.63030848333096,331.313135581158));
#20180=CARTESIAN_POINT('Ctrl Pts',(111.863585763247,4.72508212219692,331.438886480187));
#20181=CARTESIAN_POINT('Ctrl Pts',(111.870988330421,4.81978521931264,331.564543780525));
#20182=CARTESIAN_POINT('Ctrl Pts',(111.878390897595,4.90954587168814,331.694079041847));
#20183=CARTESIAN_POINT('Ctrl Pts',(111.885793464769,4.99403670271017,331.827063194061));
#20184=CARTESIAN_POINT('Ctrl Pts',(111.893192134523,5.07848304967887,331.9599773307));
#20185=CARTESIAN_POINT('Ctrl Pts',(111.900590804278,5.15766490131545,332.09633642769));
#20186=CARTESIAN_POINT('Ctrl Pts',(111.907989474033,5.23129752554913,332.235681501403));
#20187=CARTESIAN_POINT('Ctrl Pts',(111.915386923237,5.30491800268633,332.375003587506));
#20188=CARTESIAN_POINT('Ctrl Pts',(111.922784372441,5.37299089509791,332.517310343039));
#20189=CARTESIAN_POINT('Ctrl Pts',(111.930181821645,5.43527681458859,332.66211708777));
#20190=CARTESIAN_POINT('Ctrl Pts',(111.937578950108,5.49756003347035,332.806917553934));
#20191=CARTESIAN_POINT('Ctrl Pts',(111.944976078572,5.55405663086222,332.954217450929));
#20192=CARTESIAN_POINT('Ctrl Pts',(111.952373207035,5.60457499442688,333.103511219557));
#20193=CARTESIAN_POINT('Ctrl Pts',(111.959771474472,5.65510113655845,333.252827975699));
#20194=CARTESIAN_POINT('Ctrl Pts',(111.967169741908,5.69964709239634,333.404138861223));
#20195=CARTESIAN_POINT('Ctrl Pts',(111.974568009345,5.73807088881975,333.556922373058));
#20196=CARTESIAN_POINT('Ctrl Pts',(111.981968875871,5.77650818392695,333.709759559348));
#20197=CARTESIAN_POINT('Ctrl Pts',(111.989369742396,5.80881894645461,333.864070040278));
#20198=CARTESIAN_POINT('Ctrl Pts',(111.996770608922,5.83491218308189,334.0193214705));
#20199=CARTESIAN_POINT('Ctrl Pts',(112.004179602307,5.86103407257759,334.174743381634));
#20200=CARTESIAN_POINT('Ctrl Pts',(112.011588595692,5.88092473951966,334.331107937252));
#20201=CARTESIAN_POINT('Ctrl Pts',(112.018997589076,5.89454492326482,334.487876274605));
#20202=CARTESIAN_POINT('Ctrl Pts',(112.026411146657,5.90817349751299,334.64474118666));
#20203=CARTESIAN_POINT('Ctrl Pts',(112.033824704237,5.91552387397367,334.802010004172));
#20204=CARTESIAN_POINT('Ctrl Pts',(112.041238261817,5.91660893808531,334.959143712002));
#20205=CARTESIAN_POINT('Ctrl Pts',(112.048662373954,5.91769554698436,335.116501128431));
#20206=CARTESIAN_POINT('Ctrl Pts',(112.056086486091,5.91249904116674,335.273722679009));
#20207=CARTESIAN_POINT('Ctrl Pts',(112.063510598227,5.90108424659031,335.4302734911));
#20208=CARTESIAN_POINT('Ctrl Pts',(112.067367723382,5.89515380124041,335.511607940825));
#20209=CARTESIAN_POINT('Ctrl Pts',(112.071224848537,5.88754575000308,335.592761483817));
#20210=CARTESIAN_POINT('Ctrl Pts',(112.075081973692,5.87827460760497,335.673660300216));
#20211=CARTESIAN_POINT('Ctrl Pts',(112.08250595113,5.86043003445131,335.829369789433));
#20212=CARTESIAN_POINT('Ctrl Pts',(112.089929928568,5.83636739138287,335.984604657669));
#20213=CARTESIAN_POINT('Ctrl Pts',(112.097353906006,5.80611745341878,336.138828643654));
#20214=CARTESIAN_POINT('Ctrl Pts',(112.104769122033,5.77590321493284,336.292870622131));
#20215=CARTESIAN_POINT('Ctrl Pts',(112.112184338061,5.7395162873123,336.445903730358));
#20216=CARTESIAN_POINT('Ctrl Pts',(112.119599554089,5.69703924472344,336.597396133268));
#20217=CARTESIAN_POINT('Ctrl Pts',(112.127007635233,5.65460307333107,336.748742770951));
#20218=CARTESIAN_POINT('Ctrl Pts',(112.134415716377,5.60608855298068,336.898551297666));
#20219=CARTESIAN_POINT('Ctrl Pts',(112.141823797521,5.55162939330956,337.046299499546));
#20220=CARTESIAN_POINT('Ctrl Pts',(112.149226364695,5.4972107685856,337.19393772974));
#20221=CARTESIAN_POINT('Ctrl Pts',(112.156628931869,5.43685644329193,337.339518339916));
#20222=CARTESIAN_POINT('Ctrl Pts',(112.164031499043,5.37075006935111,337.482533837648));
#20223=CARTESIAN_POINT('Ctrl Pts',(112.171430168798,5.30467850012722,337.625474038345));
#20224=CARTESIAN_POINT('Ctrl Pts',(112.178828838553,5.23286106974775,337.765851478322));
#20225=CARTESIAN_POINT('Ctrl Pts',(112.186227508307,5.15552966247693,337.903178337929));
#20226=CARTESIAN_POINT('Ctrl Pts',(112.193624957511,5.07821101248703,338.040482542868));
#20227=CARTESIAN_POINT('Ctrl Pts',(112.201022406715,4.99538037388325,338.174736841347));
#20228=CARTESIAN_POINT('Ctrl Pts',(112.208419855919,4.90731577792332,338.305477638443));
#20229=CARTESIAN_POINT('Ctrl Pts',(112.215816984383,4.81925500029074,338.436212766845));
#20230=CARTESIAN_POINT('Ctrl Pts',(112.223214112846,4.72596092502395,338.563434387225));
#20231=CARTESIAN_POINT('Ctrl Pts',(112.23061124131,4.62775499520856,338.686707781588));
#20232=CARTESIAN_POINT('Ctrl Pts',(112.238009508747,4.52953394413146,338.810000156977));
#20233=CARTESIAN_POINT('Ctrl Pts',(112.245407776183,4.42639976516784,338.929342803961));
#20234=CARTESIAN_POINT('Ctrl Pts',(112.25280604362,4.31871417157305,339.04433411908));
#20235=CARTESIAN_POINT('Ctrl Pts',(112.260206910146,4.21099074689679,339.159365831857));
#20236=CARTESIAN_POINT('Ctrl Pts',(112.267607776671,4.09871297900713,339.270042896951));
#20237=CARTESIAN_POINT('Ctrl Pts',(112.275008643197,3.98227928675753,339.376000713524));
#20238=CARTESIAN_POINT('Ctrl Pts',(112.282417636582,3.86571773918234,339.482074881909));
#20239=CARTESIAN_POINT('Ctrl Pts',(112.289826629967,3.74499142967971,339.583419201331));
#20240=CARTESIAN_POINT('Ctrl Pts',(112.297235623351,3.6205322532438,339.679709047123));
#20241=CARTESIAN_POINT('Ctrl Pts',(112.304649180932,3.49599640566206,339.776058210781));
#20242=CARTESIAN_POINT('Ctrl Pts',(112.312062738512,3.36772341229982,339.867346480399));
#20243=CARTESIAN_POINT('Ctrl Pts',(112.319476296092,3.23617351553603,339.953292999596));
#20244=CARTESIAN_POINT('Ctrl Pts',(112.326900408229,3.10443633341096,340.039361879397));
#20245=CARTESIAN_POINT('Ctrl Pts',(112.334324520366,2.96941324988094,340.120073629181));
#20246=CARTESIAN_POINT('Ctrl Pts',(112.341748632502,2.83158913180129,340.195193312204));
#20247=CARTESIAN_POINT('Ctrl Pts',(112.345605757657,2.75998395357303,340.2342210119));
#20248=CARTESIAN_POINT('Ctrl Pts',(112.349462882811,2.68762305486854,340.271740078002));
#20249=CARTESIAN_POINT('Ctrl Pts',(112.353320007966,2.61457636713573,340.307722768091));
#20250=CARTESIAN_POINT('Ctrl Pts',(112.360743985404,2.47398021328188,340.376980225053));
#20251=CARTESIAN_POINT('Ctrl Pts',(112.368167962842,2.33041822391381,340.44075192972));
#20252=CARTESIAN_POINT('Ctrl Pts',(112.37559194028,2.18435800670142,340.498773559719));
#20253=CARTESIAN_POINT('Ctrl Pts',(112.383007156307,2.0384701625215,340.556726715464));
#20254=CARTESIAN_POINT('Ctrl Pts',(112.390422372335,1.89009030257854,340.608943167646));
#20255=CARTESIAN_POINT('Ctrl Pts',(112.397837588363,1.739710343946,340.655204548172));
#20256=CARTESIAN_POINT('Ctrl Pts',(112.405245669507,1.58947508015237,340.701421416231));
#20257=CARTESIAN_POINT('Ctrl Pts',(112.412653750651,1.4372439032895,340.741694510873));
#20258=CARTESIAN_POINT('Ctrl Pts',(112.420061831795,1.28352831209565,340.775853671497));
#20259=CARTESIAN_POINT('Ctrl Pts',(112.427464398969,1.12992713422372,340.809987406835));
#20260=CARTESIAN_POINT('Ctrl Pts',(112.434866966143,0.974844104754665,340.838016188672));
#20261=CARTESIAN_POINT('Ctrl Pts',(112.442269533317,0.818805369488226,340.859819820557));
#20262=CARTESIAN_POINT('Ctrl Pts',(112.449668203072,0.662848787933832,340.881611972926));
#20263=CARTESIAN_POINT('Ctrl Pts',(112.457066872826,0.505937871374166,340.89718545119));
#20264=CARTESIAN_POINT('Ctrl Pts',(112.464465542581,0.348608323641791,340.90647126457));
#20265=CARTESIAN_POINT('Ctrl Pts',(112.471862991785,0.191304730399448,340.915755546078));
#20266=CARTESIAN_POINT('Ctrl Pts',(112.479260440989,0.0335830152491352,
340.91875419938));
#20267=CARTESIAN_POINT('Ctrl Pts',(112.486657890193,-0.12401651627988,340.915450149075));
#20268=CARTESIAN_POINT('Ctrl Pts',(112.494055018657,-0.281609214567851,
340.912146242028));
#20269=CARTESIAN_POINT('Ctrl Pts',(112.50145214712,-0.43907936663873,340.902540182557));
#20270=CARTESIAN_POINT('Ctrl Pts',(112.508849275583,-0.595887457559155,
340.88666702816));
#20271=CARTESIAN_POINT('Ctrl Pts',(112.51624754302,-0.752719693011461,340.870791429693));
#20272=CARTESIAN_POINT('Ctrl Pts',(112.523645810457,-0.90888929299925,340.848646852494));
#20273=CARTESIAN_POINT('Ctrl Pts',(112.531044077893,-1.0638627968066,340.82032013828));
#20274=CARTESIAN_POINT('Ctrl Pts',(112.538444944419,-1.21889074443568,340.791983472594));
#20275=CARTESIAN_POINT('Ctrl Pts',(112.545845810945,-1.37272139236702,340.757460412805));
#20276=CARTESIAN_POINT('Ctrl Pts',(112.553246677471,-1.52483253267406,340.716888691395));
#20277=CARTESIAN_POINT('Ctrl Pts',(112.560655670855,-1.67711070555533,340.676272418355));
#20278=CARTESIAN_POINT('Ctrl Pts',(112.56806466424,-1.82766523918877,340.629594315487));
#20279=CARTESIAN_POINT('Ctrl Pts',(112.575473657625,-1.97598942660418,340.57704189947));
#20280=CARTESIAN_POINT('Ctrl Pts',(112.582887215205,-2.12440498683539,340.524457109353));
#20281=CARTESIAN_POINT('Ctrl Pts',(112.590300772785,-2.27058711731749,340.46599093346));
#20282=CARTESIAN_POINT('Ctrl Pts',(112.597714330366,-2.41405057636902,340.401878411926));
#20283=CARTESIAN_POINT('Ctrl Pts',(112.605138442502,-2.5577182819189,340.33767461448));
#20284=CARTESIAN_POINT('Ctrl Pts',(112.612562554639,-2.69865925234245,340.267808581996));
#20285=CARTESIAN_POINT('Ctrl Pts',(112.619986666776,-2.83641353504342,340.192560911604));
#20286=CARTESIAN_POINT('Ctrl Pts',(112.62384379193,-2.90798243098363,340.153466717316));
#20287=CARTESIAN_POINT('Ctrl Pts',(112.627700917085,-2.97869164846253,340.112920613353));
#20288=CARTESIAN_POINT('Ctrl Pts',(112.631558042239,-3.04848001436847,340.070966393548));
#20289=CARTESIAN_POINT('Ctrl Pts',(112.638982019677,-3.18280473372633,339.99021527224));
#20290=CARTESIAN_POINT('Ctrl Pts',(112.646405997115,-3.31412135072215,339.904001461234));
#20291=CARTESIAN_POINT('Ctrl Pts',(112.653829974553,-3.44195454169205,339.812575141795));
#20292=CARTESIAN_POINT('Ctrl Pts',(112.661245190581,-3.56963687026307,339.721256719169));
#20293=CARTESIAN_POINT('Ctrl Pts',(112.668660406609,-3.69384365514196,339.624738247853));
#20294=CARTESIAN_POINT('Ctrl Pts',(112.676075622636,-3.81412506138573,339.523315219903));
#20295=CARTESIAN_POINT('Ctrl Pts',(112.68348370378,-3.93429073346604,339.421989780681));
#20296=CARTESIAN_POINT('Ctrl Pts',(112.690891784924,-4.05053826276284,339.315769418728));
#20297=CARTESIAN_POINT('Ctrl Pts',(112.698299866068,-4.16244775627929,339.204992180581));
#20298=CARTESIAN_POINT('Ctrl Pts',(112.705702433242,-4.27427395351608,339.094297395955));
#20299=CARTESIAN_POINT('Ctrl Pts',(112.713105000416,-4.38176828003886,338.979052750067));
#20300=CARTESIAN_POINT('Ctrl Pts',(112.72050756759,-4.48454493240522,338.859635644946));
#20301=CARTESIAN_POINT('Ctrl Pts',(112.727906237345,-4.58726747331329,338.74028141241));
#20302=CARTESIAN_POINT('Ctrl Pts',(112.7353049071,-4.68527704392799,338.616759377822));
#20303=CARTESIAN_POINT('Ctrl Pts',(112.742703576854,-4.77822572834857,338.489482691094));
#20304=CARTESIAN_POINT('Ctrl Pts',(112.750101026058,-4.8711590791223,338.362227001069));
#20305=CARTESIAN_POINT('Ctrl Pts',(112.757498475262,-4.95903298079465,338.231218189318));
#20306=CARTESIAN_POINT('Ctrl Pts',(112.764895924466,-5.04154068397413,338.09690136981));
#20307=CARTESIAN_POINT('Ctrl Pts',(112.77229305293,-5.12404480976344,337.962590374046));
#20308=CARTESIAN_POINT('Ctrl Pts',(112.779690181393,-5.20118300433905,337.824971973716));
#20309=CARTESIAN_POINT('Ctrl Pts',(112.787087309857,-5.27269278581095,337.684518830062));
#20310=CARTESIAN_POINT('Ctrl Pts',(112.794485577293,-5.34421357800407,337.54404406013));
#20311=CARTESIAN_POINT('Ctrl Pts',(112.80188384473,-5.410104062167,337.40073401039));
#20312=CARTESIAN_POINT('Ctrl Pts',(112.809282112166,-5.47014857914836,337.255084274377));
#20313=CARTESIAN_POINT('Ctrl Pts',(112.816682978692,-5.53021419040002,337.109383370079));
#20314=CARTESIAN_POINT('Ctrl Pts',(112.824083845218,-5.58442960330336,336.961341487817));
#20315=CARTESIAN_POINT('Ctrl Pts',(112.831484711744,-5.63262804336511,336.811472298324));
#20316=CARTESIAN_POINT('Ctrl Pts',(112.838893705128,-5.680879409922,336.661438538134));
#20317=CARTESIAN_POINT('Ctrl Pts',(112.846302698513,-5.72310049435268,336.50957381901));
#20318=CARTESIAN_POINT('Ctrl Pts',(112.853711691898,-5.7591747752185,336.356405717692));
#20319=CARTESIAN_POINT('Ctrl Pts',(112.861125249478,-5.79527127908566,336.203143259539));
#20320=CARTESIAN_POINT('Ctrl Pts',(112.868538807058,-5.82521336318953,336.048576184795));
#20321=CARTESIAN_POINT('Ctrl Pts',(112.875952364639,-5.84893608567506,335.893239737242));
#20322=CARTESIAN_POINT('Ctrl Pts',(112.883376476775,-5.87269258179906,335.737682139818));
#20323=CARTESIAN_POINT('Ctrl Pts',(112.890800588912,-5.89021199084438,335.581353351856));
#20324=CARTESIAN_POINT('Ctrl Pts',(112.898224701049,-5.90148136618252,335.424792004516));
#20325=CARTESIAN_POINT('Ctrl Pts',(112.902081826204,-5.90733626038337,335.343452081306));
#20326=CARTESIAN_POINT('Ctrl Pts',(112.905938951358,-5.91150499142025,335.26204936842));
#20327=CARTESIAN_POINT('Ctrl Pts',(112.909796076513,-5.91399128217944,335.180659006987));
#20328=CARTESIAN_POINT('Ctrl Pts',(112.912631257774,-5.91581883111431,335.12083299195));
#20329=CARTESIAN_POINT('Ctrl Pts',(112.915466439034,-5.9167386071917,335.060979105019));
#20330=CARTESIAN_POINT('Ctrl Pts',(112.918301620294,-5.91674989481959,335.001115639915));
#20331=CARTESIAN_POINT('',(114.668301620294,-5.91183534194015,335.004818938716));
#20332=CARTESIAN_POINT('Ctrl Pts',(112.918302791716,-5.92624301184832,335.001092656212));
#20333=CARTESIAN_POINT('Ctrl Pts',(113.008213231406,-5.92131010852706,333.099630750775));
#20334=CARTESIAN_POINT('Ctrl Pts',(113.190869682522,-3.8962064387588,329.227734848842));
#20335=CARTESIAN_POINT('Ctrl Pts',(113.46627214506,2.70289327938773,328.546552019156));
#20336=CARTESIAN_POINT('Ctrl Pts',(113.744510179335,6.88953273082826,333.780589621136));
#20337=CARTESIAN_POINT('Ctrl Pts',(114.022748213608,4.7537496845221,340.133662129328));
#20338=CARTESIAN_POINT('Ctrl Pts',(114.300986247883,-1.74447928203647,341.775648674169));
#20339=CARTESIAN_POINT('Ctrl Pts',(114.516170716778,-5.5320017806064,338.236706706155));
#20340=CARTESIAN_POINT('Ctrl Pts',(114.638609174248,-5.91666024635598,335.636725282272));
#20341=CARTESIAN_POINT('Ctrl Pts',(114.668301620294,-5.91183534194015,335.004818938716));
#20342=CARTESIAN_POINT('',(116.418301620294,-5.90886619475503,334.996662217394));
#20343=CARTESIAN_POINT('Ctrl Pts',(114.668301620294,-5.91183534194015,335.004818938716));
#20344=CARTESIAN_POINT('Ctrl Pts',(114.731355185673,-5.90158938828715,333.662930571381));
#20345=CARTESIAN_POINT('Ctrl Pts',(114.887154762477,-4.78309971499823,330.33179209936));
#20346=CARTESIAN_POINT('Ctrl Pts',(115.135700350704,0.74963200781035,328.043659383405));
#20347=CARTESIAN_POINT('Ctrl Pts',(115.413938384979,6.25540412481643,331.865906485686));
#20348=CARTESIAN_POINT('Ctrl Pts',(115.692176419252,6.0206842060895,338.564264946907));
#20349=CARTESIAN_POINT('Ctrl Pts',(115.970414453527,0.260871256591412,341.991750074816));
#20350=CARTESIAN_POINT('Ctrl Pts',(116.212456187207,-4.95789529531347,339.391818017654));
#20351=CARTESIAN_POINT('Ctrl Pts',(116.361751909463,-5.90270235742463,336.201657451435));
#20352=CARTESIAN_POINT('Ctrl Pts',(116.418301620294,-5.90886619475503,334.996662217394));
#20353=CARTESIAN_POINT('',(118.168300196814,-5.92087836980671,334.996633443784));
#20354=CARTESIAN_POINT('Ctrl Pts',(116.418301620294,-5.90886619475503,334.996662217394));
#20355=CARTESIAN_POINT('Ctrl Pts',(116.454497920888,-5.91281153957713,334.225369684439));
#20356=CARTESIAN_POINT('Ctrl Pts',(116.583440232905,-5.41355607546623,331.482697059055));
#20357=CARTESIAN_POINT('Ctrl Pts',(116.805128556348,-1.2659262506568,328.118862474187));
#20358=CARTESIAN_POINT('Ctrl Pts',(117.083366590623,5.10143001502218,330.211677253667));
#20359=CARTESIAN_POINT('Ctrl Pts',(117.361604624895,6.7872792528987,336.698665141928));
#20360=CARTESIAN_POINT('Ctrl Pts',(117.63984265917,2.24454250046778,341.626813101694));
#20361=CARTESIAN_POINT('Ctrl Pts',(117.908740818052,-4.13634482415734,340.512342377915));
#20362=CARTESIAN_POINT('Ctrl Pts',(118.084892965511,-5.91195779426516,336.762288914003));
#20363=CARTESIAN_POINT('Ctrl Pts',(118.168299101544,-5.92405561514005,334.99665480686));
#20364=CARTESIAN_POINT('',(119.918302439026,-5.91853562323323,335.00514099704));
#20365=CARTESIAN_POINT('Ctrl Pts',(118.168301620294,-5.91674902637294,334.996605679018));
#20366=CARTESIAN_POINT('Ctrl Pts',(118.177640656102,-5.9166357507117,334.799151265657));
#20367=CARTESIAN_POINT('Ctrl Pts',(118.18697969191,-5.90663908245873,334.601984314875));
#20368=CARTESIAN_POINT('Ctrl Pts',(118.196318727718,-5.88683994509542,334.405823238986));
#20369=CARTESIAN_POINT('Ctrl Pts',(118.203742705156,-5.87110080969631,334.249886862729));
#20370=CARTESIAN_POINT('Ctrl Pts',(118.211166682594,-5.84913775930447,334.094341051069));
#20371=CARTESIAN_POINT('Ctrl Pts',(118.218590660032,-5.82097432064191,333.93972243213));
#20372=CARTESIAN_POINT('Ctrl Pts',(118.22600587606,-5.79284411907441,333.785286286426));
#20373=CARTESIAN_POINT('Ctrl Pts',(118.233421092088,-5.7585281608484,333.631775518965));
#20374=CARTESIAN_POINT('Ctrl Pts',(118.240836308115,-5.71810182690776,333.47972303194));
#20375=CARTESIAN_POINT('Ctrl Pts',(118.248244389259,-5.67771439098206,333.327816849052));
#20376=CARTESIAN_POINT('Ctrl Pts',(118.255652470403,-5.63122837933056,333.177366511459));
#20377=CARTESIAN_POINT('Ctrl Pts',(118.263060551548,-5.57877043369371,333.028895991926));
#20378=CARTESIAN_POINT('Ctrl Pts',(118.270463118722,-5.52635153346386,332.880535981713));
#20379=CARTESIAN_POINT('Ctrl Pts',(118.277865685896,-5.46796967372883,332.734153205764));
#20380=CARTESIAN_POINT('Ctrl Pts',(118.28526825307,-5.40380163285874,332.590257591523));
#20381=CARTESIAN_POINT('Ctrl Pts',(118.292666922824,-5.33966737618174,332.446437737694));
#20382=CARTESIAN_POINT('Ctrl Pts',(118.300065592579,-5.2697531570709,332.305102777663));
#20383=CARTESIAN_POINT('Ctrl Pts',(118.307464262334,-5.19428424763646,332.166743619569));
#20384=CARTESIAN_POINT('Ctrl Pts',(118.314861711538,-5.11882778822859,332.028407286439));
#20385=CARTESIAN_POINT('Ctrl Pts',(118.322259160742,-5.03781863569839,331.89304610826));
#20386=CARTESIAN_POINT('Ctrl Pts',(118.329656609946,-4.95152853224047,331.761127394153));
#20387=CARTESIAN_POINT('Ctrl Pts',(118.337053738409,-4.86524217017103,331.629214399811));
#20388=CARTESIAN_POINT('Ctrl Pts',(118.344450866873,-4.77367551674591,331.500743885091));
#20389=CARTESIAN_POINT('Ctrl Pts',(118.351847995336,-4.67714411218454,331.376154871361));
#20390=CARTESIAN_POINT('Ctrl Pts',(118.359246262773,-4.5805978441965,331.251546674034));
#20391=CARTESIAN_POINT('Ctrl Pts',(118.366644530209,-4.47908553155157,331.130821462744));
#20392=CARTESIAN_POINT('Ctrl Pts',(118.374042797646,-4.37296342837738,331.014385691443));
#20393=CARTESIAN_POINT('Ctrl Pts',(118.381443664171,-4.26680404339248,330.897909015032));
#20394=CARTESIAN_POINT('Ctrl Pts',(118.388844530697,-4.15603189476303,330.785725054556));
#20395=CARTESIAN_POINT('Ctrl Pts',(118.396245397223,-4.04104043881098,330.678203760658));
#20396=CARTESIAN_POINT('Ctrl Pts',(118.403654390607,-3.92592271124648,330.570564398099));
#20397=CARTESIAN_POINT('Ctrl Pts',(118.411063383992,-3.80657669637475,330.467598182187));
#20398=CARTESIAN_POINT('Ctrl Pts',(118.418472377377,-3.68342986372551,330.369635543338));
#20399=CARTESIAN_POINT('Ctrl Pts',(118.425885934957,-3.5602071683796,330.271612556126));
#20400=CARTESIAN_POINT('Ctrl Pts',(118.433299492537,-3.43317929005262,330.17859950799));
#20401=CARTESIAN_POINT('Ctrl Pts',(118.440713050118,-3.30280263442986,330.090883448063));
#20402=CARTESIAN_POINT('Ctrl Pts',(118.448137162254,-3.17224036376924,330.003042508266));
#20403=CARTESIAN_POINT('Ctrl Pts',(118.455561274391,-3.03832011083527,329.920513813298));
#20404=CARTESIAN_POINT('Ctrl Pts',(118.462985386528,-2.90152352396745,329.84353882955));
#20405=CARTESIAN_POINT('Ctrl Pts',(118.466842511682,-2.83045218956942,329.803547226429));
#20406=CARTESIAN_POINT('Ctrl Pts',(118.470699636837,-2.75860482035376,329.765053908568));
#20407=CARTESIAN_POINT('Ctrl Pts',(118.474556761991,-2.68605096655409,329.728087560707));
#20408=CARTESIAN_POINT('Ctrl Pts',(118.481980739429,-2.54640339172725,329.656936814624));
#20409=CARTESIAN_POINT('Ctrl Pts',(118.489404716867,-2.40371613347195,329.591231248354));
#20410=CARTESIAN_POINT('Ctrl Pts',(118.496828694305,-2.25845318548505,329.531241478043));
#20411=CARTESIAN_POINT('Ctrl Pts',(118.504243910333,-2.11336166963261,329.471322504688));
#20412=CARTESIAN_POINT('Ctrl Pts',(118.511659126361,-1.96570085622135,329.417106041341));
#20413=CARTESIAN_POINT('Ctrl Pts',(118.519074342388,-1.8159596670263,329.36881708251));
#20414=CARTESIAN_POINT('Ctrl Pts',(118.526482423532,-1.6663625580496,329.320574587072));
#20415=CARTESIAN_POINT('Ctrl Pts',(118.533890504676,-1.51468941117923,329.278248355495));
#20416=CARTESIAN_POINT('Ctrl Pts',(118.54129858582,-1.36144937940466,329.242015443767));
#20417=CARTESIAN_POINT('Ctrl Pts',(118.548701152994,-1.20832340698424,329.205809500856));
#20418=CARTESIAN_POINT('Ctrl Pts',(118.556103720168,-1.05363323349634,329.175687932722));
#20419=CARTESIAN_POINT('Ctrl Pts',(118.563506287342,-0.897903332726364,
329.15177803366));
#20420=CARTESIAN_POINT('Ctrl Pts',(118.570904957097,-0.742255423068583,
329.127880723056));
#20421=CARTESIAN_POINT('Ctrl Pts',(118.578303626852,-0.585569244291613,
329.110188624789));
#20422=CARTESIAN_POINT('Ctrl Pts',(118.585702296607,-0.428379519186952,
329.0987779613));
#20423=CARTESIAN_POINT('Ctrl Pts',(118.593099745811,-0.271215725506044,
329.087369180215));
#20424=CARTESIAN_POINT('Ctrl Pts',(118.600497195015,-0.113548922233473,
329.082239804297));
#20425=CARTESIAN_POINT('Ctrl Pts',(118.607894644219,0.0440808651278728,
329.083414207515));
#20426=CARTESIAN_POINT('Ctrl Pts',(118.615291772682,0.201703817936448,329.084588559814));
#20427=CARTESIAN_POINT('Ctrl Pts',(118.622688901146,0.359289384824021,329.092066145016));
#20428=CARTESIAN_POINT('Ctrl Pts',(118.630086029609,0.516297626437871,329.105819198274));
#20429=CARTESIAN_POINT('Ctrl Pts',(118.637484297046,0.673330043401532,329.119574369159));
#20430=CARTESIAN_POINT('Ctrl Pts',(118.644882564482,0.829784586282144,329.139606899491));
#20431=CARTESIAN_POINT('Ctrl Pts',(118.652280831919,0.985126669729223,329.165837163132));
#20432=CARTESIAN_POINT('Ctrl Pts',(118.659681698445,1.14052332648389,329.192076641741));
#20433=CARTESIAN_POINT('Ctrl Pts',(118.667082564971,1.29480637791557,329.224518126616));
#20434=CARTESIAN_POINT('Ctrl Pts',(118.674483431496,1.44745180284501,329.263030953462));
#20435=CARTESIAN_POINT('Ctrl Pts',(118.681892424881,1.60026484704455,329.301586071073));
#20436=CARTESIAN_POINT('Ctrl Pts',(118.689301418266,1.75143631141262,329.346225753484));
#20437=CARTESIAN_POINT('Ctrl Pts',(118.696710411651,1.90045700167132,329.396769347305));
#20438=CARTESIAN_POINT('Ctrl Pts',(118.704123969231,2.0495694938156,329.447344077724));
#20439=CARTESIAN_POINT('Ctrl Pts',(118.711537526811,2.19652822415995,329.503829833196));
#20440=CARTESIAN_POINT('Ctrl Pts',(118.718951084391,2.34084481966104,329.5659981512));
#20441=CARTESIAN_POINT('Ctrl Pts',(118.726375196528,2.4853668762563,329.628254977186));
#20442=CARTESIAN_POINT('Ctrl Pts',(118.733799308665,2.62723894973204,329.696210362598));
#20443=CARTESIAN_POINT('Ctrl Pts',(118.741223420802,2.76599733829589,329.769589950392));
#20444=CARTESIAN_POINT('Ctrl Pts',(118.745080545956,2.83808790766069,329.807713600562));
#20445=CARTESIAN_POINT('Ctrl Pts',(118.748937671111,2.90933849395444,329.847300643093));
#20446=CARTESIAN_POINT('Ctrl Pts',(118.752794796266,2.97968733794584,329.888308114666));
#20447=CARTESIAN_POINT('Ctrl Pts',(118.760218773704,3.11509083397726,329.967236988254));
#20448=CARTESIAN_POINT('Ctrl Pts',(118.767642751142,3.24756030925623,330.051668695727));
#20449=CARTESIAN_POINT('Ctrl Pts',(118.77506672858,3.37661710327811,330.141359500812));
#20450=CARTESIAN_POINT('Ctrl Pts',(118.782481944608,3.50552159086535,330.230944457252));
#20451=CARTESIAN_POINT('Ctrl Pts',(118.789897160635,3.63102111046476,330.325775946197));
#20452=CARTESIAN_POINT('Ctrl Pts',(118.797312376663,3.7526618757666,330.425564580337));
#20453=CARTESIAN_POINT('Ctrl Pts',(118.804720457807,3.87418559893657,330.525257198355));
#20454=CARTESIAN_POINT('Ctrl Pts',(118.812128538951,3.99185767283532,330.629897230779));
#20455=CARTESIAN_POINT('Ctrl Pts',(118.819536620095,4.10525367540771,330.739152335151));
#20456=CARTESIAN_POINT('Ctrl Pts',(118.826939187269,4.21856527526431,330.848326118953));
#20457=CARTESIAN_POINT('Ctrl Pts',(118.834341754443,4.32760687351862,330.962107877117));
#20458=CARTESIAN_POINT('Ctrl Pts',(118.841744321617,4.4319876028216,331.080125454694));
#20459=CARTESIAN_POINT('Ctrl Pts',(118.849142991372,4.53631337612679,331.198080896533));
#20460=CARTESIAN_POINT('Ctrl Pts',(118.856541661127,4.63598292099064,331.320267437476));
#20461=CARTESIAN_POINT('Ctrl Pts',(118.863940330882,4.73064277115367,331.446276666054));
#20462=CARTESIAN_POINT('Ctrl Pts',(118.871337780085,4.82528700538084,331.572265107023));
#20463=CARTESIAN_POINT('Ctrl Pts',(118.878735229289,4.91492296119113,331.702074685936));
#20464=CARTESIAN_POINT('Ctrl Pts',(118.886132678493,4.99923790320661,331.835264473982));
#20465=CARTESIAN_POINT('Ctrl Pts',(118.893529806957,5.08354918947314,331.96844848715));
#20466=CARTESIAN_POINT('Ctrl Pts',(118.90092693542,5.16253972104985,332.105012102704));
#20467=CARTESIAN_POINT('Ctrl Pts',(118.908324063884,5.23594065382523,332.244486248969));
#20468=CARTESIAN_POINT('Ctrl Pts',(118.915722331321,5.30935288851201,332.383981870771));
#20469=CARTESIAN_POINT('Ctrl Pts',(118.923120598757,5.37717363689238,332.526388585321));
#20470=CARTESIAN_POINT('Ctrl Pts',(118.930518866194,5.43918056347867,332.671213758119));
#20471=CARTESIAN_POINT('Ctrl Pts',(118.93791973272,5.50120927375035,332.816089809523));
#20472=CARTESIAN_POINT('Ctrl Pts',(118.945320599245,5.55741994889959,332.963385667914));
#20473=CARTESIAN_POINT('Ctrl Pts',(118.952721465771,5.60763888939149,333.112589962757));
#20474=CARTESIAN_POINT('Ctrl Pts',(118.960130459156,5.6579129750812,333.261958098181));
#20475=CARTESIAN_POINT('Ctrl Pts',(118.967539452541,5.70218206738238,333.413238501247));
#20476=CARTESIAN_POINT('Ctrl Pts',(118.974948445925,5.74032252734205,333.565905217711));
#20477=CARTESIAN_POINT('Ctrl Pts',(118.982362003506,5.77848648314067,333.718665982138));
#20478=CARTESIAN_POINT('Ctrl Pts',(118.989775561086,5.81051420777265,333.87281439715));
#20479=CARTESIAN_POINT('Ctrl Pts',(118.997189118666,5.83633353357012,334.027816145256));
#20480=CARTESIAN_POINT('Ctrl Pts',(119.004613230803,5.86218961790471,334.183038566727));
#20481=CARTESIAN_POINT('Ctrl Pts',(119.012037342939,5.88181960412198,334.339116378348));
#20482=CARTESIAN_POINT('Ctrl Pts',(119.019461455076,5.8952032692673,334.495511173047));
#20483=CARTESIAN_POINT('Ctrl Pts',(119.023318580231,5.90215662214518,334.576764565448));
#20484=CARTESIAN_POINT('Ctrl Pts',(119.027175705385,5.90742481412969,334.658103523739));
#20485=CARTESIAN_POINT('Ctrl Pts',(119.03103283054,5.91101055252681,334.73945286335));
#20486=CARTESIAN_POINT('Ctrl Pts',(119.038456807978,5.91791218000646,334.896029494305));
#20487=CARTESIAN_POINT('Ctrl Pts',(119.045880785416,5.91859859009121,335.053116743783));
#20488=CARTESIAN_POINT('Ctrl Pts',(119.053304762854,5.91301571514873,335.21018019627));
#20489=CARTESIAN_POINT('Ctrl Pts',(119.060719978881,5.90743942883867,335.367058290252));
#20490=CARTESIAN_POINT('Ctrl Pts',(119.068135194909,5.89560859785933,335.523912273796));
#20491=CARTESIAN_POINT('Ctrl Pts',(119.075550410936,5.87752100436485,335.680203944233));
#20492=CARTESIAN_POINT('Ctrl Pts',(119.082958492081,5.85945081466177,335.836345231612));
#20493=CARTESIAN_POINT('Ctrl Pts',(119.090366573225,5.83513589020854,335.991924914765));
#20494=CARTESIAN_POINT('Ctrl Pts',(119.097774654369,5.80462602573991,336.146406238557));
#20495=CARTESIAN_POINT('Ctrl Pts',(119.105177221543,5.77413887032061,336.300772579079));
#20496=CARTESIAN_POINT('Ctrl Pts',(119.112579788717,5.73746602807457,336.45404182349));
#20497=CARTESIAN_POINT('Ctrl Pts',(119.119982355891,5.69470893128614,336.6056838887));
#20498=CARTESIAN_POINT('Ctrl Pts',(119.127381025646,5.65197434592228,336.757246115025));
#20499=CARTESIAN_POINT('Ctrl Pts',(119.1347796954,5.60316198667137,336.907182510024));
#20500=CARTESIAN_POINT('Ctrl Pts',(119.142178365155,5.54842401457511,337.054974821497));
#20501=CARTESIAN_POINT('Ctrl Pts',(119.149575814359,5.49369507254455,337.202742751828));
#20502=CARTESIAN_POINT('Ctrl Pts',(119.156973263563,5.4330425872697,337.34836695099));
#20503=CARTESIAN_POINT('Ctrl Pts',(119.164370712767,5.36666810613794,337.49134582125));
#20504=CARTESIAN_POINT('Ctrl Pts',(119.17176784123,5.300296502888,337.634318492197));
#20505=CARTESIAN_POINT('Ctrl Pts',(119.179164969694,5.22820355422409,337.774645723783));
#20506=CARTESIAN_POINT('Ctrl Pts',(119.186562098157,5.1506382255489,337.911847597663));
#20507=CARTESIAN_POINT('Ctrl Pts',(119.193960365594,5.07306095374933,338.049070597206));
#20508=CARTESIAN_POINT('Ctrl Pts',(119.201358633031,4.99000980787323,338.18316695595));
#20509=CARTESIAN_POINT('Ctrl Pts',(119.208756900467,4.90177873629108,338.313683114443));
#20510=CARTESIAN_POINT('Ctrl Pts',(119.216157766993,4.81351666820564,338.444245124635));
#20511=CARTESIAN_POINT('Ctrl Pts',(119.223558633519,4.72007126015613,338.571224121381));
#20512=CARTESIAN_POINT('Ctrl Pts',(119.230959500045,4.62177853575142,338.694197305095));
#20513=CARTESIAN_POINT('Ctrl Pts',(119.238368493429,4.52337787653811,338.817305525121));
#20514=CARTESIAN_POINT('Ctrl Pts',(119.245777486814,4.42011950417836,338.936398855843));
#20515=CARTESIAN_POINT('Ctrl Pts',(119.253186480199,4.31237879668635,339.051088702607));
#20516=CARTESIAN_POINT('Ctrl Pts',(119.260600037779,4.20457171720212,339.165849202273));
#20517=CARTESIAN_POINT('Ctrl Pts',(119.268013595359,4.09227706595556,339.276200551594));
#20518=CARTESIAN_POINT('Ctrl Pts',(119.27542715294,3.9759051078579,339.381792913387));
#20519=CARTESIAN_POINT('Ctrl Pts',(119.282851265076,3.85936747297324,339.487535605238));
#20520=CARTESIAN_POINT('Ctrl Pts',(119.290275377213,3.73874122331871,339.588505539046));
#20521=CARTESIAN_POINT('Ctrl Pts',(119.29769948935,3.6144681730844,339.684394345938));
#20522=CARTESIAN_POINT('Ctrl Pts',(119.301556614504,3.54990332017233,339.734212441666));
#20523=CARTESIAN_POINT('Ctrl Pts',(119.305413739659,3.48435457582328,339.78265975426));
#20524=CARTESIAN_POINT('Ctrl Pts',(119.309270864814,3.41788662942578,339.829697873666));
#20525=CARTESIAN_POINT('Ctrl Pts',(119.316694842252,3.28995286668404,339.920234198828));
#20526=CARTESIAN_POINT('Ctrl Pts',(119.32411881969,3.15822630317177,340.00582034007));
#20527=CARTESIAN_POINT('Ctrl Pts',(119.331542797128,3.02312708119711,340.086121627865));
#20528=CARTESIAN_POINT('Ctrl Pts',(119.338958013155,2.88818729663119,340.166328148058));
#20529=CARTESIAN_POINT('Ctrl Pts',(119.346373229183,2.74988309404062,340.241262040663));
#20530=CARTESIAN_POINT('Ctrl Pts',(119.353788445211,2.60866585932778,340.310630188299));
#20531=CARTESIAN_POINT('Ctrl Pts',(119.361196526355,2.46758450312711,340.379931590253));
#20532=CARTESIAN_POINT('Ctrl Pts',(119.368604607499,2.32359602760543,340.443677745259));
#20533=CARTESIAN_POINT('Ctrl Pts',(119.376012688643,2.17717874839424,340.501620057768));
#20534=CARTESIAN_POINT('Ctrl Pts',(119.383415255817,2.03087045023813,340.559519242757));
#20535=CARTESIAN_POINT('Ctrl Pts',(119.390817822991,1.88213729353113,340.611623050069));
#20536=CARTESIAN_POINT('Ctrl Pts',(119.398220390165,1.73147992728075,340.657729917902));
#20537=CARTESIAN_POINT('Ctrl Pts',(119.40561905992,1.58090188147526,340.703812510671));
#20538=CARTESIAN_POINT('Ctrl Pts',(119.413017729674,1.42840199972534,340.743904343093));
#20539=CARTESIAN_POINT('Ctrl Pts',(119.420416399429,1.2744984344318,340.777852914633));
#20540=CARTESIAN_POINT('Ctrl Pts',(119.427813848633,1.12062025844746,340.811795885713));
#20541=CARTESIAN_POINT('Ctrl Pts',(119.435211297837,0.965339222595319,340.839597526962));
#20542=CARTESIAN_POINT('Ctrl Pts',(119.442608747041,0.809186199965505,340.861155880565));
#20543=CARTESIAN_POINT('Ctrl Pts',(119.450005875504,0.653039947858573,340.882713299436));
#20544=CARTESIAN_POINT('Ctrl Pts',(119.457403003968,0.496022153852965,340.898027917855));
#20545=CARTESIAN_POINT('Ctrl Pts',(119.464800132431,0.338671120990257,340.907049384787));
#20546=CARTESIAN_POINT('Ctrl Pts',(119.472198399868,0.181295859996387,340.916072240799));
#20547=CARTESIAN_POINT('Ctrl Pts',(119.479596667304,0.0235876306015942,
340.918799994577));
#20548=CARTESIAN_POINT('Ctrl Pts',(119.486994934741,-0.133913087046379,
340.915234386533));
#20549=CARTESIAN_POINT('Ctrl Pts',(119.494395801267,-0.291469136352832,
340.911667525853));
#20550=CARTESIAN_POINT('Ctrl Pts',(119.501796667793,-0.448817155885963,
340.901802909846));
#20551=CARTESIAN_POINT('Ctrl Pts',(119.509197534318,-0.605419762799319,
340.885694306818));
#20552=CARTESIAN_POINT('Ctrl Pts',(119.516606527703,-0.762194334346921,
340.869568015004));
#20553=CARTESIAN_POINT('Ctrl Pts',(119.524015521088,-0.918221487144169,
340.847184081594));
#20554=CARTESIAN_POINT('Ctrl Pts',(119.531424514473,-1.07297130507276,340.818647879103));
#20555=CARTESIAN_POINT('Ctrl Pts',(119.538838072053,-1.22781645422714,340.790094097327));
#20556=CARTESIAN_POINT('Ctrl Pts',(119.546251629633,-1.38138233736974,340.75538057647));
#20557=CARTESIAN_POINT('Ctrl Pts',(119.553665187213,-1.53315275106377,340.714663000073));
#20558=CARTESIAN_POINT('Ctrl Pts',(119.56108929935,-1.68513923772676,340.673887454753));
#20559=CARTESIAN_POINT('Ctrl Pts',(119.568513411487,-1.83532479438577,340.627090892807));
#20560=CARTESIAN_POINT('Ctrl Pts',(119.575937523623,-1.98321101606706,340.574477969124));
#20561=CARTESIAN_POINT('Ctrl Pts',(119.579794648778,-2.06004386223038,340.547143437039));
#20562=CARTESIAN_POINT('Ctrl Pts',(119.583651773933,-2.13625642772459,340.518239720244));
#20563=CARTESIAN_POINT('Ctrl Pts',(119.587508899088,-2.21178140557564,340.487800431544));
#20564=CARTESIAN_POINT('Ctrl Pts',(119.594932876526,-2.35714763277035,340.429212601625));
#20565=CARTESIAN_POINT('Ctrl Pts',(119.602356853964,-2.50040364682574,340.364756496062));
#20566=CARTESIAN_POINT('Ctrl Pts',(119.609780831402,-2.64104065388809,340.294604312601));
#20567=CARTESIAN_POINT('Ctrl Pts',(119.617196047429,-2.78151168812214,340.224534919271));
#20568=CARTESIAN_POINT('Ctrl Pts',(119.624611263457,-2.91936953697372,340.148782993716));
#20569=CARTESIAN_POINT('Ctrl Pts',(119.632026479485,-3.05412344097235,340.067569493337));
#20570=CARTESIAN_POINT('Ctrl Pts',(119.639434560629,-3.18874768544304,339.98643413618));
#20571=CARTESIAN_POINT('Ctrl Pts',(119.646842641773,-3.32027361331372,339.899847857481));
#20572=CARTESIAN_POINT('Ctrl Pts',(119.654250722917,-3.44823333125121,339.808078353745));
#20573=CARTESIAN_POINT('Ctrl Pts',(119.661653290091,-3.57609780643372,339.716377155726));
#20574=CARTESIAN_POINT('Ctrl Pts',(119.669055857265,-3.70040105498996,339.61950063102));
#20575=CARTESIAN_POINT('Ctrl Pts',(119.676458424439,-3.82070264939387,339.517760709402));
#20576=CARTESIAN_POINT('Ctrl Pts',(119.683857094194,-3.9409409055341,339.416074353407));
#20577=CARTESIAN_POINT('Ctrl Pts',(119.691255763949,-4.05718141919617,339.309529940394));
#20578=CARTESIAN_POINT('Ctrl Pts',(119.698654433703,-4.16901554743048,339.198480668978));
#20579=CARTESIAN_POINT('Ctrl Pts',(119.706051882907,-4.28083122650625,339.087449717244));
#20580=CARTESIAN_POINT('Ctrl Pts',(119.713449332111,-4.38824169827882,338.971915644758));
#20581=CARTESIAN_POINT('Ctrl Pts',(119.720846781315,-4.49087393835445,338.852269698802));
#20582=CARTESIAN_POINT('Ctrl Pts',(119.728243909779,-4.59350172847507,338.732628940486));
#20583=CARTESIAN_POINT('Ctrl Pts',(119.735641038242,-4.69135145584257,338.608876946457));
#20584=CARTESIAN_POINT('Ctrl Pts',(119.743038166706,-4.7840894725324,338.481439139394));
#20585=CARTESIAN_POINT('Ctrl Pts',(119.750436434142,-4.87684176856185,338.353981710089));
#20586=CARTESIAN_POINT('Ctrl Pts',(119.757834701579,-4.96448056712965,338.222837639521));
#20587=CARTESIAN_POINT('Ctrl Pts',(119.765232969016,-5.04671484696492,338.088462370812));
#20588=CARTESIAN_POINT('Ctrl Pts',(119.772633835541,-5.12897801656741,337.954039894659));
#20589=CARTESIAN_POINT('Ctrl Pts',(119.780034702067,-5.20583269251164,337.816384278407));
#20590=CARTESIAN_POINT('Ctrl Pts',(119.787435568593,-5.27703328101997,337.675976515874));
#20591=CARTESIAN_POINT('Ctrl Pts',(119.794844561978,-5.3483120545816,337.535414572193));
#20592=CARTESIAN_POINT('Ctrl Pts',(119.802253555362,-5.41392417265137,337.392094779954));
#20593=CARTESIAN_POINT('Ctrl Pts',(119.809662548747,-5.47367147720706,337.24651978004));
#20594=CARTESIAN_POINT('Ctrl Pts',(119.817076106328,-5.5334555881633,337.100855100904));
#20595=CARTESIAN_POINT('Ctrl Pts',(119.824489663908,-5.58736755887069,336.952932795587));
#20596=CARTESIAN_POINT('Ctrl Pts',(119.831903221488,-5.63525895964167,336.803271199869));
#20597=CARTESIAN_POINT('Ctrl Pts',(119.839327333625,-5.68321854258926,336.653396533471));
#20598=CARTESIAN_POINT('Ctrl Pts',(119.846751445761,-5.72514033764196,336.501777989953));
#20599=CARTESIAN_POINT('Ctrl Pts',(119.854175557898,-5.76092672793034,336.348945439192));
#20600=CARTESIAN_POINT('Ctrl Pts',(119.858032683053,-5.77951919846822,336.269542775936));
#20601=CARTESIAN_POINT('Ctrl Pts',(119.861889808207,-5.79645643864578,336.189812544041));
#20602=CARTESIAN_POINT('Ctrl Pts',(119.865746933362,-5.81173029052009,336.109829533195));
#20603=CARTESIAN_POINT('Ctrl Pts',(119.876717981006,-5.85517460459028,335.882329157253));
#20604=CARTESIAN_POINT('Ctrl Pts',(119.88768902865,-5.88527075000024,335.652204915708));
#20605=CARTESIAN_POINT('Ctrl Pts',(119.898660076294,-5.90177227769661,335.420730964765));
#20606=CARTESIAN_POINT('Ctrl Pts',(119.905207257627,-5.91161987818216,335.282594482274));
#20607=CARTESIAN_POINT('Ctrl Pts',(119.911754438961,-5.91662676190817,335.143977687089));
#20608=CARTESIAN_POINT('Ctrl Pts',(119.918301620294,-5.91674775276501,335.005156806208));
#20609=CARTESIAN_POINT('',(121.668301620294,-5.90704278596851,335.000701560224));
#20610=CARTESIAN_POINT('Ctrl Pts',(119.918302821709,-5.91937129153481,335.005133607679));
#20611=CARTESIAN_POINT('Ctrl Pts',(119.993530203684,-5.9047448003301,333.409354599871));
#20612=CARTESIAN_POINT('Ctrl Pts',(120.161503597084,-4.41496513658335,329.822132368592));
#20613=CARTESIAN_POINT('Ctrl Pts',(120.42222300191,1.6527734744595,328.201399940917));
#20614=CARTESIAN_POINT('Ctrl Pts',(120.700461036183,6.6114983946026,332.710739879489));
#20615=CARTESIAN_POINT('Ctrl Pts',(120.978699070458,5.50294882358002,339.320900041228));
#20616=CARTESIAN_POINT('Ctrl Pts',(121.256937104732,-0.655575659453675,
341.965834011514));
#20617=CARTESIAN_POINT('Ctrl Pts',(121.486804621343,-5.24644207849654,338.869813694043));
#20618=CARTESIAN_POINT('Ctrl Pts',(121.623926126531,-5.90804155338697,335.94701070509));
#20619=CARTESIAN_POINT('Ctrl Pts',(121.668301620294,-5.90704278596851,335.000701560224));
#20620=CARTESIAN_POINT('',(123.418301620294,-5.91678917890862,334.994557826597));
#20621=CARTESIAN_POINT('Ctrl Pts',(121.668301620294,-5.90704278596851,335.000701560224));
#20622=CARTESIAN_POINT('Ctrl Pts',(121.716672137956,-5.90595410181071,333.96919837404));
#20623=CARTESIAN_POINT('Ctrl Pts',(121.85778866704,-5.15714314318895,330.95840379715));
#20624=CARTESIAN_POINT('Ctrl Pts',(122.091651207554,-0.355313788212134,
328.012412788873));
#20625=CARTESIAN_POINT('Ctrl Pts',(122.369889241826,5.68373048077245,330.919824667594));
#20626=CARTESIAN_POINT('Ctrl Pts',(122.648127276101,6.50689917927394,337.571553225575));
#20627=CARTESIAN_POINT('Ctrl Pts',(122.926365310375,1.35878254263427,341.86340534451));
#20628=CARTESIAN_POINT('Ctrl Pts',(123.183090091772,-4.5418059823907,340.011960697189));
#20629=CARTESIAN_POINT('Ctrl Pts',(123.347068861746,-5.90282340540148,336.507293395397));
#20630=CARTESIAN_POINT('Ctrl Pts',(123.418301620294,-5.91678917890862,334.994557826597));
#20631=CARTESIAN_POINT('',(125.168301620294,-5.92166611962084,335.002060437347));
#20632=CARTESIAN_POINT('Ctrl Pts',(123.418301620294,-5.91678917890862,334.994557826597));
#20633=CARTESIAN_POINT('Ctrl Pts',(123.43981487317,-5.92100703068346,334.537691302128));
#20634=CARTESIAN_POINT('Ctrl Pts',(123.554074137475,-5.66376034564121,332.115921753525));
#20635=CARTESIAN_POINT('Ctrl Pts',(123.761079413193,-2.33387325834533,328.404118062362));
#20636=CARTESIAN_POINT('Ctrl Pts',(124.039317447472,4.28362510061816,329.467985997979));
#20637=CARTESIAN_POINT('Ctrl Pts',(124.317555481744,6.97010393094322,335.608501530848));
#20638=CARTESIAN_POINT('Ctrl Pts',(124.595793516019,3.2602212624124,341.190604190331));
#20639=CARTESIAN_POINT('Ctrl Pts',(124.874031550292,-3.44151833785114,341.091680757513));
#20640=CARTESIAN_POINT('Ctrl Pts',(125.064867585051,-5.8719165109706,337.189631756557));
#20641=CARTESIAN_POINT('Ctrl Pts',(125.162957608385,-5.92613979826577,335.115110298055));
#20642=CARTESIAN_POINT('Ctrl Pts',(125.168301620294,-5.92563084334104,335.002061816868));
#20643=CARTESIAN_POINT('',(126.918301605958,-5.91317602257575,335.004338125692));
#20644=CARTESIAN_POINT('Ctrl Pts',(125.168301620294,-5.91674964183415,335.002058726664));
#20645=CARTESIAN_POINT('Ctrl Pts',(125.175660465658,-5.91680372602739,334.846621564152));
#20646=CARTESIAN_POINT('Ctrl Pts',(125.183019311023,-5.91072843215637,334.690935239553));
#20647=CARTESIAN_POINT('Ctrl Pts',(125.190378156387,-5.89849104658582,334.535528326109));
#20648=CARTESIAN_POINT('Ctrl Pts',(125.197728580823,-5.88626766459175,334.380299249066));
#20649=CARTESIAN_POINT('Ctrl Pts',(125.205079005259,-5.86789625240156,334.225349322313));
#20650=CARTESIAN_POINT('Ctrl Pts',(125.212429429694,-5.84339606690749,334.071208867533));
#20651=CARTESIAN_POINT('Ctrl Pts',(125.219773114474,-5.81891834580424,333.917209745209));
#20652=CARTESIAN_POINT('Ctrl Pts',(125.227116799254,-5.78832309503642,333.764018990799));
#20653=CARTESIAN_POINT('Ctrl Pts',(125.234460484035,-5.7516814910038,333.612163342268));
#20654=CARTESIAN_POINT('Ctrl Pts',(125.241799104385,-5.71506515614384,333.460412418044));
#20655=CARTESIAN_POINT('Ctrl Pts',(125.249137724735,-5.67241085738215,333.309995135077));
#20656=CARTESIAN_POINT('Ctrl Pts',(125.256476345085,-5.62384108261946,333.161429348667));
#20657=CARTESIAN_POINT('Ctrl Pts',(125.263812275111,-5.57528911344133,333.012918026185));
#20658=CARTESIAN_POINT('Ctrl Pts',(125.271148205138,-5.52082609893917,332.866257211193));
#20659=CARTESIAN_POINT('Ctrl Pts',(125.278484135164,-5.46062473218843,332.721950813369));
#20660=CARTESIAN_POINT('Ctrl Pts',(125.285818790569,-5.40043382545311,332.577669488847));
#20661=CARTESIAN_POINT('Ctrl Pts',(125.293153445974,-5.33450669609768,332.435742118593));
#20662=CARTESIAN_POINT('Ctrl Pts',(125.300488101379,-5.26306455513068,332.296653545876));
#20663=CARTESIAN_POINT('Ctrl Pts',(125.307822991486,-5.19162012807683,332.157560522443));
#20664=CARTESIAN_POINT('Ctrl Pts',(125.315157881594,-5.1146605117602,332.021306815763));
#20665=CARTESIAN_POINT('Ctrl Pts',(125.322492771702,-5.03245322137383,331.888353307783));
#20666=CARTESIAN_POINT('Ctrl Pts',(125.329829405769,-4.95022638519947,331.755368188481));
#20667=CARTESIAN_POINT('Ctrl Pts',(125.337166039837,-4.8627495918676,331.625685152828));
#20668=CARTESIAN_POINT('Ctrl Pts',(125.344502673904,-4.77033394129497,331.499736488344));
#20669=CARTESIAN_POINT('Ctrl Pts',(125.351846889461,-4.67782279076226,331.373657671745));
#20670=CARTESIAN_POINT('Ctrl Pts',(125.359191105017,-4.58036281404226,331.251321241386));
#20671=CARTESIAN_POINT('Ctrl Pts',(125.366535320574,-4.47830613495872,331.13312726818));
#20672=CARTESIAN_POINT('Ctrl Pts',(125.373883425499,-4.37619540844046,331.014870701511));
#20673=CARTESIAN_POINT('Ctrl Pts',(125.381231530424,-4.26948338942717,330.900761239732));
#20674=CARTESIAN_POINT('Ctrl Pts',(125.388579635349,-4.1585589029352,330.791161868957));
#20675=CARTESIAN_POINT('Ctrl Pts',(125.395938932375,-4.04746546430145,330.681395564361));
#20676=CARTESIAN_POINT('Ctrl Pts',(125.403298229401,-3.93214702006758,330.576153331447));
#20677=CARTESIAN_POINT('Ctrl Pts',(125.410657526427,-3.81302603730524,330.475758295434));
#20678=CARTESIAN_POINT('Ctrl Pts',(125.417274223898,-3.7059251141289,330.385493752698));
#20679=CARTESIAN_POINT('Ctrl Pts',(125.423890921369,-3.59575091723202,330.299147088162));
#20680=CARTESIAN_POINT('Ctrl Pts',(125.43050761884,-3.48282925362775,330.216922439206));
#20681=CARTESIAN_POINT('Ctrl Pts',(125.437931596278,-3.35613041534751,330.124665850272));
#20682=CARTESIAN_POINT('Ctrl Pts',(125.445355573716,-3.22557223999351,330.037307748441));
#20683=CARTESIAN_POINT('Ctrl Pts',(125.452779551154,-3.09157030976495,329.95518844928));
#20684=CARTESIAN_POINT('Ctrl Pts',(125.460194767182,-2.95772652197589,329.873166063247));
#20685=CARTESIAN_POINT('Ctrl Pts',(125.46760998321,-2.82044738418279,329.79637036648));
#20686=CARTESIAN_POINT('Ctrl Pts',(125.475025199237,-2.68018028074308,329.725100548331));
#20687=CARTESIAN_POINT('Ctrl Pts',(125.482433280381,-2.54004814160414,329.653899305642));
#20688=CARTESIAN_POINT('Ctrl Pts',(125.489841361525,-2.39693409092009,329.588213524397));
#20689=CARTESIAN_POINT('Ctrl Pts',(125.497249442669,-2.25131304185891,329.52829824003));
#20690=CARTESIAN_POINT('Ctrl Pts',(125.504652009843,-2.10580038120366,329.468427551703));
#20691=CARTESIAN_POINT('Ctrl Pts',(125.512054577017,-1.95778478131893,329.41431894951));
#20692=CARTESIAN_POINT('Ctrl Pts',(125.519457144191,-1.80776412218853,329.366180741182));
#20693=CARTESIAN_POINT('Ctrl Pts',(125.526855813946,-1.65782244827945,329.31806787741));
#20694=CARTESIAN_POINT('Ctrl Pts',(125.534254483701,-1.50587817199397,329.275919261005));
#20695=CARTESIAN_POINT('Ctrl Pts',(125.541653153456,-1.35244733798393,329.239894379399));
#20696=CARTESIAN_POINT('Ctrl Pts',(125.54905060266,-1.19904181529744,329.20387544078));
#20697=CARTESIAN_POINT('Ctrl Pts',(125.556448051864,-1.04415058457771,329.173978317212));
#20698=CARTESIAN_POINT('Ctrl Pts',(125.563845501068,-0.888303092893294,
329.150312129895));
#20699=CARTESIAN_POINT('Ctrl Pts',(125.571242629531,-0.732462358484304,
329.126646968702));
#20700=CARTESIAN_POINT('Ctrl Pts',(125.578639757995,-0.575665814531576,
329.109212262618));
#20701=CARTESIAN_POINT('Ctrl Pts',(125.586036886458,-0.418451034642092,
329.098065631159));
#20702=CARTESIAN_POINT('Ctrl Pts',(125.593435153895,-0.261212047601114,
329.086917283397));
#20703=CARTESIAN_POINT('Ctrl Pts',(125.600833421331,-0.103555068698107,
329.082058964482));
#20704=CARTESIAN_POINT('Ctrl Pts',(125.608231688768,0.0539794477389267,
329.083496236651));
#20705=CARTESIAN_POINT('Ctrl Pts',(125.615632555294,0.211569307707187,329.084934013749));
#20706=CARTESIAN_POINT('Ctrl Pts',(125.623033421819,0.36903624659141,329.092671782033));
#20707=CARTESIAN_POINT('Ctrl Pts',(125.630434288345,0.525842204127269,329.106663038748));
#20708=CARTESIAN_POINT('Ctrl Pts',(125.63784328173,0.682820349596862,329.1206696592));
#20709=CARTESIAN_POINT('Ctrl Pts',(125.645252275115,0.839135692259169,329.140943448517));
#20710=CARTESIAN_POINT('Ctrl Pts',(125.652661268499,0.994256940666024,329.167386203559));
#20711=CARTESIAN_POINT('Ctrl Pts',(125.66007482608,1.14947374911271,329.19384524825));
#20712=CARTESIAN_POINT('Ctrl Pts',(125.66748838366,1.30349463326513,329.226480754076));
#20713=CARTESIAN_POINT('Ctrl Pts',(125.67490194124,1.45580133334682,329.265144026192));
#20714=CARTESIAN_POINT('Ctrl Pts',(125.682326053377,1.60832486989955,329.303862342553));
#20715=CARTESIAN_POINT('Ctrl Pts',(125.689750165513,1.75912899148776,329.348625458518));
#20716=CARTESIAN_POINT('Ctrl Pts',(125.69717427765,1.90771257351594,329.399235471889));
#20717=CARTESIAN_POINT('Ctrl Pts',(125.701031402805,1.98490772645645,329.425529411429));
#20718=CARTESIAN_POINT('Ctrl Pts',(125.70488852796,2.06150385678267,329.453400773127));
#20719=CARTESIAN_POINT('Ctrl Pts',(125.708745653115,2.13743320951783,329.482816856642));
#20720=CARTESIAN_POINT('Ctrl Pts',(125.716169630553,2.28357775473181,329.5394352788));
#20721=CARTESIAN_POINT('Ctrl Pts',(125.723593607991,2.42769156637605,329.601949952284));
#20722=CARTESIAN_POINT('Ctrl Pts',(125.731017585429,2.5692635704555,329.670195569439));
#20723=CARTESIAN_POINT('Ctrl Pts',(125.738432801456,2.71066849826958,329.738360646497));
#20724=CARTESIAN_POINT('Ctrl Pts',(125.745848017484,2.8495372565809,329.812243044133));
#20725=CARTESIAN_POINT('Ctrl Pts',(125.753263233512,2.98537614533413,329.891628455822));
#20726=CARTESIAN_POINT('Ctrl Pts',(125.760671314656,3.12108433059251,329.970937483267));
#20727=CARTESIAN_POINT('Ctrl Pts',(125.7680793958,3.25376813009427,330.055738796411));
#20728=CARTESIAN_POINT('Ctrl Pts',(125.775487476944,3.3829560763368,330.145771044947));
#20729=CARTESIAN_POINT('Ctrl Pts',(125.782890044118,3.51204786563145,330.235736280836));
#20730=CARTESIAN_POINT('Ctrl Pts',(125.790292611292,3.63764867780338,330.330924487156));
#20731=CARTESIAN_POINT('Ctrl Pts',(125.797695178466,3.75931391100921,330.431029713273));
#20732=CARTESIAN_POINT('Ctrl Pts',(125.805093848221,3.88091508800178,330.531082234427));
#20733=CARTESIAN_POINT('Ctrl Pts',(125.812492517976,3.99858452519743,330.636046383121));
#20734=CARTESIAN_POINT('Ctrl Pts',(125.81989118773,4.1119088448398,330.7455745142));
#20735=CARTESIAN_POINT('Ctrl Pts',(125.827288636934,4.2252144694881,330.855084576537));
#20736=CARTESIAN_POINT('Ctrl Pts',(125.834686086138,4.33417613112258,330.969156867851));
#20737=CARTESIAN_POINT('Ctrl Pts',(125.842083535342,4.43841555321163,331.087405216546));
#20738=CARTESIAN_POINT('Ctrl Pts',(125.849480663806,4.54265045566111,331.2056484382));
#20739=CARTESIAN_POINT('Ctrl Pts',(125.856877792269,4.64216327887674,331.328067077253));
#20740=CARTESIAN_POINT('Ctrl Pts',(125.864274920733,4.73661465745414,331.454240257816));
#20741=CARTESIAN_POINT('Ctrl Pts',(125.871673188169,4.83108057918615,331.5804328659));
#20742=CARTESIAN_POINT('Ctrl Pts',(125.879071455606,4.92048328084934,331.71038086779));
#20743=CARTESIAN_POINT('Ctrl Pts',(125.886469723043,5.00452561419233,331.843632793956));
#20744=CARTESIAN_POINT('Ctrl Pts',(125.893870589569,5.08859747249114,331.976931532925));
#20745=CARTESIAN_POINT('Ctrl Pts',(125.901271456094,5.16730501414479,332.113536191656));
#20746=CARTESIAN_POINT('Ctrl Pts',(125.90867232262,5.24039616903024,332.252969138485));
#20747=CARTESIAN_POINT('Ctrl Pts',(125.916081316005,5.31356758499118,332.39255519602));
#20748=CARTESIAN_POINT('Ctrl Pts',(125.92349030939,5.38111012431931,332.534975413216));
#20749=CARTESIAN_POINT('Ctrl Pts',(125.930899302774,5.44281885584106,332.679729872407));
#20750=CARTESIAN_POINT('Ctrl Pts',(125.938312860355,5.50456560207012,332.824573505338));
#20751=CARTESIAN_POINT('Ctrl Pts',(125.945726417935,5.5604712471035,332.971753897542));
#20752=CARTESIAN_POINT('Ctrl Pts',(125.953139975515,5.61038037150751,333.120754766002));
#20753=CARTESIAN_POINT('Ctrl Pts',(125.960564087652,5.66036055068711,333.269967764477));
#20754=CARTESIAN_POINT('Ctrl Pts',(125.967988199788,5.70432705482221,333.421006058142));
#20755=CARTESIAN_POINT('Ctrl Pts',(125.975412311925,5.74217511682058,333.573341144398));
#20756=CARTESIAN_POINT('Ctrl Pts',(125.97926943708,5.76183870881543,333.652485354815));
#20757=CARTESIAN_POINT('Ctrl Pts',(125.983126562234,5.77985164735605,333.731979467978));
#20758=CARTESIAN_POINT('Ctrl Pts',(125.986983687388,5.79620476475206,333.81174881125));
#20759=CARTESIAN_POINT('Ctrl Pts',(125.994407664826,5.82768032484627,333.965284354171));
#20760=CARTESIAN_POINT('Ctrl Pts',(126.001831642264,5.85309865495061,334.120303009829));
#20761=CARTESIAN_POINT('Ctrl Pts',(126.009255619702,5.87232219433602,334.276285547741));
#20762=CARTESIAN_POINT('Ctrl Pts',(126.01667083573,5.89152304705262,334.432084002789));
#20763=CARTESIAN_POINT('Ctrl Pts',(126.024086051758,5.90454361607854,334.58884370902));
#20764=CARTESIAN_POINT('Ctrl Pts',(126.031501267785,5.91129694691432,334.746033529966));
#20765=CARTESIAN_POINT('Ctrl Pts',(126.038909348929,5.91804377972916,334.903072103658));
#20766=CARTESIAN_POINT('Ctrl Pts',(126.046317430073,5.91853536365466,335.060539597784));
#20767=CARTESIAN_POINT('Ctrl Pts',(126.053725511217,5.91273633562185,335.217898113615));
#20768=CARTESIAN_POINT('Ctrl Pts',(126.061128078391,5.90694162391154,335.375139504628));
#20769=CARTESIAN_POINT('Ctrl Pts',(126.068530645565,5.89486563690517,335.532271707497));
#20770=CARTESIAN_POINT('Ctrl Pts',(126.075933212739,5.87652505544912,335.688755279601));
#20771=CARTESIAN_POINT('Ctrl Pts',(126.083331882494,5.858194130229,335.84515646379));
#20772=CARTESIAN_POINT('Ctrl Pts',(126.090730552249,5.83360522261793,336.000909327594));
#20773=CARTESIAN_POINT('Ctrl Pts',(126.098129222003,5.80282697242064,336.155478122098));
#20774=CARTESIAN_POINT('Ctrl Pts',(126.105526671207,5.77205379967888,336.310021417551));
#20775=CARTESIAN_POINT('Ctrl Pts',(126.112924120411,5.73509338361726,336.463380665711));
#20776=CARTESIAN_POINT('Ctrl Pts',(126.120321569615,5.69206575703082,336.615028786164));
#20777=CARTESIAN_POINT('Ctrl Pts',(126.127718698079,5.64903999604724,336.766670331418));
#20778=CARTESIAN_POINT('Ctrl Pts',(126.135115826542,5.59994764946738,336.916600537445));
#20779=CARTESIAN_POINT('Ctrl Pts',(126.142512955006,5.54495899071204,337.064306264541));
#20780=CARTESIAN_POINT('Ctrl Pts',(126.149911222442,5.48996186507595,337.212034734631));
#20781=CARTESIAN_POINT('Ctrl Pts',(126.157309489879,5.42906674976437,337.35753769402));
#20782=CARTESIAN_POINT('Ctrl Pts',(126.164707757315,5.36249249116697,337.500320948334));
#20783=CARTESIAN_POINT('Ctrl Pts',(126.172108623841,5.29589484433234,337.643154363907));
#20784=CARTESIAN_POINT('Ctrl Pts',(126.179509490367,5.22361423949961,337.783265834048));
#20785=CARTESIAN_POINT('Ctrl Pts',(126.186910356893,5.14591591771836,337.920184913712));
#20786=CARTESIAN_POINT('Ctrl Pts',(126.194319350277,5.06813227575147,338.057254343616));
#20787=CARTESIAN_POINT('Ctrl Pts',(126.201728343662,4.9849192203301,338.191124057489));
#20788=CARTESIAN_POINT('Ctrl Pts',(126.209137337047,4.8965862428685,338.321351190201));
#20789=CARTESIAN_POINT('Ctrl Pts',(126.216550894627,4.80819884924603,338.451658547319));
#20790=CARTESIAN_POINT('Ctrl Pts',(126.223964452207,4.7146854698793,338.578318552352));
#20791=CARTESIAN_POINT('Ctrl Pts',(126.231378009788,4.61639615179771,338.70092111942));
#20792=CARTESIAN_POINT('Ctrl Pts',(126.238802121924,4.51796690087738,338.823698233687));
#20793=CARTESIAN_POINT('Ctrl Pts',(126.246226234061,4.41474837565924,338.942406092276));
#20794=CARTESIAN_POINT('Ctrl Pts',(126.253650346198,4.30712830976852,339.056670591223));
#20795=CARTESIAN_POINT('Ctrl Pts',(126.257507471352,4.25121535268365,339.116035598789));
#20796=CARTESIAN_POINT('Ctrl Pts',(126.261364596507,4.19411489161567,339.174201889104));
#20797=CARTESIAN_POINT('Ctrl Pts',(126.265221721662,4.13588475921477,339.231121343213));
#20798=CARTESIAN_POINT('Ctrl Pts',(126.2726456991,4.02380667726986,339.34067670534));
#20799=CARTESIAN_POINT('Ctrl Pts',(126.280069676538,3.9072034994721,339.445941010946));
#20800=CARTESIAN_POINT('Ctrl Pts',(126.287493653976,3.78643741580906,339.546517596871));
#20801=CARTESIAN_POINT('Ctrl Pts',(126.294908870003,3.6658138542949,339.646975487293));
#20802=CARTESIAN_POINT('Ctrl Pts',(126.302324086031,3.54103745002422,339.74275643348));
#20803=CARTESIAN_POINT('Ctrl Pts',(126.309739302058,3.41250779091417,339.833499885119));
#20804=CARTESIAN_POINT('Ctrl Pts',(126.317147383202,3.28410180239487,339.924156023867));
#20805=CARTESIAN_POINT('Ctrl Pts',(126.324555464347,3.15195005143188,340.009784103832));
#20806=CARTESIAN_POINT('Ctrl Pts',(126.331963545491,3.01648573155637,340.090063299588));
#20807=CARTESIAN_POINT('Ctrl Pts',(126.339366112665,2.88112224024904,340.170282742073));
#20808=CARTESIAN_POINT('Ctrl Pts',(126.346768679839,2.74245140909999,340.245161038185));
#20809=CARTESIAN_POINT('Ctrl Pts',(126.354171247013,2.60093589387887,340.314420291851));
#20810=CARTESIAN_POINT('Ctrl Pts',(126.361569916767,2.45949488595717,340.383643080822));
#20811=CARTESIAN_POINT('Ctrl Pts',(126.368968586522,2.31521251112293,340.447252555533));
#20812=CARTESIAN_POINT('Ctrl Pts',(126.376367256277,2.1685764370063,340.505016512179));
#20813=CARTESIAN_POINT('Ctrl Pts',(126.383764705481,2.02196455328866,340.562770939565));
#20814=CARTESIAN_POINT('Ctrl Pts',(126.391162154685,1.87300008781617,340.614681626114));
#20815=CARTESIAN_POINT('Ctrl Pts',(126.398559603889,1.72219123038617,340.660564276508));
#20816=CARTESIAN_POINT('Ctrl Pts',(126.405956732352,1.57138891176553,340.70644493751));
#20817=CARTESIAN_POINT('Ctrl Pts',(126.413353860816,1.4187427172452,340.746297973406));
#20818=CARTESIAN_POINT('Ctrl Pts',(126.420750989279,1.26477630166613,340.779988881412));
#20819=CARTESIAN_POINT('Ctrl Pts',(126.428149256716,1.11078617910208,340.813684976976));
#20820=CARTESIAN_POINT('Ctrl Pts',(126.435547524152,0.95547579532685,340.841216975654));
#20821=CARTESIAN_POINT('Ctrl Pts',(126.442945791589,0.799379159269492,340.862501473111));
#20822=CARTESIAN_POINT('Ctrl Pts',(126.450346658115,0.64322768482256,340.883793448036));
#20823=CARTESIAN_POINT('Ctrl Pts',(126.45774752464,0.486289777699041,340.898833501481));
#20824=CARTESIAN_POINT('Ctrl Pts',(126.465148391166,0.329104582324897,340.907590095495));
#20825=CARTESIAN_POINT('Ctrl Pts',(126.472557384551,0.171746782578905,340.916356305087));
#20826=CARTESIAN_POINT('Ctrl Pts',(126.479966377936,0.0141415251459065,
340.91882525513));
#20827=CARTESIAN_POINT('Ctrl Pts',(126.48737537132,-0.143171291674783,340.915017543824));
#20828=CARTESIAN_POINT('Ctrl Pts',(126.494788928901,-0.300581018617045,
340.911207486835));
#20829=CARTESIAN_POINT('Ctrl Pts',(126.502202486481,-0.457697574394116,
340.901113087579));
#20830=CARTESIAN_POINT('Ctrl Pts',(126.509616044061,-0.613986678505744,
340.884806787068));
#20831=CARTESIAN_POINT('Ctrl Pts',(126.517040156198,-0.7704982887694,340.868477271552));
#20832=CARTESIAN_POINT('Ctrl Pts',(126.524464268334,-0.926179726250687,
340.845918245364));
#20833=CARTESIAN_POINT('Ctrl Pts',(126.531888380471,-1.08050657403185,340.817253312859));
#20834=CARTESIAN_POINT('Ctrl Pts',(126.535745505626,-1.1606855847594,340.802360726353));
#20835=CARTESIAN_POINT('Ctrl Pts',(126.539602630781,-1.24049919512095,340.785820847726));
#20836=CARTESIAN_POINT('Ctrl Pts',(126.543459755936,-1.3198756442952,340.76765626976));
#20837=CARTESIAN_POINT('Ctrl Pts',(126.550883733374,-1.4726549667486,340.732694112303));
#20838=CARTESIAN_POINT('Ctrl Pts',(126.558307710812,-1.624274637244,340.691604568301));
#20839=CARTESIAN_POINT('Ctrl Pts',(126.56573168825,-1.77420509148286,340.644477553845));
#20840=CARTESIAN_POINT('Ctrl Pts',(126.573146904277,-1.92395860522736,340.597406156356));
#20841=CARTESIAN_POINT('Ctrl Pts',(126.580562120305,-2.07202651829239,340.544311581908));
#20842=CARTESIAN_POINT('Ctrl Pts',(126.587977336333,-2.21788939627793,340.485334738043));
#20843=CARTESIAN_POINT('Ctrl Pts',(126.595385417477,-2.36361192573639,340.4264146414));
#20844=CARTESIAN_POINT('Ctrl Pts',(126.602793498621,-2.50713330028566,340.361623682088));
#20845=CARTESIAN_POINT('Ctrl Pts',(126.610201579765,-2.6479493051041,340.291152524743));
#20846=CARTESIAN_POINT('Ctrl Pts',(126.617604146939,-2.7886604979979,340.220733820368));
#20847=CARTESIAN_POINT('Ctrl Pts',(126.625006714113,-2.9266699983226,340.144643502584));
#20848=CARTESIAN_POINT('Ctrl Pts',(126.632409281287,-3.06149374775632,340.063120242987));
#20849=CARTESIAN_POINT('Ctrl Pts',(126.639807951042,-3.19624651307612,339.98163990503));
#20850=CARTESIAN_POINT('Ctrl Pts',(126.647206620796,-3.32781654935287,339.894732514579));
#20851=CARTESIAN_POINT('Ctrl Pts',(126.654605290551,-3.45574468651726,339.802682502946));
#20852=CARTESIAN_POINT('Ctrl Pts',(126.662002739755,-3.58365171951144,339.710647676708));
#20853=CARTESIAN_POINT('Ctrl Pts',(126.669400188959,-3.70791774314308,339.6134721308));
#20854=CARTESIAN_POINT('Ctrl Pts',(126.676797638163,-3.82811276888865,339.511483480095));
#20855=CARTESIAN_POINT('Ctrl Pts',(126.684194766626,-3.94830258318694,339.409499251441));
#20856=CARTESIAN_POINT('Ctrl Pts',(126.69159189509,-4.06442146599077,339.302702574395));
#20857=CARTESIAN_POINT('Ctrl Pts',(126.698989023553,-4.17607293135745,339.19146101431));
#20858=CARTESIAN_POINT('Ctrl Pts',(126.70638729099,-4.28774158826329,339.080202325802));
#20859=CARTESIAN_POINT('Ctrl Pts',(126.713785558427,-4.39494119368948,338.964497654954));
#20860=CARTESIAN_POINT('Ctrl Pts',(126.721183825863,-4.49731262827982,338.844750926395));
#20861=CARTESIAN_POINT('Ctrl Pts',(126.728584692389,-4.59972002703177,338.724962129551));
#20862=CARTESIAN_POINT('Ctrl Pts',(126.735985558915,-4.6972956354792,338.601128731244));
#20863=CARTESIAN_POINT('Ctrl Pts',(126.743386425441,-4.78972117070168,338.473687042529));
#20864=CARTESIAN_POINT('Ctrl Pts',(126.750795418825,-4.88224819799774,338.346105410656));
#20865=CARTESIAN_POINT('Ctrl Pts',(126.75820441221,-4.96961363894644,338.214907877856));
#20866=CARTESIAN_POINT('Ctrl Pts',(126.765613405595,-5.05154264506381,338.080559602995));
#20867=CARTESIAN_POINT('Ctrl Pts',(126.773026963175,-5.13352212227506,337.946128564962));
#20868=CARTESIAN_POINT('Ctrl Pts',(126.780440520755,-5.21005831026275,337.808543242619));
#20869=CARTESIAN_POINT('Ctrl Pts',(126.787854078336,-5.28092299638487,337.668292125828));
#20870=CARTESIAN_POINT('Ctrl Pts',(126.795278190472,-5.35188857136094,337.527841335895));
#20871=CARTESIAN_POINT('Ctrl Pts',(126.802702302609,-5.41716636378353,337.384717510292));
#20872=CARTESIAN_POINT('Ctrl Pts',(126.810126414746,-5.47657652310742,337.239428531802));
#20873=CARTESIAN_POINT('Ctrl Pts',(126.8139835399,-5.5074424927685,337.163945058046));
#20874=CARTESIAN_POINT('Ctrl Pts',(126.817840665055,-5.53672548023707,337.087877412965));
#20875=CARTESIAN_POINT('Ctrl Pts',(126.82169779021,-5.56440565036725,337.011298168015));
#20876=CARTESIAN_POINT('Ctrl Pts',(126.830305803929,-5.62617997053476,336.840394926689));
#20877=CARTESIAN_POINT('Ctrl Pts',(126.838913817648,-5.68012201448321,336.666518829418));
#20878=CARTESIAN_POINT('Ctrl Pts',(126.847521831367,-5.7259766090411,336.490343059572));
#20879=CARTESIAN_POINT('Ctrl Pts',(126.856096835013,-5.77165536006907,336.314842889838));
#20880=CARTESIAN_POINT('Ctrl Pts',(126.864671838659,-5.80930848155199,336.137060763736));
#20881=CARTESIAN_POINT('Ctrl Pts',(126.873246842305,-5.83873032688343,335.957684046245));
#20882=CARTESIAN_POINT('Ctrl Pts',(126.88175746393,-5.86793126993042,335.779654107863));
#20883=CARTESIAN_POINT('Ctrl Pts',(126.890268085554,-5.88902400299891,335.60005356052));
#20884=CARTESIAN_POINT('Ctrl Pts',(126.898778707178,-5.90185462755575,335.419574210002));
#20885=CARTESIAN_POINT('Ctrl Pts',(126.90528633359,-5.9116655338497,335.281571107497));
#20886=CARTESIAN_POINT('Ctrl Pts',(126.911793960003,-5.91664663233737,335.143054595291));
#20887=CARTESIAN_POINT('Ctrl Pts',(126.918301586416,-5.91674840742824,335.004341162903));
#20888=CARTESIAN_POINT('',(128.668301620294,-5.90987324019195,334.996005152984));
#20889=CARTESIAN_POINT('Ctrl Pts',(126.918301620294,-5.91055548896683,335.004335897736));
#20890=CARTESIAN_POINT('Ctrl Pts',(126.978846355024,-5.90182962359021,333.715137151976));
#20891=CARTESIAN_POINT('Ctrl Pts',(127.132137101179,-4.85228408488346,330.438137618077));
#20892=CARTESIAN_POINT('Ctrl Pts',(127.378173858758,0.561399630138656,328.025944266319));
#20893=CARTESIAN_POINT('Ctrl Pts',(127.656411893032,6.16843780437573,331.698031197188));
#20894=CARTESIAN_POINT('Ctrl Pts',(127.934649927306,6.11479165153577,338.400286161418));
#20895=CARTESIAN_POINT('Ctrl Pts',(128.21288796158,0.449691454254745,341.982148703458));
#20896=CARTESIAN_POINT('Ctrl Pts',(128.457438525909,-4.89222166567316,339.498698145784));
#20897=CARTESIAN_POINT('Ctrl Pts',(128.609243078814,-5.90208820652118,336.253922582036));
#20898=CARTESIAN_POINT('Ctrl Pts',(128.668301620294,-5.90987324019195,334.996005152984));
#20899=CARTESIAN_POINT('',(130.418301620294,-5.92512223992695,334.997412588165));
#20900=CARTESIAN_POINT('Ctrl Pts',(128.668301620294,-5.90987324019195,334.996005152984));
#20901=CARTESIAN_POINT('Ctrl Pts',(128.701989090239,-5.91431388639194,334.278478872759));
#20902=CARTESIAN_POINT('Ctrl Pts',(128.828422571606,-5.46072358895401,331.590931601405));
#20903=CARTESIAN_POINT('Ctrl Pts',(129.047602064403,-1.45139077720003,328.155579810305));
#20904=CARTESIAN_POINT('Ctrl Pts',(129.325840098675,4.97018812648249,330.075586033998));
#20905=CARTESIAN_POINT('Ctrl Pts',(129.60407813295,6.83069874635309,336.514654270055));
#20906=CARTESIAN_POINT('Ctrl Pts',(129.882316167224,2.42277794764036,341.563746638746));
#20907=CARTESIAN_POINT('Ctrl Pts',(130.153723996339,-4.04570561128838,340.613304275294));
#20908=CARTESIAN_POINT('Ctrl Pts',(130.332385814028,-5.91517505445709,336.815309996308));
#20909=CARTESIAN_POINT('Ctrl Pts',(130.418301620294,-5.92512223992695,334.997412588165));
#20910=CARTESIAN_POINT('',(132.168301620294,-5.91772602350224,335.005383180983));
#20911=CARTESIAN_POINT('Ctrl Pts',(130.418301620294,-5.92512223992695,334.997412588165));
#20912=CARTESIAN_POINT('Ctrl Pts',(130.425131825453,-5.92591302942736,334.852891890574));
#20913=CARTESIAN_POINT('Ctrl Pts',(130.431962030612,-5.92108494976179,334.708424922706));
#20914=CARTESIAN_POINT('Ctrl Pts',(130.531538247196,-5.76631470651247,332.608488631998));
#20915=CARTESIAN_POINT('Ctrl Pts',(130.717030270046,-3.34356564080936,328.854010110094));
#20916=CARTESIAN_POINT('Ctrl Pts',(130.995268304318,3.35889879536448,328.862376534545));
#20917=CARTESIAN_POINT('Ctrl Pts',(131.273506338593,6.9789513843005,334.503149422067));
#20918=CARTESIAN_POINT('Ctrl Pts',(131.551744372867,4.19452329701571,340.599874751459));
#20919=CARTESIAN_POINT('Ctrl Pts',(131.829982407141,-2.43915690887765,341.557677675449));
#20920=CARTESIAN_POINT('Ctrl Pts',(132.035501489616,-5.68572389466333,337.82007499618));
#20921=CARTESIAN_POINT('Ctrl Pts',(132.148274560668,-5.92169754062293,335.430510874451));
#20922=CARTESIAN_POINT('Ctrl Pts',(132.168301620294,-5.91775274132979,335.005383205287));
#20923=CARTESIAN_POINT('',(133.918301620327,-5.91674999725183,334.999819665701));
#20924=CARTESIAN_POINT('Ctrl Pts',(132.168301620294,-5.91674755194479,335.005382290896));
#20925=CARTESIAN_POINT('Ctrl Pts',(132.175608191324,-5.91688861786857,334.850308647478));
#20926=CARTESIAN_POINT('Ctrl Pts',(132.182914762354,-5.91092897118882,334.695048870305));
#20927=CARTESIAN_POINT('Ctrl Pts',(132.190221333384,-5.89885154245384,334.54012931971));
#20928=CARTESIAN_POINT('Ctrl Pts',(132.197522434716,-5.88678315488013,334.385325741867));
#20929=CARTESIAN_POINT('Ctrl Pts',(132.204823536047,-5.86860612946989,334.230862265239));
#20930=CARTESIAN_POINT('Ctrl Pts',(132.212124637379,-5.84435546471036,334.077265062648));
#20931=CARTESIAN_POINT('Ctrl Pts',(132.219422532179,-5.82011545047365,333.92373531761));
#20932=CARTESIAN_POINT('Ctrl Pts',(132.226720426978,-5.78980716211582,333.771071468783));
#20933=CARTESIAN_POINT('Ctrl Pts',(132.234018321778,-5.7535174123303,333.619794236894));
#20934=CARTESIAN_POINT('Ctrl Pts',(132.241314622808,-5.71723558777236,333.46855004206));
#20935=CARTESIAN_POINT('Ctrl Pts',(132.248610923838,-5.67497498934015,333.318692235538));
#20936=CARTESIAN_POINT('Ctrl Pts',(132.255907224869,-5.62687342336098,333.170730736066));
#20937=CARTESIAN_POINT('Ctrl Pts',(132.263203465538,-5.57877225532201,333.022770460667));
#20938=CARTESIAN_POINT('Ctrl Pts',(132.270499706206,-5.52483033456661,332.87670682684));
#20939=CARTESIAN_POINT('Ctrl Pts',(132.277795946875,-5.46523506958358,332.733033701906));
#20940=CARTESIAN_POINT('Ctrl Pts',(132.285093660387,-5.40562777450211,332.589331574637));
#20941=CARTESIAN_POINT('Ctrl Pts',(132.292391373899,-5.34036501207566,332.448021271395));
#20942=CARTESIAN_POINT('Ctrl Pts',(132.299689087412,-5.26968184756498,332.309575537588));
#20943=CARTESIAN_POINT('Ctrl Pts',(132.306994129754,-5.19892769849957,332.17099076772));
#20944=CARTESIAN_POINT('Ctrl Pts',(132.314299172097,-5.12274244955002,332.035276656283));
#20945=CARTESIAN_POINT('Ctrl Pts',(132.32160421444,-5.04140685708058,331.902880779841));
#20946=CARTESIAN_POINT('Ctrl Pts',(132.328912947963,-4.96003016638047,331.77041800481));
#20947=CARTESIAN_POINT('Ctrl Pts',(132.336221681486,-4.87349816264455,331.641277123254));
#20948=CARTESIAN_POINT('Ctrl Pts',(132.343530415009,-4.78213378647513,331.515875000699));
#20949=CARTESIAN_POINT('Ctrl Pts',(132.350850335794,-4.69062956156016,331.390280928828));
#20950=CARTESIAN_POINT('Ctrl Pts',(132.358170256578,-4.59427842480844,331.268437350721));
#20951=CARTESIAN_POINT('Ctrl Pts',(132.365490177363,-4.49344291375054,331.150727166936));
#20952=CARTESIAN_POINT('Ctrl Pts',(132.372479610139,-4.39716003766225,331.038331494808));
#20953=CARTESIAN_POINT('Ctrl Pts',(132.379469042914,-4.2967890634065,330.929704339512));
#20954=CARTESIAN_POINT('Ctrl Pts',(132.386458475689,-4.19267440833758,330.825145287777));
#20955=CARTESIAN_POINT('Ctrl Pts',(132.393882453127,-4.08208677196621,330.71408562586));
#20956=CARTESIAN_POINT('Ctrl Pts',(132.401306430565,-3.96691647582864,330.607255489685));
#20957=CARTESIAN_POINT('Ctrl Pts',(132.408730408003,-3.84752031749017,330.505056399798));
#20958=CARTESIAN_POINT('Ctrl Pts',(132.416145624031,-3.72826506458258,330.402977920213));
#20959=CARTESIAN_POINT('Ctrl Pts',(132.423560840059,-3.60479415725262,330.305519848415));
#20960=CARTESIAN_POINT('Ctrl Pts',(132.430976056086,-3.47750227550635,330.213048100686));
#20961=CARTESIAN_POINT('Ctrl Pts',(132.43838413723,-3.35033287336785,330.120665328806));
#20962=CARTESIAN_POINT('Ctrl Pts',(132.445792218375,-3.21935011601256,330.033259547323));
#20963=CARTESIAN_POINT('Ctrl Pts',(132.453200299519,-3.0849828227206,329.951157405304));
#20964=CARTESIAN_POINT('Ctrl Pts',(132.460602866693,-2.95071554145869,329.869116373408));
#20965=CARTESIAN_POINT('Ctrl Pts',(132.468005433867,-2.81306905740038,329.792371314498));
#20966=CARTESIAN_POINT('Ctrl Pts',(132.475408001041,-2.6725022293984,329.721206350277));
#20967=CARTESIAN_POINT('Ctrl Pts',(132.482806670795,-2.53200940921738,329.650078854098));
#20968=CARTESIAN_POINT('Ctrl Pts',(132.49020534055,-2.38859963934369,329.584525769764));
#20969=CARTESIAN_POINT('Ctrl Pts',(132.497604010305,-2.24275740556107,329.524785868817));
#20970=CARTESIAN_POINT('Ctrl Pts',(132.505001459509,-2.09693923121828,329.465055823099));
#20971=CARTESIAN_POINT('Ctrl Pts',(132.512398908713,-1.94868973440439,329.411137198802));
#20972=CARTESIAN_POINT('Ctrl Pts',(132.519796357917,-1.79851456849425,329.363221140632));
#20973=CARTESIAN_POINT('Ctrl Pts',(132.52719348638,-1.64834591391749,329.315307160019));
#20974=CARTESIAN_POINT('Ctrl Pts',(132.534590614844,-1.4962521118089,329.273395341495));
#20975=CARTESIAN_POINT('Ctrl Pts',(132.541987743307,-1.3427549519279,329.237627250726));
#20976=CARTESIAN_POINT('Ctrl Pts',(132.549386010744,-1.18923415731613,329.201853652565));
#20977=CARTESIAN_POINT('Ctrl Pts',(132.55678427818,-1.03430993817985,329.172225750434));
#20978=CARTESIAN_POINT('Ctrl Pts',(132.564182545617,-0.87851512781858,329.148834156111));
#20979=CARTESIAN_POINT('Ctrl Pts',(132.571583412143,-0.722665585101663,
329.125434344075));
#20980=CARTESIAN_POINT('Ctrl Pts',(132.578984278668,-0.565945211059111,
329.108275257264));
#20981=CARTESIAN_POINT('Ctrl Pts',(132.586385145194,-0.408892674791273,
329.097395715195));
#20982=CARTESIAN_POINT('Ctrl Pts',(132.593794138579,-0.251667679824081,
329.086504226348));
#20983=CARTESIAN_POINT('Ctrl Pts',(132.601203131964,-0.0941101667556998,
329.081906078811));
#20984=CARTESIAN_POINT('Ctrl Pts',(132.608612125348,0.0632397370914502,
329.083587970894));
#20985=CARTESIAN_POINT('Ctrl Pts',(132.616025682928,0.220686573906835,329.08527089908));
#20986=CARTESIAN_POINT('Ctrl Pts',(132.623439240509,0.377925174792565,329.093241556974));
#20987=CARTESIAN_POINT('Ctrl Pts',(132.630852798089,0.534420329258209,329.1074347289));
#20988=CARTESIAN_POINT('Ctrl Pts',(132.638276910226,0.691138283226448,329.121648107404));
#20989=CARTESIAN_POINT('Ctrl Pts',(132.645701022362,0.847110307828953,329.142101644517));
#20990=CARTESIAN_POINT('Ctrl Pts',(132.653125134499,1.0018103639836,329.168678832622));
#20991=CARTESIAN_POINT('Ctrl Pts',(132.656982259653,1.08218327147926,329.182486751857));
#20992=CARTESIAN_POINT('Ctrl Pts',(132.660839384808,1.16221306871678,329.197946749815));
#20993=CARTESIAN_POINT('Ctrl Pts',(132.664696509963,1.2418276961715,329.215037205347));
#20994=CARTESIAN_POINT('Ctrl Pts',(132.6721204874,1.39506545078927,329.24793195239));
#20995=CARTESIAN_POINT('Ctrl Pts',(132.679544464838,1.54722644712942,329.286969194867));
#20996=CARTESIAN_POINT('Ctrl Pts',(132.686968442276,1.69777995436494,329.332066179898));
#20997=CARTESIAN_POINT('Ctrl Pts',(132.694383658304,1.84815578580951,329.377109943702));
#20998=CARTESIAN_POINT('Ctrl Pts',(132.701798874332,1.99692755027547,329.428199109019));
#20999=CARTESIAN_POINT('Ctrl Pts',(132.709214090359,2.14357395695826,329.485199799308));
#21000=CARTESIAN_POINT('Ctrl Pts',(132.716622171503,2.29007926120713,329.54214564382));
#21001=CARTESIAN_POINT('Ctrl Pts',(132.724030252647,2.43446293337107,329.604991555171));
#21002=CARTESIAN_POINT('Ctrl Pts',(132.731438333792,2.57621822856086,329.673553698634));
#21003=CARTESIAN_POINT('Ctrl Pts',(132.738840900966,2.71786801269573,329.742064810042));
#21004=CARTESIAN_POINT('Ctrl Pts',(132.74624346814,2.85689298069465,329.816283520038));
#21005=CARTESIAN_POINT('Ctrl Pts',(132.753646035314,2.99280589370071,329.895977718982));
#21006=CARTESIAN_POINT('Ctrl Pts',(132.761044705068,3.12864724915136,329.975629959277));
#21007=CARTESIAN_POINT('Ctrl Pts',(132.768443374823,3.26137949161004,330.060751758909));
#21008=CARTESIAN_POINT('Ctrl Pts',(132.775842044578,3.39053964993582,330.151064916426));
#21009=CARTESIAN_POINT('Ctrl Pts',(132.783239493782,3.51967850084685,330.241363175078));
#21010=CARTESIAN_POINT('Ctrl Pts',(132.790636942986,3.64524613160197,330.336850878255));
#21011=CARTESIAN_POINT('Ctrl Pts',(132.79803439219,3.76680816648433,330.437206250617));
#21012=CARTESIAN_POINT('Ctrl Pts',(132.805431520653,3.88836493064862,330.537557271745));
#21013=CARTESIAN_POINT('Ctrl Pts',(132.812828649117,4.00591615645688,330.642775304813));
#21014=CARTESIAN_POINT('Ctrl Pts',(132.82022577758,4.11906042793937,330.752498174988));
#21015=CARTESIAN_POINT('Ctrl Pts',(132.827624045017,4.23222212081522,330.862237939745));
#21016=CARTESIAN_POINT('Ctrl Pts',(132.835022312454,4.34097524032482,330.976483662888));
#21017=CARTESIAN_POINT('Ctrl Pts',(132.84242057989,4.44495524241974,331.094836308759));
#21018=CARTESIAN_POINT('Ctrl Pts',(132.849821446416,4.5489717737832,331.21323053316));
#21019=CARTESIAN_POINT('Ctrl Pts',(132.857222312942,4.64821160296261,331.335734272713));
#21020=CARTESIAN_POINT('Ctrl Pts',(132.864623179468,4.74235058104108,331.461915556548));
#21021=CARTESIAN_POINT('Ctrl Pts',(132.872032172852,4.83659293271748,331.588235399495));
#21022=CARTESIAN_POINT('Ctrl Pts',(132.879441166237,4.92572302404798,331.718240552102));
#21023=CARTESIAN_POINT('Ctrl Pts',(132.886850159622,5.00945974682138,331.851469611473));
#21024=CARTESIAN_POINT('Ctrl Pts',(132.894263717202,5.09324805430448,331.98478074454));
#21025=CARTESIAN_POINT('Ctrl Pts',(132.901677274782,5.17163618732362,332.121319418906));
#21026=CARTESIAN_POINT('Ctrl Pts',(132.909090832363,5.24438935402489,332.260600272707));
#21027=CARTESIAN_POINT('Ctrl Pts',(132.916514944499,5.31724609817802,332.400079418302));
#21028=CARTESIAN_POINT('Ctrl Pts',(132.923939056636,5.38445169464843,332.542308203863));
#21029=CARTESIAN_POINT('Ctrl Pts',(132.931363168773,5.44581944724451,332.686781222946));
#21030=CARTESIAN_POINT('Ctrl Pts',(132.935220293928,5.47770246542406,332.761840772939));
#21031=CARTESIAN_POINT('Ctrl Pts',(132.939077419082,5.50801053871094,332.837505828788));
#21032=CARTESIAN_POINT('Ctrl Pts',(132.942934544237,5.53672285324849,332.913704093659));
#21033=CARTESIAN_POINT('Ctrl Pts',(132.950358521675,5.59198670048542,333.060366225826));
#21034=CARTESIAN_POINT('Ctrl Pts',(132.957782499113,5.64150249657939,333.209446945721));
#21035=CARTESIAN_POINT('Ctrl Pts',(132.965206476551,5.68505262128808,333.360455168138));
#21036=CARTESIAN_POINT('Ctrl Pts',(132.972621692578,5.72855135029715,333.511285178132));
#21037=CARTESIAN_POINT('Ctrl Pts',(132.980036908606,5.76609831951695,333.664037807627));
#21038=CARTESIAN_POINT('Ctrl Pts',(132.987452124634,5.79752400822152,333.818202243785));
#21039=CARTESIAN_POINT('Ctrl Pts',(132.994860205778,5.82891945928666,333.972218343699));
#21040=CARTESIAN_POINT('Ctrl Pts',(133.002268286922,5.85420528141425,334.127643182641));
#21041=CARTESIAN_POINT('Ctrl Pts',(133.009676368066,5.87326183641131,334.283951144506));
#21042=CARTESIAN_POINT('Ctrl Pts',(133.01707893524,5.89230420726639,334.440142763499));
#21043=CARTESIAN_POINT('Ctrl Pts',(133.024481502414,5.90512649807899,334.597215827704));
#21044=CARTESIAN_POINT('Ctrl Pts',(133.031884069588,5.91166022189539,334.754634999725));
#21045=CARTESIAN_POINT('Ctrl Pts',(133.039282739343,5.91819050573482,334.911971291242));
#21046=CARTESIAN_POINT('Ctrl Pts',(133.046681409097,5.91843880099984,335.069652955714));
#21047=CARTESIAN_POINT('Ctrl Pts',(133.054080078852,5.91238851297488,335.227140120064));
#21048=CARTESIAN_POINT('Ctrl Pts',(133.061477528056,5.90633922305962,335.384601303921));
#21049=CARTESIAN_POINT('Ctrl Pts',(133.06887497726,5.89399342638746,335.541867678763));
#21050=CARTESIAN_POINT('Ctrl Pts',(133.076272426464,5.87538664508347,335.698399837682));
#21051=CARTESIAN_POINT('Ctrl Pts',(133.083669554928,5.85678067053709,335.85492520964));
#21052=CARTESIAN_POINT('Ctrl Pts',(133.091066683391,5.83191429517451,336.01071605837));
#21053=CARTESIAN_POINT('Ctrl Pts',(133.098463811854,5.80087485032623,336.165238831035));
#21054=CARTESIAN_POINT('Ctrl Pts',(133.105862079291,5.76983062617831,336.31978539635));
#21055=CARTESIAN_POINT('Ctrl Pts',(133.113260346728,5.73261151348119,336.473063130902));
#21056=CARTESIAN_POINT('Ctrl Pts',(133.120658614164,5.68935579413008,336.624549540734));
#21057=CARTESIAN_POINT('Ctrl Pts',(133.12805948069,5.64608487858958,336.776089169335));
#21058=CARTESIAN_POINT('Ctrl Pts',(133.135460347216,5.59677323644561,336.925835861617));
#21059=CARTESIAN_POINT('Ctrl Pts',(133.142861213742,5.54160870564134,337.073283269614));
#21060=CARTESIAN_POINT('Ctrl Pts',(133.150270207126,5.4863835989086,337.22089258896));
#21061=CARTESIAN_POINT('Ctrl Pts',(133.157679200511,5.42529289924552,337.366197232037));
#21062=CARTESIAN_POINT('Ctrl Pts',(133.165088193896,5.35857248640835,337.508711117368));
#21063=CARTESIAN_POINT('Ctrl Pts',(133.172501751476,5.29181097149536,337.651312796169));
#21064=CARTESIAN_POINT('Ctrl Pts',(133.179915309056,5.21941300398327,337.791119960849));
#21065=CARTESIAN_POINT('Ctrl Pts',(133.187328866636,5.1416596756735,337.927672512774));
#21066=CARTESIAN_POINT('Ctrl Pts',(133.194752978773,5.06379565126632,338.064419472256));
#21067=CARTESIAN_POINT('Ctrl Pts',(133.20217709091,4.98056123567708,338.197902249049));
#21068=CARTESIAN_POINT('Ctrl Pts',(133.209601203046,4.89228040394408,338.327690341917));
#21069=CARTESIAN_POINT('Ctrl Pts',(133.213458328201,4.84641495761344,338.395120481517));
#21070=CARTESIAN_POINT('Ctrl Pts',(133.217315453356,4.7991880354374,338.46155389032));
#21071=CARTESIAN_POINT('Ctrl Pts',(133.221172578511,4.75064916979636,338.526933941544));
#21072=CARTESIAN_POINT('Ctrl Pts',(133.228596555949,4.65722429273634,338.652773784875));
#21073=CARTESIAN_POINT('Ctrl Pts',(133.236020533387,4.55865497336079,338.775088805969));
#21074=CARTESIAN_POINT('Ctrl Pts',(133.243444510825,4.45523640889637,338.893430248938));
#21075=CARTESIAN_POINT('Ctrl Pts',(133.250859726852,4.35193989389799,339.011632031199));
#21076=CARTESIAN_POINT('Ctrl Pts',(133.25827494288,4.24380576841043,339.125869291409));
#21077=CARTESIAN_POINT('Ctrl Pts',(133.265690158908,4.13117184845439,339.235723045837));
#21078=CARTESIAN_POINT('Ctrl Pts',(133.273098240052,4.01864630428893,339.345471099536));
#21079=CARTESIAN_POINT('Ctrl Pts',(133.280506321196,3.90162985063131,339.45084378544));
#21080=CARTESIAN_POINT('Ctrl Pts',(133.28791440234,3.78049974618856,339.551456056205));
#21081=CARTESIAN_POINT('Ctrl Pts',(133.295316969514,3.65945980109538,339.651993439419));
#21082=CARTESIAN_POINT('Ctrl Pts',(133.302719536688,3.5343125876999,339.747777225207));
#21083=CARTESIAN_POINT('Ctrl Pts',(133.310122103862,3.40547122041814,339.838460119646));
#21084=CARTESIAN_POINT('Ctrl Pts',(133.317520773617,3.27669768755225,339.929095269938));
#21085=CARTESIAN_POINT('Ctrl Pts',(133.324919443371,3.14423417872232,340.014634663141));
#21086=CARTESIAN_POINT('Ctrl Pts',(133.332318113126,3.00852570436372,340.094772188104));
#21087=CARTESIAN_POINT('Ctrl Pts',(133.33971556233,2.87283961769004,340.174896492864));
#21088=CARTESIAN_POINT('Ctrl Pts',(133.347113011534,2.73390994897294,340.249620508427));
#21089=CARTESIAN_POINT('Ctrl Pts',(133.354510460738,2.59220952004958,340.318682202075));
#21090=CARTESIAN_POINT('Ctrl Pts',(133.361907589202,2.45051523500969,340.387740901328));
#21091=CARTESIAN_POINT('Ctrl Pts',(133.369304717665,2.30605076411907,340.451137603309));
#21092=CARTESIAN_POINT('Ctrl Pts',(133.376701846129,2.15931204333547,340.508657010743));
#21093=CARTESIAN_POINT('Ctrl Pts',(133.384100113565,2.0125507284519,340.566185274729));
#21094=CARTESIAN_POINT('Ctrl Pts',(133.391498381002,1.86351481391656,340.617834306068));
#21095=CARTESIAN_POINT('Ctrl Pts',(133.398896648439,1.71271850831408,340.663437637494));
#21096=CARTESIAN_POINT('Ctrl Pts',(133.406297514964,1.56186922638492,340.709056989849));
#21097=CARTESIAN_POINT('Ctrl Pts',(133.41369838149,1.40925867907596,340.748626305608));
#21098=CARTESIAN_POINT('Ctrl Pts',(133.421099248016,1.25541431508246,340.782029527768));
#21099=CARTESIAN_POINT('Ctrl Pts',(133.4285082414,1.10140101526794,340.81546942986));
#21100=CARTESIAN_POINT('Ctrl Pts',(133.435917234785,0.946151557994752,340.842729637148));
#21101=CARTESIAN_POINT('Ctrl Pts',(133.44332622817,0.790202347615889,340.863745459373));
#21102=CARTESIAN_POINT('Ctrl Pts',(133.45073978575,0.634157067144336,340.88477422807));
#21103=CARTESIAN_POINT('Ctrl Pts',(133.45815334333,0.477411545294794,340.899550911588));
#21104=CARTESIAN_POINT('Ctrl Pts',(133.465566900911,0.320504803726773,340.908062900248));
#21105=CARTESIAN_POINT('Ctrl Pts',(133.472991013047,0.163374676686341,340.916587007282));
#21106=CARTESIAN_POINT('Ctrl Pts',(133.480415125184,0.00608324368542446,
340.918828601248));
#21107=CARTESIAN_POINT('Ctrl Pts',(133.487839237321,-0.150832156118545,
340.914827150744));
#21108=CARTESIAN_POINT('Ctrl Pts',(133.491696362475,-0.232356023833892,
340.912748236107));
#21109=CARTESIAN_POINT('Ctrl Pts',(133.49555348763,-0.313778492059307,340.908985039158));
#21110=CARTESIAN_POINT('Ctrl Pts',(133.499410612785,-0.395025137311746,
340.903548568733));
#21111=CARTESIAN_POINT('Ctrl Pts',(133.506834590223,-0.551404107939601,
340.893084756396));
#21112=CARTESIAN_POINT('Ctrl Pts',(133.514258567661,-0.707602933274411,
340.876387389198));
#21113=CARTESIAN_POINT('Ctrl Pts',(133.521682545099,-0.86308449675833,340.853461857222));
#21114=CARTESIAN_POINT('Ctrl Pts',(133.529097761126,-1.01838256860399,340.830563380824));
#21115=CARTESIAN_POINT('Ctrl Pts',(133.536512977154,-1.17296469789577,340.801451424193));
#21116=CARTESIAN_POINT('Ctrl Pts',(133.543928193182,-1.32629574064238,340.766183327891));
#21117=CARTESIAN_POINT('Ctrl Pts',(133.551336274326,-1.47947924903135,340.730949166374));
#21118=CARTESIAN_POINT('Ctrl Pts',(133.55874435547,-1.63141370611187,340.689570740683));
#21119=CARTESIAN_POINT('Ctrl Pts',(133.566152436614,-1.78157116102391,340.642156924502));
#21120=CARTESIAN_POINT('Ctrl Pts',(133.573555003788,-1.9316168510008,340.59477839929));
#21121=CARTESIAN_POINT('Ctrl Pts',(133.580957570962,-2.07988781804193,340.541373540209));
#21122=CARTESIAN_POINT('Ctrl Pts',(133.588360138136,-2.22586845536354,340.482101803316));
#21123=CARTESIAN_POINT('Ctrl Pts',(133.595758807891,-2.37177223451766,340.422861272733));
#21124=CARTESIAN_POINT('Ctrl Pts',(133.603157477646,-2.51538774054721,340.357760156084));
#21125=CARTESIAN_POINT('Ctrl Pts',(133.6105561474,-2.65621673737412,340.287007017831));
#21126=CARTESIAN_POINT('Ctrl Pts',(133.617953596604,-2.79702250178873,340.216265551649));
#21127=CARTESIAN_POINT('Ctrl Pts',(133.625351045808,-2.93504233616722,340.139874081774));
#21128=CARTESIAN_POINT('Ctrl Pts',(133.632748495012,-3.06980002058145,340.058088413239));
#21129=CARTESIAN_POINT('Ctrl Pts',(133.640145623476,-3.20455186213775,339.976306290787));
#21130=CARTESIAN_POINT('Ctrl Pts',(133.647542751939,-3.33604151591193,339.889130628345));
#21131=CARTESIAN_POINT('Ctrl Pts',(133.654939880403,-3.46381955442744,339.79686195933));
#21132=CARTESIAN_POINT('Ctrl Pts',(133.662338147839,-3.59161726757216,339.704579083242));
#21133=CARTESIAN_POINT('Ctrl Pts',(133.669736415276,-3.71570192494373,339.607201857645));
#21134=CARTESIAN_POINT('Ctrl Pts',(133.677134682713,-3.83565527289649,339.505072606518));
#21135=CARTESIAN_POINT('Ctrl Pts',(133.684535549238,-3.9556507617203,339.402907476313));
#21136=CARTESIAN_POINT('Ctrl Pts',(133.691936415764,-4.07151176745755,339.295987238521));
#21137=CARTESIAN_POINT('Ctrl Pts',(133.69933728229,-4.18285526254338,339.184692630901));
#21138=CARTESIAN_POINT('Ctrl Pts',(133.706746275674,-4.29432102343238,339.07327581116));
#21139=CARTESIAN_POINT('Ctrl Pts',(133.714155269059,-4.40125910285416,338.95747529279));
#21140=CARTESIAN_POINT('Ctrl Pts',(133.721564262444,-4.50332482221643,338.837707142046));
#21141=CARTESIAN_POINT('Ctrl Pts',(133.728977820024,-4.60545341758201,338.71786520999));
#21142=CARTESIAN_POINT('Ctrl Pts',(133.736391377604,-4.70270344192746,338.594051067985));
#21143=CARTESIAN_POINT('Ctrl Pts',(133.743804935185,-4.79477259595615,338.466711167024));
#21144=CARTESIAN_POINT('Ctrl Pts',(133.751229047321,-4.88697282728141,338.339189974401));
#21145=CARTESIAN_POINT('Ctrl Pts',(133.758653159458,-4.97397725124649,338.208133307842));
#21146=CARTESIAN_POINT('Ctrl Pts',(133.766077271595,-5.05552827278849,338.074014386033));
#21147=CARTESIAN_POINT('Ctrl Pts',(133.769934396749,-5.09789731177662,338.004334206438));
#21148=CARTESIAN_POINT('Ctrl Pts',(133.773791521904,-5.13879512875485,337.933827834035));
#21149=CARTESIAN_POINT('Ctrl Pts',(133.777648647058,-5.17819070646937,337.862563810631));
#21150=CARTESIAN_POINT('Ctrl Pts',(133.785435791969,-5.25772638659632,337.71868896734));
#21151=CARTESIAN_POINT('Ctrl Pts',(133.79322293688,-5.331356706861,337.571325915128));
#21152=CARTESIAN_POINT('Ctrl Pts',(133.801010081791,-5.39877815383162,337.420976044535));
#21153=CARTESIAN_POINT('Ctrl Pts',(133.808784649618,-5.46609070785334,337.270869005288));
#21154=CARTESIAN_POINT('Ctrl Pts',(133.816559217445,-5.52721424522438,337.117785053094));
#21155=CARTESIAN_POINT('Ctrl Pts',(133.824333785272,-5.58189044811685,336.962251153069));
#21156=CARTESIAN_POINT('Ctrl Pts',(133.83216443819,-5.63696108062936,336.805595244312));
#21157=CARTESIAN_POINT('Ctrl Pts',(133.839995091109,-5.68549079118679,336.646454167424));
#21158=CARTESIAN_POINT('Ctrl Pts',(133.847825744027,-5.72726324714731,336.485390945299));
#21159=CARTESIAN_POINT('Ctrl Pts',(133.855573568673,-5.76859385739756,336.326031359987));
#21160=CARTESIAN_POINT('Ctrl Pts',(133.863321393318,-5.80330934948144,336.16479040582));
#21161=CARTESIAN_POINT('Ctrl Pts',(133.871069217963,-5.8312485558455,336.002232928241));
#21162=CARTESIAN_POINT('Ctrl Pts',(133.878941285018,-5.85963578917091,335.837068714744));
#21163=CARTESIAN_POINT('Ctrl Pts',(133.886813352073,-5.88102741061079,335.670545696006));
#21164=CARTESIAN_POINT('Ctrl Pts',(133.894685419128,-5.89530726613627,335.503272093743));
#21165=CARTESIAN_POINT('Ctrl Pts',(133.902557486184,-5.90958712166176,335.335998491481));
#21166=CARTESIAN_POINT('Ctrl Pts',(133.910429553239,-5.91675512236119,335.167974647051));
#21167=CARTESIAN_POINT('Ctrl Pts',(133.918301620294,-5.91674999725185,334.999819666414));
#21168=CARTESIAN_POINT('',(135.668301620294,-5.91694958252063,334.994690602227));
#21169=CARTESIAN_POINT('Ctrl Pts',(133.918301620327,-5.91674999725183,334.999819665701));
#21170=CARTESIAN_POINT('Ctrl Pts',(133.926068049142,-5.91674494089828,334.833921220247));
#21171=CARTESIAN_POINT('Ctrl Pts',(133.933834477957,-5.90975819896838,334.668163927719));
#21172=CARTESIAN_POINT('Ctrl Pts',(133.941600906772,-5.89585107127789,334.503139146429));
#21173=CARTESIAN_POINT('Ctrl Pts',(133.949377678458,-5.88192542289534,334.337894594872));
#21174=CARTESIAN_POINT('Ctrl Pts',(133.957154450145,-5.86106101844648,334.173384815219));
#21175=CARTESIAN_POINT('Ctrl Pts',(133.964931221831,-5.83337059116754,334.010192893235));
#21176=CARTESIAN_POINT('Ctrl Pts',(133.972726562797,-5.80561404502803,333.846611303594));
#21177=CARTESIAN_POINT('Ctrl Pts',(133.980521903763,-5.77099893364784,333.684354176176));
#21178=CARTESIAN_POINT('Ctrl Pts',(133.988317244729,-5.72968894103705,333.523993495455));
#21179=CARTESIAN_POINT('Ctrl Pts',(133.996122144138,-5.68832829519387,333.363436184663));
#21180=CARTESIAN_POINT('Ctrl Pts',(134.003927043548,-5.64025647230966,333.20478026353));
#21181=CARTESIAN_POINT('Ctrl Pts',(134.011731942957,-5.58568624137394,333.048580061743));
#21182=CARTESIAN_POINT('Ctrl Pts',(134.019555047678,-5.53098872268916,332.892015515299));
#21183=CARTESIAN_POINT('Ctrl Pts',(134.027378152399,-5.46976259593421,332.737918438187));
#21184=CARTESIAN_POINT('Ctrl Pts',(134.03520125712,-5.40226868233612,332.586822914424));
#21185=CARTESIAN_POINT('Ctrl Pts',(134.042096398524,-5.34278078146086,332.453650083554));
#21186=CARTESIAN_POINT('Ctrl Pts',(134.048991539929,-5.27842461240621,332.322808720411));
#21187=CARTESIAN_POINT('Ctrl Pts',(134.055886681333,-5.20940709427122,332.194646494886));
#21188=CARTESIAN_POINT('Ctrl Pts',(134.063310658771,-5.1350961458186,332.056654622794));
#21189=CARTESIAN_POINT('Ctrl Pts',(134.070734636209,-5.05518641366889,331.92140925387));
#21190=CARTESIAN_POINT('Ctrl Pts',(134.078158613647,-4.96990532954527,331.789397007125));
#21191=CARTESIAN_POINT('Ctrl Pts',(134.085573829675,-4.88472488993215,331.657540554694));
#21192=CARTESIAN_POINT('Ctrl Pts',(134.092989045702,-4.79418591677853,331.528909939925));
#21193=CARTESIAN_POINT('Ctrl Pts',(134.10040426173,-4.69856230686571,331.40396846357));
#21194=CARTESIAN_POINT('Ctrl Pts',(134.107812342874,-4.60303070550889,331.279147205274));
#21195=CARTESIAN_POINT('Ctrl Pts',(134.115220424018,-4.50242443258408,331.158008313049));
#21196=CARTESIAN_POINT('Ctrl Pts',(134.122628505162,-4.3970613072146,331.04098719084));
#21197=CARTESIAN_POINT('Ctrl Pts',(134.130031072336,-4.2917766055436,330.924053169589));
#21198=CARTESIAN_POINT('Ctrl Pts',(134.13743363951,-4.18174234995567,330.811231091794));
#21199=CARTESIAN_POINT('Ctrl Pts',(134.144836206684,-4.06731728257649,330.702924170397));
#21200=CARTESIAN_POINT('Ctrl Pts',(134.152234876439,-3.95295245949564,330.594674272122));
#21201=CARTESIAN_POINT('Ctrl Pts',(134.159633546194,-3.83420169896169,330.490935051799));
#21202=CARTESIAN_POINT('Ctrl Pts',(134.167032215949,-3.71146124206279,330.392073567084));
#21203=CARTESIAN_POINT('Ctrl Pts',(134.174429665153,-3.58874103352752,330.293228391444));
#21204=CARTESIAN_POINT('Ctrl Pts',(134.181827114357,-3.46203272526591,330.199259588275));
#21205=CARTESIAN_POINT('Ctrl Pts',(134.18922456356,-3.33176643274027,330.110494605774));
#21206=CARTESIAN_POINT('Ctrl Pts',(134.196621692024,-3.20150578833396,330.021733471968));
#21207=CARTESIAN_POINT('Ctrl Pts',(134.204018820487,-3.06768777481492,329.938175920366));
#21208=CARTESIAN_POINT('Ctrl Pts',(134.211415948951,-2.93077211676588,329.86010648339));
#21209=CARTESIAN_POINT('Ctrl Pts',(134.218814216388,-2.79383537712312,329.782025025669));
#21210=CARTESIAN_POINT('Ctrl Pts',(134.226212483824,-2.65380036748951,329.709433550022));
#21211=CARTESIAN_POINT('Ctrl Pts',(134.233610751261,-2.51115193253958,329.64257090255));
#21212=CARTESIAN_POINT('Ctrl Pts',(134.241011617787,-2.36845338369463,329.575684765527));
#21213=CARTESIAN_POINT('Ctrl Pts',(134.248412484312,-2.22313991926851,329.514531622055));
#21214=CARTESIAN_POINT('Ctrl Pts',(134.255813350838,-2.0757167518377,329.459302342787));
#21215=CARTESIAN_POINT('Ctrl Pts',(134.263222344223,-1.92813169967469,329.404012416491));
#21216=CARTESIAN_POINT('Ctrl Pts',(134.270631337608,-1.77843266772151,329.35465947618));
#21217=CARTESIAN_POINT('Ctrl Pts',(134.278040330992,-1.62714113460999,329.31138485301));
#21218=CARTESIAN_POINT('Ctrl Pts',(134.285453888573,-1.47575640069542,329.26808357118));
#21219=CARTESIAN_POINT('Ctrl Pts',(134.292867446153,-1.32277757256699,329.230868155821));
#21220=CARTESIAN_POINT('Ctrl Pts',(134.300281003733,-1.16873622563934,329.199828778615));
#21221=CARTESIAN_POINT('Ctrl Pts',(134.30770511587,-1.01447557265346,329.168745211173));
#21222=CARTESIAN_POINT('Ctrl Pts',(134.315129228006,-0.85914974723988,329.143855301598));
#21223=CARTESIAN_POINT('Ctrl Pts',(134.322553340143,-0.703296166356293,
329.125197444604));
#21224=CARTESIAN_POINT('Ctrl Pts',(134.326410465298,-0.622323956322832,
329.115503936718));
#21225=CARTESIAN_POINT('Ctrl Pts',(134.330267590452,-0.541209317292771,
329.107491738661));
#21226=CARTESIAN_POINT('Ctrl Pts',(134.334124715607,-0.460027482380483,
329.101160683833));
#21227=CARTESIAN_POINT('Ctrl Pts',(134.341548693045,-0.30377325504216,329.088975025781));
#21228=CARTESIAN_POINT('Ctrl Pts',(134.348972670483,-0.146798797695722,
329.082983794843));
#21229=CARTESIAN_POINT('Ctrl Pts',(134.356396647921,0.0103636049962139,
329.0832590763));
#21230=CARTESIAN_POINT('Ctrl Pts',(134.363811863948,0.167340532406615,329.083534032883));
#21231=CARTESIAN_POINT('Ctrl Pts',(134.371227079976,0.324504594077193,329.090060780498));
#21232=CARTESIAN_POINT('Ctrl Pts',(134.378642296003,0.481317969259022,329.102859712117));
#21233=CARTESIAN_POINT('Ctrl Pts',(134.386050377148,0.637980459400758,329.115646328669));
#21234=CARTESIAN_POINT('Ctrl Pts',(134.393458458292,0.794292565323229,329.134693084381));
#21235=CARTESIAN_POINT('Ctrl Pts',(134.400866539436,0.949716156397051,329.15996834043));
#21236=CARTESIAN_POINT('Ctrl Pts',(134.40826910661,1.10502406285349,329.185224783644));
#21237=CARTESIAN_POINT('Ctrl Pts',(134.415671673784,1.25944440448697,329.216700436622));
#21238=CARTESIAN_POINT('Ctrl Pts',(134.423074240958,1.41244397498346,329.254311827115));
#21239=CARTESIAN_POINT('Ctrl Pts',(134.430472910712,1.56536299187487,329.291903415375));
#21240=CARTESIAN_POINT('Ctrl Pts',(134.437871580467,1.71686236586658,329.335624218672));
#21241=CARTESIAN_POINT('Ctrl Pts',(134.445270250222,1.86641900155446,329.385339665382));
#21242=CARTESIAN_POINT('Ctrl Pts',(134.452667699426,2.01595096504142,329.435046910586));
#21243=CARTESIAN_POINT('Ctrl Pts',(134.46006514863,2.16354047248464,329.490746718882));
#21244=CARTESIAN_POINT('Ctrl Pts',(134.467462597834,2.30867940555075,329.552254598012));
#21245=CARTESIAN_POINT('Ctrl Pts',(134.474859726297,2.4538120456457,329.613759810267));
#21246=CARTESIAN_POINT('Ctrl Pts',(134.482256854761,2.59649397900092,329.681072447013));
#21247=CARTESIAN_POINT('Ctrl Pts',(134.489653983224,2.73623715288133,329.753959892863));
#21248=CARTESIAN_POINT('Ctrl Pts',(134.497052250661,2.87600184372211,329.82685856156));
#21249=CARTESIAN_POINT('Ctrl Pts',(134.504450518098,3.01282654318477,329.905333575905));
#21250=CARTESIAN_POINT('Ctrl Pts',(134.511848785534,3.14624802321231,329.989106473));
#21251=CARTESIAN_POINT('Ctrl Pts',(134.51924965206,3.27971637560892,330.072908800394));
#21252=CARTESIAN_POINT('Ctrl Pts',(134.526650518586,3.40977881228578,330.162012517857));
#21253=CARTESIAN_POINT('Ctrl Pts',(134.534051385111,3.53600142652282,330.256096072418));
#21254=CARTESIAN_POINT('Ctrl Pts',(134.541460378496,3.66236264525769,330.350282939716));
#21255=CARTESIAN_POINT('Ctrl Pts',(134.548869371881,3.78487532158267,330.449460341501));
#21256=CARTESIAN_POINT('Ctrl Pts',(134.556278365266,3.90313840510259,330.553266237662));
#21257=CARTESIAN_POINT('Ctrl Pts',(134.563691922846,4.02147434276138,330.657136081837));
#21258=CARTESIAN_POINT('Ctrl Pts',(134.571105480426,4.13555520131591,330.765639845399));
#21259=CARTESIAN_POINT('Ctrl Pts',(134.578519038006,4.24501748751773,330.878379312313));
#21260=CARTESIAN_POINT('Ctrl Pts',(134.585943150143,4.35463561332356,330.991279284498));
#21261=CARTESIAN_POINT('Ctrl Pts',(134.59336726228,4.45962178601344,331.108426726565));
#21262=CARTESIAN_POINT('Ctrl Pts',(134.600791374417,4.55965289150053,331.229390490712));
#21263=CARTESIAN_POINT('Ctrl Pts',(134.604648499571,4.61162307811934,331.292236036268));
#21264=CARTESIAN_POINT('Ctrl Pts',(134.608505624726,4.66225649193679,331.356111206627));
#21265=CARTESIAN_POINT('Ctrl Pts',(134.612362749881,4.71151256009419,331.420952646503));
#21266=CARTESIAN_POINT('Ctrl Pts',(134.619786727318,4.8063178681985,331.545755801024));
#21267=CARTESIAN_POINT('Ctrl Pts',(134.627210704756,4.89630390817413,331.674516772272));
#21268=CARTESIAN_POINT('Ctrl Pts',(134.634634682194,4.98112201219741,331.806826960201));
#21269=CARTESIAN_POINT('Ctrl Pts',(134.642049898222,5.0658400180964,331.9389810022));
#21270=CARTESIAN_POINT('Ctrl Pts',(134.64946511425,5.14540202862682,332.074675612246));
#21271=CARTESIAN_POINT('Ctrl Pts',(134.656880330277,5.21949984923519,332.213469561204));
#21272=CARTESIAN_POINT('Ctrl Pts',(134.664288411421,5.29352637329363,332.352129963324));
#21273=CARTESIAN_POINT('Ctrl Pts',(134.671696492565,5.36209899977196,332.493883440385));
#21274=CARTESIAN_POINT('Ctrl Pts',(134.679104573709,5.42495312107051,332.638260345278));
#21275=CARTESIAN_POINT('Ctrl Pts',(134.686507140883,5.48776045889865,332.782529787803));
#21276=CARTESIAN_POINT('Ctrl Pts',(134.693909708057,5.54485761830156,332.929418429395));
#21277=CARTESIAN_POINT('Ctrl Pts',(134.701312275231,5.59602624434115,333.078432713865));
#21278=CARTESIAN_POINT('Ctrl Pts',(134.708710944986,5.64716793032276,333.227368542965));
#21279=CARTESIAN_POINT('Ctrl Pts',(134.716109614741,5.69238717838704,333.378427434015));
#21280=CARTESIAN_POINT('Ctrl Pts',(134.723508284495,5.73151407574537,333.531096680502));
#21281=CARTESIAN_POINT('Ctrl Pts',(134.730905733699,5.7706345183806,333.683740741303));
#21282=CARTESIAN_POINT('Ctrl Pts',(134.738303182903,5.80366451244279,333.83799426912));
#21283=CARTESIAN_POINT('Ctrl Pts',(134.745700632107,5.83048422942221,333.993330137056));
#21284=CARTESIAN_POINT('Ctrl Pts',(134.753097760571,5.85730278354544,334.148659269901));
#21285=CARTESIAN_POINT('Ctrl Pts',(134.760494889034,5.8779115324792,334.305070281786));
#21286=CARTESIAN_POINT('Ctrl Pts',(134.767892017498,5.89224197412736,334.462026877222));
#21287=CARTESIAN_POINT('Ctrl Pts',(134.775290284934,5.90657462230582,334.619007640055));
#21288=CARTESIAN_POINT('Ctrl Pts',(134.782688552371,5.91462700443071,334.776533782018));
#21289=CARTESIAN_POINT('Ctrl Pts',(134.790086819807,5.91638260661324,334.934065072501));
#21290=CARTESIAN_POINT('Ctrl Pts',(134.797487686333,5.91813882555728,335.091651705383));
#21291=CARTESIAN_POINT('Ctrl Pts',(134.804888552859,5.91359385606546,335.249243117434));
#21292=CARTESIAN_POINT('Ctrl Pts',(134.812289419384,5.90278328706665,335.406300416474));
#21293=CARTESIAN_POINT('Ctrl Pts',(134.819698412769,5.89196084702955,335.563530179442));
#21294=CARTESIAN_POINT('Ctrl Pts',(134.827107406154,5.87485909294768,335.720224285561));
#21295=CARTESIAN_POINT('Ctrl Pts',(134.834516399539,5.8515654406907,335.875849562319));
#21296=CARTESIAN_POINT('Ctrl Pts',(134.841929957119,5.82825743874044,336.031570709616));
#21297=CARTESIAN_POINT('Ctrl Pts',(134.849343514699,5.79875000765694,336.186221349791));
#21298=CARTESIAN_POINT('Ctrl Pts',(134.856757072279,5.76318130874689,336.339280316069));
#21299=CARTESIAN_POINT('Ctrl Pts',(134.864181184416,5.72756197128225,336.492557189807));
#21300=CARTESIAN_POINT('Ctrl Pts',(134.871605296553,5.685864230165,336.644237505025));
#21301=CARTESIAN_POINT('Ctrl Pts',(134.879029408689,5.63827579120752,336.793816229379));
#21302=CARTESIAN_POINT('Ctrl Pts',(134.882886533844,5.61355168122619,336.871528398822));
#21303=CARTESIAN_POINT('Ctrl Pts',(134.886743658999,5.58723833331448,336.948673636558));
#21304=CARTESIAN_POINT('Ctrl Pts',(134.890600784154,5.55936706798296,337.025183538825));
#21305=CARTESIAN_POINT('Ctrl Pts',(134.898024761592,5.50572202493012,337.172445493107));
#21306=CARTESIAN_POINT('Ctrl Pts',(134.90544873903,5.44614078684118,337.317796623737));
#21307=CARTESIAN_POINT('Ctrl Pts',(134.912872716468,5.38077827004688,337.46072261157));
#21308=CARTESIAN_POINT('Ctrl Pts',(134.920287932495,5.31549289085666,337.603479925233));
#21309=CARTESIAN_POINT('Ctrl Pts',(134.927703148523,5.24443996751648,337.743817456921));
#21310=CARTESIAN_POINT('Ctrl Pts',(134.935118364551,5.16782375726106,337.881237264855));
#21311=CARTESIAN_POINT('Ctrl Pts',(134.942526445695,5.09128126673744,338.018524848142));
#21312=CARTESIAN_POINT('Ctrl Pts',(134.949934526839,5.0091863265827,338.152899972931));
#21313=CARTESIAN_POINT('Ctrl Pts',(134.957342607983,4.92179067871552,338.283885972047));
#21314=CARTESIAN_POINT('Ctrl Pts',(134.964745175157,4.8344600810252,338.414774475892));
#21315=CARTESIAN_POINT('Ctrl Pts',(134.972147742331,4.74183683776611,338.542278567782));
#21316=CARTESIAN_POINT('Ctrl Pts',(134.979550309505,4.64421782647985,338.665947536819));
#21317=CARTESIAN_POINT('Ctrl Pts',(134.98694897926,4.54665021117636,338.789551394683));
#21318=CARTESIAN_POINT('Ctrl Pts',(134.994347649015,4.44409229679957,338.909323858795));
#21319=CARTESIAN_POINT('Ctrl Pts',(135.00174631877,4.3368832796346,339.024844590953));
#21320=CARTESIAN_POINT('Ctrl Pts',(135.009143767974,4.22969194862836,339.140346265778));
#21321=CARTESIAN_POINT('Ctrl Pts',(135.016541217178,4.11785129128037,339.251597327416));
#21322=CARTESIAN_POINT('Ctrl Pts',(135.023938666382,4.00173973375924,339.358211750908));
#21323=CARTESIAN_POINT('Ctrl Pts',(135.031335794845,3.88563321063289,339.464821551785));
#21324=CARTESIAN_POINT('Ctrl Pts',(135.038732923309,3.7652564304331,339.566794861825));
#21325=CARTESIAN_POINT('Ctrl Pts',(135.046130051772,3.64102330506524,339.663783855891));
#21326=CARTESIAN_POINT('Ctrl Pts',(135.053528319209,3.51677105089727,339.760787783842));
#21327=CARTESIAN_POINT('Ctrl Pts',(135.060926586646,3.38866156346105,339.852805638024));
#21328=CARTESIAN_POINT('Ctrl Pts',(135.068324854082,3.257140197588,339.939531181778));
#21329=CARTESIAN_POINT('Ctrl Pts',(135.075725720608,3.12557262687596,340.026287193127));
#21330=CARTESIAN_POINT('Ctrl Pts',(135.083126587134,2.99059110263412,340.107746986973));
#21331=CARTESIAN_POINT('Ctrl Pts',(135.09052745366,2.85266805000558,340.183648865324));
#21332=CARTESIAN_POINT('Ctrl Pts',(135.097936447044,2.71459354467929,340.259634091195));
#21333=CARTESIAN_POINT('Ctrl Pts',(135.105345440429,2.5735713874897,340.330049033264));
#21334=CARTESIAN_POINT('Ctrl Pts',(135.112754433814,2.43009724031796,340.394678671163));
#21335=CARTESIAN_POINT('Ctrl Pts',(135.120167991394,2.28653470812265,340.459348123148));
#21336=CARTESIAN_POINT('Ctrl Pts',(135.127581548974,2.14051752137725,340.518225030087));
#21337=CARTESIAN_POINT('Ctrl Pts',(135.134995106555,1.9925587073517,340.571143541523));
#21338=CARTESIAN_POINT('Ctrl Pts',(135.142419218691,1.8443892468669,340.624137392149));
#21339=CARTESIAN_POINT('Ctrl Pts',(135.149843330828,1.69427299350774,340.67115579404));
#21340=CARTESIAN_POINT('Ctrl Pts',(135.157267442965,1.54273621813229,340.712083291039));
#21341=CARTESIAN_POINT('Ctrl Pts',(135.161124568119,1.46400676235506,340.733346773497));
#21342=CARTESIAN_POINT('Ctrl Pts',(135.164981693274,1.38489402371016,340.752967032599));
#21343=CARTESIAN_POINT('Ctrl Pts',(135.168838818429,1.30547247370716,340.770933389227));
#21344=CARTESIAN_POINT('Ctrl Pts',(135.176262795867,1.15260634370706,340.805514021408));
#21345=CARTESIAN_POINT('Ctrl Pts',(135.183686773305,0.998134650330004,340.834068724219));
#21346=CARTESIAN_POINT('Ctrl Pts',(135.191110750743,0.842573729630976,340.856449442507));
#21347=CARTESIAN_POINT('Ctrl Pts',(135.19852596677,0.687196394223663,340.878803748179));
#21348=CARTESIAN_POINT('Ctrl Pts',(135.205941182798,0.530732756022619,340.894998520057));
#21349=CARTESIAN_POINT('Ctrl Pts',(135.213356398825,0.373712080201323,340.904936057538));
#21350=CARTESIAN_POINT('Ctrl Pts',(135.22076447997,0.216842488883807,340.914864033171));
#21351=CARTESIAN_POINT('Ctrl Pts',(135.228172561114,0.0594172969566546,
340.918546737042));
#21352=CARTESIAN_POINT('Ctrl Pts',(135.235580642258,-0.0980264239861944,
340.915937912343));
#21353=CARTESIAN_POINT('Ctrl Pts',(135.242983209432,-0.255352956691995,
340.91333102944));
#21354=CARTESIAN_POINT('Ctrl Pts',(135.250385776606,-0.412697619390957,
340.904441948458));
#21355=CARTESIAN_POINT('Ctrl Pts',(135.25778834378,-0.569520742199788,340.889276414527));
#21356=CARTESIAN_POINT('Ctrl Pts',(135.265187013534,-0.726261298319962,
340.874118865183));
#21357=CARTESIAN_POINT('Ctrl Pts',(135.272585683289,-0.882480490866497,
340.85269147988));
#21358=CARTESIAN_POINT('Ctrl Pts',(135.279984353044,-1.03764128990488,340.825052026891));
#21359=CARTESIAN_POINT('Ctrl Pts',(135.287381802248,-1.19277649222948,340.797417133553));
#21360=CARTESIAN_POINT('Ctrl Pts',(135.294779251452,-1.34685328050463,340.76357227181));
#21361=CARTESIAN_POINT('Ctrl Pts',(135.302176700656,-1.49934224999276,340.723626768045));
#21362=CARTESIAN_POINT('Ctrl Pts',(135.309573829119,-1.65182460782507,340.683682996248));
#21363=CARTESIAN_POINT('Ctrl Pts',(135.316970957582,-1.80271892272736,340.637639202942));
#21364=CARTESIAN_POINT('Ctrl Pts',(135.324368086046,-1.95150870963899,340.585655227339));
#21365=CARTESIAN_POINT('Ctrl Pts',(135.331766353482,-2.1003214064634,340.533663247502));
#21366=CARTESIAN_POINT('Ctrl Pts',(135.339164620919,-2.24702857773313,340.475729387303));
#21367=CARTESIAN_POINT('Ctrl Pts',(135.346562888356,-2.3911316954519,340.412062432891));
#21368=CARTESIAN_POINT('Ctrl Pts',(135.353963754881,-2.5352854381114,340.348373111608));
#21369=CARTESIAN_POINT('Ctrl Pts',(135.361364621407,-2.6768329646302,340.27894683678));
#21370=CARTESIAN_POINT('Ctrl Pts',(135.368765487933,-2.8152985512318,340.204039260991));
#21371=CARTESIAN_POINT('Ctrl Pts',(135.376174481318,-2.95391618628547,340.129049429521));
#21372=CARTESIAN_POINT('Ctrl Pts',(135.383583474702,-3.08944479441327,340.048566454527));
#21373=CARTESIAN_POINT('Ctrl Pts',(135.390992468087,-3.22143532931494,339.962890788799));
#21374=CARTESIAN_POINT('Ctrl Pts',(135.398406025667,-3.3535071749389,339.877162343905));
#21375=CARTESIAN_POINT('Ctrl Pts',(135.405819583247,-3.48203630027982,339.786235049131));
#21376=CARTESIAN_POINT('Ctrl Pts',(135.413233140828,-3.60660560965785,339.690450568856));
#21377=CARTESIAN_POINT('Ctrl Pts',(135.420657252964,-3.73135226625324,339.594529721838));
#21378=CARTESIAN_POINT('Ctrl Pts',(135.428081365101,-3.85212756185855,339.493738116977));
#21379=CARTESIAN_POINT('Ctrl Pts',(135.435505477238,-3.96854961156869,339.388455826714));
#21380=CARTESIAN_POINT('Ctrl Pts',(135.439362602392,-4.02903555362147,339.333757438188));
#21381=CARTESIAN_POINT('Ctrl Pts',(135.443219727547,-4.08834709044893,339.277847496475));
#21382=CARTESIAN_POINT('Ctrl Pts',(135.447076852702,-4.14643494094762,339.220782847173));
#21383=CARTESIAN_POINT('Ctrl Pts',(135.45439526703,-4.25664939870424,339.112509786182));
#21384=CARTESIAN_POINT('Ctrl Pts',(135.461713681359,-4.36280933909392,338.999730679644));
#21385=CARTESIAN_POINT('Ctrl Pts',(135.469032095688,-4.4645159647071,338.882786082618));
#21386=CARTESIAN_POINT('Ctrl Pts',(135.476341726381,-4.56610052098445,338.765981843699));
#21387=CARTESIAN_POINT('Ctrl Pts',(135.483651357074,-4.66324214693022,338.645022348695));
#21388=CARTESIAN_POINT('Ctrl Pts',(135.490960987767,-4.75557691634672,338.520286743322));
#21389=CARTESIAN_POINT('Ctrl Pts',(135.498350180789,-4.84891671182039,338.394193442095));
#21390=CARTESIAN_POINT('Ctrl Pts',(135.505739373811,-4.93734408256862,338.26424159311));
#21391=CARTESIAN_POINT('Ctrl Pts',(135.513128566833,-5.02052234680356,338.130860253628));
#21392=CARTESIAN_POINT('Ctrl Pts',(135.520425267282,-5.10265944569908,337.999148485264));
#21393=CARTESIAN_POINT('Ctrl Pts',(135.527721967731,-5.17967786748907,337.864092916784));
#21394=CARTESIAN_POINT('Ctrl Pts',(135.53501866818,-5.25129509341039,337.72613836854));
#21395=CARTESIAN_POINT('Ctrl Pts',(135.542312273334,-5.32288193896001,337.588242341278));
#21396=CARTESIAN_POINT('Ctrl Pts',(135.549605878488,-5.38907197012852,337.447450121665));
#21397=CARTESIAN_POINT('Ctrl Pts',(135.556899483641,-5.44962772291846,337.304232680113));
#21398=CARTESIAN_POINT('Ctrl Pts',(135.564191530132,-5.51017053478007,337.161045844516));
#21399=CARTESIAN_POINT('Ctrl Pts',(135.571483576623,-5.56508131525385,337.015435172785));
#21400=CARTESIAN_POINT('Ctrl Pts',(135.578775623113,-5.61417014868265,336.867892958427));
#21401=CARTESIAN_POINT('Ctrl Pts',(135.586236122878,-5.66439298129037,336.716942377273));
#21402=CARTESIAN_POINT('Ctrl Pts',(135.593696622643,-5.70852144370212,336.563970311823));
#21403=CARTESIAN_POINT('Ctrl Pts',(135.601157122408,-5.74640579729457,336.409521541275));
#21404=CARTESIAN_POINT('Ctrl Pts',(135.608453037332,-5.78345439047947,336.258480039301));
#21405=CARTESIAN_POINT('Ctrl Pts',(135.615748952256,-5.8145314537954,336.106026699703));
#21406=CARTESIAN_POINT('Ctrl Pts',(135.62304486718,-5.83954861303036,335.952681771923));
#21407=CARTESIAN_POINT('Ctrl Pts',(135.630587659365,-5.86541229635978,335.794147998564));
#21408=CARTESIAN_POINT('Ctrl Pts',(135.638130451551,-5.88479868119094,335.634661679324));
#21409=CARTESIAN_POINT('Ctrl Pts',(135.645673243737,-5.89766840383677,335.474803075901));
#21410=CARTESIAN_POINT('Ctrl Pts',(135.653216035923,-5.9105381264826,335.314944472479));
#21411=CARTESIAN_POINT('Ctrl Pts',(135.660758828108,-5.91689121004861,335.154714037125));
#21412=CARTESIAN_POINT('Ctrl Pts',(135.668301620294,-5.91674761796713,334.994690783454));
#21413=CARTESIAN_POINT('',(137.418301620294,-5.92471687767985,335.002930573287));
#21414=CARTESIAN_POINT('Ctrl Pts',(135.668301620294,-5.91841553383544,334.9946892868));
#21415=CARTESIAN_POINT('Ctrl Pts',(135.687306042521,-5.92215085104165,334.591385784948));
#21416=CARTESIAN_POINT('Ctrl Pts',(135.799056476177,-5.70049280571943,332.223948443518));
#21417=CARTESIAN_POINT('Ctrl Pts',(136.003552921246,-2.51124033804167,328.469586928391));
#21418=CARTESIAN_POINT('Ctrl Pts',(136.281790955525,4.13258743031318,329.354263196709));
#21419=CARTESIAN_POINT('Ctrl Pts',(136.560028989797,6.98400071075933,335.419948798467));
#21420=CARTESIAN_POINT('Ctrl Pts',(136.838267024072,3.42629962262258,341.100253586306));
#21421=CARTESIAN_POINT('Ctrl Pts',(137.116505058345,-3.27566605709539,341.182445697587));
#21422=CARTESIAN_POINT('Ctrl Pts',(137.309849923753,-5.84393503100964,337.297073785147));
#21423=CARTESIAN_POINT('Ctrl Pts',(137.410448777736,-5.92572569476417,335.169119395345));
#21424=CARTESIAN_POINT('Ctrl Pts',(137.418301620294,-5.92471687767985,335.002930573287));
#21425=CARTESIAN_POINT('',(139.168300422869,-5.91261848715546,335.003766165052));
#21426=CARTESIAN_POINT('Ctrl Pts',(137.418301620294,-5.92471687767985,335.002930573287));
#21427=CARTESIAN_POINT('Ctrl Pts',(137.503194789161,-5.91381105874106,333.206346007866));
#21428=CARTESIAN_POINT('Ctrl Pts',(137.680833969451,-4.08295784035911,329.427749411782));
#21429=CARTESIAN_POINT('Ctrl Pts',(137.951219161168,2.35033272298692,328.409965173652));
#21430=CARTESIAN_POINT('Ctrl Pts',(138.229457195441,6.81360077617479,333.410198948256));
#21431=CARTESIAN_POINT('Ctrl Pts',(138.507695229716,5.02412796564901,339.869369682618));
#21432=CARTESIAN_POINT('Ctrl Pts',(138.78593326399,-1.37591292294527,341.859991731022));
#21433=CARTESIAN_POINT('Ctrl Pts',(139.006134687901,-5.44171109823543,338.453199721582));
#21434=CARTESIAN_POINT('Ctrl Pts',(139.133590100387,-5.91369737005363,335.74321261132));
#21435=CARTESIAN_POINT('Ctrl Pts',(139.16829950145,-5.9094401988413,335.003783783589));
#21436=CARTESIAN_POINT('',(140.918302830788,-5.91342774936137,334.995424942681));
#21437=CARTESIAN_POINT('Ctrl Pts',(139.168301620294,-5.9167488158986,335.00374326897));
#21438=CARTESIAN_POINT('Ctrl Pts',(139.175753102405,-5.91684936887011,334.844805538364));
#21439=CARTESIAN_POINT('Ctrl Pts',(139.183204584516,-5.91054143042238,334.685840579607));
#21440=CARTESIAN_POINT('Ctrl Pts',(139.190656066627,-5.89784510831784,334.527396952198));
#21441=CARTESIAN_POINT('Ctrl Pts',(139.19810809896,-5.88514784870938,334.368941625219));
#21442=CARTESIAN_POINT('Ctrl Pts',(139.205560131292,-5.86606129405076,334.211008070705));
#21443=CARTESIAN_POINT('Ctrl Pts',(139.213012163625,-5.84065751797578,334.054140433144));
#21444=CARTESIAN_POINT('Ctrl Pts',(139.220466135568,-5.8152471298227,333.897231966177));
#21445=CARTESIAN_POINT('Ctrl Pts',(139.227920107511,-5.78351630303407,333.741390329624));
#21446=CARTESIAN_POINT('Ctrl Pts',(139.235374079454,-5.74558837734309,333.58715012806));
#21447=CARTESIAN_POINT('Ctrl Pts',(139.242831381279,-5.70764350826209,333.432841023391));
#21448=CARTESIAN_POINT('Ctrl Pts',(139.250288683105,-5.66349611268614,333.280135133418));
#21449=CARTESIAN_POINT('Ctrl Pts',(139.257745984931,-5.61331957911448,333.129552495997));
#21450=CARTESIAN_POINT('Ctrl Pts',(139.265212769917,-5.56307923800034,332.978778368504));
#21451=CARTESIAN_POINT('Ctrl Pts',(139.272679554903,-5.50679455822665,332.83013323447));
#21452=CARTESIAN_POINT('Ctrl Pts',(139.280146339889,-5.44468769455522,332.684118640504));
#21453=CARTESIAN_POINT('Ctrl Pts',(139.28761818195,-5.38253876738727,332.538005154339));
#21454=CARTESIAN_POINT('Ctrl Pts',(139.295090024011,-5.31455995236136,332.394526089145));
#21455=CARTESIAN_POINT('Ctrl Pts',(139.302561866072,-5.24101952035768,332.254158608053));
#21456=CARTESIAN_POINT('Ctrl Pts',(139.310045923778,-5.16735885779002,332.113561641479));
#21457=CARTESIAN_POINT('Ctrl Pts',(139.317529981484,-5.08811859171075,331.976086740265));
#21458=CARTESIAN_POINT('Ctrl Pts',(139.32501403919,-5.00361112229794,331.842183301818));
#21459=CARTESIAN_POINT('Ctrl Pts',(139.330812470306,-4.93813718297193,331.738438796565));
#21460=CARTESIAN_POINT('Ctrl Pts',(139.336610901421,-4.86950239493759,331.636837564401));
#21461=CARTESIAN_POINT('Ctrl Pts',(139.342409332537,-4.79786834624722,331.537574564763));
#21462=CARTESIAN_POINT('Ctrl Pts',(139.349833309975,-4.70615223361802,331.410483933685));
#21463=CARTESIAN_POINT('Ctrl Pts',(139.357257287413,-4.60924452397342,331.286848295946));
#21464=CARTESIAN_POINT('Ctrl Pts',(139.364681264851,-4.50743432440201,331.167120354916));
#21465=CARTESIAN_POINT('Ctrl Pts',(139.372096480879,-4.40574427618426,331.04753371087));
#21466=CARTESIAN_POINT('Ctrl Pts',(139.379511696906,-4.29916349393508,330.931845865481));
#21467=CARTESIAN_POINT('Ctrl Pts',(139.386926912934,-4.18802410190193,330.820480328508));
#21468=CARTESIAN_POINT('Ctrl Pts',(139.394334994078,-4.07699164763216,330.709221946894));
#21469=CARTESIAN_POINT('Ctrl Pts',(139.401743075222,-3.96140957769699,330.602277856496));
#21470=CARTESIAN_POINT('Ctrl Pts',(139.409151156366,-3.84164991394839,330.5000381667));
#21471=CARTESIAN_POINT('Ctrl Pts',(139.41655372354,-3.72197938950464,330.397874575771));
#21472=CARTESIAN_POINT('Ctrl Pts',(139.423956290715,-3.59813774526255,330.300408654587));
#21473=CARTESIAN_POINT('Ctrl Pts',(139.431358857889,-3.470533365601,330.207993247005));
#21474=CARTESIAN_POINT('Ctrl Pts',(139.438757527643,-3.34299616908793,330.115626495732));
#21475=CARTESIAN_POINT('Ctrl Pts',(139.446156197398,-3.21170048406593,330.028305180718));
#21476=CARTESIAN_POINT('Ctrl Pts',(139.453554867153,-3.07708714444699,329.946341397762));
#21477=CARTESIAN_POINT('Ctrl Pts',(139.460952316357,-2.94249601184888,329.864391136283));
#21478=CARTESIAN_POINT('Ctrl Pts',(139.468349765561,-2.80458862934737,329.787796846657));
#21479=CARTESIAN_POINT('Ctrl Pts',(139.475747214765,-2.66383423526644,329.71682692603));
#21480=CARTESIAN_POINT('Ctrl Pts',(139.483144343228,-2.5230859440508,329.645860082535));
#21481=CARTESIAN_POINT('Ctrl Pts',(139.490541471692,-2.37949121994516,329.580517291188));
#21482=CARTESIAN_POINT('Ctrl Pts',(139.497938600155,-2.23354304473216,329.52102053026));
#21483=CARTESIAN_POINT('Ctrl Pts',(139.505336867592,-2.08757239714333,329.461514608317));
#21484=CARTESIAN_POINT('Ctrl Pts',(139.512735135029,-1.93924792253438,329.407856649989));
#21485=CARTESIAN_POINT('Ctrl Pts',(139.520133402465,-1.78908153339491,329.360220054881));
#21486=CARTESIAN_POINT('Ctrl Pts',(139.527534268991,-1.63886238922354,329.312566724536));
#21487=CARTESIAN_POINT('Ctrl Pts',(139.534935135517,-1.48680039769533,329.270939081883));
#21488=CARTESIAN_POINT('Ctrl Pts',(139.542336002043,-1.33342139130082,329.235460299753));
#21489=CARTESIAN_POINT('Ctrl Pts',(139.549744995427,-1.17987396009384,329.199942558529));
#21490=CARTESIAN_POINT('Ctrl Pts',(139.557153988812,-1.02500698969268,329.170587246164));
#21491=CARTESIAN_POINT('Ctrl Pts',(139.564562982197,-0.869355961450153,
329.147466294434));
#21492=CARTESIAN_POINT('Ctrl Pts',(139.571976539777,-0.713609046805256,
329.124331099399));
#21493=CARTESIAN_POINT('Ctrl Pts',(139.579390097358,-0.557077482054096,
329.107437957816));
#21494=CARTESIAN_POINT('Ctrl Pts',(139.586803654938,-0.400300069283826,
329.096806760995));
#21495=CARTESIAN_POINT('Ctrl Pts',(139.594227767075,-0.243299455164703,
329.08616042872));
#21496=CARTESIAN_POINT('Ctrl Pts',(139.601651879211,-0.0860526660484347,
329.081793856626));
#21497=CARTESIAN_POINT('Ctrl Pts',(139.609075991348,0.0709024746906525,
329.083674839769));
#21498=CARTESIAN_POINT('Ctrl Pts',(139.612933116502,0.152446989411648,329.084652086241));
#21499=CARTESIAN_POINT('Ctrl Pts',(139.616790241656,0.233912870431467,329.087314831304));
#21500=CARTESIAN_POINT('Ctrl Pts',(139.620647366811,0.315225552318783,329.091653072672));
#21501=CARTESIAN_POINT('Ctrl Pts',(139.628071344249,0.471731626564145,329.100003075524));
#21502=CARTESIAN_POINT('Ctrl Pts',(139.635495321687,0.628141794240556,329.114588498208));
#21503=CARTESIAN_POINT('Ctrl Pts',(139.642919299125,0.783918914991726,329.135411208173));
#21504=CARTESIAN_POINT('Ctrl Pts',(139.650334515152,0.939512195302699,329.156209344208));
#21505=CARTESIAN_POINT('Ctrl Pts',(139.65774973118,1.09447354946046,329.183230066496));
#21506=CARTESIAN_POINT('Ctrl Pts',(139.665164947208,1.24826710758629,329.216423270102));
#21507=CARTESIAN_POINT('Ctrl Pts',(139.672573028352,1.40191268632479,329.249584535375));
#21508=CARTESIAN_POINT('Ctrl Pts',(139.679981109496,1.55439234363106,329.288906380054));
#21509=CARTESIAN_POINT('Ctrl Pts',(139.68738919064,1.70517670583118,329.334287073599));
#21510=CARTESIAN_POINT('Ctrl Pts',(139.694791757814,1.85584883647644,329.379633989465));
#21511=CARTESIAN_POINT('Ctrl Pts',(139.702194324988,2.00482782867516,329.431030667607));
#21512=CARTESIAN_POINT('Ctrl Pts',(139.709596892162,2.15159596827859,329.488324632946));
#21513=CARTESIAN_POINT('Ctrl Pts',(139.716995561917,2.2982868350989,329.545588433264));
#21514=CARTESIAN_POINT('Ctrl Pts',(139.724394231672,2.44276882072263,329.60874320182));
#21515=CARTESIAN_POINT('Ctrl Pts',(139.731792901426,2.58454091661175,329.677587124916));
#21516=CARTESIAN_POINT('Ctrl Pts',(139.73919035063,2.7262896245066,329.746419690902));
#21517=CARTESIAN_POINT('Ctrl Pts',(139.746587799834,2.86532899451625,329.820939385876));
#21518=CARTESIAN_POINT('Ctrl Pts',(139.753985249038,3.00117939397023,329.900896862417));
#21519=CARTESIAN_POINT('Ctrl Pts',(139.761382377502,3.13702390318764,329.980850872141));
#21520=CARTESIAN_POINT('Ctrl Pts',(139.768779505965,3.26967939513561,330.066242005334));
#21521=CARTESIAN_POINT('Ctrl Pts',(139.776176634429,3.39869242281925,330.156775828276));
#21522=CARTESIAN_POINT('Ctrl Pts',(139.783574901865,3.5277253152887,330.247323591167));
#21523=CARTESIAN_POINT('Ctrl Pts',(139.790973169302,3.65311432125548,330.343015406085));
#21524=CARTESIAN_POINT('Ctrl Pts',(139.798371436739,3.77443660007292,330.443514631371));
#21525=CARTESIAN_POINT('Ctrl Pts',(139.805772303264,3.89580150068341,330.544049163092));
#21526=CARTESIAN_POINT('Ctrl Pts',(139.81317316979,4.01309654240838,330.649394229835));
#21527=CARTESIAN_POINT('Ctrl Pts',(139.820574036316,4.1259335884536,330.759174303727));
#21528=CARTESIAN_POINT('Ctrl Pts',(139.827983029701,4.23889454036246,330.869074926635));
#21529=CARTESIAN_POINT('Ctrl Pts',(139.835392023086,4.34738745274674,330.983420022058));
#21530=CARTESIAN_POINT('Ctrl Pts',(139.84280101647,4.45106205695689,331.101798218714));
#21531=CARTESIAN_POINT('Ctrl Pts',(139.850214574051,4.55480052829927,331.220249340423));
#21532=CARTESIAN_POINT('Ctrl Pts',(139.857628131631,4.65371454292192,331.342738224437));
#21533=CARTESIAN_POINT('Ctrl Pts',(139.865041689211,4.74749579707092,331.468822544916));
#21534=CARTESIAN_POINT('Ctrl Pts',(139.872465801348,4.84141056600413,331.595086369508));
#21535=CARTESIAN_POINT('Ctrl Pts',(139.879889913485,4.93017777004392,331.724955546475));
#21536=CARTESIAN_POINT('Ctrl Pts',(139.887314025621,5.01353344392814,331.857960380722));
#21537=CARTESIAN_POINT('Ctrl Pts',(139.891171150776,5.05684007246314,331.927061746972));
#21538=CARTESIAN_POINT('Ctrl Pts',(139.89502827593,5.09868677606702,331.997009108466));
#21539=CARTESIAN_POINT('Ctrl Pts',(139.898885401085,5.13904161424091,332.067734348733));
#21540=CARTESIAN_POINT('Ctrl Pts',(139.906309378523,5.21671433579345,332.203862311142));
#21541=CARTESIAN_POINT('Ctrl Pts',(139.913733355961,5.28909165923555,332.343283967131));
#21542=CARTESIAN_POINT('Ctrl Pts',(139.921157333399,5.35588133671999,332.485548634498));
#21543=CARTESIAN_POINT('Ctrl Pts',(139.928572549426,5.42259219233598,332.627645408153));
#21544=CARTESIAN_POINT('Ctrl Pts',(139.935987765454,5.48372837091779,332.772578180098));
#21545=CARTESIAN_POINT('Ctrl Pts',(139.943402981481,5.53904201683372,332.919869211263));
#21546=CARTESIAN_POINT('Ctrl Pts',(139.950811062626,5.59430244023815,333.067018519741));
#21547=CARTESIAN_POINT('Ctrl Pts',(139.95821914377,5.64375135400219,333.216521223023));
#21548=CARTESIAN_POINT('Ctrl Pts',(139.965627224914,5.68718783103696,333.36787710726));
#21549=CARTESIAN_POINT('Ctrl Pts',(139.973029792088,5.73059197750871,333.51912033455));
#21550=CARTESIAN_POINT('Ctrl Pts',(139.980432359262,5.76799249545076,333.672213639101));
#21551=CARTESIAN_POINT('Ctrl Pts',(139.987834926436,5.79923743957738,333.826639151026));
#21552=CARTESIAN_POINT('Ctrl Pts',(139.99523359619,5.83046593337704,333.980983358593));
#21553=CARTESIAN_POINT('Ctrl Pts',(140.002632265945,5.85554523394587,334.136658011775));
#21554=CARTESIAN_POINT('Ctrl Pts',(140.0100309357,5.8743739262603,334.293132588831));
#21555=CARTESIAN_POINT('Ctrl Pts',(140.017428384904,5.89319951242533,334.449581352442));
#21556=CARTESIAN_POINT('Ctrl Pts',(140.024825834108,5.90577649230412,334.606829407846));
#21557=CARTESIAN_POINT('Ctrl Pts',(140.032223283312,5.91205499070205,334.764338485503));
#21558=CARTESIAN_POINT('Ctrl Pts',(140.039620411775,5.91833321687523,334.921840733841));
#21559=CARTESIAN_POINT('Ctrl Pts',(140.047017540238,5.91831348969795,335.079603609012));
#21560=CARTESIAN_POINT('Ctrl Pts',(140.054414668702,5.91199801857741,335.237086462787));
#21561=CARTESIAN_POINT('Ctrl Pts',(140.061812936138,5.90568157503197,335.39459356499));
#21562=CARTESIAN_POINT('Ctrl Pts',(140.069211203575,5.89306747232098,335.551820187011));
#21563=CARTESIAN_POINT('Ctrl Pts',(140.076609471012,5.87420997626101,335.708228577011));
#21564=CARTESIAN_POINT('Ctrl Pts',(140.084010337537,5.85534585536425,335.864691914925));
#21565=CARTESIAN_POINT('Ctrl Pts',(140.091411204063,5.83023401876787,336.020336078204));
#21566=CARTESIAN_POINT('Ctrl Pts',(140.098812070589,5.79898021278113,336.174631454658));
#21567=CARTESIAN_POINT('Ctrl Pts',(140.106221063974,5.76769208712762,336.329096262186));
#21568=CARTESIAN_POINT('Ctrl Pts',(140.113630057358,5.73024859715437,336.482208959058));
#21569=CARTESIAN_POINT('Ctrl Pts',(140.121039050743,5.68680612328484,336.633452380288));
#21570=CARTESIAN_POINT('Ctrl Pts',(140.128452608323,5.64333688735305,336.784788972683));
#21571=CARTESIAN_POINT('Ctrl Pts',(140.135866165903,5.59386142059843,336.934253641367));
#21572=CARTESIAN_POINT('Ctrl Pts',(140.143279723484,5.53858484340473,337.081347759243));
#21573=CARTESIAN_POINT('Ctrl Pts',(140.15070383562,5.4832295698835,337.228651292526));
#21574=CARTESIAN_POINT('Ctrl Pts',(140.158127947757,5.42205683590311,337.373577191717));
#21575=CARTESIAN_POINT('Ctrl Pts',(140.165552059894,5.35531877133848,337.515649303828));
#21576=CARTESIAN_POINT('Ctrl Pts',(140.169409185049,5.32064565987542,337.589461485993));
#21577=CARTESIAN_POINT('Ctrl Pts',(140.173266310204,5.2844710838117,337.662503802708));
#21578=CARTESIAN_POINT('Ctrl Pts',(140.177123435359,5.24683503890533,337.734712532793));
#21579=CARTESIAN_POINT('Ctrl Pts',(140.184547412797,5.17439529764409,337.873695832903));
#21580=CARTESIAN_POINT('Ctrl Pts',(140.191971390235,5.09632017541685,338.010008526357));
#21581=CARTESIAN_POINT('Ctrl Pts',(140.199395367673,5.01283050842129,338.143160965706));
#21582=CARTESIAN_POINT('Ctrl Pts',(140.2068105837,4.9294393717946,338.276156265144));
#21583=CARTESIAN_POINT('Ctrl Pts',(140.214225799728,4.84064660608486,338.405998421137));
#21584=CARTESIAN_POINT('Ctrl Pts',(140.221641015756,4.7467198233623,338.532220474574));
#21585=CARTESIAN_POINT('Ctrl Pts',(140.2290490969,4.65288341651675,338.658321077787));
#21586=CARTESIAN_POINT('Ctrl Pts',(140.236457178044,4.55392304844181,338.780808215528));
#21587=CARTESIAN_POINT('Ctrl Pts',(140.243865259188,4.45015062645744,338.899242229503));
#21588=CARTESIAN_POINT('Ctrl Pts',(140.251267826362,4.34645544418261,339.017588090878));
#21589=CARTESIAN_POINT('Ctrl Pts',(140.258670393536,4.23795558458325,339.131886555905));
#21590=CARTESIAN_POINT('Ctrl Pts',(140.26607296071,4.12500430918265,339.241729601439));
#21591=CARTESIAN_POINT('Ctrl Pts',(140.273471630465,4.01211250213469,339.35151481509));
#21592=CARTESIAN_POINT('Ctrl Pts',(140.280870300219,3.89477421368746,339.456849021429));
#21593=CARTESIAN_POINT('Ctrl Pts',(140.288268969974,3.77338068940207,339.557359842644));
#21594=CARTESIAN_POINT('Ctrl Pts',(140.295666419178,3.65200719127845,339.657854082695));
#21595=CARTESIAN_POINT('Ctrl Pts',(140.303063868382,3.5265800722271,339.753526279065));
#21596=CARTESIAN_POINT('Ctrl Pts',(140.310461317586,3.39752498425916,339.844043202102));
#21597=CARTESIAN_POINT('Ctrl Pts',(140.31785844605,3.26847549189494,339.934556200484));
#21598=CARTESIAN_POINT('Ctrl Pts',(140.325255574513,3.13579864893123,340.019914155667));
#21599=CARTESIAN_POINT('Ctrl Pts',(140.332652702977,2.99995029363697,340.099826349809));
#21600=CARTESIAN_POINT('Ctrl Pts',(140.340050970413,2.86408102108679,340.179750848434));
#21601=CARTESIAN_POINT('Ctrl Pts',(140.34744923785,2.72503958557102,340.254227727192));
#21602=CARTESIAN_POINT('Ctrl Pts',(140.354847505287,2.58330756043057,340.323011610989));
#21603=CARTESIAN_POINT('Ctrl Pts',(140.362248371812,2.44152574334001,340.391819659287));
#21604=CARTESIAN_POINT('Ctrl Pts',(140.369649238338,2.29705179021712,340.454930567766));
#21605=CARTESIAN_POINT('Ctrl Pts',(140.377050104864,2.15038828864746,340.512146657206));
#21606=CARTESIAN_POINT('Ctrl Pts',(140.384459098249,2.00356373653097,340.569425575383));
#21607=CARTESIAN_POINT('Ctrl Pts',(140.391868091633,1.8545451822827,340.620796611725));
#21608=CARTESIAN_POINT('Ctrl Pts',(140.399277085018,1.7038521473927,340.666111402216));
#21609=CARTESIAN_POINT('Ctrl Pts',(140.406690642598,1.55306628039536,340.711454108182));
#21610=CARTESIAN_POINT('Ctrl Pts',(140.414104200179,1.4006042378463,340.750733041181));
#21611=CARTESIAN_POINT('Ctrl Pts',(140.421517757759,1.24699632831833,340.783850855586));
#21612=CARTESIAN_POINT('Ctrl Pts',(140.428941869896,1.09316972980945,340.817015819263));
#21613=CARTESIAN_POINT('Ctrl Pts',(140.436365982032,0.938194372873399,340.844002082093));
#21614=CARTESIAN_POINT('Ctrl Pts',(140.443790094169,0.782607106657409,340.864763991766));
#21615=CARTESIAN_POINT('Ctrl Pts',(140.447647219324,0.701773257814375,340.875550639728));
#21616=CARTESIAN_POINT('Ctrl Pts',(140.451504344478,0.620774276604041,340.884658055706));
#21617=CARTESIAN_POINT('Ctrl Pts',(140.455361469633,0.539685391524491,340.892085389798));
#21618=CARTESIAN_POINT('Ctrl Pts',(140.462785447071,0.383610068795989,340.906381104487));
#21619=CARTESIAN_POINT('Ctrl Pts',(140.470209424509,0.226730888180403,340.914492688595));
#21620=CARTESIAN_POINT('Ctrl Pts',(140.477633401947,0.0695791118012303,
340.916340871662));
#21621=CARTESIAN_POINT('Ctrl Pts',(140.485048617974,-0.0873872018372228,
340.918186873595));
#21622=CARTESIAN_POINT('Ctrl Pts',(140.492463834002,-0.244625101325928,
340.913784183549));
#21623=CARTESIAN_POINT('Ctrl Pts',(140.49987905003,-0.401597090539684,340.903105143852));
#21624=CARTESIAN_POINT('Ctrl Pts',(140.507287131174,-0.558418042095502,
340.892436379474));
#21625=CARTESIAN_POINT('Ctrl Pts',(140.514695212318,-0.714973222878964,
340.875503313274));
#21626=CARTESIAN_POINT('Ctrl Pts',(140.522103293462,-0.870724123905083,
340.852330310445));
#21627=CARTESIAN_POINT('Ctrl Pts',(140.529505860636,-1.02635909669033,340.829174555704));
#21628=CARTESIAN_POINT('Ctrl Pts',(140.53690842781,-1.18119061413119,340.799788166895));
#21629=CARTESIAN_POINT('Ctrl Pts',(140.544310994984,-1.33468439078115,340.764247404432));
#21630=CARTESIAN_POINT('Ctrl Pts',(140.551709664739,-1.48809735362897,340.728725354026));
#21631=CARTESIAN_POINT('Ctrl Pts',(140.559108334493,-1.64017361569421,340.687055467094));
#21632=CARTESIAN_POINT('Ctrl Pts',(140.566507004248,-1.79038831110776,340.639365235374));
#21633=CARTESIAN_POINT('Ctrl Pts',(140.573904453452,-1.9405782257613,340.591682871062));
#21634=CARTESIAN_POINT('Ctrl Pts',(140.581301902656,-2.08890682789001,340.537982245907));
#21635=CARTESIAN_POINT('Ctrl Pts',(140.58869935186,-2.23486355284494,340.478440970081));
#21636=CARTESIAN_POINT('Ctrl Pts',(140.596096480323,-2.38081394937115,340.418902275861));
#21637=CARTESIAN_POINT('Ctrl Pts',(140.603493608787,-2.52439232764025,340.353523575465));
#21638=CARTESIAN_POINT('Ctrl Pts',(140.61089073725,-2.66510753657285,340.282530868911));
#21639=CARTESIAN_POINT('Ctrl Pts',(140.618289004687,-2.80584441213424,340.211527231254));
#21640=CARTESIAN_POINT('Ctrl Pts',(140.625687272124,-2.94371690732875,340.134908034389));
#21641=CARTESIAN_POINT('Ctrl Pts',(140.63308553956,-3.07825807403807,340.05294545707));
#21642=CARTESIAN_POINT('Ctrl Pts',(140.640486406086,-3.21284650647498,339.970954085435));
#21643=CARTESIAN_POINT('Ctrl Pts',(140.647887272612,-3.34410096177593,339.883615789918));
#21644=CARTESIAN_POINT('Ctrl Pts',(140.655288139137,-3.47158322828818,339.791246231574));
#21645=CARTESIAN_POINT('Ctrl Pts',(140.662697132522,-3.59920548251621,339.698775242624));
#21646=CARTESIAN_POINT('Ctrl Pts',(140.670106125907,-3.72304697331511,339.60126217662));
#21647=CARTESIAN_POINT('Ctrl Pts',(140.677515119292,-3.84270179533154,339.499063621984));
#21648=CARTESIAN_POINT('Ctrl Pts',(140.684928676872,-3.96243032884669,339.396802109512));
#21649=CARTESIAN_POINT('Ctrl Pts',(140.692342234452,-4.07796678107884,339.289849609767));
#21650=CARTESIAN_POINT('Ctrl Pts',(140.699755792033,-4.188942311616,339.178599391238));
#21651=CARTESIAN_POINT('Ctrl Pts',(140.707179904169,-4.30007583613704,339.067190787656));
#21652=CARTESIAN_POINT('Ctrl Pts',(140.714604016306,-4.40663521840024,338.951472519044));
#21653=CARTESIAN_POINT('Ctrl Pts',(140.722028128443,-4.5082915485246,338.831871328216));
#21654=CARTESIAN_POINT('Ctrl Pts',(140.725885253597,-4.56110610477527,338.769733694358));
#21655=CARTESIAN_POINT('Ctrl Pts',(140.729742378752,-4.61259792162402,338.706548468387));
#21656=CARTESIAN_POINT('Ctrl Pts',(140.733599503907,-4.662725573915,338.642378451625));
#21657=CARTESIAN_POINT('Ctrl Pts',(140.741295425423,-4.76274267534399,338.514343349601));
#21658=CARTESIAN_POINT('Ctrl Pts',(140.748991346939,-4.85764424144846,338.381978211866));
#21659=CARTESIAN_POINT('Ctrl Pts',(140.756687268455,-4.94703476755112,338.245732208784));
#21660=CARTESIAN_POINT('Ctrl Pts',(140.764101460594,-5.0331529191608,338.114473847735));
#21661=CARTESIAN_POINT('Ctrl Pts',(140.771515652732,-5.11415610924468,337.979614061909));
#21662=CARTESIAN_POINT('Ctrl Pts',(140.778929844871,-5.18973002977055,337.84158983328));
#21663=CARTESIAN_POINT('Ctrl Pts',(140.786336986061,-5.26523207896498,337.703696866665));
#21664=CARTESIAN_POINT('Ctrl Pts',(140.793744127251,-5.33531495722257,337.562645771215));
#21665=CARTESIAN_POINT('Ctrl Pts',(140.80115126844,-5.39970745023283,337.418902646739));
#21666=CARTESIAN_POINT('Ctrl Pts',(140.80855282343,-5.46405138073848,337.275267928162));
#21667=CARTESIAN_POINT('Ctrl Pts',(140.81595437842,-5.52271331729638,337.128945560625));
#21668=CARTESIAN_POINT('Ctrl Pts',(140.82335593341,-5.57546790057303,336.98042628042));
#21669=CARTESIAN_POINT('Ctrl Pts',(140.830753363167,-5.62819308124973,336.831989776966));
#21670=CARTESIAN_POINT('Ctrl Pts',(140.838150792923,-5.67501734023533,336.681359149259));
#21671=CARTESIAN_POINT('Ctrl Pts',(140.84554822268,-5.71576345500202,336.529045025159));
#21672=CARTESIAN_POINT('Ctrl Pts',(140.852943502287,-5.75649772643343,336.376775172942));
#21673=CARTESIAN_POINT('Ctrl Pts',(140.860338781894,-5.79115727330841,336.222823157763));
#21674=CARTESIAN_POINT('Ctrl Pts',(140.867734061501,-5.81961476231465,336.067714653243));
#21675=CARTESIAN_POINT('Ctrl Pts',(140.875128144217,-5.84806764560735,335.912631252319));
#21676=CARTESIAN_POINT('Ctrl Pts',(140.882522226932,-5.87032040608578,335.756392101837));
#21677=CARTESIAN_POINT('Ctrl Pts',(140.889916309647,-5.88629689205176,335.599532702296));
#21678=CARTESIAN_POINT('Ctrl Pts',(140.897311781641,-5.90227637985019,335.442643830339));
#21679=CARTESIAN_POINT('Ctrl Pts',(140.904707253635,-5.91197720194651,335.285134847513));
#21680=CARTESIAN_POINT('Ctrl Pts',(140.91210272563,-5.91537509813926,335.1275461125));
#21681=CARTESIAN_POINT('Ctrl Pts',(140.914169023851,-5.916324471873,335.083515748632));
#21682=CARTESIAN_POINT('Ctrl Pts',(140.916235322073,-5.91678212280831,335.039479167637));
#21683=CARTESIAN_POINT('Ctrl Pts',(140.918301620294,-5.91674824910051,334.995448157951));
#21684=CARTESIAN_POINT('',(142.668300681201,-5.92181077008912,334.998336726183));
#21685=CARTESIAN_POINT('Ctrl Pts',(140.91830369428,-5.9110591082604,334.99540838233));
#21686=CARTESIAN_POINT('Ctrl Pts',(140.949481642247,-5.91579322684826,334.331668430357));
#21687=CARTESIAN_POINT('Ctrl Pts',(141.073405601637,-5.50601630485396,331.699164255947));
#21688=CARTESIAN_POINT('Ctrl Pts',(141.290075572456,-1.63579549677484,328.197294948772));
#21689=CARTESIAN_POINT('Ctrl Pts',(141.568313606728,4.83531700169147,329.943090626247));
#21690=CARTESIAN_POINT('Ctrl Pts',(141.846551641003,6.86913045686709,336.329537396148));
#21691=CARTESIAN_POINT('Ctrl Pts',(142.124789675277,2.59924427997537,341.495887321548));
#21692=CARTESIAN_POINT('Ctrl Pts',(142.398705767854,-3.9525535038928,340.713403626196));
#21693=CARTESIAN_POINT('Ctrl Pts',(142.579875849006,-5.91886630634388,336.86865198698));
#21694=CARTESIAN_POINT('Ctrl Pts',(142.668299918733,-5.92591990352904,334.998351685574));
#21695=CARTESIAN_POINT('',(144.418301620294,-5.91612998447623,335.005450957973));
#21696=CARTESIAN_POINT('Ctrl Pts',(142.668301620294,-5.91674976100815,334.998318301469));
#21697=CARTESIAN_POINT('Ctrl Pts',(142.672622994804,-5.9167238219269,334.907056371931));
#21698=CARTESIAN_POINT('Ctrl Pts',(142.676944369314,-5.91458651643603,334.81582708582));
#21699=CARTESIAN_POINT('Ctrl Pts',(142.681265743824,-5.91034167140472,334.7246967313));
#21700=CARTESIAN_POINT('Ctrl Pts',(142.688689721262,-5.90304916906167,334.568137818322));
#21701=CARTESIAN_POINT('Ctrl Pts',(142.6961136987,-5.88952074126305,334.411632685024));
#21702=CARTESIAN_POINT('Ctrl Pts',(142.703537676138,-5.86975089183501,334.255718446889));
#21703=CARTESIAN_POINT('Ctrl Pts',(142.710952892166,-5.85000437380384,334.099988211013));
#21704=CARTESIAN_POINT('Ctrl Pts',(142.718368108193,-5.82403114240898,333.944847848869));
#21705=CARTESIAN_POINT('Ctrl Pts',(142.725783324221,-5.79187768125842,333.790833556602));
#21706=CARTESIAN_POINT('Ctrl Pts',(142.733191405365,-5.75975515800627,333.636967456111));
#21707=CARTESIAN_POINT('Ctrl Pts',(142.740599486509,-5.72146431930344,333.484225631346));
#21708=CARTESIAN_POINT('Ctrl Pts',(142.748007567654,-5.67710331707251,333.333138131163));
#21709=CARTESIAN_POINT('Ctrl Pts',(142.755410134828,-5.63277533354574,333.182163088165));
#21710=CARTESIAN_POINT('Ctrl Pts',(142.762812702002,-5.58238628744325,333.032840274525));
#21711=CARTESIAN_POINT('Ctrl Pts',(142.770215269176,-5.52608515283655,332.885688422654));
#21712=CARTESIAN_POINT('Ctrl Pts',(142.77761393893,-5.4698136605311,332.73861404559));
#21713=CARTESIAN_POINT('Ctrl Pts',(142.785012608685,-5.40763641185448,332.593708701631));
#21714=CARTESIAN_POINT('Ctrl Pts',(142.79241127844,-5.33975183122995,332.451474751277));
#21715=CARTESIAN_POINT('Ctrl Pts',(142.799808727644,-5.27187844945332,332.309264265109));
#21716=CARTESIAN_POINT('Ctrl Pts',(142.807206176848,-5.19829976496392,332.169724634393));
#21717=CARTESIAN_POINT('Ctrl Pts',(142.814603626052,-5.11926187923096,332.033337165374));
#21718=CARTESIAN_POINT('Ctrl Pts',(142.822000754515,-5.04022742044303,331.896955609878));
#21719=CARTESIAN_POINT('Ctrl Pts',(142.829397882979,-4.95573441818043,331.763726267237));
#21720=CARTESIAN_POINT('Ctrl Pts',(142.836795011442,-4.86607423608487,331.634104563209));
#21721=CARTESIAN_POINT('Ctrl Pts',(142.844193278879,-4.7764002485594,331.504462900674));
#21722=CARTESIAN_POINT('Ctrl Pts',(142.851591546316,-4.68155770934711,331.378430289754));
#21723=CARTESIAN_POINT('Ctrl Pts',(142.858989813752,-4.58188039583534,331.2564318357));
#21724=CARTESIAN_POINT('Ctrl Pts',(142.866390680278,-4.48216806463516,331.134390522307));
#21725=CARTESIAN_POINT('Ctrl Pts',(142.873791546804,-4.37761781339542,331.016386476335));
#21726=CARTESIAN_POINT('Ctrl Pts',(142.88119241333,-4.26860253927908,330.90281036268));
#21727=CARTESIAN_POINT('Ctrl Pts',(142.888601406714,-4.15946755596934,330.789109531594));
#21728=CARTESIAN_POINT('Ctrl Pts',(142.896010400099,-4.04585801677911,330.679846612496));
#21729=CARTESIAN_POINT('Ctrl Pts',(142.903419393484,-3.92818291728981,330.575374645146));
#21730=CARTESIAN_POINT('Ctrl Pts',(142.910832951064,-3.81043532588013,330.470838319462));
#21731=CARTESIAN_POINT('Ctrl Pts',(142.918246508644,-3.68861747166693,330.371099062443));
#21732=CARTESIAN_POINT('Ctrl Pts',(142.925660066225,-3.56316958758489,330.276468159035));
#21733=CARTESIAN_POINT('Ctrl Pts',(142.933084178361,-3.4375431054737,330.181702531211));
#21734=CARTESIAN_POINT('Ctrl Pts',(142.940508290498,-3.30827657779703,330.092059994091));
#21735=CARTESIAN_POINT('Ctrl Pts',(142.947932402635,-3.1758379056566,330.007807680037));
#21736=CARTESIAN_POINT('Ctrl Pts',(142.951789527789,-3.10703068341109,329.964035210832));
#21737=CARTESIAN_POINT('Ctrl Pts',(142.955646652944,-3.03736762239442,329.921716917943));
#21738=CARTESIAN_POINT('Ctrl Pts',(142.959503778099,-2.96691662174357,329.880885201314));
#21739=CARTESIAN_POINT('Ctrl Pts',(142.966927755537,-2.8313165003209,329.802294610952));
#21740=CARTESIAN_POINT('Ctrl Pts',(142.974351732975,-2.69238698629703,329.728977046614));
#21741=CARTESIAN_POINT('Ctrl Pts',(142.981775710413,-2.55057677724521,329.661227794157));
#21742=CARTESIAN_POINT('Ctrl Pts',(142.98919092644,-2.40893392557663,329.593558496012));
#21743=CARTESIAN_POINT('Ctrl Pts',(142.996606142468,-2.26441747942392,329.531444588498));
#21744=CARTESIAN_POINT('Ctrl Pts',(143.004021358496,-2.11750349251186,329.47513714906));
#21745=CARTESIAN_POINT('Ctrl Pts',(143.01142943964,-1.97073086549829,329.418883888356));
#21746=CARTESIAN_POINT('Ctrl Pts',(143.018837520784,-1.82156563649957,329.368426105816));
#21747=CARTESIAN_POINT('Ctrl Pts',(143.026245601928,-1.67050665054391,329.323968103244));
#21748=CARTESIAN_POINT('Ctrl Pts',(143.033648169102,-1.51956010055028,329.279543191576));
#21749=CARTESIAN_POINT('Ctrl Pts',(143.041050736276,-1.36672295672868,329.241109272844));
#21750=CARTESIAN_POINT('Ctrl Pts',(143.04845330345,-1.21251205064942,329.208821787449));
#21751=CARTESIAN_POINT('Ctrl Pts',(143.055851973205,-1.05838233593813,329.176551301273));
#21752=CARTESIAN_POINT('Ctrl Pts',(143.06325064296,-0.902880663794444,329.150420879895));
#21753=CARTESIAN_POINT('Ctrl Pts',(143.070649312714,-0.746536858721354,
329.130535520078));
#21754=CARTESIAN_POINT('Ctrl Pts',(143.078046761918,-0.590218845521367,
329.110653440727));
#21755=CARTESIAN_POINT('Ctrl Pts',(143.085444211122,-0.433059344983441,
329.097014425284));
#21756=CARTESIAN_POINT('Ctrl Pts',(143.092841660326,-0.275596277423134,
329.089671984198));
#21757=CARTESIAN_POINT('Ctrl Pts',(143.10023878879,-0.118140037187029,329.082329861468));
#21758=CARTESIAN_POINT('Ctrl Pts',(143.107635917253,0.0396193710945745,
329.081283787649));
#21759=CARTESIAN_POINT('Ctrl Pts',(143.115033045717,0.197141296601919,329.086535205848));
#21760=CARTESIAN_POINT('Ctrl Pts',(143.122431313153,0.354687476553515,329.091787432634));
#21761=CARTESIAN_POINT('Ctrl Pts',(143.12982958059,0.51199572789554,329.103339069716));
#21762=CARTESIAN_POINT('Ctrl Pts',(143.137227848026,0.66852794445636,329.121139485412));
#21763=CARTESIAN_POINT('Ctrl Pts',(143.144628714552,0.825115152431099,329.138946154581));
#21764=CARTESIAN_POINT('Ctrl Pts',(143.152029581078,0.980925412232693,329.163005930985));
#21765=CARTESIAN_POINT('Ctrl Pts',(143.159430447604,1.13542840936469,329.193216648633));
#21766=CARTESIAN_POINT('Ctrl Pts',(143.166839440988,1.29010106555872,329.223460540538));
#21767=CARTESIAN_POINT('Ctrl Pts',(143.174248434373,1.44346322582083,329.259868790768));
#21768=CARTESIAN_POINT('Ctrl Pts',(143.181657427758,1.59499668050585,329.302288516283));
#21769=CARTESIAN_POINT('Ctrl Pts',(143.189070985338,1.74662348502579,329.344734373813));
#21770=CARTESIAN_POINT('Ctrl Pts',(143.196484542918,1.89641898491813,329.393198971281));
#21771=CARTESIAN_POINT('Ctrl Pts',(143.203898100499,2.04388317873062,329.447480561565));
#21772=CARTESIAN_POINT('Ctrl Pts',(143.211322212635,2.19155731481988,329.50183943163));
#21773=CARTESIAN_POINT('Ctrl Pts',(143.218746324772,2.33689317216164,329.56203169201));
#21774=CARTESIAN_POINT('Ctrl Pts',(143.226170436909,2.47941290531834,329.627808435337));
#21775=CARTESIAN_POINT('Ctrl Pts',(143.230027562063,2.55345764463177,329.66198210171));
#21776=CARTESIAN_POINT('Ctrl Pts',(143.233884687218,2.62674267952514,329.697662399409));
#21777=CARTESIAN_POINT('Ctrl Pts',(143.237741812373,2.69920402007419,329.734809764072));
#21778=CARTESIAN_POINT('Ctrl Pts',(143.245165789811,2.83867353060131,329.806308921106));
#21779=CARTESIAN_POINT('Ctrl Pts',(143.252589767249,2.97551056642688,329.883461372355));
#21780=CARTESIAN_POINT('Ctrl Pts',(143.260013744687,3.10922399937078,329.966049594579));
#21781=CARTESIAN_POINT('Ctrl Pts',(143.267428960714,3.24277963034558,330.048540350275));
#21782=CARTESIAN_POINT('Ctrl Pts',(143.274844176742,3.37321868168104,330.136453913517));
#21783=CARTESIAN_POINT('Ctrl Pts',(143.282259392769,3.50007239701229,330.229525832983));
#21784=CARTESIAN_POINT('Ctrl Pts',(143.289667473914,3.62680405433742,330.322508199118));
#21785=CARTESIAN_POINT('Ctrl Pts',(143.297075555058,3.74995694465513,330.420638821084));
#21786=CARTESIAN_POINT('Ctrl Pts',(143.304483636202,3.86908931255105,330.523608768885));
#21787=CARTESIAN_POINT('Ctrl Pts',(143.311886203376,3.98813300804967,330.626502074273));
#21788=CARTESIAN_POINT('Ctrl Pts',(143.31928877055,4.1031618585777,330.734227290387));
#21789=CARTESIAN_POINT('Ctrl Pts',(143.326691337724,4.2137654637697,330.846433920251));
#21790=CARTESIAN_POINT('Ctrl Pts',(143.334090007479,4.32431083664691,330.958581473815));
#21791=CARTESIAN_POINT('Ctrl Pts',(143.341488677233,4.43043534293211,331.075205477032));
#21792=CARTESIAN_POINT('Ctrl Pts',(143.348887346988,4.53176397016878,331.195917208948));
#21793=CARTESIAN_POINT('Ctrl Pts',(143.356284796192,4.63307588132849,331.316609027176));
#21794=CARTESIAN_POINT('Ctrl Pts',(143.363682245396,4.72959324394162,331.441386950166));
#21795=CARTESIAN_POINT('Ctrl Pts',(143.3710796946,4.82097996038017,331.569827586824));
#21796=CARTESIAN_POINT('Ctrl Pts',(143.378476823063,4.91236271444998,331.69826265452));
#21797=CARTESIAN_POINT('Ctrl Pts',(143.385873951527,4.99861504829554,331.830359816026));
#21798=CARTESIAN_POINT('Ctrl Pts',(143.39327107999,5.07944317119631,331.965665207482));
#21799=CARTESIAN_POINT('Ctrl Pts',(143.400669347427,5.16028373961033,332.10099143259));
#21800=CARTESIAN_POINT('Ctrl Pts',(143.408067614864,5.23569824269158,332.239526550826));
#21801=CARTESIAN_POINT('Ctrl Pts',(143.4154658823,5.3054380575754,332.380790657521));
#21802=CARTESIAN_POINT('Ctrl Pts',(143.422866748826,5.37520237278961,332.522104391782));
#21803=CARTESIAN_POINT('Ctrl Pts',(143.430267615352,5.43928786548871,332.666148688877));
#21804=CARTESIAN_POINT('Ctrl Pts',(143.437668481877,5.49749346562875,332.812422308152));
#21805=CARTESIAN_POINT('Ctrl Pts',(143.445077475262,5.55576298108242,332.958856549846));
#21806=CARTESIAN_POINT('Ctrl Pts',(143.452486468647,5.60813957156559,333.107524655552));
#21807=CARTESIAN_POINT('Ctrl Pts',(143.459895462032,5.65447136671199,333.257908117941));
#21808=CARTESIAN_POINT('Ctrl Pts',(143.467309019612,5.70083170384236,333.408384221731));
#21809=CARTESIAN_POINT('Ctrl Pts',(143.474722577192,5.74113973014074,333.560577427925));
#21810=CARTESIAN_POINT('Ctrl Pts',(143.482136134772,5.77529451959006,333.713958097692));
#21811=CARTESIAN_POINT('Ctrl Pts',(143.489560246909,5.80949793463501,333.867557132922));
#21812=CARTESIAN_POINT('Ctrl Pts',(143.496984359046,5.83753055051313,334.022346641888));
#21813=CARTESIAN_POINT('Ctrl Pts',(143.504408471183,5.85934308915607,334.177790096107));
#21814=CARTESIAN_POINT('Ctrl Pts',(143.508265596337,5.87067558116844,334.258549228832));
#21815=CARTESIAN_POINT('Ctrl Pts',(143.512122721492,5.88032999510254,334.339484834562));
#21816=CARTESIAN_POINT('Ctrl Pts',(143.515979846647,5.88830497285585,334.42052169226));
#21817=CARTESIAN_POINT('Ctrl Pts',(143.523403824085,5.90365476124339,334.576496875606));
#21818=CARTESIAN_POINT('Ctrl Pts',(143.530827801523,5.91282599080499,334.7333176767));
#21819=CARTESIAN_POINT('Ctrl Pts',(143.538251778961,5.91573580383548,334.89045338107));
#21820=CARTESIAN_POINT('Ctrl Pts',(143.545666994988,5.91864218284879,335.047403641667));
#21821=CARTESIAN_POINT('Ctrl Pts',(143.553082211016,5.91530184723368,335.20466769628));
#21822=CARTESIAN_POINT('Ctrl Pts',(143.560497427044,5.90568350878237,335.361708247896));
#21823=CARTESIAN_POINT('Ctrl Pts',(143.567905508188,5.89607442504789,335.518597695884));
#21824=CARTESIAN_POINT('Ctrl Pts',(143.575313589332,5.88019938697362,335.675263698984));
#21825=CARTESIAN_POINT('Ctrl Pts',(143.582721670476,5.85807912118249,335.831167595895));
#21826=CARTESIAN_POINT('Ctrl Pts',(143.59012423765,5.83597531990917,335.986955450688));
#21827=CARTESIAN_POINT('Ctrl Pts',(143.597526804824,5.8076355988372,336.141981960841));
#21828=CARTESIAN_POINT('Ctrl Pts',(143.604929371998,5.77313260716383,336.295712337906));
#21829=CARTESIAN_POINT('Ctrl Pts',(143.612328041753,5.73864778116478,336.449361776599));
#21830=CARTESIAN_POINT('Ctrl Pts',(143.619726711507,5.6980062285689,336.601716078027));
#21831=CARTESIAN_POINT('Ctrl Pts',(143.627125381262,5.6513318923623,336.752249526999));
#21832=CARTESIAN_POINT('Ctrl Pts',(143.634522830466,5.60466525597187,336.902758142627));
#21833=CARTESIAN_POINT('Ctrl Pts',(143.64192027967,5.5519679215841,337.051446145841));
#21834=CARTESIAN_POINT('Ctrl Pts',(143.649317728874,5.49341404609098,337.197801783763));
#21835=CARTESIAN_POINT('Ctrl Pts',(143.656714857338,5.43486270939183,337.344151075959));
#21836=CARTESIAN_POINT('Ctrl Pts',(143.664111985801,5.37045547511358,337.488167857427));
#21837=CARTESIAN_POINT('Ctrl Pts',(143.671509114265,5.30041502004282,337.629359461505));
#21838=CARTESIAN_POINT('Ctrl Pts',(143.678907381701,5.2303637804904,337.770572805565));
#21839=CARTESIAN_POINT('Ctrl Pts',(143.686305649138,5.15467775894931,337.908959771725));
#21840=CARTESIAN_POINT('Ctrl Pts',(143.693703916574,5.07362597339506,338.04405158376));
#21841=CARTESIAN_POINT('Ctrl Pts',(143.7011047831,4.99254571349615,338.179190854969));
#21842=CARTESIAN_POINT('Ctrl Pts',(143.708505649626,4.906096128343,338.311032347402));
#21843=CARTESIAN_POINT('Ctrl Pts',(143.715906516152,4.81458991135569,338.43913572689));
#21844=CARTESIAN_POINT('Ctrl Pts',(143.723315509536,4.72298321179376,338.567379776136));
#21845=CARTESIAN_POINT('Ctrl Pts',(143.730724502921,4.62630900848876,338.691877211051));
#21846=CARTESIAN_POINT('Ctrl Pts',(143.738133496306,4.52492113954678,338.812219726535));
#21847=CARTESIAN_POINT('Ctrl Pts',(143.745547053886,4.42347081218027,338.93263637716));
#21848=CARTESIAN_POINT('Ctrl Pts',(143.752960611466,4.31730128409592,339.048892733124));
#21849=CARTESIAN_POINT('Ctrl Pts',(143.760374169047,4.20680332302805,339.160617305624));
#21850=CARTESIAN_POINT('Ctrl Pts',(143.767798281183,4.09614804788336,339.272500938507));
#21851=CARTESIAN_POINT('Ctrl Pts',(143.77522239332,3.98115230446707,339.37983964837));
#21852=CARTESIAN_POINT('Ctrl Pts',(143.782646505457,3.86224060383601,339.482301649887));
#21853=CARTESIAN_POINT('Ctrl Pts',(143.786503630611,3.80046118789527,339.535534784862));
#21854=CARTESIAN_POINT('Ctrl Pts',(143.790360755766,3.73762526770217,339.587452287851));
#21855=CARTESIAN_POINT('Ctrl Pts',(143.794217880921,3.67379536328656,339.638012310375));
#21856=CARTESIAN_POINT('Ctrl Pts',(143.801641858359,3.5509391552939,339.735327396466));
#21857=CARTESIAN_POINT('Ctrl Pts',(143.809065835797,3.42402827659011,339.827904412912));
#21858=CARTESIAN_POINT('Ctrl Pts',(143.816489813235,3.29346417723805,339.915386482846));
#21859=CARTESIAN_POINT('Ctrl Pts',(143.823905029262,3.1630541631676,340.002765310777));
#21860=CARTESIAN_POINT('Ctrl Pts',(143.83132024529,3.02899981729281,340.085060955055));
#21861=CARTESIAN_POINT('Ctrl Pts',(143.838735461318,2.89173603228946,340.161956342518));
#21862=CARTESIAN_POINT('Ctrl Pts',(143.846143542462,2.75460432180896,340.238777741626));
#21863=CARTESIAN_POINT('Ctrl Pts',(143.853551623606,2.6142696434686,340.3102090472));
#21864=CARTESIAN_POINT('Ctrl Pts',(143.86095970475,2.47119618541267,340.375976188164));
#21865=CARTESIAN_POINT('Ctrl Pts',(143.868362271924,2.32822921954471,340.441694377443));
#21866=CARTESIAN_POINT('Ctrl Pts',(143.875764839098,2.18252787060725,340.501756641455));
#21867=CARTESIAN_POINT('Ctrl Pts',(143.883167406272,2.03458116826425,340.555934667744));
#21868=CARTESIAN_POINT('Ctrl Pts',(143.890566076026,1.88671235921323,340.61008416954));
#21869=CARTESIAN_POINT('Ctrl Pts',(143.897964745781,1.73660090068536,340.658355475503));
#21870=CARTESIAN_POINT('Ctrl Pts',(143.905363415536,1.58475595046043,340.70056831728));
#21871=CARTESIAN_POINT('Ctrl Pts',(143.91276086474,1.43293604993725,340.742774195249));
#21872=CARTESIAN_POINT('Ctrl Pts',(143.920158313944,1.27938358450519,340.77892349277));
#21873=CARTESIAN_POINT('Ctrl Pts',(143.927555763148,1.124623144367,340.808885723239));
#21874=CARTESIAN_POINT('Ctrl Pts',(143.934952891611,0.969869414371734,340.838846654599));
#21875=CARTESIAN_POINT('Ctrl Pts',(143.942350020075,0.813908180217969,340.86262098136));
#21876=CARTESIAN_POINT('Ctrl Pts',(143.949747148538,0.657274238999061,340.880129346983));
#21877=CARTESIAN_POINT('Ctrl Pts',(143.957145415975,0.500616180063091,340.897640408457));
#21878=CARTESIAN_POINT('Ctrl Pts',(143.964543683411,0.3432855787443,340.908883546284));
#21879=CARTESIAN_POINT('Ctrl Pts',(143.971941950848,0.185822220032969,340.913831301706));
#21880=CARTESIAN_POINT('Ctrl Pts',(143.979342817374,0.0283035427879143,
340.918780795327));
#21881=CARTESIAN_POINT('Ctrl Pts',(143.986743683899,-0.129347611915808,
340.91743049147));
#21882=CARTESIAN_POINT('Ctrl Pts',(143.994144550425,-0.286591741330341,
340.909805050617));
#21883=CARTESIAN_POINT('Ctrl Pts',(144.00155354381,-0.444008539832157,340.902171236302));
#21884=CARTESIAN_POINT('Ctrl Pts',(144.008962537195,-0.601017047460843,
340.888248541983));
#21885=CARTESIAN_POINT('Ctrl Pts',(144.016371530579,-0.757082429645215,
340.868113560355));
#21886=CARTESIAN_POINT('Ctrl Pts',(144.02378508816,-0.913243953488337,340.847966174884));
#21887=CARTESIAN_POINT('Ctrl Pts',(144.03119864574,-1.06846082709166,340.821598938691));
#21888=CARTESIAN_POINT('Ctrl Pts',(144.03861220332,-1.22220919075155,340.789139422794));
#21889=CARTESIAN_POINT('Ctrl Pts',(144.046036315457,-1.3761764433544,340.756633694832));
#21890=CARTESIAN_POINT('Ctrl Pts',(144.053460427593,-1.528670649666,340.718018455868));
#21891=CARTESIAN_POINT('Ctrl Pts',(144.06088453973,-1.67918307703539,340.673471138227));
#21892=CARTESIAN_POINT('Ctrl Pts',(144.064741664885,-1.75738034278653,340.650327013207));
#21893=CARTESIAN_POINT('Ctrl Pts',(144.06859879004,-1.83504300060573,340.625582487263));
#21894=CARTESIAN_POINT('Ctrl Pts',(144.072455915194,-1.91210202603938,340.599267488209));
#21895=CARTESIAN_POINT('Ctrl Pts',(144.079879892632,-2.06042090169271,340.548617858908));
#21896=CARTESIAN_POINT('Ctrl Pts',(144.08730387007,-2.20694964847762,340.491994529147));
#21897=CARTESIAN_POINT('Ctrl Pts',(144.094727847508,-2.35117091336048,340.429541960301));
#21898=CARTESIAN_POINT('Ctrl Pts',(144.102143063536,-2.49522197545173,340.367163094882));
#21899=CARTESIAN_POINT('Ctrl Pts',(144.109558279564,-2.63697063701664,340.298968830754));
#21900=CARTESIAN_POINT('Ctrl Pts',(144.116973495591,-2.77591491908541,340.225153291962));
#21901=CARTESIAN_POINT('Ctrl Pts',(144.124381576735,-2.91472550966543,340.15140877811));
#21902=CARTESIAN_POINT('Ctrl Pts',(144.131789657879,-3.0507367652961,340.072053931358));
#21903=CARTESIAN_POINT('Ctrl Pts',(144.139197739024,-3.18346701492038,339.987330781832));
#21904=CARTESIAN_POINT('Ctrl Pts',(144.146600306198,-3.31609847099563,339.902670693295));
#21905=CARTESIAN_POINT('Ctrl Pts',(144.154002873372,-3.44545347042777,339.812650458));
#21906=CARTESIAN_POINT('Ctrl Pts',(144.161405440546,-3.5710753783907,339.717557758454));
#21907=CARTESIAN_POINT('Ctrl Pts',(144.1688041103,-3.69663114696838,339.622515124799));
#21908=CARTESIAN_POINT('Ctrl Pts',(144.176202780055,-3.81845744157945,339.522405570298));
#21909=CARTESIAN_POINT('Ctrl Pts',(144.18360144981,-3.9361271362298,339.417559703041));
#21910=CARTESIAN_POINT('Ctrl Pts',(144.190998899014,-4.05377741903429,339.312731132097));
#21911=CARTESIAN_POINT('Ctrl Pts',(144.198396348218,-4.16727218441492,339.203168047151));
#21912=CARTESIAN_POINT('Ctrl Pts',(144.205793797422,-4.27621781754429,339.089240973508));
#21913=CARTESIAN_POINT('Ctrl Pts',(144.213190925885,-4.38515872698083,338.975318839545));
#21914=CARTESIAN_POINT('Ctrl Pts',(144.220588054349,-4.48955063841171,338.857033362838));
#21915=CARTESIAN_POINT('Ctrl Pts',(144.227985182812,-4.58903740983581,338.734791321296));
#21916=CARTESIAN_POINT('Ctrl Pts',(144.235383450249,-4.68853949973932,338.612530457531));
#21917=CARTESIAN_POINT('Ctrl Pts',(144.242781717685,-4.78313471020176,338.486312105389));
#21918=CARTESIAN_POINT('Ctrl Pts',(144.250179985122,-4.87250784193644,338.356575322076));
#21919=CARTESIAN_POINT('Ctrl Pts',(144.257580851648,-4.96191237139198,338.226792960866));
#21920=CARTESIAN_POINT('Ctrl Pts',(144.264981718174,-5.04609095790214,338.093490014637));
#21921=CARTESIAN_POINT('Ctrl Pts',(144.272382584699,-5.12477238309994,337.957133507963));
#21922=CARTESIAN_POINT('Ctrl Pts',(144.279791578084,-5.20354020802499,337.820627268807));
#21923=CARTESIAN_POINT('Ctrl Pts',(144.287200571469,-5.27679862996858,337.681061096332));
#21924=CARTESIAN_POINT('Ctrl Pts',(144.294609564854,-5.34432262768628,337.538926193039));
#21925=CARTESIAN_POINT('Ctrl Pts',(144.302023122434,-5.41188822251574,337.396703729743));
#21926=CARTESIAN_POINT('Ctrl Pts',(144.309436680014,-5.47371220772978,337.251909724867));
#21927=CARTESIAN_POINT('Ctrl Pts',(144.316850237595,-5.5296183699733,337.105053739208));
#21928=CARTESIAN_POINT('Ctrl Pts',(144.324274349731,-5.58560412487372,336.957988677168));
#21929=CARTESIAN_POINT('Ctrl Pts',(144.331698461868,-5.63565511175932,336.808856124213));
#21930=CARTESIAN_POINT('Ctrl Pts',(144.339122574005,-5.67964523282997,336.658179903295));
#21931=CARTESIAN_POINT('Ctrl Pts',(144.342979699159,-5.70249987179603,336.579897540209));
#21932=CARTESIAN_POINT('Ctrl Pts',(144.346836824314,-5.72371939245442,336.501198671567));
#21933=CARTESIAN_POINT('Ctrl Pts',(144.350693949468,-5.74329160865003,336.422157537163));
#21934=CARTESIAN_POINT('Ctrl Pts',(144.360547443046,-5.79329120650338,336.220237381848));
#21935=CARTESIAN_POINT('Ctrl Pts',(144.370400936624,-5.83266066500019,336.015588525642));
#21936=CARTESIAN_POINT('Ctrl Pts',(144.380254430202,-5.8611578583291,335.809171874355));
#21937=CARTESIAN_POINT('Ctrl Pts',(144.389879845096,-5.88899542750374,335.607533146545));
#21938=CARTESIAN_POINT('Ctrl Pts',(144.399505259989,-5.90645829256422,335.40420720989));
#21939=CARTESIAN_POINT('Ctrl Pts',(144.409130674883,-5.91336500329359,335.200112219323));
#21940=CARTESIAN_POINT('Ctrl Pts',(144.412187650663,-5.91555853444581,335.135292837514));
#21941=CARTESIAN_POINT('Ctrl Pts',(144.415244626444,-5.91668764623935,335.070396075559));
#21942=CARTESIAN_POINT('Ctrl Pts',(144.418301602224,-5.91674748820401,335.005451910815));
#21943=CARTESIAN_POINT('',(146.168301649435,-5.91279607591744,334.998941304638));
#21944=CARTESIAN_POINT('Ctrl Pts',(144.418301620294,-5.91612998447623,335.005450957973));
#21945=CARTESIAN_POINT('Ctrl Pts',(144.488511741443,-5.90248000309968,333.51400828609));
#21946=CARTESIAN_POINT('Ctrl Pts',(144.651467874018,-4.57331437570988,330.03073686821));
#21947=CARTESIAN_POINT('Ctrl Pts',(144.907170018015,1.28310118904558,328.122044325536));
#21948=CARTESIAN_POINT('Ctrl Pts',(145.18540805229,6.47817933912946,332.356930691166));
#21949=CARTESIAN_POINT('Ctrl Pts',(145.463646086563,5.72832792746371,339.017322749874));
#21950=CARTESIAN_POINT('Ctrl Pts',(145.741884120838,-0.27832547325347,341.991077016609));
#21951=CARTESIAN_POINT('Ctrl Pts',(145.976769298748,-5.1334511087582,339.085505629792));
#21952=CARTESIAN_POINT('Ctrl Pts',(146.118908465233,-5.90546254146294,336.052211088219));
#21953=CARTESIAN_POINT('Ctrl Pts',(146.168301620294,-5.90713908955371,334.998942939345));
#21954=CARTESIAN_POINT('',(147.918301620294,-5.91753216870106,334.994978908048));
#21955=CARTESIAN_POINT('Ctrl Pts',(146.168301669802,-5.91674990507826,334.998940162095));
#21956=CARTESIAN_POINT('Ctrl Pts',(146.176163441027,-5.91671982668063,334.831021695044));
#21957=CARTESIAN_POINT('Ctrl Pts',(146.184025212251,-5.9095371589622,334.663280561601));
#21958=CARTESIAN_POINT('Ctrl Pts',(146.191886983476,-5.89527254671868,334.496321369914));
#21959=CARTESIAN_POINT('Ctrl Pts',(146.19976273157,-5.88098257446191,334.329065353664));
#21960=CARTESIAN_POINT('Ctrl Pts',(146.207638479665,-5.85958553624748,334.162594350689));
#21961=CARTESIAN_POINT('Ctrl Pts',(146.215514227759,-5.83120336401502,333.997504169585));
#21962=CARTESIAN_POINT('Ctrl Pts',(146.223412142684,-5.80274130822188,333.831949330899));
#21963=CARTESIAN_POINT('Ctrl Pts',(146.231310057608,-5.76725484106339,333.667783381872));
#21964=CARTESIAN_POINT('Ctrl Pts',(146.239207972533,-5.72491673570582,333.50559077501));
#21965=CARTESIAN_POINT('Ctrl Pts',(146.24711774866,-5.68251504637494,333.343154584967));
#21966=CARTESIAN_POINT('Ctrl Pts',(146.255027524786,-5.63324125649986,333.182697938438));
#21967=CARTESIAN_POINT('Ctrl Pts',(146.262937300913,-5.5773170522976,333.024787337867));
#21968=CARTESIAN_POINT('Ctrl Pts',(146.270866048282,-5.52125871640332,332.866497995813));
#21969=CARTESIAN_POINT('Ctrl Pts',(146.278794795651,-5.45851817538879,332.710767188446));
#21970=CARTESIAN_POINT('Ctrl Pts',(146.286723543021,-5.38936493378601,332.558140836785));
#21971=CARTESIAN_POINT('Ctrl Pts',(146.290602425142,-5.35553395645441,332.483473351594));
#21972=CARTESIAN_POINT('Ctrl Pts',(146.294481307264,-5.3201688896589,332.409548469094));
#21973=CARTESIAN_POINT('Ctrl Pts',(146.298360189386,-5.28330512879898,332.336427684761));
#21974=CARTESIAN_POINT('Ctrl Pts',(146.305784166824,-5.2127498192254,332.196478329228));
#21975=CARTESIAN_POINT('Ctrl Pts',(146.313208144262,-5.13652356020408,332.059123196295));
#21976=CARTESIAN_POINT('Ctrl Pts',(146.3206321217,-5.0548405520916,331.92485487246));
#21977=CARTESIAN_POINT('Ctrl Pts',(146.328047337728,-4.97325394221863,331.79074500545));
#21978=CARTESIAN_POINT('Ctrl Pts',(146.335462553755,-4.8862235938338,331.659715012031));
#21979=CARTESIAN_POINT('Ctrl Pts',(146.342877769783,-4.79401078544132,331.532235424431));
#21980=CARTESIAN_POINT('Ctrl Pts',(146.350285850927,-4.70188670374885,331.404878497048));
#21981=CARTESIAN_POINT('Ctrl Pts',(146.357693932071,-4.60459030658873,331.281065474871));
#21982=CARTESIAN_POINT('Ctrl Pts',(146.365102013215,-4.50242753253622,331.161240190275));
#21983=CARTESIAN_POINT('Ctrl Pts',(146.372504580389,-4.40034080010215,331.041504093827));
#21984=CARTESIAN_POINT('Ctrl Pts',(146.379907147563,-4.29339514407098,330.925750107733));
#21985=CARTESIAN_POINT('Ctrl Pts',(146.387309714737,-4.18193828087265,330.814390990851));
#21986=CARTESIAN_POINT('Ctrl Pts',(146.394708384492,-4.07054009922543,330.703090504056));
#21987=CARTESIAN_POINT('Ctrl Pts',(146.402107054246,-3.95463570397611,330.596180541364));
#21988=CARTESIAN_POINT('Ctrl Pts',(146.409505724001,-3.83461127373347,330.494038732761));
#21989=CARTESIAN_POINT('Ctrl Pts',(146.416903173205,-3.71460664379512,330.391913774385));
#21990=CARTESIAN_POINT('Ctrl Pts',(146.424300622409,-3.59048361175089,330.294555650596));
#21991=CARTESIAN_POINT('Ctrl Pts',(146.431698071613,-3.46266328845441,330.202303311662));
#21992=CARTESIAN_POINT('Ctrl Pts',(146.439095200077,-3.33484850722429,330.110054972628));
#21993=CARTESIAN_POINT('Ctrl Pts',(146.44649232854,-3.20333705611192,330.022912196691));
#21994=CARTESIAN_POINT('Ctrl Pts',(146.453889457003,-3.06858080385524,329.94117183404));
#21995=CARTESIAN_POINT('Ctrl Pts',(146.46128772444,-2.93380380249963,329.859418885414));
#21996=CARTESIAN_POINT('Ctrl Pts',(146.468685991877,-2.79578132430925,329.783070199939));
#21997=CARTESIAN_POINT('Ctrl Pts',(146.476084259313,-2.65499158337609,329.712377636905));
#21998=CARTESIAN_POINT('Ctrl Pts',(146.483485125839,-2.51415238152651,329.64166023883));
#21999=CARTESIAN_POINT('Ctrl Pts',(146.490885992365,-2.37054431466596,329.576603086783));
#22000=CARTESIAN_POINT('Ctrl Pts',(146.49828685889,-2.22466725363737,329.517410632457));
#22001=CARTESIAN_POINT('Ctrl Pts',(146.505695852275,-2.07863000564912,329.458153179157));
#22002=CARTESIAN_POINT('Ctrl Pts',(146.51310484566,-1.93031913372141,329.404773425009));
#22003=CARTESIAN_POINT('Ctrl Pts',(146.520513839045,-1.78025210735936,329.357426739798));
#22004=CARTESIAN_POINT('Ctrl Pts',(146.527927396625,-1.63009263453265,329.310050887397));
#22005=CARTESIAN_POINT('Ctrl Pts',(146.535340954205,-1.47817521081658,329.268715607464));
#22006=CARTESIAN_POINT('Ctrl Pts',(146.542754511785,-1.32502878112974,329.233525401801));
#22007=CARTESIAN_POINT('Ctrl Pts',(146.550178623922,-1.17166431946315,329.198285096437));
#22008=CARTESIAN_POINT('Ctrl Pts',(146.557602736059,-1.01706772308561,329.169207406925));
#22009=CARTESIAN_POINT('Ctrl Pts',(146.565026848195,-0.861775175327489,
329.146345234839));
#22010=CARTESIAN_POINT('Ctrl Pts',(146.56888397335,-0.781094444583926,329.134467415994));
#22011=CARTESIAN_POINT('Ctrl Pts',(146.572741098505,-0.700225908248673,
329.124266444733));
#22012=CARTESIAN_POINT('Ctrl Pts',(146.57659822366,-0.619244776469927,329.115744187298));
#22013=CARTESIAN_POINT('Ctrl Pts',(146.584022201098,-0.463376851240116,
329.099341025779));
#22014=CARTESIAN_POINT('Ctrl Pts',(146.591446178536,-0.306621586995413,
329.08911056934));
#22015=CARTESIAN_POINT('Ctrl Pts',(146.598870155974,-0.14950912633372,329.08513925915));
#22016=CARTESIAN_POINT('Ctrl Pts',(146.606285372001,0.00741791798549277,
329.081172635704));
#22017=CARTESIAN_POINT('Ctrl Pts',(146.613700588029,0.16470095016472,329.083450464434));
#22018=CARTESIAN_POINT('Ctrl Pts',(146.621115804056,0.321802896826992,329.092007662658));
#22019=CARTESIAN_POINT('Ctrl Pts',(146.628523885201,0.47875368078709,329.100556627188));
#22020=CARTESIAN_POINT('Ctrl Pts',(146.635931966345,0.635523355940499,329.115372912598));
#22021=CARTESIAN_POINT('Ctrl Pts',(146.643340047489,0.791573133256018,329.136439431778));
#22022=CARTESIAN_POINT('Ctrl Pts',(146.650742614663,0.947506759872355,329.157490270763));
#22023=CARTESIAN_POINT('Ctrl Pts',(146.658145181837,1.10272118730054,329.184782030668));
#22024=CARTESIAN_POINT('Ctrl Pts',(146.665547749011,1.25668114849993,329.218245676829));
#22025=CARTESIAN_POINT('Ctrl Pts',(146.672946418765,1.41056005045274,329.251691704527));
#22026=CARTESIAN_POINT('Ctrl Pts',(146.68034508852,1.56318543776627,329.291303067899));
#22027=CARTESIAN_POINT('Ctrl Pts',(146.687743758275,1.71403076992517,329.336959378368));
#22028=CARTESIAN_POINT('Ctrl Pts',(146.695141207479,1.86485121728831,329.382608156964));
#22029=CARTESIAN_POINT('Ctrl Pts',(146.702538656683,2.01389183544407,329.434299795469));
#22030=CARTESIAN_POINT('Ctrl Pts',(146.709936105887,2.16063970663593,329.491863598221));
#22031=CARTESIAN_POINT('Ctrl Pts',(146.71733323435,2.30738121509588,329.549424905106));
#22032=CARTESIAN_POINT('Ctrl Pts',(146.724730362814,2.45182982681364,329.612857733709));
#22033=CARTESIAN_POINT('Ctrl Pts',(146.732127491277,2.59349138202934,329.681942740639));
#22034=CARTESIAN_POINT('Ctrl Pts',(146.739525758714,2.73517474958819,329.751038384936));
#22035=CARTESIAN_POINT('Ctrl Pts',(146.746924026151,2.87406987070856,329.82578777683));
#22036=CARTESIAN_POINT('Ctrl Pts',(146.754322293587,3.00970616245622,329.905925071402));
#22037=CARTESIAN_POINT('Ctrl Pts',(146.761723160113,3.14539010465955,329.986090519048));
#22038=CARTESIAN_POINT('Ctrl Pts',(146.769124026639,3.27781261695689,330.071647448264));
#22039=CARTESIAN_POINT('Ctrl Pts',(146.776524893164,3.40653126276212,330.162286147536));
#22040=CARTESIAN_POINT('Ctrl Pts',(146.783933886549,3.53539125394656,330.253024376765));
#22041=CARTESIAN_POINT('Ctrl Pts',(146.791342879934,3.66053895089339,330.348855305143));
#22042=CARTESIAN_POINT('Ctrl Pts',(146.798751873319,3.78156366739261,330.449427861031));
#22043=CARTESIAN_POINT('Ctrl Pts',(146.806165430899,3.90266293929173,330.550062373083));
#22044=CARTESIAN_POINT('Ctrl Pts',(146.813578988479,4.01963389302959,330.655444083913));
#22045=CARTESIAN_POINT('Ctrl Pts',(146.82099254606,4.1321024083657,330.765184744374));
#22046=CARTESIAN_POINT('Ctrl Pts',(146.828416658196,4.24473104322347,330.875081640757));
#22047=CARTESIAN_POINT('Ctrl Pts',(146.835840770333,4.35284418173045,330.989349610552));
#22048=CARTESIAN_POINT('Ctrl Pts',(146.84326488247,4.45610717825678,331.107566393837));
#22049=CARTESIAN_POINT('Ctrl Pts',(146.847122007624,4.50975646238894,331.168984772239));
#22050=CARTESIAN_POINT('Ctrl Pts',(146.850979132779,4.56209728199605,331.231468518815));
#22051=CARTESIAN_POINT('Ctrl Pts',(146.854836257934,4.61308736718765,331.294955397678));
#22052=CARTESIAN_POINT('Ctrl Pts',(146.862260235372,4.71123021369702,331.417151369389));
#22053=CARTESIAN_POINT('Ctrl Pts',(146.86968421281,4.80466249087155,331.543433928317));
#22054=CARTESIAN_POINT('Ctrl Pts',(146.877108190248,4.89302461790924,331.673404044517));
#22055=CARTESIAN_POINT('Ctrl Pts',(146.884523406275,4.98128246434223,331.803220776426));
#22056=CARTESIAN_POINT('Ctrl Pts',(146.891938622303,5.06448186317861,331.936716097499));
#22057=CARTESIAN_POINT('Ctrl Pts',(146.899353838331,5.1423028104795,332.073457267041));
#22058=CARTESIAN_POINT('Ctrl Pts',(146.906761919475,5.2200488788567,332.210066864918));
#22059=CARTESIAN_POINT('Ctrl Pts',(146.914170000619,5.29242661503159,332.349915771483));
#22060=CARTESIAN_POINT('Ctrl Pts',(146.921578081763,5.35915881825845,332.492541660728));
#22061=CARTESIAN_POINT('Ctrl Pts',(146.928980648937,5.4258413514877,332.63506139092));
#22062=CARTESIAN_POINT('Ctrl Pts',(146.936383216111,5.48688656122312,332.780353651584));
#22063=CARTESIAN_POINT('Ctrl Pts',(146.943785783285,5.54206283647608,332.92793096663));
#22064=CARTESIAN_POINT('Ctrl Pts',(146.95118445304,5.59721006166128,333.075430582865));
#22065=CARTESIAN_POINT('Ctrl Pts',(146.958583122794,5.64649437584844,333.225212508797));
#22066=CARTESIAN_POINT('Ctrl Pts',(146.965981792549,5.68973207507486,333.376768816106));
#22067=CARTESIAN_POINT('Ctrl Pts',(146.973379241753,5.73296264142352,333.528300121332));
#22068=CARTESIAN_POINT('Ctrl Pts',(146.980776690957,5.77014847024491,333.681604868442));
#22069=CARTESIAN_POINT('Ctrl Pts',(146.988174140161,5.80115553393411,333.836159360735));
#22070=CARTESIAN_POINT('Ctrl Pts',(146.995571268625,5.83216125321106,333.990707151814));
#22071=CARTESIAN_POINT('Ctrl Pts',(147.002968397088,5.85698866661858,334.146504214416));
#22072=CARTESIAN_POINT('Ctrl Pts',(147.010365525551,5.87555480649272,334.30301629976));
#22073=CARTESIAN_POINT('Ctrl Pts',(147.017763792988,5.89412380508894,334.459552484058));
#22074=CARTESIAN_POINT('Ctrl Pts',(147.025162060425,5.90642956657555,334.616803539679));
#22075=CARTESIAN_POINT('Ctrl Pts',(147.032560327861,5.91244098618906,334.774229879453));
#22076=CARTESIAN_POINT('Ctrl Pts',(147.039961194387,5.91845451767749,334.931711524756));
#22077=CARTESIAN_POINT('Ctrl Pts',(147.047362060913,5.91816929042905,335.089368204112));
#22078=CARTESIAN_POINT('Ctrl Pts',(147.054762927439,5.91160631963916,335.246660260485));
#22079=CARTESIAN_POINT('Ctrl Pts',(147.062171920823,5.9050361420799,335.404125038573));
#22080=CARTESIAN_POINT('Ctrl Pts',(147.069580914208,5.89217446973443,335.561224020968));
#22081=CARTESIAN_POINT('Ctrl Pts',(147.076989907593,5.87309428036108,335.717421867864));
#22082=CARTESIAN_POINT('Ctrl Pts',(147.084403465173,5.85400233693294,335.873715938022));
#22083=CARTESIAN_POINT('Ctrl Pts',(147.091817022753,5.82868430293561,336.029107399018));
#22084=CARTESIAN_POINT('Ctrl Pts',(147.099230580334,5.79726420742942,336.183071541268));
#22085=CARTESIAN_POINT('Ctrl Pts',(147.10665469247,5.76579937966508,336.337254879661));
#22086=CARTESIAN_POINT('Ctrl Pts',(147.114078804607,5.72821522884073,336.490006479475));
#22087=CARTESIAN_POINT('Ctrl Pts',(147.121502916744,5.68468574638215,336.640816420987));
#22088=CARTESIAN_POINT('Ctrl Pts',(147.125360041898,5.66207042771921,336.71916825731));
#22089=CARTESIAN_POINT('Ctrl Pts',(147.129217167053,5.63785113299624,336.796996309748));
#22090=CARTESIAN_POINT('Ctrl Pts',(147.133074292208,5.61205732303508,336.87423135324));
#22091=CARTESIAN_POINT('Ctrl Pts',(147.140498269646,5.56241084916839,337.022889018552));
#22092=CARTESIAN_POINT('Ctrl Pts',(147.147922247084,5.50677871756783,337.169796952446));
#22093=CARTESIAN_POINT('Ctrl Pts',(147.155346224522,5.44530189122188,337.314436837755));
#22094=CARTESIAN_POINT('Ctrl Pts',(147.162761440549,5.38389761678068,337.458906026237));
#22095=CARTESIAN_POINT('Ctrl Pts',(147.170176656577,5.31666252198309,337.601112153892));
#22096=CARTESIAN_POINT('Ctrl Pts',(147.177591872605,5.24378733521979,337.740551941761));
#22097=CARTESIAN_POINT('Ctrl Pts',(147.184999953749,5.17098226859426,337.879857561367));
#22098=CARTESIAN_POINT('Ctrl Pts',(147.192408034893,5.09254808559639,338.016401811699));
#22099=CARTESIAN_POINT('Ctrl Pts',(147.199816116037,5.00872355679883,338.149701397604));
#22100=CARTESIAN_POINT('Ctrl Pts',(147.207218683211,4.92496142012899,338.282901766193));
#22101=CARTESIAN_POINT('Ctrl Pts',(147.214621250385,4.83581712422319,338.412861964516));
#22102=CARTESIAN_POINT('Ctrl Pts',(147.222023817559,4.74157526013046,338.539123424666));
#22103=CARTESIAN_POINT('Ctrl Pts',(147.229422487314,4.64738301396727,338.665318408709));
#22104=CARTESIAN_POINT('Ctrl Pts',(147.236821157068,4.54809876733374,338.787818234551));
#22105=CARTESIAN_POINT('Ctrl Pts',(147.244219826823,4.44405023523495,338.906193552451));
#22106=CARTESIAN_POINT('Ctrl Pts',(147.251617276027,4.34001886791312,339.024549342099));
#22107=CARTESIAN_POINT('Ctrl Pts',(147.259014725231,4.23122502115273,339.138781694165));
#22108=CARTESIAN_POINT('Ctrl Pts',(147.266412174435,4.11803655265524,339.248494499643));
#22109=CARTESIAN_POINT('Ctrl Pts',(147.273809302899,4.00485299181242,339.358202548164));
#22110=CARTESIAN_POINT('Ctrl Pts',(147.281206431362,3.88727545607765,339.463391179976));
#22111=CARTESIAN_POINT('Ctrl Pts',(147.288603559826,3.76570830808351,339.563701513128));
#22112=CARTESIAN_POINT('Ctrl Pts',(147.296001827262,3.64412244178326,339.664027291568));
#22113=CARTESIAN_POINT('Ctrl Pts',(147.303400094699,3.51854602795255,339.759473038194));
#22114=CARTESIAN_POINT('Ctrl Pts',(147.310798362135,3.38941598438095,339.849720594769));
#22115=CARTESIAN_POINT('Ctrl Pts',(147.318199228661,3.26024057606695,339.939999856259));
#22116=CARTESIAN_POINT('Ctrl Pts',(147.325600095187,3.12750935810849,340.025077078118));
#22117=CARTESIAN_POINT('Ctrl Pts',(147.333000961713,2.9916875121479,340.104677893086));
#22118=CARTESIAN_POINT('Ctrl Pts',(147.340409955097,2.85571652081542,340.184366117358));
#22119=CARTESIAN_POINT('Ctrl Pts',(147.347818948482,2.71664844605113,340.258565736403));
#22120=CARTESIAN_POINT('Ctrl Pts',(147.355227941867,2.57497295897001,340.327048415687));
#22121=CARTESIAN_POINT('Ctrl Pts',(147.362641499447,2.4332101949019,340.395573282664));
#22122=CARTESIAN_POINT('Ctrl Pts',(147.370055057027,2.28883715927508,340.458374043644));
#22123=CARTESIAN_POINT('Ctrl Pts',(147.377468614608,2.14236221081269,340.515271046846));
#22124=CARTESIAN_POINT('Ctrl Pts',(147.384892726744,1.99567872844555,340.572249053349));
#22125=CARTESIAN_POINT('Ctrl Pts',(147.392316838881,1.84688770876028,340.623306394643));
#22126=CARTESIAN_POINT('Ctrl Pts',(147.399740951018,1.69651211087499,340.668313437007));
#22127=CARTESIAN_POINT('Ctrl Pts',(147.403598076172,1.61838593355299,340.691696407528));
#22128=CARTESIAN_POINT('Ctrl Pts',(147.407455201327,1.53983221379161,340.713447110847));
#22129=CARTESIAN_POINT('Ctrl Pts',(147.411312326482,1.46092510736363,340.733552859543));
#22130=CARTESIAN_POINT('Ctrl Pts',(147.41873630392,1.30904914940758,340.772251273183));
#22131=CARTESIAN_POINT('Ctrl Pts',(147.426160281358,1.15540539507283,340.804969339466));
#22132=CARTESIAN_POINT('Ctrl Pts',(147.433584258796,1.00050599148444,340.831545106016));
#22133=CARTESIAN_POINT('Ctrl Pts',(147.440999474823,0.845789392498042,340.858089509164));
#22134=CARTESIAN_POINT('Ctrl Pts',(147.448414690851,0.689820458173766,340.878505979011));
#22135=CARTESIAN_POINT('Ctrl Pts',(147.455829906879,0.533125620602867,340.892682550007));
#22136=CARTESIAN_POINT('Ctrl Pts',(147.463237988023,0.376581554015769,340.906845480377));
#22137=CARTESIAN_POINT('Ctrl Pts',(147.470646069167,0.219313343895595,340.914780431336));
#22138=CARTESIAN_POINT('Ctrl Pts',(147.478054150311,0.0618566159030756,
340.916426651415));
#22139=CARTESIAN_POINT('Ctrl Pts',(147.485456717485,-0.0954829141711237,
340.918071646181));
#22140=CARTESIAN_POINT('Ctrl Pts',(147.492859284659,-0.253010311133119,
340.913437226371));
#22141=CARTESIAN_POINT('Ctrl Pts',(147.500261851833,-0.410185946901329,
340.902514553262));
#22142=CARTESIAN_POINT('Ctrl Pts',(147.507660521588,-0.567278830384351,
340.891597630892));
#22143=CARTESIAN_POINT('Ctrl Pts',(147.515059191342,-0.724019950136165,
340.874399074563));
#22144=CARTESIAN_POINT('Ctrl Pts',(147.522457861097,-0.879870911407023,
340.850962121033));
#22145=CARTESIAN_POINT('Ctrl Pts',(147.529855310301,-1.03569616210859,340.827529033872));
#22146=CARTESIAN_POINT('Ctrl Pts',(147.537252759505,-1.19063117707332,340.797859647471));
#22147=CARTESIAN_POINT('Ctrl Pts',(147.544650208709,-1.34414379087642,340.762048943904));
#22148=CARTESIAN_POINT('Ctrl Pts',(147.552047337173,-1.49764974864022,340.726239793028));
#22149=CARTESIAN_POINT('Ctrl Pts',(147.559444465636,-1.6497330644151,340.684289939217));
#22150=CARTESIAN_POINT('Ctrl Pts',(147.5668415941,-1.79987312289148,340.636345208022));
#22151=CARTESIAN_POINT('Ctrl Pts',(147.574239861536,-1.95003629918897,340.588393094535));
#22152=CARTESIAN_POINT('Ctrl Pts',(147.581638128973,-2.09825526686946,340.534444379265));
#22153=CARTESIAN_POINT('Ctrl Pts',(147.589036396409,-2.24402603859688,340.474694302023));
#22154=CARTESIAN_POINT('Ctrl Pts',(147.596437262935,-2.38984802112968,340.41492323395));
#22155=CARTESIAN_POINT('Ctrl Pts',(147.603838129461,-2.53321975018744,340.34934688755));
#22156=CARTESIAN_POINT('Ctrl Pts',(147.611238995987,-2.67365876800804,340.278207968123));
#22157=CARTESIAN_POINT('Ctrl Pts',(147.618647989371,-2.81425200129645,340.206990931361));
#22158=CARTESIAN_POINT('Ctrl Pts',(147.626056982756,-2.95190575890977,340.130199291842));
#22159=CARTESIAN_POINT('Ctrl Pts',(147.633465976141,-3.08616304033104,340.048121259538));
#22160=CARTESIAN_POINT('Ctrl Pts',(147.640879533721,-3.22050302886869,339.965992664334));
#22161=CARTESIAN_POINT('Ctrl Pts',(147.648293091301,-3.3514420622727,339.878571393885));
#22162=CARTESIAN_POINT('Ctrl Pts',(147.655706648882,-3.47855396545394,339.786187717999));
#22163=CARTESIAN_POINT('Ctrl Pts',(147.663130761018,-3.60584683570027,339.693672517038));
#22164=CARTESIAN_POINT('Ctrl Pts',(147.670554873155,-3.72930140163319,339.59618103131));
#22165=CARTESIAN_POINT('Ctrl Pts',(147.677978985292,-3.84852564830608,339.494082876053));
#22166=CARTESIAN_POINT('Ctrl Pts',(147.681836110446,-3.91046744449855,339.441038773858));
#22167=CARTESIAN_POINT('Ctrl Pts',(147.685693235601,-3.97126800012368,339.386751828662));
#22168=CARTESIAN_POINT('Ctrl Pts',(147.689550360756,-4.0308765161159,339.331277533745));
#22169=CARTESIAN_POINT('Ctrl Pts',(147.696863948988,-4.14390166402496,339.226091382341));
#22170=CARTESIAN_POINT('Ctrl Pts',(147.70417753722,-4.25300172650221,339.116296409232));
#22171=CARTESIAN_POINT('Ctrl Pts',(147.711491125452,-4.35776915270144,339.002221704786));
#22172=CARTESIAN_POINT('Ctrl Pts',(147.718795981515,-4.46241149023985,338.888283201568));
#22173=CARTESIAN_POINT('Ctrl Pts',(147.726100837577,-4.56273122552003,338.77007541406));
#22174=CARTESIAN_POINT('Ctrl Pts',(147.73340569364,-4.65835459729738,338.647966969195));
#22175=CARTESIAN_POINT('Ctrl Pts',(147.740703533841,-4.75388612875338,338.525975801922));
#22176=CARTESIAN_POINT('Ctrl Pts',(147.748001374042,-4.84473003641664,338.400091733477));
#22177=CARTESIAN_POINT('Ctrl Pts',(147.755299214243,-4.93055029611225,338.270719238945));
#22178=CARTESIAN_POINT('Ctrl Pts',(147.762591395003,-5.01630400259889,338.141447072177));
#22179=CARTESIAN_POINT('Ctrl Pts',(147.769883575763,-5.09704160545529,338.008692185167));
#22180=CARTESIAN_POINT('Ctrl Pts',(147.777175756523,-5.17246839520712,337.872890750287));
#22181=CARTESIAN_POINT('Ctrl Pts',(147.784464896139,-5.24786372883292,337.737145950285));
#22182=CARTESIAN_POINT('Ctrl Pts',(147.791754035754,-5.3179524685946,337.598357465983));
#22183=CARTESIAN_POINT('Ctrl Pts',(147.79904317537,-5.38248419701184,337.456988895257));
#22184=CARTESIAN_POINT('Ctrl Pts',(147.806330812989,-5.44700262804597,337.315649454885));
#22185=CARTESIAN_POINT('Ctrl Pts',(147.813618450607,-5.50596616673139,337.171731336426));
#22186=CARTESIAN_POINT('Ctrl Pts',(147.820906088225,-5.55917132215087,337.025720803436));
#22187=CARTESIAN_POINT('Ctrl Pts',(147.828193761638,-5.61237673889338,336.8797095533));
#22188=CARTESIAN_POINT('Ctrl Pts',(147.83548143505,-5.65982358579274,336.731606230687));
#22189=CARTESIAN_POINT('Ctrl Pts',(147.842769108463,-5.70135740753455,336.581914749299));
#22190=CARTESIAN_POINT('Ctrl Pts',(147.85006117729,-5.74291627957087,336.432132984487));
#22191=CARTESIAN_POINT('Ctrl Pts',(147.857353246117,-5.77855490092662,336.280761519495));
#22192=CARTESIAN_POINT('Ctrl Pts',(147.864645314944,-5.80816929984917,336.128317307671));
#22193=CARTESIAN_POINT('Ctrl Pts',(147.871939876106,-5.83779382058973,335.975820992389));
#22194=CARTESIAN_POINT('Ctrl Pts',(147.879234437268,-5.86138995737384,335.822251580241));
#22195=CARTESIAN_POINT('Ctrl Pts',(147.886528998429,-5.87890541429882,335.668132989926));
#22196=CARTESIAN_POINT('Ctrl Pts',(147.893830941335,-5.8964385960224,335.513858439023));
#22197=CARTESIAN_POINT('Ctrl Pts',(147.901132884242,-5.90787878264885,335.359033983944));
#22198=CARTESIAN_POINT('Ctrl Pts',(147.908434827148,-5.91322574581222,335.204185801572));
#22199=CARTESIAN_POINT('Ctrl Pts',(147.911723758197,-5.9156341175826,335.134439296925));
#22200=CARTESIAN_POINT('Ctrl Pts',(147.915012689245,-5.91680701839214,335.064687952162));
#22201=CARTESIAN_POINT('Ctrl Pts',(147.918301620294,-5.9167478700565,334.994979573534));
#22202=CARTESIAN_POINT('',(149.668301620294,-5.92062882697594,335.003695392425));
#22203=CARTESIAN_POINT('Ctrl Pts',(147.918301620294,-5.92002000212284,334.994976797094));
#22204=CARTESIAN_POINT('Ctrl Pts',(147.934797211872,-5.92318185887226,334.645159030833));
#22205=CARTESIAN_POINT('Ctrl Pts',(148.044038814879,-5.735551808118,332.331887814483));
#22206=CARTESIAN_POINT('Ctrl Pts',(148.246026429301,-2.68677370757217,328.53982430846));
#22207=CARTESIAN_POINT('Ctrl Pts',(148.524264463577,3.97853214060743,329.244662918007));
#22208=CARTESIAN_POINT('Ctrl Pts',(148.80250249785,6.99279776638912,335.231089419058));
#22209=CARTESIAN_POINT('Ctrl Pts',(149.080740532125,3.58987609548163,341.005448571115));
#22210=CARTESIAN_POINT('Ctrl Pts',(149.358978566399,-3.10742188176739,341.268696209736));
#22211=CARTESIAN_POINT('Ctrl Pts',(149.554832262455,-5.81441077913725,337.404639393051));
#22212=CARTESIAN_POINT('Ctrl Pts',(149.657939947087,-5.92516035764709,335.223093199081));
#22213=CARTESIAN_POINT('Ctrl Pts',(149.668301620294,-5.92355705250644,335.003697220093));
#22214=CARTESIAN_POINT('',(151.4183015929,-5.9121545373304,335.003046556256));
#22215=CARTESIAN_POINT('Ctrl Pts',(149.668301620294,-5.91674884750632,335.003692970715));
#22216=CARTESIAN_POINT('Ctrl Pts',(149.67562186246,-5.91684547825825,334.848874551005));
#22217=CARTESIAN_POINT('Ctrl Pts',(149.682942104626,-5.91086145436701,334.693814183029));
#22218=CARTESIAN_POINT('Ctrl Pts',(149.690262346792,-5.89876627030689,334.53903682274));
#22219=CARTESIAN_POINT('Ctrl Pts',(149.697574904694,-5.88668378290076,334.384421936587));
#22220=CARTESIAN_POINT('Ctrl Pts',(149.704887462596,-5.86850292911253,334.230089846584));
#22221=CARTESIAN_POINT('Ctrl Pts',(149.712200020498,-5.84424520377401,334.076566970125));
#22222=CARTESIAN_POINT('Ctrl Pts',(149.719506597661,-5.82000731816153,333.923169655801));
#22223=CARTESIAN_POINT('Ctrl Pts',(149.726813174823,-5.78970251150662,333.7705806152));
#22224=CARTESIAN_POINT('Ctrl Pts',(149.734119751986,-5.75340418977252,333.619322343337));
#22225=CARTESIAN_POINT('Ctrl Pts',(149.741675372109,-5.7158686482948,333.462908468917));
#22226=CARTESIAN_POINT('Ctrl Pts',(149.749230992232,-5.67192379597278,333.307918107546));
#22227=CARTESIAN_POINT('Ctrl Pts',(149.756786612356,-5.62170869794327,333.15491954702));
#22228=CARTESIAN_POINT('Ctrl Pts',(149.764087191177,-5.57318861948603,333.007085480138));
#22229=CARTESIAN_POINT('Ctrl Pts',(149.771387769998,-5.51881485905228,332.861111323308));
#22230=CARTESIAN_POINT('Ctrl Pts',(149.778688348819,-5.45876389216768,332.717495381808));
#22231=CARTESIAN_POINT('Ctrl Pts',(149.785988453333,-5.3987168267073,332.573888770828));
#22232=CARTESIAN_POINT('Ctrl Pts',(149.793288557846,-5.33299343645006,332.432640424818));
#22233=CARTESIAN_POINT('Ctrl Pts',(149.800588662359,-5.26181845823944,332.294228931519));
#22234=CARTESIAN_POINT('Ctrl Pts',(149.807889823491,-5.190633178144,332.155797404504));
#22235=CARTESIAN_POINT('Ctrl Pts',(149.815190984623,-5.11399491584785,332.020203888682));
#22236=CARTESIAN_POINT('Ctrl Pts',(149.822492145756,-5.03217435700199,331.887902346771));
#22237=CARTESIAN_POINT('Ctrl Pts',(149.82979589504,-4.9503247939981,331.755553905953));
#22238=CARTESIAN_POINT('Ctrl Pts',(149.837099644324,-4.8632894812332,331.626500087206));
#22239=CARTESIAN_POINT('Ctrl Pts',(149.844403393608,-4.77138222962384,331.501165596755));
#22240=CARTESIAN_POINT('Ctrl Pts',(149.851714988852,-4.679376247809,331.375696467309));
#22241=CARTESIAN_POINT('Ctrl Pts',(149.859026584097,-4.58248810750462,331.25395495101));
#22242=CARTESIAN_POINT('Ctrl Pts',(149.866338179341,-4.48107199398705,331.136332785137));
#22243=CARTESIAN_POINT('Ctrl Pts',(149.873654464745,-4.37959082521267,331.018635168334));
#22244=CARTESIAN_POINT('Ctrl Pts',(149.880970750149,-4.27357616084882,330.905062443029));
#22245=CARTESIAN_POINT('Ctrl Pts',(149.888287035552,-4.1634181836864,330.795968650182));
#22246=CARTESIAN_POINT('Ctrl Pts',(149.895613120946,-4.05311265254148,330.686728728803));
#22247=CARTESIAN_POINT('Ctrl Pts',(149.902939206339,-3.93865301503498,330.581979969939));
#22248=CARTESIAN_POINT('Ctrl Pts',(149.910265291733,-3.82046190193295,330.482035699745));
#22249=CARTESIAN_POINT('Ctrl Pts',(149.911995072804,-3.79255549090281,330.458437598238));
#22250=CARTESIAN_POINT('Ctrl Pts',(149.913724853875,-3.76444117656519,330.435107150208));
#22251=CARTESIAN_POINT('Ctrl Pts',(149.915454634946,-3.73612474250915,330.412048118069));
#22252=CARTESIAN_POINT('Ctrl Pts',(149.922878612384,-3.61459458412496,330.313081990397));
#22253=CARTESIAN_POINT('Ctrl Pts',(149.930302589822,-3.48894610853022,330.218798716758));
#22254=CARTESIAN_POINT('Ctrl Pts',(149.93772656726,-3.3595759073391,330.12956056548));
#22255=CARTESIAN_POINT('Ctrl Pts',(149.945141783288,-3.23035838245033,330.040427728647));
#22256=CARTESIAN_POINT('Ctrl Pts',(149.952556999316,-3.0974281789271,329.956328372487));
#22257=CARTESIAN_POINT('Ctrl Pts',(149.959972215343,-2.96121586573633,329.877585417109));
#22258=CARTESIAN_POINT('Ctrl Pts',(149.967380296487,-2.82513461534728,329.798918227806));
#22259=CARTESIAN_POINT('Ctrl Pts',(149.974788377631,-2.68577786328597,329.725597364363));
#22260=CARTESIAN_POINT('Ctrl Pts',(149.982196458776,-2.54360605231989,329.657903144541));
#22261=CARTESIAN_POINT('Ctrl Pts',(149.98959902595,-2.40154006242959,329.590259310764));
#22262=CARTESIAN_POINT('Ctrl Pts',(149.997001593124,-2.25666352120201,329.528233941419));
#22263=CARTESIAN_POINT('Ctrl Pts',(150.004404160298,-2.10946232890685,329.472061935457));
#22264=CARTESIAN_POINT('Ctrl Pts',(150.011802830052,-1.96233863739557,329.415919503811));
#22265=CARTESIAN_POINT('Ctrl Pts',(150.019201499807,-1.81289308013125,329.365624430744));
#22266=CARTESIAN_POINT('Ctrl Pts',(150.026600169562,-1.66163233279155,329.321363847443));
#22267=CARTESIAN_POINT('Ctrl Pts',(150.033997618766,-1.51039653877853,329.277110565765));
#22268=CARTESIAN_POINT('Ctrl Pts',(150.04139506797,-1.35734650684511,329.23888990281));
#22269=CARTESIAN_POINT('Ctrl Pts',(150.048792517174,-1.20300501629026,329.206839421069));
#22270=CARTESIAN_POINT('Ctrl Pts',(150.056189645637,-1.04867021771348,329.174790328981));
#22271=CARTESIAN_POINT('Ctrl Pts',(150.063586774101,-0.89304443726818,329.148910962054));
#22272=CARTESIAN_POINT('Ctrl Pts',(150.070983902564,-0.736661351036444,
329.12928789529));
#22273=CARTESIAN_POINT('Ctrl Pts',(150.078382170001,-0.580254185713053,
329.109661807064));
#22274=CARTESIAN_POINT('Ctrl Pts',(150.085780437438,-0.423089852754835,
329.096293983554));
#22275=CARTESIAN_POINT('Ctrl Pts',(150.093178704874,-0.265707716882427,
329.089219174112));
#22276=CARTESIAN_POINT('Ctrl Pts',(150.1005795714,-0.1082702910109,329.082141879214));
#22277=CARTESIAN_POINT('Ctrl Pts',(150.107980437926,0.0493847175190642,
329.081362016835));
#22278=CARTESIAN_POINT('Ctrl Pts',(150.115381304451,0.206717522014393,329.086862218027));
#22279=CARTESIAN_POINT('Ctrl Pts',(150.122790297836,0.364223092970947,329.092368458966));
#22280=CARTESIAN_POINT('Ctrl Pts',(150.130199291221,0.521405380107819,329.104168522329));
#22281=CARTESIAN_POINT('Ctrl Pts',(150.137608284606,0.677728562820399,329.122193048625));
#22282=CARTESIAN_POINT('Ctrl Pts',(150.145021842186,0.834148046005747,329.14022867865));
#22283=CARTESIAN_POINT('Ctrl Pts',(150.152435399766,0.989707002300638,329.164496354932));
#22284=CARTESIAN_POINT('Ctrl Pts',(150.159848957346,1.14387989619223,329.194875596028));
#22285=CARTESIAN_POINT('Ctrl Pts',(150.167273069483,1.29827228342318,329.225298087536));
#22286=CARTESIAN_POINT('Ctrl Pts',(150.17469718162,1.45127430513113,329.261849434873));
#22287=CARTESIAN_POINT('Ctrl Pts',(150.182121293757,1.60237487779323,329.304359095456));
#22288=CARTESIAN_POINT('Ctrl Pts',(150.185978418911,1.68087770870112,329.326444575596));
#22289=CARTESIAN_POINT('Ctrl Pts',(150.189835544066,1.75886760367768,329.350137533726));
#22290=CARTESIAN_POINT('Ctrl Pts',(150.193692669221,1.83627514021165,329.375408977362));
#22291=CARTESIAN_POINT('Ctrl Pts',(150.201116646659,1.98526481042163,329.424050029921));
#22292=CARTESIAN_POINT('Ctrl Pts',(150.208540624097,2.13254522652256,329.478688424302));
#22293=CARTESIAN_POINT('Ctrl Pts',(150.215964601535,2.27759713087014,329.539186702335));
#22294=CARTESIAN_POINT('Ctrl Pts',(150.223379817562,2.42247785214635,329.599613583298));
#22295=CARTESIAN_POINT('Ctrl Pts',(150.23079503359,2.56513495558217,329.665886440144));
#22296=CARTESIAN_POINT('Ctrl Pts',(150.238210249618,2.70506388519565,329.737817948844));
#22297=CARTESIAN_POINT('Ctrl Pts',(150.245618330762,2.84485817589713,329.809680245408));
#22298=CARTESIAN_POINT('Ctrl Pts',(150.253026411906,2.98192918902718,329.887190184902));
#22299=CARTESIAN_POINT('Ctrl Pts',(150.26043449305,3.11579202739832,329.970112267207));
#22300=CARTESIAN_POINT('Ctrl Pts',(150.267837060224,3.24955522921416,330.052972629091));
#22301=CARTESIAN_POINT('Ctrl Pts',(150.275239627398,3.38011469502222,330.141236917048));
#22302=CARTESIAN_POINT('Ctrl Pts',(150.282642194572,3.50700994476609,330.234623644473));
#22303=CARTESIAN_POINT('Ctrl Pts',(150.290040864327,3.63383838471556,330.327961204195));
#22304=CARTESIAN_POINT('Ctrl Pts',(150.297439534081,3.75700615087568,330.426415611613));
#22305=CARTESIAN_POINT('Ctrl Pts',(150.304838203836,3.87608168935596,330.529662059761));
#22306=CARTESIAN_POINT('Ctrl Pts',(150.31223565304,3.9951375840701,330.632891475452));
#22307=CARTESIAN_POINT('Ctrl Pts',(150.319633102244,4.11010230923926,330.740911118658));
#22308=CARTESIAN_POINT('Ctrl Pts',(150.327030551448,4.22057727975467,330.85335581607));
#22309=CARTESIAN_POINT('Ctrl Pts',(150.334427679911,4.33104746026778,330.965795638076));
#22310=CARTESIAN_POINT('Ctrl Pts',(150.341824808375,4.43702801163296,331.082659866581));
#22311=CARTESIAN_POINT('Ctrl Pts',(150.349221936838,4.53815732833411,331.203546572683));
#22312=CARTESIAN_POINT('Ctrl Pts',(150.356620204275,4.63930221642586,331.32445189232));
#22313=CARTESIAN_POINT('Ctrl Pts',(150.364018471712,4.73559414305612,331.449380636512));
#22314=CARTESIAN_POINT('Ctrl Pts',(150.371416739148,4.8267120055567,331.577898046826));
#22315=CARTESIAN_POINT('Ctrl Pts',(150.378817605674,4.91786187872068,331.706460606658));
#22316=CARTESIAN_POINT('Ctrl Pts',(150.3862184722,5.00383385299093,331.838614038472));
#22317=CARTESIAN_POINT('Ctrl Pts',(150.393619338726,5.0843504247341,331.973895024787));
#22318=CARTESIAN_POINT('Ctrl Pts',(150.40102833211,5.16495541137057,332.109324562559));
#22319=CARTESIAN_POINT('Ctrl Pts',(150.408437325495,5.24009284103292,332.247888192523));
#22320=CARTESIAN_POINT('Ctrl Pts',(150.41584631888,5.3095310763227,332.3890977973));
#22321=CARTESIAN_POINT('Ctrl Pts',(150.42325987646,5.37901208796064,332.530394392065));
#22322=CARTESIAN_POINT('Ctrl Pts',(150.43067343404,5.4427867584689,332.674339869234));
#22323=CARTESIAN_POINT('Ctrl Pts',(150.438086991621,5.50067200584216,332.820427095359));
#22324=CARTESIAN_POINT('Ctrl Pts',(150.445511103757,5.55863966346232,332.966722303396));
#22325=CARTESIAN_POINT('Ctrl Pts',(150.452935215894,5.61070102889794,333.115164998965));
#22326=CARTESIAN_POINT('Ctrl Pts',(150.460359328031,5.65672293842651,333.265233110652));
#22327=CARTESIAN_POINT('Ctrl Pts',(150.464216453185,5.68063317329919,333.343199536514));
#22328=CARTESIAN_POINT('Ctrl Pts',(150.46807357834,5.70291406657114,333.421604522187));
#22329=CARTESIAN_POINT('Ctrl Pts',(150.471930703495,5.72355243013718,333.500373999302));
#22330=CARTESIAN_POINT('Ctrl Pts',(150.479354680933,5.76327599090508,333.651985056099));
#22331=CARTESIAN_POINT('Ctrl Pts',(150.486778658371,5.79703128351163,333.805404270438));
#22332=CARTESIAN_POINT('Ctrl Pts',(150.494202635809,5.82465289935838,333.960120600985));
#22333=CARTESIAN_POINT('Ctrl Pts',(150.501617851836,5.85224191754258,334.114654342983));
#22334=CARTESIAN_POINT('Ctrl Pts',(150.509033067864,5.8737116026831,334.270481790294));
#22335=CARTESIAN_POINT('Ctrl Pts',(150.516448283892,5.88894643536034,334.427077279245));
#22336=CARTESIAN_POINT('Ctrl Pts',(150.523856365036,5.90416660915828,334.583522092806));
#22337=CARTESIAN_POINT('Ctrl Pts',(150.53126444618,5.91316383777285,334.740733107809));
#22338=CARTESIAN_POINT('Ctrl Pts',(150.538672527324,5.91587375258846,334.898175121238));
#22339=CARTESIAN_POINT('Ctrl Pts',(150.546075094498,5.91858165036497,335.0554999477));
#22340=CARTESIAN_POINT('Ctrl Pts',(150.553477661672,5.91501154603593,335.213055058679));
#22341=CARTESIAN_POINT('Ctrl Pts',(150.560880228846,5.90515095550929,335.370300898119));
#22342=CARTESIAN_POINT('Ctrl Pts',(150.568278898601,5.89529555654051,335.527463948312));
#22343=CARTESIAN_POINT('Ctrl Pts',(150.575677568355,5.87915629054507,335.68431767971));
#22344=CARTESIAN_POINT('Ctrl Pts',(150.58307623811,5.85677275605526,335.840323417756));
#22345=CARTESIAN_POINT('Ctrl Pts',(150.590473687314,5.83439291415345,335.9963034197));
#22346=CARTESIAN_POINT('Ctrl Pts',(150.597871136518,5.80577090114714,336.151435336864));
#22347=CARTESIAN_POINT('Ctrl Pts',(150.605268585722,5.77099810178896,336.305186374296));
#22348=CARTESIAN_POINT('Ctrl Pts',(150.612665714185,5.73622681011875,336.458930745351));
#22349=CARTESIAN_POINT('Ctrl Pts',(150.620062842649,5.69530534468638,336.611293991702));
#22350=CARTESIAN_POINT('Ctrl Pts',(150.627459971112,5.64837601058656,336.761754524765));
#22351=CARTESIAN_POINT('Ctrl Pts',(150.634858238549,5.6014394505408,336.912238224994));
#22352=CARTESIAN_POINT('Ctrl Pts',(150.642256505986,5.54849329104085,337.060818272288));
#22353=CARTESIAN_POINT('Ctrl Pts',(150.649654773422,5.48972936265013,337.206989371827));
#22354=CARTESIAN_POINT('Ctrl Pts',(150.657055639948,5.43094478987323,337.353211822811));
#22355=CARTESIAN_POINT('Ctrl Pts',(150.664456506474,5.36633851803954,337.497023295023));
#22356=CARTESIAN_POINT('Ctrl Pts',(150.671857373,5.29614998756381,337.637939702064));
#22357=CARTESIAN_POINT('Ctrl Pts',(150.679266366384,5.22588438337137,337.779010848793));
#22358=CARTESIAN_POINT('Ctrl Pts',(150.686675359769,5.1500244453845,337.917180247335));
#22359=CARTESIAN_POINT('Ctrl Pts',(150.694084353154,5.0688552896325,338.051988960541));
#22360=CARTESIAN_POINT('Ctrl Pts',(150.701497910734,4.98763613088067,338.186880720564));
#22361=CARTESIAN_POINT('Ctrl Pts',(150.708911468314,4.90110144178917,338.318407358853));
#22362=CARTESIAN_POINT('Ctrl Pts',(150.716325025895,4.8095786055142,338.446140478837));
#22363=CARTESIAN_POINT('Ctrl Pts',(150.723749138031,4.7179254697265,338.574055450302));
#22364=CARTESIAN_POINT('Ctrl Pts',(150.731173250168,4.62127023225375,338.69816582339));
#22365=CARTESIAN_POINT('Ctrl Pts',(150.738597362305,4.51997985155643,338.818077095086));
#22366=CARTESIAN_POINT('Ctrl Pts',(150.742454487459,4.46735542076684,338.88037582844));
#22367=CARTESIAN_POINT('Ctrl Pts',(150.746311612614,4.41348046544508,338.941541743558));
#22368=CARTESIAN_POINT('Ctrl Pts',(150.750168737769,4.35841013442152,339.001523667639));
#22369=CARTESIAN_POINT('Ctrl Pts',(150.757592715207,4.25241386034981,339.116973499627));
#22370=CARTESIAN_POINT('Ctrl Pts',(150.765016692645,4.14166729566465,339.228382985388));
#22371=CARTESIAN_POINT('Ctrl Pts',(150.772440670083,4.02651067384282,339.335336475515));
#22372=CARTESIAN_POINT('Ctrl Pts',(150.77985588611,3.91148995416092,339.442163744431));
#22373=CARTESIAN_POINT('Ctrl Pts',(150.787271102138,3.79206980784507,339.544545233818));
#22374=CARTESIAN_POINT('Ctrl Pts',(150.794686318166,3.66862976250432,339.642099334156));
#22375=CARTESIAN_POINT('Ctrl Pts',(150.80209439931,3.5453084905537,339.739559568429));
#22376=CARTESIAN_POINT('Ctrl Pts',(150.809502480454,3.41797531075208,339.832201430903));
#22377=CARTESIAN_POINT('Ctrl Pts',(150.816910561598,3.28704545318422,339.919681163572));
#22378=CARTESIAN_POINT('Ctrl Pts',(150.824313128772,3.15621304910097,340.007095783477));
#22379=CARTESIAN_POINT('Ctrl Pts',(150.831715695946,3.02178960668352,340.089355717643));
#22380=CARTESIAN_POINT('Ctrl Pts',(150.83911826312,2.88422209427119,340.166158483188));
#22381=CARTESIAN_POINT('Ctrl Pts',(150.846516932874,2.74672701055279,340.242920812413));
#22382=CARTESIAN_POINT('Ctrl Pts',(150.853915602629,2.60609147859102,340.314231513647));
#22383=CARTESIAN_POINT('Ctrl Pts',(150.861314272384,2.46278991035233,340.379832378427));
#22384=CARTESIAN_POINT('Ctrl Pts',(150.868711721588,2.31951198242234,340.445422421101));
#22385=CARTESIAN_POINT('Ctrl Pts',(150.876109170792,2.17356923011666,340.505304341585));
#22386=CARTESIAN_POINT('Ctrl Pts',(150.883506619996,2.02545914561065,340.559266661347));
#22387=CARTESIAN_POINT('Ctrl Pts',(150.890903748459,1.87735548289982,340.613226641396));
#22388=CARTESIAN_POINT('Ctrl Pts',(150.898300876923,1.72708502549775,340.661267403295));
#22389=CARTESIAN_POINT('Ctrl Pts',(150.905698005386,1.57516339782496,340.703226352921));
#22390=CARTESIAN_POINT('Ctrl Pts',(150.913096272823,1.42321837801344,340.745191763178));
#22391=CARTESIAN_POINT('Ctrl Pts',(150.920494540259,1.26962204147258,340.78107339721));
#22392=CARTESIAN_POINT('Ctrl Pts',(150.927892807696,1.11490311192077,340.810759125409));
#22393=CARTESIAN_POINT('Ctrl Pts',(150.935293674222,0.960129827981612,340.840455282518));
#22394=CARTESIAN_POINT('Ctrl Pts',(150.942694540747,0.804233532118901,340.863951129733));
#22395=CARTESIAN_POINT('Ctrl Pts',(150.950095407273,0.647750877860981,340.881186050681));
#22396=CARTESIAN_POINT('Ctrl Pts',(150.957504400658,0.491096390688802,340.898439897221));
#22397=CARTESIAN_POINT('Ctrl Pts',(150.964913394043,0.333854630452807,340.909419046677));
#22398=CARTESIAN_POINT('Ctrl Pts',(150.972322387427,0.176565819838281,340.914114901975));
#22399=CARTESIAN_POINT('Ctrl Pts',(150.979735945008,0.0191801138904138,
340.918813650082));
#22400=CARTESIAN_POINT('Ctrl Pts',(150.987149502588,-0.138252327871474,
340.917221394864));
#22401=CARTESIAN_POINT('Ctrl Pts',(150.994563060168,-0.295194091819947,
340.909381609835));
#22402=CARTESIAN_POINT('Ctrl Pts',(151.001987172305,-0.452359291100679,
340.901530663436));
#22403=CARTESIAN_POINT('Ctrl Pts',(151.009411284441,-0.609032046681527,
340.887414456526));
#22404=CARTESIAN_POINT('Ctrl Pts',(151.016835396578,-0.76468203028186,340.867128084085));
#22405=CARTESIAN_POINT('Ctrl Pts',(151.020692521733,-0.845548463337213,
340.856588496859));
#22406=CARTESIAN_POINT('Ctrl Pts',(151.024549646888,-0.926139015950719,
340.844384283927));
#22407=CARTESIAN_POINT('Ctrl Pts',(151.028406772043,-1.00638081162408,340.830534128576));
#22408=CARTESIAN_POINT('Ctrl Pts',(151.035830749481,-1.16082570432244,340.803876128977));
#22409=CARTESIAN_POINT('Ctrl Pts',(151.043254726919,-1.3144436385046,340.771037045479));
#22410=CARTESIAN_POINT('Ctrl Pts',(151.050678704357,-1.46670096585834,340.732078055928));
#22411=CARTESIAN_POINT('Ctrl Pts',(151.058093920384,-1.61877860665737,340.693165043846));
#22412=CARTESIAN_POINT('Ctrl Pts',(151.065509136412,-1.76949847879413,340.648146593647));
#22413=CARTESIAN_POINT('Ctrl Pts',(151.072924352439,-1.91833429451591,340.597135347388));
#22414=CARTESIAN_POINT('Ctrl Pts',(151.080332433584,-2.06702690116564,340.546173183893));
#22415=CARTESIAN_POINT('Ctrl Pts',(151.087740514728,-2.21383870971484,340.489229824037));
#22416=CARTESIAN_POINT('Ctrl Pts',(151.095148595872,-2.35825594189839,340.426468416475));
#22417=CARTESIAN_POINT('Ctrl Pts',(151.102551163046,-2.50256568169828,340.363753723375));
#22418=CARTESIAN_POINT('Ctrl Pts',(151.10995373022,-2.64448405318538,340.295229753298));
#22419=CARTESIAN_POINT('Ctrl Pts',(151.117356297394,-2.78351481183673,340.221108680614));
#22420=CARTESIAN_POINT('Ctrl Pts',(151.124754967149,-2.92247237140334,340.14702663235));
#22421=CARTESIAN_POINT('Ctrl Pts',(151.132153636904,-3.05854501742987,340.067353525439));
#22422=CARTESIAN_POINT('Ctrl Pts',(151.139552306658,-3.19125888537502,339.982348571609));
#22423=CARTESIAN_POINT('Ctrl Pts',(151.146949755862,-3.32395085965103,339.897357640959));
#22424=CARTESIAN_POINT('Ctrl Pts',(151.154347205066,-3.4532848415771,339.80703681019));
#22425=CARTESIAN_POINT('Ctrl Pts',(151.16174465427,-3.57881377278148,339.711689987918));
#22426=CARTESIAN_POINT('Ctrl Pts',(151.169141782734,-3.70433726127045,339.616347299719));
#22427=CARTESIAN_POINT('Ctrl Pts',(151.176538911197,-3.82605572987341,339.51597927905));
#22428=CARTESIAN_POINT('Ctrl Pts',(151.183936039661,-3.94355341576413,339.41093153648));
#22429=CARTESIAN_POINT('Ctrl Pts',(151.191334307098,-4.06106919336495,339.30586761918));
#22430=CARTESIAN_POINT('Ctrl Pts',(151.198732574534,-4.17436261598112,339.196122794011));
#22431=CARTESIAN_POINT('Ctrl Pts',(151.206130841971,-4.28305326869173,339.082080996263));
#22432=CARTESIAN_POINT('Ctrl Pts',(151.213531708496,-4.39178210557177,338.967999134431));
#22433=CARTESIAN_POINT('Ctrl Pts',(151.220932575022,-4.49590469577555,338.849617564458));
#22434=CARTESIAN_POINT('Ctrl Pts',(151.228333441548,-4.59507965168306,338.727354766747));
#22435=CARTESIAN_POINT('Ctrl Pts',(151.235742434933,-4.69436351117357,338.604957712794));
#22436=CARTESIAN_POINT('Ctrl Pts',(151.243151428318,-4.78868865117479,338.47867120976));
#22437=CARTESIAN_POINT('Ctrl Pts',(151.250560421702,-4.87775549673004,338.348944890054));
#22438=CARTESIAN_POINT('Ctrl Pts',(151.257973979282,-4.9668772105343,338.219138654461));
#22439=CARTESIAN_POINT('Ctrl Pts',(151.265387536863,-5.05073397686028,338.085888694848));
#22440=CARTESIAN_POINT('Ctrl Pts',(151.272801094443,-5.12907152816297,337.949670459812));
#22441=CARTESIAN_POINT('Ctrl Pts',(151.28022520658,-5.20752060731175,337.81325829318));
#22442=CARTESIAN_POINT('Ctrl Pts',(151.287649318716,-5.28043460569062,337.673869740998));
#22443=CARTESIAN_POINT('Ctrl Pts',(151.295073430853,-5.34760649963432,337.532002228982));
#22444=CARTESIAN_POINT('Ctrl Pts',(151.298930556008,-5.38250500292219,337.458296344811));
#22445=CARTESIAN_POINT('Ctrl Pts',(151.302787681162,-5.41585439220377,337.383921629904));
#22446=CARTESIAN_POINT('Ctrl Pts',(151.306644806317,-5.44763094099968,337.308949478261));
#22447=CARTESIAN_POINT('Ctrl Pts',(151.314899635015,-5.51563754084358,337.148497783242));
#22448=CARTESIAN_POINT('Ctrl Pts',(151.323154463714,-5.57661208907137,336.984896632829));
#22449=CARTESIAN_POINT('Ctrl Pts',(151.331409292412,-5.63028344227576,336.818746524982));
#22450=CARTESIAN_POINT('Ctrl Pts',(151.339630362242,-5.68373530162608,336.653275903032));
#22451=CARTESIAN_POINT('Ctrl Pts',(151.347851432071,-5.72994346593964,336.485277332685));
#22452=CARTESIAN_POINT('Ctrl Pts',(151.356072501901,-5.76868604797543,336.31536756931));
#22453=CARTESIAN_POINT('Ctrl Pts',(151.364271623208,-5.80732519548824,336.145911429169));
#22454=CARTESIAN_POINT('Ctrl Pts',(151.372470744515,-5.83853845578075,335.974554492344));
#22455=CARTESIAN_POINT('Ctrl Pts',(151.380669865822,-5.86215321702131,335.801929063363));
#22456=CARTESIAN_POINT('Ctrl Pts',(151.388833272724,-5.8856651151465,335.630055570395));
#22457=CARTESIAN_POINT('Ctrl Pts',(151.396996679625,-5.90164447442005,335.456924828824));
#22458=CARTESIAN_POINT('Ctrl Pts',(151.405160086527,-5.90996960527333,335.283178083978));
#22459=CARTESIAN_POINT('Ctrl Pts',(151.409540577134,-5.91443687708099,335.189945443122));
#22460=CARTESIAN_POINT('Ctrl Pts',(151.413921067741,-5.91670102869276,335.096535704654));
#22461=CARTESIAN_POINT('Ctrl Pts',(151.418301558348,-5.91674921405907,335.003049660855));
#22462=CARTESIAN_POINT('',(153.168301655484,-5.91514362196022,334.995017318901));
#22463=CARTESIAN_POINT('Ctrl Pts',(151.418301620294,-5.90851180222765,335.003044094879));
#22464=CARTESIAN_POINT('Ctrl Pts',(151.473828693726,-5.90301154998691,333.819662210617));
#22465=CARTESIAN_POINT('Ctrl Pts',(151.622101778582,-4.98404225688584,330.651831516879));
#22466=CARTESIAN_POINT('Ctrl Pts',(151.863120874865,0.183842817904274,328.005800636274));
#22467=CARTESIAN_POINT('Ctrl Pts',(152.141358909138,5.98105935732207,331.369634744905));
#22468=CARTESIAN_POINT('Ctrl Pts',(152.419596943413,6.2895460048169,338.06500146403));
#22469=CARTESIAN_POINT('Ctrl Pts',(152.697834977687,0.826209117236143,341.947661578966));
#22470=CARTESIAN_POINT('Ctrl Pts',(152.947403203314,-4.75425691722228,339.711446338383));
#22471=CARTESIAN_POINT('Ctrl Pts',(153.104225417516,-5.90156738596128,336.358344737351));
#22472=CARTESIAN_POINT('Ctrl Pts',(153.168301620294,-5.91239802015065,334.995020380605));
#22473=CARTESIAN_POINT('',(154.918301620294,-5.92100069945767,334.999282630589));
#22474=CARTESIAN_POINT('Ctrl Pts',(153.168301676046,-5.91674790045664,334.995015529921));
#22475=CARTESIAN_POINT('Ctrl Pts',(153.177127639827,-5.91658958741957,334.807092177029));
#22476=CARTESIAN_POINT('Ctrl Pts',(153.185953603608,-5.90747449529418,334.6195553215));
#22477=CARTESIAN_POINT('Ctrl Pts',(153.194779567389,-5.88953568797227,334.433166741801));
#22478=CARTESIAN_POINT('Ctrl Pts',(153.203671549467,-5.87146269819447,334.245383973685));
#22479=CARTESIAN_POINT('Ctrl Pts',(153.212563531544,-5.84443359370318,334.058766748309));
#22480=CARTESIAN_POINT('Ctrl Pts',(153.221455513621,-5.80863311473178,333.874072870501));
#22481=CARTESIAN_POINT('Ctrl Pts',(153.230419364663,-5.77254328032391,333.687886214407));
#22482=CARTESIAN_POINT('Ctrl Pts',(153.239383215705,-5.72753976335944,333.503654142379));
#22483=CARTESIAN_POINT('Ctrl Pts',(153.248347066747,-5.67385995749029,333.322131189488));
#22484=CARTESIAN_POINT('Ctrl Pts',(153.250335059909,-5.66195490836465,333.281873225872));
#22485=CARTESIAN_POINT('Ctrl Pts',(153.252323053071,-5.64962329295002,333.241748427726));
#22486=CARTESIAN_POINT('Ctrl Pts',(153.254311046233,-5.63686801497755,333.201764880717));
#22487=CARTESIAN_POINT('Ctrl Pts',(153.261735023671,-5.58923460371215,333.052450005522));
#22488=CARTESIAN_POINT('Ctrl Pts',(153.269159001109,-5.53559244025597,332.904803829118));
#22489=CARTESIAN_POINT('Ctrl Pts',(153.276582978547,-5.47607547168731,332.759346525925));
#22490=CARTESIAN_POINT('Ctrl Pts',(153.283998194575,-5.41662874209636,332.614060884235));
#22491=CARTESIAN_POINT('Ctrl Pts',(153.291413410602,-5.35132114790566,332.470959315914));
#22492=CARTESIAN_POINT('Ctrl Pts',(153.29882862663,-5.2803366002361,332.330547630935));
#22493=CARTESIAN_POINT('Ctrl Pts',(153.306236707774,-5.20942035354087,332.190271049372));
#22494=CARTESIAN_POINT('Ctrl Pts',(153.313644788918,-5.13283819511548,332.052679529387));
#22495=CARTESIAN_POINT('Ctrl Pts',(153.321052870062,-5.05082234388107,331.918259548072));
#22496=CARTESIAN_POINT('Ctrl Pts',(153.328455437236,-4.96886753854256,331.783939618003));
#22497=CARTESIAN_POINT('Ctrl Pts',(153.33585800441,-4.88148728693261,331.652786843465));
#22498=CARTESIAN_POINT('Ctrl Pts',(153.343260571584,-4.78895995835898,331.525263595647));
#22499=CARTESIAN_POINT('Ctrl Pts',(153.350659241339,-4.69648134501969,331.397807488263));
#22500=CARTESIAN_POINT('Ctrl Pts',(153.358057911093,-4.59886127029452,331.273977403181));
#22501=CARTESIAN_POINT('Ctrl Pts',(153.365456580848,-4.49642161828097,331.154207078748));
#22502=CARTESIAN_POINT('Ctrl Pts',(153.372854030052,-4.39399886562891,331.034456512698));
#22503=CARTESIAN_POINT('Ctrl Pts',(153.380251479256,-4.28675835601205,330.918764661436));
#22504=CARTESIAN_POINT('Ctrl Pts',(153.38764892846,-4.17506256167947,330.807532567978));
#22505=CARTESIAN_POINT('Ctrl Pts',(153.395046056924,-4.06337161028184,330.696305297351));
#22506=CARTESIAN_POINT('Ctrl Pts',(153.402443185387,-3.9472260227094,330.589537663401));
#22507=CARTESIAN_POINT('Ctrl Pts',(153.409840313851,-3.82702527578928,330.48759397871));
#22508=CARTESIAN_POINT('Ctrl Pts',(153.417238581287,-3.70680602095469,330.385634597237));
#22509=CARTESIAN_POINT('Ctrl Pts',(153.424636848724,-3.58253064816983,330.288500885382));
#22510=CARTESIAN_POINT('Ctrl Pts',(153.432035116161,-3.45463173667,330.19651687559));
#22511=CARTESIAN_POINT('Ctrl Pts',(153.439435982686,-3.32668789293758,330.104500550848));
#22512=CARTESIAN_POINT('Ctrl Pts',(153.446836849212,-3.19511827877351,330.017637747942));
#22513=CARTESIAN_POINT('Ctrl Pts',(153.454237715738,-3.06038432635086,329.936209094213));
#22514=CARTESIAN_POINT('Ctrl Pts',(153.461646709123,-2.92550242316721,329.854691024038));
#22515=CARTESIAN_POINT('Ctrl Pts',(153.469055702508,-2.7874495620714,329.778619213042));
#22516=CARTESIAN_POINT('Ctrl Pts',(153.476464695892,-2.64671228442733,329.70822859092));
#22517=CARTESIAN_POINT('Ctrl Pts',(153.483878253473,-2.50588830776578,329.637794605745));
#22518=CARTESIAN_POINT('Ctrl Pts',(153.491291811053,-2.36237695875122,329.573048936395));
#22519=CARTESIAN_POINT('Ctrl Pts',(153.498705368633,-2.21668412240818,329.514178086744));
#22520=CARTESIAN_POINT('Ctrl Pts',(153.50612948077,-2.07078386564008,329.45522342366));
#22521=CARTESIAN_POINT('Ctrl Pts',(153.513553592907,-1.92269626913605,329.402160410171));
#22522=CARTESIAN_POINT('Ctrl Pts',(153.520977705043,-1.77294249278271,329.355125733926));
#22523=CARTESIAN_POINT('Ctrl Pts',(153.524834830198,-1.69513937677696,329.330689325968));
#22524=CARTESIAN_POINT('Ctrl Pts',(153.528691955353,-1.61688670360662,329.307879259645));
#22525=CARTESIAN_POINT('Ctrl Pts',(153.532549080508,-1.5382584508544,329.286709223147));
#22526=CARTESIAN_POINT('Ctrl Pts',(153.539973057946,-1.38691921476956,329.245962328241));
#22527=CARTESIAN_POINT('Ctrl Pts',(153.547397035384,-1.23373154250453,329.211171349908));
#22528=CARTESIAN_POINT('Ctrl Pts',(153.554821012822,-1.07920534627867,329.18250514542));
#22529=CARTESIAN_POINT('Ctrl Pts',(153.56223622885,-0.924861514214024,329.153872771367));
#22530=CARTESIAN_POINT('Ctrl Pts',(153.569651444877,-0.769182665908337,
329.131350850813));
#22531=CARTESIAN_POINT('Ctrl Pts',(153.577066660905,-0.612693672621006,
329.115058451775));
#22532=CARTESIAN_POINT('Ctrl Pts',(153.584474742049,-0.45635525225506,329.0987817292));
#22533=CARTESIAN_POINT('Ctrl Pts',(153.591882823193,-0.299208607505325,
329.088722633565));
#22534=CARTESIAN_POINT('Ctrl Pts',(153.599290904337,-0.14178849432088,329.084949147693));
#22535=CARTESIAN_POINT('Ctrl Pts',(153.606693471511,0.0155144481982303,
329.081178470495));
#22536=CARTESIAN_POINT('Ctrl Pts',(153.614096038685,0.173090082353266,329.083684096403));
#22537=CARTESIAN_POINT('Ctrl Pts',(153.621498605859,0.33039894874051,329.092482154308));
#22538=CARTESIAN_POINT('Ctrl Pts',(153.628897275614,0.487624992697058,329.101275580074));
#22539=CARTESIAN_POINT('Ctrl Pts',(153.636295945369,0.644584176913965,329.116354819137));
#22540=CARTESIAN_POINT('Ctrl Pts',(153.643694615124,0.80073757160893,329.137683912999));
#22541=CARTESIAN_POINT('Ctrl Pts',(153.651092064327,0.956865205842703,329.159009488222));
#22542=CARTESIAN_POINT('Ctrl Pts',(153.658489513531,1.11218694495993,329.18658282152));
#22543=CARTESIAN_POINT('Ctrl Pts',(153.665886962735,1.26616938879767,329.220316129634));
#22544=CARTESIAN_POINT('Ctrl Pts',(153.673284091199,1.42014515622504,329.25404797513));
#22545=CARTESIAN_POINT('Ctrl Pts',(153.680681219662,1.57278137926868,329.293939184522));
#22546=CARTESIAN_POINT('Ctrl Pts',(153.688078348126,1.72355551987454,329.339850979664));
#22547=CARTESIAN_POINT('Ctrl Pts',(153.695476615562,1.87435287593434,329.385769844077));
#22548=CARTESIAN_POINT('Ctrl Pts',(153.702874882999,2.02328722162326,329.437711031335));
#22549=CARTESIAN_POINT('Ctrl Pts',(153.710273150435,2.16985197770115,329.495486128879));
#22550=CARTESIAN_POINT('Ctrl Pts',(153.717674016961,2.31646822351918,329.553281523422));
#22551=CARTESIAN_POINT('Ctrl Pts',(153.725074883487,2.46071287530637,329.616914772049));
#22552=CARTESIAN_POINT('Ctrl Pts',(153.732475750013,2.60210024011964,329.686149710157));
#22553=CARTESIAN_POINT('Ctrl Pts',(153.739884743397,2.74364286177669,329.755460674845));
#22554=CARTESIAN_POINT('Ctrl Pts',(153.747293736782,2.88232159517437,329.83038544904));
#22555=CARTESIAN_POINT('Ctrl Pts',(153.754702730167,3.01767558747218,329.910642023666));
#22556=CARTESIAN_POINT('Ctrl Pts',(153.762116287747,3.15311296249817,329.99094803911));
#22557=CARTESIAN_POINT('Ctrl Pts',(153.769529845327,3.28522120277456,330.076592197386));
#22558=CARTESIAN_POINT('Ctrl Pts',(153.776943402907,3.41356970979961,330.167250016933));
#22559=CARTESIAN_POINT('Ctrl Pts',(153.784367515044,3.54210094442163,330.258036904482));
#22560=CARTESIAN_POINT('Ctrl Pts',(153.791791627181,3.66686146024687,330.35385148234));
#22561=CARTESIAN_POINT('Ctrl Pts',(153.799215739317,3.78745428419734,330.454329465567));
#22562=CARTESIAN_POINT('Ctrl Pts',(153.803072864472,3.85010711138703,330.506531823164));
#22563=CARTESIAN_POINT('Ctrl Pts',(153.806929989627,3.91163559437647,330.55999232975));
#22564=CARTESIAN_POINT('Ctrl Pts',(153.810787114781,3.97198818896083,330.614656183461));
#22565=CARTESIAN_POINT('Ctrl Pts',(153.818211092219,4.08815146667361,330.719870092876));
#22566=CARTESIAN_POINT('Ctrl Pts',(153.825635069657,4.20030658195626,330.829861479918));
#22567=CARTESIAN_POINT('Ctrl Pts',(153.833059047095,4.30803559636577,330.944292926881));
#22568=CARTESIAN_POINT('Ctrl Pts',(153.840474263123,4.41563747432958,331.05858932752));
#22569=CARTESIAN_POINT('Ctrl Pts',(153.847889479151,4.51882339547609,331.177315088804));
#22570=CARTESIAN_POINT('Ctrl Pts',(153.855304695178,4.61720919501505,331.300093269828));
#22571=CARTESIAN_POINT('Ctrl Pts',(153.862712776322,4.71550032823311,331.422753314305));
#22572=CARTESIAN_POINT('Ctrl Pts',(153.870120857467,4.8090003029009,331.549457726613));
#22573=CARTESIAN_POINT('Ctrl Pts',(153.877528938611,4.89736256368294,331.679793608473));
#22574=CARTESIAN_POINT('Ctrl Pts',(153.884931505785,4.98565905482044,331.810032478956));
#22575=CARTESIAN_POINT('Ctrl Pts',(153.892334072959,5.06882523786897,331.943897129397));
#22576=CARTESIAN_POINT('Ctrl Pts',(153.899736640133,5.14655561726123,332.080942645144));
#22577=CARTESIAN_POINT('Ctrl Pts',(153.907135309888,5.22424507194852,332.217916007027));
#22578=CARTESIAN_POINT('Ctrl Pts',(153.914533979642,5.29650423901483,332.358066575116));
#22579=CARTESIAN_POINT('Ctrl Pts',(153.921932649397,5.36307171089967,332.500921692654));
#22580=CARTESIAN_POINT('Ctrl Pts',(153.929330098601,5.42962820121868,332.643753243533));
#22581=CARTESIAN_POINT('Ctrl Pts',(153.936727547805,5.49049470239322,332.789288120406));
#22582=CARTESIAN_POINT('Ctrl Pts',(153.944124997009,5.54545637980306,332.937030271138));
#22583=CARTESIAN_POINT('Ctrl Pts',(153.951522125473,5.60041567417038,333.084766016028));
#22584=CARTESIAN_POINT('Ctrl Pts',(153.958919253936,5.6494705237047,333.234708494695));
#22585=CARTESIAN_POINT('Ctrl Pts',(153.9663163824,5.69245485458461,333.386343192926));
#22586=CARTESIAN_POINT('Ctrl Pts',(153.973714649836,5.73544580397847,333.538001239115));
#22587=CARTESIAN_POINT('Ctrl Pts',(153.981112917273,5.77236427179964,333.69135166459));
#22588=CARTESIAN_POINT('Ctrl Pts',(153.988511184709,5.80309455909471,333.845866515214));
#22589=CARTESIAN_POINT('Ctrl Pts',(153.995912051235,5.83383564226289,334.000435648529));
#22590=CARTESIAN_POINT('Ctrl Pts',(154.003312917761,5.85838414377514,334.156169655649));
#22591=CARTESIAN_POINT('Ctrl Pts',(154.010713784287,5.8766758231634,334.312532304798));
#22592=CARTESIAN_POINT('Ctrl Pts',(154.018122777672,5.89498758856439,334.469066655084));
#22593=CARTESIAN_POINT('Ctrl Pts',(154.025531771056,5.90702876751917,334.626230655079));
#22594=CARTESIAN_POINT('Ctrl Pts',(154.032940764441,5.91278711356018,334.783484152505));
#22595=CARTESIAN_POINT('Ctrl Pts',(154.040354322021,5.91854900694098,334.940834523509));
#22596=CARTESIAN_POINT('Ctrl Pts',(154.047767879602,5.91802035629129,335.098274129467));
#22597=CARTESIAN_POINT('Ctrl Pts',(154.055181437182,5.91124100352163,335.255265275321));
#22598=CARTESIAN_POINT('Ctrl Pts',(154.062605549319,5.90445199910218,335.412479926812));
#22599=CARTESIAN_POINT('Ctrl Pts',(154.070029661455,5.89139455033729,335.569244472136));
#22600=CARTESIAN_POINT('Ctrl Pts',(154.077453773592,5.87216016729201,335.725027952681));
#22601=CARTESIAN_POINT('Ctrl Pts',(154.081310898747,5.86216713091127,335.805963742768));
#22602=CARTESIAN_POINT('Ctrl Pts',(154.085168023901,5.85050764304288,335.88663490444));
#22603=CARTESIAN_POINT('Ctrl Pts',(154.089025149056,5.83719989421586,335.966968436644));
#22604=CARTESIAN_POINT('Ctrl Pts',(154.096449126494,5.81158588816656,336.121589898665));
#22605=CARTESIAN_POINT('Ctrl Pts',(154.103873103932,5.7797853525786,336.275426178662));
#22606=CARTESIAN_POINT('Ctrl Pts',(154.11129708137,5.74185585872572,336.427943227204));
#22607=CARTESIAN_POINT('Ctrl Pts',(154.118712297397,5.70397112738237,336.58028028268));
#22608=CARTESIAN_POINT('Ctrl Pts',(154.126127513425,5.65997192455523,336.731300847061));
#22609=CARTESIAN_POINT('Ctrl Pts',(154.133542729453,5.60996733428095,336.880477883624));
#22610=CARTESIAN_POINT('Ctrl Pts',(154.140950810597,5.56001085817168,337.029511382795));
#22611=CARTESIAN_POINT('Ctrl Pts',(154.148358891741,5.50406061606234,337.176704534024));
#22612=CARTESIAN_POINT('Ctrl Pts',(154.155766972885,5.44227628194723,337.321542468587));
#22613=CARTESIAN_POINT('Ctrl Pts',(154.163169540059,5.38053793504038,337.46627259763));
#22614=CARTESIAN_POINT('Ctrl Pts',(154.170572107233,5.31297428832971,337.608650658734));
#22615=CARTESIAN_POINT('Ctrl Pts',(154.177974674407,5.23979415885737,337.748178985311));
#22616=CARTESIAN_POINT('Ctrl Pts',(154.185373344162,5.1666525584033,337.887633850833));
#22617=CARTESIAN_POINT('Ctrl Pts',(154.192772013916,5.08790053724582,338.024241640232));
#22618=CARTESIAN_POINT('Ctrl Pts',(154.200170683671,5.00379409990611,338.157526748619));
#22619=CARTESIAN_POINT('Ctrl Pts',(154.207568132875,4.91970153751694,338.290789869102));
#22620=CARTESIAN_POINT('Ctrl Pts',(154.214965582079,4.83025651100921,338.420731081134));
#22621=CARTESIAN_POINT('Ctrl Pts',(154.222363031283,4.73575990186539,338.546901283428));
#22622=CARTESIAN_POINT('Ctrl Pts',(154.229760159746,4.64126738992983,338.673066015202));
#22623=CARTESIAN_POINT('Ctrl Pts',(154.23715728821,4.54172395458583,338.795459763619));
#22624=CARTESIAN_POINT('Ctrl Pts',(154.244554416673,4.43747238973926,338.913664440496));
#22625=CARTESIAN_POINT('Ctrl Pts',(154.25195268411,4.33320477275411,339.031887317942));
#22626=CARTESIAN_POINT('Ctrl Pts',(154.259350951546,4.22422782970407,339.145919559624));
#22627=CARTESIAN_POINT('Ctrl Pts',(154.266749218983,4.1109229171443,339.255378165545));
#22628=CARTESIAN_POINT('Ctrl Pts',(154.274150085509,3.99757819937722,339.364875225425));
#22629=CARTESIAN_POINT('Ctrl Pts',(154.281550952035,3.87990275311245,339.469795191334));
#22630=CARTESIAN_POINT('Ctrl Pts',(154.28895181856,3.75831274288632,339.569793856309));
#22631=CARTESIAN_POINT('Ctrl Pts',(154.296360811945,3.63658921520443,339.669902329378));
#22632=CARTESIAN_POINT('Ctrl Pts',(154.30376980533,3.5109428275175,339.765078472114));
#22633=CARTESIAN_POINT('Ctrl Pts',(154.311178798714,3.38182117813344,339.85501967881));
#22634=CARTESIAN_POINT('Ctrl Pts',(154.318592356295,3.2526199853595,339.945016292391));
#22635=CARTESIAN_POINT('Ctrl Pts',(154.326005913875,3.11993957868273,340.029771343448));
#22636=CARTESIAN_POINT('Ctrl Pts',(154.333419471455,2.98425367809265,340.109027358244));
#22637=CARTESIAN_POINT('Ctrl Pts',(154.340843583592,2.84837460378246,340.188396208488));
#22638=CARTESIAN_POINT('Ctrl Pts',(154.348267695728,2.70948181843196,340.262250211876));
#22639=CARTESIAN_POINT('Ctrl Pts',(154.355691807865,2.56807133781314,340.330378989003));
#22640=CARTESIAN_POINT('Ctrl Pts',(154.35954893302,2.49460289984933,340.365774631631));
#22641=CARTESIAN_POINT('Ctrl Pts',(154.363406058175,2.42045518104374,340.399625714032));
#22642=CARTESIAN_POINT('Ctrl Pts',(154.36726318333,2.34569941347926,340.43190802795));
#22643=CARTESIAN_POINT('Ctrl Pts',(154.374687160768,2.20181371895697,340.494043209089));
#22644=CARTESIAN_POINT('Ctrl Pts',(154.382111138206,2.05524041463205,340.550551098509));
#22645=CARTESIAN_POINT('Ctrl Pts',(154.389535115644,1.90645974918681,340.60119110433));
#22646=CARTESIAN_POINT('Ctrl Pts',(154.396950331671,1.75785466731193,340.651771347326));
#22647=CARTESIAN_POINT('Ctrl Pts',(154.404365547699,1.60704775951795,340.696497371931));
#22648=CARTESIAN_POINT('Ctrl Pts',(154.411780763727,1.45454125385807,340.735175699429));
#22649=CARTESIAN_POINT('Ctrl Pts',(154.419188844871,1.30218148919004,340.773816810836));
#22650=CARTESIAN_POINT('Ctrl Pts',(154.426596926015,1.1481257416625,340.806421718672));
#22651=CARTESIAN_POINT('Ctrl Pts',(154.434005007159,0.992893384131786,340.832846071194));
#22652=CARTESIAN_POINT('Ctrl Pts',(154.441407574333,0.837776568879942,340.859250755589));
#22653=CARTESIAN_POINT('Ctrl Pts',(154.448810141507,0.681485253758091,340.879483982177));
#22654=CARTESIAN_POINT('Ctrl Pts',(154.456212708681,0.52455094010036,340.893452033718));
#22655=CARTESIAN_POINT('Ctrl Pts',(154.463611378436,0.367699251672922,340.907412731142));
#22656=CARTESIAN_POINT('Ctrl Pts',(154.471010048191,0.210205609729445,340.915114789846));
#22657=CARTESIAN_POINT('Ctrl Pts',(154.478408717945,0.0526084993023518,
340.916516112401));
#22658=CARTESIAN_POINT('Ctrl Pts',(154.485806167149,-0.104962612495201,
340.917917203781));
#22659=CARTESIAN_POINT('Ctrl Pts',(154.493203616353,-0.262636786066086,
340.913019618621));
#22660=CARTESIAN_POINT('Ctrl Pts',(154.500601065557,-0.419873538320556,
340.9018333401));
#22661=CARTESIAN_POINT('Ctrl Pts',(154.507998194021,-0.577103473063572,
340.890647546597));
#22662=CARTESIAN_POINT('Ctrl Pts',(154.515395322484,-0.733895651930085,
340.873173628371));
#22663=CARTESIAN_POINT('Ctrl Pts',(154.522792450948,-0.889712990194715,
340.849473596622));
#22664=CARTESIAN_POINT('Ctrl Pts',(154.530190718384,-1.04555432043963,340.82576991566));
#22665=CARTESIAN_POINT('Ctrl Pts',(154.537588985821,-1.20042014222144,340.795838268471));
#22666=CARTESIAN_POINT('Ctrl Pts',(154.544987253258,-1.35378200875829,340.759792082642));
#22667=CARTESIAN_POINT('Ctrl Pts',(154.552388119783,-1.50719775293166,340.723733233409));
#22668=CARTESIAN_POINT('Ctrl Pts',(154.559788986309,-1.65910812682363,340.681555654008));
#22669=CARTESIAN_POINT('Ctrl Pts',(154.567189852835,-1.8089984689459,340.633423035939));
#22670=CARTESIAN_POINT('Ctrl Pts',(154.57459884622,-1.95905340499408,340.585237563654));
#22671=CARTESIAN_POINT('Ctrl Pts',(154.582007839605,-2.10708352388084,340.53108410774));
#22672=CARTESIAN_POINT('Ctrl Pts',(154.589416832989,-2.25259213688343,340.471175305851));
#22673=CARTESIAN_POINT('Ctrl Pts',(154.59683039057,-2.3981903882106,340.411229598073));
#22674=CARTESIAN_POINT('Ctrl Pts',(154.60424394815,-2.54126370006746,340.345521634857));
#22675=CARTESIAN_POINT('Ctrl Pts',(154.61165750573,-2.68133920022774,340.274310443634));
#22676=CARTESIAN_POINT('Ctrl Pts',(154.619081617867,-2.82161412350682,340.202997870243));
#22677=CARTESIAN_POINT('Ctrl Pts',(154.626505730004,-2.95888238638172,340.126166602868));
#22678=CARTESIAN_POINT('Ctrl Pts',(154.63392984214,-3.09269865372623,340.044119903387));
#22679=CARTESIAN_POINT('Ctrl Pts',(154.637786967295,-3.16222159213994,340.001493339753));
#22680=CARTESIAN_POINT('Ctrl Pts',(154.641644092449,-3.23081327474718,339.957459704203));
#22681=CARTESIAN_POINT('Ctrl Pts',(154.645501217604,-3.29841479654227,339.912065796836));
#22682=CARTESIAN_POINT('Ctrl Pts',(154.652900495726,-3.42809751130321,339.824984840898));
#22683=CARTESIAN_POINT('Ctrl Pts',(154.660299773847,-3.5545314263883,339.732628997538));
#22684=CARTESIAN_POINT('Ctrl Pts',(154.667699051969,-3.67725610131445,339.635268938028));
#22685=CARTESIAN_POINT('Ctrl Pts',(154.675089582152,-3.79983568263393,339.53802398432));
#22686=CARTESIAN_POINT('Ctrl Pts',(154.682480112335,-3.91871446016488,339.435786820934));
#22687=CARTESIAN_POINT('Ctrl Pts',(154.689870642517,-4.03345957138276,339.32887219129));
#22688=CARTESIAN_POINT('Ctrl Pts',(154.697254074777,-4.14809448049912,339.222060243291));
#22689=CARTESIAN_POINT('Ctrl Pts',(154.704637507037,-4.25860335270168,339.11058002586));
#22690=CARTESIAN_POINT('Ctrl Pts',(154.712020939297,-4.36458525258753,338.994787370486));
#22691=CARTESIAN_POINT('Ctrl Pts',(154.719398917832,-4.47048886961645,338.879080244621));
#22692=CARTESIAN_POINT('Ctrl Pts',(154.726776896366,-4.57187191886398,338.759067298811));
#22693=CARTESIAN_POINT('Ctrl Pts',(154.734154874901,-4.66836941033831,338.635142034518));
#22694=CARTESIAN_POINT('Ctrl Pts',(154.741827655959,-4.76872266038726,338.506265077769));
#22695=CARTESIAN_POINT('Ctrl Pts',(154.749500437017,-4.86379154784705,338.373156971735));
#22696=CARTESIAN_POINT('Ctrl Pts',(154.757173218075,-4.95321046000594,338.236299847262));
#22697=CARTESIAN_POINT('Ctrl Pts',(154.764546233667,-5.03913589285325,338.104789550674));
#22698=CARTESIAN_POINT('Ctrl Pts',(154.771919249259,-5.11984426264736,337.969817982963));
#22699=CARTESIAN_POINT('Ctrl Pts',(154.779292264851,-5.19505466459128,337.831843497513));
#22700=CARTESIAN_POINT('Ctrl Pts',(154.786665137011,-5.27026360342517,337.693871696158));
#22701=CARTESIAN_POINT('Ctrl Pts',(154.794038009172,-5.33997460689103,337.552897423265));
#22702=CARTESIAN_POINT('Ctrl Pts',(154.801410881332,-5.40395247186991,337.409404126391));
#22703=CARTESIAN_POINT('Ctrl Pts',(154.808785090685,-5.46794194029385,337.265884804632));
#22704=CARTESIAN_POINT('Ctrl Pts',(154.816159300038,-5.52619604719842,337.119845892829));
#22705=CARTESIAN_POINT('Ctrl Pts',(154.823533509391,-5.57852760379302,336.971791149239));
#22706=CARTESIAN_POINT('Ctrl Pts',(154.830910537117,-5.63087916115778,336.82367982012));
#22707=CARTESIAN_POINT('Ctrl Pts',(154.838287564843,-5.67730353701384,336.673551479729));
#22708=CARTESIAN_POINT('Ctrl Pts',(154.84566459257,-5.71766335604758,336.521925198363));
#22709=CARTESIAN_POINT('Ctrl Pts',(154.853049733589,-5.75806756301706,336.370132157635));
#22710=CARTESIAN_POINT('Ctrl Pts',(154.860434874608,-5.79239379978253,336.216838250088));
#22711=CARTESIAN_POINT('Ctrl Pts',(154.867820015627,-5.82055564983954,336.062573521984));
#22712=CARTESIAN_POINT('Ctrl Pts',(154.875209958905,-5.84873581240917,335.908208481763));
#22713=CARTESIAN_POINT('Ctrl Pts',(154.882599902183,-5.87074355018513,335.752871734394));
#22714=CARTESIAN_POINT('Ctrl Pts',(154.889989845461,-5.88654436198352,335.597098012809));
#22715=CARTESIAN_POINT('Ctrl Pts',(154.89738978996,-5.90236655789945,335.441113473981));
#22716=CARTESIAN_POINT('Ctrl Pts',(154.904789734459,-5.91196503569743,335.284691153918));
#22717=CARTESIAN_POINT('Ctrl Pts',(154.912189678958,-5.91535736389914,335.128365960691));
#22718=CARTESIAN_POINT('Ctrl Pts',(154.914226992737,-5.91629132184814,335.085327331125));
#22719=CARTESIAN_POINT('Ctrl Pts',(154.916264306515,-5.91675516787735,335.042296033567));
#22720=CARTESIAN_POINT('Ctrl Pts',(154.918301620294,-5.91674995657411,334.999283145596));
#22721=CARTESIAN_POINT('',(156.668300924438,-5.91517048090566,335.005379803398));
#22722=CARTESIAN_POINT('Ctrl Pts',(154.918301620294,-5.92639295407506,334.999281977281));
#22723=CARTESIAN_POINT('Ctrl Pts',(154.920114164155,-5.92645845110932,334.960952179359));
#22724=CARTESIAN_POINT('Ctrl Pts',(154.921926708016,-5.92611884753196,334.922623573182));
#22725=CARTESIAN_POINT('Ctrl Pts',(155.016485263302,-5.88708407117718,332.923475726914));
#22726=CARTESIAN_POINT('Ctrl Pts',(155.201977286152,-3.67068872424052,329.043602833008));
#22727=CARTESIAN_POINT('Ctrl Pts',(155.480215320426,3.02244115912318,328.68989125602));
#22728=CARTESIAN_POINT('Ctrl Pts',(155.7584533547,6.94192140191797,334.126873336331));
#22729=CARTESIAN_POINT('Ctrl Pts',(156.036691388974,4.49090283676372,340.365110868564));
#22730=CARTESIAN_POINT('Ctrl Pts',(156.314929423248,-2.08135097606897,341.67986534562));
#22731=CARTESIAN_POINT('Ctrl Pts',(156.525465843093,-5.609153889735,338.036267632335));
#22732=CARTESIAN_POINT('Ctrl Pts',(156.643256251513,-5.91922902505516,335.537755193878));
#22733=CARTESIAN_POINT('Ctrl Pts',(156.668300648508,-5.91454511534654,335.0053851016));
#22734=CARTESIAN_POINT('',(158.418302357817,-5.91166820494994,334.998075736246));
#22735=CARTESIAN_POINT('Ctrl Pts',(156.668301620294,-5.91674756634078,335.005366442065));
#22736=CARTESIAN_POINT('Ctrl Pts',(156.675633488304,-5.91688897598109,334.849455852701));
#22737=CARTESIAN_POINT('Ctrl Pts',(156.682965356315,-5.9108636352077,334.693405342462));
#22738=CARTESIAN_POINT('Ctrl Pts',(156.690297224325,-5.89866525491898,334.537745986592));
#22739=CARTESIAN_POINT('Ctrl Pts',(156.697843402136,-5.88611031714083,334.377536722634));
#22740=CARTESIAN_POINT('Ctrl Pts',(156.705389579948,-5.86701591486274,334.217742239667));
#22741=CARTESIAN_POINT('Ctrl Pts',(156.712935757759,-5.84143288569137,334.058940807142));
#22742=CARTESIAN_POINT('Ctrl Pts',(156.720262482015,-5.81659384729707,333.904757545529));
#22743=CARTESIAN_POINT('Ctrl Pts',(156.727589206272,-5.78563839821375,333.751510778622));
#22744=CARTESIAN_POINT('Ctrl Pts',(156.734915930528,-5.74866554615006,333.599723241281));
#22745=CARTESIAN_POINT('Ctrl Pts',(156.742242472371,-5.71169361460261,333.447939483008));
#22746=CARTESIAN_POINT('Ctrl Pts',(156.749569014213,-5.6687046679693,333.297615252379));
#22747=CARTESIAN_POINT('Ctrl Pts',(156.756895556055,-5.61984841418772,333.149261130237));
#22748=CARTESIAN_POINT('Ctrl Pts',(156.764223429155,-5.57098328306163,333.000880051655));
#22749=CARTESIAN_POINT('Ctrl Pts',(156.771551302255,-5.51624884236344,332.854470155897));
#22750=CARTESIAN_POINT('Ctrl Pts',(156.778879175354,-5.45584397225896,332.710524707959));
#22751=CARTESIAN_POINT('Ctrl Pts',(156.786589701724,-5.3922848279483,332.559062591039));
#22752=CARTESIAN_POINT('Ctrl Pts',(156.794300228094,-5.32244733029172,332.410329655211));
#22753=CARTESIAN_POINT('Ctrl Pts',(156.802010754465,-5.24661907655998,332.264873160532));
#22754=CARTESIAN_POINT('Ctrl Pts',(156.809349811636,-5.17444399244361,332.126424307736));
#22755=CARTESIAN_POINT('Ctrl Pts',(156.816688868807,-5.09684209173963,331.990943901949));
#22756=CARTESIAN_POINT('Ctrl Pts',(156.824027925979,-5.01410656628233,331.858875057489));
#22757=CARTESIAN_POINT('Ctrl Pts',(156.831371939168,-4.93131517006361,331.726717027799));
#22758=CARTESIAN_POINT('Ctrl Pts',(156.838715952357,-4.84338345930787,331.597975460644));
#22759=CARTESIAN_POINT('Ctrl Pts',(156.846059965546,-4.75064585436508,331.473061592698));
#22760=CARTESIAN_POINT('Ctrl Pts',(156.853413787207,-4.65778439148889,331.347980893038));
#22761=CARTESIAN_POINT('Ctrl Pts',(156.860767608869,-4.56010446362926,331.226738388744));
#22762=CARTESIAN_POINT('Ctrl Pts',(156.868121430531,-4.45797865208204,331.109709920831));
#22763=CARTESIAN_POINT('Ctrl Pts',(156.869216117619,-4.44277624272213,331.092289107728));
#22764=CARTESIAN_POINT('Ctrl Pts',(156.870310804708,-4.42747537810144,331.074961603319));
#22765=CARTESIAN_POINT('Ctrl Pts',(156.871405491796,-4.41207735084086,331.057728571915));
#22766=CARTESIAN_POINT('Ctrl Pts',(156.878829469234,-4.30765060806387,330.940857150189));
#22767=CARTESIAN_POINT('Ctrl Pts',(156.886253446672,-4.1984194186915,330.827961524164));
#22768=CARTESIAN_POINT('Ctrl Pts',(156.89367742411,-4.08471836925703,330.719461902242));
#22769=CARTESIAN_POINT('Ctrl Pts',(156.901092640137,-3.97115150416818,330.611090326199));
#22770=CARTESIAN_POINT('Ctrl Pts',(156.908507856165,-3.85312554658059,330.507104682716));
#22771=CARTESIAN_POINT('Ctrl Pts',(156.915923072193,-3.73101483348997,330.40789167432));
#22772=CARTESIAN_POINT('Ctrl Pts',(156.923331153337,-3.60902161471262,330.308774128182));
#22773=CARTESIAN_POINT('Ctrl Pts',(156.930739234481,-3.4829517527098,330.214420308675));
#22774=CARTESIAN_POINT('Ctrl Pts',(156.938147315625,-3.3532157951102,330.125179552648));
#22775=CARTESIAN_POINT('Ctrl Pts',(156.945549882799,-3.22357640235326,330.036005220145));
#22776=CARTESIAN_POINT('Ctrl Pts',(156.952952449973,-3.09027665349441,329.951936583933));
#22777=CARTESIAN_POINT('Ctrl Pts',(156.960355017147,-2.95375938919286,329.873282138321));
#22778=CARTESIAN_POINT('Ctrl Pts',(156.967753686902,-2.81731400063397,329.794669103931));
#22779=CARTESIAN_POINT('Ctrl Pts',(156.975152356656,-2.67765479291337,329.721464768953));
#22780=CARTESIAN_POINT('Ctrl Pts',(156.982551026411,-2.53525264600912,329.653933728113));
#22781=CARTESIAN_POINT('Ctrl Pts',(156.989948475615,-2.39287399103746,329.586413827799));
#22782=CARTESIAN_POINT('Ctrl Pts',(156.997345924819,-2.24775363183439,329.524565523891));
#22783=CARTESIAN_POINT('Ctrl Pts',(157.004743374023,-2.10038615785365,329.468606997293));
#22784=CARTESIAN_POINT('Ctrl Pts',(157.012140502486,-1.95302507346984,329.412650896959));
#22785=CARTESIAN_POINT('Ctrl Pts',(157.01953763095,-1.80341741693734,329.36258419866));
#22786=CARTESIAN_POINT('Ctrl Pts',(157.026934759413,-1.65207656878288,329.318576448338));
#22787=CARTESIAN_POINT('Ctrl Pts',(157.03433302685,-1.50071241791526,329.274561921921));
#22788=CARTESIAN_POINT('Ctrl Pts',(157.041731294287,-1.34761490244525,329.236608305275));
#22789=CARTESIAN_POINT('Ctrl Pts',(157.049129561723,-1.19331118283358,329.204834861419));
#22790=CARTESIAN_POINT('Ctrl Pts',(157.056530428249,-1.03895325470312,329.173050255218));
#22791=CARTESIAN_POINT('Ctrl Pts',(157.063931294775,-0.883388644052891,
329.147450219807));
#22792=CARTESIAN_POINT('Ctrl Pts',(157.0713321613,-0.727153136431057,329.128102616813));
#22793=CARTESIAN_POINT('Ctrl Pts',(157.078741154685,-0.570746067284901,
329.108733768302));
#22794=CARTESIAN_POINT('Ctrl Pts',(157.08615014807,-0.41366700052293,329.095631109409));
#22795=CARTESIAN_POINT('Ctrl Pts',(157.093559141454,-0.256455993363195,
329.088810535436));
#22796=CARTESIAN_POINT('Ctrl Pts',(157.100972699035,-0.0991481388001783,
329.081985759755));
#22797=CARTESIAN_POINT('Ctrl Pts',(157.108386256615,0.0582914457842649,
329.081450781708));
#22798=CARTESIAN_POINT('Ctrl Pts',(157.115799814195,0.215324808441732,329.087169392806));
#22799=CARTESIAN_POINT('Ctrl Pts',(157.123223926332,0.372581736839745,329.092896145394));
#22800=CARTESIAN_POINT('Ctrl Pts',(157.130648038468,0.529430917147036,329.104894240069));
#22801=CARTESIAN_POINT('Ctrl Pts',(157.138072150605,0.685340784651717,329.123075755857));
#22802=CARTESIAN_POINT('Ctrl Pts',(157.14192927576,0.766342237857799,329.132521785309));
#22803=CARTESIAN_POINT('Ctrl Pts',(157.145786400915,0.847090326754616,329.143636015974));
#22804=CARTESIAN_POINT('Ctrl Pts',(157.14964352607,0.92751192906392,329.156400750912));
#22805=CARTESIAN_POINT('Ctrl Pts',(157.157067503508,1.08230290345749,329.180969594383));
#22806=CARTESIAN_POINT('Ctrl Pts',(157.164491480946,1.23635050815835,329.21173013068));
#22807=CARTESIAN_POINT('Ctrl Pts',(157.171915458384,1.38912031698442,329.248628397726));
#22808=CARTESIAN_POINT('Ctrl Pts',(157.179330674411,1.5417098344505,329.285483119266));
#22809=CARTESIAN_POINT('Ctrl Pts',(157.186745890439,1.69302419847087,329.328461066591));
#22810=CARTESIAN_POINT('Ctrl Pts',(157.194161106466,1.84253564741217,329.377456718662));
#22811=CARTESIAN_POINT('Ctrl Pts',(157.20156918761,1.99190323719024,329.426405227364));
#22812=CARTESIAN_POINT('Ctrl Pts',(157.208977268755,2.13947101318137,329.481359798149));
#22813=CARTESIAN_POINT('Ctrl Pts',(157.216385349899,2.28472303969744,329.54216423897));
#22814=CARTESIAN_POINT('Ctrl Pts',(157.223787917073,2.42986695247754,329.602923421936));
#22815=CARTESIAN_POINT('Ctrl Pts',(157.231190484247,2.57269820504026,329.669523661665));
#22816=CARTESIAN_POINT('Ctrl Pts',(157.238593051421,2.71271773144703,329.741759507973));
#22817=CARTESIAN_POINT('Ctrl Pts',(157.245991721175,2.85266353818495,329.813957322424));
#22818=CARTESIAN_POINT('Ctrl Pts',(157.25339039093,2.98980023615567,329.891784663573));
#22819=CARTESIAN_POINT('Ctrl Pts',(157.260789060685,3.12365050183226,329.974988745793));
#22820=CARTESIAN_POINT('Ctrl Pts',(157.268186509889,3.25747868637105,330.058179101923));
#22821=CARTESIAN_POINT('Ctrl Pts',(157.275583959093,3.38802119797191,330.146744241885));
#22822=CARTESIAN_POINT('Ctrl Pts',(157.282981408297,3.51482691292582,330.24038632506));
#22823=CARTESIAN_POINT('Ctrl Pts',(157.29037853676,3.64162712980491,330.334024348078));
#22824=CARTESIAN_POINT('Ctrl Pts',(157.297775665224,3.76469057196565,330.43273865492));
#22825=CARTESIAN_POINT('Ctrl Pts',(157.305172793687,3.88359684494801,330.536189283985));
#22826=CARTESIAN_POINT('Ctrl Pts',(157.312571061124,4.0025214265282,330.639655841865));
#22827=CARTESIAN_POINT('Ctrl Pts',(157.31996932856,4.11728728282484,330.74785992907));
#22828=CARTESIAN_POINT('Ctrl Pts',(157.327367595997,4.2275088462469,330.860422785186));
#22829=CARTESIAN_POINT('Ctrl Pts',(157.334768462523,4.33776913166372,330.973025185818));
#22830=CARTESIAN_POINT('Ctrl Pts',(157.342169329049,4.44348168471309,331.089989137649));
#22831=CARTESIAN_POINT('Ctrl Pts',(157.349570195574,4.54429949479953,331.210900811002));
#22832=CARTESIAN_POINT('Ctrl Pts',(157.356979188959,4.6452280124797,331.331945256932));
#22833=CARTESIAN_POINT('Ctrl Pts',(157.364388182344,4.74125081409529,331.45694579475));
#22834=CARTESIAN_POINT('Ctrl Pts',(157.371797175728,4.83206227699911,331.585456880679));
#22835=CARTESIAN_POINT('Ctrl Pts',(157.379210733309,4.9229296828966,331.71404713387));
#22836=CARTESIAN_POINT('Ctrl Pts',(157.386624290889,5.00857915044992,331.846151932055));
#22837=CARTESIAN_POINT('Ctrl Pts',(157.394037848469,5.08875001148244,331.981299305473));
#22838=CARTESIAN_POINT('Ctrl Pts',(157.401461960606,5.16903501041282,332.116639085919));
#22839=CARTESIAN_POINT('Ctrl Pts',(157.408886072742,5.24382564810089,332.255029765349));
#22840=CARTESIAN_POINT('Ctrl Pts',(157.416310184879,5.31290819900202,332.395976760573));
#22841=CARTESIAN_POINT('Ctrl Pts',(157.420167310034,5.34879936550541,332.469204399213));
#22842=CARTESIAN_POINT('Ctrl Pts',(157.424024435189,5.3831505960538,332.543121737798));
#22843=CARTESIAN_POINT('Ctrl Pts',(157.427881560343,5.41593720172094,332.617657709414));
#22844=CARTESIAN_POINT('Ctrl Pts',(157.435305537781,5.47904301524107,332.761120353065));
#22845=CARTESIAN_POINT('Ctrl Pts',(157.442729515219,5.53653982217527,332.907308561549));
#22846=CARTESIAN_POINT('Ctrl Pts',(157.450153492657,5.58818379171178,333.055743722512));
#22847=CARTESIAN_POINT('Ctrl Pts',(157.457568708685,5.63976681359408,333.204003707653));
#22848=CARTESIAN_POINT('Ctrl Pts',(157.464983924713,5.68551062558205,333.354505017881));
#22849=CARTESIAN_POINT('Ctrl Pts',(157.47239914074,5.72521836046588,333.506746743689));
#22850=CARTESIAN_POINT('Ctrl Pts',(157.479807221884,5.76488788876708,333.658841983275));
#22851=CARTESIAN_POINT('Ctrl Pts',(157.487215303028,5.79853280881599,333.81267394587));
#22852=CARTESIAN_POINT('Ctrl Pts',(157.494623384173,5.82600526343079,333.96772424567));
#22853=CARTESIAN_POINT('Ctrl Pts',(157.502025951347,5.85345726979598,334.122659138701));
#22854=CARTESIAN_POINT('Ctrl Pts',(157.509428518521,5.87474589377109,334.278810197391));
#22855=CARTESIAN_POINT('Ctrl Pts',(157.516831085695,5.88977382958386,334.435646565662));
#22856=CARTESIAN_POINT('Ctrl Pts',(157.524229755449,5.90479385325413,334.592400360271));
#22857=CARTESIAN_POINT('Ctrl Pts',(157.531628425204,5.9135597178815,334.749838375306));
#22858=CARTESIAN_POINT('Ctrl Pts',(157.539027094959,5.91602568914555,334.907422422423));
#22859=CARTESIAN_POINT('Ctrl Pts',(157.546424544163,5.9184912536009,335.064980473065));
#22860=CARTESIAN_POINT('Ctrl Pts',(157.553821993367,5.91465898150763,335.222684135173));
#22861=CARTESIAN_POINT('Ctrl Pts',(157.561219442571,5.90453520447066,335.379992870547));
#22862=CARTESIAN_POINT('Ctrl Pts',(157.568616571034,5.894411866383,335.537294785289));
#22863=CARTESIAN_POINT('Ctrl Pts',(157.576013699498,5.87799758971425,335.694201434904));
#22864=CARTESIAN_POINT('Ctrl Pts',(157.583410827961,5.85535075586203,335.850175327992));
#22865=CARTESIAN_POINT('Ctrl Pts',(157.590809095398,5.83270043496279,336.006173237166));
#22866=CARTESIAN_POINT('Ctrl Pts',(157.598207362834,5.80381569970409,336.161237734484));
#22867=CARTESIAN_POINT('Ctrl Pts',(157.605605630271,5.76880640505196,336.314839618939));
#22868=CARTESIAN_POINT('Ctrl Pts',(157.613006496796,5.73378481126629,336.468495465352));
#22869=CARTESIAN_POINT('Ctrl Pts',(157.620407363322,5.69263445709513,336.620687312216));
#22870=CARTESIAN_POINT('Ctrl Pts',(157.627808229848,5.64551555339729,336.770899403933));
#22871=CARTESIAN_POINT('Ctrl Pts',(157.635217223233,5.59834490863842,336.921276442887));
#22872=CARTESIAN_POINT('Ctrl Pts',(157.642626216617,5.54519273735874,337.069669028866));
#22873=CARTESIAN_POINT('Ctrl Pts',(157.650035210002,5.48626831687429,337.21557904796));
#22874=CARTESIAN_POINT('Ctrl Pts',(157.657448767582,5.42730759691433,337.36157895266));
#22875=CARTESIAN_POINT('Ctrl Pts',(157.664862325163,5.36256769524638,337.505092903647));
#22876=CARTESIAN_POINT('Ctrl Pts',(157.672275882743,5.29230443880382,337.64564628957));
#22877=CARTESIAN_POINT('Ctrl Pts',(157.67969999488,5.22194114975245,337.78639977897));
#22878=CARTESIAN_POINT('Ctrl Pts',(157.687124107016,5.14603898052259,337.924183959286));
#22879=CARTESIAN_POINT('Ctrl Pts',(157.694548219153,5.06489817751462,338.058551456803));
#22880=CARTESIAN_POINT('Ctrl Pts',(157.698405344307,5.02274226357107,338.128360781484));
#22881=CARTESIAN_POINT('Ctrl Pts',(157.702262469462,4.97917301852347,338.197248377384));
#22882=CARTESIAN_POINT('Ctrl Pts',(157.706119594616,4.93423684346073,338.265155024671));
#22883=CARTESIAN_POINT('Ctrl Pts',(157.713543572054,4.8477462224802,338.395857917928));
#22884=CARTESIAN_POINT('Ctrl Pts',(157.720967549492,4.75592826057564,338.523319037407));
#22885=CARTESIAN_POINT('Ctrl Pts',(157.72839152693,4.65905348224265,338.647074335972));
#22886=CARTESIAN_POINT('Ctrl Pts',(157.735806742958,4.56229303072363,338.770683584664));
#22887=CARTESIAN_POINT('Ctrl Pts',(157.743221958986,4.46048786959514,338.890595426793));
#22888=CARTESIAN_POINT('Ctrl Pts',(157.750637175013,4.35395268820359,339.006373241647));
#22889=CARTESIAN_POINT('Ctrl Pts',(157.758045256157,4.24752001442733,339.12203965567));
#22890=CARTESIAN_POINT('Ctrl Pts',(157.765453337302,4.13636663200349,339.233579688559));
#22891=CARTESIAN_POINT('Ctrl Pts',(157.772861418446,4.02084844861,339.34058847575));
#22892=CARTESIAN_POINT('Ctrl Pts',(157.78026398562,3.90541624751008,339.447517614346));
#22893=CARTESIAN_POINT('Ctrl Pts',(157.787666552794,3.78562598689547,339.549921970222));
#22894=CARTESIAN_POINT('Ctrl Pts',(157.795069119968,3.66187141723115,339.647432440194));
#22895=CARTESIAN_POINT('Ctrl Pts',(157.802467789722,3.53818200380669,339.744891571329));
#22896=CARTESIAN_POINT('Ctrl Pts',(157.809866459477,3.41053273050614,339.837461717633));
#22897=CARTESIAN_POINT('Ctrl Pts',(157.817265129232,3.27935142192641,339.924813175544));
#22898=CARTESIAN_POINT('Ctrl Pts',(157.824662578436,3.1481917541891,340.012150223176));
#22899=CARTESIAN_POINT('Ctrl Pts',(157.83206002764,3.01350151793727,340.094270084416));
#22900=CARTESIAN_POINT('Ctrl Pts',(157.839457476844,2.87573868966934,340.170885567409));
#22901=CARTESIAN_POINT('Ctrl Pts',(157.846854605307,2.73798183455781,340.247497728488));
#22902=CARTESIAN_POINT('Ctrl Pts',(157.854251733771,2.59715297848425,340.318605804462));
#22903=CARTESIAN_POINT('Ctrl Pts',(157.861648862234,2.45373570295703,340.383968022057));
#22904=CARTESIAN_POINT('Ctrl Pts',(157.869047129671,2.31029634474955,340.449340303802));
#22905=CARTESIAN_POINT('Ctrl Pts',(157.876445397108,2.16426811314458,340.508964810792));
#22906=CARTESIAN_POINT('Ctrl Pts',(157.883843664544,2.0161554733843,340.562647541382));
#22907=CARTESIAN_POINT('Ctrl Pts',(157.89124453107,1.8679908000963,340.616349131279));
#22908=CARTESIAN_POINT('Ctrl Pts',(157.898645397596,1.7177406113502,340.664104661657));
#22909=CARTESIAN_POINT('Ctrl Pts',(157.906046264121,1.56592531631867,340.705769752296));
#22910=CARTESIAN_POINT('Ctrl Pts',(157.913455257506,1.41394331357857,340.747480595188));
#22911=CARTESIAN_POINT('Ctrl Pts',(157.920864250891,1.26039313246243,340.783087543445));
#22912=CARTESIAN_POINT('Ctrl Pts',(157.928273244276,1.10580689954551,340.812497024809));
#22913=CARTESIAN_POINT('Ctrl Pts',(157.935686801856,0.951125436176458,340.841924623429));
#22914=CARTESIAN_POINT('Ctrl Pts',(157.943100359436,0.795407017488464,340.865147092659));
#22915=CARTESIAN_POINT('Ctrl Pts',(157.950513917017,0.639189196924143,340.882122723391));
#22916=CARTESIAN_POINT('Ctrl Pts',(157.957938029153,0.482748971693086,340.899122522041));
#22917=CARTESIAN_POINT('Ctrl Pts',(157.96536214129,0.32580829593344,340.909857694657));
#22918=CARTESIAN_POINT('Ctrl Pts',(157.972786253427,0.168905856300576,340.914338625257));
#22919=CARTESIAN_POINT('Ctrl Pts',(157.976643378581,0.0873887219144972,
340.916666649109));
#22920=CARTESIAN_POINT('Ctrl Pts',(157.980500503736,0.00588185436856069,
340.91730737235));
#22921=CARTESIAN_POINT('Ctrl Pts',(157.984357628891,-0.0755398368275449,
340.916267767398));
#22922=CARTESIAN_POINT('Ctrl Pts',(157.991781606329,-0.232255726034468,
340.914266794291));
#22923=CARTESIAN_POINT('Ctrl Pts',(157.999205583767,-0.389128468368965,
340.906031636743));
#22924=CARTESIAN_POINT('Ctrl Pts',(158.006629561205,-0.545621440364771,
340.89153866204));
#22925=CARTESIAN_POINT('Ctrl Pts',(158.014044777232,-0.701929727107513,
340.877062791229));
#22926=CARTESIAN_POINT('Ctrl Pts',(158.02145999326,-0.857858767626078,340.856343837634));
#22927=CARTESIAN_POINT('Ctrl Pts',(158.028875209288,-1.01287110178623,340.829410149721));
#22928=CARTESIAN_POINT('Ctrl Pts',(158.036283290432,-1.1677342838595,340.802502377266));
#22929=CARTESIAN_POINT('Ctrl Pts',(158.043691371576,-1.32168215032732,340.769391838594));
#22930=CARTESIAN_POINT('Ctrl Pts',(158.05109945272,-1.47418163987487,340.730158728618));
#22931=CARTESIAN_POINT('Ctrl Pts',(158.058502019894,-1.62656762126736,340.690954820562));
#22932=CARTESIAN_POINT('Ctrl Pts',(158.065904587068,-1.77750701240742,340.645637507723));
#22933=CARTESIAN_POINT('Ctrl Pts',(158.073307154242,-1.9264763455828,340.594338160356));
#22934=CARTESIAN_POINT('Ctrl Pts',(158.080705823997,-2.07536724705518,340.54306582187));
#22935=CARTESIAN_POINT('Ctrl Pts',(158.088104493752,-2.22228980427606,340.485817842513));
#22936=CARTESIAN_POINT('Ctrl Pts',(158.095503163506,-2.36673524204908,340.422775567598));
#22937=CARTESIAN_POINT('Ctrl Pts',(158.10290061271,-2.51115685081043,340.359743692702));
#22938=CARTESIAN_POINT('Ctrl Pts',(158.110298061914,-2.65310180943753,340.290919568501));
#22939=CARTESIAN_POINT('Ctrl Pts',(158.117695511118,-2.79208077481128,340.216532901212));
#22940=CARTESIAN_POINT('Ctrl Pts',(158.125092639582,-2.93105371429922,340.1421494592));
#22941=CARTESIAN_POINT('Ctrl Pts',(158.132489768045,-3.06706058718992,340.062204129766));
#22942=CARTESIAN_POINT('Ctrl Pts',(158.139886896509,-3.19963638747686,339.976972729525));
#22943=CARTESIAN_POINT('Ctrl Pts',(158.147285163945,-3.33223260112725,339.891728205776));
#22944=CARTESIAN_POINT('Ctrl Pts',(158.154683431382,-3.46139637630798,339.80119619243));
#22945=CARTESIAN_POINT('Ctrl Pts',(158.162081698818,-3.58669157780754,339.705695919647));
#22946=CARTESIAN_POINT('Ctrl Pts',(158.169482565344,-3.712030796829,339.610162096615));
#22947=CARTESIAN_POINT('Ctrl Pts',(158.17688343187,-3.83349843962747,339.509656765149));
#22948=CARTESIAN_POINT('Ctrl Pts',(158.184284298396,-3.95069147053294,339.404539416007));
#22949=CARTESIAN_POINT('Ctrl Pts',(158.19169329178,-4.06801319059056,339.299306637965));
#22950=CARTESIAN_POINT('Ctrl Pts',(158.199102285165,-4.18105064673004,339.189451977643));
#22951=CARTESIAN_POINT('Ctrl Pts',(158.20651127855,-4.28943718782086,339.075372274313));
#22952=CARTESIAN_POINT('Ctrl Pts',(158.21392483613,-4.39789049875953,338.961222293951));
#22953=CARTESIAN_POINT('Ctrl Pts',(158.22133839371,-4.50168694003735,338.842842364175));
#22954=CARTESIAN_POINT('Ctrl Pts',(158.228751951291,-4.6005005365625,338.720661953952));
#22955=CARTESIAN_POINT('Ctrl Pts',(158.236176063427,-4.69945481233254,338.598307597548));
#22956=CARTESIAN_POINT('Ctrl Pts',(158.243600175564,-4.79341185291784,338.472142253006));
#22957=CARTESIAN_POINT('Ctrl Pts',(158.251024287701,-4.88208887620064,338.342624532815));
#22958=CARTESIAN_POINT('Ctrl Pts',(158.254881412855,-4.92816015999168,338.275334862707));
#22959=CARTESIAN_POINT('Ctrl Pts',(158.25873853801,-4.97280700072594,338.207140731026));
#22960=CARTESIAN_POINT('Ctrl Pts',(158.262595663165,-5.01599472382435,338.138108903953));
#22961=CARTESIAN_POINT('Ctrl Pts',(158.27022228883,-5.10138904840625,338.001613487555));
#22962=CARTESIAN_POINT('Ctrl Pts',(158.277848914495,-5.18132210798116,337.86144817117));
#22963=CARTESIAN_POINT('Ctrl Pts',(158.285475540161,-5.25547266730665,337.718076085339));
#22964=CARTESIAN_POINT('Ctrl Pts',(158.293091648239,-5.32952096843845,337.574901718456));
#22965=CARTESIAN_POINT('Ctrl Pts',(158.300707756317,-5.39780249676258,337.428529695603));
#22966=CARTESIAN_POINT('Ctrl Pts',(158.308323864396,-5.46003945974696,337.279451613987));
#22967=CARTESIAN_POINT('Ctrl Pts',(158.315930634586,-5.52220011580696,337.130556312657));
#22968=CARTESIAN_POINT('Ctrl Pts',(158.323537404776,-5.57833083869148,336.978961879332));
#22969=CARTESIAN_POINT('Ctrl Pts',(158.331144174967,-5.62819983144839,336.825184160512));
#22970=CARTESIAN_POINT('Ctrl Pts',(158.338740327179,-5.6779992141233,336.671621093704));
#22971=CARTESIAN_POINT('Ctrl Pts',(158.34633647939,-5.72155418874964,336.515881145363));
#22972=CARTESIAN_POINT('Ctrl Pts',(158.353932631602,-5.7586812573137,336.358499443932));
#22973=CARTESIAN_POINT('Ctrl Pts',(158.361522571177,-5.79577796089941,336.201246459692));
#22974=CARTESIAN_POINT('Ctrl Pts',(158.369112510752,-5.82645715137391,336.042354732067));
#22975=CARTESIAN_POINT('Ctrl Pts',(158.376702450327,-5.85058504998213,335.882374713727));
#22976=CARTESIAN_POINT('Ctrl Pts',(158.384286117463,-5.87469300893786,335.722526905242));
#22977=CARTESIAN_POINT('Ctrl Pts',(158.3918697846,-5.89226041819555,335.561592939988));
#22978=CARTESIAN_POINT('Ctrl Pts',(158.399453451737,-5.90320452748765,335.400133564137));
#22979=CARTESIAN_POINT('Ctrl Pts',(158.405736174589,-5.91227122362711,335.266371824316));
#22980=CARTESIAN_POINT('Ctrl Pts',(158.412018897442,-5.91679300422876,335.132249777994));
#22981=CARTESIAN_POINT('Ctrl Pts',(158.418301620294,-5.91674969165613,334.998089820131));
#22982=CARTESIAN_POINT('',(160.168301620294,-5.92155652207472,334.995416553942));
#22983=CARTESIAN_POINT('Ctrl Pts',(158.418302957134,-5.90753895514141,334.998064291588));
#22984=CARTESIAN_POINT('Ctrl Pts',(158.459146537236,-5.91004580971049,334.127255823406));
#22985=CARTESIAN_POINT('Ctrl Pts',(158.592736128762,-5.32113314713912,331.282283490978));
#22986=CARTESIAN_POINT('Ctrl Pts',(158.819071731712,-0.92000436045686,328.064135605567));
#22987=CARTESIAN_POINT('Ctrl Pts',(159.097309765987,5.33464919017363,330.472954502217));
#22988=CARTESIAN_POINT('Ctrl Pts',(159.375547800261,6.69377391827487,337.0361762331));
#22989=CARTESIAN_POINT('Ctrl Pts',(159.653785834535,1.91012112151633,341.73082908878));
#22990=CARTESIAN_POINT('Ctrl Pts',(159.918037107879,-4.29783585754292,340.32320468228));
#22991=CARTESIAN_POINT('Ctrl Pts',(160.089542369799,-5.90729764126013,336.664520679854));
#22992=CARTESIAN_POINT('Ctrl Pts',(160.168301620294,-5.92155652207472,334.995416553942));
#22993=CARTESIAN_POINT('',(161.918301620294,-5.9222056262964,335.004340868688));
#22994=CARTESIAN_POINT('Ctrl Pts',(160.168301620294,-5.92155652207472,334.995416553942));
#22995=CARTESIAN_POINT('Ctrl Pts',(160.182288381224,-5.9240887396342,334.69900235207));
#22996=CARTESIAN_POINT('Ctrl Pts',(160.289021153575,-5.76896797440835,332.439729074422));
#22997=CARTESIAN_POINT('Ctrl Pts',(160.48849993736,-2.86034519230075,328.614778915175));
#22998=CARTESIAN_POINT('Ctrl Pts',(160.766737971629,3.82157172282052,329.139265192097));
#22999=CARTESIAN_POINT('Ctrl Pts',(161.044976005905,6.99648867421634,335.042061297929));
#23000=CARTESIAN_POINT('Ctrl Pts',(161.323214040178,3.75083123728682,340.906258371475));
#23001=CARTESIAN_POINT('Ctrl Pts',(161.601452074453,-2.93690866392185,341.350369313749));
#23002=CARTESIAN_POINT('Ctrl Pts',(161.799814601158,-5.78331565926206,337.512322992919));
#23003=CARTESIAN_POINT('Ctrl Pts',(161.905431116438,-5.9244497178173,335.277020989329));
#23004=CARTESIAN_POINT('Ctrl Pts',(161.918301620294,-5.9222056262964,335.004340868688));
#23005=CARTESIAN_POINT('',(163.668300761703,-5.91179366464294,335.002290923672));
#23006=CARTESIAN_POINT('Ctrl Pts',(161.918301620294,-5.9222056262964,335.004340868688));
#23007=CARTESIAN_POINT('Ctrl Pts',(161.998177127863,-5.90827859194964,333.312063450199));
#23008=CARTESIAN_POINT('Ctrl Pts',(162.170798646855,-4.25981713968337,329.631137126993));
#23009=CARTESIAN_POINT('Ctrl Pts',(162.436166177274,1.99090855870963,328.292623014017));
#23010=CARTESIAN_POINT('Ctrl Pts',(162.714404211547,6.71777126255143,333.044450924867));
#23011=CARTESIAN_POINT('Ctrl Pts',(162.992642245822,5.27983443289055,339.590857358107));
#23012=CARTESIAN_POINT('Ctrl Pts',(163.270880280096,-1.00332852560485,341.924301754756));
#23013=CARTESIAN_POINT('Ctrl Pts',(163.496099554182,-5.34393227885399,338.669603558887));
#23014=CARTESIAN_POINT('Ctrl Pts',(163.628572816844,-5.91070066925879,335.849222013648));
#23015=CARTESIAN_POINT('Ctrl Pts',(163.668300068081,-5.90778998552529,335.002304171406));
#23016=CARTESIAN_POINT('',(165.41830244586,-5.91482905803173,334.994703811423));
#23017=CARTESIAN_POINT('Ctrl Pts',(163.668301620294,-5.91674956281194,335.002274525151));
#23018=CARTESIAN_POINT('Ctrl Pts',(163.675857115675,-5.91681157553319,334.8409600894));
#23019=CARTESIAN_POINT('Ctrl Pts',(163.683412611056,-5.91027211048072,334.679685551574));
#23020=CARTESIAN_POINT('Ctrl Pts',(163.690968106437,-5.89716734275482,334.519013623846));
#23021=CARTESIAN_POINT('Ctrl Pts',(163.698527137371,-5.88405644272485,334.358266510572));
#23022=CARTESIAN_POINT('Ctrl Pts',(163.706086168305,-5.86437414400719,334.198122918836));
#23023=CARTESIAN_POINT('Ctrl Pts',(163.713645199238,-5.83820841926096,334.039139439996));
#23024=CARTESIAN_POINT('Ctrl Pts',(163.721208980901,-5.81202624977905,333.880056042606));
#23025=CARTESIAN_POINT('Ctrl Pts',(163.728772762564,-5.77935258811635,333.722134557066));
#23026=CARTESIAN_POINT('Ctrl Pts',(163.736336544226,-5.74032635561207,333.565920541405));
#23027=CARTESIAN_POINT('Ctrl Pts',(163.743921527928,-5.70119072866306,333.409268642186));
#23028=CARTESIAN_POINT('Ctrl Pts',(163.751506511629,-5.65566697243352,333.254334136229));
#23029=CARTESIAN_POINT('Ctrl Pts',(163.75909149533,-5.60394482166675,333.10164992738));
#23030=CARTESIAN_POINT('Ctrl Pts',(163.766672870695,-5.55224727621628,332.949038353626));
#23031=CARTESIAN_POINT('Ctrl Pts',(163.77425424606,-5.49435739914961,332.798675247789));
#23032=CARTESIAN_POINT('Ctrl Pts',(163.781835621425,-5.43051209425154,332.651070678652));
#23033=CARTESIAN_POINT('Ctrl Pts',(163.789431241455,-5.36654683025353,332.503188774929));
#23034=CARTESIAN_POINT('Ctrl Pts',(163.797026861485,-5.29660392036394,332.35807608578));
#23035=CARTESIAN_POINT('Ctrl Pts',(163.804622481514,-5.22096663919529,332.216218773878));
#23036=CARTESIAN_POINT('Ctrl Pts',(163.812200437224,-5.14550525955161,332.074691364335));
#23037=CARTESIAN_POINT('Ctrl Pts',(163.819778392934,-5.06437620414303,331.93640446396));
#23038=CARTESIAN_POINT('Ctrl Pts',(163.827356348643,-4.97790233694105,331.801810060929));
#23039=CARTESIAN_POINT('Ctrl Pts',(163.834780326081,-4.89318555266768,331.669950513358));
#23040=CARTESIAN_POINT('Ctrl Pts',(163.842204303519,-4.80309811376579,331.541260465337));
#23041=CARTESIAN_POINT('Ctrl Pts',(163.849628280957,-4.70790425024316,331.416207576736));
#23042=CARTESIAN_POINT('Ctrl Pts',(163.857043496985,-4.61282272980215,331.291302269359));
#23043=CARTESIAN_POINT('Ctrl Pts',(163.864458713012,-4.51264700414154,331.170025871393));
#23044=CARTESIAN_POINT('Ctrl Pts',(163.87187392904,-4.40768583465019,331.0528192155));
#23045=CARTESIAN_POINT('Ctrl Pts',(163.879282010184,-4.30282565826751,330.935725335262));
#23046=CARTESIAN_POINT('Ctrl Pts',(163.886690091328,-4.19318945212747,330.822693677464));
#23047=CARTESIAN_POINT('Ctrl Pts',(163.894098172472,-4.07912762124907,330.714133878425));
#23048=CARTESIAN_POINT('Ctrl Pts',(163.901500739646,-3.96515068867476,330.605654882427));
#23049=CARTESIAN_POINT('Ctrl Pts',(163.908903306821,-3.84675495952377,330.501641373885));
#23050=CARTESIAN_POINT('Ctrl Pts',(163.916305873995,-3.724329161324,330.402467742298));
#23051=CARTESIAN_POINT('Ctrl Pts',(163.923704543749,-3.60196781977197,330.303346325195));
#23052=CARTESIAN_POINT('Ctrl Pts',(163.931103213504,-3.47558092415764,330.209059944536));
#23053=CARTESIAN_POINT('Ctrl Pts',(163.938501883259,-3.34559180536345,330.119944054175));
#23054=CARTESIAN_POINT('Ctrl Pts',(163.945899332463,-3.21562413073736,330.030842865168));
#23055=CARTESIAN_POINT('Ctrl Pts',(163.953296781667,-3.08205571985588,329.946910684414));
#23056=CARTESIAN_POINT('Ctrl Pts',(163.960694230871,-2.94534062713134,329.868440865325));
#23057=CARTESIAN_POINT('Ctrl Pts',(163.968091359334,-2.80863146213506,329.78997444855));
#23058=CARTESIAN_POINT('Ctrl Pts',(163.975488487798,-2.66877621025649,329.716970108311));
#23059=CARTESIAN_POINT('Ctrl Pts',(163.982885616261,-2.52625514223635,329.649676129539));
#23060=CARTESIAN_POINT('Ctrl Pts',(163.990283883698,-2.38371212952913,329.582371789174));
#23061=CARTESIAN_POINT('Ctrl Pts',(163.997682151135,-2.23850282088555,329.520779720343));
#23062=CARTESIAN_POINT('Ctrl Pts',(164.005080418571,-2.09112901432192,329.465100722871));
#23063=CARTESIAN_POINT('Ctrl Pts',(164.012481285097,-1.94370343379014,329.409402164782));
#23064=CARTESIAN_POINT('Ctrl Pts',(164.019882151623,-1.79411219026686,329.359620945821));
#23065=CARTESIAN_POINT('Ctrl Pts',(164.027283018149,-1.64287369468434,329.315908464335));
#23066=CARTESIAN_POINT('Ctrl Pts',(164.034692011533,-1.49146912477484,329.272147982366));
#23067=CARTESIAN_POINT('Ctrl Pts',(164.042101004918,-1.33841404920527,329.234469650033));
#23068=CARTESIAN_POINT('Ctrl Pts',(164.049509998303,-1.18423928171315,329.202974220676));
#23069=CARTESIAN_POINT('Ctrl Pts',(164.056923555883,-1.02996953724637,329.171459389048));
#23070=CARTESIAN_POINT('Ctrl Pts',(164.064337113463,-0.874579093892461,
329.146135109987));
#23071=CARTESIAN_POINT('Ctrl Pts',(164.071750671044,-0.718604892489981,
329.127050351741));
#23072=CARTESIAN_POINT('Ctrl Pts',(164.07917478318,-0.56240863325677,329.107938422847));
#23073=CARTESIAN_POINT('Ctrl Pts',(164.086598895317,-0.405627327088993,
329.095083786511));
#23074=CARTESIAN_POINT('Ctrl Pts',(164.094023007454,-0.248799751770714,
329.088483337923));
#23075=CARTESIAN_POINT('Ctrl Pts',(164.097880132609,-0.167321512411918,
329.085054139142));
#23076=CARTESIAN_POINT('Ctrl Pts',(164.101737257763,-0.0858307416424396,
329.083312225674));
#23077=CARTESIAN_POINT('Ctrl Pts',(164.105594382918,-0.0044024363394424,
329.083251637846));
#23078=CARTESIAN_POINT('Ctrl Pts',(164.113018360356,0.152326183331536,329.083135021805));
#23079=CARTESIAN_POINT('Ctrl Pts',(164.120442337794,0.30929587259952,329.089249901891));
#23080=CARTESIAN_POINT('Ctrl Pts',(164.127866315232,0.465970376285192,329.101627159044));
#23081=CARTESIAN_POINT('Ctrl Pts',(164.135281531259,0.622459980483371,329.113989809172));
#23082=CARTESIAN_POINT('Ctrl Pts',(164.142696747287,0.778654724088107,329.132600096257));
#23083=CARTESIAN_POINT('Ctrl Pts',(164.150111963315,0.934016813004763,329.157436936111));
#23084=CARTESIAN_POINT('Ctrl Pts',(164.157520044459,1.08922941330183,329.182249878082));
#23085=CARTESIAN_POINT('Ctrl Pts',(164.164928125603,1.24361058783445,329.213277387022));
#23086=CARTESIAN_POINT('Ctrl Pts',(164.172336206747,1.3966262404225,329.250446477589));
#23087=CARTESIAN_POINT('Ctrl Pts',(164.179738773921,1.54952800066658,329.287587902525));
#23088=CARTESIAN_POINT('Ctrl Pts',(164.187141341095,1.70106590162092,329.330861719264));
#23089=CARTESIAN_POINT('Ctrl Pts',(164.194543908269,1.85071474839632,329.380143642177));
#23090=CARTESIAN_POINT('Ctrl Pts',(164.201942578024,2.00028480570807,329.429399618372));
#23091=CARTESIAN_POINT('Ctrl Pts',(164.209341247779,2.14796743601218,329.484657284515));
#23092=CARTESIAN_POINT('Ctrl Pts',(164.216739917533,2.29325146037542,329.545742185963));
#23093=CARTESIAN_POINT('Ctrl Pts',(164.224137366737,2.43851151738538,329.606817010298));
#23094=CARTESIAN_POINT('Ctrl Pts',(164.231534815941,2.5813734100781,329.673717017532));
#23095=CARTESIAN_POINT('Ctrl Pts',(164.238932265145,2.72134473641413,329.746219133986));
#23096=CARTESIAN_POINT('Ctrl Pts',(164.246329393609,2.86130999383728,329.818718106875));
#23097=CARTESIAN_POINT('Ctrl Pts',(164.253726522072,2.99838460270778,329.89681853437));
#23098=CARTESIAN_POINT('Ctrl Pts',(164.261123650536,3.1320998728743,329.98025090778));
#23099=CARTESIAN_POINT('Ctrl Pts',(164.268521917972,3.26583573185466,330.063696127694));
#23100=CARTESIAN_POINT('Ctrl Pts',(164.275920185409,3.39621090555928,330.15247473064));
#23101=CARTESIAN_POINT('Ctrl Pts',(164.283318452846,3.52278498543111,330.24627340827));
#23102=CARTESIAN_POINT('Ctrl Pts',(164.290719319371,3.64940353210877,330.340105038362));
#23103=CARTESIAN_POINT('Ctrl Pts',(164.298120185897,3.77221802658342,330.438960032405));
#23104=CARTESIAN_POINT('Ctrl Pts',(164.305521052423,3.89082061285271,330.542484377919));
#23105=CARTESIAN_POINT('Ctrl Pts',(164.312930045808,4.00955343610021,330.646122403061));
#23106=CARTESIAN_POINT('Ctrl Pts',(164.320339039192,4.12406483328007,330.754439773787));
#23107=CARTESIAN_POINT('Ctrl Pts',(164.327748032577,4.23398282498811,330.867044640913));
#23108=CARTESIAN_POINT('Ctrl Pts',(164.335161590157,4.34396852997044,330.979718876522));
#23109=CARTESIAN_POINT('Ctrl Pts',(164.342575147738,4.44935494170331,331.096685594941));
#23110=CARTESIAN_POINT('Ctrl Pts',(164.349988705318,4.54981031224479,331.217519770694));
#23111=CARTESIAN_POINT('Ctrl Pts',(164.357412817455,4.65040869939692,331.338525976018));
#23112=CARTESIAN_POINT('Ctrl Pts',(164.364836929591,4.74606179820977,331.463410339836));
#23113=CARTESIAN_POINT('Ctrl Pts',(164.372261041728,4.83648065601138,331.591718112226));
#23114=CARTESIAN_POINT('Ctrl Pts',(164.376118166883,4.88345689296068,331.658379165736));
#23115=CARTESIAN_POINT('Ctrl Pts',(164.379975292037,4.92902103716036,331.725963844075));
#23116=CARTESIAN_POINT('Ctrl Pts',(164.383832417192,4.97313751511081,331.794405855649));
#23117=CARTESIAN_POINT('Ctrl Pts',(164.39125639463,5.05805042921793,331.926139187957));
#23118=CARTESIAN_POINT('Ctrl Pts',(164.398680372068,5.13785360187958,332.061447460951));
#23119=CARTESIAN_POINT('Ctrl Pts',(164.406104349506,5.21223086620783,332.199896437656));
#23120=CARTESIAN_POINT('Ctrl Pts',(164.413519565533,5.28652035417359,332.338182023739));
#23121=CARTESIAN_POINT('Ctrl Pts',(164.420934781561,5.35539650494734,332.479600610105));
#23122=CARTESIAN_POINT('Ctrl Pts',(164.428349997588,5.41858601743149,332.623688544362));
#23123=CARTESIAN_POINT('Ctrl Pts',(164.435758078733,5.48171472928466,332.767637837934));
#23124=CARTESIAN_POINT('Ctrl Pts',(164.443166159877,5.53916754700382,332.914251026621));
#23125=CARTESIAN_POINT('Ctrl Pts',(164.450574241021,5.59071681542903,333.063039480996));
#23126=CARTESIAN_POINT('Ctrl Pts',(164.457976808195,5.6422277147924,333.211717189408));
#23127=CARTESIAN_POINT('Ctrl Pts',(164.465379375369,5.6878436925393,333.362566588527));
#23128=CARTESIAN_POINT('Ctrl Pts',(164.472781942543,5.7273850500172,333.515078772682));
#23129=CARTESIAN_POINT('Ctrl Pts',(164.480180612297,5.76690558914336,333.667510659839));
#23130=CARTESIAN_POINT('Ctrl Pts',(164.487579282052,5.80035778409847,333.821603228166));
#23131=CARTESIAN_POINT('Ctrl Pts',(164.494977951807,5.82761170926055,333.976832208976));
#23132=CARTESIAN_POINT('Ctrl Pts',(164.502375401011,5.85486113837116,334.132035581823));
#23133=CARTESIAN_POINT('Ctrl Pts',(164.509772850215,5.87591426258902,334.288374627849));
#23134=CARTESIAN_POINT('Ctrl Pts',(164.517170299419,5.8906922023313,334.445314557706));
#23135=CARTESIAN_POINT('Ctrl Pts',(164.524567427882,5.90546950132787,334.602247682921));
#23136=CARTESIAN_POINT('Ctrl Pts',(164.531964556346,5.91397212184771,334.759781268597));
#23137=CARTESIAN_POINT('Ctrl Pts',(164.539361684809,5.91617306436292,334.917375336572));
#23138=CARTESIAN_POINT('Ctrl Pts',(164.546759952246,5.91837434576833,335.074993670098));
#23139=CARTESIAN_POINT('Ctrl Pts',(164.554158219683,5.91427201195984,335.232672131268));
#23140=CARTESIAN_POINT('Ctrl Pts',(164.561556487119,5.90389120027205,335.389870822004));
#23141=CARTESIAN_POINT('Ctrl Pts',(164.568957353645,5.89350674169596,335.547124738293));
#23142=CARTESIAN_POINT('Ctrl Pts',(164.576358220171,5.87683943828142,335.703898176403));
#23143=CARTESIAN_POINT('Ctrl Pts',(164.583759086696,5.85396627238938,335.859656585055));
#23144=CARTESIAN_POINT('Ctrl Pts',(164.591168080081,5.83106798957435,336.01558603133));
#23145=CARTESIAN_POINT('Ctrl Pts',(164.598577073466,5.8019502893581,336.170497852761));
#23146=CARTESIAN_POINT('Ctrl Pts',(164.605986066851,5.76674138667862,336.323867191854));
#23147=CARTESIAN_POINT('Ctrl Pts',(164.613399624431,5.7315107941005,336.477331011751));
#23148=CARTESIAN_POINT('Ctrl Pts',(164.620813182011,5.69018161966588,336.629250096583));
#23149=CARTESIAN_POINT('Ctrl Pts',(164.628226739592,5.64293174851916,336.779115466757));
#23150=CARTESIAN_POINT('Ctrl Pts',(164.635650851728,5.59561460853084,336.929194197721));
#23151=CARTESIAN_POINT('Ctrl Pts',(164.643074963865,5.54236006304602,337.077213024308));
#23152=CARTESIAN_POINT('Ctrl Pts',(164.650499076002,5.48339415210699,337.222682868773));
#23153=CARTESIAN_POINT('Ctrl Pts',(164.654356201156,5.4527589873675,337.298260309686));
#23154=CARTESIAN_POINT('Ctrl Pts',(164.658213326311,5.42058296239184,337.373150118072));
#23155=CARTESIAN_POINT('Ctrl Pts',(164.662070451466,5.38690257233349,337.447286505231));
#23156=CARTESIAN_POINT('Ctrl Pts',(164.669494428904,5.32207645291337,337.58998005121));
#23157=CARTESIAN_POINT('Ctrl Pts',(164.676918406342,5.25147891531012,337.730311312131));
#23158=CARTESIAN_POINT('Ctrl Pts',(164.68434238378,5.17530402261369,337.86777942597));
#23159=CARTESIAN_POINT('Ctrl Pts',(164.691757599807,5.09921902775163,338.005085306752));
#23160=CARTESIAN_POINT('Ctrl Pts',(164.699172815835,5.01756995873937,338.139534443025));
#23161=CARTESIAN_POINT('Ctrl Pts',(164.706588031863,4.93059881185969,338.270646101153));
#23162=CARTESIAN_POINT('Ctrl Pts',(164.713996113007,4.84371134817957,338.401631604304));
#23163=CARTESIAN_POINT('Ctrl Pts',(164.721404194151,4.75151220626657,338.529285713488));
#23164=CARTESIAN_POINT('Ctrl Pts',(164.728812275295,4.65428908776097,338.653152563205));
#23165=CARTESIAN_POINT('Ctrl Pts',(164.736214842469,4.55713833419801,338.776927216563));
#23166=CARTESIAN_POINT('Ctrl Pts',(164.743617409643,4.45497127925033,338.896919931025));
#23167=CARTESIAN_POINT('Ctrl Pts',(164.751019976817,4.34811862730315,339.0127041961));
#23168=CARTESIAN_POINT('Ctrl Pts',(164.758418646572,4.24132223281057,339.128427501265));
#23169=CARTESIAN_POINT('Ctrl Pts',(164.765817316326,4.1298454068607,339.239946496225));
#23170=CARTESIAN_POINT('Ctrl Pts',(164.773215986081,4.0140587079684,339.346868211883));
#23171=CARTESIAN_POINT('Ctrl Pts',(164.780613435285,3.89829111028591,339.453772288779));
#23172=CARTESIAN_POINT('Ctrl Pts',(164.788010884489,3.77821532467789,339.55608033862));
#23173=CARTESIAN_POINT('Ctrl Pts',(164.795408333693,3.65423838064705,339.653436624679));
#23174=CARTESIAN_POINT('Ctrl Pts',(164.802805462157,3.53026681204053,339.75078868954));
#23175=CARTESIAN_POINT('Ctrl Pts',(164.81020259062,3.4023947148572,339.843189187015));
#23176=CARTESIAN_POINT('Ctrl Pts',(164.817599719084,3.27106155726081,339.930323199458));
#23177=CARTESIAN_POINT('Ctrl Pts',(164.82499798652,3.13970817763637,340.017470628363));
#23178=CARTESIAN_POINT('Ctrl Pts',(164.832396253957,3.00489298750044,340.099349751271));
#23179=CARTESIAN_POINT('Ctrl Pts',(164.839794521393,2.86708360191832,340.175689536874));
#23180=CARTESIAN_POINT('Ctrl Pts',(164.847195387919,2.72922580245032,340.252056141447));
#23181=CARTESIAN_POINT('Ctrl Pts',(164.854596254445,2.58837203948197,340.322879353443));
#23182=CARTESIAN_POINT('Ctrl Pts',(164.861997120971,2.44501348816116,340.387934632604));
#23183=CARTESIAN_POINT('Ctrl Pts',(164.869406114355,2.3014975154447,340.453061348681));
#23184=CARTESIAN_POINT('Ctrl Pts',(164.87681510774,2.15547160154408,340.512407328785));
#23185=CARTESIAN_POINT('Ctrl Pts',(164.884224101125,2.00744649478331,340.565796361086));
#23186=CARTESIAN_POINT('Ctrl Pts',(164.891637658705,1.85933019945115,340.619218282873));
#23187=CARTESIAN_POINT('Ctrl Pts',(164.899051216285,1.70921261221028,340.66667583229));
#23188=CARTESIAN_POINT('Ctrl Pts',(164.906464773866,1.55761800871999,340.708043158685));
#23189=CARTESIAN_POINT('Ctrl Pts',(164.913888886002,1.40580758255848,340.749469379042));
#23190=CARTESIAN_POINT('Ctrl Pts',(164.921312998139,1.2525163031314,340.784787975993));
#23191=CARTESIAN_POINT('Ctrl Pts',(164.928737110276,1.09827776958484,340.8139243634));
#23192=CARTESIAN_POINT('Ctrl Pts',(164.93259423543,1.01814464166175,340.829061889708));
#23193=CARTESIAN_POINT('Ctrl Pts',(164.936451360585,0.937755910711731,340.842531556355));
#23194=CARTESIAN_POINT('Ctrl Pts',(164.94030848574,0.857186649477655,340.854328450852));
#23195=CARTESIAN_POINT('Ctrl Pts',(164.947732463178,0.702111469489997,340.877034449511));
#23196=CARTESIAN_POINT('Ctrl Pts',(164.955156440616,0.545899539862234,340.893608771498));
#23197=CARTESIAN_POINT('Ctrl Pts',(164.962580418054,0.38907706482888,340.903943563426));
#23198=CARTESIAN_POINT('Ctrl Pts',(164.969995634081,0.232439663911139,340.914266158745));
#23199=CARTESIAN_POINT('Ctrl Pts',(164.977410850109,0.0751935206070489,
340.918363857034));
#23200=CARTESIAN_POINT('Ctrl Pts',(164.984826066137,-0.0821261478370629,
340.916180005573));
#23201=CARTESIAN_POINT('Ctrl Pts',(164.992234147281,-0.239294444088226,
340.913998255403));
#23202=CARTESIAN_POINT('Ctrl Pts',(164.999642228425,-0.396535753957013,
340.905546993257));
#23203=CARTESIAN_POINT('Ctrl Pts',(165.007050309569,-0.553311038551743,
340.890821458601));
#23204=CARTESIAN_POINT('Ctrl Pts',(165.014452876743,-0.709969632438892,
340.87610688443));
#23205=CARTESIAN_POINT('Ctrl Pts',(165.021855443917,-0.866162521738701,
340.855127371262));
#23206=CARTESIAN_POINT('Ctrl Pts',(165.029258011091,-1.02135208156133,340.82793020617));
#23207=CARTESIAN_POINT('Ctrl Pts',(165.036656680846,-1.1764599347584,340.800747360267));
#23208=CARTESIAN_POINT('Ctrl Pts',(165.0440553506,-1.33056514383375,340.767353446203));
#23209=CARTESIAN_POINT('Ctrl Pts',(165.051454020355,-1.48313672221534,340.727847416414));
#23210=CARTESIAN_POINT('Ctrl Pts',(165.058851469559,-1.63568313102466,340.688347903892));
#23211=CARTESIAN_POINT('Ctrl Pts',(165.066248918763,-1.78669605032176,340.642738370273));
#23212=CARTESIAN_POINT('Ctrl Pts',(165.073646367967,-1.9356560664853,340.591168585795));
#23213=CARTESIAN_POINT('Ctrl Pts',(165.08104349643,-2.08460962400221,340.539601037293));
#23214=CARTESIAN_POINT('Ctrl Pts',(165.088440624894,-2.23151010269279,340.482073873863));
#23215=CARTESIAN_POINT('Ctrl Pts',(165.095837753357,-2.37585486014896,340.418786233651));
#23216=CARTESIAN_POINT('Ctrl Pts',(165.103236020794,-2.52022184309527,340.355488848722));
#23217=CARTESIAN_POINT('Ctrl Pts',(165.110634288231,-2.66203197944046,340.286429370809));
#23218=CARTESIAN_POINT('Ctrl Pts',(165.118032555667,-2.80080429983198,340.211854356805));
#23219=CARTESIAN_POINT('Ctrl Pts',(165.125433422193,-2.93962537239833,340.137253143813));
#23220=CARTESIAN_POINT('Ctrl Pts',(165.132834288719,-3.07540617564299,340.057132713396));
#23221=CARTESIAN_POINT('Ctrl Pts',(165.140235155245,-3.20769208581463,339.971784593594));
#23222=CARTESIAN_POINT('Ctrl Pts',(165.147644148629,-3.3401232585626,339.886342753398));
#23223=CARTESIAN_POINT('Ctrl Pts',(165.155053142014,-3.46905156029963,339.795661962178));
#23224=CARTESIAN_POINT('Ctrl Pts',(165.162462135399,-3.59405241551403,339.700076360767));
#23225=CARTESIAN_POINT('Ctrl Pts',(165.169875692979,-3.71913027556667,339.604431875328));
#23226=CARTESIAN_POINT('Ctrl Pts',(165.177289250559,-3.84027558153471,339.503876796702));
#23227=CARTESIAN_POINT('Ctrl Pts',(165.184702808139,-3.95709878727818,339.398783894467));
#23228=CARTESIAN_POINT('Ctrl Pts',(165.192126920276,-4.07408831224296,339.293541373245));
#23229=CARTESIAN_POINT('Ctrl Pts',(165.199551032413,-4.18674318105786,339.183748385439));
#23230=CARTESIAN_POINT('Ctrl Pts',(165.20697514455,-4.29471191153351,339.069813283117));
#23231=CARTESIAN_POINT('Ctrl Pts',(165.210832269704,-4.35080601390779,339.010619410358));
#23232=CARTESIAN_POINT('Ctrl Pts',(165.214689394859,-4.40563589897465,338.950308020996));
#23233=CARTESIAN_POINT('Ctrl Pts',(165.218546520014,-4.4591568095499,338.888939586873));
#23234=CARTESIAN_POINT('Ctrl Pts',(165.225910699378,-4.56134109692491,338.77177249011));
#23235=CARTESIAN_POINT('Ctrl Pts',(165.233274878743,-4.65907261310312,338.650382016011));
#23236=CARTESIAN_POINT('Ctrl Pts',(165.240639058108,-4.75197758073249,338.52514391688));
#23237=CARTESIAN_POINT('Ctrl Pts',(165.248041664866,-4.84536734042338,338.399252306556));
#23238=CARTESIAN_POINT('Ctrl Pts',(165.255444271623,-4.93387972720829,338.269473038242));
#23239=CARTESIAN_POINT('Ctrl Pts',(165.262846878381,-5.01717244490983,338.136225632912));
#23240=CARTESIAN_POINT('Ctrl Pts',(165.270193032476,-5.09982996802607,338.003994379207));
#23241=CARTESIAN_POINT('Ctrl Pts',(165.277539186571,-5.1773469283478,337.868348013314));
#23242=CARTESIAN_POINT('Ctrl Pts',(165.284885340665,-5.24942928621526,337.7297294246));
#23243=CARTESIAN_POINT('Ctrl Pts',(165.292226440061,-5.32146204607451,337.591206215756));
#23244=CARTESIAN_POINT('Ctrl Pts',(165.299567539457,-5.38806746989197,337.449715189005));
#23245=CARTESIAN_POINT('Ctrl Pts',(165.306908638853,-5.44899585100362,337.305726518528));
#23246=CARTESIAN_POINT('Ctrl Pts',(165.314246194793,-5.50989482275996,337.161807349553));
#23247=CARTESIAN_POINT('Ctrl Pts',(165.321583750734,-5.56512205836557,337.015393285453));
#23248=CARTESIAN_POINT('Ctrl Pts',(165.328921306674,-5.61447478306401,336.866977094889));
#23249=CARTESIAN_POINT('Ctrl Pts',(165.336369666142,-5.66457277717538,336.716319689722));
#23250=CARTESIAN_POINT('Ctrl Pts',(165.343818025611,-5.70861722990409,336.563599560885));
#23251=CARTESIAN_POINT('Ctrl Pts',(165.351266385079,-5.74644758458795,336.409351169895));
#23252=CARTESIAN_POINT('Ctrl Pts',(165.358602757873,-5.78370915689436,336.257421915673));
#23253=CARTESIAN_POINT('Ctrl Pts',(165.365939130667,-5.81494212088197,336.104010418292));
#23254=CARTESIAN_POINT('Ctrl Pts',(165.373275503461,-5.84004403237057,335.94964006996));
#23255=CARTESIAN_POINT('Ctrl Pts',(165.380779856267,-5.86572069919064,335.791735123046));
#23256=CARTESIAN_POINT('Ctrl Pts',(165.388284209072,-5.88498207564688,335.632827293128));
#23257=CARTESIAN_POINT('Ctrl Pts',(165.395788561878,-5.89777443037654,335.473484245669));
#23258=CARTESIAN_POINT('Ctrl Pts',(165.403292914683,-5.9105667851062,335.31414119821));
#23259=CARTESIAN_POINT('Ctrl Pts',(165.410797267489,-5.91689011634911,335.154363357795));
#23260=CARTESIAN_POINT('Ctrl Pts',(165.418301620294,-5.9167476438022,334.994719653312));
#23261=CARTESIAN_POINT('',(167.168301620294,-5.92209282452846,335.000276467281));
#23262=CARTESIAN_POINT('Ctrl Pts',(165.418302861901,-5.9138621938537,334.994695827962));
#23263=CARTESIAN_POINT('Ctrl Pts',(165.44446342603,-5.91863216628149,334.438436333665));
#23264=CARTESIAN_POINT('Ctrl Pts',(165.563370001584,-5.59117675901454,331.91560276841));
#23265=CARTESIAN_POINT('Ctrl Pts',(165.775022588561,-2.00088777716957,328.295593163865));
#23266=CARTESIAN_POINT('Ctrl Pts',(166.053260622836,4.55508355360873,329.689271543295));
#23267=CARTESIAN_POINT('Ctrl Pts',(166.331498657109,6.93092194016336,335.956527041217));
#23268=CARTESIAN_POINT('Ctrl Pts',(166.609736691382,2.94635556247053,341.345991791731));
#23269=CARTESIAN_POINT('Ctrl Pts',(166.887974725657,-3.74203782676519,340.911833541658));
#23270=CARTESIAN_POINT('Ctrl Pts',(167.074163035294,-5.91976887378537,336.990930151837));
#23271=CARTESIAN_POINT('Ctrl Pts',(167.167605333506,-5.92649389691024,335.015000414505));
#23272=CARTESIAN_POINT('Ctrl Pts',(167.168301620294,-5.92648390138188,335.000276672274));
#23273=CARTESIAN_POINT('',(168.91830160198,-5.91441582040877,335.005131115878));
#23274=CARTESIAN_POINT('Ctrl Pts',(167.168301620294,-5.91674999355252,335.000276217856));
#23275=CARTESIAN_POINT('Ctrl Pts',(167.175715681463,-5.9167573005817,334.843755326903));
#23276=CARTESIAN_POINT('Ctrl Pts',(167.183129742633,-5.91054944576592,334.686995018447));
#23277=CARTESIAN_POINT('Ctrl Pts',(167.190543803802,-5.89809535193679,334.530530318379));
#23278=CARTESIAN_POINT('Ctrl Pts',(167.197949113985,-5.88565595796128,334.374250297197));
#23279=CARTESIAN_POINT('Ctrl Pts',(167.205354424167,-5.86698502891278,334.218265559408));
#23280=CARTESIAN_POINT('Ctrl Pts',(167.212759734349,-5.84210345250691,334.063112700104));
#23281=CARTESIAN_POINT('Ctrl Pts',(167.22015792973,-5.8172457815783,333.908108907044));
#23282=CARTESIAN_POINT('Ctrl Pts',(167.227556125111,-5.78618940081505,333.753935768526));
#23283=CARTESIAN_POINT('Ctrl Pts',(167.234954320492,-5.7490071008753,333.601126197048));
#23284=CARTESIAN_POINT('Ctrl Pts',(167.242347031577,-5.71185236424428,333.448429903592));
#23285=CARTESIAN_POINT('Ctrl Pts',(167.249739742662,-5.6685808382736,333.297095526752));
#23286=CARTESIAN_POINT('Ctrl Pts',(167.257132453747,-5.61931661459518,333.147647078056));
#23287=CARTESIAN_POINT('Ctrl Pts',(167.264521306644,-5.57007810146327,332.998276625135));
#23288=CARTESIAN_POINT('Ctrl Pts',(167.27191015954,-5.51485323596182,332.850790494876));
#23289=CARTESIAN_POINT('Ctrl Pts',(167.279299012437,-5.45381627519081,332.705698668665));
#23290=CARTESIAN_POINT('Ctrl Pts',(167.286686699553,-5.39278894456899,332.560629734419));
#23291=CARTESIAN_POINT('Ctrl Pts',(167.294074386668,-5.32595148320592,332.417954699395));
#23292=CARTESIAN_POINT('Ctrl Pts',(167.301462073783,-5.2535267570549,332.278164741317));
#23293=CARTESIAN_POINT('Ctrl Pts',(167.308849493468,-5.18110465263808,332.138379843557));
#23294=CARTESIAN_POINT('Ctrl Pts',(167.316236913154,-5.10309585771362,332.001480147508));
#23295=CARTESIAN_POINT('Ctrl Pts',(167.323624332839,-5.01976965201283,331.867933078105));
#23296=CARTESIAN_POINT('Ctrl Pts',(167.331012953445,-4.93642990055476,331.73436429889));
#23297=CARTESIAN_POINT('Ctrl Pts',(167.338401574051,-4.84777121546881,331.604149549024));
#23298=CARTESIAN_POINT('Ctrl Pts',(167.345790194658,-4.75410664191021,331.477727920809));
#23299=CARTESIAN_POINT('Ctrl Pts',(167.353181484987,-4.6604082246238,331.351260612793));
#23300=CARTESIAN_POINT('Ctrl Pts',(167.360572775316,-4.56170054051903,331.228589455613));
#23301=CARTESIAN_POINT('Ctrl Pts',(167.367964065645,-4.45833728934662,331.110120930296));
#23302=CARTESIAN_POINT('Ctrl Pts',(167.375363486064,-4.35486034321604,330.991522094894));
#23303=CARTESIAN_POINT('Ctrl Pts',(167.382762906482,-4.24671785033054,330.877135404564));
#23304=CARTESIAN_POINT('Ctrl Pts',(167.390162326901,-4.13430126835267,330.767331387293));
#23305=CARTESIAN_POINT('Ctrl Pts',(167.397566391386,-4.0218141308228,330.657458454182));
#23306=CARTESIAN_POINT('Ctrl Pts',(167.404970455872,-3.90504783664909,330.552174174841));
#23307=CARTESIAN_POINT('Ctrl Pts',(167.412374520358,-3.78442693156098,330.451808781265));
#23308=CARTESIAN_POINT('Ctrl Pts',(167.419788972678,-3.66363679646266,330.351302575974));
#23309=CARTESIAN_POINT('Ctrl Pts',(167.427203424997,-3.53898154728273,330.255729264417));
#23310=CARTESIAN_POINT('Ctrl Pts',(167.434617877317,-3.41091529904489,330.165376189894));
#23311=CARTESIAN_POINT('Ctrl Pts',(167.43789551628,-3.35430222677227,330.125434634579));
#23312=CARTESIAN_POINT('Ctrl Pts',(167.441173155242,-3.29702291921798,330.086512609086));
#23313=CARTESIAN_POINT('Ctrl Pts',(167.444450794205,-3.23911807713838,330.048632043076));
#23314=CARTESIAN_POINT('Ctrl Pts',(167.451874771643,-3.10796139818704,329.962831114237));
#23315=CARTESIAN_POINT('Ctrl Pts',(167.459298749081,-2.97319534018959,329.882115658969));
#23316=CARTESIAN_POINT('Ctrl Pts',(167.466722726519,-2.83525199427725,329.806804770525));
#23317=CARTESIAN_POINT('Ctrl Pts',(167.474137942547,-2.69747144226737,329.73158276026));
#23318=CARTESIAN_POINT('Ctrl Pts',(167.481553158574,-2.55652139052194,329.661752798007));
#23319=CARTESIAN_POINT('Ctrl Pts',(167.488968374602,-2.41286363450969,329.597591310928));
#23320=CARTESIAN_POINT('Ctrl Pts',(167.496376455746,-2.26934410526747,329.533491559709));
#23321=CARTESIAN_POINT('Ctrl Pts',(167.50378453689,-2.12312239699419,329.475049576592));
#23322=CARTESIAN_POINT('Ctrl Pts',(167.511192618034,-1.97468558999428,329.422496312581));
#23323=CARTESIAN_POINT('Ctrl Pts',(167.518595185208,-1.82635926722023,329.369982164924));
#23324=CARTESIAN_POINT('Ctrl Pts',(167.525997752382,-1.67582147890356,329.323348133044));
#23325=CARTESIAN_POINT('Ctrl Pts',(167.533400319556,-1.52357990511136,329.282777349513));
#23326=CARTESIAN_POINT('Ctrl Pts',(167.540798989311,-1.37141848584261,329.242227926322));
#23327=CARTESIAN_POINT('Ctrl Pts',(167.548197659066,-1.2175554273154,329.207735489739));
#23328=CARTESIAN_POINT('Ctrl Pts',(167.55559632882,-1.06251410851324,329.179433504227));
#23329=CARTESIAN_POINT('Ctrl Pts',(167.562993778024,-0.907498366714359,
329.151136187665));
#23330=CARTESIAN_POINT('Ctrl Pts',(167.570391227228,-0.751305117202117,
329.129027362314));
#23331=CARTESIAN_POINT('Ctrl Pts',(167.577788676432,-0.59446860423178,329.113189518841));
#23332=CARTESIAN_POINT('Ctrl Pts',(167.585185804896,-0.437638891419135,
329.097352362069));
#23333=CARTESIAN_POINT('Ctrl Pts',(167.592582933359,-0.280166341927268,
329.087785684047));
#23334=CARTESIAN_POINT('Ctrl Pts',(167.599980061823,-0.122590739196191,
329.084520131624));
#23335=CARTESIAN_POINT('Ctrl Pts',(167.607378329259,0.0350091262437524,
329.081254076387));
#23336=CARTESIAN_POINT('Ctrl Pts',(167.614776596696,0.192711703363562,329.08429108631));
#23337=CARTESIAN_POINT('Ctrl Pts',(167.622174864132,0.349976936586156,329.093609672028));
#23338=CARTESIAN_POINT('Ctrl Pts',(167.629575730658,0.507297418738823,329.102931531463));
#23339=CARTESIAN_POINT('Ctrl Pts',(167.636976597184,0.664179878767207,329.118539338334));
#23340=CARTESIAN_POINT('Ctrl Pts',(167.64437746371,0.820089257519572,329.140359723311));
#23341=CARTESIAN_POINT('Ctrl Pts',(167.651786457094,0.976169839675887,329.162204069156));
#23342=CARTESIAN_POINT('Ctrl Pts',(167.659195450479,1.13127483680275,329.190274565255));
#23343=CARTESIAN_POINT('Ctrl Pts',(167.666604443864,1.28487853720021,329.224446545383));
#23344=CARTESIAN_POINT('Ctrl Pts',(167.674018001444,1.43857686277542,329.258639576628));
#23345=CARTESIAN_POINT('Ctrl Pts',(167.681431559024,1.59077168880065,329.298941486346));
#23346=CARTESIAN_POINT('Ctrl Pts',(167.688845116605,1.74095284555439,329.345177831969));
#23347=CARTESIAN_POINT('Ctrl Pts',(167.696269228741,1.8913478126791,329.391480003495));
#23348=CARTESIAN_POINT('Ctrl Pts',(167.703693340878,2.03972303383535,329.443733361146));
#23349=CARTESIAN_POINT('Ctrl Pts',(167.711117453015,2.1855879153784,329.501715174106));
#23350=CARTESIAN_POINT('Ctrl Pts',(167.714974578169,2.26137059395679,329.531839060326));
#23351=CARTESIAN_POINT('Ctrl Pts',(167.718831703324,2.33647606530862,329.563508417066));
#23352=CARTESIAN_POINT('Ctrl Pts',(167.722688828479,2.41083829568462,329.596687194456));
#23353=CARTESIAN_POINT('Ctrl Pts',(167.730112805917,2.55396653197773,329.66054783804));
#23354=CARTESIAN_POINT('Ctrl Pts',(167.737536783355,2.69477152715902,329.73019572702));
#23355=CARTESIAN_POINT('Ctrl Pts',(167.744960760793,2.83275111960009,329.805440186416));
#23356=CARTESIAN_POINT('Ctrl Pts',(167.75237597682,2.97056787536166,329.880595846028));
#23357=CARTESIAN_POINT('Ctrl Pts',(167.759791192848,3.10556554108869,329.96133475216));
#23358=CARTESIAN_POINT('Ctrl Pts',(167.767206408876,3.23726175925666,330.047418161751));
#23359=CARTESIAN_POINT('Ctrl Pts',(167.77461449002,3.36883125998668,330.133418742318));
#23360=CARTESIAN_POINT('Ctrl Pts',(167.782022571164,3.49710532694165,330.224753385844));
#23361=CARTESIAN_POINT('Ctrl Pts',(167.789430652308,3.62162616139335,330.321137476949));
#23362=CARTESIAN_POINT('Ctrl Pts',(167.796833219482,3.74605431271341,330.417449827614));
#23363=CARTESIAN_POINT('Ctrl Pts',(167.804235786656,3.86673450012886,330.518803914882));
#23364=CARTESIAN_POINT('Ctrl Pts',(167.81163835383,3.98323798873801,330.624871923295));
#23365=CARTESIAN_POINT('Ctrl Pts',(167.819037023585,4.09968013877036,330.730884087366));
#23366=CARTESIAN_POINT('Ctrl Pts',(167.826435693339,4.2119496941873,330.841604979195));
#23367=CARTESIAN_POINT('Ctrl Pts',(167.833834363094,4.31965119147316,330.95666670351));
#23368=CARTESIAN_POINT('Ctrl Pts',(167.841231812298,4.42733492135617,331.071709446213));
#23369=CARTESIAN_POINT('Ctrl Pts',(167.848629261502,4.53045183394266,331.191091327964));
#23370=CARTESIAN_POINT('Ctrl Pts',(167.856026710706,4.62864345085063,331.314407731802));
#23371=CARTESIAN_POINT('Ctrl Pts',(167.86342383917,4.72683081034106,331.437718788857));
#23372=CARTESIAN_POINT('Ctrl Pts',(167.870820967633,4.8200930662888,331.56496373684));
#23373=CARTESIAN_POINT('Ctrl Pts',(167.878218096097,4.90811233931278,331.695705245111));
#23374=CARTESIAN_POINT('Ctrl Pts',(167.885616363533,4.99614516510755,331.826466884311));
#23375=CARTESIAN_POINT('Ctrl Pts',(167.89301463097,5.07893319212297,331.960725846181));
#23376=CARTESIAN_POINT('Ctrl Pts',(167.900412898406,5.15620223616344,332.098016357337));
#23377=CARTESIAN_POINT('Ctrl Pts',(167.907813764932,5.2334984256317,332.235355100094));
#23378=CARTESIAN_POINT('Ctrl Pts',(167.915214631458,5.30527158889137,332.375727187546));
#23379=CARTESIAN_POINT('Ctrl Pts',(167.922615497984,5.3712938725684,332.518642972684));
#23380=CARTESIAN_POINT('Ctrl Pts',(167.930024491368,5.437388655025,332.661715693018));
#23381=CARTESIAN_POINT('Ctrl Pts',(167.937433484753,5.49771978986544,332.807337350247));
#23382=CARTESIAN_POINT('Ctrl Pts',(167.944842478138,5.55210761881268,332.954998398137));
#23383=CARTESIAN_POINT('Ctrl Pts',(167.952256035718,5.60652895253851,333.102750410326));
#23384=CARTESIAN_POINT('Ctrl Pts',(167.959669593299,5.65499957015316,333.252543962336));
#23385=CARTESIAN_POINT('Ctrl Pts',(167.967083150879,5.69739008202169,333.403855640683));
#23386=CARTESIAN_POINT('Ctrl Pts',(167.974507263016,5.73984094454449,333.555382738904));
#23387=CARTESIAN_POINT('Ctrl Pts',(167.981931375152,5.77619432725514,333.708431917943));
#23388=CARTESIAN_POINT('Ctrl Pts',(167.989355487289,5.80637204087687,333.862470094713));
#23389=CARTESIAN_POINT('Ctrl Pts',(167.993212612444,5.82205057807774,333.942499129221));
#23390=CARTESIAN_POINT('Ctrl Pts',(167.997069737598,5.83606302045804,334.022795028504));
#23391=CARTESIAN_POINT('Ctrl Pts',(168.000926862753,5.84840394847278,334.103282754717));
#23392=CARTESIAN_POINT('Ctrl Pts',(168.008350840191,5.8721570722303,334.258201000689));
#23393=CARTESIAN_POINT('Ctrl Pts',(168.015774817629,5.8897863387954,334.414297394202));
#23394=CARTESIAN_POINT('Ctrl Pts',(168.023198795067,5.90118034235701,334.571046471656));
#23395=CARTESIAN_POINT('Ctrl Pts',(168.030614011094,5.9125608992801,334.727610561614));
#23396=CARTESIAN_POINT('Ctrl Pts',(168.038029227122,5.91772081371359,334.884825433678));
#23397=CARTESIAN_POINT('Ctrl Pts',(168.04544444315,5.91659981845783,335.042156265546));
#23398=CARTESIAN_POINT('Ctrl Pts',(168.052852524294,5.91547990181807,335.199335714479));
#23399=CARTESIAN_POINT('Ctrl Pts',(168.060260605438,5.90809110953202,335.35663053038));
#23400=CARTESIAN_POINT('Ctrl Pts',(168.067668686582,5.89442503958346,335.51350171882));
#23401=CARTESIAN_POINT('Ctrl Pts',(168.075071253756,5.88076914154034,335.67025614517));
#23402=CARTESIAN_POINT('Ctrl Pts',(168.08247382093,5.8608453013008,335.826587201684));
#23403=CARTESIAN_POINT('Ctrl Pts',(168.089876388104,5.8346971728197,335.981956956282));
#23404=CARTESIAN_POINT('Ctrl Pts',(168.097275057859,5.80856281121377,336.137244909384));
#23405=CARTESIAN_POINT('Ctrl Pts',(168.104673727613,5.7762107496097,336.291572201433));
#23406=CARTESIAN_POINT('Ctrl Pts',(168.112072397368,5.73773635099095,336.444407189478));
#23407=CARTESIAN_POINT('Ctrl Pts',(168.119469846572,5.69926829945352,336.597216964496));
#23408=CARTESIAN_POINT('Ctrl Pts',(168.126867295776,5.65468000643663,336.748534562539));
#23409=CARTESIAN_POINT('Ctrl Pts',(168.13426474498,5.60411772975157,336.897839570033));
#23410=CARTESIAN_POINT('Ctrl Pts',(168.141661873444,5.55355764535874,337.047138103923));
#23411=CARTESIAN_POINT('Ctrl Pts',(168.149059001907,5.49702421202805,337.19442386728));
#23412=CARTESIAN_POINT('Ctrl Pts',(168.15645613037,5.43471316765349,337.339192883846));
#23413=CARTESIAN_POINT('Ctrl Pts',(168.163854397807,5.37239252893368,337.483984191226));
#23414=CARTESIAN_POINT('Ctrl Pts',(168.171252665244,5.30429265540206,337.626257637394));
#23415=CARTESIAN_POINT('Ctrl Pts',(168.17865093268,5.23065684903385,337.765530598304));
#23416=CARTESIAN_POINT('Ctrl Pts',(168.186051799206,5.15699517363221,337.904852487271));
#23417=CARTESIAN_POINT('Ctrl Pts',(168.193452665732,5.07779386756958,338.041171462538));
#23418=CARTESIAN_POINT('Ctrl Pts',(168.200853532257,4.99334138092783,338.17403094125));
#23419=CARTESIAN_POINT('Ctrl Pts',(168.208262525642,4.90879615738172,338.307036312372));
#23420=CARTESIAN_POINT('Ctrl Pts',(168.215671519027,4.81898843797882,338.436574285263));
#23421=CARTESIAN_POINT('Ctrl Pts',(168.223080512412,4.72424948761407,338.56221803674));
#23422=CARTESIAN_POINT('Ctrl Pts',(168.230494069992,4.62945217478809,338.687939189103));
#23423=CARTESIAN_POINT('Ctrl Pts',(168.237907627572,4.52971781363256,338.809761051675));
#23424=CARTESIAN_POINT('Ctrl Pts',(168.245321185152,4.42541653355728,338.927291568883));
#23425=CARTESIAN_POINT('Ctrl Pts',(168.252745297289,4.32096676151517,339.044989412298));
#23426=CARTESIAN_POINT('Ctrl Pts',(168.260169409426,4.21193734304222,339.158383440123));
#23427=CARTESIAN_POINT('Ctrl Pts',(168.267593521562,4.09873424637482,339.267119419479));
#23428=CARTESIAN_POINT('Ctrl Pts',(168.271450646717,4.03992068002348,339.323612138538));
#23429=CARTESIAN_POINT('Ctrl Pts',(168.275307771872,3.97998108188275,339.378848218759));
#23430=CARTESIAN_POINT('Ctrl Pts',(168.279164897027,3.91897562004839,339.43278249545));
#23431=CARTESIAN_POINT('Ctrl Pts',(168.286588874465,3.80155574019379,339.536592156071));
#23432=CARTESIAN_POINT('Ctrl Pts',(168.294012851903,3.67983116042366,339.635889697768));
#23433=CARTESIAN_POINT('Ctrl Pts',(168.301436829341,3.55418346621271,339.730297078514));
#23434=CARTESIAN_POINT('Ctrl Pts',(168.308852045368,3.42868405518537,339.824593044347));
#23435=CARTESIAN_POINT('Ctrl Pts',(168.316267261396,3.29927104100951,339.914010114737));
#23436=CARTESIAN_POINT('Ctrl Pts',(168.323682477424,3.16636155312993,339.998208186677));
#23437=CARTESIAN_POINT('Ctrl Pts',(168.331090558568,3.03357995009088,340.082325243654));
#23438=CARTESIAN_POINT('Ctrl Pts',(168.338498639712,2.89730888418641,340.161233101047));
#23439=CARTESIAN_POINT('Ctrl Pts',(168.345906720856,2.75799706051858,340.234633012607));
#23440=CARTESIAN_POINT('Ctrl Pts',(168.35330928803,2.61878892918522,340.307978291271));
#23441=CARTESIAN_POINT('Ctrl Pts',(168.360711855204,2.47654487540259,340.375823613911));
#23442=CARTESIAN_POINT('Ctrl Pts',(168.368114422378,2.33174088139209,340.437914584153));
#23443=CARTESIAN_POINT('Ctrl Pts',(168.375513092133,2.18701312605077,340.499972863771));
#23444=CARTESIAN_POINT('Ctrl Pts',(168.382911761887,2.03972845684378,340.556282677993));
#23445=CARTESIAN_POINT('Ctrl Pts',(168.390310431642,1.89038555005136,340.60663651708));
#23446=CARTESIAN_POINT('Ctrl Pts',(168.397707880846,1.74106728020185,340.656982049348));
#23447=CARTESIAN_POINT('Ctrl Pts',(168.40510533005,1.589691799961,340.701373437403));
#23448=CARTESIAN_POINT('Ctrl Pts',(168.412502779254,1.43677588469872,340.739652046914));
#23449=CARTESIAN_POINT('Ctrl Pts',(168.419899907718,1.28386659960428,340.777928996732));
#23450=CARTESIAN_POINT('Ctrl Pts',(168.427297036181,1.12941737433057,340.810093604364));
#23451=CARTESIAN_POINT('Ctrl Pts',(168.434694164645,0.97395793827043,340.83603773951));
#23452=CARTESIAN_POINT('Ctrl Pts',(168.442092432081,0.818474565337374,340.861985869405));
#23453=CARTESIAN_POINT('Ctrl Pts',(168.449490699518,0.661981040045436,340.881711558275));
#23454=CARTESIAN_POINT('Ctrl Pts',(168.456888966955,0.505014875909126,340.895158228378));
#23455=CARTESIAN_POINT('Ctrl Pts',(168.46428983348,0.347993567909082,340.908609622438));
#23456=CARTESIAN_POINT('Ctrl Pts',(168.471690700006,0.190499662088425,340.915777573982));
#23457=CARTESIAN_POINT('Ctrl Pts',(168.479091566532,0.0330732056023354,
340.916657563656));
#23458=CARTESIAN_POINT('Ctrl Pts',(168.486500559917,-0.124526120183621,
340.917538519643));
#23459=CARTESIAN_POINT('Ctrl Pts',(168.493909553301,-0.282057475293545,
340.912117722452));
#23460=CARTESIAN_POINT('Ctrl Pts',(168.501318546686,-0.438982668565141,
340.900442761285));
#23461=CARTESIAN_POINT('Ctrl Pts',(168.508732104266,-0.596004533168329,
340.888760607939));
#23462=CARTESIAN_POINT('Ctrl Pts',(168.516145661847,-0.752419121938149,
340.870816655879));
#23463=CARTESIAN_POINT('Ctrl Pts',(168.523559219427,-0.907696448716301,
340.846709991054));
#23464=CARTESIAN_POINT('Ctrl Pts',(168.530983331563,-1.06319484119689,340.822569005978));
#23465=CARTESIAN_POINT('Ctrl Pts',(168.5384074437,-1.21755237279293,340.792247856947));
#23466=CARTESIAN_POINT('Ctrl Pts',(168.545831555837,-1.37025146881332,340.755896235576));
#23467=CARTESIAN_POINT('Ctrl Pts',(168.549688680991,-1.44958479696107,340.737010104733));
#23468=CARTESIAN_POINT('Ctrl Pts',(168.553545806146,-1.52847075111401,340.716497030356));
#23469=CARTESIAN_POINT('Ctrl Pts',(168.557402931301,-1.60683879090904,340.694383167871));
#23470=CARTESIAN_POINT('Ctrl Pts',(168.564826908739,-1.75767718374787,340.651819649817));
#23471=CARTESIAN_POINT('Ctrl Pts',(168.572250886177,-1.90705075965012,340.603194451312));
#23472=CARTESIAN_POINT('Ctrl Pts',(168.579674863615,-2.05443511721323,340.54862387549));
#23473=CARTESIAN_POINT('Ctrl Pts',(168.587090079642,-2.20164553905876,340.494117701158));
#23474=CARTESIAN_POINT('Ctrl Pts',(168.59450529567,-2.34687106886702,340.433680244172));
#23475=CARTESIAN_POINT('Ctrl Pts',(168.601920511698,-2.48959997408339,340.367478228325));
#23476=CARTESIAN_POINT('Ctrl Pts',(168.609328592842,-2.63219154626606,340.301339911725));
#23477=CARTESIAN_POINT('Ctrl Pts',(168.616736673986,-2.77229093996604,340.229448234557));
#23478=CARTESIAN_POINT('Ctrl Pts',(168.62414475513,-2.90940411301229,340.152018853778));
#23479=CARTESIAN_POINT('Ctrl Pts',(168.631547322304,-3.04641523022074,340.074647105101));
#23480=CARTESIAN_POINT('Ctrl Pts',(168.638949889478,-3.18044422890968,339.991746042675));
#23481=CARTESIAN_POINT('Ctrl Pts',(168.646352456652,-3.31101960045029,339.90357826163));
#23482=CARTESIAN_POINT('Ctrl Pts',(168.653751126407,-3.44152622462612,339.815456900539));
#23483=CARTESIAN_POINT('Ctrl Pts',(168.661149796161,-3.56858253442073,339.722074551555));
#23484=CARTESIAN_POINT('Ctrl Pts',(168.668548465916,-3.69174416811905,339.623738266777));
#23485=CARTESIAN_POINT('Ctrl Pts',(168.67594591512,-3.81488548397373,339.525418204431));
#23486=CARTESIAN_POINT('Ctrl Pts',(168.683343364324,-3.93413310751987,339.422146060897));
#23487=CARTESIAN_POINT('Ctrl Pts',(168.690740813528,-4.0490739829583,339.314270557467));
#23488=CARTESIAN_POINT('Ctrl Pts',(168.698137941991,-4.16400987476056,339.206399731332));
#23489=CARTESIAN_POINT('Ctrl Pts',(168.705535070455,-4.27463911761045,339.093926197564));
#23490=CARTESIAN_POINT('Ctrl Pts',(168.712932198918,-4.3805841154613,338.977236901401));
#23491=CARTESIAN_POINT('Ctrl Pts',(168.720330466355,-4.48654542619685,338.860529638));
#23492=CARTESIAN_POINT('Ctrl Pts',(168.727728733792,-4.58782080492842,338.739605596047));
#23493=CARTESIAN_POINT('Ctrl Pts',(168.735127001228,-4.68407179482079,338.614886164662));
#23494=CARTESIAN_POINT('Ctrl Pts',(168.742527867754,-4.78035659869837,338.490122918029));
#23495=CARTESIAN_POINT('Ctrl Pts',(168.74992873428,-4.87161327151175,338.361561922517));
#23496=CARTESIAN_POINT('Ctrl Pts',(168.757329600805,-4.95754576233568,338.229654869618));
#23497=CARTESIAN_POINT('Ctrl Pts',(168.76473859419,-5.04357261525004,338.097602970164));
#23498=CARTESIAN_POINT('Ctrl Pts',(168.772147587575,-5.12426340664172,337.962197988463));
#23499=CARTESIAN_POINT('Ctrl Pts',(168.77955658096,-5.199366909167,337.823918254192));
#23500=CARTESIAN_POINT('Ctrl Pts',(168.78697013854,-5.27451667804029,337.685553334835));
#23501=CARTESIAN_POINT('Ctrl Pts',(168.79438369612,-5.34407213498622,337.544310468096));
#23502=CARTESIAN_POINT('Ctrl Pts',(168.8017972537,-5.40782979757288,337.400688951735));
#23503=CARTESIAN_POINT('Ctrl Pts',(168.809221365837,-5.47167823086492,337.256862963851));
#23504=CARTESIAN_POINT('Ctrl Pts',(168.816645477974,-5.52971224715164,337.11065190889));
#23505=CARTESIAN_POINT('Ctrl Pts',(168.824069590111,-5.58177763594187,336.962572033175));
#23506=CARTESIAN_POINT('Ctrl Pts',(168.827926715265,-5.6088277016056,336.885638575946));
#23507=CARTESIAN_POINT('Ctrl Pts',(168.83178384042,-5.63426753600211,336.808200892553));
#23508=CARTESIAN_POINT('Ctrl Pts',(168.835640965575,-5.65808096035101,336.730332456094));
#23509=CARTESIAN_POINT('Ctrl Pts',(168.844722579275,-5.71414974530112,336.546990969619));
#23510=CARTESIAN_POINT('Ctrl Pts',(168.853804192976,-5.76133633025571,336.360814347924));
#23511=CARTESIAN_POINT('Ctrl Pts',(168.862885806677,-5.79939577498008,336.172578017721));
#23512=CARTESIAN_POINT('Ctrl Pts',(168.872121767402,-5.83810206092365,335.981142507441));
#23513=CARTESIAN_POINT('Ctrl Pts',(168.881357728128,-5.86736807475161,335.78757655681));
#23514=CARTESIAN_POINT('Ctrl Pts',(168.890593688854,-5.8869869065239,335.592718925728));
#23515=CARTESIAN_POINT('Ctrl Pts',(168.89982964958,-5.90660573829619,335.397861294646));
#23516=CARTESIAN_POINT('Ctrl Pts',(168.909065610306,-5.91657720739726,335.201711926091));
#23517=CARTESIAN_POINT('Ctrl Pts',(168.918301571032,-5.91674777277373,335.005133797532));
#23518=CARTESIAN_POINT('',(170.668301648409,-5.91237984572483,334.997288801065));
#23519=CARTESIAN_POINT('Ctrl Pts',(168.918301620294,-5.91303584273221,335.005129528958));
#23520=CARTESIAN_POINT('Ctrl Pts',(168.983494080146,-5.90159674938227,333.618433153161));
#23521=CARTESIAN_POINT('Ctrl Pts',(169.141432551421,-4.72234553782323,330.241434468658));
#23522=CARTESIAN_POINT('Ctrl Pts',(169.392117034123,0.909681900777421,328.062774202851));
#23523=CARTESIAN_POINT('Ctrl Pts',(169.670355068396,6.32594224609055,332.010839980807));
#23524=CARTESIAN_POINT('Ctrl Pts',(169.948593102671,5.93697876292119,338.702013788446));
#23525=CARTESIAN_POINT('Ctrl Pts',(170.226831136945,0.0997374986817368,
341.995904184061));
#23526=CARTESIAN_POINT('Ctrl Pts',(170.466733976153,-5.01217502092496,339.300472229507));
#23527=CARTESIAN_POINT('Ctrl Pts',(170.613890803935,-5.90338482414133,336.157054398344));
#23528=CARTESIAN_POINT('Ctrl Pts',(170.668301620294,-5.90816417193379,334.997291333922));
#23529=CARTESIAN_POINT('',(172.418301620294,-5.91993927450693,334.996002217447));
#23530=CARTESIAN_POINT('Ctrl Pts',(170.668301677549,-5.91674937762772,334.997286175768));
#23531=CARTESIAN_POINT('Ctrl Pts',(170.676397060957,-5.91667011842481,334.824483223407));
#23532=CARTESIAN_POINT('Ctrl Pts',(170.684492444364,-5.90901649277877,334.651929759933));
#23533=CARTESIAN_POINT('Ctrl Pts',(170.692587827772,-5.89387862062504,334.48026413647));
#23534=CARTESIAN_POINT('Ctrl Pts',(170.700721293948,-5.87866953602089,334.307790953691));
#23535=CARTESIAN_POINT('Ctrl Pts',(170.708854760125,-5.85590570417694,334.136214224814));
#23536=CARTESIAN_POINT('Ctrl Pts',(170.716988226301,-5.82572901074834,333.966166330677));
#23537=CARTESIAN_POINT('Ctrl Pts',(170.725140880512,-5.7954811260924,333.795717268722));
#23538=CARTESIAN_POINT('Ctrl Pts',(170.733293534724,-5.75778547547219,333.626804490581));
#23539=CARTESIAN_POINT('Ctrl Pts',(170.741446188935,-5.71283407193777,333.460046289979));
#23540=CARTESIAN_POINT('Ctrl Pts',(170.749627290116,-5.66772581994414,333.292706221743));
#23541=CARTESIAN_POINT('Ctrl Pts',(170.757808391298,-5.61531120803269,333.127536016234));
#23542=CARTESIAN_POINT('Ctrl Pts',(170.76598949248,-5.55583196071568,332.965138386329));
#23543=CARTESIAN_POINT('Ctrl Pts',(170.771762063484,-5.51386350551883,332.85055089637));
#23544=CARTESIAN_POINT('Ctrl Pts',(170.777534634488,-5.46837878791062,332.737343328152));
#23545=CARTESIAN_POINT('Ctrl Pts',(170.783307205492,-5.41947643066687,332.625719944921));
#23546=CARTESIAN_POINT('Ctrl Pts',(170.79073118293,-5.35658417752928,332.482163550711));
#23547=CARTESIAN_POINT('Ctrl Pts',(170.798155160368,-5.28788911591296,332.340891247634));
#23548=CARTESIAN_POINT('Ctrl Pts',(170.805579137806,-5.21357852398914,332.202406474003));
#23549=CARTESIAN_POINT('Ctrl Pts',(170.812994353834,-5.13935562974441,332.064085133241));
#23550=CARTESIAN_POINT('Ctrl Pts',(170.820409569861,-5.05953057142885,331.928545099377));
#23551=CARTESIAN_POINT('Ctrl Pts',(170.827824785889,-4.97433882798822,331.796270331806));
#23552=CARTESIAN_POINT('Ctrl Pts',(170.835232867033,-4.88922905561418,331.66412283835));
#23553=CARTESIAN_POINT('Ctrl Pts',(170.842640948177,-4.79876307900438,331.535234668074));
#23554=CARTESIAN_POINT('Ctrl Pts',(170.850049029321,-4.70322241428641,331.410065532039));
#23555=CARTESIAN_POINT('Ctrl Pts',(170.857451596495,-4.60775286223001,331.284989561678));
#23556=CARTESIAN_POINT('Ctrl Pts',(170.864854163669,-4.50721636845959,331.163627409172));
#23557=CARTESIAN_POINT('Ctrl Pts',(170.872256730843,-4.40193784454133,331.046410014266));
#23558=CARTESIAN_POINT('Ctrl Pts',(170.879655400598,-4.29671474930606,330.929254333807));
#23559=CARTESIAN_POINT('Ctrl Pts',(170.887054070353,-4.18675484491862,330.816239341935));
#23560=CARTESIAN_POINT('Ctrl Pts',(170.894452740108,-4.07242334661865,330.707762978537));
#23561=CARTESIAN_POINT('Ctrl Pts',(170.901850189311,-3.95811070946542,330.599304510371));
#23562=CARTESIAN_POINT('Ctrl Pts',(170.909247638515,-3.83942818018199,330.495383441311));
#23563=CARTESIAN_POINT('Ctrl Pts',(170.916645087719,-3.71677794471765,330.396360975037));
#23564=CARTESIAN_POINT('Ctrl Pts',(170.924042216183,-3.59413302715377,330.297342802204));
#23565=CARTESIAN_POINT('Ctrl Pts',(170.931439344646,-3.46752103585102,330.203223044289));
#23566=CARTESIAN_POINT('Ctrl Pts',(170.93883647311,-3.33737714397006,330.114322527898));
#23567=CARTESIAN_POINT('Ctrl Pts',(170.946234740546,-3.20721321317848,330.025408323046));
#23568=CARTESIAN_POINT('Ctrl Pts',(170.953633007983,-3.07351660717547,329.941715170383));
#23569=CARTESIAN_POINT('Ctrl Pts',(170.96103127542,-2.93675123640743,329.863520394476));
#23570=CARTESIAN_POINT('Ctrl Pts',(170.968432141945,-2.79993781852641,329.785298147923));
#23571=CARTESIAN_POINT('Ctrl Pts',(170.975833008471,-2.66005381319633,329.712578309139));
#23572=CARTESIAN_POINT('Ctrl Pts',(170.983233874997,-2.51758731694154,329.645592034214));
#23573=CARTESIAN_POINT('Ctrl Pts',(170.990642868382,-2.37496437885351,329.578532201954));
#23574=CARTESIAN_POINT('Ctrl Pts',(170.998051861766,-2.22975362449477,329.5172186659));
#23575=CARTESIAN_POINT('Ctrl Pts',(171.005460855151,-2.08246337475019,329.461834522577));
#23576=CARTESIAN_POINT('Ctrl Pts',(171.012874412731,-1.93508238913122,329.40641626071));
#23577=CARTESIAN_POINT('Ctrl Pts',(171.020287970312,-1.78561970895525,329.356934787105));
#23578=CARTESIAN_POINT('Ctrl Pts',(171.027701527892,-1.63459786164334,329.313523024472));
#23579=CARTESIAN_POINT('Ctrl Pts',(171.035125640029,-1.48336100708356,329.270049457248));
#23580=CARTESIAN_POINT('Ctrl Pts',(171.042549752165,-1.33056091362334,329.232662947951));
#23581=CARTESIAN_POINT('Ctrl Pts',(171.049973864302,-1.17673012396027,329.20144528543));
#23582=CARTESIAN_POINT('Ctrl Pts',(171.053830989457,-1.09680883539672,329.185226452906));
#23583=CARTESIAN_POINT('Ctrl Pts',(171.057688114612,-1.01660943249272,329.17067187432));
#23584=CARTESIAN_POINT('Ctrl Pts',(171.061545239767,-0.936206914765374,
329.157787476029));
#23585=CARTESIAN_POINT('Ctrl Pts',(171.068969217205,-0.781452673303419,
329.132988311269));
#23586=CARTESIAN_POINT('Ctrl Pts',(171.076393194643,-0.625478940170516,
329.114304904729));
#23587=CARTESIAN_POINT('Ctrl Pts',(171.083817172081,-0.468810414350018,
329.101852209558));
#23588=CARTESIAN_POINT('Ctrl Pts',(171.091232388108,-0.312326780961899,
329.089414210441));
#23589=CARTESIAN_POINT('Ctrl Pts',(171.098647604136,-0.155150355449397,
329.083192315362));
#23590=CARTESIAN_POINT('Ctrl Pts',(171.106062820163,0.00218445923684952,
329.08325040325));
#23591=CARTESIAN_POINT('Ctrl Pts',(171.113470901307,0.15936788715658,329.083308435247));
#23592=CARTESIAN_POINT('Ctrl Pts',(171.120878982452,0.316709030130614,329.089634420447));
#23593=CARTESIAN_POINT('Ctrl Pts',(171.128287063596,0.473668962790444,329.102240401967));
#23594=CARTESIAN_POINT('Ctrl Pts',(171.13568963077,0.630512067305668,329.114837000625));
#23595=CARTESIAN_POINT('Ctrl Pts',(171.143092197944,0.786974156057978,329.133704258609));
#23596=CARTESIAN_POINT('Ctrl Pts',(171.150494765118,0.942517014330444,329.158802157074));
#23597=CARTESIAN_POINT('Ctrl Pts',(171.157893434872,1.09797797996798,329.183886841606));
#23598=CARTESIAN_POINT('Ctrl Pts',(171.165292104627,1.25252031146456,329.215195574197));
#23599=CARTESIAN_POINT('Ctrl Pts',(171.172690774382,1.40561173375845,329.252636585666));
#23600=CARTESIAN_POINT('Ctrl Pts',(171.180088223586,1.55867790072137,329.290071420531));
#23601=CARTESIAN_POINT('Ctrl Pts',(171.18748567279,1.71029327134949,329.333636437929));
#23602=CARTESIAN_POINT('Ctrl Pts',(171.194883121994,1.85993645587018,329.383188899151));
#23603=CARTESIAN_POINT('Ctrl Pts',(171.202280250457,2.00957315212322,329.432739211864));
#23604=CARTESIAN_POINT('Ctrl Pts',(171.20967737892,2.15723747799994,329.4882763349));
#23605=CARTESIAN_POINT('Ctrl Pts',(171.217074507384,2.3024241463946,329.549607939552));
#23606=CARTESIAN_POINT('Ctrl Pts',(171.22447277482,2.44763316991191,329.610948987739));
#23607=CARTESIAN_POINT('Ctrl Pts',(171.231871042257,2.59036343251988,329.678086148801));
#23608=CARTESIAN_POINT('Ctrl Pts',(171.239269309694,2.73013067750983,329.750779386783));
#23609=CARTESIAN_POINT('Ctrl Pts',(171.246670176219,2.86994702420269,329.823498162664));
#23610=CARTESIAN_POINT('Ctrl Pts',(171.254071042745,3.00679794987236,329.901776729612));
#23611=CARTESIAN_POINT('Ctrl Pts',(171.261471909271,3.14022493339615,329.985329728668));
#23612=CARTESIAN_POINT('Ctrl Pts',(171.268880902655,3.27379843250413,330.068974476906));
#23613=CARTESIAN_POINT('Ctrl Pts',(171.27628989604,3.40394016441382,330.157905025653));
#23614=CARTESIAN_POINT('Ctrl Pts',(171.283698889425,3.53022107775309,330.25179300107));
#23615=CARTESIAN_POINT('Ctrl Pts',(171.291112447005,3.65657978449077,330.345738814718));
#23616=CARTESIAN_POINT('Ctrl Pts',(171.298526004585,3.77907264369696,330.44464790651));
#23617=CARTESIAN_POINT('Ctrl Pts',(171.305939562166,3.89730510825632,330.548152804098));
#23618=CARTESIAN_POINT('Ctrl Pts',(171.313363674302,4.01570589837432,330.651805059857));
#23619=CARTESIAN_POINT('Ctrl Pts',(171.320787786439,4.12983390988703,330.760065932877));
#23620=CARTESIAN_POINT('Ctrl Pts',(171.328211898576,4.23933217539608,330.872531857282));
#23621=CARTESIAN_POINT('Ctrl Pts',(171.33206902373,4.29622093280032,330.930962432963));
#23622=CARTESIAN_POINT('Ctrl Pts',(171.335926148885,4.35186068719005,330.990527504226));
#23623=CARTESIAN_POINT('Ctrl Pts',(171.339783274039,4.40620586842443,331.05116720947));
#23624=CARTESIAN_POINT('Ctrl Pts',(171.347207251477,4.51080641498988,331.167883101625));
#23625=CARTESIAN_POINT('Ctrl Pts',(171.354631228915,4.61092402691169,331.288934078038));
#23626=CARTESIAN_POINT('Ctrl Pts',(171.362055206353,4.70617809290688,331.413941115885));
#23627=CARTESIAN_POINT('Ctrl Pts',(171.369470422381,4.80131974477244,331.538800626618));
#23628=CARTESIAN_POINT('Ctrl Pts',(171.376885638409,4.89160905170896,331.667606611604));
#23629=CARTESIAN_POINT('Ctrl Pts',(171.384300854436,4.97670310046095,331.799944248554));
#23630=CARTESIAN_POINT('Ctrl Pts',(171.39170893558,5.06171527214768,331.932154550896));
#23631=CARTESIAN_POINT('Ctrl Pts',(171.399117016725,5.14154193692978,332.067889428326));
#23632=CARTESIAN_POINT('Ctrl Pts',(171.406525097869,5.21588132405397,332.206702204224));
#23633=CARTESIAN_POINT('Ctrl Pts',(171.413927665043,5.29016537901464,332.345411659239));
#23634=CARTESIAN_POINT('Ctrl Pts',(171.421330232217,5.35897011327729,332.487194123541));
#23635=CARTESIAN_POINT('Ctrl Pts',(171.428732799391,5.42203792067594,332.6315753444));
#23636=CARTESIAN_POINT('Ctrl Pts',(171.436131469145,5.4850725231496,332.775880549178));
#23637=CARTESIAN_POINT('Ctrl Pts',(171.4435301389,5.54237606518131,332.922781444449));
#23638=CARTESIAN_POINT('Ctrl Pts',(171.450928808655,5.59373767285501,333.071780767189));
#23639=CARTESIAN_POINT('Ctrl Pts',(171.458326257859,5.64509080745834,333.220755509667));
#23640=CARTESIAN_POINT('Ctrl Pts',(171.465723707063,5.69050383164459,333.371827640075));
#23641=CARTESIAN_POINT('Ctrl Pts',(171.473121156267,5.72981462351643,333.524481466522));
#23642=CARTESIAN_POINT('Ctrl Pts',(171.48051828473,5.76912371094086,333.677128674165));
#23643=CARTESIAN_POINT('Ctrl Pts',(171.487915413194,5.80233099905596,333.83135708007));
#23644=CARTESIAN_POINT('Ctrl Pts',(171.495312541657,5.82932478132986,333.986637697428));
#23645=CARTESIAN_POINT('Ctrl Pts',(171.502710809094,5.85632271997239,334.141942224125));
#23646=CARTESIAN_POINT('Ctrl Pts',(171.510109076531,5.87710518388487,334.298298917149));
#23647=CARTESIAN_POINT('Ctrl Pts',(171.517507343967,5.89161196533026,334.455170657474));
#23648=CARTESIAN_POINT('Ctrl Pts',(171.524908210493,5.90612384316053,334.612097508491));
#23649=CARTESIAN_POINT('Ctrl Pts',(171.532309077019,5.91435561459879,334.769539395672));
#23650=CARTESIAN_POINT('Ctrl Pts',(171.539709943545,5.91629911199055,334.926956314716));
#23651=CARTESIAN_POINT('Ctrl Pts',(171.547118936929,5.91824474352825,335.084546092588));
#23652=CARTESIAN_POINT('Ctrl Pts',(171.554527930314,5.91388830650375,335.242110474164));
#23653=CARTESIAN_POINT('Ctrl Pts',(171.561936923699,5.90327375316903,335.399110959065));
#23654=CARTESIAN_POINT('Ctrl Pts',(171.569350481279,5.89265266090333,335.55620816168));
#23655=CARTESIAN_POINT('Ctrl Pts',(171.576764038859,5.87576581023745,335.712740405228));
#23656=CARTESIAN_POINT('Ctrl Pts',(171.58417759644,5.85270870442605,335.86817704625));
#23657=CARTESIAN_POINT('Ctrl Pts',(171.591601708576,5.82961877260337,336.023834979787));
#23658=CARTESIAN_POINT('Ctrl Pts',(171.599025820713,5.80034111052963,336.178393829881));
#23659=CARTESIAN_POINT('Ctrl Pts',(171.60644993285,5.76502190981836,336.33133502238));
#23660=CARTESIAN_POINT('Ctrl Pts',(171.610307058004,5.74667216307458,336.410794129396));
#23661=CARTESIAN_POINT('Ctrl Pts',(171.614164183159,5.72669248759253,336.489816863788));
#23662=CARTESIAN_POINT('Ctrl Pts',(171.618021308314,5.70510856165326,336.568332510104));
#23663=CARTESIAN_POINT('Ctrl Pts',(171.625445285752,5.66356503564055,336.719455007668));
#23664=CARTESIAN_POINT('Ctrl Pts',(171.63286926319,5.61595007162408,336.869153672689));
#23665=CARTESIAN_POINT('Ctrl Pts',(171.640293240628,5.56237642737782,337.016903330021));
#23666=CARTESIAN_POINT('Ctrl Pts',(171.647708456655,5.50886600809237,337.164478620528));
#23667=CARTESIAN_POINT('Ctrl Pts',(171.655123672683,5.44941103214534,337.310109134331));
#23668=CARTESIAN_POINT('Ctrl Pts',(171.662538888711,5.38417476240957,337.453282024214));
#23669=CARTESIAN_POINT('Ctrl Pts',(171.669946969855,5.31900126268406,337.596317153863));
#23670=CARTESIAN_POINT('Ctrl Pts',(171.677355050999,5.24805769724341,337.736899029949));
#23671=CARTESIAN_POINT('Ctrl Pts',(171.684763132143,5.17155638051572,337.874532164657));
#23672=CARTESIAN_POINT('Ctrl Pts',(171.692165699317,5.09511200511524,338.012062856509));
#23673=CARTESIAN_POINT('Ctrl Pts',(171.699568266491,5.01311829581158,338.146648852345));
#23674=CARTESIAN_POINT('Ctrl Pts',(171.706970833665,4.92583465636595,338.277816880279));
#23675=CARTESIAN_POINT('Ctrl Pts',(171.71436950342,4.838596971375,338.40891584882));
#23676=CARTESIAN_POINT('Ctrl Pts',(171.721768173175,4.74607510921836,338.536600123435));
#23677=CARTESIAN_POINT('Ctrl Pts',(171.729166842929,4.64857311300592,338.660423278193));
#23678=CARTESIAN_POINT('Ctrl Pts',(171.736564292133,4.55108720159523,338.784226005976));
#23679=CARTESIAN_POINT('Ctrl Pts',(171.743961741337,4.44862301733904,338.904168585139));
#23680=CARTESIAN_POINT('Ctrl Pts',(171.751359190541,4.3415264830876,339.019835613448));
#23681=CARTESIAN_POINT('Ctrl Pts',(171.758756319005,4.23443459235523,339.135497626637));
#23682=CARTESIAN_POINT('Ctrl Pts',(171.766153447468,4.12271100454429,339.246884183718));
#23683=CARTESIAN_POINT('Ctrl Pts',(171.773550575932,4.00674010513229,339.353615083172));
#23684=CARTESIAN_POINT('Ctrl Pts',(171.780948843368,3.89075134909677,339.46036241652));
#23685=CARTESIAN_POINT('Ctrl Pts',(171.788347110805,3.77051425393001,339.562452412139));
#23686=CARTESIAN_POINT('Ctrl Pts',(171.795745378241,3.64644791261821,339.659543774133));
#23687=CARTESIAN_POINT('Ctrl Pts',(171.803146244767,3.52233798549585,339.756669245344));
#23688=CARTESIAN_POINT('Ctrl Pts',(171.810547111293,3.39439642755439,339.848792356731));
#23689=CARTESIAN_POINT('Ctrl Pts',(171.817947977819,3.26307291994351,339.935614012626));
#23690=CARTESIAN_POINT('Ctrl Pts',(171.825356971203,3.1316052065663,340.022531007));
#23691=CARTESIAN_POINT('Ctrl Pts',(171.832765964588,2.99674843856413,340.104134714079));
#23692=CARTESIAN_POINT('Ctrl Pts',(171.840174957973,2.85897923748019,340.180170680794));
#23693=CARTESIAN_POINT('Ctrl Pts',(171.847588515553,2.72112516581621,340.256253488287));
#23694=CARTESIAN_POINT('Ctrl Pts',(171.855002073133,2.58035541888477,340.3267615541));
#23695=CARTESIAN_POINT('Ctrl Pts',(171.862415630714,2.43716790838336,340.39148802733));
#23696=CARTESIAN_POINT('Ctrl Pts',(171.86983974285,2.29377654424685,340.456306650546));
#23697=CARTESIAN_POINT('Ctrl Pts',(171.877263854987,2.14796088693417,340.515327102267));
#23698=CARTESIAN_POINT('Ctrl Pts',(171.884687967124,2.00023612918477,340.568391687912));
#23699=CARTESIAN_POINT('Ctrl Pts',(171.888545092278,1.92348717003776,340.595960876569));
#23700=CARTESIAN_POINT('Ctrl Pts',(171.892402217433,1.8462231179741,340.621923277112));
#23701=CARTESIAN_POINT('Ctrl Pts',(171.896259342588,1.76851733511725,340.646262214766));
#23702=CARTESIAN_POINT('Ctrl Pts',(171.903683320026,1.61895361716687,340.693108432288));
#23703=CARTESIAN_POINT('Ctrl Pts',(171.911107297464,1.46730162689439,340.734078530576));
#23704=CARTESIAN_POINT('Ctrl Pts',(171.918531274902,1.31406401498585,340.768983127642));
#23705=CARTESIAN_POINT('Ctrl Pts',(171.925946490929,1.16100724651521,340.803846532032));
#23706=CARTESIAN_POINT('Ctrl Pts',(171.933361706957,1.00636894155728,340.832658601637));
#23707=CARTESIAN_POINT('Ctrl Pts',(171.940776922984,0.850668715184559,340.855279096636));
#23708=CARTESIAN_POINT('Ctrl Pts',(171.948185004129,0.695118302785645,340.877877826309));
#23709=CARTESIAN_POINT('Ctrl Pts',(171.955593085273,0.538508370001836,340.894296788351));
#23710=CARTESIAN_POINT('Ctrl Pts',(171.963001166417,0.381370478625698,340.904446385609));
#23711=CARTESIAN_POINT('Ctrl Pts',(171.970403733591,0.22434954785202,340.914588428336));
#23712=CARTESIAN_POINT('Ctrl Pts',(171.977806300765,0.0668018117849019,
340.918470373814));
#23713=CARTESIAN_POINT('Ctrl Pts',(171.985208867939,-0.0907343668901057,
340.916054245624));
#23714=CARTESIAN_POINT('Ctrl Pts',(171.992607537694,-0.2481876034558,340.913639389515));
#23715=CARTESIAN_POINT('Ctrl Pts',(172.000006207448,-0.405628922520294,
340.904933069276));
#23716=CARTESIAN_POINT('Ctrl Pts',(172.007404877203,-0.562518379822016,
340.889949374559));
#23717=CARTESIAN_POINT('Ctrl Pts',(172.014802326407,-0.719381955234808,
340.874968151685));
#23718=CARTESIAN_POINT('Ctrl Pts',(172.022199775611,-0.875693478410385,
340.853711645055));
#23719=CARTESIAN_POINT('Ctrl Pts',(172.029597224815,-1.03091643004478,340.82624595059));
#23720=CARTESIAN_POINT('Ctrl Pts',(172.036994353278,-1.18613265148262,340.798781446989));
#23721=CARTESIAN_POINT('Ctrl Pts',(172.044391481742,-1.340260027723,340.765108355876));
#23722=CARTESIAN_POINT('Ctrl Pts',(172.051788610205,-1.49277082615823,340.725344166342));
#23723=CARTESIAN_POINT('Ctrl Pts',(172.059186877642,-1.64530510744938,340.685573854116));
#23724=CARTESIAN_POINT('Ctrl Pts',(172.066585145079,-1.79622195415762,340.639710670196));
#23725=CARTESIAN_POINT('Ctrl Pts',(172.073983412515,-1.9450075680211,340.587922344024));
#23726=CARTESIAN_POINT('Ctrl Pts',(172.081384279041,-2.0938454518356,340.536115824068));
#23727=CARTESIAN_POINT('Ctrl Pts',(172.088785145567,-2.24055025984838,340.478380140076));
#23728=CARTESIAN_POINT('Ctrl Pts',(172.096186012093,-2.38462712785935,340.414931580692));
#23729=CARTESIAN_POINT('Ctrl Pts',(172.103595005477,-2.52886220604546,340.351413348724));
#23730=CARTESIAN_POINT('Ctrl Pts',(172.111003998862,-2.67046323951235,340.282169863788));
#23731=CARTESIAN_POINT('Ctrl Pts',(172.118412992247,-2.80895832598085,340.207464227952));
#23732=CARTESIAN_POINT('Ctrl Pts',(172.125826549827,-2.94753873019977,340.132712570868));
#23733=CARTESIAN_POINT('Ctrl Pts',(172.133240107407,-3.08300905439576,340.052492247645));
#23734=CARTESIAN_POINT('Ctrl Pts',(172.140653664988,-3.21492590464417,339.967110023962));
#23735=CARTESIAN_POINT('Ctrl Pts',(172.148077777124,-3.34703056267942,339.881606243053));
#23736=CARTESIAN_POINT('Ctrl Pts',(172.155501889261,-3.47557133875071,339.790926098998));
#23737=CARTESIAN_POINT('Ctrl Pts',(172.162926001398,-3.60013682376539,339.695417490774));
#23738=CARTESIAN_POINT('Ctrl Pts',(172.166783126552,-3.66485360831885,339.645796923563));
#23739=CARTESIAN_POINT('Ctrl Pts',(172.170640251707,-3.72849795680047,339.594873678482));
#23740=CARTESIAN_POINT('Ctrl Pts',(172.174497376862,-3.79101614658229,339.54270042363));
#23741=CARTESIAN_POINT('Ctrl Pts',(172.181818212763,-3.9096758710846,339.443675418768));
#23742=CARTESIAN_POINT('Ctrl Pts',(172.189139048664,-4.02465609841748,339.339828283579));
#23743=CARTESIAN_POINT('Ctrl Pts',(172.196459884565,-4.1355316721976,339.231466453932));
#23744=CARTESIAN_POINT('Ctrl Pts',(172.203772028285,-4.24627560109991,339.123233284541));
#23745=CARTESIAN_POINT('Ctrl Pts',(172.211084172005,-4.35292430052376,339.010496351369));
#23746=CARTESIAN_POINT('Ctrl Pts',(172.218396315725,-4.45508423787825,338.893604370748));
#23747=CARTESIAN_POINT('Ctrl Pts',(172.225701478377,-4.55714664083613,338.776823989538));
#23748=CARTESIAN_POINT('Ctrl Pts',(172.233006641028,-4.65472855823844,338.655896742196));
#23749=CARTESIAN_POINT('Ctrl Pts',(172.24031180368,-4.74747221290994,338.531209162617));
#23750=CARTESIAN_POINT('Ctrl Pts',(172.247728046039,-4.84162609463798,338.404625628009));
#23751=CARTESIAN_POINT('Ctrl Pts',(172.255144288398,-4.93079307559503,338.274166738327));
#23752=CARTESIAN_POINT('Ctrl Pts',(172.262560530756,-5.01463975739856,338.140273661008));
#23753=CARTESIAN_POINT('Ctrl Pts',(172.269857201924,-5.09713458914619,338.008539325813));
#23754=CARTESIAN_POINT('Ctrl Pts',(172.277153873091,-5.17447917821394,337.873481047779));
#23755=CARTESIAN_POINT('Ctrl Pts',(172.284450544259,-5.24639872171483,337.735549490557));
#23756=CARTESIAN_POINT('Ctrl Pts',(172.291745787673,-5.31830419258919,337.597644922652));
#23757=CARTESIAN_POINT('Ctrl Pts',(172.299041031088,-5.38478655221305,337.456868534898));
#23758=CARTESIAN_POINT('Ctrl Pts',(172.306336274503,-5.44561666873498,337.313696103575));
#23759=CARTESIAN_POINT('Ctrl Pts',(172.31363162386,-5.50644766864442,337.170521593071));
#23760=CARTESIAN_POINT('Ctrl Pts',(172.320926973218,-5.56162611251567,337.024951323964));
#23761=CARTESIAN_POINT('Ctrl Pts',(172.328222322576,-5.61097090855777,336.877481298394));
#23762=CARTESIAN_POINT('Ctrl Pts',(172.335728930719,-5.66174463160155,336.725740834634));
#23763=CARTESIAN_POINT('Ctrl Pts',(172.343235538862,-5.70634157861289,336.571989327393));
#23764=CARTESIAN_POINT('Ctrl Pts',(172.350742147005,-5.74461968890823,336.416783396398));
#23765=CARTESIAN_POINT('Ctrl Pts',(172.358045506196,-5.78186138093522,336.265779821814));
#23766=CARTESIAN_POINT('Ctrl Pts',(172.365348865387,-5.81312196157397,336.113399956991));
#23767=CARTESIAN_POINT('Ctrl Pts',(172.372652224578,-5.83832275100674,335.960165619868));
#23768=CARTESIAN_POINT('Ctrl Pts',(172.380260457197,-5.86457552910289,335.800534626564));
#23769=CARTESIAN_POINT('Ctrl Pts',(172.387868689817,-5.88425161840677,335.6399767522));
#23770=CARTESIAN_POINT('Ctrl Pts',(172.395476922436,-5.89732206354305,335.479085630497));
#23771=CARTESIAN_POINT('Ctrl Pts',(172.403085155055,-5.91039250867933,335.318194508793));
#23772=CARTESIAN_POINT('Ctrl Pts',(172.410693387675,-5.91685735265219,335.156970607304));
#23773=CARTESIAN_POINT('Ctrl Pts',(172.418301620294,-5.91674865086034,334.9960043721));
#23774=CARTESIAN_POINT('',(174.168301620294,-5.92071488197934,335.004845951965));
#23775=CARTESIAN_POINT('Ctrl Pts',(172.418301620294,-5.92297626124348,334.996000166545));
#23776=CARTESIAN_POINT('Ctrl Pts',(172.429779550575,-5.92486170322552,334.752906339495));
#23777=CARTESIAN_POINT('Ctrl Pts',(172.534003492275,-5.80077126720912,332.547462997274));
#23778=CARTESIAN_POINT('Ctrl Pts',(172.730973445414,-3.03182805015908,328.694396016598));
#23779=CARTESIAN_POINT('Ctrl Pts',(173.009211479682,3.66182078960602,329.038146980508));
#23780=CARTESIAN_POINT('Ctrl Pts',(173.287449513959,6.99507073913546,334.853002463598));
#23781=CARTESIAN_POINT('Ctrl Pts',(173.565687548231,3.9090475184357,340.802755416165));
#23782=CARTESIAN_POINT('Ctrl Pts',(173.843925582506,-2.7642509124862,341.427405371847));
#23783=CARTESIAN_POINT('Ctrl Pts',(174.04479693986,-5.75062076917938,337.620117542955));
#23784=CARTESIAN_POINT('Ctrl Pts',(174.152922285789,-5.92360130403154,335.330892503762));
#23785=CARTESIAN_POINT('Ctrl Pts',(174.168301620294,-5.92071488197934,335.004845951965));
#23786=CARTESIAN_POINT('',(175.918301620294,-5.90728851166745,335.001439949397));
#23787=CARTESIAN_POINT('Ctrl Pts',(174.168301620294,-5.92071488197934,335.004845951965));
#23788=CARTESIAN_POINT('Ctrl Pts',(174.245668297214,-5.90619456042088,333.364648957377));
#23789=CARTESIAN_POINT('Ctrl Pts',(174.415780985559,-4.34459534383266,329.7339498889));
#23790=CARTESIAN_POINT('Ctrl Pts',(174.678639685327,1.80894992907605,328.24127799985));
#23791=CARTESIAN_POINT('Ctrl Pts',(174.956877719602,6.66248012508402,332.863652297945));
#23792=CARTESIAN_POINT('Ctrl Pts',(175.235115753876,5.40195064834963,339.446521349778));
#23793=CARTESIAN_POINT('Ctrl Pts',(175.513353788148,-0.815869205717351,
341.948883389464));
#23794=CARTESIAN_POINT('Ctrl Pts',(175.741082410288,-5.29215368564465,338.777712355323));
#23795=CARTESIAN_POINT('Ctrl Pts',(175.876065021004,-5.90924419443841,335.902043646341));
#23796=CARTESIAN_POINT('Ctrl Pts',(175.918301620294,-5.90728851166745,335.001439949397));
#23797=CARTESIAN_POINT('',(177.66830162302,-5.91560657051319,334.994568519548));
#23798=CARTESIAN_POINT('Ctrl Pts',(175.918301620294,-5.90728851166745,335.001439949397));
#23799=CARTESIAN_POINT('Ctrl Pts',(175.968811032428,-5.90494977254684,333.924436495925));
#23800=CARTESIAN_POINT('Ctrl Pts',(176.112066455989,-5.10719719425614,330.866599509878));
#23801=CARTESIAN_POINT('Ctrl Pts',(176.348067890969,-0.194250865120091,
328.006081961981));
#23802=CARTESIAN_POINT('Ctrl Pts',(176.626305925245,5.77621459762169,331.051839942032));
#23803=CARTESIAN_POINT('Ctrl Pts',(176.904543959518,6.44593318097529,337.720766132576));
#23804=CARTESIAN_POINT('Ctrl Pts',(177.182781993793,1.20031402584974,341.892885401616));
#23805=CARTESIAN_POINT('Ctrl Pts',(177.437367880718,-4.60726590443529,339.922557586672));
#23806=CARTESIAN_POINT('Ctrl Pts',(177.599207756218,-5.90217096337117,336.462749761299));
#23807=CARTESIAN_POINT('Ctrl Pts',(177.668301620294,-5.91541773274628,334.994568750865));
#23808=CARTESIAN_POINT('',(179.418302336057,-5.92193779621029,335.001244208886));
#23809=CARTESIAN_POINT('Ctrl Pts',(177.668301639489,-5.91674750571091,334.994567121961));
#23810=CARTESIAN_POINT('Ctrl Pts',(177.677735650211,-5.91656339584637,334.794059844961));
#23811=CARTESIAN_POINT('Ctrl Pts',(177.687169660932,-5.90618360898286,334.594007430929));
#23812=CARTESIAN_POINT('Ctrl Pts',(177.696603671654,-5.88576758330674,334.395293031464));
#23813=CARTESIAN_POINT('Ctrl Pts',(177.706233207941,-5.86492842317771,334.19246015615));
#23814=CARTESIAN_POINT('Ctrl Pts',(177.715862744228,-5.83363270039088,333.991021115608));
#23815=CARTESIAN_POINT('Ctrl Pts',(177.725492280515,-5.79209813957887,333.79189002819));
#23816=CARTESIAN_POINT('Ctrl Pts',(177.730080874457,-5.77230640418817,333.697001585573));
#23817=CARTESIAN_POINT('Ctrl Pts',(177.734669468399,-5.75019049164024,333.602636854439));
#23818=CARTESIAN_POINT('Ctrl Pts',(177.739258062341,-5.72577772529589,333.508893027645));
#23819=CARTESIAN_POINT('Ctrl Pts',(177.746682039777,-5.68627982489756,333.357223025097));
#23820=CARTESIAN_POINT('Ctrl Pts',(177.754106017213,-5.64069180312919,333.206894693222));
#23821=CARTESIAN_POINT('Ctrl Pts',(177.761529994649,-5.5891193117699,333.058434682711));
#23822=CARTESIAN_POINT('Ctrl Pts',(177.768945210675,-5.53760768371,332.91014987735));
#23823=CARTESIAN_POINT('Ctrl Pts',(177.7763604267,-5.48012576550352,332.763729353581));
#23824=CARTESIAN_POINT('Ctrl Pts',(177.783775642726,-5.41682987598247,332.61968811767));
#23825=CARTESIAN_POINT('Ctrl Pts',(177.791183723868,-5.3535948894477,332.475785477511));
#23826=CARTESIAN_POINT('Ctrl Pts',(177.79859180501,-5.28455721769547,332.334257906957));
#23827=CARTESIAN_POINT('Ctrl Pts',(177.805999886152,-5.20992246118055,332.195603717199));
#23828=CARTESIAN_POINT('Ctrl Pts',(177.813402453324,-5.13534325667828,332.057052730288));
#23829=CARTESIAN_POINT('Ctrl Pts',(177.820805020496,-5.05517543868624,331.921371192908));
#23830=CARTESIAN_POINT('Ctrl Pts',(177.828207587668,-4.969671992856,331.78903583858));
#23831=CARTESIAN_POINT('Ctrl Pts',(177.83560625742,-4.88421356421617,331.656770158238));
#23832=CARTESIAN_POINT('Ctrl Pts',(177.843004927173,-4.79342530442435,331.527847464999));
#23833=CARTESIAN_POINT('Ctrl Pts',(177.850403596926,-4.69760519712498,331.402718252007));
#23834=CARTESIAN_POINT('Ctrl Pts',(177.857801046128,-4.60180089716821,331.277609681449));
#23835=CARTESIAN_POINT('Ctrl Pts',(177.86519849533,-4.50096662386682,331.156293645137));
#23836=CARTESIAN_POINT('Ctrl Pts',(177.872595944531,-4.39544265594761,331.039190181191));
#23837=CARTESIAN_POINT('Ctrl Pts',(177.879993072993,-4.28992326336374,330.922091794646));
#23838=CARTESIAN_POINT('Ctrl Pts',(177.887390201454,-4.17971483029927,330.80920589455));
#23839=CARTESIAN_POINT('Ctrl Pts',(177.894787329916,-4.06519657019832,330.700917841196));
#23840=CARTESIAN_POINT('Ctrl Pts',(177.90218559735,-3.95066067714397,330.592613114184));
#23841=CARTESIAN_POINT('Ctrl Pts',(177.909583864785,-3.83181390691669,330.488907899979));
#23842=CARTESIAN_POINT('Ctrl Pts',(177.916982132219,-3.70907070295967,330.390149125737));
#23843=CARTESIAN_POINT('Ctrl Pts',(177.924382998743,-3.58628437802431,330.291355656498));
#23844=CARTESIAN_POINT('Ctrl Pts',(177.931783865266,-3.45959918455769,330.197512320861));
#23845=CARTESIAN_POINT('Ctrl Pts',(177.93918473179,-3.32946072154656,330.108924262887));
#23846=CARTESIAN_POINT('Ctrl Pts',(177.946593725173,-3.19917935406093,330.020238926755));
#23847=CARTESIAN_POINT('Ctrl Pts',(177.954002718555,-3.06543745286287,329.936820603013));
#23848=CARTESIAN_POINT('Ctrl Pts',(177.961411711938,-2.92870815804487,329.858930161192));
#23849=CARTESIAN_POINT('Ctrl Pts',(177.968825269516,-2.79189463326487,329.780991736172));
#23850=CARTESIAN_POINT('Ctrl Pts',(177.976238827094,-2.65209037837958,329.708588149946));
#23851=CARTESIAN_POINT('Ctrl Pts',(177.983652384672,-2.50979046485076,329.641932961875));
#23852=CARTESIAN_POINT('Ctrl Pts',(177.991076496807,-2.36728796134321,329.57518287794));
#23853=CARTESIAN_POINT('Ctrl Pts',(177.998500608942,-2.22228304618235,329.514197681338));
#23854=CARTESIAN_POINT('Ctrl Pts',(178.005924721076,-2.07528873445123,329.459142013085));
#23855=CARTESIAN_POINT('Ctrl Pts',(178.009781846256,-1.99891927090797,329.430538376659));
#23856=CARTESIAN_POINT('Ctrl Pts',(178.013638971435,-1.92201305195829,329.403534422221));
#23857=CARTESIAN_POINT('Ctrl Pts',(178.017496096615,-1.84464320773582,329.378147814229));
#23858=CARTESIAN_POINT('Ctrl Pts',(178.02492007406,-1.69572608636336,329.32928510006));
#23859=CARTESIAN_POINT('Ctrl Pts',(178.032344051506,-1.54464149035693,329.286269753881));
#23860=CARTESIAN_POINT('Ctrl Pts',(178.039768028952,-1.39188946576013,329.249297931765));
#23861=CARTESIAN_POINT('Ctrl Pts',(178.047183244987,-1.23931771153463,329.212369741961));
#23862=CARTESIAN_POINT('Ctrl Pts',(178.054598461023,-1.085082804899,329.181470966271));
#23863=CARTESIAN_POINT('Ctrl Pts',(178.062013677058,-0.929702418700275,
329.156748852294));
#23864=CARTESIAN_POINT('Ctrl Pts',(178.06942175821,-0.774471538726483,329.132050525811));
#23865=CARTESIAN_POINT('Ctrl Pts',(178.076829839362,-0.61809773952573,329.113517087583));
#23866=CARTESIAN_POINT('Ctrl Pts',(178.084237920514,-0.461111323813465,
329.10124530858));
#23867=CARTESIAN_POINT('Ctrl Pts',(178.091640487696,-0.304241755957706,
329.088982663685));
#23868=CARTESIAN_POINT('Ctrl Pts',(178.099043054877,-0.146760849998787,
329.082972426909));
#23869=CARTESIAN_POINT('Ctrl Pts',(178.106445622059,0.0107935936219287,
329.083259845081));
#23870=CARTESIAN_POINT('Ctrl Pts',(178.113844291822,0.168265085516562,329.083547111928));
#23871=CARTESIAN_POINT('Ctrl Pts',(178.121242961584,0.325809665694562,329.090125429655));
#23872=CARTESIAN_POINT('Ctrl Pts',(178.128641631347,0.482887248812271,329.102988005147));
#23873=CARTESIAN_POINT('Ctrl Pts',(178.136039080558,0.639938919005676,329.115848458714));
#23874=CARTESIAN_POINT('Ctrl Pts',(178.14343652977,0.796523373433738,329.134991082086));
#23875=CARTESIAN_POINT('Ctrl Pts',(178.150833978982,0.952103248735099,329.160357034351));
#23876=CARTESIAN_POINT('Ctrl Pts',(178.158231107453,1.10767637836364,329.185721886793));
#23877=CARTESIAN_POINT('Ctrl Pts',(178.165628235924,1.26224464712315,329.217309471555));
#23878=CARTESIAN_POINT('Ctrl Pts',(178.173025364395,1.41527878316743,329.255009440529));
#23879=CARTESIAN_POINT('Ctrl Pts',(178.18042363184,1.5683364826479,329.292715214356));
#23880=CARTESIAN_POINT('Ctrl Pts',(178.187821899284,1.71985921667248,329.33653515708));
#23881=CARTESIAN_POINT('Ctrl Pts',(178.195220166728,1.86933096766575,329.386308496557));
#23882=CARTESIAN_POINT('Ctrl Pts',(178.202621033262,2.01885522965619,329.436099321932));
#23883=CARTESIAN_POINT('Ctrl Pts',(178.210021899795,2.16632672016538,329.491847590378));
#23884=CARTESIAN_POINT('Ctrl Pts',(178.217422766329,2.31124769786232,329.553343719159));
#23885=CARTESIAN_POINT('Ctrl Pts',(178.224831759721,2.45632781264585,329.614907376568));
#23886=CARTESIAN_POINT('Ctrl Pts',(178.232240753113,2.59885147769186,329.682231353241));
#23887=CARTESIAN_POINT('Ctrl Pts',(178.239649746506,2.73834327899274,329.755058947052));
#23888=CARTESIAN_POINT('Ctrl Pts',(178.247063304093,2.87792101205398,329.827931405173));
#23889=CARTESIAN_POINT('Ctrl Pts',(178.254476861681,3.01446283675097,329.906314050916));
#23890=CARTESIAN_POINT('Ctrl Pts',(178.261890419269,3.14752125488427,329.989906137351));
#23891=CARTESIAN_POINT('Ctrl Pts',(178.269314531413,3.28076910603264,330.073617232423));
#23892=CARTESIAN_POINT('Ctrl Pts',(178.276738643557,3.41052333895812,330.162552370178));
#23893=CARTESIAN_POINT('Ctrl Pts',(178.284162755701,3.53636788161693,330.256369241987));
#23894=CARTESIAN_POINT('Ctrl Pts',(178.288019880764,3.60174918648625,330.305110882809));
#23895=CARTESIAN_POINT('Ctrl Pts',(178.291877005826,3.66607575385617,330.355169572337));
#23896=CARTESIAN_POINT('Ctrl Pts',(178.295734130889,3.7292931544016,330.406493373137));
#23897=CARTESIAN_POINT('Ctrl Pts',(178.303158108318,3.85097045217884,330.505278538917));
#23898=CARTESIAN_POINT('Ctrl Pts',(178.310582085748,3.96890351837916,330.609050726683));
#23899=CARTESIAN_POINT('Ctrl Pts',(178.318006063177,4.08265679756999,330.717495588355));
#23900=CARTESIAN_POINT('Ctrl Pts',(178.325421279196,4.19627583077655,330.825812468775));
#23901=CARTESIAN_POINT('Ctrl Pts',(178.332836495216,4.3057246282449,330.938790791468));
#23902=CARTESIAN_POINT('Ctrl Pts',(178.340251711235,4.41059922384577,331.056074918421));
#23903=CARTESIAN_POINT('Ctrl Pts',(178.34765979237,4.51537290963921,331.173246195177));
#23904=CARTESIAN_POINT('Ctrl Pts',(178.355067873506,4.61558090857261,331.294714751858));
#23905=CARTESIAN_POINT('Ctrl Pts',(178.362475954642,4.71085486664632,331.420087013921));
#23906=CARTESIAN_POINT('Ctrl Pts',(178.369878521807,4.80605791057351,331.545365959121));
#23907=CARTESIAN_POINT('Ctrl Pts',(178.377281088973,4.89633400127358,331.674542528359));
#23908=CARTESIAN_POINT('Ctrl Pts',(178.384683656138,4.98135405504422,331.807188959429));
#23909=CARTESIAN_POINT('Ctrl Pts',(178.392082325885,5.06632934612877,331.939765552733));
#23910=CARTESIAN_POINT('Ctrl Pts',(178.399480995631,5.14605391060109,332.075808056136));
#23911=CARTESIAN_POINT('Ctrl Pts',(178.406879665378,5.22024118976822,332.214858624208));
#23912=CARTESIAN_POINT('Ctrl Pts',(178.414277114573,5.2944162303389,332.353886253256));
#23913=CARTESIAN_POINT('Ctrl Pts',(178.421674563769,5.36305562305941,332.495920633145));
#23914=CARTESIAN_POINT('Ctrl Pts',(178.429072012965,5.4259180503607,332.640478041367));
#23915=CARTESIAN_POINT('Ctrl Pts',(178.43646914142,5.48877775205724,332.785029181834));
#23916=CARTESIAN_POINT('Ctrl Pts',(178.443866269875,5.54586083753778,332.932102790871));
#23917=CARTESIAN_POINT('Ctrl Pts',(178.451263398331,5.59697368151684,333.0811940768));
#23918=CARTESIAN_POINT('Ctrl Pts',(178.458661665759,5.64809439559847,333.230308319067));
#23919=CARTESIAN_POINT('Ctrl Pts',(178.466059933188,5.69324291675456,333.381440503752));
#23920=CARTESIAN_POINT('Ctrl Pts',(178.473458200616,5.73227519499158,333.534069697638));
#23921=CARTESIAN_POINT('Ctrl Pts',(178.480859067134,5.77132118567885,333.686752511766));
#23922=CARTESIAN_POINT('Ctrl Pts',(178.488259933652,5.80424656297964,333.840933020843));
#23923=CARTESIAN_POINT('Ctrl Pts',(178.495660800169,5.83095821309311,333.996079246324));
#23924=CARTESIAN_POINT('Ctrl Pts',(178.503069793546,5.85769919515275,334.151395837196));
#23925=CARTESIAN_POINT('Ctrl Pts',(178.510478786923,5.878212760235,334.307679894225));
#23926=CARTESIAN_POINT('Ctrl Pts',(178.5178877803,5.89245750083646,334.464392715382));
#23927=CARTESIAN_POINT('Ctrl Pts',(178.525301337873,5.90671101668964,334.621202077044));
#23928=CARTESIAN_POINT('Ctrl Pts',(178.532714895445,5.91468799402555,334.778440357292));
#23929=CARTESIAN_POINT('Ctrl Pts',(178.540128453017,5.91639917040129,334.935568493927));
#23930=CARTESIAN_POINT('Ctrl Pts',(178.547552565147,5.91811278294993,335.092920331234));
#23931=CARTESIAN_POINT('Ctrl Pts',(178.554976677276,5.91354278929872,335.250161339698));
#23932=CARTESIAN_POINT('Ctrl Pts',(178.562400789405,5.90275188361823,335.406756392625));
#23933=CARTESIAN_POINT('Ctrl Pts',(178.566257914657,5.89714557352008,335.488113829391));
#23934=CARTESIAN_POINT('Ctrl Pts',(178.57011503991,5.88986094992002,335.569297045502));
#23935=CARTESIAN_POINT('Ctrl Pts',(178.573972165163,5.88091223328538,335.650232163842));
#23936=CARTESIAN_POINT('Ctrl Pts',(178.58139614259,5.86368824755755,335.806011520824));
#23937=CARTESIAN_POINT('Ctrl Pts',(178.588820120018,5.84024435010495,335.96134103735));
#23938=CARTESIAN_POINT('Ctrl Pts',(178.596244097446,5.81060917889468,336.115684333781));
#23939=CARTESIAN_POINT('Ctrl Pts',(178.603659313463,5.78100898164574,336.269845481898));
#23940=CARTESIAN_POINT('Ctrl Pts',(178.61107452948,5.74523212430144,336.423022363707));
#23941=CARTESIAN_POINT('Ctrl Pts',(178.618489745497,5.70335906120161,336.574682819335));
#23942=CARTESIAN_POINT('Ctrl Pts',(178.625897826631,5.66152628815285,336.726197348035));
#23943=CARTESIAN_POINT('Ctrl Pts',(178.633305907764,5.61360908560313,336.876197997999));
#23944=CARTESIAN_POINT('Ctrl Pts',(178.640713988898,5.55973908129434,337.024162026723));
#23945=CARTESIAN_POINT('Ctrl Pts',(178.648116556061,5.50590917341429,337.172015923117));
#23946=CARTESIAN_POINT('Ctrl Pts',(178.655519123224,5.44613541323306,337.317835867448));
#23947=CARTESIAN_POINT('Ctrl Pts',(178.662921690388,5.38059942904098,337.461113639535));
#23948=CARTESIAN_POINT('Ctrl Pts',(178.670320360132,5.31509794925878,337.6043159765));
#23949=CARTESIAN_POINT('Ctrl Pts',(178.677719029876,5.24384044227906,337.744978468271));
#23950=CARTESIAN_POINT('Ctrl Pts',(178.68511769962,5.16705684673975,337.882612375097));
#23951=CARTESIAN_POINT('Ctrl Pts',(178.692515148813,5.09028591811017,338.0202235766));
#23952=CARTESIAN_POINT('Ctrl Pts',(178.699912598006,5.00799089186809,338.154806859141));
#23953=CARTESIAN_POINT('Ctrl Pts',(178.707310047199,4.92044794980542,338.285897523624));
#23954=CARTESIAN_POINT('Ctrl Pts',(178.714707175652,4.83290880345264,338.416982504242));
#23955=CARTESIAN_POINT('Ctrl Pts',(178.722104304105,4.74012240096959,338.544574857535));
#23956=CARTESIAN_POINT('Ctrl Pts',(178.729501432557,4.64240845069552,338.668238588125));
#23957=CARTESIAN_POINT('Ctrl Pts',(178.736899699983,4.54467945491274,338.791921359843));
#23958=CARTESIAN_POINT('Ctrl Pts',(178.744297967409,4.44202163202471,338.911674011555));
#23959=CARTESIAN_POINT('Ctrl Pts',(178.751696234834,4.33479509217015,339.027093501695));
#23960=CARTESIAN_POINT('Ctrl Pts',(178.759097101349,4.22753088250479,339.142553539916));
#23961=CARTESIAN_POINT('Ctrl Pts',(178.766497967864,4.11569501410163,339.253677112442));
#23962=CARTESIAN_POINT('Ctrl Pts',(178.773898834379,3.99968444984814,339.360098033777));
#23963=CARTESIAN_POINT('Ctrl Pts',(178.781307827753,3.88354649490353,339.466635815457));
#23964=CARTESIAN_POINT('Ctrl Pts',(178.788716821127,3.76322496437232,339.568460380802));
#23965=CARTESIAN_POINT('Ctrl Pts',(178.796125814501,3.63915045630747,339.665245386778));
#23966=CARTESIAN_POINT('Ctrl Pts',(178.80353937207,3.51499951406585,339.762090015657));
#23967=CARTESIAN_POINT('Ctrl Pts',(178.81095292964,3.38709128989435,339.853888681856));
#23968=CARTESIAN_POINT('Ctrl Pts',(178.818366487209,3.25588490340638,339.940358697329));
#23969=CARTESIAN_POINT('Ctrl Pts',(178.825790599335,3.12449172060499,340.0269518187));
#23970=CARTESIAN_POINT('Ctrl Pts',(178.833214711461,2.989791316273,340.108200945721));
#23971=CARTESIAN_POINT('Ctrl Pts',(178.840638823587,2.85226761727777,340.183869211499));
#23972=CARTESIAN_POINT('Ctrl Pts',(178.84449594887,2.78081851636686,340.223181923394));
#23973=CARTESIAN_POINT('Ctrl Pts',(178.848353074153,2.70860768957039,340.260989024843));
#23974=CARTESIAN_POINT('Ctrl Pts',(178.852210199437,2.6357049572448,340.297262494993));
#23975=CARTESIAN_POINT('Ctrl Pts',(178.859634176926,2.49538588437414,340.367079627202));
#23976=CARTESIAN_POINT('Ctrl Pts',(178.867058154416,2.35207914078279,340.431422868358));
#23977=CARTESIAN_POINT('Ctrl Pts',(178.874482131905,2.20625127720746,340.49002603494));
#23978=CARTESIAN_POINT('Ctrl Pts',(178.881897347984,2.06059551244881,340.54856004097));
#23979=CARTESIAN_POINT('Ctrl Pts',(178.889312564064,1.91242489301706,340.601367318671));
#23980=CARTESIAN_POINT('Ctrl Pts',(178.896727780143,1.76223046197014,340.648227541575));
#23981=CARTESIAN_POINT('Ctrl Pts',(178.904135861339,1.61218054724618,340.695042675809));
#23982=CARTESIAN_POINT('Ctrl Pts',(178.911543942534,1.46011105151351,340.735922036717));
#23983=CARTESIAN_POINT('Ctrl Pts',(178.91895202373,1.30653279142841,340.770693426913));
#23984=CARTESIAN_POINT('Ctrl Pts',(178.926354590956,1.15306884244633,340.805438936129));
#23985=CARTESIAN_POINT('Ctrl Pts',(178.933757158182,0.998098727609406,340.834085444868));
#23986=CARTESIAN_POINT('Ctrl Pts',(178.941159725407,0.842148109607813,340.856510661135));
#23987=CARTESIAN_POINT('Ctrl Pts',(178.948558395214,0.686279598925004,340.878924070623));
#23988=CARTESIAN_POINT('Ctrl Pts',(178.95595706502,0.529431981662636,340.895122657971));
#23989=CARTESIAN_POINT('Ctrl Pts',(178.963355734827,0.372140682503567,340.905035298364));
#23990=CARTESIAN_POINT('Ctrl Pts',(178.970753184082,0.214875331529375,340.914946303479));
#23991=CARTESIAN_POINT('Ctrl Pts',(178.978150633337,0.0571668160346099,
340.918573396271));
#23992=CARTESIAN_POINT('Ctrl Pts',(178.985548082593,-0.100444630773965,
340.915897348556));
#23993=CARTESIAN_POINT('Ctrl Pts',(178.992945211107,-0.258049243821911,
340.91322141687));
#23994=CARTESIAN_POINT('Ctrl Pts',(179.000342339622,-0.4155564233945,340.90424289441));
#23995=CARTESIAN_POINT('Ctrl Pts',(179.007739468137,-0.572426519144063,
340.888994688627));
#23996=CARTESIAN_POINT('Ctrl Pts',(179.015137735625,-0.729320768968311,
340.873744135002));
#23997=CARTESIAN_POINT('Ctrl Pts',(179.022536003112,-0.885577368166346,
340.852222011973));
#23998=CARTESIAN_POINT('Ctrl Pts',(179.0299342706,-1.04066251421858,340.824513034924));
#23999=CARTESIAN_POINT('Ctrl Pts',(179.037335137177,-1.1958021433088,340.79679432342));
#24000=CARTESIAN_POINT('Ctrl Pts',(179.044736003753,-1.34976913270849,340.762884496048));
#24001=CARTESIAN_POINT('Ctrl Pts',(179.05213687033,-1.50204072981682,340.722919203385));
#24002=CARTESIAN_POINT('Ctrl Pts',(179.059545863765,-1.65447953568255,340.682910025013));
#24003=CARTESIAN_POINT('Ctrl Pts',(179.0669548572,-1.80521887013696,340.636832196786));
#24004=CARTESIAN_POINT('Ctrl Pts',(179.074363850635,-1.95375128304053,340.584871214855));
#24005=CARTESIAN_POINT('Ctrl Pts',(179.081777408265,-2.10237519702791,340.532878223169));
#24006=CARTESIAN_POINT('Ctrl Pts',(179.089190965895,-2.24878913413984,340.474994992921));
#24007=CARTESIAN_POINT('Ctrl Pts',(179.096604523526,-2.39250691999123,340.411454628868));
#24008=CARTESIAN_POINT('Ctrl Pts',(179.104028635712,-2.53642931440393,340.347823803482));
#24009=CARTESIAN_POINT('Ctrl Pts',(179.111452747897,-2.67764755723836,340.278519922891));
#24010=CARTESIAN_POINT('Ctrl Pts',(179.118876860083,-2.81570058146565,340.203821749256));
#24011=CARTESIAN_POINT('Ctrl Pts',(179.122733984626,-2.88742467379915,340.165013047072));
#24012=CARTESIAN_POINT('Ctrl Pts',(179.126591109168,-2.95829488009628,340.124749021696));
#24013=CARTESIAN_POINT('Ctrl Pts',(179.130448233711,-3.0282498532578,340.083073222839));
#24014=CARTESIAN_POINT('Ctrl Pts',(179.13787221108,-3.1628952690151,340.002857978511));
#24015=CARTESIAN_POINT('Ctrl Pts',(179.14529618845,-3.29455437319437,339.917168101739));
#24016=CARTESIAN_POINT('Ctrl Pts',(179.15272016582,-3.42275084902876,339.826251877801));
#24017=CARTESIAN_POINT('Ctrl Pts',(179.160135381779,-3.55079603373473,339.735442948685));
#24018=CARTESIAN_POINT('Ctrl Pts',(179.167550597739,-3.67538642271923,339.639420163455));
#24019=CARTESIAN_POINT('Ctrl Pts',(179.174965813698,-3.79607100718653,339.538477219387));
#24020=CARTESIAN_POINT('Ctrl Pts',(179.182373894774,-3.91663946955667,339.43763140211));
#24021=CARTESIAN_POINT('Ctrl Pts',(179.189781975851,-4.03330932481586,339.331875088652));
#24022=CARTESIAN_POINT('Ctrl Pts',(179.197190056927,-4.1456593363124,339.22154464974));
#24023=CARTESIAN_POINT('Ctrl Pts',(179.204592624033,-4.25792572364706,339.111296331784));
#24024=CARTESIAN_POINT('Ctrl Pts',(179.21199519114,-4.36587840428412,338.996480927814));
#24025=CARTESIAN_POINT('Ctrl Pts',(179.219397758246,-4.46913007403816,338.87747429957));
#24026=CARTESIAN_POINT('Ctrl Pts',(179.226796427933,-4.57232738224324,338.758530327792));
#24027=CARTESIAN_POINT('Ctrl Pts',(179.234195097621,-4.67082836483336,338.635399807627));
#24028=CARTESIAN_POINT('Ctrl Pts',(179.241593767308,-4.76428346242158,338.508494499382));
#24029=CARTESIAN_POINT('Ctrl Pts',(179.248991216446,-4.85772314282943,338.381610126561));
#24030=CARTESIAN_POINT('Ctrl Pts',(179.256388665583,-4.94611836921755,338.250952501788));
#24031=CARTESIAN_POINT('Ctrl Pts',(179.26378611472,-5.02916062101619,338.116965513207));
#24032=CARTESIAN_POINT('Ctrl Pts',(179.271183243118,-5.11219927225257,337.98298433406));
#24033=CARTESIAN_POINT('Ctrl Pts',(179.278580371515,-5.18988521377237,337.845674395355));
#24034=CARTESIAN_POINT('Ctrl Pts',(179.285977499912,-5.26195408239006,337.70550730868));
#24035=CARTESIAN_POINT('Ctrl Pts',(179.293375767283,-5.33403404781942,337.565318639762));
#24036=CARTESIAN_POINT('Ctrl Pts',(179.300774034654,-5.40049504757217,337.422272278846));
#24037=CARTESIAN_POINT('Ctrl Pts',(179.308172302025,-5.46111944945291,337.276862956198));
#24038=CARTESIAN_POINT('Ctrl Pts',(179.315573168486,-5.52176514932835,337.131402549715));
#24039=CARTESIAN_POINT('Ctrl Pts',(179.322974034946,-5.57657002534469,336.98357787296));
#24040=CARTESIAN_POINT('Ctrl Pts',(179.330374901407,-5.6253652575456,336.833901928048));
#24041=CARTESIAN_POINT('Ctrl Pts',(179.337783894728,-5.67421407158467,336.684061624614));
#24042=CARTESIAN_POINT('Ctrl Pts',(179.345192888049,-5.71703994717826,336.532366348315));
#24043=CARTESIAN_POINT('Ctrl Pts',(179.35260188137,-5.75372426161535,336.379343207399));
#24044=CARTESIAN_POINT('Ctrl Pts',(179.360015438886,-5.79043117485847,336.226225798938));
#24045=CARTESIAN_POINT('Ctrl Pts',(179.367428996403,-5.8209889157249,336.071779261123));
#24046=CARTESIAN_POINT('Ctrl Pts',(179.37484255392,-5.84533041012745,335.916538574714));
#24047=CARTESIAN_POINT('Ctrl Pts',(179.382266665995,-5.86970655910858,335.761076874735));
#24048=CARTESIAN_POINT('Ctrl Pts',(179.38969077807,-5.88784874354698,335.604819137816));
#24049=CARTESIAN_POINT('Ctrl Pts',(179.397114890144,-5.89974187067178,335.448303939245));
#24050=CARTESIAN_POINT('Ctrl Pts',(179.400972016091,-5.90592083035877,335.366987974803));
#24051=CARTESIAN_POINT('Ctrl Pts',(179.404829142038,-5.91041388977135,335.285602502405));
#24052=CARTESIAN_POINT('Ctrl Pts',(179.408686267985,-5.91322447235937,335.204222677463));
#24053=CARTESIAN_POINT('Ctrl Pts',(179.411891385421,-5.91555995411032,335.136599296867));
#24054=CARTESIAN_POINT('Ctrl Pts',(179.415096502858,-5.9167354740858,335.068935624112));
#24055=CARTESIAN_POINT('Ctrl Pts',(179.418301620294,-5.91674986621234,335.001258243328));
#24056=CARTESIAN_POINT('',(181.168300457419,-5.91371740678573,335.004781946015));
#24057=CARTESIAN_POINT('Ctrl Pts',(179.418302920498,-5.92617389382204,335.001232749351));
#24058=CARTESIAN_POINT('Ctrl Pts',(179.507843381084,-5.92068436070428,333.107536126472));
#24059=CARTESIAN_POINT('Ctrl Pts',(179.690129853096,-3.91031427291091,329.242355225545));
#24060=CARTESIAN_POINT('Ctrl Pts',(179.965162336533,2.6771571405124,328.535833178706));
#24061=CARTESIAN_POINT('Ctrl Pts',(180.243400370805,6.88461919736723,333.753147063498));
#24062=CARTESIAN_POINT('Ctrl Pts',(180.52163840508,4.77416759640351,340.114679321284));
#24063=CARTESIAN_POINT('Ctrl Pts',(180.799876439354,-1.71746669328536,341.782546166841));
#24064=CARTESIAN_POINT('Ctrl Pts',(181.015430190788,-5.52558505666044,338.252676518138));
#24065=CARTESIAN_POINT('Ctrl Pts',(181.138237930799,-5.91644287689095,335.644616494525));
#24066=CARTESIAN_POINT('Ctrl Pts',(181.168299659384,-5.91163757001288,335.004797257822));
#24067=CARTESIAN_POINT('',(182.918301620326,-5.91674900113458,334.996561966701));
#24068=CARTESIAN_POINT('Ctrl Pts',(181.168301620294,-5.91674808559426,335.004759634086));
#24069=CARTESIAN_POINT('Ctrl Pts',(181.175682633724,-5.91687456571228,334.847530951683));
#24070=CARTESIAN_POINT('Ctrl Pts',(181.183063647155,-5.91072959315671,334.690217571805));
#24071=CARTESIAN_POINT('Ctrl Pts',(181.190444660585,-5.8983197483079,334.533358050299));
#24072=CARTESIAN_POINT('Ctrl Pts',(181.197824885786,-5.88591122872514,334.376515280057));
#24073=CARTESIAN_POINT('Ctrl Pts',(181.205205110986,-5.86723919029723,334.220126645509));
#24074=CARTESIAN_POINT('Ctrl Pts',(181.212585336187,-5.84236226494832,334.064727992717));
#24075=CARTESIAN_POINT('Ctrl Pts',(181.219965521659,-5.8174854735172,333.909330176468));
#24076=CARTESIAN_POINT('Ctrl Pts',(181.22734570713,-5.78640392014178,333.754922701516));
#24077=CARTESIAN_POINT('Ctrl Pts',(181.234725892601,-5.74922774037012,333.602033279417));
#24078=CARTESIAN_POINT('Ctrl Pts',(181.242107508479,-5.71204435521699,333.449114224724));
#24079=CARTESIAN_POINT('Ctrl Pts',(181.249489124357,-5.66876408028079,333.297714172808));
#24080=CARTESIAN_POINT('Ctrl Pts',(181.256870740235,-5.61954745989454,333.148347519513));
#24081=CARTESIAN_POINT('Ctrl Pts',(181.264255257255,-5.5703114962613,332.998922161739));
#24082=CARTESIAN_POINT('Ctrl Pts',(181.271639774276,-5.51513465925886,332.851532149276));
#24083=CARTESIAN_POINT('Ctrl Pts',(181.279024291296,-5.45422627296556,332.706673523941));
#24084=CARTESIAN_POINT('Ctrl Pts',(181.286417357171,-5.39324737468555,332.561647199705));
#24085=CARTESIAN_POINT('Ctrl Pts',(181.293810423046,-5.32652382228588,332.419158460163));
#24086=CARTESIAN_POINT('Ctrl Pts',(181.301203488922,-5.25431202131066,332.279680947901));
#24087=CARTESIAN_POINT('Ctrl Pts',(181.308601398843,-5.18205290609127,332.140112047903));
#24088=CARTESIAN_POINT('Ctrl Pts',(181.315999308765,-5.10429856273563,332.003558630727));
#24089=CARTESIAN_POINT('Ctrl Pts',(181.323397218687,-5.02134936621406,331.870466311905));
#24090=CARTESIAN_POINT('Ctrl Pts',(181.330805981087,-4.9382784860901,331.737178751254));
#24091=CARTESIAN_POINT('Ctrl Pts',(181.338214743487,-4.84999774448374,331.607362736975));
#24092=CARTESIAN_POINT('Ctrl Pts',(181.345623505886,-4.75684897720122,331.481432341051));
#24093=CARTESIAN_POINT('Ctrl Pts',(181.349199839891,-4.71188450324754,331.420643624542));
#24094=CARTESIAN_POINT('Ctrl Pts',(181.352776173896,-4.6657862783406,331.360759791651));
#24095=CARTESIAN_POINT('Ctrl Pts',(181.356352507901,-4.61859582054146,331.301824340438));
#24096=CARTESIAN_POINT('Ctrl Pts',(181.363776498333,-4.52063475016631,331.179482236693));
#24097=CARTESIAN_POINT('Ctrl Pts',(181.371200488764,-4.4176614625104,331.060850606176));
#24098=CARTESIAN_POINT('Ctrl Pts',(181.378624479195,-4.30998735794272,330.946367118636));
#24099=CARTESIAN_POINT('Ctrl Pts',(181.386039708267,-4.20244032405714,330.832018737814));
#24100=CARTESIAN_POINT('Ctrl Pts',(181.393454937339,-4.09020376910877,330.721809024822));
#24101=CARTESIAN_POINT('Ctrl Pts',(181.400870166411,-3.97363059578821,330.616144339658));
#24102=CARTESIAN_POINT('Ctrl Pts',(181.408278260637,-3.85716958779107,330.510581323799));
#24103=CARTESIAN_POINT('Ctrl Pts',(181.415686354864,-3.73638054304779,330.409554878568));
#24104=CARTESIAN_POINT('Ctrl Pts',(181.42309444909,-3.61165454041747,330.313436008846));
#24105=CARTESIAN_POINT('Ctrl Pts',(181.430497029372,-3.48702137303549,330.217388681697));
#24106=CARTESIAN_POINT('Ctrl Pts',(181.437899609654,-3.35845737682992,330.126241883687));
#24107=CARTESIAN_POINT('Ctrl Pts',(181.445302189936,-3.22638808277122,330.040327581195));
#24108=CARTESIAN_POINT('Ctrl Pts',(181.452700872812,-3.09438832226619,329.954458511979));
#24109=CARTESIAN_POINT('Ctrl Pts',(181.460099555687,-2.95888725141271,329.873816654786));
#24110=CARTESIAN_POINT('Ctrl Pts',(181.467498238563,-2.82034077094226,329.798691655145));
#24111=CARTESIAN_POINT('Ctrl Pts',(181.474895700865,-2.68181714672183,329.723579049003));
#24112=CARTESIAN_POINT('Ctrl Pts',(181.482293163167,-2.54024943776219,329.653981671833));
#24113=CARTESIAN_POINT('Ctrl Pts',(181.489690625469,-2.39611972686203,329.590144103856));
#24114=CARTESIAN_POINT('Ctrl Pts',(181.497087767015,-2.25199626546311,329.526309303893));
#24115=CARTESIAN_POINT('Ctrl Pts',(181.504484908562,-2.10531136424191,329.468233967683));
#24116=CARTESIAN_POINT('Ctrl Pts',(181.511882050108,-1.956568496847,329.416115126577));
#24117=CARTESIAN_POINT('Ctrl Pts',(181.519280330601,-1.80780272733961,329.363988260671));
#24118=CARTESIAN_POINT('Ctrl Pts',(181.526678611094,-1.65697871296884,329.317819839414));
#24119=CARTESIAN_POINT('Ctrl Pts',(181.534076891586,-1.50461640345109,329.277757429035));
#24120=CARTESIAN_POINT('Ctrl Pts',(181.54147777113,-1.35220056832682,329.23768094454));
#24121=CARTESIAN_POINT('Ctrl Pts',(181.548878650674,-1.1982457228128,329.203714836601));
#24122=CARTESIAN_POINT('Ctrl Pts',(181.556279530218,-1.04328320581177,329.175955811039));
#24123=CARTESIAN_POINT('Ctrl Pts',(181.563688536498,-0.888150528031741,
329.148166303929));
#24124=CARTESIAN_POINT('Ctrl Pts',(181.571097542778,-0.732008336604633,
329.126597556666));
#24125=CARTESIAN_POINT('Ctrl Pts',(181.578506549058,-0.575395043081121,
329.111294615376));
#24126=CARTESIAN_POINT('Ctrl Pts',(181.585920119482,-0.418685271604262,
329.095982247068));
#24127=CARTESIAN_POINT('Ctrl Pts',(181.593333689907,-0.261504191470108,
329.086943397476));
#24128=CARTESIAN_POINT('Ctrl Pts',(181.600747260332,-0.104390926711651,
329.084170971291));
#24129=CARTESIAN_POINT('Ctrl Pts',(181.608171385123,0.0529460131384107,
329.081394598127));
#24130=CARTESIAN_POINT('Ctrl Pts',(181.615595509915,0.210214572680946,329.084902457541));
#24131=CARTESIAN_POINT('Ctrl Pts',(181.623019634707,0.366879212260065,329.094635472207));
#24132=CARTESIAN_POINT('Ctrl Pts',(181.626876603863,0.448269369311689,329.099691952051));
#24133=CARTESIAN_POINT('Ctrl Pts',(181.630733573019,0.529496660050726,329.106427748144));
#24134=CARTESIAN_POINT('Ctrl Pts',(181.634590542176,0.610487122077327,329.114829141284));
#24135=CARTESIAN_POINT('Ctrl Pts',(181.642014491516,0.766378720569057,329.131000262838));
#24136=CARTESIAN_POINT('Ctrl Pts',(181.649438440856,0.921862522342883,329.153394149161));
#24137=CARTESIAN_POINT('Ctrl Pts',(181.656862390196,1.07640196975953,329.181985788777));
#24138=CARTESIAN_POINT('Ctrl Pts',(181.664277578124,1.23075903663928,329.210543685819));
#24139=CARTESIAN_POINT('Ctrl Pts',(181.671692766052,1.38417360414381,329.245284709667));
#24140=CARTESIAN_POINT('Ctrl Pts',(181.679107953979,1.53611298402458,329.286132005129));
#24141=CARTESIAN_POINT('Ctrl Pts',(181.686516007047,1.68790616853565,329.326939997512));
#24142=CARTESIAN_POINT('Ctrl Pts',(181.693924060115,1.83822663321251,329.373842468387));
#24143=CARTESIAN_POINT('Ctrl Pts',(181.701332113183,1.98655076106678,329.426711326676));
#24144=CARTESIAN_POINT('Ctrl Pts',(181.708734652331,2.13476448914581,329.479540833915));
#24145=CARTESIAN_POINT('Ctrl Pts',(181.716137191479,2.2809844890056,329.538327761386));
#24146=CARTESIAN_POINT('Ctrl Pts',(181.723539730627,2.4247013277235,329.602893920457));
#24147=CARTESIAN_POINT('Ctrl Pts',(181.730938372431,2.56834250134204,329.667426086262));
#24148=CARTESIAN_POINT('Ctrl Pts',(181.738337014236,2.70948279888093,329.737731271405));
#24149=CARTESIAN_POINT('Ctrl Pts',(181.745735656041,2.84763194093631,329.813582846371));
#24150=CARTESIAN_POINT('Ctrl Pts',(181.753133077496,2.98575829634621,329.889421910198));
#24151=CARTESIAN_POINT('Ctrl Pts',(181.760530498951,3.12089414861938,329.970805368751));
#24152=CARTESIAN_POINT('Ctrl Pts',(181.767927920406,3.25257294598057,330.057460187963));
#24153=CARTESIAN_POINT('Ctrl Pts',(181.775325021248,3.38424603622782,330.144111251452));
#24154=CARTESIAN_POINT('Ctrl Pts',(181.78272212209,3.51246205771631,330.236033016168));
#24155=CARTESIAN_POINT('Ctrl Pts',(181.790119222932,3.63678286766842,330.332908728562));
#24156=CARTESIAN_POINT('Ctrl Pts',(181.797517462899,3.76112282253035,330.42979935943));
#24157=CARTESIAN_POINT('Ctrl Pts',(181.804915702865,3.88156607707473,330.531645227573));
#24158=CARTESIAN_POINT('Ctrl Pts',(181.812313942831,3.99770716865451,330.638088955952));
#24159=CARTESIAN_POINT('Ctrl Pts',(181.819714782061,4.11388906471168,330.744570081781));
#24160=CARTESIAN_POINT('Ctrl Pts',(181.827115621291,4.22576551344088,330.855652032078));
#24161=CARTESIAN_POINT('Ctrl Pts',(181.834516460521,4.33296765850278,330.970940328952));
#24162=CARTESIAN_POINT('Ctrl Pts',(181.841925427011,4.44028752802186,331.086355230121));
#24163=CARTESIAN_POINT('Ctrl Pts',(181.849334393502,4.54292258849431,331.205985429211));
#24164=CARTESIAN_POINT('Ctrl Pts',(181.856743359993,4.64054359794924,331.329402544812));
#24165=CARTESIAN_POINT('Ctrl Pts',(181.864156890866,4.73822474800165,331.452895693012));
#24166=CARTESIAN_POINT('Ctrl Pts',(181.87157042174,4.83088547272313,331.580180105459));
#24167=CARTESIAN_POINT('Ctrl Pts',(181.878983952613,4.91823999153433,331.71079858504));
#24168=CARTESIAN_POINT('Ctrl Pts',(181.886408038565,5.00571888208932,331.8416030338));
#24169=CARTESIAN_POINT('Ctrl Pts',(181.893832124516,5.08787628398089,331.975750712805));
#24170=CARTESIAN_POINT('Ctrl Pts',(181.901256210468,5.16447206921048,332.112759308813));
#24171=CARTESIAN_POINT('Ctrl Pts',(181.905113665795,5.20427021024835,332.183947134762));
#24172=CARTESIAN_POINT('Ctrl Pts',(181.908971121122,5.24256766562074,332.255906973951));
#24173=CARTESIAN_POINT('Ctrl Pts',(181.91282857645,5.2793359363705,332.328569178615));
#24174=CARTESIAN_POINT('Ctrl Pts',(181.920252564985,5.35009948315099,332.468413539364));
#24175=CARTESIAN_POINT('Ctrl Pts',(181.92767655352,5.41540943627099,332.611282488728));
#24176=CARTESIAN_POINT('Ctrl Pts',(181.935100542055,5.47499646572596,332.756711284121));
#24177=CARTESIAN_POINT('Ctrl Pts',(181.942515769003,5.53451317220456,332.901968448443));
#24178=CARTESIAN_POINT('Ctrl Pts',(181.94993099595,5.58832025891396,333.049779103337));
#24179=CARTESIAN_POINT('Ctrl Pts',(181.957346222898,5.63619408637256,333.199653704634));
#24180=CARTESIAN_POINT('Ctrl Pts',(181.964754314777,5.68402184874883,333.349384093817));
#24181=CARTESIAN_POINT('Ctrl Pts',(181.972162406656,5.72592760481096,333.501174122574));
#24182=CARTESIAN_POINT('Ctrl Pts',(181.979570498535,5.76173570945806,333.6545141484));
#24183=CARTESIAN_POINT('Ctrl Pts',(181.986973076251,5.79751716058468,333.807740036615));
#24184=CARTESIAN_POINT('Ctrl Pts',(181.994375653968,5.82720991309449,333.96251326278));
#24185=CARTESIAN_POINT('Ctrl Pts',(182.001778231684,5.85068812582356,334.118309001494));
#24186=CARTESIAN_POINT('Ctrl Pts',(182.009176911779,5.87415397675598,334.274022710316));
#24187=CARTESIAN_POINT('Ctrl Pts',(182.016575591875,5.89141174899934,334.430757491367));
#24188=CARTESIAN_POINT('Ctrl Pts',(182.023974271971,5.90238670143731,334.587978411736));
#24189=CARTESIAN_POINT('Ctrl Pts',(182.031371731185,5.91335984286074,334.745173388541));
#24190=CARTESIAN_POINT('Ctrl Pts',(182.038769190399,5.91805219613118,334.902853973512));
#24191=CARTESIAN_POINT('Ctrl Pts',(182.046166649613,5.91644088308741,335.060480074669));
#24192=CARTESIAN_POINT('Ctrl Pts',(182.053563787881,5.91482963995212,335.218099337053));
#24193=CARTESIAN_POINT('Ctrl Pts',(182.060960926148,5.90691527810846,335.375663747132));
#24194=CARTESIAN_POINT('Ctrl Pts',(182.068358064416,5.89272705777317,335.532633443456));
#24195=CARTESIAN_POINT('Ctrl Pts',(182.075756341443,5.8785366532187,335.689627304631));
#24196=CARTESIAN_POINT('Ctrl Pts',(182.083154618471,5.85807050066655,335.846025898037));
#24197=CARTESIAN_POINT('Ctrl Pts',(182.090552895498,5.83140970659936,336.001294859808));
#24198=CARTESIAN_POINT('Ctrl Pts',(182.097953771393,5.80473954712484,336.156618364481));
#24199=CARTESIAN_POINT('Ctrl Pts',(182.105354647288,5.77187047673323,336.31081107986));
#24200=CARTESIAN_POINT('Ctrl Pts',(182.112755523183,5.73293461061827,336.463349347516));
#24201=CARTESIAN_POINT('Ctrl Pts',(182.120164525555,5.69395599126166,336.616055108695));
#24202=CARTESIAN_POINT('Ctrl Pts',(182.127573527927,5.64889736496822,336.767102432364));
#24203=CARTESIAN_POINT('Ctrl Pts',(182.1349825303,5.59794079477748,336.915982625356));
#24204=CARTESIAN_POINT('Ctrl Pts',(182.142396096665,5.54695283501408,337.064954529498));
#24205=CARTESIAN_POINT('Ctrl Pts',(182.14980966303,5.49005982632769,337.211756295688));
#24206=CARTESIAN_POINT('Ctrl Pts',(182.157223229395,5.42749158307523,337.35590018425));
#24207=CARTESIAN_POINT('Ctrl Pts',(182.164647349926,5.36483426587322,337.500249280194));
#24208=CARTESIAN_POINT('Ctrl Pts',(182.172071470458,5.29648573959151,337.641932606207));
#24209=CARTESIAN_POINT('Ctrl Pts',(182.179495590989,5.22272164463501,337.780487220823));
#24210=CARTESIAN_POINT('Ctrl Pts',(182.183352597567,5.18439944899157,337.852469627057));
#24211=CARTESIAN_POINT('Ctrl Pts',(182.187209604146,5.14461628326591,337.923608050044));
#24212=CARTESIAN_POINT('Ctrl Pts',(182.191066610724,5.10341527751716,337.99384085544));
#24213=CARTESIAN_POINT('Ctrl Pts',(182.198490665663,5.02411063438275,338.129026574018));
#24214=CARTESIAN_POINT('Ctrl Pts',(182.205914720603,4.93931120921902,338.261262938105));
#24215=CARTESIAN_POINT('Ctrl Pts',(182.213338775543,4.84926207516582,338.390071959245));
#24216=CARTESIAN_POINT('Ctrl Pts',(182.220754069442,4.75931920704098,338.518728974368));
#24217=CARTESIAN_POINT('Ctrl Pts',(182.228169363342,4.66413917326874,338.643966394428));
#24218=CARTESIAN_POINT('Ctrl Pts',(182.235584657241,4.56401262852332,338.765331232333));
#24219=CARTESIAN_POINT('Ctrl Pts',(182.24299281655,4.46398242007042,338.886579299619));
#24220=CARTESIAN_POINT('Ctrl Pts',(182.250400975859,4.35901541136668,339.003961916544));
#24221=CARTESIAN_POINT('Ctrl Pts',(182.257809135167,4.2494451302821,339.117055579807));
#24222=CARTESIAN_POINT('Ctrl Pts',(182.265211780722,4.13995640030056,339.23006506958));
#24223=CARTESIAN_POINT('Ctrl Pts',(182.272614426277,4.02587147843684,339.338791694916));
#24224=CARTESIAN_POINT('Ctrl Pts',(182.280017071832,3.90756361151544,339.442845617896));
#24225=CARTESIAN_POINT('Ctrl Pts',(182.287415820107,3.78931803026757,339.546844759493));
#24226=CARTESIAN_POINT('Ctrl Pts',(182.294814568383,3.66685421124456,339.646175852206));
#24227=CARTESIAN_POINT('Ctrl Pts',(182.302213316659,3.54058155364649,339.740486559888));
#24228=CARTESIAN_POINT('Ctrl Pts',(182.309610844342,3.41432972760946,339.834781708863));
#24229=CARTESIAN_POINT('Ctrl Pts',(182.317008372025,3.28427060879882,339.924057893467));
#24230=CARTESIAN_POINT('Ctrl Pts',(182.324405899708,3.15084600044121,340.008003598641));
#24231=CARTESIAN_POINT('Ctrl Pts',(182.331803106617,3.0174271776934,340.091945663729));
#24232=CARTESIAN_POINT('Ctrl Pts',(182.339200313526,2.88064347144987,340.170557510235));
#24233=CARTESIAN_POINT('Ctrl Pts',(182.346597520434,2.74096470582782,340.243571592332));
#24234=CARTESIAN_POINT('Ctrl Pts',(182.353995866214,2.60126443531217,340.316596915651));
#24235=CARTESIAN_POINT('Ctrl Pts',(182.361394211994,2.45866854868735,340.384022585646));
#24236=CARTESIAN_POINT('Ctrl Pts',(182.368792557775,2.31367030378293,340.445627630301));
#24237=CARTESIAN_POINT('Ctrl Pts',(182.376193502474,2.16862112333624,340.507254315812));
#24238=CARTESIAN_POINT('Ctrl Pts',(182.383594447173,2.02116824765639,340.56305615916));
#24239=CARTESIAN_POINT('Ctrl Pts',(182.390995391873,1.87182353572629,340.612860876024));
#24240=CARTESIAN_POINT('Ctrl Pts',(182.398404462779,1.72231484392265,340.66272027826));
#24241=CARTESIAN_POINT('Ctrl Pts',(182.405813533685,1.57091052177811,340.706569285638));
#24242=CARTESIAN_POINT('Ctrl Pts',(182.413222604591,1.41813687320069,340.744285714636));
#24243=CARTESIAN_POINT('Ctrl Pts',(182.420636239438,1.26526911701207,340.782025376718));
#24244=CARTESIAN_POINT('Ctrl Pts',(182.428049874286,1.11103071836581,340.813624858261));
#24245=CARTESIAN_POINT('Ctrl Pts',(182.435463509133,0.955956201956742,340.839013469966));
#24246=CARTESIAN_POINT('Ctrl Pts',(182.442887697474,0.800660933103974,340.864438222993));
#24247=CARTESIAN_POINT('Ctrl Pts',(182.450311885816,0.644527538766438,340.88363440286));
#24248=CARTESIAN_POINT('Ctrl Pts',(182.457736074157,0.488094489432406,340.896583276092));
#24249=CARTESIAN_POINT('Ctrl Pts',(182.461592264438,0.406841754914568,340.903309037454));
#24250=CARTESIAN_POINT('Ctrl Pts',(182.465448454718,0.325508170214552,340.908350223537));
#24251=CARTESIAN_POINT('Ctrl Pts',(182.469304644998,0.244168856578803,340.911709746933));
#24252=CARTESIAN_POINT('Ctrl Pts',(182.476728424502,0.0875777431645812,
340.918177363705));
#24253=CARTESIAN_POINT('Ctrl Pts',(182.484152204007,-0.0695068156684068,
340.918428695711));
#24254=CARTESIAN_POINT('Ctrl Pts',(182.491575983512,-0.226550281635667,
340.912411143721));
#24255=CARTESIAN_POINT('Ctrl Pts',(182.498991001481,-0.383408405106118,
340.906400693638));
#24256=CARTESIAN_POINT('Ctrl Pts',(182.506406019451,-0.540225162915335,
340.894136100585));
#24257=CARTESIAN_POINT('Ctrl Pts',(182.513821037421,-0.696462371684638,
340.875616625285));
#24258=CARTESIAN_POINT('Ctrl Pts',(182.521228920568,-0.852549247077918,
340.857114969653));
#24259=CARTESIAN_POINT('Ctrl Pts',(182.528636803716,-1.00805731544565,340.832370457163));
#24260=CARTESIAN_POINT('Ctrl Pts',(182.536044686863,-1.16244998371425,340.801434356938));
#24261=CARTESIAN_POINT('Ctrl Pts',(182.543447056287,-1.31672773676139,340.770521282605));
#24262=CARTESIAN_POINT('Ctrl Pts',(182.550849425711,-1.4698913783617,340.733425869595));
#24263=CARTESIAN_POINT('Ctrl Pts',(182.558251795135,-1.62141112949147,340.690251006033));
#24264=CARTESIAN_POINT('Ctrl Pts',(182.565650267569,-1.77285111280959,340.647098871946));
#24265=CARTESIAN_POINT('Ctrl Pts',(182.573048740004,-1.92264857116719,340.59787376338));
#24266=CARTESIAN_POINT('Ctrl Pts',(182.580447212439,-2.07028569619649,340.542729264417));
#24267=CARTESIAN_POINT('Ctrl Pts',(182.587844465587,-2.21789849027097,340.4875938534));
#24268=CARTESIAN_POINT('Ctrl Pts',(182.595241718736,-2.36335130831283,340.42654111855));
#24269=CARTESIAN_POINT('Ctrl Pts',(182.602638971884,-2.50614313261334,340.359773984167));
#24270=CARTESIAN_POINT('Ctrl Pts',(182.610035905096,-2.64892878104972,340.293009737518));
#24271=CARTESIAN_POINT('Ctrl Pts',(182.617432838307,-2.78905332648191,340.220531740842));
#24272=CARTESIAN_POINT('Ctrl Pts',(182.624829771518,-2.9260375617218,340.1425902763));
#24273=CARTESIAN_POINT('Ctrl Pts',(182.632227844672,-3.0630429076182,340.064636800189));
#24274=CARTESIAN_POINT('Ctrl Pts',(182.639625917825,-3.19690665528948,339.981218364317));
#24275=CARTESIAN_POINT('Ctrl Pts',(182.647023990979,-3.32717608107599,339.892630160559));
#24276=CARTESIAN_POINT('Ctrl Pts',(182.654424664357,-3.4574912930801,339.804010820419));
#24277=CARTESIAN_POINT('Ctrl Pts',(182.661825337735,-3.58420935952138,339.710218304431));
#24278=CARTESIAN_POINT('Ctrl Pts',(182.669226011114,-3.70690843339046,339.61158979409));
#24279=CARTESIAN_POINT('Ctrl Pts',(182.676634814044,-3.82974229073642,339.512852941501));
#24280=CARTESIAN_POINT('Ctrl Pts',(182.684043616974,-3.94854804781382,339.409269719623));
#24281=CARTESIAN_POINT('Ctrl Pts',(182.691452419904,-4.06293817176402,339.301216569172));
#24282=CARTESIAN_POINT('Ctrl Pts',(182.698865788272,-4.17739878495709,339.193096834435));
#24283=CARTESIAN_POINT('Ctrl Pts',(182.706279156639,-4.28743808283587,339.080501948831));
#24284=CARTESIAN_POINT('Ctrl Pts',(182.713692525006,-4.39270738723038,338.963843131693));
#24285=CARTESIAN_POINT('Ctrl Pts',(182.721116451491,-4.49812661614684,338.847018169092));
#24286=CARTESIAN_POINT('Ctrl Pts',(182.728540377976,-4.59876204562417,338.72611800155));
#24287=CARTESIAN_POINT('Ctrl Pts',(182.735964304461,-4.69430655360297,338.60158528197));
#24288=CARTESIAN_POINT('Ctrl Pts',(182.739823762731,-4.74397704027127,338.536844765549));
#24289=CARTESIAN_POINT('Ctrl Pts',(182.743683221002,-4.79227237015983,338.471122966409));
#24290=CARTESIAN_POINT('Ctrl Pts',(182.747542679272,-4.83915424449997,338.404484801029));
#24291=CARTESIAN_POINT('Ctrl Pts',(182.755048836972,-4.93033355450777,338.274882006239));
#24292=CARTESIAN_POINT('Ctrl Pts',(182.762554994673,-5.01643598000011,338.141424467438));
#24293=CARTESIAN_POINT('Ctrl Pts',(182.770061152373,-5.09712241388912,338.004542171501));
#24294=CARTESIAN_POINT('Ctrl Pts',(182.777558024154,-5.17770903003509,337.867829213596));
#24295=CARTESIAN_POINT('Ctrl Pts',(182.785054895935,-5.25289281146279,337.727700242247));
#24296=CARTESIAN_POINT('Ctrl Pts',(182.792551767716,-5.32237623071385,337.584616377963));
#24297=CARTESIAN_POINT('Ctrl Pts',(182.800040731471,-5.39178635583995,337.441683444746));
#24298=CARTESIAN_POINT('Ctrl Pts',(182.807529695227,-5.45550793449517,337.295802148505));
#24299=CARTESIAN_POINT('Ctrl Pts',(182.815018658982,-5.51328793537044,337.14746052448));
#24300=CARTESIAN_POINT('Ctrl Pts',(182.822501087381,-5.57101751365697,336.999248353009));
#24301=CARTESIAN_POINT('Ctrl Pts',(182.829983515779,-5.62281570936212,336.848580465654));
#24302=CARTESIAN_POINT('Ctrl Pts',(182.837465944177,-5.66847646330246,336.695967319109));
#24303=CARTESIAN_POINT('Ctrl Pts',(182.844942536867,-5.71410160542619,336.543473198881));
#24304=CARTESIAN_POINT('Ctrl Pts',(182.852419129556,-5.75359874162882,336.389037189035));
#24305=CARTESIAN_POINT('Ctrl Pts',(182.859895722245,-5.78681083456673,336.233187304282));
#24306=CARTESIAN_POINT('Ctrl Pts',(182.867368876273,-5.82000765247827,336.077409098573));
#24307=CARTESIAN_POINT('Ctrl Pts',(182.874842030301,-5.846925109297,335.920218666881));
#24308=CARTESIAN_POINT('Ctrl Pts',(182.882315184329,-5.86745664008178,335.762156899372));
#24309=CARTESIAN_POINT('Ctrl Pts',(182.889786702774,-5.88798367731465,335.604129725423));
#24310=CARTESIAN_POINT('Ctrl Pts',(182.89725822122,-5.90212752351781,335.445231954273));
#24311=CARTESIAN_POINT('Ctrl Pts',(182.904729739665,-5.90983311565753,335.286012425565));
#24312=CARTESIAN_POINT('Ctrl Pts',(182.909253699875,-5.91449880610392,335.189605943039));
#24313=CARTESIAN_POINT('Ctrl Pts',(182.913777660084,-5.9168050856102,335.093081634052));
#24314=CARTESIAN_POINT('Ctrl Pts',(182.918301620294,-5.91674900113497,334.996561967377));
#24315=CARTESIAN_POINT('Ctrl Pts',(182.918301620326,-5.91674900113458,334.996561966701));
#24316=CARTESIAN_POINT('Ctrl Pts',(182.926539808851,-5.91664687057866,334.820798437922));
#24317=CARTESIAN_POINT('Ctrl Pts',(182.934777997377,-5.90870884398697,334.645319786239));
#24318=CARTESIAN_POINT('Ctrl Pts',(182.943016185902,-5.89303513855422,334.470786037349));
#24319=CARTESIAN_POINT('Ctrl Pts',(182.951302560027,-5.87726975679178,334.295231431356));
#24320=CARTESIAN_POINT('Ctrl Pts',(182.959588934152,-5.85367802089785,334.120633019713));
#24321=CARTESIAN_POINT('Ctrl Pts',(182.967875308277,-5.82241199872577,333.947645934301));
#24322=CARTESIAN_POINT('Ctrl Pts',(182.976186416185,-5.79105265141491,333.774142504223));
#24323=CARTESIAN_POINT('Ctrl Pts',(182.984497524093,-5.75197324614276,333.602260224294));
#24324=CARTESIAN_POINT('Ctrl Pts',(182.992808632001,-5.70537596478024,333.432640544416));
#24325=CARTESIAN_POINT('Ctrl Pts',(183.001151291127,-5.65860178750894,333.262376942263));
#24326=CARTESIAN_POINT('Ctrl Pts',(183.009493950253,-5.60425265350634,333.094393338494));
#24327=CARTESIAN_POINT('Ctrl Pts',(183.017836609379,-5.54258047112392,332.929315986536));
#24328=CARTESIAN_POINT('Ctrl Pts',(183.020484644101,-5.52300516810979,332.876918956619));
#24329=CARTESIAN_POINT('Ctrl Pts',(183.023132678823,-5.50269242956288,332.824814546121));
#24330=CARTESIAN_POINT('Ctrl Pts',(183.025780713545,-5.48165127710042,332.773022263523));
#24331=CARTESIAN_POINT('Ctrl Pts',(183.033205134754,-5.42265719469586,332.627809771338));
#24332=CARTESIAN_POINT('Ctrl Pts',(183.040629555963,-5.35780005342511,332.484724222657));
#24333=CARTESIAN_POINT('Ctrl Pts',(183.048053977172,-5.28725352347771,332.344273971026));
#24334=CARTESIAN_POINT('Ctrl Pts',(183.055469639593,-5.21679021915741,332.20398941231));
#24335=CARTESIAN_POINT('Ctrl Pts',(183.062885302014,-5.14065105225165,332.066334292474));
#24336=CARTESIAN_POINT('Ctrl Pts',(183.070300964435,-5.0590584006965,331.931798790685));
#24337=CARTESIAN_POINT('Ctrl Pts',(183.077709494145,-4.97754422855538,331.79739269108));
#24338=CARTESIAN_POINT('Ctrl Pts',(183.085118023854,-4.89058720662411,331.666100552837));
#24339=CARTESIAN_POINT('Ctrl Pts',(183.092526553564,-4.79845638643319,331.538389555424));
#24340=CARTESIAN_POINT('Ctrl Pts',(183.09992957103,-4.70639411526576,331.410773580112));
#24341=CARTESIAN_POINT('Ctrl Pts',(183.107332588496,-4.6091659281835,331.286733741523));
#24342=CARTESIAN_POINT('Ctrl Pts',(183.114735605963,-4.50708503167518,331.16670962752));
#24343=CARTESIAN_POINT('Ctrl Pts',(183.122134727296,-4.40505785931685,331.046748681002));
#24344=CARTESIAN_POINT('Ctrl Pts',(183.129533848628,-4.29818330500363,330.930799533569));
#24345=CARTESIAN_POINT('Ctrl Pts',(183.136932969961,-4.18681575387772,330.819269871711));
#24346=CARTESIAN_POINT('Ctrl Pts',(183.144330871211,-4.07546656676774,330.707758600601));
#24347=CARTESIAN_POINT('Ctrl Pts',(183.151728772462,-3.95962611666547,330.60066563252));
#24348=CARTESIAN_POINT('Ctrl Pts',(183.159126673712,-3.83968673673909,330.498362928199));
#24349=CARTESIAN_POINT('Ctrl Pts',(183.166524254465,-3.71975255291265,330.39606465591));
#24350=CARTESIAN_POINT('Ctrl Pts',(183.173921835218,-3.59572007625608,330.298556476909));
#24351=CARTESIAN_POINT('Ctrl Pts',(183.181319415972,-3.46801570464513,330.206170879679));
#24352=CARTESIAN_POINT('Ctrl Pts',(183.188718135548,-3.34029167353395,330.113771060112));
#24353=CARTESIAN_POINT('Ctrl Pts',(183.196116855125,-3.20889492429432,330.026495611256));
#24354=CARTESIAN_POINT('Ctrl Pts',(183.203515574702,-3.07428175601834,329.944634311238));
#24355=CARTESIAN_POINT('Ctrl Pts',(183.210916892824,-2.9396213094921,329.86274426025));
#24356=CARTESIAN_POINT('Ctrl Pts',(183.218318210947,-2.80174251341328,329.786272337828));
#24357=CARTESIAN_POINT('Ctrl Pts',(183.22571952907,-2.66112709113199,329.715462823733));
#24358=CARTESIAN_POINT('Ctrl Pts',(183.233128970942,-2.52035732817522,329.644575588518));
#24359=CARTESIAN_POINT('Ctrl Pts',(183.240538412814,-2.37684527386209,329.579363341473));
#24360=CARTESIAN_POINT('Ctrl Pts',(183.247947854686,-2.23109416682969,329.520022866723));
#24361=CARTESIAN_POINT('Ctrl Pts',(183.255361859659,-2.0852532990533,329.460645847172));
#24362=CARTESIAN_POINT('Ctrl Pts',(183.262775864632,-1.93717098101059,329.407147932048));
#24363=CARTESIAN_POINT('Ctrl Pts',(183.270189869605,-1.7873660092298,329.359676134161));
#24364=CARTESIAN_POINT('Ctrl Pts',(183.277614423569,-1.63734788795967,329.31213679119));
#24365=CARTESIAN_POINT('Ctrl Pts',(183.285038977534,-1.48560257664327,329.270640788103));
#24366=CARTESIAN_POINT('Ctrl Pts',(183.292463531498,-1.33266026578227,329.235284293349));
#24367=CARTESIAN_POINT('Ctrl Pts',(183.296315270272,-1.25331626320317,329.21694191448));
#24368=CARTESIAN_POINT('Ctrl Pts',(183.300167009046,-1.1736502202182,329.200251052964));
#24369=CARTESIAN_POINT('Ctrl Pts',(183.30401874782,-1.09373663000128,329.185219630399));
#24370=CARTESIAN_POINT('Ctrl Pts',(183.311441361916,-0.939736637768514,
329.156252855763));
#24371=CARTESIAN_POINT('Ctrl Pts',(183.318863976013,-0.784352309190427,
329.133364376445));
#24372=CARTESIAN_POINT('Ctrl Pts',(183.32628659011,-0.628104860476675,329.116683346381));
#24373=CARTESIAN_POINT('Ctrl Pts',(183.333700441245,-0.47204187378618,329.100022009545));
#24374=CARTESIAN_POINT('Ctrl Pts',(183.341114292379,-0.315118162870769,
329.089553574084));
#24375=CARTESIAN_POINT('Ctrl Pts',(183.348528143514,-0.157866035844739,
329.085356403195));
#24376=CARTESIAN_POINT('Ctrl Pts',(183.355934859503,-0.000765249449437844,
329.081163271695));
#24377=CARTESIAN_POINT('Ctrl Pts',(183.363341575492,0.156662953096641,329.083229399167));
#24378=CARTESIAN_POINT('Ctrl Pts',(183.370748291481,0.313880332588857,329.091581455303));
#24379=CARTESIAN_POINT('Ctrl Pts',(183.378149494515,0.470980692309217,329.099927294852));
#24380=CARTESIAN_POINT('Ctrl Pts',(183.38555069755,0.627870170187996,329.114549727371));
#24381=CARTESIAN_POINT('Ctrl Pts',(183.392951900584,0.784009822882335,329.135423360538));
#24382=CARTESIAN_POINT('Ctrl Pts',(183.400349208488,0.940067301855593,329.156286008257));
#24383=CARTESIAN_POINT('Ctrl Pts',(183.407746516391,1.09537537241413,329.18339325528));
#24384=CARTESIAN_POINT('Ctrl Pts',(183.415143824295,1.24939962459685,329.216667816859));
#24385=CARTESIAN_POINT('Ctrl Pts',(183.422539919361,1.40339862349636,329.249936922855));
#24386=CARTESIAN_POINT('Ctrl Pts',(183.429936014428,1.55611385716661,329.289371257896));
#24387=CARTESIAN_POINT('Ctrl Pts',(183.437332109494,1.70702041513273,329.334842291267));
#24388=CARTESIAN_POINT('Ctrl Pts',(183.444727888732,1.85792052907156,329.380311382929));
#24389=CARTESIAN_POINT('Ctrl Pts',(183.45212366797,2.0070117633814,329.431816552673));
#24390=CARTESIAN_POINT('Ctrl Pts',(183.459519447208,2.1537839627113,329.489179262173));
#24391=CARTESIAN_POINT('Ctrl Pts',(183.466916371476,2.30057888562481,329.546550852689));
#24392=CARTESIAN_POINT('Ctrl Pts',(183.474313295744,2.44505371090248,329.609781652746));
#24393=CARTESIAN_POINT('Ctrl Pts',(183.481710220012,2.5867180170615,329.678644865947));
#24394=CARTESIAN_POINT('Ctrl Pts',(183.489109750576,2.72843223845886,329.747532343014));
#24395=CARTESIAN_POINT('Ctrl Pts',(183.496509281141,2.86733363352001,329.822056021361));
#24396=CARTESIAN_POINT('Ctrl Pts',(183.503908811706,3.00295628429228,329.901943103777));
#24397=CARTESIAN_POINT('Ctrl Pts',(183.511316486777,3.13872821204158,329.981918116211));
#24398=CARTESIAN_POINT('Ctrl Pts',(183.518724161849,3.27121386656859,330.067268132464));
#24399=CARTESIAN_POINT('Ctrl Pts',(183.52613183692,3.39997562864591,330.15767656108));
#24400=CARTESIAN_POINT('Ctrl Pts',(183.533544084214,3.52881686606072,330.248140792291));
#24401=CARTESIAN_POINT('Ctrl Pts',(183.540956331509,3.65392933497888,330.343669431135));
#24402=CARTESIAN_POINT('Ctrl Pts',(183.548368578803,3.77490885653954,330.443905873742));
#24403=CARTESIAN_POINT('Ctrl Pts',(183.555791404439,3.89606103325496,330.544285368151));
#24404=CARTESIAN_POINT('Ctrl Pts',(183.563214230074,4.01306820552597,330.649385836092));
#24405=CARTESIAN_POINT('Ctrl Pts',(183.57063705571,4.12556278929575,330.758813581782));
#24406=CARTESIAN_POINT('Ctrl Pts',(183.574510297838,4.18426264059047,330.815913152128));
#24407=CARTESIAN_POINT('Ctrl Pts',(183.578383539966,4.24173447469739,330.874190378549));
#24408=CARTESIAN_POINT('Ctrl Pts',(183.582256782094,4.29793053209515,330.933585891257));
#24409=CARTESIAN_POINT('Ctrl Pts',(183.589681965407,4.40566095892533,331.04744982108));
#24410=CARTESIAN_POINT('Ctrl Pts',(183.59710714872,4.50902576428197,331.165769412846));
#24411=CARTESIAN_POINT('Ctrl Pts',(183.604532332033,4.60763417503468,331.288175937419));
#24412=CARTESIAN_POINT('Ctrl Pts',(183.611948747775,4.70612615011179,331.410437925779));
#24413=CARTESIAN_POINT('Ctrl Pts',(183.619365163517,4.7998726781938,331.53677695334));
#24414=CARTESIAN_POINT('Ctrl Pts',(183.626781579259,4.88851970687147,331.666787489819));
#24415=CARTESIAN_POINT('Ctrl Pts',(183.634190852915,4.97708136753446,331.796672824793));
#24416=CARTESIAN_POINT('Ctrl Pts',(183.641600126571,5.06055309669955,331.930222323533));
#24417=CARTESIAN_POINT('Ctrl Pts',(183.649009400228,5.13862111105372,332.066997504343));
#24418=CARTESIAN_POINT('Ctrl Pts',(183.656413151672,5.21663094047282,332.203670745131));
#24419=CARTESIAN_POINT('Ctrl Pts',(183.663816903116,5.28924489020512,332.343564558347));
#24420=CARTESIAN_POINT('Ctrl Pts',(183.671220654561,5.35619258140474,332.486211704736));
#24421=CARTESIAN_POINT('Ctrl Pts',(183.678620499305,5.42310494664703,332.628783581211));
#24422=CARTESIAN_POINT('Ctrl Pts',(183.686020344048,5.48435684981207,332.774105560543));
#24423=CARTESIAN_POINT('Ctrl Pts',(183.693420188792,5.53972400567662,332.921686139336));
#24424=CARTESIAN_POINT('Ctrl Pts',(183.700818795492,5.59508189824538,333.069242026909));
#24425=CARTESIAN_POINT('Ctrl Pts',(183.708217402192,5.64455686679045,333.219055414939));
#24426=CARTESIAN_POINT('Ctrl Pts',(183.715616008892,5.68797286237348,333.370615061011));
#24427=CARTESIAN_POINT('Ctrl Pts',(183.723014283895,5.73138691151746,333.522167912316));
#24428=CARTESIAN_POINT('Ctrl Pts',(183.730412558898,5.76874242509563,333.675466507332));
#24429=CARTESIAN_POINT('Ctrl Pts',(183.737810833902,5.79991339090287,333.82998494859));
#24430=CARTESIAN_POINT('Ctrl Pts',(183.74521023597,5.8310891053442,333.984526929432));
#24431=CARTESIAN_POINT('Ctrl Pts',(183.752609638039,5.85607832225718,334.140288760794));
#24432=CARTESIAN_POINT('Ctrl Pts',(183.760009040107,5.87480628874774,334.296735019932));
#24433=CARTESIAN_POINT('Ctrl Pts',(183.767411028395,5.89354080098971,334.45323595977));
#24434=CARTESIAN_POINT('Ctrl Pts',(183.774813016684,5.90600966134355,334.61042143346));
#24435=CARTESIAN_POINT('Ctrl Pts',(183.782215004973,5.91219005950291,334.76775172161));
#24436=CARTESIAN_POINT('Ctrl Pts',(183.789625095016,5.91837722234083,334.925254213687));
#24437=CARTESIAN_POINT('Ctrl Pts',(183.79703518506,5.91826216267396,335.082901463745));
#24438=CARTESIAN_POINT('Ctrl Pts',(183.804445275103,5.91187421168256,335.240153841824));
#24439=CARTESIAN_POINT('Ctrl Pts',(183.811859916752,5.90548233692874,335.397502811278));
#24440=CARTESIAN_POINT('Ctrl Pts',(183.819274558401,5.89280992294359,335.554456054423));
#24441=CARTESIAN_POINT('Ctrl Pts',(183.82668920005,5.87393804654573,335.7104803923));
#24442=CARTESIAN_POINT('Ctrl Pts',(183.834114367373,5.85503938001932,335.866726219126));
#24443=CARTESIAN_POINT('Ctrl Pts',(183.841539534695,5.82992373382684,336.022040139743));
#24444=CARTESIAN_POINT('Ctrl Pts',(183.848964702017,5.79872318251752,336.175899661975));
#24445=CARTESIAN_POINT('Ctrl Pts',(183.852808073467,5.78257333660411,336.255539523199));
#24446=CARTESIAN_POINT('Ctrl Pts',(183.856651444917,5.76479401531116,336.334789961192));
#24447=CARTESIAN_POINT('Ctrl Pts',(183.860494816368,5.745408700489,336.413580357406));
#24448=CARTESIAN_POINT('Ctrl Pts',(183.86792119583,5.70795129994161,336.565823612539));
#24449=CARTESIAN_POINT('Ctrl Pts',(183.875347575292,5.66438224827763,336.71680545197));
#24450=CARTESIAN_POINT('Ctrl Pts',(183.882773954755,5.61480040370371,336.865997585494));
#24451=CARTESIAN_POINT('Ctrl Pts',(183.890191591026,5.5652769326017,337.015014072813));
#24452=CARTESIAN_POINT('Ctrl Pts',(183.897609227296,5.50975487603878,337.162244697913));
#24453=CARTESIAN_POINT('Ctrl Pts',(183.905026863567,5.44838390601436,337.307172159849));
#24454=CARTESIAN_POINT('Ctrl Pts',(183.912437380672,5.3870718375205,337.451960525902));
#24455=CARTESIAN_POINT('Ctrl Pts',(183.919847897777,5.31992217573912,337.59444978839));
#24456=CARTESIAN_POINT('Ctrl Pts',(183.927258414882,5.24713408733631,337.734138700215));
#24457=CARTESIAN_POINT('Ctrl Pts',(183.934663431263,5.17440002851701,337.873723922907));
#24458=CARTESIAN_POINT('Ctrl Pts',(183.942068447645,5.09603604838222,338.01051260459));
#24459=CARTESIAN_POINT('Ctrl Pts',(183.949473464026,5.01228897675539,338.144024455375));
#24460=CARTESIAN_POINT('Ctrl Pts',(183.956874593786,4.92858586089307,338.277466230689));
#24461=CARTESIAN_POINT('Ctrl Pts',(183.964275723546,4.83950547821191,338.407634285279));
#24462=CARTESIAN_POINT('Ctrl Pts',(183.971676853306,4.74533999730428,338.534073976657));
#24463=CARTESIAN_POINT('Ctrl Pts',(183.979076770668,4.65118994188332,338.660492955628));
#24464=CARTESIAN_POINT('Ctrl Pts',(183.98647668803,4.55195666401408,338.783184484726));
#24465=CARTESIAN_POINT('Ctrl Pts',(183.993876605392,4.44797502577763,338.901723815515));
#24466=CARTESIAN_POINT('Ctrl Pts',(184.001276206797,4.34399782728575,339.020258084984));
#24467=CARTESIAN_POINT('Ctrl Pts',(184.008675808202,4.23527291747377,339.1346402283));
#24468=CARTESIAN_POINT('Ctrl Pts',(184.016075409607,4.12217454982721,339.244479655182));
#24469=CARTESIAN_POINT('Ctrl Pts',(184.023476152596,4.00905873375754,339.35433602771));
#24470=CARTESIAN_POINT('Ctrl Pts',(184.030876895586,3.89156838392223,339.4596480285));
#24471=CARTESIAN_POINT('Ctrl Pts',(184.038277638576,3.77011349337935,339.560063026926));
#24472=CARTESIAN_POINT('Ctrl Pts',(184.045680981094,3.64861594152358,339.660513296354));
#24473=CARTESIAN_POINT('Ctrl Pts',(184.053084323611,3.52315136358953,339.75606290121));
#24474=CARTESIAN_POINT('Ctrl Pts',(184.060487666129,3.39416146581732,339.846400572225));
#24475=CARTESIAN_POINT('Ctrl Pts',(184.0678991236,3.26503017962389,339.936837264177));
#24476=CARTESIAN_POINT('Ctrl Pts',(184.07531058107,3.1323661622583,340.022050399218));
#24477=CARTESIAN_POINT('Ctrl Pts',(184.082722038541,2.99663925388541,340.101772608082));
#24478=CARTESIAN_POINT('Ctrl Pts',(184.090138057114,2.86082881748993,340.181543878982));
#24479=CARTESIAN_POINT('Ctrl Pts',(184.097554075688,2.72195206212223,340.255817314652));
#24480=CARTESIAN_POINT('Ctrl Pts',(184.104970094261,2.58050139879679,340.324372553955));
#24481=CARTESIAN_POINT('Ctrl Pts',(184.112396641331,2.43884991844474,340.393025120898));
#24482=CARTESIAN_POINT('Ctrl Pts',(184.1198231884,2.29461757291683,340.455943129235));
#24483=CARTESIAN_POINT('Ctrl Pts',(184.12724973547,2.14831537803079,340.512954888172));
#24484=CARTESIAN_POINT('Ctrl Pts',(184.131077440527,2.07290999165573,340.542339230039));
#24485=CARTESIAN_POINT('Ctrl Pts',(184.134905145584,1.99695499345246,340.570155418434));
#24486=CARTESIAN_POINT('Ctrl Pts',(184.138732850641,1.92052157876961,340.596385210829));
#24487=CARTESIAN_POINT('Ctrl Pts',(184.146147643844,1.77245950104464,340.647195940354));
#24488=CARTESIAN_POINT('Ctrl Pts',(184.153562437047,1.6221530117845,340.692204502841));
#24489=CARTESIAN_POINT('Ctrl Pts',(184.16097723025,1.47009814711048,340.731207726157));
#24490=CARTESIAN_POINT('Ctrl Pts',(184.168383247424,1.31822325210573,340.770164785892));
#24491=CARTESIAN_POINT('Ctrl Pts',(184.175789264598,1.16460445945112,340.803130561944));
#24492=CARTESIAN_POINT('Ctrl Pts',(184.183195281773,1.0097561678994,340.829950518134));
#24493=CARTESIAN_POINT('Ctrl Pts',(184.190594158053,0.855057181322792,340.856744614478));
#24494=CARTESIAN_POINT('Ctrl Pts',(184.197993034333,0.699131422039454,340.877404624149));
#24495=CARTESIAN_POINT('Ctrl Pts',(184.205391910613,0.542506666056472,340.891826294095));
#24496=CARTESIAN_POINT('Ctrl Pts',(184.212785275444,0.385998580423634,340.906237221286));
#24497=CARTESIAN_POINT('Ctrl Pts',(184.220178640274,0.228792905828073,340.914419026937));
#24498=CARTESIAN_POINT('Ctrl Pts',(184.227572005105,0.0714256663736467,
340.916318867056));
#24499=CARTESIAN_POINT('Ctrl Pts',(184.234961483519,-0.0858588509889629,
340.9182177085));
#24500=CARTESIAN_POINT('Ctrl Pts',(184.242350961933,-0.243304390835582,
340.913841156131));
#24501=CARTESIAN_POINT('Ctrl Pts',(184.249740440347,-0.400371899099182,
340.903188367731));
#24502=CARTESIAN_POINT('Ctrl Pts',(184.257128743439,-0.557414425237863,
340.892537273693));
#24503=CARTESIAN_POINT('Ctrl Pts',(184.264517046532,-0.714078666085097,
340.875611949497));
#24504=CARTESIAN_POINT('Ctrl Pts',(184.271905349624,-0.869827551905739,
340.85246363444));
#24505=CARTESIAN_POINT('Ctrl Pts',(184.279293360726,-1.02557028243996,340.829316234219));
#24506=CARTESIAN_POINT('Ctrl Pts',(184.286681371828,-1.18039735969538,340.799946387029));
#24507=CARTESIAN_POINT('Ctrl Pts',(184.294069382931,-1.3337790936864,340.76445694682));
#24508=CARTESIAN_POINT('Ctrl Pts',(184.301458569383,-1.48718522899295,340.728961860639));
#24509=CARTESIAN_POINT('Ctrl Pts',(184.308847755835,-1.63914519859986,340.687345327382));
#24510=CARTESIAN_POINT('Ctrl Pts',(184.316236942287,-1.78914188283228,340.639760800388));
#24511=CARTESIAN_POINT('Ctrl Pts',(184.323628771864,-1.93919222114951,340.592159252323));
#24512=CARTESIAN_POINT('Ctrl Pts',(184.331020601442,-2.08727751945924,340.538585573466));
#24513=CARTESIAN_POINT('Ctrl Pts',(184.338412431019,-2.23289828462096,340.479242266321));
#24514=CARTESIAN_POINT('Ctrl Pts',(184.345812499641,-2.37868136087638,340.419832814233));
#24515=CARTESIAN_POINT('Ctrl Pts',(184.353212568262,-2.521994071378,340.354641032428));
#24516=CARTESIAN_POINT('Ctrl Pts',(184.360612636884,-2.66235862400008,340.283916835049));
#24517=CARTESIAN_POINT('Ctrl Pts',(184.368017319712,-2.80281069890818,340.21314853862));
#24518=CARTESIAN_POINT('Ctrl Pts',(184.375422002539,-2.94031062676973,340.136841134336));
#24519=CARTESIAN_POINT('Ctrl Pts',(184.382826685367,-3.07440796947533,340.055288933357));
#24520=CARTESIAN_POINT('Ctrl Pts',(184.390242077437,-3.20869925445112,339.973618785082));
#24521=CARTESIAN_POINT('Ctrl Pts',(184.397657469507,-3.33957781514952,339.886688897118));
#24522=CARTESIAN_POINT('Ctrl Pts',(184.405072861577,-3.46662410392826,339.794835543015));
#24523=CARTESIAN_POINT('Ctrl Pts',(184.409038869357,-3.53457284687054,339.74570919697));
#24524=CARTESIAN_POINT('Ctrl Pts',(184.413004877136,-3.60142596182236,339.695175174371));
#24525=CARTESIAN_POINT('Ctrl Pts',(184.416970884915,-3.66712353095129,339.643289305142));
#24526=CARTESIAN_POINT('Ctrl Pts',(184.424315854089,-3.78879414960982,339.547197685734));
#24527=CARTESIAN_POINT('Ctrl Pts',(184.431660823263,-3.90688829422341,339.446159993294));
#24528=CARTESIAN_POINT('Ctrl Pts',(184.439005792438,-4.02097117590753,339.340474785668));
#24529=CARTESIAN_POINT('Ctrl Pts',(184.446342029751,-4.13491843334505,339.234915218949));
#24530=CARTESIAN_POINT('Ctrl Pts',(184.453678267064,-4.24486363906911,339.124719387582));
#24531=CARTESIAN_POINT('Ctrl Pts',(184.461014504377,-4.35040260922375,339.010227886313));
#24532=CARTESIAN_POINT('Ctrl Pts',(184.468343705105,-4.45584035120531,338.895846200077));
#24533=CARTESIAN_POINT('Ctrl Pts',(184.475672905833,-4.55688001118919,338.77717732259));
#24534=CARTESIAN_POINT('Ctrl Pts',(184.483002106562,-4.65315220035627,338.654600547641));
#24535=CARTESIAN_POINT('Ctrl Pts',(184.490325959316,-4.74935414159845,338.532113214557));
#24536=CARTESIAN_POINT('Ctrl Pts',(184.497649812071,-4.84079530148923,338.4057239592));
#24537=CARTESIAN_POINT('Ctrl Pts',(184.504973664825,-4.92714490377433,338.275847014088));
#24538=CARTESIAN_POINT('Ctrl Pts',(184.512294282053,-5.01345635858973,338.146027445927));
#24539=CARTESIAN_POINT('Ctrl Pts',(184.519614899281,-5.09468052050149,338.012723571383));
#24540=CARTESIAN_POINT('Ctrl Pts',(184.526935516509,-5.17052857858857,337.876380499951));
#24541=CARTESIAN_POINT('Ctrl Pts',(184.53425459916,-5.24636073710885,337.740066009288));
#24542=CARTESIAN_POINT('Ctrl Pts',(184.541573681811,-5.31681884834582,337.600713922922));
#24543=CARTESIAN_POINT('Ctrl Pts',(184.548892764463,-5.38165903229536,337.458795766755));
#24544=CARTESIAN_POINT('Ctrl Pts',(184.556211832807,-5.44649908949729,337.316877888006));
#24545=CARTESIAN_POINT('Ctrl Pts',(184.563530901151,-5.50572108288589,337.172394297112));
#24546=CARTESIAN_POINT('Ctrl Pts',(184.570849969495,-5.55912855969106,337.025838152303));
#24547=CARTESIAN_POINT('Ctrl Pts',(184.578170543571,-5.61254702386355,336.879251856918));
#24548=CARTESIAN_POINT('Ctrl Pts',(184.585491117646,-5.66014846107913,336.730592518268));
#24549=CARTESIAN_POINT('Ctrl Pts',(184.592811691721,-5.70178581912152,336.5803699046));
#24550=CARTESIAN_POINT('Ctrl Pts',(184.600138780446,-5.74346023065446,336.430013606364));
#24551=CARTESIAN_POINT('Ctrl Pts',(184.607465869172,-5.7791598637499,336.278091623847));
#24552=CARTESIAN_POINT('Ctrl Pts',(184.614792957897,-5.80878836913647,336.125125879662));
#24553=CARTESIAN_POINT('Ctrl Pts',(184.622123775781,-5.83843195410075,335.972082282787));
#24554=CARTESIAN_POINT('Ctrl Pts',(184.629454593666,-5.8619981987883,335.817994243005));
#24555=CARTESIAN_POINT('Ctrl Pts',(184.63678541155,-5.87944255883285,335.663389598867));
#24556=CARTESIAN_POINT('Ctrl Pts',(184.644125337449,-5.89690859224144,335.508592869567));
#24557=CARTESIAN_POINT('Ctrl Pts',(184.651465263347,-5.90823752770803,335.353278634368));
#24558=CARTESIAN_POINT('Ctrl Pts',(184.658805189246,-5.91343690518207,335.197976086765));
#24559=CARTESIAN_POINT('Ctrl Pts',(184.661970666252,-5.91567923161252,335.130999028657));
#24560=CARTESIAN_POINT('Ctrl Pts',(184.665136143258,-5.91678216518749,335.064024102548));
#24561=CARTESIAN_POINT('Ctrl Pts',(184.668301620265,-5.91674928609117,334.997093448832));
#24562=CARTESIAN_POINT('Origin',(188.466817376509,0.,335.));
#24563=CARTESIAN_POINT('',(5.59181737646044,-4.91824899013927,335.003151744596));
#24564=CARTESIAN_POINT('',(5.23193167942401,-1.34848449270165,339.730361626982));
#24565=CARTESIAN_POINT('Ctrl Pts',(5.59181737646048,-4.91824899013927,335.003151744596));
#24566=CARTESIAN_POINT('Ctrl Pts',(5.58294884481862,-4.91814826821296,335.160326762204));
#24567=CARTESIAN_POINT('Ctrl Pts',(5.57408031317672,-4.9105091665031,335.317206178995));
#24568=CARTESIAN_POINT('Ctrl Pts',(5.56521178153488,-4.89544054547172,335.47312252985));
#24569=CARTESIAN_POINT('Ctrl Pts',(5.55630199600642,-4.88030182950141,335.62976415922));
#24570=CARTESIAN_POINT('Ctrl Pts',(5.54739221047797,-4.85766442287388,335.785433593565));
#24571=CARTESIAN_POINT('Ctrl Pts',(5.53848242494951,-4.82768834052904,335.939472378104));
#24572=CARTESIAN_POINT('Ctrl Pts',(5.5295184298106,-4.79752987537137,336.094448377402));
#24573=CARTESIAN_POINT('Ctrl Pts',(5.52055443467166,-4.75994324974078,336.247773676907));
#24574=CARTESIAN_POINT('Ctrl Pts',(5.51159043953274,-4.71514005962174,336.398798513243));
#24575=CARTESIAN_POINT('Ctrl Pts',(5.50436251686681,-4.67901398097615,336.520574107802));
#24576=CARTESIAN_POINT('Ctrl Pts',(5.49713459420093,-4.63819689184413,336.640854391806));
#24577=CARTESIAN_POINT('Ctrl Pts',(5.48990667153501,-4.59282194495883,336.759309422587));
#24578=CARTESIAN_POINT('Ctrl Pts',(5.48227368227759,-4.54490409938414,336.884402899542));
#24579=CARTESIAN_POINT('Ctrl Pts',(5.47464069302027,-4.49178076133987,337.007774141784));
#24580=CARTESIAN_POINT('Ctrl Pts',(5.46700770376285,-4.43359543719221,337.128946819864));
#24581=CARTESIAN_POINT('Ctrl Pts',(5.45938429306256,-4.37548312918977,337.249967439637));
#24582=CARTESIAN_POINT('Ctrl Pts',(5.4517608823622,-4.31232163831185,337.368794618869));
#24583=CARTESIAN_POINT('Ctrl Pts',(5.44413747166192,-4.24430379017305,337.484968490589));
#24584=CARTESIAN_POINT('Ctrl Pts',(5.43652165353137,-4.17635368471205,337.601026658427));
#24585=CARTESIAN_POINT('Ctrl Pts',(5.4289058354008,-4.1035570438768,337.714436426043));
#24586=CARTESIAN_POINT('Ctrl Pts',(5.42129001727025,-4.02615396193197,337.8247596955));
#24587=CARTESIAN_POINT('Ctrl Pts',(5.41339890657748,-3.94595295435561,337.9390708721));
#24588=CARTESIAN_POINT('Ctrl Pts',(5.40550779588471,-3.86080638509852,338.050067802952));
#24589=CARTESIAN_POINT('Ctrl Pts',(5.39761668519193,-3.77103258556973,338.157292558676));
#24590=CARTESIAN_POINT('Ctrl Pts',(5.39000943705944,-3.68448816927644,338.26066017757));
#24591=CARTESIAN_POINT('Ctrl Pts',(5.38240218892692,-3.59364395540761,338.360521977631));
#24592=CARTESIAN_POINT('Ctrl Pts',(5.37479494079443,-3.49882770338158,338.456499351157));
#24593=CARTESIAN_POINT('Ctrl Pts',(5.36718883430481,-3.40402568071896,338.552462321067));
#24594=CARTESIAN_POINT('Ctrl Pts',(5.3595827278152,-3.30525309005061,338.644541734526));
#24595=CARTESIAN_POINT('Ctrl Pts',(5.35197662132558,-3.20287540405726,338.732394969532));
#24596=CARTESIAN_POINT('Ctrl Pts',(5.34436987818154,-3.10048914873791,338.820255558122));
#24597=CARTESIAN_POINT('Ctrl Pts',(5.33676313503756,-2.99449750653069,338.903889000905));
#24598=CARTESIAN_POINT('Ctrl Pts',(5.32915639189352,-2.8852994839743,338.982992587274));
#24599=CARTESIAN_POINT('Ctrl Pts',(5.32154723335298,-2.77606678737726,339.062121291689));
#24600=CARTESIAN_POINT('Ctrl Pts',(5.31393807481246,-2.66362601507148,339.136717042431));
#24601=CARTESIAN_POINT('Ctrl Pts',(5.30632891627192,-2.54840511175222,339.206520468142));
#24602=CARTESIAN_POINT('Ctrl Pts',(5.29871147467145,-2.4330587830468,339.276399879385));
#24603=CARTESIAN_POINT('Ctrl Pts',(5.29109403307089,-2.31492663129186,339.341476344963));
#24604=CARTESIAN_POINT('Ctrl Pts',(5.28347659147042,-2.19446132130872,339.401536387647));
#24605=CARTESIAN_POINT('Ctrl Pts',(5.27585421093814,-2.07391790505556,339.461635371549));
#24606=CARTESIAN_POINT('Ctrl Pts',(5.26823183040589,-1.95103868932618,339.51671129508));
#24607=CARTESIAN_POINT('Ctrl Pts',(5.26060944987361,-1.82629492513081,339.566599381262));
#24608=CARTESIAN_POINT('Ctrl Pts',(5.25297632621633,-1.70137534475228,339.616557780641));
#24609=CARTESIAN_POINT('Ctrl Pts',(5.24534320255909,-1.57458635373703,339.661313621609));
#24610=CARTESIAN_POINT('Ctrl Pts',(5.23771007890181,-1.44641306659626,339.700752312479));
#24611=CARTESIAN_POINT('Ctrl Pts',(5.23577450614907,-1.41391146785913,339.710752996194));
#24612=CARTESIAN_POINT('Ctrl Pts',(5.23383893339626,-1.38132090062803,339.72041204255));
#24613=CARTESIAN_POINT('Ctrl Pts',(5.23190336064351,-1.3486493481772,339.729728110384));
#24614=CARTESIAN_POINT('',(5.23167681249902,-4.9112521298426,335.262270050933));
#24615=CARTESIAN_POINT('Origin',(5.23167681249902,0.,335.));
#24616=CARTESIAN_POINT('',(5.24653624849023,-4.91824999747317,335.000157655271));
#24617=CARTESIAN_POINT('Ctrl Pts',(5.24642228163471,-4.91824999767384,335.000151265622));
#24618=CARTESIAN_POINT('Ctrl Pts',(5.24397986243382,-4.91824865336932,335.043859978905));
#24619=CARTESIAN_POINT('Ctrl Pts',(5.24153110386067,-4.91766464706679,335.087566327886));
#24620=CARTESIAN_POINT('Ctrl Pts',(5.23758208828115,-4.91578984846743,335.157789839972));
#24621=CARTESIAN_POINT('Ctrl Pts',(5.23608712158552,-4.91486678856396,335.184314674874));
#24622=CARTESIAN_POINT('Ctrl Pts',(5.23402713173893,-4.91330267985276,335.220768624878));
#24623=CARTESIAN_POINT('Ctrl Pts',(5.23346506070249,-4.91284612511964,335.230705351861));
#24624=CARTESIAN_POINT('Ctrl Pts',(5.23268937633593,-4.91217505978087,335.244404262925));
#24625=CARTESIAN_POINT('Ctrl Pts',(5.23247619177751,-4.91198636488289,335.248167711058));
#24626=CARTESIAN_POINT('Ctrl Pts',(5.2320676217224,-4.91161656743763,335.255377499067));
#24627=CARTESIAN_POINT('Ctrl Pts',(5.23187224807966,-4.91143616218491,335.25882387311));
#24628=CARTESIAN_POINT('Ctrl Pts',(5.23167681249902,-4.91125212984261,335.262270050933));
#24629=CARTESIAN_POINT('',(6.99653624843812,-4.91824865609062,335.003635844163));
#24630=CARTESIAN_POINT('Ctrl Pts',(6.99653624843808,-4.91824865609062,335.003635844164));
#24631=CARTESIAN_POINT('Ctrl Pts',(6.9875721074894,-4.91813125822212,335.162441305286));
#24632=CARTESIAN_POINT('Ctrl Pts',(6.97860796654071,-4.91031842803173,335.320932586525));
#24633=CARTESIAN_POINT('Ctrl Pts',(6.96964382559202,-4.89492490528823,335.478427877625));
#24634=CARTESIAN_POINT('Ctrl Pts',(6.96063104327979,-4.8794478539679,335.636777772168));
#24635=CARTESIAN_POINT('Ctrl Pts',(6.95161826096759,-4.85630772715498,335.79412071973));
#24636=CARTESIAN_POINT('Ctrl Pts',(6.94260547865537,-4.8256704477217,335.949783023898));
#24637=CARTESIAN_POINT('Ctrl Pts',(6.93353337589111,-4.79483151942994,336.106469868317));
#24638=CARTESIAN_POINT('Ctrl Pts',(6.92446127312678,-4.75639650641198,336.261453756748));
#24639=CARTESIAN_POINT('Ctrl Pts',(6.91538917036252,-4.71058301455425,336.41406885458));
#24640=CARTESIAN_POINT('Ctrl Pts',(6.91062778628924,-4.68653835411107,336.494167053976));
#24641=CARTESIAN_POINT('Ctrl Pts',(6.90586640221596,-4.66046204998375,336.57361312166));
#24642=CARTESIAN_POINT('Ctrl Pts',(6.90110501814269,-4.63239073199686,336.652313277986));
#24643=CARTESIAN_POINT('Ctrl Pts',(6.89333955794828,-4.58660851844781,336.780667328371));
#24644=CARTESIAN_POINT('Ctrl Pts',(6.8855740977539,-4.5354142221827,336.907322892402));
#24645=CARTESIAN_POINT('Ctrl Pts',(6.8778086375595,-4.4789526218565,337.031788983547));
#24646=CARTESIAN_POINT('Ctrl Pts',(6.87005276090548,-4.42256070214335,337.15610146811));
#24647=CARTESIAN_POINT('Ctrl Pts',(6.86229688425144,-4.36091457216383,337.278229502424));
#24648=CARTESIAN_POINT('Ctrl Pts',(6.85454100759742,-4.29420840917725,337.397698313185));
#24649=CARTESIAN_POINT('Ctrl Pts',(6.84679283639659,-4.22756851867525,337.517048431841));
#24650=CARTESIAN_POINT('Ctrl Pts',(6.83904466519573,-4.15587878875334,337.633744244314));
#24651=CARTESIAN_POINT('Ctrl Pts',(6.8312964939949,-4.0793808491045,337.747332333457));
#24652=CARTESIAN_POINT('Ctrl Pts',(6.82355415692612,-4.00294051002624,337.860834894301));
#24653=CARTESIAN_POINT('Ctrl Pts',(6.81581181985734,-3.92169938519247,337.971234065519));
#24654=CARTESIAN_POINT('Ctrl Pts',(6.80806948278857,-3.83594406774055,338.078102690241));
#24655=CARTESIAN_POINT('Ctrl Pts',(6.80033038945911,-3.75022467844475,338.184926541148));
#24656=CARTESIAN_POINT('Ctrl Pts',(6.7925912961297,-3.65999510250297,338.28822248214));
#24657=CARTESIAN_POINT('Ctrl Pts',(6.78485220280024,-3.56558398808006,338.387594114773));
#24658=CARTESIAN_POINT('Ctrl Pts',(6.77711469667717,-3.47119223638064,338.486945367333));
#24659=CARTESIAN_POINT('Ctrl Pts',(6.76937719055405,-3.37262092166138,338.582373628314));
#24660=CARTESIAN_POINT('Ctrl Pts',(6.76163968443097,-3.2702372611815,338.673517567411));
#24661=CARTESIAN_POINT('Ctrl Pts',(6.75390207966681,-3.16785229547017,338.764662668451));
#24662=CARTESIAN_POINT('Ctrl Pts',(6.74616447490265,-3.06165517986055,338.851523078124));
#24663=CARTESIAN_POINT('Ctrl Pts',(6.73842687013848,-2.95204776861541,338.933776434206));
#24664=CARTESIAN_POINT('Ctrl Pts',(6.73068748116974,-2.84241508313472,339.016048756986));
#24665=CARTESIAN_POINT('Ctrl Pts',(6.72294809220104,-2.72937085069569,339.093711677129));
#24666=CARTESIAN_POINT('Ctrl Pts',(6.71520870323229,-2.61334722851598,339.166485248469));
#24667=CARTESIAN_POINT('Ctrl Pts',(6.70746096922121,-2.49719850317336,339.239337288346));
#24668=CARTESIAN_POINT('Ctrl Pts',(6.69971323521017,-2.37806430335908,339.307289239703));
#24669=CARTESIAN_POINT('Ctrl Pts',(6.69196550119909,-2.25640327777048,339.370106098319));
#24670=CARTESIAN_POINT('Ctrl Pts',(6.68421357162419,-2.134676370132,339.432956973609));
#24671=CARTESIAN_POINT('Ctrl Pts',(6.67646164204922,-2.01042026567888,339.490667050703));
#24672=CARTESIAN_POINT('Ctrl Pts',(6.66870971247431,-1.88411412421237,339.543049309599));
#24673=CARTESIAN_POINT('Ctrl Pts',(6.66094518694225,-1.757602750393,339.595516683392));
#24674=CARTESIAN_POINT('Ctrl Pts',(6.65318066141019,-1.62903505135232,339.642638804876));
#24675=CARTESIAN_POINT('Ctrl Pts',(6.64541613587812,-1.49890674927308,339.684278132165));
#24676=CARTESIAN_POINT('Ctrl Pts',(6.63789975187495,-1.37293713476548,339.7245867347));
#24677=CARTESIAN_POINT('Ctrl Pts',(6.63038336787179,-1.2455054622397,339.759757597904));
#24678=CARTESIAN_POINT('Ctrl Pts',(6.62286698386862,-1.11706899699421,339.789711882614));
#24679=CARTESIAN_POINT('Ctrl Pts',(6.61508110872127,-0.984027592730366,
339.820740143115));
#24680=CARTESIAN_POINT('Ctrl Pts',(6.60729523357391,-0.849484422885444,
339.84626958899));
#24681=CARTESIAN_POINT('Ctrl Pts',(6.59950935842656,-0.713933148047497,
339.866156853475));
#24682=CARTESIAN_POINT('Ctrl Pts',(6.59173308917978,-0.578549110937317,
339.886019581849));
#24683=CARTESIAN_POINT('Ctrl Pts',(6.583956819933,-0.442159825650675,339.900253924114));
#24684=CARTESIAN_POINT('Ctrl Pts',(6.57618055068622,-0.305271916830737,
339.908766863408));
#24685=CARTESIAN_POINT('Ctrl Pts',(6.56841202985661,-0.168520405631501,
339.917271320253));
#24686=CARTESIAN_POINT('Ctrl Pts',(6.56064350902701,-0.0312716461794746,
339.920065695812));
#24687=CARTESIAN_POINT('Ctrl Pts',(6.5528749881974,0.105960125494544,339.917108450533));
#24688=CARTESIAN_POINT('Ctrl Pts',(6.54511236494098,0.243087715891905,339.914153450286));
#24689=CARTESIAN_POINT('Ctrl Pts',(6.53734974168456,0.380197956106048,339.905455529135));
#24690=CARTESIAN_POINT('Ctrl Pts',(6.52958711842814,0.516774441849578,339.891025172574));
#24691=CARTESIAN_POINT('Ctrl Pts',(6.52182790550408,0.653290925813578,339.876601155662));
#24692=CARTESIAN_POINT('Ctrl Pts',(6.51406869257998,0.789273735022939,339.856449754032));
#24693=CARTESIAN_POINT('Ctrl Pts',(6.50630947965593,0.924209640464846,339.830633457733));
#24694=CARTESIAN_POINT('Ctrl Pts',(6.49855195806881,1.0591161328615,339.804822788817));
#24695=CARTESIAN_POINT('Ctrl Pts',(6.49079443648172,1.19297579291594,339.773349754805));
#24696=CARTESIAN_POINT('Ctrl Pts',(6.4830369148946,1.32528403122262,339.736328250775));
#24697=CARTESIAN_POINT('Ctrl Pts',(6.47527941721663,1.45759186174725,339.699306860846));
#24698=CARTESIAN_POINT('Ctrl Pts',(6.46752191953871,1.58834790469237,339.656737139788));
#24699=CARTESIAN_POINT('Ctrl Pts',(6.45976442186074,1.7170615883802,339.608783197788));
#24700=CARTESIAN_POINT('Ctrl Pts',(6.45200528104205,1.84580253533055,339.560819098507));
#24701=CARTESIAN_POINT('Ctrl Pts',(6.44424614022329,1.97249989704015,339.507468644903));
#24702=CARTESIAN_POINT('Ctrl Pts',(6.43648699940459,2.09668233708145,339.448944396132));
#24703=CARTESIAN_POINT('Ctrl Pts',(6.4287198465573,2.2209930069466,339.390359715675));
#24704=CARTESIAN_POINT('Ctrl Pts',(6.42095269371003,2.34278321442726,339.326590734277));
#24705=CARTESIAN_POINT('Ctrl Pts',(6.41318554086274,2.46160504845533,339.257896622503));
#24706=CARTESIAN_POINT('Ctrl Pts',(6.40541434316659,2.5804887605448,339.18916673735));
#24707=CARTESIAN_POINT('Ctrl Pts',(6.39764314547041,2.69640068985791,339.115506819574));
#24708=CARTESIAN_POINT('Ctrl Pts',(6.38987194777425,2.80892209012275,339.037219309639));
#24709=CARTESIAN_POINT('Ctrl Pts',(6.38208860479573,2.92161934541431,338.958809447403));
#24710=CARTESIAN_POINT('Ctrl Pts',(6.37430526181726,3.03091517216052,338.875757776469));
#24711=CARTESIAN_POINT('Ctrl Pts',(6.36652191883874,3.1364234047622,338.788407487132));
#24712=CARTESIAN_POINT('Ctrl Pts',(6.35922426242407,3.23534784283099,338.70650792276));
#24713=CARTESIAN_POINT('Ctrl Pts',(6.35192660600942,3.33094277749661,338.620830027704));
#24714=CARTESIAN_POINT('Ctrl Pts',(6.34462894959475,3.42292067035136,338.531684746262));
#24715=CARTESIAN_POINT('Ctrl Pts',(6.33684095463579,3.52107867138376,338.436549683301));
#24716=CARTESIAN_POINT('Ctrl Pts',(6.32905295967686,3.61541782527226,338.337173565241));
#24717=CARTESIAN_POINT('Ctrl Pts',(6.32126496471793,3.70555070628905,338.233895023902));
#24718=CARTESIAN_POINT('Ctrl Pts',(6.31348639933423,3.79557445590721,338.13074153051));
#24719=CARTESIAN_POINT('Ctrl Pts',(6.3057078339505,3.88140181321909,338.023695306643));
#24720=CARTESIAN_POINT('Ctrl Pts',(6.2979292685668,3.962680769067,337.913133053083));
#24721=CARTESIAN_POINT('Ctrl Pts',(6.2901582801599,4.04388055237707,337.802678496456));
#24722=CARTESIAN_POINT('Ctrl Pts',(6.28238729175301,4.12054052275392,337.688715038205));
#24723=CARTESIAN_POINT('Ctrl Pts',(6.27461630334611,4.19234791897143,337.571653551471));
#24724=CARTESIAN_POINT('Ctrl Pts',(6.26685104578577,4.26410235961257,337.454678393707));
#24725=CARTESIAN_POINT('Ctrl Pts',(6.25908578822542,4.33101114693228,337.33461008598));
#24726=CARTESIAN_POINT('Ctrl Pts',(6.25132053066508,4.39280416044029,337.211889389305));
#24727=CARTESIAN_POINT('Ctrl Pts',(6.24355844243135,4.4545719536333,337.089218780082));
#24728=CARTESIAN_POINT('Ctrl Pts',(6.23579635419759,4.51122795118491,336.963898282126));
#24729=CARTESIAN_POINT('Ctrl Pts',(6.22803426596386,4.5625475281804,336.836394052374));
#24730=CARTESIAN_POINT('Ctrl Pts',(6.22027372317695,4.61385688734857,336.708915208962));
#24731=CARTESIAN_POINT('Ctrl Pts',(6.21251318039004,4.6598317942243,336.579253859601));
#24732=CARTESIAN_POINT('Ctrl Pts',(6.20475263760312,4.70029556895248,336.44789662165));
#24733=CARTESIAN_POINT('Ctrl Pts',(6.19699197664848,4.7407599598118,336.316537383558));
#24734=CARTESIAN_POINT('Ctrl Pts',(6.18923131569386,4.77571293670882,336.183482577497));
#24735=CARTESIAN_POINT('Ctrl Pts',(6.18147065473923,4.80502766201519,336.049234115805));
#24736=CARTESIAN_POINT('Ctrl Pts',(6.17370821228768,4.83434911665723,335.914954836735));
#24737=CARTESIAN_POINT('Ctrl Pts',(6.16594576983614,4.85802966096728,335.779481737024));
#24738=CARTESIAN_POINT('Ctrl Pts',(6.15818332738459,4.87599362602538,335.643326683311));
#24739=CARTESIAN_POINT('Ctrl Pts',(6.15041267564842,4.89397658913765,335.507027636828));
#24740=CARTESIAN_POINT('Ctrl Pts',(6.14264202391224,4.90623084514752,335.370045582226));
#24741=CARTESIAN_POINT('Ctrl Pts',(6.13487137217606,4.91273260609387,335.232897839239));
#24742=CARTESIAN_POINT('Ctrl Pts',(6.12709656270277,4.91923784584918,335.095676714471));
#24743=CARTESIAN_POINT('Ctrl Pts',(6.11932175322947,4.91998445487191,334.958290113788));
#24744=CARTESIAN_POINT('Ctrl Pts',(6.11154694375617,4.91500081266808,334.821254163763));
#24745=CARTESIAN_POINT('Ctrl Pts',(6.10375983529211,4.91000928682805,334.684001436222));
#24746=CARTESIAN_POINT('Ctrl Pts',(6.09597272682799,4.89926942609259,334.547100856136));
#24747=CARTESIAN_POINT('Ctrl Pts',(6.08818561836392,4.88286150040578,334.41106313551));
#24748=CARTESIAN_POINT('Ctrl Pts',(6.08092071734951,4.86755389855118,334.28414817354));
#24749=CARTESIAN_POINT('Ctrl Pts',(6.07365581633523,4.84731351523526,334.157984389752));
#24750=CARTESIAN_POINT('Ctrl Pts',(6.06639091532082,4.82224507075424,334.032975936139));
#24751=CARTESIAN_POINT('Ctrl Pts',(6.05868386149048,4.79565092299157,333.900359279789));
#24752=CARTESIAN_POINT('Ctrl Pts',(6.05097680766012,4.76353558103867,333.768609417271));
#24753=CARTESIAN_POINT('Ctrl Pts',(6.04326975382978,4.72596638014111,333.638227318428));
#24754=CARTESIAN_POINT('Ctrl Pts',(6.03557234821298,4.68844421092145,333.508008440753));
#24755=CARTESIAN_POINT('Ctrl Pts',(6.02787494259624,4.64548187143294,333.379154299647));
#24756=CARTESIAN_POINT('Ctrl Pts',(6.02017753697945,4.59719799306904,333.2521574227));
#24757=CARTESIAN_POINT('Ctrl Pts',(6.01248784812709,4.54896252001646,333.125287862025));
#24758=CARTESIAN_POINT('Ctrl Pts',(6.00479815927465,4.4954162614158,333.000272231084));
#24759=CARTESIAN_POINT('Ctrl Pts',(5.99710847042229,4.43672799044302,332.877589153505));
#24760=CARTESIAN_POINT('Ctrl Pts',(5.98942457450589,4.37808393158358,332.754998497768));
#24761=CARTESIAN_POINT('Ctrl Pts',(5.98174067858953,4.31430573899637,332.6347372567));
#24762=CARTESIAN_POINT('Ctrl Pts',(5.97405678267313,4.24561058229956,332.517264845787));
#24763=CARTESIAN_POINT('Ctrl Pts',(5.96631078677204,4.17636024262972,332.398843042144));
#24764=CARTESIAN_POINT('Ctrl Pts',(5.95856479087094,4.10211325683485,332.283255729738));
#24765=CARTESIAN_POINT('Ctrl Pts',(5.95081879496985,4.02313991562323,332.170949226009));
#24766=CARTESIAN_POINT('Ctrl Pts',(5.94313933023576,3.94484488467923,332.059607334558));
#24767=CARTESIAN_POINT('Ctrl Pts',(5.9354598655017,3.86190462297316,331.951490431564));
#24768=CARTESIAN_POINT('Ctrl Pts',(5.9277804007676,3.77462613599108,331.847004504286));
#24769=CARTESIAN_POINT('Ctrl Pts',(5.92010062424812,3.68734410551248,331.742514334892));
#24770=CARTESIAN_POINT('Ctrl Pts',(5.91242084772856,3.59572375435876,331.641655740437));
#24771=CARTESIAN_POINT('Ctrl Pts',(5.90474107120909,3.50011199266095,331.5448011488));
#24772=CARTESIAN_POINT('Ctrl Pts',(5.89705925050953,3.40447478130869,331.447920776696));
#24773=CARTESIAN_POINT('Ctrl Pts',(5.88937742981002,3.30484432563591,331.355046810899));
#24774=CARTESIAN_POINT('Ctrl Pts',(5.88169560911047,3.20160358580878,331.266514022815));
#24775=CARTESIAN_POINT('Ctrl Pts',(5.87390038177184,3.09683870401358,331.176674226102));
#24776=CARTESIAN_POINT('Ctrl Pts',(5.86610515443318,2.98835641543208,331.09130508047));
#24777=CARTESIAN_POINT('Ctrl Pts',(5.85830992709455,2.87658965774756,331.010712469195));
#24778=CARTESIAN_POINT('Ctrl Pts',(5.85061448468494,2.76625360086214,330.931151505573));
#24779=CARTESIAN_POINT('Ctrl Pts',(5.84291904227532,2.65271704010501,330.856245667595));
#24780=CARTESIAN_POINT('Ctrl Pts',(5.83522359986571,2.53642289726112,330.786243724567));
#24781=CARTESIAN_POINT('Ctrl Pts',(5.82737848006257,2.41786681764243,330.714880234299));
#24782=CARTESIAN_POINT('Ctrl Pts',(5.81953336025945,2.29644516878371,330.648613573096));
#24783=CARTESIAN_POINT('Ctrl Pts',(5.81168824045631,2.17264941458252,330.587656225563));
#24784=CARTESIAN_POINT('Ctrl Pts',(5.80384312065317,2.04885366038149,330.52669887803));
#24785=CARTESIAN_POINT('Ctrl Pts',(5.79599800085003,1.92268422390205,330.471050949101));
#24786=CARTESIAN_POINT('Ctrl Pts',(5.7881528810469,1.79464876300254,330.420871384209));
#24787=CARTESIAN_POINT('Ctrl Pts',(5.78026078471884,1.66584662661929,330.370391344419));
#24788=CARTESIAN_POINT('Ctrl Pts',(5.77236868839078,1.53472896145545,330.325277599703));
#24789=CARTESIAN_POINT('Ctrl Pts',(5.76447659206272,1.40177576443656,330.285744197783));
#24790=CARTESIAN_POINT('Ctrl Pts',(5.75659477697891,1.26899576909125,330.246262297079));
#24791=CARTESIAN_POINT('Ctrl Pts',(5.74871296189506,1.13438536093766,330.212346373245));
#24792=CARTESIAN_POINT('Ctrl Pts',(5.74083114681125,0.998444213537087,330.184162355835));
#24793=CARTESIAN_POINT('Ctrl Pts',(5.73295789406051,0.862650744478501,330.156008955859));
#24794=CARTESIAN_POINT('Ctrl Pts',(5.72508464130977,0.72552978188081,330.133575140134));
#24795=CARTESIAN_POINT('Ctrl Pts',(5.71721138855904,0.587595675319844,330.116976921533));
#24796=CARTESIAN_POINT('Ctrl Pts',(5.70934498637394,0.4497815860733,330.100393145143));
#24797=CARTESIAN_POINT('Ctrl Pts',(5.70147858418885,0.311156135015818,330.089634898965));
#24798=CARTESIAN_POINT('Ctrl Pts',(5.69361218200376,0.172243187547443,330.084767009913));
#24799=CARTESIAN_POINT('Ctrl Pts',(5.68575106428807,0.0334235586259079,
330.079902390997));
#24800=CARTESIAN_POINT('Ctrl Pts',(5.6778899465724,-0.105682805793181,330.080920259691));
#24801=CARTESIAN_POINT('Ctrl Pts',(5.67002882885672,-0.244547816333455,
330.087833530098));
#24802=CARTESIAN_POINT('Ctrl Pts',(5.66217060126191,-0.383361773488972,
330.094744258859));
#24803=CARTESIAN_POINT('Ctrl Pts',(5.6543123736671,-0.521934177033776,330.107546055514));
#24804=CARTESIAN_POINT('Ctrl Pts',(5.6464541460723,-0.659737884083653,330.126199738725));
#24805=CARTESIAN_POINT('Ctrl Pts',(5.6385972681182,-0.797517923520168,330.144850218189));
#24806=CARTESIAN_POINT('Ctrl Pts',(5.63074039016412,-0.934529155614134,
330.169350531977));
#24807=CARTESIAN_POINT('Ctrl Pts',(5.62288351221002,-1.0702507171905,330.199609759108));
#24808=CARTESIAN_POINT('Ctrl Pts',(5.61502644467577,-1.2059755536192,330.229869716369));
#24809=CARTESIAN_POINT('Ctrl Pts',(5.60716937714152,-1.34041028952876,330.265888780584));
#24810=CARTESIAN_POINT('Ctrl Pts',(5.59931230960726,-1.47304560802506,330.30752520527));
#24811=CARTESIAN_POINT('Ctrl Pts',(5.5914500955778,-1.60576780461264,330.349188902428));
#24812=CARTESIAN_POINT('Ctrl Pts',(5.58358788154838,-1.73668786801434,330.396477199504));
#24813=CARTESIAN_POINT('Ctrl Pts',(5.57572566751892,-1.86531252992189,330.449198726794));
#24814=CARTESIAN_POINT('Ctrl Pts',(5.56786087237617,-1.99397941846229,330.501937562214));
#24815=CARTESIAN_POINT('Ctrl Pts',(5.55999607723336,-2.12034905829143,330.560113030222));
#24816=CARTESIAN_POINT('Ctrl Pts',(5.55213128209061,-2.24394998899759,330.623486375049));
#24817=CARTESIAN_POINT('Ctrl Pts',(5.54425770267667,-2.36768897086402,330.686930502223));
#24818=CARTESIAN_POINT('Ctrl Pts',(5.53638412326274,-2.48865273318168,330.755583925014));
#24819=CARTESIAN_POINT('Ctrl Pts',(5.5285105438488,-2.60639555360929,330.829162520473));
#24820=CARTESIAN_POINT('Ctrl Pts',(5.52231197815687,-2.69908993932676,330.887088113586));
#24821=CARTESIAN_POINT('Ctrl Pts',(5.51611341246493,-2.78978853945073,330.948065313056));
#24822=CARTESIAN_POINT('Ctrl Pts',(5.509914846773,-2.87828766110725,331.011937412425));
#24823=CARTESIAN_POINT('Ctrl Pts',(5.50212555639797,-2.98949812345911,331.092200872324));
#24824=CARTESIAN_POINT('Ctrl Pts',(5.49433626602291,-3.09747411330485,331.177210125069));
#24825=CARTESIAN_POINT('Ctrl Pts',(5.48654697564788,-3.20178911311133,331.266673127402));
#24826=CARTESIAN_POINT('Ctrl Pts',(5.47876407696554,-3.30601851469403,331.356062718681));
#24827=CARTESIAN_POINT('Ctrl Pts',(5.47098117828319,-3.40659261136152,331.449898535112));
#24828=CARTESIAN_POINT('Ctrl Pts',(5.46319827960085,-3.50311582346135,331.547846673464));
#24829=CARTESIAN_POINT('Ctrl Pts',(5.45541994514562,-3.5995824301908,331.645737370807));
#24830=CARTESIAN_POINT('Ctrl Pts',(5.44764161069039,-3.69200260886747,331.747735314344));
#24831=CARTESIAN_POINT('Ctrl Pts',(5.43986327623517,-3.78001594856677,331.853468180507));
#24832=CARTESIAN_POINT('Ctrl Pts',(5.4320878010631,-3.8679969349313,331.959162179712));
#24833=CARTESIAN_POINT('Ctrl Pts',(5.42431232589101,-3.95157405965888,332.068588069951));
#24834=CARTESIAN_POINT('Ctrl Pts',(5.41653685071893,-4.03042593523069,332.181338998191));
#24835=CARTESIAN_POINT('Ctrl Pts',(5.4087605973133,-4.10928570294714,332.294101211471));
#24836=CARTESIAN_POINT('Ctrl Pts',(5.40098434390764,-4.18341904663606,332.410188814677));
#24837=CARTESIAN_POINT('Ctrl Pts',(5.39320809050201,-4.25254681278462,332.529164378682));
#24838=CARTESIAN_POINT('Ctrl Pts',(5.38573733687997,-4.31895880869057,332.643465839727));
#24839=CARTESIAN_POINT('Ctrl Pts',(5.37826658325798,-4.38075090673827,332.760432357873));
#24840=CARTESIAN_POINT('Ctrl Pts',(5.37079582963594,-4.43771507093567,332.879653799095));
#24841=CARTESIAN_POINT('Ctrl Pts',(5.36187472659634,-4.50573808495532,333.02202052881));
#24842=CARTESIAN_POINT('Ctrl Pts',(5.35295362355671,-4.56683857097974,333.167520696865));
#24843=CARTESIAN_POINT('Ctrl Pts',(5.34403252051712,-4.62078803516182,333.315511651389));
#24844=CARTESIAN_POINT('Ctrl Pts',(5.33507957933183,-4.67493003729503,333.464030764545));
#24845=CARTESIAN_POINT('Ctrl Pts',(5.32612663814647,-4.72186985838296,333.615058315507));
#24846=CARTESIAN_POINT('Ctrl Pts',(5.31717369696119,-4.76142762282966,333.76793260937));
#24847=CARTESIAN_POINT('Ctrl Pts',(5.30821146906304,-4.80102641978095,333.920965476783));
#24848=CARTESIAN_POINT('Ctrl Pts',(5.29924924116492,-4.83322782295187,334.075848763131));
#24849=CARTESIAN_POINT('Ctrl Pts',(5.29028701326675,-4.85790275767711,334.231908951066));
#24850=CARTESIAN_POINT('Ctrl Pts',(5.28132449551006,-4.88257849044498,334.387974186336));
#24851=CARTESIAN_POINT('Ctrl Pts',(5.27236197775338,-4.89972725055652,334.545216245031));
#24852=CARTESIAN_POINT('Ctrl Pts',(5.26339945999669,-4.9092715151488,334.70295412299));
#24853=CARTESIAN_POINT('Ctrl Pts',(5.25777838949452,-4.9152574429451,334.801883436933));
#24854=CARTESIAN_POINT('Ctrl Pts',(5.2521573189924,-4.91825317574233,334.901007641494));
#24855=CARTESIAN_POINT('Ctrl Pts',(5.24653624849023,-4.91824999747317,335.000157655271));
#24856=CARTESIAN_POINT('',(8.74653624854529,-4.91824892942493,334.996754894379));
#24857=CARTESIAN_POINT('Ctrl Pts',(8.74653624849026,-4.91824892942558,334.996754895354));
#24858=CARTESIAN_POINT('Ctrl Pts',(8.73874364056494,-4.91834007680728,335.134896977485));
#24859=CARTESIAN_POINT('Ctrl Pts',(8.73095103263955,-4.91260676554203,335.27307124222));
#24860=CARTESIAN_POINT('Ctrl Pts',(8.72315842471423,-4.90106754548729,335.410755373758));
#24861=CARTESIAN_POINT('Ctrl Pts',(8.71536551879347,-4.88952788416372,335.548444770446));
#24862=CARTESIAN_POINT('Ctrl Pts',(8.70757261287277,-4.87218190333353,335.685643613584));
#24863=CARTESIAN_POINT('Ctrl Pts',(8.699779706952,-4.84910010958536,335.821834040253));
#24864=CARTESIAN_POINT('Ctrl Pts',(8.69198489074262,-4.82601265775683,335.95805785152));
#24865=CARTESIAN_POINT('Ctrl Pts',(8.68419007453323,-4.79718665772279,336.093272375284));
#24866=CARTESIAN_POINT('Ctrl Pts',(8.67639525832385,-4.76274382037261,336.226969585606));
#24867=CARTESIAN_POINT('Ctrl Pts',(8.66859691864463,-4.7282854139191,336.360727230719));
#24868=CARTESIAN_POINT('Ctrl Pts',(8.66079857896543,-4.68820521096132,336.492965825072));
#24869=CARTESIAN_POINT('Ctrl Pts',(8.6530002392862,-4.64267480297804,336.623192452019));
#24870=CARTESIAN_POINT('Ctrl Pts',(8.64519192752529,-4.59708617324934,336.753585605512));
#24871=CARTESIAN_POINT('Ctrl Pts',(8.63738361576436,-4.54603354725092,336.881961290696));
#24872=CARTESIAN_POINT('Ctrl Pts',(8.62957530400345,-4.48973694012501,337.007845928097));
#24873=CARTESIAN_POINT('Ctrl Pts',(8.62176139640016,-4.43339998792199,337.133820780978));
#24874=CARTESIAN_POINT('Ctrl Pts',(8.61394748879692,-4.37181173745019,337.257300685956));
#24875=CARTESIAN_POINT('Ctrl Pts',(8.60613358119363,-4.3052377803483,337.377837403432));
#24876=CARTESIAN_POINT('Ctrl Pts',(8.59830717128388,-4.23855730445237,337.498566980494));
#24877=CARTESIAN_POINT('Ctrl Pts',(8.59048076137409,-4.16687538867154,337.616343637309));
#24878=CARTESIAN_POINT('Ctrl Pts',(8.58265435146433,-4.09050086762669,337.730748196822));
#24879=CARTESIAN_POINT('Ctrl Pts',(8.57861397557166,-4.05107260138437,337.789809430465));
#24880=CARTESIAN_POINT('Ctrl Pts',(8.57457359967899,-4.01039435681843,337.847972493624));
#24881=CARTESIAN_POINT('Ctrl Pts',(8.57053322378633,-3.9685126605159,337.905183354941));
#24882=CARTESIAN_POINT('Ctrl Pts',(8.56275835230203,-3.88791995950315,338.01527387772));
#24883=CARTESIAN_POINT('Ctrl Pts',(8.55498348081771,-3.80261536607146,338.122182290313));
#24884=CARTESIAN_POINT('Ctrl Pts',(8.54720860933341,-3.71287886078536,338.225478821452));
#24885=CARTESIAN_POINT('Ctrl Pts',(8.53944330571045,-3.62325278644864,338.328648234491));
#24886=CARTESIAN_POINT('Ctrl Pts',(8.53167800208752,-3.52920590598831,338.42821431773));
#24887=CARTESIAN_POINT('Ctrl Pts',(8.52391269846456,-3.43106087603816,338.523776997402));
#24888=CARTESIAN_POINT('Ctrl Pts',(8.51615509428656,-3.33301315873585,338.619244924876));
#24889=CARTESIAN_POINT('Ctrl Pts',(8.50839749010855,-3.23087565657685,338.710717077265));
#24890=CARTESIAN_POINT('Ctrl Pts',(8.50063988593055,-3.12501037171476,338.797827436729));
#24891=CARTESIAN_POINT('Ctrl Pts',(8.49288811945772,-3.01922475195361,338.884872244436));
#24892=CARTESIAN_POINT('Ctrl Pts',(8.48513635298485,-2.90971723374499,338.967561545116));
#24893=CARTESIAN_POINT('Ctrl Pts',(8.47738458651202,-2.79688538493468,339.0455673528));
#24894=CARTESIAN_POINT('Ctrl Pts',(8.46963610183688,-2.68410130475901,339.123540135845));
#24895=CARTESIAN_POINT('Ctrl Pts',(8.46188761716177,-2.56799601404754,339.196833147722));
#24896=CARTESIAN_POINT('Ctrl Pts',(8.45413913248663,-2.44899857882953,339.265159905958));
#24897=CARTESIAN_POINT('Ctrl Pts',(8.44639225925284,-2.33002589133903,339.333472454375));
#24898=CARTESIAN_POINT('Ctrl Pts',(8.43864538601905,-2.20816259449402,339.396820608989));
#24899=CARTESIAN_POINT('Ctrl Pts',(8.43089851278526,-2.08386469503069,339.454962513344));
#24900=CARTESIAN_POINT('Ctrl Pts',(8.42315157369512,-1.959565738908,339.513104911966));
#24901=CARTESIAN_POINT('Ctrl Pts',(8.41540463460496,-1.83283249296259,339.566040806431));
#24902=CARTESIAN_POINT('Ctrl Pts',(8.40765769551481,-1.70414303495464,339.613575574207));
#24903=CARTESIAN_POINT('Ctrl Pts',(8.39990901358327,-1.57542462547148,339.661121035956));
#24904=CARTESIAN_POINT('Ctrl Pts',(8.39216033165171,-1.44474949480223,339.703262817687));
#24905=CARTESIAN_POINT('Ctrl Pts',(8.38441164972016,-1.31261266715699,339.739855593636));
#24906=CARTESIAN_POINT('Ctrl Pts',(8.37665474013633,-1.18033553489204,339.776487224274));
#24907=CARTESIAN_POINT('Ctrl Pts',(8.36889783055252,-1.04659398260185,339.807557974806));
#24908=CARTESIAN_POINT('Ctrl Pts',(8.36114092096869,-0.911895608651636,
339.832973149255));
#24909=CARTESIAN_POINT('Ctrl Pts',(8.35337986496807,-0.777125232366675,
339.858401909258));
#24910=CARTESIAN_POINT('Ctrl Pts',(8.34561880896741,-0.641397401904383,
339.878169012965));
#24911=CARTESIAN_POINT('Ctrl Pts',(8.33785775296678,-0.505225718564822,
339.892231600793));
#24912=CARTESIAN_POINT('Ctrl Pts',(8.33008427732382,-0.368836126270194,
339.906316692301));
#24913=CARTESIAN_POINT('Ctrl Pts',(8.3223108016809,-0.232001652130057,339.91467900231));
#24914=CARTESIAN_POINT('Ctrl Pts',(8.31453732603794,-0.0952376816340296,
339.917327815643));
#24915=CARTESIAN_POINT('Ctrl Pts',(8.30712328052938,0.0352025934450748,
339.919854153088));
#24916=CARTESIAN_POINT('Ctrl Pts',(8.29970923502085,0.165578450703937,339.917183551418));
#24917=CARTESIAN_POINT('Ctrl Pts',(8.29229518951229,0.295448212965507,339.909367924281));
#24918=CARTESIAN_POINT('Ctrl Pts',(8.28451997644765,0.431644446327098,339.901171566953));
#24919=CARTESIAN_POINT('Ctrl Pts',(8.27674476338299,0.56771454764716,339.887290407692));
#24920=CARTESIAN_POINT('Ctrl Pts',(8.26896955031836,0.703145564399604,339.867727331904));
#24921=CARTESIAN_POINT('Ctrl Pts',(8.26120390615335,0.838409907159359,339.848188332254));
#24922=CARTESIAN_POINT('Ctrl Pts',(8.25343826198836,0.973036347147702,339.822981384888));
#24923=CARTESIAN_POINT('Ctrl Pts',(8.24567261782335,1.10651381254502,339.79216133338));
#24924=CARTESIAN_POINT('Ctrl Pts',(8.23791467447588,1.23985891473,339.761371844643));
#24925=CARTESIAN_POINT('Ctrl Pts',(8.23015673112841,1.37205693137504,339.724980416286));
#24926=CARTESIAN_POINT('Ctrl Pts',(8.22239878778095,1.50260413832473,339.68309340778));
#24927=CARTESIAN_POINT('Ctrl Pts',(8.21464668384396,1.63305308228202,339.641237927659));
#24928=CARTESIAN_POINT('Ctrl Pts',(8.20689457990702,1.76185331913804,339.593895219883));
#24929=CARTESIAN_POINT('Ctrl Pts',(8.19914247597004,1.88851386084796,339.54122213285));
#24930=CARTESIAN_POINT('Ctrl Pts',(8.19139365757884,2.01512072048488,339.488571370058));
#24931=CARTESIAN_POINT('Ctrl Pts',(8.18364483918755,2.13958932851358,339.430594871093));
#24932=CARTESIAN_POINT('Ctrl Pts',(8.17589602079636,2.26144655336154,339.367498431458));
#24933=CARTESIAN_POINT('Ctrl Pts',(8.16814881617046,2.38327840028077,339.304415132259));
#24934=CARTESIAN_POINT('Ctrl Pts',(8.16040161154464,2.50249959889433,339.236214192899));
#24935=CARTESIAN_POINT('Ctrl Pts',(8.15265440691874,2.61865996541526,339.163148213556));
#24936=CARTESIAN_POINT('Ctrl Pts',(8.14490713906141,2.73482128001834,339.090081637859));
#24937=CARTESIAN_POINT('Ctrl Pts',(8.13715987120404,2.84792138184613,339.012150151083));
#24938=CARTESIAN_POINT('Ctrl Pts',(8.12941260334671,2.95753786279379,338.929650474615));
#24939=CARTESIAN_POINT('Ctrl Pts',(8.12166359557585,3.06717896186511,338.847132270027));
#24940=CARTESIAN_POINT('Ctrl Pts',(8.113914587805,3.17333457100083,338.76004406923));
#24941=CARTESIAN_POINT('Ctrl Pts',(8.10616558003414,3.27561456532418,338.668723522144));
#24942=CARTESIAN_POINT('Ctrl Pts',(8.09840835104594,3.37800307238731,338.577306089614));
#24943=CARTESIAN_POINT('Ctrl Pts',(8.09065112205773,3.47650745893542,338.481647601813));
#24944=CARTESIAN_POINT('Ctrl Pts',(8.08289389306952,3.5707733705158,338.382123681789));
#24945=CARTESIAN_POINT('Ctrl Pts',(8.07513252066287,3.66508963295176,338.282546602415));
#24946=CARTESIAN_POINT('Ctrl Pts',(8.06737114825622,3.75516265280226,338.179100271403));
#24947=CARTESIAN_POINT('Ctrl Pts',(8.05960977584957,3.84067841605557,338.07219341301));
#24948=CARTESIAN_POINT('Ctrl Pts',(8.05183599209126,3.9263309291198,337.965115597918));
#24949=CARTESIAN_POINT('Ctrl Pts',(8.04406220833293,4.00741139153291,337.85456651263));
#24950=CARTESIAN_POINT('Ctrl Pts',(8.03628842457462,4.08364867213382,337.740984601394));
#24951=CARTESIAN_POINT('Ctrl Pts',(8.02887800146253,4.156322485007,337.632711713145));
#24952=CARTESIAN_POINT('Ctrl Pts',(8.02146757835047,4.22459548850642,337.521683354024));
#24953=CARTESIAN_POINT('Ctrl Pts',(8.01405715523839,4.28827258877716,337.408298417315));
#24954=CARTESIAN_POINT('Ctrl Pts',(8.00628161170165,4.35508713606542,337.289326868936));
#24955=CARTESIAN_POINT('Ctrl Pts',(7.99850606816487,4.41705239200587,337.167384885051));
#24956=CARTESIAN_POINT('Ctrl Pts',(7.99073052462813,4.4738932078585,337.042905437649));
#24957=CARTESIAN_POINT('Ctrl Pts',(7.98296454595626,4.53066410258984,336.918579115118));
#24958=CARTESIAN_POINT('Ctrl Pts',(7.97519856728445,4.58232293900728,336.791721891872));
#24959=CARTESIAN_POINT('Ctrl Pts',(7.96743258861258,4.62863928146743,336.662793271744));
#24960=CARTESIAN_POINT('Ctrl Pts',(7.95967430711986,4.67490971790587,336.533992438045));
#24961=CARTESIAN_POINT('Ctrl Pts',(7.95191602562709,4.71584806681081,336.403124658593));
#24962=CARTESIAN_POINT('Ctrl Pts',(7.94415774413437,4.75127119149535,336.270671132656));
#24963=CARTESIAN_POINT('Ctrl Pts',(7.93640529880406,4.78666766915647,336.138317244802));
#24964=CARTESIAN_POINT('Ctrl Pts',(7.92865285347378,4.81655708008462,336.004380360865));
#24965=CARTESIAN_POINT('Ctrl Pts',(7.92090040814347,4.84080563832996,335.869358288862));
#24966=CARTESIAN_POINT('Ctrl Pts',(7.91315124466932,4.86504393139098,335.734393375987));
#24967=CARTESIAN_POINT('Ctrl Pts',(7.90540208119514,4.88364605231357,335.598344572619));
#24968=CARTESIAN_POINT('Ctrl Pts',(7.89765291772099,4.89652903970712,335.461721155899));
#24969=CARTESIAN_POINT('Ctrl Pts',(7.8899053658207,4.90940934785847,335.325126152405));
#24970=CARTESIAN_POINT('Ctrl Pts',(7.88215781392046,4.91657285161,335.187957162106));
#24971=CARTESIAN_POINT('Ctrl Pts',(7.87441026202018,4.91798836733782,335.050729490732));
#24972=CARTESIAN_POINT('Ctrl Pts',(7.86666264503729,4.91940389495654,334.913500666589));
#24973=CARTESIAN_POINT('Ctrl Pts',(7.85891502805435,4.91507133421292,334.776213551186));
#24974=CARTESIAN_POINT('Ctrl Pts',(7.85116741107146,4.90501163499754,334.639383967302));
#24975=CARTESIAN_POINT('Ctrl Pts',(7.84341805266317,4.89494967467197,334.502523628347));
#24976=CARTESIAN_POINT('Ctrl Pts',(7.83566869425488,4.87915804296702,334.366121415241));
#24977=CARTESIAN_POINT('Ctrl Pts',(7.82791933584659,4.85770957758364,334.230688150129));
#24978=CARTESIAN_POINT('Ctrl Pts',(7.8201617558454,4.83623835669697,334.095111198648));
#24979=CARTESIAN_POINT('Ctrl Pts',(7.81240417584421,4.80909837469085,333.960505635297));
#24980=CARTESIAN_POINT('Ctrl Pts',(7.80464659584302,4.77641375883196,333.827372750214));
#24981=CARTESIAN_POINT('Ctrl Pts',(7.79688487166486,4.74371168252373,333.69416874421));
#24982=CARTESIAN_POINT('Ctrl Pts',(7.78912314748676,4.70545917922386,333.562439359217));
#24983=CARTESIAN_POINT('Ctrl Pts',(7.7813614233086,4.66183004198195,333.43266987454));
#24984=CARTESIAN_POINT('Ctrl Pts',(7.77358729007109,4.61813115264107,333.302692920852));
#24985=CARTESIAN_POINT('Ctrl Pts',(7.76581315683357,4.56903859222243,333.174682494026));
#24986=CARTESIAN_POINT('Ctrl Pts',(7.75803902359607,4.51477435199853,333.049103894864));
#24987=CARTESIAN_POINT('Ctrl Pts',(7.75063238938553,4.46307529233841,332.929461650481));
#24988=CARTESIAN_POINT('Ctrl Pts',(7.74322575517492,4.40668244441044,332.812026836026));
#24989=CARTESIAN_POINT('Ctrl Pts',(7.73581912096438,4.34582529282009,332.697178776634));
#24990=CARTESIAN_POINT('Ctrl Pts',(7.72804547000375,4.28195252126459,332.576639716401));
#24991=CARTESIAN_POINT('Ctrl Pts',(7.72027181904308,4.21295976613436,332.458569235784));
#24992=CARTESIAN_POINT('Ctrl Pts',(7.71249816808239,4.13906200126668,332.343432889579));
#24993=CARTESIAN_POINT('Ctrl Pts',(7.70473408651929,4.06525520486368,332.228438276709));
#24994=CARTESIAN_POINT('Ctrl Pts',(7.69697000495611,3.98655562188279,332.116370937523));
#24995=CARTESIAN_POINT('Ctrl Pts',(7.68920592339302,3.90322474152287,332.007673199722));
#24996=CARTESIAN_POINT('Ctrl Pts',(7.68144954154498,3.819976501206,331.899083258522));
#24997=CARTESIAN_POINT('Ctrl Pts',(7.67369315969695,3.73210633994887,331.793856576977));
#24998=CARTESIAN_POINT('Ctrl Pts',(7.66593677784891,3.63991959477862,331.692407460698));
#24999=CARTESIAN_POINT('Ctrl Pts',(7.65818623272046,3.54780222063615,331.591034685431));
#25000=CARTESIAN_POINT('Ctrl Pts',(7.65043568759202,3.45137498993476,331.493434105567));
#25001=CARTESIAN_POINT('Ctrl Pts',(7.64268514246356,3.35098391989302,331.399987523477));
#25002=CARTESIAN_POINT('Ctrl Pts',(7.63493787337777,3.25063528369594,331.306580439899));
#25003=CARTESIAN_POINT('Ctrl Pts',(7.62719060429197,3.1463264260956,331.217324127791));
#25004=CARTESIAN_POINT('Ctrl Pts',(7.61944333520617,3.0384405196533,331.132563863355));
#25005=CARTESIAN_POINT('Ctrl Pts',(7.61169767389807,2.93057700259133,331.047821189073));
#25006=CARTESIAN_POINT('Ctrl Pts',(7.60395201259002,2.81913822052735,330.967572947991));
#25007=CARTESIAN_POINT('Ctrl Pts',(7.59620635128192,2.70454044007389,330.892124141298));
#25008=CARTESIAN_POINT('Ctrl Pts',(7.58846061933131,2.58994161445792,330.816674646493));
#25009=CARTESIAN_POINT('Ctrl Pts',(7.58071488738061,2.47218405959718,330.7460248884));
#25010=CARTESIAN_POINT('Ctrl Pts',(7.57296915543,2.35171269187729,330.680436309375));
#25011=CARTESIAN_POINT('Ctrl Pts',(7.56522167472535,2.23121412533453,330.614832922416));
#25012=CARTESIAN_POINT('Ctrl Pts',(7.55747419402075,2.10800087010399,330.554293175222));
#25013=CARTESIAN_POINT('Ctrl Pts',(7.54972671331609,1.98254171704078,330.499032170445));
#25014=CARTESIAN_POINT('Ctrl Pts',(7.54197098888234,1.85694906880536,330.443712365036));
#25015=CARTESIAN_POINT('Ctrl Pts',(7.53421526444858,1.72910610740857,330.393682680104));
#25016=CARTESIAN_POINT('Ctrl Pts',(7.52645954001483,1.59950136356103,330.349109929221));
#25017=CARTESIAN_POINT('Ctrl Pts',(7.5186996622906,1.46982721470147,330.304513309056));
#25018=CARTESIAN_POINT('Ctrl Pts',(7.5109397845664,1.33838977806884,330.265379557255));
#25019=CARTESIAN_POINT('Ctrl Pts',(7.50317990684218,1.20569099186815,330.231825056206));
#25020=CARTESIAN_POINT('Ctrl Pts',(7.49540758585675,1.07277941808026,330.198216749229));
#25021=CARTESIAN_POINT('Ctrl Pts',(7.48763526487133,0.938602835910154,330.170205650762));
#25022=CARTESIAN_POINT('Ctrl Pts',(7.47986294388591,0.803672461776946,330.147856799652));
#25023=CARTESIAN_POINT('Ctrl Pts',(7.47243565815412,0.674732027579236,330.126500077087));
#25024=CARTESIAN_POINT('Ctrl Pts',(7.4650083724223,0.545103583458626,330.110313680698));
#25025=CARTESIAN_POINT('Ctrl Pts',(7.45758108669051,0.415234142492321,330.099309878251));
#25026=CARTESIAN_POINT('Ctrl Pts',(7.4498047450077,0.279261300787976,330.087788936317));
#25027=CARTESIAN_POINT('Ctrl Pts',(7.44202840332493,0.142593965360228,330.081913076826));
#25028=CARTESIAN_POINT('Ctrl Pts',(7.43425206164218,0.00574026669514989,
330.081753349837));
#25029=CARTESIAN_POINT('Ctrl Pts',(7.42648529447328,-0.130944932733913,
330.08159381951));
#25030=CARTESIAN_POINT('Ctrl Pts',(7.41871852730447,-0.267815651832061,
330.087136418631));
#25031=CARTESIAN_POINT('Ctrl Pts',(7.41095176013556,-0.404358136988321,
330.098400510083));
#25032=CARTESIAN_POINT('Ctrl Pts',(7.40319270047437,-0.540765121461374,
330.109653423388));
#25033=CARTESIAN_POINT('Ctrl Pts',(7.39543364081317,-0.676844133303198,
330.126616497821));
#25034=CARTESIAN_POINT('Ctrl Pts',(7.38767458115197,-0.812081267898217,
330.149257059292));
#25035=CARTESIAN_POINT('Ctrl Pts',(7.37992136866472,-0.947216488719585,
330.171880558992));
#25036=CARTESIAN_POINT('Ctrl Pts',(7.37216815617745,-1.08151071128066,330.200172965249));
#25037=CARTESIAN_POINT('Ctrl Pts',(7.36441494369021,-1.21445535861207,330.234049806761));
#25038=CARTESIAN_POINT('Ctrl Pts',(7.3566650323184,-1.34734340158386,330.267912224398));
#25039=CARTESIAN_POINT('Ctrl Pts',(7.34891512094654,-1.4788826343657,330.307354251804));
#25040=CARTESIAN_POINT('Ctrl Pts',(7.34116520957474,-1.60857509649862,330.352240408388));
#25041=CARTESIAN_POINT('Ctrl Pts',(7.33341692158451,-1.73824039182361,330.397117162623));
#25042=CARTESIAN_POINT('Ctrl Pts',(7.32566863359428,-1.8660593169516,330.447435649982));
#25043=CARTESIAN_POINT('Ctrl Pts',(7.31792034560405,-1.9915498719978,330.503010766096));
#25044=CARTESIAN_POINT('Ctrl Pts',(7.31017200497487,-2.11704127957955,330.558586259767));
#25045=CARTESIAN_POINT('Ctrl Pts',(7.3024236643457,-2.24020392824123,330.619418295232));
#25046=CARTESIAN_POINT('Ctrl Pts',(7.29467532371652,-2.36057694154306,330.68527410308));
#25047=CARTESIAN_POINT('Ctrl Pts',(7.28692525475024,-2.48097680512852,330.751144600658));
#25048=CARTESIAN_POINT('Ctrl Pts',(7.27917518578401,-2.59858545240846,330.822040912983));
#25049=CARTESIAN_POINT('Ctrl Pts',(7.27142511681774,-2.71296804983267,330.897685114099));
#25050=CARTESIAN_POINT('Ctrl Pts',(7.26366685078835,-2.82747162700243,330.973409322282));
#25051=CARTESIAN_POINT('Ctrl Pts',(7.25590858475895,-2.93874201184566,331.053891234774));
#25052=CARTESIAN_POINT('Ctrl Pts',(7.24815031872956,-3.04637429115085,331.138810191053));
#25053=CARTESIAN_POINT('Ctrl Pts',(7.24038792079743,-3.15406389333046,331.22377437353));
#25054=CARTESIAN_POINT('Ctrl Pts',(7.23262552286524,-3.25811123289397,331.31318005398));
#25055=CARTESIAN_POINT('Ctrl Pts',(7.22486312493311,-3.35814653861724,331.406667996459));
#25056=CARTESIAN_POINT('Ctrl Pts',(7.21708834555284,-3.45834140611,331.500305057306));
#25057=CARTESIAN_POINT('Ctrl Pts',(7.20931356617262,-3.55451117760251,331.598037113311));
#25058=CARTESIAN_POINT('Ctrl Pts',(7.20153878679236,-3.64632422870232,331.699469333323));
#25059=CARTESIAN_POINT('Ctrl Pts',(7.19414020866709,-3.73369468621071,331.795993513298));
#25060=CARTESIAN_POINT('Ctrl Pts',(7.18674163054182,-3.81711998063126,331.895867948561));
#25061=CARTESIAN_POINT('Ctrl Pts',(7.17934305241656,-3.89635070610417,331.998727896784));
#25062=CARTESIAN_POINT('Ctrl Pts',(7.17155910472168,-3.97970832056288,332.106945508779));
#25063=CARTESIAN_POINT('Ctrl Pts',(7.16377515702676,-4.05868905964504,332.218813772232));
#25064=CARTESIAN_POINT('Ctrl Pts',(7.15599120933189,-4.13295648073021,332.333944150831));
#25065=CARTESIAN_POINT('Ctrl Pts',(7.14821668385917,-4.20713400345435,332.448935167753));
#25066=CARTESIAN_POINT('Ctrl Pts',(7.14044215838654,-4.27660934838268,332.56718012173));
#25067=CARTESIAN_POINT('Ctrl Pts',(7.13266763291381,-4.34108626003702,332.688257552101));
#25068=CARTESIAN_POINT('Ctrl Pts',(7.12490085180615,-4.40549894491065,332.809214374748));
#25069=CARTESIAN_POINT('Ctrl Pts',(7.11713407069846,-4.46492292106192,332.932997719246));
#25070=CARTESIAN_POINT('Ctrl Pts',(7.10936728959081,-4.51910542188317,333.059157593104));
#25071=CARTESIAN_POINT('Ctrl Pts',(7.10160658069208,-4.57324556185245,333.185218832907));
#25072=CARTESIAN_POINT('Ctrl Pts',(7.09384587179335,-4.62215222859229,333.313652548546));
#25073=CARTESIAN_POINT('Ctrl Pts',(7.08608516289462,-4.66561895164036,333.443984942041));
#25074=CARTESIAN_POINT('Ctrl Pts',(7.07832857773713,-4.7090625781491,333.574248081932));
#25075=CARTESIAN_POINT('Ctrl Pts',(7.0705719925796,-4.74707189055904,333.706407523644));
#25076=CARTESIAN_POINT('Ctrl Pts',(7.06281540742211,-4.77948897741175,333.839970613605));
#25077=CARTESIAN_POINT('Ctrl Pts',(7.05506139088635,-4.81189532922681,333.973489473657));
#25078=CARTESIAN_POINT('Ctrl Pts',(7.0473073743506,-4.83871305151345,334.108410678542));
#25079=CARTESIAN_POINT('Ctrl Pts',(7.03955335781484,-4.85983453256771,334.2442279586));
#25080=CARTESIAN_POINT('Ctrl Pts',(7.03179833874714,-4.8809587444595,334.380062798738));
#25081=CARTESIAN_POINT('Ctrl Pts',(7.02404331967943,-4.89638517703035,334.516793561927));
#25082=CARTESIAN_POINT('Ctrl Pts',(7.01628830061173,-4.90605763941331,334.653905357952));
#25083=CARTESIAN_POINT('Ctrl Pts',(7.00970428323788,-4.91426956769117,334.770313382137));
#25084=CARTESIAN_POINT('Ctrl Pts',(7.00312026586403,-4.91833488291597,334.886995785808));
#25085=CARTESIAN_POINT('Ctrl Pts',(6.99653624849017,-4.9182486560913,335.003635843242));
#25086=CARTESIAN_POINT('',(10.4965362484546,-4.91824948156304,334.997741769529));
#25087=CARTESIAN_POINT('Ctrl Pts',(10.4965362484546,-4.91824948156304,334.997741769529));
#25088=CARTESIAN_POINT('Ctrl Pts',(10.4888471502769,-4.91831149438634,335.132800852283));
#25089=CARTESIAN_POINT('Ctrl Pts',(10.4811580520993,-4.91280606153683,335.268086508271));
#25090=CARTESIAN_POINT('Ctrl Pts',(10.4734689539216,-4.90170348255283,335.403095561411));
#25091=CARTESIAN_POINT('Ctrl Pts',(10.4657887887527,-4.89061380227713,335.537947764292));
#25092=CARTESIAN_POINT('Ctrl Pts',(10.4581086235838,-4.87393994179174,335.672523608465));
#25093=CARTESIAN_POINT('Ctrl Pts',(10.4504284584148,-4.85170419160826,335.806318485234));
#25094=CARTESIAN_POINT('Ctrl Pts',(10.442755282694,-4.82948867739849,335.939991599995));
#25095=CARTESIAN_POINT('Ctrl Pts',(10.435082106973,-4.80172140816308,336.072884768922));
#25096=CARTESIAN_POINT('Ctrl Pts',(10.4274089312521,-4.76847655892465,336.204497558937));
#25097=CARTESIAN_POINT('Ctrl Pts',(10.4195986186762,-4.73463754968828,336.338462564614));
#25098=CARTESIAN_POINT('Ctrl Pts',(10.4117883061003,-4.69512331937017,336.47110056669));
#25099=CARTESIAN_POINT('Ctrl Pts',(10.4039779935244,-4.65006680406456,336.601893186276));
#25100=CARTESIAN_POINT('Ctrl Pts',(10.3963121106908,-4.60584348215994,336.730267164588));
#25101=CARTESIAN_POINT('Ctrl Pts',(10.3886462278573,-4.55628122659596,336.856863030108));
#25102=CARTESIAN_POINT('Ctrl Pts',(10.3809803450237,-4.50155618192456,336.981205442017));
#25103=CARTESIAN_POINT('Ctrl Pts',(10.3733151953191,-4.44683637089871,337.105535962403));
#25104=CARTESIAN_POINT('Ctrl Pts',(10.3656500456145,-4.3869549137158,337.227613091595));
#25105=CARTESIAN_POINT('Ctrl Pts',(10.3579848959099,-4.32213588798339,337.346981982953));
#25106=CARTESIAN_POINT('Ctrl Pts',(10.3503187339676,-4.25730830243618,337.466366637825));
#25107=CARTESIAN_POINT('Ctrl Pts',(10.3426525720253,-4.18754204271593,337.583041992139));
#25108=CARTESIAN_POINT('Ctrl Pts',(10.3349864100829,-4.11310661810113,337.696578760324));
#25109=CARTESIAN_POINT('Ctrl Pts',(10.3270676616952,-4.03621867820436,337.813856363743));
#25110=CARTESIAN_POINT('Ctrl Pts',(10.3191489133075,-3.95434884352145,337.927784611801));
#25111=CARTESIAN_POINT('Ctrl Pts',(10.3112301649197,-3.867841204291,338.03792486426));
#25112=CARTESIAN_POINT('Ctrl Pts',(10.3035526386729,-3.78396877417725,338.144710007275));
#25113=CARTESIAN_POINT('Ctrl Pts',(10.2958751124261,-3.69573728881549,338.24793430924));
#25114=CARTESIAN_POINT('Ctrl Pts',(10.2881975861793,-3.60349921123578,338.347234156303));
#25115=CARTESIAN_POINT('Ctrl Pts',(10.2801582267211,-3.50691405638744,338.45121389392));
#25116=CARTESIAN_POINT('Ctrl Pts',(10.2721188672629,-3.40593582994268,338.550889908336));
#25117=CARTESIAN_POINT('Ctrl Pts',(10.2640795078046,-3.30100881357484,338.645891369089));
#25118=CARTESIAN_POINT('Ctrl Pts',(10.2560401483464,-3.19608179720701,338.740892829843));
#25119=CARTESIAN_POINT('Ctrl Pts',(10.2480007888882,-3.08720642071983,338.831219479815));
#25120=CARTESIAN_POINT('Ctrl Pts',(10.23996142943,-2.97486136344552,338.916552429214));
#25121=CARTESIAN_POINT('Ctrl Pts',(10.2321863547283,-2.86620952156538,338.999080155401));
#25122=CARTESIAN_POINT('Ctrl Pts',(10.2244112800266,-2.7539491960901,339.077213585137));
#25123=CARTESIAN_POINT('Ctrl Pts',(10.2166362053249,-2.63847135919566,339.150620670358));
#25124=CARTESIAN_POINT('Ctrl Pts',(10.2088706983503,-2.52313562517027,339.223937423462));
#25125=CARTESIAN_POINT('Ctrl Pts',(10.2011051913756,-2.40459058441866,339.292539196675));
#25126=CARTESIAN_POINT('Ctrl Pts',(10.193339684401,-2.28325963898628,339.356134580506));
#25127=CARTESIAN_POINT('Ctrl Pts',(10.1855818769466,-2.16204899350117,339.419666909348));
#25128=CARTESIAN_POINT('Ctrl Pts',(10.1778240694924,-2.0380582843033,339.478202546856));
#25129=CARTESIAN_POINT('Ctrl Pts',(10.170066262038,-1.91173890797882,339.531493949044));
#25130=CARTESIAN_POINT('Ctrl Pts',(10.1623142925723,-1.78551459086761,339.584745247814));
#25131=CARTESIAN_POINT('Ctrl Pts',(10.1545623231064,-1.65696545337093,339.632760015154));
#25132=CARTESIAN_POINT('Ctrl Pts',(10.1468103536407,-1.52656612983506,339.675337304809));
#25133=CARTESIAN_POINT('Ctrl Pts',(10.1390616671101,-1.39622203001107,339.717896563114));
#25134=CARTESIAN_POINT('Ctrl Pts',(10.1313129805795,-1.26402967336585,339.75502280268));
#25135=CARTESIAN_POINT('Ctrl Pts',(10.1235642940489,-1.1304820432802,339.786563841872));
#25136=CARTESIAN_POINT('Ctrl Pts',(10.1158172196792,-0.996962198582865,
339.818098318762));
#25137=CARTESIAN_POINT('Ctrl Pts',(10.1080701453095,-0.862088021479138,
339.844049816859));
#25138=CARTESIAN_POINT('Ctrl Pts',(10.1003230709398,-0.726365585908918,
339.864316611623));
#25139=CARTESIAN_POINT('Ctrl Pts',(10.0925759316195,-0.590642012457482,
339.884583576301));
#25140=CARTESIAN_POINT('Ctrl Pts',(10.0848287922992,-0.454070552943152,
339.899165684858));
#25141=CARTESIAN_POINT('Ctrl Pts',(10.077081652979,-0.317164960868917,339.908012780148));
#25142=CARTESIAN_POINT('Ctrl Pts',(10.0693327719101,-0.180228589030351,
339.916861864485));
#25143=CARTESIAN_POINT('Ctrl Pts',(10.0615838908412,-0.0429583251338626,
339.919973344645));
#25144=CARTESIAN_POINT('Ctrl Pts',(10.0538350097723,0.0941298975525665,
339.917349146124));
#25145=CARTESIAN_POINT('Ctrl Pts',(10.0460779038931,0.231363628296001,339.914722162228));
#25146=CARTESIAN_POINT('Ctrl Pts',(10.038320798014,0.368414540429873,339.906347345875));
#25147=CARTESIAN_POINT('Ctrl Pts',(10.0305636921348,0.504769091797421,339.892278735565));
#25148=CARTESIAN_POINT('Ctrl Pts',(10.0228024410756,0.64119650721525,339.878202607385));
#25149=CARTESIAN_POINT('Ctrl Pts',(10.0150411900165,0.776926433798234,339.858426678913));
#25150=CARTESIAN_POINT('Ctrl Pts',(10.0072799389574,0.911454362244702,339.833056383702));
#25151=CARTESIAN_POINT('Ctrl Pts',(9.99950627233217,1.0461974931591,339.807645503981));
#25152=CARTESIAN_POINT('Ctrl Pts',(9.99173260570696,1.17973440263807,339.776622462804));
#25153=CARTESIAN_POINT('Ctrl Pts',(9.98395893908176,1.31157374575264,339.740143180533));
#25154=CARTESIAN_POINT('Ctrl Pts',(9.97654709110647,1.43727673964733,339.705361795187));
#25155=CARTESIAN_POINT('Ctrl Pts',(9.96913524313119,1.56143636007777,339.665620737365));
#25156=CARTESIAN_POINT('Ctrl Pts',(9.9617233951559,1.68364446007505,339.621095583794));
#25157=CARTESIAN_POINT('Ctrl Pts',(9.95394831592372,1.81184159302493,339.574388393091));
#25158=CARTESIAN_POINT('Ctrl Pts',(9.94617323669155,1.93829622334815,339.52226874059));
#25159=CARTESIAN_POINT('Ctrl Pts',(9.93839815745937,2.06251754688526,339.464885713128));
#25160=CARTESIAN_POINT('Ctrl Pts',(9.93063264598798,2.18658600768336,339.407573299361));
#25161=CARTESIAN_POINT('Ctrl Pts',(9.92286713451661,2.30842627844374,339.345010560234));
#25162=CARTESIAN_POINT('Ctrl Pts',(9.91510162304522,2.42756417920079,339.277395845414));
#25163=CARTESIAN_POINT('Ctrl Pts',(9.90734381113198,2.54658395390795,339.209848171049));
#25164=CARTESIAN_POINT('Ctrl Pts',(9.89958599921864,2.66290635305307,339.137258681006));
#25165=CARTESIAN_POINT('Ctrl Pts',(9.89182818730541,2.77607893466425,339.059873004296));
#25166=CARTESIAN_POINT('Ctrl Pts',(9.88407621342275,2.88916634986523,338.982545563073));
#25167=CARTESIAN_POINT('Ctrl Pts',(9.87632423954012,2.99910834424228,338.90042933906));
#25168=CARTESIAN_POINT('Ctrl Pts',(9.86857226565746,3.10547908556348,338.813814719101));
#25169=CARTESIAN_POINT('Ctrl Pts',(9.86082357478872,3.21180477814875,338.727236781025));
#25170=CARTESIAN_POINT('Ctrl Pts',(9.85307488392002,3.31456192336565,338.636164482408));
#25171=CARTESIAN_POINT('Ctrl Pts',(9.84532619305128,3.41335576647654,338.540930029521));
#25172=CARTESIAN_POINT('Ctrl Pts',(9.83757911439184,3.5121290543278,338.445715391318));
#25173=CARTESIAN_POINT('Ctrl Pts',(9.82983203573236,3.60694039905087,338.346340592457));
#25174=CARTESIAN_POINT('Ctrl Pts',(9.82208495707292,3.6974303922948,338.243176152576));
#25175=CARTESIAN_POINT('Ctrl Pts',(9.81433781351512,3.78792114358594,338.140010848471));
#25176=CARTESIAN_POINT('Ctrl Pts',(9.80659066995731,3.87409021344412,338.033056133875));
#25177=CARTESIAN_POINT('Ctrl Pts',(9.79884352639951,3.95561740177701,337.922716892424));
#25178=CARTESIAN_POINT('Ctrl Pts',(9.79109464114915,4.03716291883921,337.812352844792));
#25179=CARTESIAN_POINT('Ctrl Pts',(9.78334575589884,4.11406424554177,337.698603070507));
#25180=CARTESIAN_POINT('Ctrl Pts',(9.77559687064849,4.18604379958458,337.581902471136));
#25181=CARTESIAN_POINT('Ctrl Pts',(9.76783976069935,4.25809975302312,337.465078005268));
#25182=CARTESIAN_POINT('Ctrl Pts',(9.76008265075019,4.32522329287327,337.345296791023));
#25183=CARTESIAN_POINT('Ctrl Pts',(9.75232554080105,4.38718195373206,337.223019920592));
#25184=CARTESIAN_POINT('Ctrl Pts',(9.74456428572623,4.44917372311168,337.100677709718));
#25185=CARTESIAN_POINT('Ctrl Pts',(9.73680303065142,4.50599495225126,336.975837540934));
#25186=CARTESIAN_POINT('Ctrl Pts',(9.7290417755766,4.5574612831223,336.848980723356));
#25187=CARTESIAN_POINT('Ctrl Pts',(9.72126810506841,4.6090099430491,336.721920976953));
#25188=CARTESIAN_POINT('Ctrl Pts',(9.71349443456021,4.6551864554554,336.592838503541));
#25189=CARTESIAN_POINT('Ctrl Pts',(9.70572076405202,4.69585604173562,336.462230863371));
#25190=CARTESIAN_POINT('Ctrl Pts',(9.69830896299535,4.73463243214838,336.337703094359));
#25191=CARTESIAN_POINT('Ctrl Pts',(9.6908971619387,4.76840298317807,336.211789235325));
#25192=CARTESIAN_POINT('Ctrl Pts',(9.68348536088203,4.79709447026861,336.084927511781));
#25193=CARTESIAN_POINT('Ctrl Pts',(9.67571026849582,4.8271922779568,335.951847628322));
#25194=CARTESIAN_POINT('Ctrl Pts',(9.66793517610962,4.85179564187078,335.817304059386));
#25195=CARTESIAN_POINT('Ctrl Pts',(9.66016008372341,4.87076433084771,335.681790213953));
#25196=CARTESIAN_POINT('Ctrl Pts',(9.65239455901105,4.8897096778217,335.546443125672));
#25197=CARTESIAN_POINT('Ctrl Pts',(9.64462903429864,4.90303409241489,335.410128519967));
#25198=CARTESIAN_POINT('Ctrl Pts',(9.63686350958628,4.91064776597322,335.273352484975));
#25199=CARTESIAN_POINT('Ctrl Pts',(9.62910568435987,4.91825389060538,335.136712062863));
#25200=CARTESIAN_POINT('Ctrl Pts',(9.62134785913349,4.92016052067019,334.999611509679));
#25201=CARTESIAN_POINT('Ctrl Pts',(9.61359003390709,4.91632936941955,334.862564219059));
#25202=CARTESIAN_POINT('Ctrl Pts',(9.60583804665353,4.91250110121362,334.725620060224));
#25203=CARTESIAN_POINT('Ctrl Pts',(9.59808605939994,4.90294365701153,334.588729473318));
#25204=CARTESIAN_POINT('Ctrl Pts',(9.59033407214639,4.88767078794349,334.452407696197));
#25205=CARTESIAN_POINT('Ctrl Pts',(9.58258536786679,4.87240438694997,334.316143651478));
#25206=CARTESIAN_POINT('Ctrl Pts',(9.57483666358718,4.8514274186996,334.180448325063));
#25207=CARTESIAN_POINT('Ctrl Pts',(9.56708795930757,4.82480561898035,334.045833451878));
#25208=CARTESIAN_POINT('Ctrl Pts',(9.55934086721488,4.79818935816356,333.911246586516));
#25209=CARTESIAN_POINT('Ctrl Pts',(9.55159377512222,4.76593067774082,333.777740110451));
#25210=CARTESIAN_POINT('Ctrl Pts',(9.54384668302953,4.72814665997359,333.645816768572));
#25211=CARTESIAN_POINT('Ctrl Pts',(9.53609952602892,4.69036232563831,333.513892321392));
#25212=CARTESIAN_POINT('Ctrl Pts',(9.52835236902829,4.64705266924542,333.383551410618));
#25213=CARTESIAN_POINT('Ctrl Pts',(9.52060521202768,4.59838488829934,333.255282406359));
#25214=CARTESIAN_POINT('Ctrl Pts',(9.5128563133378,4.54970616602966,333.126984565102));
#25215=CARTESIAN_POINT('Ctrl Pts',(9.50510741464794,4.49566706082928,333.000759922629));
#25216=CARTESIAN_POINT('Ctrl Pts',(9.49735851595807,4.43648307584502,332.877077255235));
#25217=CARTESIAN_POINT('Ctrl Pts',(9.48960139265084,4.37723627346574,332.753263312075));
#25218=CARTESIAN_POINT('Ctrl Pts',(9.48184426934362,4.31283385195929,332.631997086707));
#25219=CARTESIAN_POINT('Ctrl Pts',(9.4740871460364,4.24353775405405,332.513723588895));
#25220=CARTESIAN_POINT('Ctrl Pts',(9.46632587762673,4.17420462703208,332.395386890364));
#25221=CARTESIAN_POINT('Ctrl Pts',(9.45856460921701,4.09997282444036,332.28004643445));
#25222=CARTESIAN_POINT('Ctrl Pts',(9.45080334080734,4.02114732351632,332.168117716946));
#25223=CARTESIAN_POINT('Ctrl Pts',(9.44302965713918,3.94219572993343,332.056009953455));
#25224=CARTESIAN_POINT('Ctrl Pts',(9.43525597347108,3.85863599234976,331.94732514424));
#25225=CARTESIAN_POINT('Ctrl Pts',(9.42748228980292,3.77081358420248,331.842445887131));
#25226=CARTESIAN_POINT('Ctrl Pts',(9.42007063540466,3.68708116526223,331.742450976041));
#25227=CARTESIAN_POINT('Ctrl Pts',(9.41265898100637,3.59947436273894,331.645915354763));
#25228=CARTESIAN_POINT('Ctrl Pts',(9.40524732660811,3.50832204309355,331.553137730567));
#25229=CARTESIAN_POINT('Ctrl Pts',(9.39747227725628,3.41270050629583,331.455811200198));
#25230=CARTESIAN_POINT('Ctrl Pts',(9.38969722790442,3.31287480120373,331.362312928328));
#25231=CARTESIAN_POINT('Ctrl Pts',(9.3819221785526,3.2091839533473,331.273027848765));
#25232=CARTESIAN_POINT('Ctrl Pts',(9.37415669693203,3.10562070418771,331.183852640614));
#25233=CARTESIAN_POINT('Ctrl Pts',(9.36639121531147,2.99820206935068,331.098880561473));
#25234=CARTESIAN_POINT('Ctrl Pts',(9.3586257336909,2.88730502329413,331.01846100547));
#25235=CARTESIAN_POINT('Ctrl Pts',(9.35086795156883,2.77651793199397,330.9381211857));
#25236=CARTESIAN_POINT('Ctrl Pts',(9.34311016944679,2.6622596072842,330.862325134263));
#25237=CARTESIAN_POINT('Ctrl Pts',(9.33535238732472,2.54494104864929,330.791382873033));
#25238=CARTESIAN_POINT('Ctrl Pts',(9.32760044314372,2.42771077540587,330.720493997775));
#25239=CARTESIAN_POINT('Ctrl Pts',(9.31984849896273,2.30742518519683,330.654451843832));
#25240=CARTESIAN_POINT('Ctrl Pts',(9.31209655478173,2.18452498922378,330.593523671463));
#25241=CARTESIAN_POINT('Ctrl Pts',(9.30434789337568,2.06167683873446,330.532621300812));
#25242=CARTESIAN_POINT('Ctrl Pts',(9.29659923196962,1.93621663415238,330.476828777653));
#25243=CARTESIAN_POINT('Ctrl Pts',(9.28885057056357,1.80861027304298,330.426367751694));
#25244=CARTESIAN_POINT('Ctrl Pts',(9.28110352121754,1.68103045963037,330.375917223833));
#25245=CARTESIAN_POINT('Ctrl Pts',(9.27335647187147,1.55130574105981,330.330796130575));
#25246=CARTESIAN_POINT('Ctrl Pts',(9.26560942252544,1.41992224160266,330.291178078298));
#25247=CARTESIAN_POINT('Ctrl Pts',(9.25786230810484,1.28853763853482,330.251559693232));
#25248=CARTESIAN_POINT('Ctrl Pts',(9.25011519368424,1.15549460102207,330.217444554194));
#25249=CARTESIAN_POINT('Ctrl Pts',(9.24236807926363,1.02129428555199,330.188956345573));
#25250=CARTESIAN_POINT('Ctrl Pts',(9.23461922294723,0.887063795883884,330.160461731537));
#25251=CARTESIAN_POINT('Ctrl Pts',(9.22687036663084,0.75167589275711,330.137596646645));
#25252=CARTESIAN_POINT('Ctrl Pts',(9.21912151031444,0.615641396738061,330.120433550701));
#25253=CARTESIAN_POINT('Ctrl Pts',(9.21136442881664,0.479462504131856,330.103252236639));
#25254=CARTESIAN_POINT('Ctrl Pts',(9.20360734731886,0.342636036022161,330.091785050952));
#25255=CARTESIAN_POINT('Ctrl Pts',(9.19585026582106,0.205677958286601,330.086052539966));
#25256=CARTESIAN_POINT('Ctrl Pts',(9.18808903897985,0.0686466908771019,
330.080316965556));
#25257=CARTESIAN_POINT('Ctrl Pts',(9.18032781213862,-0.0685159356209527,
330.080322172283));
#25258=CARTESIAN_POINT('Ctrl Pts',(9.1725665852974,-0.205295485973605,330.086036546133));
#25259=CARTESIAN_POINT('Ctrl Pts',(9.16479294236726,-0.342293850580163,
330.091760061602));
#25260=CARTESIAN_POINT('Ctrl Pts',(9.15701929943711,-0.478907524710492,
330.103210962543));
#25261=CARTESIAN_POINT('Ctrl Pts',(9.14924565650696,-0.6146278230349,330.120305777853));
#25262=CARTESIAN_POINT('Ctrl Pts',(9.14183353511603,-0.744036304416612,
330.136605580581));
#25263=CARTESIAN_POINT('Ctrl Pts',(9.13442141372511,-0.872632352247695,
330.158036102549));
#25264=CARTESIAN_POINT('Ctrl Pts',(9.12700929233418,-0.999986725793719,
330.184482415073));
#25265=CARTESIAN_POINT('Ctrl Pts',(9.11923420193379,-1.13357759876798,330.212223794334));
#25266=CARTESIAN_POINT('Ctrl Pts',(9.1114591115334,-1.26622430565804,330.245572289037));
#25267=CARTESIAN_POINT('Ctrl Pts',(9.10368402113301,-1.39741967742271,330.284451112792));
#25268=CARTESIAN_POINT('Ctrl Pts',(9.09591849865652,-1.5284536018898,330.323282092777));
#25269=CARTESIAN_POINT('Ctrl Pts',(9.08815297618008,-1.65803937366631,330.367629750723));
#25270=CARTESIAN_POINT('Ctrl Pts',(9.08038745370359,-1.78567917362964,330.417366155652));
#25271=CARTESIAN_POINT('Ctrl Pts',(9.07262963095745,-1.91319241520053,330.467053245559));
#25272=CARTESIAN_POINT('Ctrl Pts',(9.06487180821126,-2.03876316288809,330.522118308392));
#25273=CARTESIAN_POINT('Ctrl Pts',(9.05711398546512,-2.16190829377092,330.582383494256));
#25274=CARTESIAN_POINT('Ctrl Pts',(9.04936200093086,-2.28496075079552,330.642603327069));
#25275=CARTESIAN_POINT('Ctrl Pts',(9.04161001639658,-2.40559087474751,330.708015322369));
#25276=CARTESIAN_POINT('Ctrl Pts',(9.03385803186231,-2.52333542321499,330.77839350431));
#25277=CARTESIAN_POINT('Ctrl Pts',(9.0261093306521,-2.64103010141928,330.848741877836));
#25278=CARTESIAN_POINT('Ctrl Pts',(9.01836062944187,-2.75584130014947,330.924052054346));
#25279=CARTESIAN_POINT('Ctrl Pts',(9.01061192823167,-2.86733050215,331.004052195794));
#25280=CARTESIAN_POINT('Ctrl Pts',(9.00286483942059,-2.97879650476691,331.084035690303));
#25281=CARTESIAN_POINT('Ctrl Pts',(8.99511775060953,-3.08694156824916,331.168706980846));
#25282=CARTESIAN_POINT('Ctrl Pts',(8.98737066179845,-3.19135663013834,331.257751221288));
#25283=CARTESIAN_POINT('Ctrl Pts',(8.97962350828745,-3.29577256405141,331.346796205384));
#25284=CARTESIAN_POINT('Ctrl Pts',(8.97187635477651,-3.396458136826,331.440213958594));
#25285=CARTESIAN_POINT('Ctrl Pts',(8.96412920126551,-3.49303813159524,331.537649978162));
#25286=CARTESIAN_POINT('Ctrl Pts',(8.95638030626916,-3.58963983661529,331.635107900407));
#25287=CARTESIAN_POINT('Ctrl Pts',(8.9486314112728,-3.68213385206024,331.736585608859));
#25288=CARTESIAN_POINT('Ctrl Pts',(8.94088251627645,-3.77018280701602,331.84169275336));
#25289=CARTESIAN_POINT('Ctrl Pts',(8.93312539696105,-3.85832521306356,331.946911453726));
#25290=CARTESIAN_POINT('Ctrl Pts',(8.92536827764563,-3.94201288301005,332.055766984999));
#25291=CARTESIAN_POINT('Ctrl Pts',(8.91761115833023,-4.02094931658228,332.167836576753));
#25292=CARTESIAN_POINT('Ctrl Pts',(8.90984989408107,-4.09992792899377,332.279966051696));
#25293=CARTESIAN_POINT('Ctrl Pts',(8.90208862983192,-4.17415003489472,332.395312680657));
#25294=CARTESIAN_POINT('Ctrl Pts',(8.89432736558277,-4.24336382492132,332.51342675317));
#25295=CARTESIAN_POINT('Ctrl Pts',(8.8865536863183,-4.31268833019164,332.63172976243));
#25296=CARTESIAN_POINT('Ctrl Pts',(8.87878000705385,-4.37698832708292,332.752808715978));
#25297=CARTESIAN_POINT('Ctrl Pts',(8.87100632778939,-4.43605872546199,332.876190675519));
#25298=CARTESIAN_POINT('Ctrl Pts',(8.86359463787971,-4.49237845010362,332.99382722746));
#25299=CARTESIAN_POINT('Ctrl Pts',(8.85618294796999,-4.5439445387058,333.113556867035));
#25300=CARTESIAN_POINT('Ctrl Pts',(8.84877125806031,-4.59062137118073,333.234956519244));
#25301=CARTESIAN_POINT('Ctrl Pts',(8.83991442260744,-4.64639934216028,333.380026908961));
#25302=CARTESIAN_POINT('Ctrl Pts',(8.83105758715456,-4.69534296381877,333.527863253388));
#25303=CARTESIAN_POINT('Ctrl Pts',(8.8222007517017,-4.73720468645838,333.67785219393));
#25304=CARTESIAN_POINT('Ctrl Pts',(8.81337370149808,-4.77892562948784,333.827336726548));
#25305=CARTESIAN_POINT('Ctrl Pts',(8.80454665129447,-4.81361211826951,333.978959243898));
#25306=CARTESIAN_POINT('Ctrl Pts',(8.79571960109084,-4.84106555254952,334.132090224494));
#25307=CARTESIAN_POINT('Ctrl Pts',(8.7869498317336,-4.86834083490837,334.284227501421));
#25308=CARTESIAN_POINT('Ctrl Pts',(8.77818006237633,-4.88847654611716,334.437853555313));
#25309=CARTESIAN_POINT('Ctrl Pts',(8.76941029301909,-4.90132527004678,334.592331434005));
#25310=CARTESIAN_POINT('Ctrl Pts',(8.76178561152781,-4.91249630813708,334.726638799967));
#25311=CARTESIAN_POINT('Ctrl Pts',(8.75416093003657,-4.91815974619261,334.861589698482));
#25312=CARTESIAN_POINT('Ctrl Pts',(8.74653624854528,-4.91824892942493,334.996754894379));
#25313=CARTESIAN_POINT('',(12.2465362485257,-4.91824798382928,335.004453320022));
#25314=CARTESIAN_POINT('Ctrl Pts',(12.2465362484902,-4.91824798382871,335.004453320647));
#25315=CARTESIAN_POINT('Ctrl Pts',(12.2356922904606,-4.9180747842582,335.195734952039));
#25316=CARTESIAN_POINT('Ctrl Pts',(12.2248483324311,-4.90673912433975,335.38653135153));
#25317=CARTESIAN_POINT('Ctrl Pts',(12.2140043744016,-4.8844305574504,335.575778769967));
#25318=CARTESIAN_POINT('Ctrl Pts',(12.2052121393835,-4.86634286636259,335.729219771392));
#25319=CARTESIAN_POINT('Ctrl Pts',(12.1964199043656,-4.84104259945817,335.881643403505));
#25320=CARTESIAN_POINT('Ctrl Pts',(12.1876276693475,-4.80865222242309,336.032495455818));
#25321=CARTESIAN_POINT('Ctrl Pts',(12.1798525905152,-4.78000902369811,336.165895734173));
#25322=CARTESIAN_POINT('Ctrl Pts',(12.1720775116828,-4.7457652275205,336.298313990164));
#25323=CARTESIAN_POINT('Ctrl Pts',(12.1643024328504,-4.706001044865,336.429243586038));
#25324=CARTESIAN_POINT('Ctrl Pts',(12.1565369217473,-4.66628579456685,336.560012064711));
#25325=CARTESIAN_POINT('Ctrl Pts',(12.1487714106443,-4.6210637867871,336.689295157775));
#25326=CARTESIAN_POINT('Ctrl Pts',(12.1410058995412,-4.57046631275356,336.816595922732));
#25327=CARTESIAN_POINT('Ctrl Pts',(12.1332480879649,-4.51991900626218,336.943770468611));
#25328=CARTESIAN_POINT('Ctrl Pts',(12.1254902763886,-4.46400698354382,337.068966236913));
#25329=CARTESIAN_POINT('Ctrl Pts',(12.1177324648123,-4.40291135431033,337.191701318288));
#25330=CARTESIAN_POINT('Ctrl Pts',(12.1099804912352,-4.3418617014748,337.314344037624));
#25331=CARTESIAN_POINT('Ctrl Pts',(12.1022285176581,-4.27563638001457,337.434529407331));
#25332=CARTESIAN_POINT('Ctrl Pts',(12.0944765440809,-4.20446449016407,337.551795723299));
#25333=CARTESIAN_POINT('Ctrl Pts',(12.0867278534694,-4.13332274165271,337.669012376911));
#25334=CARTESIAN_POINT('Ctrl Pts',(12.0789791628578,-4.0572387936894,337.783312102087));
#25335=CARTESIAN_POINT('Ctrl Pts',(12.0712304722462,-3.97648744060711,337.894258229183));
#25336=CARTESIAN_POINT('Ctrl Pts',(12.0634833938146,-3.89575288851937,338.005181273009));
#25337=CARTESIAN_POINT('Ctrl Pts',(12.0557363153829,-3.81035309275928,338.112751790787));
#25338=CARTESIAN_POINT('Ctrl Pts',(12.0479892369513,-3.72060565573107,338.216562857623));
#25339=CARTESIAN_POINT('Ctrl Pts',(12.0402420935918,-3.63085746653497,338.320374794494));
#25340=CARTESIAN_POINT('Ctrl Pts',(12.0324949502323,-3.53676181902775,338.420426921884));
#25341=CARTESIAN_POINT('Ctrl Pts',(12.0247478068729,-3.43867574261208,338.51634642771));
#25342=CARTESIAN_POINT('Ctrl Pts',(12.0169989217914,-3.34056761436709,338.612287498275));
#25343=CARTESIAN_POINT('Ctrl Pts',(12.0092500367099,-3.23846755142362,338.704093825234));
#25344=CARTESIAN_POINT('Ctrl Pts',(12.0015011516284,-3.13276817400756,338.791430683848));
#25345=CARTESIAN_POINT('Ctrl Pts',(11.9937440418009,-3.02695660618964,338.878860242699));
#25346=CARTESIAN_POINT('Ctrl Pts',(11.9859869319734,-2.91753839419017,338.961810607373));
#25347=CARTESIAN_POINT('Ctrl Pts',(11.9782298221459,-2.80493830157268,339.039988141922));
#25348=CARTESIAN_POINT('Ctrl Pts',(11.9704685671672,-2.69227803907027,339.118207452043));
#25349=CARTESIAN_POINT('Ctrl Pts',(11.9627073121885,-2.57643283791569,339.191648640863));
#25350=CARTESIAN_POINT('Ctrl Pts',(11.9549460572098,-2.45785409904911,339.260062944404));
#25351=CARTESIAN_POINT('Ctrl Pts',(11.9471723867536,-2.33908567286134,339.328586688526));
#25352=CARTESIAN_POINT('Ctrl Pts',(11.9393987162974,-2.21757531750122,339.392067297226));
#25353=CARTESIAN_POINT('Ctrl Pts',(11.9316250458413,-2.09379734547272,339.450302881669));
#25354=CARTESIAN_POINT('Ctrl Pts',(11.9242132422521,-1.97578127796429,339.505827580873));
#25355=CARTESIAN_POINT('Ctrl Pts',(11.9168014386628,-1.85570422332627,339.556584467194));
#25356=CARTESIAN_POINT('Ctrl Pts',(11.9093896350736,-1.73399018350044,339.602440777025));
#25357=CARTESIAN_POINT('Ctrl Pts',(11.9016145563667,-1.60631056706227,339.650544644573));
#25358=CARTESIAN_POINT('Ctrl Pts',(11.8938394776597,-1.47642594956655,339.693407421766));
#25359=CARTESIAN_POINT('Ctrl Pts',(11.8860643989528,-1.3448057802539,339.730822388961));
#25360=CARTESIAN_POINT('Ctrl Pts',(11.8782988879751,-1.21334757793775,339.768191314658));
#25361=CARTESIAN_POINT('Ctrl Pts',(11.8705333769974,-1.08015844563361,339.800125663294));
#25362=CARTESIAN_POINT('Ctrl Pts',(11.8627678660198,-0.94572732209144,339.826466916363));
#25363=CARTESIAN_POINT('Ctrl Pts',(11.8550100545687,-0.811429487396761,
339.852782052004));
#25364=CARTESIAN_POINT('Ctrl Pts',(11.8472522431175,-0.67589249320408,339.873515053399));
#25365=CARTESIAN_POINT('Ctrl Pts',(11.8394944316664,-0.539619596209107,
339.888557430765));
#25366=CARTESIAN_POINT('Ctrl Pts',(11.8317424582142,-0.403449248886334,
339.903588488266));
#25367=CARTESIAN_POINT('Ctrl Pts',(11.8239904847621,-0.266544488003686,
339.912937402883));
#25368=CARTESIAN_POINT('Ctrl Pts',(11.8162385113098,-0.129417549668234,
339.916546975301));
#25369=CARTESIAN_POINT('Ctrl Pts',(11.8084898208223,0.00765131533958613,
339.920155019063));
#25370=CARTESIAN_POINT('Ctrl Pts',(11.8007411303348,0.144941780731573,339.918028544682));
#25371=CARTESIAN_POINT('Ctrl Pts',(11.7929924398473,0.281937934718363,339.910162325572));
#25372=CARTESIAN_POINT('Ctrl Pts',(11.7852453615391,0.418905585518681,339.902297743094));
#25373=CARTESIAN_POINT('Ctrl Pts',(11.7774982832308,0.555578656725884,339.88869581363));
#25374=CARTESIAN_POINT('Ctrl Pts',(11.7697512049226,0.691443083642843,339.869403405406));
#25375=CARTESIAN_POINT('Ctrl Pts',(11.762004061686,0.827308649243271,339.850110835492));
#25376=CARTESIAN_POINT('Ctrl Pts',(11.7542569184493,0.962365170043431,339.825127746644));
#25377=CARTESIAN_POINT('Ctrl Pts',(11.7465097752126,1.09610593132346,339.794552622489));
#25378=CARTESIAN_POINT('Ctrl Pts',(11.7387608902531,1.22987676037613,339.763970624395));
#25379=CARTESIAN_POINT('Ctrl Pts',(11.7310120052936,1.36233086030921,339.727794176385));
#25380=CARTESIAN_POINT('Ctrl Pts',(11.7232631203341,1.49297428462808,339.686172302417));
#25381=CARTESIAN_POINT('Ctrl Pts',(11.7155060106266,1.62375637525008,339.644506250555));
#25382=CARTESIAN_POINT('Ctrl Pts',(11.7077489009192,1.75272357812367,339.597383345817));
#25383=CARTESIAN_POINT('Ctrl Pts',(11.6999917912118,1.87939910459171,339.545001877685));
#25384=CARTESIAN_POINT('Ctrl Pts',(11.6922305363523,2.00614232242113,339.492592418567));
#25385=CARTESIAN_POINT('Ctrl Pts',(11.6844692814928,2.13059106925939,339.434918961127));
#25386=CARTESIAN_POINT('Ctrl Pts',(11.6767080266333,2.25229187523389,339.37222647758));
#25387=CARTESIAN_POINT('Ctrl Pts',(11.6689343562937,2.37418736286358,339.309433706478));
#25388=CARTESIAN_POINT('Ctrl Pts',(11.6611606859541,2.49332578563743,339.241606058823));
#25389=CARTESIAN_POINT('Ctrl Pts',(11.6533870156144,2.60928069322757,339.169033140484));
#25390=CARTESIAN_POINT('Ctrl Pts',(11.6459752106761,2.71983788425184,339.099838501267));
#25391=CARTESIAN_POINT('Ctrl Pts',(11.6385634057378,2.82750103706588,339.026330595297));
#25392=CARTESIAN_POINT('Ctrl Pts',(11.6311516007995,2.93192905595593,338.948794129015));
#25393=CARTESIAN_POINT('Ctrl Pts',(11.6233765220673,3.04147539122533,338.867457378388));
#25394=CARTESIAN_POINT('Ctrl Pts',(11.6156014433349,3.14780763439471,338.781430140587));
#25395=CARTESIAN_POINT('Ctrl Pts',(11.6078263646027,3.25049790458387,338.690995317634));
#25396=CARTESIAN_POINT('Ctrl Pts',(11.6000608536006,3.35306180784718,338.600671780497));
#25397=CARTESIAN_POINT('Ctrl Pts',(11.5922953425986,3.45199236485349,338.505951705905));
#25398=CARTESIAN_POINT('Ctrl Pts',(11.5845298315965,3.54689168119188,338.407160469422));
#25399=CARTESIAN_POINT('Ctrl Pts',(11.576772020122,3.64169690457268,338.308467184747));
#25400=CARTESIAN_POINT('Ctrl Pts',(11.5690142086474,3.73247857247892,338.205711051252));
#25401=CARTESIAN_POINT('Ctrl Pts',(11.5612563971729,3.8188731124596,338.099256558182));
#25402=CARTESIAN_POINT('Ctrl Pts',(11.5535044236981,3.90520263780165,337.992882175503));
#25403=CARTESIAN_POINT('Ctrl Pts',(11.5457524502234,3.98715136128012,337.882815275219));
#25404=CARTESIAN_POINT('Ctrl Pts',(11.5380004767486,4.06439398241709,337.769455653769));
#25405=CARTESIAN_POINT('Ctrl Pts',(11.5302517862401,4.14160389124996,337.656144040197));
#25406=CARTESIAN_POINT('Ctrl Pts',(11.5225030957316,4.21411144211037,337.539542801303));
#25407=CARTESIAN_POINT('Ctrl Pts',(11.514754405223,4.28163305037375,337.42008294991));
#25408=CARTESIAN_POINT('Ctrl Pts',(11.5070073268947,4.34914061019844,337.300647953145));
#25409=CARTESIAN_POINT('Ctrl Pts',(11.4992602485664,4.41166409860948,337.178355866962));
#25410=CARTESIAN_POINT('Ctrl Pts',(11.4915131702381,4.46896473818857,337.05366434242));
#25411=CARTESIAN_POINT('Ctrl Pts',(11.4837660269823,4.52626585799893,336.92897177285));
#25412=CARTESIAN_POINT('Ctrl Pts',(11.4760188837265,4.57834387845695,336.801880079977));
#25413=CARTESIAN_POINT('Ctrl Pts',(11.4682717404706,4.62500740413147,336.672868666163));
#25414=CARTESIAN_POINT('Ctrl Pts',(11.4605228554929,4.67168142075504,336.54382824785));
#25415=CARTESIAN_POINT('Ctrl Pts',(11.4527739705152,4.71293838739378,336.412867617268));
#25416=CARTESIAN_POINT('Ctrl Pts',(11.4450250855375,4.7486363186781,336.280482789979));
#25417=CARTESIAN_POINT('Ctrl Pts',(11.4372679758134,4.7843721401144,336.14795744807));
#25418=CARTESIAN_POINT('Ctrl Pts',(11.4295108660893,4.81453703763284,336.014005267767));
#25419=CARTESIAN_POINT('Ctrl Pts',(11.4217537563652,4.83903973938198,335.87913449664));
#25420=CARTESIAN_POINT('Ctrl Pts',(11.4139925014899,4.86355553459078,335.744191654889));
#25421=CARTESIAN_POINT('Ctrl Pts',(11.4062312466147,4.88240305137542,335.60832963119));
#25422=CARTESIAN_POINT('Ctrl Pts',(11.3984699917395,4.89554289352523,335.472062326557));
#25423=CARTESIAN_POINT('Ctrl Pts',(11.3906963213856,4.90870375514054,335.335577038643));
#25424=CARTESIAN_POINT('Ctrl Pts',(11.3829226510317,4.91613867562981,335.19868556477));
#25425=CARTESIAN_POINT('Ctrl Pts',(11.3751489806778,4.91786041399784,335.06190323847));
#25426=CARTESIAN_POINT('Ctrl Pts',(11.3677371759604,4.91950200516101,334.931488152007));
#25427=CARTESIAN_POINT('Ctrl Pts',(11.3603253712431,4.91595034845745,334.801172567865));
#25428=CARTESIAN_POINT('Ctrl Pts',(11.3529135665257,4.90726027313532,334.67139739166));
#25429=CARTESIAN_POINT('Ctrl Pts',(11.3451384873979,4.89814427159027,334.535261551297));
#25430=CARTESIAN_POINT('Ctrl Pts',(11.3373634082702,4.88334460907246,334.399290217979));
#25431=CARTESIAN_POINT('Ctrl Pts',(11.3295883291424,4.86286763306565,334.263996300429));
#25432=CARTESIAN_POINT('Ctrl Pts',(11.3218228177432,4.84241585527778,334.128868870633));
#25433=CARTESIAN_POINT('Ctrl Pts',(11.3140573063439,4.81630072265831,333.994417580752));
#25434=CARTESIAN_POINT('Ctrl Pts',(11.3062917949446,4.78458052699886,333.861153108112));
#25435=CARTESIAN_POINT('Ctrl Pts',(11.2985339830716,4.75289178200195,333.728020767569));
#25436=CARTESIAN_POINT('Ctrl Pts',(11.2907761711985,4.71560912350224,333.596073280305));
#25437=CARTESIAN_POINT('Ctrl Pts',(11.2830183593254,4.67284230840082,333.465813628232));
#25438=CARTESIAN_POINT('Ctrl Pts',(11.2752663854514,4.63010767668131,333.33565200067));
#25439=CARTESIAN_POINT('Ctrl Pts',(11.2675144115773,4.58189722439204,333.207176050004));
#25440=CARTESIAN_POINT('Ctrl Pts',(11.2597624377032,4.52837111016658,333.080875681174));
#25441=CARTESIAN_POINT('Ctrl Pts',(11.2520137467954,4.47486766428751,332.954628800638));
#25442=CARTESIAN_POINT('Ctrl Pts',(11.2442650558876,4.41605318612715,332.830556028556));
#25443=CARTESIAN_POINT('Ctrl Pts',(11.2365163649798,4.35213665968466,332.709129083093));
#25444=CARTESIAN_POINT('Ctrl Pts',(11.2287692862524,4.2882334316136,332.587727401529));
#25445=CARTESIAN_POINT('Ctrl Pts',(11.221022207525,4.21923044865788,332.468970797291));
#25446=CARTESIAN_POINT('Ctrl Pts',(11.2132751287976,4.14538334322485,332.353307724685));
#25447=CARTESIAN_POINT('Ctrl Pts',(11.2055279851431,4.07153561889084,332.237643682724));
#25448=CARTESIAN_POINT('Ctrl Pts',(11.1977808414887,3.99284390144801,332.125073553557));
#25449=CARTESIAN_POINT('Ctrl Pts',(11.1900336978343,3.90960775555046,332.016017717841));
#25450=CARTESIAN_POINT('Ctrl Pts',(11.1822848124588,3.8263528964146,331.906937364076));
#25451=CARTESIAN_POINT('Ctrl Pts',(11.1745359270833,3.73855181289198,331.8013731866));
#25452=CARTESIAN_POINT('Ctrl Pts',(11.1667870417078,3.64654477865058,331.69971300645));
#25453=CARTESIAN_POINT('Ctrl Pts',(11.1590299315896,3.55444008724329,331.59794492319));
#25454=CARTESIAN_POINT('Ctrl Pts',(11.1512728214714,3.45812079008668,331.500089405032));
#25455=CARTESIAN_POINT('Ctrl Pts',(11.1435157113532,3.35796489100063,331.406498246375));
#25456=CARTESIAN_POINT('Ctrl Pts',(11.1357544560852,3.2577554718275,331.312857075617));
#25457=CARTESIAN_POINT('Ctrl Pts',(11.1279932008171,3.15370566196412,331.223485059502));
#25458=CARTESIAN_POINT('Ctrl Pts',(11.1202319455491,3.04622629221872,331.138693428502));
#25459=CARTESIAN_POINT('Ctrl Pts',(11.1124582748088,2.9385749906024,331.053766158599));
#25460=CARTESIAN_POINT('Ctrl Pts',(11.1046846040684,2.82748348300727,330.973434144725));
#25461=CARTESIAN_POINT('Ctrl Pts',(11.0969109333281,2.71339202905719,330.897965534134));
#25462=CARTESIAN_POINT('Ctrl Pts',(11.0894991329693,2.60461162047467,330.8260100457));
#25463=CARTESIAN_POINT('Ctrl Pts',(11.0820873326105,2.49310452439647,330.758475511451));
#25464=CARTESIAN_POINT('Ctrl Pts',(11.0746755322517,2.37927117827199,330.695554423303));
#25465=CARTESIAN_POINT('Ctrl Pts',(11.0669004540225,2.25985846767934,330.629549355851));
#25466=CARTESIAN_POINT('Ctrl Pts',(11.0591253757932,2.13750833988029,330.568412823143));
#25467=CARTESIAN_POINT('Ctrl Pts',(11.051350297564,2.01265554563445,330.512417051783));
#25468=CARTESIAN_POINT('Ctrl Pts',(11.0435847870634,1.88795639069944,330.456490186784));
#25469=CARTESIAN_POINT('Ctrl Pts',(11.0358192765629,1.76076105025641,330.405691654565));
#25470=CARTESIAN_POINT('Ctrl Pts',(11.0280537660624,1.63153050868936,330.360248793123));
#25471=CARTESIAN_POINT('Ctrl Pts',(11.0202959550873,1.50242809956824,330.314850988406));
#25472=CARTESIAN_POINT('Ctrl Pts',(11.0125381441123,1.37129487143893,330.274798415771));
#25473=CARTESIAN_POINT('Ctrl Pts',(11.0047803331373,1.2386131881756,330.240270970677));
#25474=CARTESIAN_POINT('Ctrl Pts',(10.9970283601597,1.10603135206214,330.205769508575));
#25475=CARTESIAN_POINT('Ctrl Pts',(10.989276387182,0.971903756963217,330.176784996093));
#25476=CARTESIAN_POINT('Ctrl Pts',(10.9815244142043,0.83672904532098,330.153447868101));
#25477=CARTESIAN_POINT('Ctrl Pts',(10.9737757241874,0.701611580171872,330.130120623383));
#25478=CARTESIAN_POINT('Ctrl Pts',(10.9660270341704,0.565448264852558,330.112436072656));
#25479=CARTESIAN_POINT('Ctrl Pts',(10.9582783441535,0.428748870367813,330.10047375059));
#25480=CARTESIAN_POINT('Ctrl Pts',(10.9505312663134,0.292077917284233,330.088513917381));
#25481=CARTESIAN_POINT('Ctrl Pts',(10.9427841884733,0.154871496029147,330.082273978787));
#25482=CARTESIAN_POINT('Ctrl Pts',(10.9350371106332,0.0176450586626147,
330.081781652427));
#25483=CARTESIAN_POINT('Ctrl Pts',(10.9272899678617,-0.119582528853916,
330.08128932194));
#25484=CARTESIAN_POINT('Ctrl Pts',(10.9195428250902,-0.256829741944676,
330.086544701175));
#25485=CARTESIAN_POINT('Ctrl Pts',(10.9117956823187,-0.393580962017785,
330.097523371923));
#25486=CARTESIAN_POINT('Ctrl Pts',(10.9040467978211,-0.530362926739534,
330.108504510916));
#25487=CARTESIAN_POINT('Ctrl Pts',(10.8962979133234,-0.666648287006521,
330.12521147058));
#25488=CARTESIAN_POINT('Ctrl Pts',(10.8885490288258,-0.801926774322948,
330.147567979752));
#25489=CARTESIAN_POINT('Ctrl Pts',(10.8807919195723,-0.937348847792901,
330.169948218383));
#25490=CARTESIAN_POINT('Ctrl Pts',(10.8730348103189,-1.07176152721795,330.197989921254));
#25491=CARTESIAN_POINT('Ctrl Pts',(10.8652777010654,-1.20466442172109,330.231565593034));
#25492=CARTESIAN_POINT('Ctrl Pts',(10.8575164466564,-1.33763833535739,330.265159206598));
#25493=CARTESIAN_POINT('Ctrl Pts',(10.8497551922474,-1.46910048204842,330.304292570055));
#25494=CARTESIAN_POINT('Ctrl Pts',(10.8419939378384,-1.59856681742754,330.348788631688));
#25495=CARTESIAN_POINT('Ctrl Pts',(10.8342202679386,-1.72824025696867,330.393355872593));
#25496=CARTESIAN_POINT('Ctrl Pts',(10.8264465980388,-1.85591114113442,330.443302811732));
#25497=CARTESIAN_POINT('Ctrl Pts',(10.8186729281391,-1.98111572953476,330.498404335273));
#25498=CARTESIAN_POINT('Ctrl Pts',(10.8112611180853,-2.10049211662678,330.550940914703));
#25499=CARTESIAN_POINT('Ctrl Pts',(10.8038493080316,-2.21762639037123,330.608162868111));
#25500=CARTESIAN_POINT('Ctrl Pts',(10.7964374979778,-2.33213997903305,330.669837626521));
#25501=CARTESIAN_POINT('Ctrl Pts',(10.7886624193224,-2.45226612264708,330.734535196239));
#25502=CARTESIAN_POINT('Ctrl Pts',(10.780887340667,-2.56988781629231,330.804337546661));
#25503=CARTESIAN_POINT('Ctrl Pts',(10.7731122620116,-2.68454087019301,330.87902640402));
#25504=CARTESIAN_POINT('Ctrl Pts',(10.7653467510906,-2.79905283613695,330.953623351936));
#25505=CARTESIAN_POINT('Ctrl Pts',(10.7575812401695,-2.91060310658166,331.03309463101));
#25506=CARTESIAN_POINT('Ctrl Pts',(10.7498157292485,-3.01875104302033,331.117175615256));
#25507=CARTESIAN_POINT('Ctrl Pts',(10.742057917859,-3.12679175039732,331.201173232909));
#25508=CARTESIAN_POINT('Ctrl Pts',(10.7343001064695,-3.23143653048037,331.289771221736));
#25509=CARTESIAN_POINT('Ctrl Pts',(10.72654229508,-3.33227307053447,331.382661303404));
#25510=CARTESIAN_POINT('Ctrl Pts',(10.7187903216942,-3.43303372783418,331.475481482284));
#25511=CARTESIAN_POINT('Ctrl Pts',(10.7110383483085,-3.52999156305906,331.572587061208));
#25512=CARTESIAN_POINT('Ctrl Pts',(10.7032863749227,-3.62276704667213,331.67362930688));
#25513=CARTESIAN_POINT('Ctrl Pts',(10.6955376845087,-3.71550323973618,331.774628761018));
#25514=CARTESIAN_POINT('Ctrl Pts',(10.6877889940946,-3.80406034023309,331.879561278677));
#25515=CARTESIAN_POINT('Ctrl Pts',(10.6800403036806,-3.88809559938438,331.988041223299));
#25516=CARTESIAN_POINT('Ctrl Pts',(10.6722932254501,-3.97211337425625,332.096498597708));
#25517=CARTESIAN_POINT('Ctrl Pts',(10.6645461472197,-4.05161093989545,332.20850162219));
#25518=CARTESIAN_POINT('Ctrl Pts',(10.6567990689892,-4.12628604724091,332.323631841685));
#25519=CARTESIAN_POINT('Ctrl Pts',(10.6490519258345,-4.2009617804004,332.438763026027));
#25520=CARTESIAN_POINT('Ctrl Pts',(10.6413047826799,-4.27081476195385,332.557021129722));
#25521=CARTESIAN_POINT('Ctrl Pts',(10.6335576395251,-4.33558649484562,332.677959343979));
#25522=CARTESIAN_POINT('Ctrl Pts',(10.6258087546516,-4.40037278976881,332.798924747661));
#25523=CARTESIAN_POINT('Ctrl Pts',(10.6180598697781,-4.46007537833466,332.922571116402));
#25524=CARTESIAN_POINT('Ctrl Pts',(10.6103109849047,-4.5144822629871,333.04842807981));
#25525=CARTESIAN_POINT('Ctrl Pts',(10.6025538752892,-4.56894689563774,333.174418629027));
#25526=CARTESIAN_POINT('Ctrl Pts',(10.5947967656736,-4.6181044407316,333.302624100607));
#25527=CARTESIAN_POINT('Ctrl Pts',(10.5870396560581,-4.66179132155541,333.432554710119));
#25528=CARTESIAN_POINT('Ctrl Pts',(10.579278401294,-4.70550154723638,333.562554750349));
#25529=CARTESIAN_POINT('Ctrl Pts',(10.5715171465298,-4.74373517471746,333.694281390203));
#25530=CARTESIAN_POINT('Ctrl Pts',(10.5637558917657,-4.77637914633891,333.827231773572));
#25531=CARTESIAN_POINT('Ctrl Pts',(10.555982221526,-4.80907533766458,333.960394834178));
#25532=CARTESIAN_POINT('Ctrl Pts',(10.5482085512865,-4.83616392784002,334.094785166774));
#25533=CARTESIAN_POINT('Ctrl Pts',(10.5404348810469,-4.85758326331165,334.229890980124));
#25534=CARTESIAN_POINT('Ctrl Pts',(10.5330230752659,-4.87800552841682,334.358707615968));
#25535=CARTESIAN_POINT('Ctrl Pts',(10.5256112694849,-4.89327443229074,334.488174334846));
#25536=CARTESIAN_POINT('Ctrl Pts',(10.5181994637039,-4.90338068022248,334.61784693208));
#25537=CARTESIAN_POINT('Ctrl Pts',(10.510978391966,-4.91322685583372,334.74418255861));
#25538=CARTESIAN_POINT('Ctrl Pts',(10.5037573202281,-4.91819124337155,334.870903575023));
#25539=CARTESIAN_POINT('Ctrl Pts',(10.4965362484902,-4.91824948156275,334.997741768903));
#25540=CARTESIAN_POINT('',(13.9965362485423,-4.91824999987318,334.999964680808));
#25541=CARTESIAN_POINT('Ctrl Pts',(13.9965362484902,-4.91824999987319,334.999964681732));
#25542=CARTESIAN_POINT('Ctrl Pts',(13.9884256421174,-4.91825103404251,335.143978065363));
#25543=CARTESIAN_POINT('Ctrl Pts',(13.9803150357447,-4.91192238318742,335.287870977352));
#25544=CARTESIAN_POINT('Ctrl Pts',(13.972204429372,-4.89932153473325,335.431081850463));
#25545=CARTESIAN_POINT('Ctrl Pts',(13.964083322496,-4.88670437242486,335.574478133416));
#25546=CARTESIAN_POINT('Ctrl Pts',(13.95596221562,-4.86779883837988,335.717190283224));
#25547=CARTESIAN_POINT('Ctrl Pts',(13.9478411087441,-4.84271384339999,335.858665064762));
#25548=CARTESIAN_POINT('Ctrl Pts',(13.9397010098725,-4.81757018472774,336.000470698789));
#25549=CARTESIAN_POINT('Ctrl Pts',(13.9315609110009,-4.78621823022439,336.141032849077));
#25550=CARTESIAN_POINT('Ctrl Pts',(13.9234208121293,-4.74881773313696,336.279809829601));
#25551=CARTESIAN_POINT('Ctrl Pts',(13.9152707060907,-4.7113712571216,336.418757417932));
#25552=CARTESIAN_POINT('Ctrl Pts',(13.9071206000521,-4.66786149995246,336.55591513884));
#25553=CARTESIAN_POINT('Ctrl Pts',(13.8989704940135,-4.61849709912264,336.690759476654));
#25554=CARTESIAN_POINT('Ctrl Pts',(13.8908017834144,-4.56902001227631,336.825911628825));
#25555=CARTESIAN_POINT('Ctrl Pts',(13.8826330728153,-4.51366168677281,336.958739529566));
#25556=CARTESIAN_POINT('Ctrl Pts',(13.8744643622162,-4.45267838032965,337.088740841714));
#25557=CARTESIAN_POINT('Ctrl Pts',(13.8686615331412,-4.40935750374523,337.181090225961));
#25558=CARTESIAN_POINT('Ctrl Pts',(13.8628587040662,-4.36319906953297,337.272013742014));
#25559=CARTESIAN_POINT('Ctrl Pts',(13.8570558749911,-4.31430829889828,337.361340078125));
#25560=CARTESIAN_POINT('Ctrl Pts',(13.8492807962115,-4.24880066660915,337.481026405496));
#25561=CARTESIAN_POINT('Ctrl Pts',(13.8415057174318,-4.17820528925671,337.598173853379));
#25562=CARTESIAN_POINT('Ctrl Pts',(13.8337306386522,-4.10274357159917,337.71231971718));
#25563=CARTESIAN_POINT('Ctrl Pts',(13.825965127602,-4.02737471438931,337.826325117228));
#25564=CARTESIAN_POINT('Ctrl Pts',(13.8181996165518,-3.94715164545592,337.937335959534));
#25565=CARTESIAN_POINT('Ctrl Pts',(13.8104341055015,-3.86234196160846,338.044913403383));
#25566=CARTESIAN_POINT('Ctrl Pts',(13.8026762939781,-3.77761636680938,338.152384183882));
#25567=CARTESIAN_POINT('Ctrl Pts',(13.7949184824547,-3.6883134475944,338.256428035543));
#25568=CARTESIAN_POINT('Ctrl Pts',(13.7871606709313,-3.59474426076282,338.356634737682));
#25569=CARTESIAN_POINT('Ctrl Pts',(13.7794086974071,-3.50124548771195,338.456766031099));
#25570=CARTESIAN_POINT('Ctrl Pts',(13.7716567238829,-3.40348710308307,338.553065638034));
#25571=CARTESIAN_POINT('Ctrl Pts',(13.7639047503587,-3.30182039623613,338.645156393558));
#25572=CARTESIAN_POINT('Ctrl Pts',(13.7561560597999,-3.20019674529963,338.737208148593));
#25573=CARTESIAN_POINT('Ctrl Pts',(13.7484073692411,-3.09466835326824,338.825054335522));
#25574=CARTESIAN_POINT('Ctrl Pts',(13.7406586786823,-2.98562316344224,338.908354818644));
#25575=CARTESIAN_POINT('Ctrl Pts',(13.7329116003032,-2.87660066137888,338.991637970405));
#25576=CARTESIAN_POINT('Ctrl Pts',(13.7251645219242,-2.76406312734088,339.070377062435));
#25577=CARTESIAN_POINT('Ctrl Pts',(13.7174174435452,-2.6484310487751,339.14427267954));
#25578=CARTESIAN_POINT('Ctrl Pts',(13.7096703002382,-2.53279800110129,339.218168915962));
#25579=CARTESIAN_POINT('Ctrl Pts',(13.7019231569312,-2.41407068653288,339.287221386012));
#25580=CARTESIAN_POINT('Ctrl Pts',(13.6941760136242,-2.29269765002026,339.351174617054));
#25581=CARTESIAN_POINT('Ctrl Pts',(13.6864271285949,-2.17129732627237,339.41514222614));
#25582=CARTESIAN_POINT('Ctrl Pts',(13.6786782435656,-2.04725044270476,339.474008132801));
#25583=CARTESIAN_POINT('Ctrl Pts',(13.6709293585364,-1.92102879119393,339.527563522018));
#25584=CARTESIAN_POINT('Ctrl Pts',(13.6631722487605,-1.79467316671826,339.581175755477));
#25585=CARTESIAN_POINT('Ctrl Pts',(13.6554151389846,-1.6661385236044,339.629466058866));
#25586=CARTESIAN_POINT('Ctrl Pts',(13.6476580292087,-1.53591574020686,339.672274168056));
#25587=CARTESIAN_POINT('Ctrl Pts',(13.6398967742814,-1.40562336991769,339.715105152531));
#25588=CARTESIAN_POINT('Ctrl Pts',(13.6321355193541,-1.27364143777154,339.752447999136));
#25589=CARTESIAN_POINT('Ctrl Pts',(13.6243742644267,-1.14047355220852,339.784193049952));
#25590=CARTESIAN_POINT('Ctrl Pts',(13.6166005940209,-1.0070926414283,339.815988882505));
#25591=CARTESIAN_POINT('Ctrl Pts',(13.6088269236151,-0.872522370068482,
339.842168950547));
#25592=CARTESIAN_POINT('Ctrl Pts',(13.6010532532093,-0.737274934218635,
339.862675059458));
#25593=CARTESIAN_POINT('Ctrl Pts',(13.5936414490453,-0.608323299292495,
339.882226604028));
#25594=CARTESIAN_POINT('Ctrl Pts',(13.5862296448812,-0.478756411163081,
339.896620515469));
#25595=CARTESIAN_POINT('Ctrl Pts',(13.5788178407172,-0.349018526858915,
339.90585050021));
#25596=CARTESIAN_POINT('Ctrl Pts',(13.5710427619398,-0.212921802153868,
339.915532874013));
#25597=CARTESIAN_POINT('Ctrl Pts',(13.5632676831624,-0.0762068045868471,
339.919562921081));
#25598=CARTESIAN_POINT('Ctrl Pts',(13.555492604385,0.0606175528599034,339.917876429394));
#25599=CARTESIAN_POINT('Ctrl Pts',(13.547727093337,0.197273539224128,339.916192013041));
#25600=CARTESIAN_POINT('Ctrl Pts',(13.5399615822891,0.334038230595531,339.908805059471));
#25601=CARTESIAN_POINT('Ctrl Pts',(13.5321960712411,0.470397784465939,339.895703114658));
#25602=CARTESIAN_POINT('Ctrl Pts',(13.5244382597199,0.606622137441573,339.882614160461));
#25603=CARTESIAN_POINT('Ctrl Pts',(13.5166804481988,0.742441765735969,339.863821528681));
#25604=CARTESIAN_POINT('Ctrl Pts',(13.5089226366776,0.877343375341519,339.839364799666));
#25605=CARTESIAN_POINT('Ctrl Pts',(13.5011706631556,1.01214346720822,339.814926475115));
#25606=CARTESIAN_POINT('Ctrl Pts',(13.4934186896336,1.14602653240934,339.784832606898));
#25607=CARTESIAN_POINT('Ctrl Pts',(13.4856667161116,1.27848530207947,339.749174496148));
#25608=CARTESIAN_POINT('Ctrl Pts',(13.477918025555,1.41088797538217,339.713531486629));
#25609=CARTESIAN_POINT('Ctrl Pts',(13.4701693349984,1.54186717620465,339.672329022805));
#25610=CARTESIAN_POINT('Ctrl Pts',(13.4624206444417,1.67092693879983,339.625709267528));
#25611=CARTESIAN_POINT('Ctrl Pts',(13.4546735660649,1.79995984943364,339.57909921188));
#25612=CARTESIAN_POINT('Ctrl Pts',(13.4469264876881,1.92707374879178,339.527074239399));
#25613=CARTESIAN_POINT('Ctrl Pts',(13.4391794093112,2.0517893023655,339.469825916207));
#25614=CARTESIAN_POINT('Ctrl Pts',(13.4314322660064,2.17650590117568,339.41257711322));
#25615=CARTESIAN_POINT('Ctrl Pts',(13.4236851227016,2.29882375887348,339.35010503527));
#25616=CARTESIAN_POINT('Ctrl Pts',(13.4159379793968,2.41828530965967,339.282648622475));
#25617=CARTESIAN_POINT('Ctrl Pts',(13.4081890943696,2.53777371793905,339.215177044045));
#25618=CARTESIAN_POINT('Ctrl Pts',(13.4004402093425,2.65440420118941,339.142719093086));
#25619=CARTESIAN_POINT('Ctrl Pts',(13.3926913243154,2.76774584874975,339.065558507663));
#25620=CARTESIAN_POINT('Ctrl Pts',(13.3849342145416,2.88120779830602,338.988316023196));
#25621=CARTESIAN_POINT('Ctrl Pts',(13.3771771047678,2.99137361534582,338.906361153738));
#25622=CARTESIAN_POINT('Ctrl Pts',(13.369419994994,3.09784288790242,338.820019961253));
#25623=CARTESIAN_POINT('Ctrl Pts',(13.3616587400688,3.20436905423441,338.733632630796));
#25624=CARTESIAN_POINT('Ctrl Pts',(13.3538974851436,3.30719444721646,338.642854565418));
#25625=CARTESIAN_POINT('Ctrl Pts',(13.3461362302183,3.40595432174344,338.548049918011));
#25626=CARTESIAN_POINT('Ctrl Pts',(13.3383625598146,3.50487217988418,338.453093614064));
#25627=CARTESIAN_POINT('Ctrl Pts',(13.3305888894108,3.59971125309843,338.354098139025));
#25628=CARTESIAN_POINT('Ctrl Pts',(13.3228152190071,3.69014542559512,338.251462717064));
#25629=CARTESIAN_POINT('Ctrl Pts',(13.3154034148191,3.7763698657418,338.153604998533));
#25630=CARTESIAN_POINT('Ctrl Pts',(13.3079916106311,3.85859009094201,338.052438809204));
#25631=CARTESIAN_POINT('Ctrl Pts',(13.3005798064431,3.93656039582682,337.948334328482));
#25632=CARTESIAN_POINT('Ctrl Pts',(13.2928047276668,4.01835225747256,337.83912737724));
#25633=CARTESIAN_POINT('Ctrl Pts',(13.2850296488905,4.0957255399037,337.726341708832));
#25634=CARTESIAN_POINT('Ctrl Pts',(13.2772545701143,4.16835084384594,337.610370530233));
#25635=CARTESIAN_POINT('Ctrl Pts',(13.2694890590674,4.24088677772781,337.494542061552));
#25636=CARTESIAN_POINT('Ctrl Pts',(13.2617235480207,4.30868615292419,337.375536210413));
#25637=CARTESIAN_POINT('Ctrl Pts',(13.2539580369738,4.37146042691334,337.253778338353));
#25638=CARTESIAN_POINT('Ctrl Pts',(13.2462002254538,4.434172460027,337.132141189579));
#25639=CARTESIAN_POINT('Ctrl Pts',(13.2384424139338,4.49186912923255,337.007757795206));
#25640=CARTESIAN_POINT('Ctrl Pts',(13.2306846024138,4.54430594564836,336.881081214314));
#25641=CARTESIAN_POINT('Ctrl Pts',(13.222932628893,4.59670330169702,336.754499961566));
#25642=CARTESIAN_POINT('Ctrl Pts',(13.2151806553722,4.64384853467592,336.625629316913));
#25643=CARTESIAN_POINT('Ctrl Pts',(13.2074286818514,4.68554390936441,336.494945261847));
#25644=CARTESIAN_POINT('Ctrl Pts',(13.199679991296,4.72722162603674,336.364316551556));
#25645=CARTESIAN_POINT('Ctrl Pts',(13.1919313007406,4.76345395634192,336.231876329916));
#25646=CARTESIAN_POINT('Ctrl Pts',(13.1841826101852,4.79409205253145,336.098118597582));
#25647=CARTESIAN_POINT('Ctrl Pts',(13.1764355318096,4.82472377420917,335.96438869466));
#25648=CARTESIAN_POINT('Ctrl Pts',(13.1686884534339,4.84976348968724,335.829342207055));
#25649=CARTESIAN_POINT('Ctrl Pts',(13.1609413750583,4.86911289559848,335.6934858848));
#25650=CARTESIAN_POINT('Ctrl Pts',(13.1531942317548,4.88846246367635,335.557628423938));
#25651=CARTESIAN_POINT('Ctrl Pts',(13.1454470884512,4.90212157195129,335.420961501859));
#25652=CARTESIAN_POINT('Ctrl Pts',(13.1376999451476,4.91004353515523,335.283999199612));
#25653=CARTESIAN_POINT('Ctrl Pts',(13.1299510601217,4.9179672793847,335.147006105331));
#25654=CARTESIAN_POINT('Ctrl Pts',(13.1222021750959,4.92015128935531,335.009717888884));
#25655=CARTESIAN_POINT('Ctrl Pts',(13.11445329007,4.91660097597461,334.872650459186));
#25656=CARTESIAN_POINT('Ctrl Pts',(13.1066961802975,4.91304689425462,334.735437544702));
#25657=CARTESIAN_POINT('Ctrl Pts',(13.098939070525,4.9037463410254,334.598446276455));
#25658=CARTESIAN_POINT('Ctrl Pts',(13.0911819607525,4.88875682285954,334.462189820249));
#25659=CARTESIAN_POINT('Ctrl Pts',(13.0834207058286,4.87375929477445,334.325860552949));
#25660=CARTESIAN_POINT('Ctrl Pts',(13.0756594509046,4.85306680321454,334.190267266305));
#25661=CARTESIAN_POINT('Ctrl Pts',(13.0678981959807,4.82678818760873,334.055913746281));
#25662=CARTESIAN_POINT('Ctrl Pts',(13.0601245255782,4.800467534782,333.921345304411));
#25663=CARTESIAN_POINT('Ctrl Pts',(13.0523508551757,4.76854299224878,333.788020972555));
#25664=CARTESIAN_POINT('Ctrl Pts',(13.0445771847733,4.73117379616419,333.656431031547));
#25665=CARTESIAN_POINT('Ctrl Pts',(13.0371653805719,4.69554414502124,333.530966633506));
#25666=CARTESIAN_POINT('Ctrl Pts',(13.0297535763706,4.65496541971395,333.407079061856));
#25667=CARTESIAN_POINT('Ctrl Pts',(13.0223417721693,4.60961594672888,333.285175260803));
#25668=CARTESIAN_POINT('Ctrl Pts',(13.0145666933827,4.56204376108948,333.157296591612));
#25669=CARTESIAN_POINT('Ctrl Pts',(13.0067916145961,4.5090710090725,333.031196950752));
#25670=CARTESIAN_POINT('Ctrl Pts',(12.9990165358095,4.45085008996464,332.907366123957));
#25671=CARTESIAN_POINT('Ctrl Pts',(12.9912510247524,4.39270081540411,332.783687678878));
#25672=CARTESIAN_POINT('Ctrl Pts',(12.9834855136953,4.32931638844699,332.66227284309));
#25673=CARTESIAN_POINT('Ctrl Pts',(12.9757200026381,4.26089835777225,332.543594445692));
#25674=CARTESIAN_POINT('Ctrl Pts',(12.9679621911077,4.19254816377381,332.425033718271));
#25675=CARTESIAN_POINT('Ctrl Pts',(12.9602043795773,4.11917449206052,332.309204366295));
#25676=CARTESIAN_POINT('Ctrl Pts',(12.9524465680469,4.04102602271569,332.196557161946));
#25677=CARTESIAN_POINT('Ctrl Pts',(12.9446945945157,3.96293636257264,332.083994728192));
#25678=CARTESIAN_POINT('Ctrl Pts',(12.9369426209846,3.88007927876489,331.974609995461));
#25679=CARTESIAN_POINT('Ctrl Pts',(12.9291906474535,3.79274802841089,331.868826824418));
#25680=CARTESIAN_POINT('Ctrl Pts',(12.9214419568877,3.70545376289335,331.76308845261));
#25681=CARTESIAN_POINT('Ctrl Pts',(12.9136932663219,3.6136893478073,331.660948909647));
#25682=CARTESIAN_POINT('Ctrl Pts',(12.9059445757562,3.51778964878551,331.562800696876));
#25683=CARTESIAN_POINT('Ctrl Pts',(12.8981974973703,3.42190990249744,331.46467290466));
#25684=CARTESIAN_POINT('Ctrl Pts',(12.8904504189844,3.32189685662842,331.370535070252));
#25685=CARTESIAN_POINT('Ctrl Pts',(12.8827033405985,3.21812345050283,331.280744090571));
#25686=CARTESIAN_POINT('Ctrl Pts',(12.8749561972846,3.11434917465628,331.190952358355));
#25687=CARTESIAN_POINT('Ctrl Pts',(12.8672090539707,3.00681477127838,331.105507809289));
#25688=CARTESIAN_POINT('Ctrl Pts',(12.8594619106568,2.89592727801453,331.024727900766));
#25689=CARTESIAN_POINT('Ctrl Pts',(12.8517130256206,2.78501485488877,330.943929831204));
#25690=CARTESIAN_POINT('Ctrl Pts',(12.8439641405845,2.67074815767828,330.867798719107));
#25691=CARTESIAN_POINT('Ctrl Pts',(12.8362152555484,2.55356395335009,330.796609202245));
#25692=CARTESIAN_POINT('Ctrl Pts',(12.8284581457657,2.43625536849858,330.725344124095));
#25693=CARTESIAN_POINT('Ctrl Pts',(12.820701035983,2.31602342522526,330.659031321944));
#25694=CARTESIAN_POINT('Ctrl Pts',(12.8129439262004,2.19333077571006,330.597900140748));
#25695=CARTESIAN_POINT('Ctrl Pts',(12.8051826712663,2.07057256316673,330.536736293005));
#25696=CARTESIAN_POINT('Ctrl Pts',(12.7974214163323,1.94535138094186,330.480759742922));
#25697=CARTESIAN_POINT('Ctrl Pts',(12.7896601613983,1.81814977266187,330.430151592594));
#25698=CARTESIAN_POINT('Ctrl Pts',(12.7818864909859,1.69074468326616,330.37946248572));
#25699=CARTESIAN_POINT('Ctrl Pts',(12.7741128205735,1.56135320625019,330.334159068585));
#25700=CARTESIAN_POINT('Ctrl Pts',(12.7663391501611,1.430473801047,330.294372755198));
#25701=CARTESIAN_POINT('Ctrl Pts',(12.7589273460726,1.30568686525819,330.256438504763));
#25702=CARTESIAN_POINT('Ctrl Pts',(12.751515541984,1.17954768845702,330.223519347463));
#25703=CARTESIAN_POINT('Ctrl Pts',(12.7441037378954,1.05249498138151,330.195685545609));
#25704=CARTESIAN_POINT('Ctrl Pts',(12.7363286591259,0.919215041222547,330.166487525899));
#25705=CARTESIAN_POINT('Ctrl Pts',(12.7285535803563,0.784508567590338,330.142793691957));
#25706=CARTESIAN_POINT('Ctrl Pts',(12.7207785015868,0.648869903754681,330.12474093914));
#25707=CARTESIAN_POINT('Ctrl Pts',(12.7130129905467,0.513398151930061,330.106710401383));
#25708=CARTESIAN_POINT('Ctrl Pts',(12.7052474795066,0.376996876094345,330.094307183815));
#25709=CARTESIAN_POINT('Ctrl Pts',(12.6974819684664,0.240172757877525,330.087617674806));
#25710=CARTESIAN_POINT('Ctrl Pts',(12.689724156953,0.103484301170844,330.080934798466));
#25711=CARTESIAN_POINT('Ctrl Pts',(12.6819663454396,-0.0336257756937801,
330.079954375664));
#25712=CARTESIAN_POINT('Ctrl Pts',(12.6742085339262,-0.170643833711854,
330.084711224708));
#25713=CARTESIAN_POINT('Ctrl Pts',(12.666456560412,-0.307558781296432,330.089464494071));
#25714=CARTESIAN_POINT('Ctrl Pts',(12.6587045868979,-0.444381458801369,
330.099946428041));
#25715=CARTESIAN_POINT('Ctrl Pts',(12.6509526133836,-0.580596734500016,
330.116139795778));
#25716=CARTESIAN_POINT('Ctrl Pts',(12.6432039228347,-0.716754322950137,
330.132326305613));
#25717=CARTESIAN_POINT('Ctrl Pts',(12.6354552322857,-0.852304633882892,
330.154219392355));
#25718=CARTESIAN_POINT('Ctrl Pts',(12.6277065417368,-0.986736389534527,
330.181749865349));
#25719=CARTESIAN_POINT('Ctrl Pts',(12.6199594633676,-1.12114017553767,330.209274610398));
#25720=CARTESIAN_POINT('Ctrl Pts',(12.6122123849984,-1.25442548647925,330.242434330338));
#25721=CARTESIAN_POINT('Ctrl Pts',(12.6044653066292,-1.38609038125846,330.281108549936));
#25722=CARTESIAN_POINT('Ctrl Pts',(12.5967181633319,-1.51775637951739,330.319783093663));
#25723=CARTESIAN_POINT('Ctrl Pts',(12.5889710200346,-1.6478015594959,330.363972119073));
#25724=CARTESIAN_POINT('Ctrl Pts',(12.5812238767374,-1.77573869307614,330.413505133938));
#25725=CARTESIAN_POINT('Ctrl Pts',(12.5734749917177,-1.90370458964197,330.463049284877));
#25726=CARTESIAN_POINT('Ctrl Pts',(12.5657261066981,-2.02956113229754,330.51793967491));
#25727=CARTESIAN_POINT('Ctrl Pts',(12.5579772216784,-2.15284101261706,330.577957639631));
#25728=CARTESIAN_POINT('Ctrl Pts',(12.550220111912,-2.27625174347826,330.638039308042));
#25729=CARTESIAN_POINT('Ctrl Pts',(12.5424630021455,-2.39707999679826,330.703259251603));
#25730=CARTESIAN_POINT('Ctrl Pts',(12.5347058923791,-2.51488254386838,330.773352527943));
#25731=CARTESIAN_POINT('Ctrl Pts',(12.5269446374611,-2.63274804085417,330.843483259889));
#25732=CARTESIAN_POINT('Ctrl Pts',(12.5191833825431,-2.747584282806,330.918492299979));
#25733=CARTESIAN_POINT('Ctrl Pts',(12.5114221276251,-2.85897784506546,330.998071871719));
#25734=CARTESIAN_POINT('Ctrl Pts',(12.5036484572285,-2.97054960072482,331.077778744841));
#25735=CARTESIAN_POINT('Ctrl Pts',(12.4958747868318,-3.07866736332111,331.162070519423));
#25736=CARTESIAN_POINT('Ctrl Pts',(12.4881011164351,-3.18295087900974,331.250599145955));
#25737=CARTESIAN_POINT('Ctrl Pts',(12.4806893121639,-3.28237997331853,331.335006744782));
#25738=CARTESIAN_POINT('Ctrl Pts',(12.4732775078927,-3.37832354385145,331.423265426778));
#25739=CARTESIAN_POINT('Ctrl Pts',(12.4658657036215,-3.47048509395734,331.515044293665));
#25740=CARTESIAN_POINT('Ctrl Pts',(12.4581989668869,-3.56581658354646,331.609979937467));
#25741=CARTESIAN_POINT('Ctrl Pts',(12.4505322301522,-3.65742082068215,331.709000872742));
#25742=CARTESIAN_POINT('Ctrl Pts',(12.4428654934176,-3.74491984483852,331.811778172988));
#25743=CARTESIAN_POINT('Ctrl Pts',(12.4352083652815,-3.83230920786664,331.914426664087));
#25744=CARTESIAN_POINT('Ctrl Pts',(12.4275512371456,-3.9156033317039,332.020821853806));
#25745=CARTESIAN_POINT('Ctrl Pts',(12.4198941090095,-3.99445959541091,332.130596646839));
#25746=CARTESIAN_POINT('Ctrl Pts',(12.412245785164,-4.07322518890332,332.24024521903));
#25747=CARTESIAN_POINT('Ctrl Pts',(12.4045974613184,-4.14756284618153,332.353265334361));
#25748=CARTESIAN_POINT('Ctrl Pts',(12.3969491374728,-4.21716938003608,332.469255942892));
#25749=CARTESIAN_POINT('Ctrl Pts',(12.3893057423903,-4.2867310577731,332.585171804298));
#25750=CARTESIAN_POINT('Ctrl Pts',(12.3816623473078,-4.35156746745738,332.704054009051));
#25751=CARTESIAN_POINT('Ctrl Pts',(12.3740189522253,-4.41141810878121,332.825471698962));
#25752=CARTESIAN_POINT('Ctrl Pts',(12.3663787195025,-4.47124398764593,332.946839153812));
#25753=CARTESIAN_POINT('Ctrl Pts',(12.3587384867798,-4.52608802306232,333.070739646857));
#25754=CARTESIAN_POINT('Ctrl Pts',(12.3510982540571,-4.57573542323469,333.196717326913));
#25755=CARTESIAN_POINT('Ctrl Pts',(12.3434594202139,-4.62537373327361,333.322671941231));
#25756=CARTESIAN_POINT('Ctrl Pts',(12.3358205863708,-4.66981715451252,333.45070261101));
#25757=CARTESIAN_POINT('Ctrl Pts',(12.3281817525277,-4.7088990670405,333.580333617034));
#25758=CARTESIAN_POINT('Ctrl Pts',(12.3205398922302,-4.74799646355784,333.710015981984));
#25759=CARTESIAN_POINT('Ctrl Pts',(12.3128980319327,-4.78172798859826,333.84129956474));
#25760=CARTESIAN_POINT('Ctrl Pts',(12.3052561716352,-4.8099769543655,333.973693632012));
#25761=CARTESIAN_POINT('Ctrl Pts',(12.2976126983372,-4.83823188276458,334.106115644274));
#25762=CARTESIAN_POINT('Ctrl Pts',(12.2899692250391,-4.8610018746485,334.239648211607));
#25763=CARTESIAN_POINT('Ctrl Pts',(12.282325751741,-4.87822163004422,334.373791735388));
#25764=CARTESIAN_POINT('Ctrl Pts',(12.2746752918931,-4.89545712523185,334.508057873636));
#25765=CARTESIAN_POINT('Ctrl Pts',(12.2670248320452,-4.90713221466497,334.642935682609));
#25766=CARTESIAN_POINT('Ctrl Pts',(12.2593743721972,-4.91323358555503,334.777921643841));
#25767=CARTESIAN_POINT('Ctrl Pts',(12.25509499764,-4.91664645901231,334.853427626431));
#25768=CARTESIAN_POINT('Ctrl Pts',(12.2508156230828,-4.91831633393994,334.928967437061));
#25769=CARTESIAN_POINT('Ctrl Pts',(12.2465362485256,-4.91824798382928,335.004453320022));
#25770=CARTESIAN_POINT('',(15.7465362484503,-4.91824799676571,334.995560989963));
#25771=CARTESIAN_POINT('Ctrl Pts',(15.7465362484503,-4.91824799676571,334.995560989963));
#25772=CARTESIAN_POINT('Ctrl Pts',(15.738885780287,-4.9183697858298,335.130498468261));
#25773=CARTESIAN_POINT('Ctrl Pts',(15.7312353121238,-4.91293416765952,335.265610303156));
#25774=CARTESIAN_POINT('Ctrl Pts',(15.7235848439605,-4.9019248808743,335.400394211703));
#25775=CARTESIAN_POINT('Ctrl Pts',(15.7159405224128,-4.89092443928026,335.535069830816));
#25776=CARTESIAN_POINT('Ctrl Pts',(15.7082962008649,-4.87435926978116,335.669417648052));
#25777=CARTESIAN_POINT('Ctrl Pts',(15.7006518793172,-4.85226517655128,335.802935687915));
#25778=CARTESIAN_POINT('Ctrl Pts',(15.6930111657414,-4.83018151130608,335.936390709846));
#25779=CARTESIAN_POINT('Ctrl Pts',(15.6853704521656,-4.80257417611059,336.069016336483));
#25780=CARTESIAN_POINT('Ctrl Pts',(15.6777297385898,-4.76953074589983,336.200316427621));
#25781=CARTESIAN_POINT('Ctrl Pts',(15.6700907439083,-4.73649474930951,336.331586980813));
#25782=CARTESIAN_POINT('Ctrl Pts',(15.6624517492269,-4.69802518718896,336.461532200858));
#25783=CARTESIAN_POINT('Ctrl Pts',(15.6548127545454,-4.65426048965109,336.58966737306));
#25784=CARTESIAN_POINT('Ctrl Pts',(15.6471737158579,-4.61049553999737,336.717803283413));
#25785=CARTESIAN_POINT('Ctrl Pts',(15.6395346771703,-4.56143552472917,336.844128743959));
#25786=CARTESIAN_POINT('Ctrl Pts',(15.6318956384828,-4.50726818798027,336.968175943385));
#25787=CARTESIAN_POINT('Ctrl Pts',(15.624254793065,-4.45308803996375,337.092252481561));
#25788=CARTESIAN_POINT('Ctrl Pts',(15.6166139476471,-4.39379833009925,337.214049318207));
#25789=CARTESIAN_POINT('Ctrl Pts',(15.6089731022292,-4.32963397083435,337.333120815795));
#25790=CARTESIAN_POINT('Ctrl Pts',(15.6013243259428,-4.26540301172684,337.452315904472));
#25791=CARTESIAN_POINT('Ctrl Pts',(15.5936755496564,-4.19628749307921,337.568779651522));
#25792=CARTESIAN_POINT('Ctrl Pts',(15.5860267733699,-4.12256726349281,337.682092880658));
#25793=CARTESIAN_POINT('Ctrl Pts',(15.5783736305095,-4.04880494811062,337.795470798652));
#25794=CARTESIAN_POINT('Ctrl Pts',(15.570720487649,-3.97043292165567,337.905694290615));
#25795=CARTESIAN_POINT('Ctrl Pts',(15.5630673447886,-3.8877721813424,338.012376226251));
#25796=CARTESIAN_POINT('Ctrl Pts',(15.555402869579,-3.80498904159278,338.119216130575));
#25797=CARTESIAN_POINT('Ctrl Pts',(15.5477383943693,-3.71790476821926,338.222503701535));
#25798=CARTESIAN_POINT('Ctrl Pts',(15.5400739191597,-3.62687844218333,338.321887389441));
#25799=CARTESIAN_POINT('Ctrl Pts',(15.5355439729847,-3.57307901741176,338.38062627822));
#25800=CARTESIAN_POINT('Ctrl Pts',(15.5310140268097,-3.51790323607385,338.438002198636));
#25801=CARTESIAN_POINT('Ctrl Pts',(15.5264840806347,-3.46143058174976,338.4939492541));
#25802=CARTESIAN_POINT('Ctrl Pts',(15.5187090018562,-3.36450242427632,338.589975287712));
#25803=CARTESIAN_POINT('Ctrl Pts',(15.5109339230777,-3.26342218309583,338.682116574258));
#25804=CARTESIAN_POINT('Ctrl Pts',(15.5031588442992,-3.15853405726114,338.769992794638));
#25805=CARTESIAN_POINT('Ctrl Pts',(15.4953933332502,-3.05377500294279,338.857760877734));
#25806=CARTESIAN_POINT('Ctrl Pts',(15.4876278222011,-2.94521768421036,338.941274088922));
#25807=CARTESIAN_POINT('Ctrl Pts',(15.4798623111521,-2.83324376524844,339.02018815843));
#25808=CARTESIAN_POINT('Ctrl Pts',(15.4721044996299,-2.72138086875325,339.099023984408));
#25809=CARTESIAN_POINT('Ctrl Pts',(15.4643466881077,-2.60610843092591,339.173269519769));
#25810=CARTESIAN_POINT('Ctrl Pts',(15.4565888765854,-2.48784160577255,339.24262032323));
#25811=CARTESIAN_POINT('Ctrl Pts',(15.4488369030624,-2.36966378015558,339.311918938013));
#25812=CARTESIAN_POINT('Ctrl Pts',(15.4410849295394,-2.24849638825972,339.376329955683));
#25813=CARTESIAN_POINT('Ctrl Pts',(15.4333329560164,-2.12478371522614,339.435592094187));
#25814=CARTESIAN_POINT('Ctrl Pts',(15.4255842654587,-2.0011234345832,339.494829135139));
#25815=CARTESIAN_POINT('Ctrl Pts',(15.4178355749011,-1.87492036850731,339.548921465377));
#25816=CARTESIAN_POINT('Ctrl Pts',(15.4100868843435,-1.74664336985366,339.597653749582));
#25817=CARTESIAN_POINT('Ctrl Pts',(15.4023398059656,-1.61839306030097,339.646375894629));
#25818=CARTESIAN_POINT('Ctrl Pts',(15.3945927275877,-1.48807004161827,339.689740073133));
#25819=CARTESIAN_POINT('Ctrl Pts',(15.3868456492099,-1.35616274235261,339.727579262028));
#25820=CARTESIAN_POINT('Ctrl Pts',(15.379098505904,-1.22425433757672,339.765418768051));
#25821=CARTESIAN_POINT('Ctrl Pts',(15.3713513625981,-1.09076200145517,339.797733084325));
#25822=CARTESIAN_POINT('Ctrl Pts',(15.3636042192923,-0.956188518868866,
339.824405308313));
#25823=CARTESIAN_POINT('Ctrl Pts',(15.3558553342642,-0.821584781306239,
339.851083528784));
#25824=CARTESIAN_POINT('Ctrl Pts',(15.3481064492361,-0.685899796948436,
339.872117056893));
#25825=CARTESIAN_POINT('Ctrl Pts',(15.3403575642079,-0.549645321806258,
339.887440340579));
#25826=CARTESIAN_POINT('Ctrl Pts',(15.3326004544332,-0.413246224756764,
339.902779888556));
#25827=CARTESIAN_POINT('Ctrl Pts',(15.3248433446585,-0.276276818489774,
339.912397041118));
#25828=CARTESIAN_POINT('Ctrl Pts',(15.3170862348837,-0.139253302482811,
339.916278224455));
#25829=CARTESIAN_POINT('Ctrl Pts',(15.3093249799575,-0.00215656548996285,
339.920161481771));
#25830=CARTESIAN_POINT('Ctrl Pts',(15.3015637250313,0.134993948217504,339.918302667632));
#25831=CARTESIAN_POINT('Ctrl Pts',(15.2938024701051,0.271684274281099,339.910740343126));
#25832=CARTESIAN_POINT('Ctrl Pts',(15.2860287997004,0.408593260318935,339.903165921366));
#25833=CARTESIAN_POINT('Ctrl Pts',(15.2782551292957,0.545040198430455,339.889869795199));
#25834=CARTESIAN_POINT('Ctrl Pts',(15.2704814588911,0.68051757418501,339.87094230039));
#25835=CARTESIAN_POINT('Ctrl Pts',(15.2630696547143,0.809688445497615,339.852895885019));
#25836=CARTESIAN_POINT('Ctrl Pts',(15.2556578505376,0.93797770610689,339.829730633964));
#25837=CARTESIAN_POINT('Ctrl Pts',(15.2482460463609,1.06495776327873,339.801567246736));
#25838=CARTESIAN_POINT('Ctrl Pts',(15.2404709675824,1.19816149131316,339.772023488006));
#25839=CARTESIAN_POINT('Ctrl Pts',(15.232695888804,1.33034538340358,339.736885893961));
#25840=CARTESIAN_POINT('Ctrl Pts',(15.2249208100256,1.46100335524586,339.696238096441));
#25841=CARTESIAN_POINT('Ctrl Pts',(15.2171552989766,1.59150054413552,339.655640318623));
#25842=CARTESIAN_POINT('Ctrl Pts',(15.2093897879276,1.7204751792831,339.609545943893));
#25843=CARTESIAN_POINT('Ctrl Pts',(15.2016242768786,1.84743121650202,339.558089617679));
#25844=CARTESIAN_POINT('Ctrl Pts',(15.1938664653564,1.97426137644032,339.506684310562));
#25845=CARTESIAN_POINT('Ctrl Pts',(15.1861086538342,2.09907656152283,339.449927777755));
#25846=CARTESIAN_POINT('Ctrl Pts',(15.178350842312,2.22139609692731,339.388004380474));
#25847=CARTESIAN_POINT('Ctrl Pts',(15.170598868789,2.34362358300259,339.326127582512));
#25848=CARTESIAN_POINT('Ctrl Pts',(15.162846895266,2.46335881024829,339.259091835239));
#25849=CARTESIAN_POINT('Ctrl Pts',(15.155094921743,2.58014163282769,339.187129352796));
#25850=CARTESIAN_POINT('Ctrl Pts',(15.1473462311854,2.69687499781225,339.115197346508));
#25851=CARTESIAN_POINT('Ctrl Pts',(15.1395975406278,2.81065811290241,339.03834295953));
#25852=CARTESIAN_POINT('Ctrl Pts',(15.1318488500702,2.92105617485242,338.956843929934));
#25853=CARTESIAN_POINT('Ctrl Pts',(15.1241017716924,3.03143126756373,338.875361856892));
#25854=CARTESIAN_POINT('Ctrl Pts',(15.1163546933145,3.13842239374486,338.789237295388));
#25855=CARTESIAN_POINT('Ctrl Pts',(15.1086076149367,3.24162478342162,338.69879058964));
#25856=CARTESIAN_POINT('Ctrl Pts',(15.1008604716309,3.34482803803353,338.608343125861));
#25857=CARTESIAN_POINT('Ctrl Pts',(15.0931133283251,3.44424219884817,338.513573703215));
#25858=CARTESIAN_POINT('Ctrl Pts',(15.0853661850193,3.53949687427885,338.414841861561));
#25859=CARTESIAN_POINT('Ctrl Pts',(15.0776172999912,3.63477296498288,338.316087822894));
#25860=CARTESIAN_POINT('Ctrl Pts',(15.0698684149631,3.72588743813857,338.213369873799));
#25861=CARTESIAN_POINT('Ctrl Pts',(15.062119529935,3.81250822907731,338.107082886844));
#25862=CARTESIAN_POINT('Ctrl Pts',(15.0543624201603,3.89922096021863,338.000683085782));
#25863=CARTESIAN_POINT('Ctrl Pts',(15.0466053103856,3.98143023401501,337.890706983022));
#25864=CARTESIAN_POINT('Ctrl Pts',(15.0388482006109,4.05884529080318,337.77758131615));
#25865=CARTESIAN_POINT('Ctrl Pts',(15.0310869456848,4.13630171572239,337.664395198538));
#25866=CARTESIAN_POINT('Ctrl Pts',(15.0233256907586,4.20895861191853,337.548056494595));
#25867=CARTESIAN_POINT('Ctrl Pts',(15.0155644358325,4.27657027062901,337.429018275533));
#25868=CARTESIAN_POINT('Ctrl Pts',(15.0077907654278,4.34429008595892,337.309789634114));
#25869=CARTESIAN_POINT('Ctrl Pts',(15.0000170950231,4.40694835734054,337.187853196088));
#25870=CARTESIAN_POINT('Ctrl Pts',(14.9922434246185,4.46434640486665,337.063684627033));
#25871=CARTESIAN_POINT('Ctrl Pts',(14.9848316204413,4.51907255947218,336.945296134739));
#25872=CARTESIAN_POINT('Ctrl Pts',(14.977419816264,4.56901708580637,336.824878911986));
#25873=CARTESIAN_POINT('Ctrl Pts',(14.9700080120868,4.61405008770027,336.702857848058));
#25874=CARTESIAN_POINT('Ctrl Pts',(14.9622329333085,4.66129029116216,336.574856168308));
#25875=CARTESIAN_POINT('Ctrl Pts',(14.9544578545301,4.70327462742217,336.444684945099));
#25876=CARTESIAN_POINT('Ctrl Pts',(14.9466827757517,4.739799553021,336.312815013504));
#25877=CARTESIAN_POINT('Ctrl Pts',(14.9389172647028,4.77627953237354,336.181107356256));
#25878=CARTESIAN_POINT('Ctrl Pts',(14.9311517536538,4.80731336492425,336.047705522947));
#25879=CARTESIAN_POINT('Ctrl Pts',(14.9233862426049,4.83274583891294,335.913099512085));
#25880=CARTESIAN_POINT('Ctrl Pts',(14.9156284310828,4.85815309652964,335.778626963474));
#25881=CARTESIAN_POINT('Ctrl Pts',(14.9078706195607,4.87796997578691,335.642952994933));
#25882=CARTESIAN_POINT('Ctrl Pts',(14.9001128080386,4.89209138923601,335.506581584607));
#25883=CARTESIAN_POINT('Ctrl Pts',(14.8923608345156,4.90620217587365,335.370312798092));
#25884=CARTESIAN_POINT('Ctrl Pts',(14.8846088609927,4.9146259877156,335.233348001703));
#25885=CARTESIAN_POINT('Ctrl Pts',(14.8768568874698,4.91730908727221,335.096199806289));
#25886=CARTESIAN_POINT('Ctrl Pts',(14.8691081969122,4.91999105053457,334.959109693217));
#25887=CARTESIAN_POINT('Ctrl Pts',(14.8613595063547,4.91693712935775,334.821836725585));
#25888=CARTESIAN_POINT('Ctrl Pts',(14.8536108157971,4.90814558262637,334.684896838725));
#25889=CARTESIAN_POINT('Ctrl Pts',(14.8458637374194,4.89935586504974,334.547985443353));
#25890=CARTESIAN_POINT('Ctrl Pts',(14.8381166590416,4.88483092142032,334.411407380737));
#25891=CARTESIAN_POINT('Ctrl Pts',(14.8303695806639,4.86462109176771,334.275676387221));
#25892=CARTESIAN_POINT('Ctrl Pts',(14.8226224373582,4.84441109273728,334.13994425615));
#25893=CARTESIAN_POINT('Ctrl Pts',(14.8148752940525,4.81851617021758,334.005059594951));
#25894=CARTESIAN_POINT('Ctrl Pts',(14.8071281507467,4.78703822880825,333.871528441462));
#25895=CARTESIAN_POINT('Ctrl Pts',(14.7993792657187,4.7555532104894,333.737967267335));
#25896=CARTESIAN_POINT('Ctrl Pts',(14.7916303806907,4.71848276527753,333.605760586808));
#25897=CARTESIAN_POINT('Ctrl Pts',(14.7838814956627,4.67597925069131,333.475401328348));
#25898=CARTESIAN_POINT('Ctrl Pts',(14.776124385888,4.63343062243545,333.344903705223));
#25899=CARTESIAN_POINT('Ctrl Pts',(14.7683672761133,4.58543752660682,333.216257793399));
#25900=CARTESIAN_POINT('Ctrl Pts',(14.7606101663387,4.53220146920776,333.089939031075));
#25901=CARTESIAN_POINT('Ctrl Pts',(14.7528489114126,4.47893696416181,332.963552768043));
#25902=CARTESIAN_POINT('Ctrl Pts',(14.7450876564865,4.4204240816234,332.839496485748));
#25903=CARTESIAN_POINT('Ctrl Pts',(14.7373264015604,4.35691085173058,332.718221988761));
#25904=CARTESIAN_POINT('Ctrl Pts',(14.7295527311558,4.29329602136885,332.596753492103));
#25905=CARTESIAN_POINT('Ctrl Pts',(14.7217790607513,4.22466505521,332.478076011616));
#25906=CARTESIAN_POINT('Ctrl Pts',(14.7140053903467,4.15131043348857,332.362614031411));
#25907=CARTESIAN_POINT('Ctrl Pts',(14.7065935861687,4.08137048704784,332.25252683415));
#25908=CARTESIAN_POINT('Ctrl Pts',(14.6991817819908,4.00713692445492,332.145362747655));
#25909=CARTESIAN_POINT('Ctrl Pts',(14.6917699778129,3.92889674990318,332.041460936357));
#25910=CARTESIAN_POINT('Ctrl Pts',(14.6839948990343,3.84682179133859,331.93246658779));
#25911=CARTESIAN_POINT('Ctrl Pts',(14.6762198202557,3.76007816606868,331.826717945627));
#25912=CARTESIAN_POINT('Ctrl Pts',(14.6684447414771,3.66895166030728,331.724640969782));
#25913=CARTESIAN_POINT('Ctrl Pts',(14.6606792304279,3.5779372915125,331.622689606154));
#25914=CARTESIAN_POINT('Ctrl Pts',(14.6529137193787,3.48255103139087,331.524401207683));
#25915=CARTESIAN_POINT('Ctrl Pts',(14.6451482083295,3.38312093615007,331.430171461557));
#25916=CARTESIAN_POINT('Ctrl Pts',(14.6373903968071,3.28378942613852,331.336035144498));
#25917=CARTESIAN_POINT('Ctrl Pts',(14.6296325852847,3.18042234197027,331.245949738606));
#25918=CARTESIAN_POINT('Ctrl Pts',(14.6218747737624,3.07338662077073,331.160276345651));
#25919=CARTESIAN_POINT('Ctrl Pts',(14.6141228002392,2.96643144734554,331.07466742464));
#25920=CARTESIAN_POINT('Ctrl Pts',(14.606370826716,2.85581343598871,330.993464151183));
#25921=CARTESIAN_POINT('Ctrl Pts',(14.5986188531928,2.74193457165876,330.916989117423));
#25922=CARTESIAN_POINT('Ctrl Pts',(14.5908701626351,2.62810393509546,330.840546470885));
#25923=CARTESIAN_POINT('Ctrl Pts',(14.5831214720773,2.51101551603632,330.768828298848));
#25924=CARTESIAN_POINT('Ctrl Pts',(14.5753727815195,2.39110223329226,330.702115267664));
#25925=CARTESIAN_POINT('Ctrl Pts',(14.5676257031415,2.27121389950805,330.635416116684));
#25926=CARTESIAN_POINT('Ctrl Pts',(14.5598786247635,2.1485022124451,330.573720225129));
#25927=CARTESIAN_POINT('Ctrl Pts',(14.5521315463855,2.02342642583465,330.517263273208));
#25928=CARTESIAN_POINT('Ctrl Pts',(14.5443844030795,1.89834959096864,330.460805848123));
#25929=CARTESIAN_POINT('Ctrl Pts',(14.5366372597734,1.77090897329795,330.409587611059));
#25930=CARTESIAN_POINT('Ctrl Pts',(14.5288901164674,1.64158525726161,330.363796714375));
#25931=CARTESIAN_POINT('Ctrl Pts',(14.5211412314391,1.51223246650829,330.317995522925));
#25932=CARTESIAN_POINT('Ctrl Pts',(14.5133923464109,1.38099610333606,330.277624230317));
#25933=CARTESIAN_POINT('Ctrl Pts',(14.5056434613826,1.24837313120486,330.242821467741));
#25934=CARTESIAN_POINT('Ctrl Pts',(14.4978863516077,1.11560939168097,330.207981765153));
#25935=CARTESIAN_POINT('Ctrl Pts',(14.4901292418328,0.981456481887707,330.178722498737));
#25936=CARTESIAN_POINT('Ctrl Pts',(14.4823721320579,0.846423254408913,330.155131504685));
#25937=CARTESIAN_POINT('Ctrl Pts',(14.4746108771315,0.711317869490973,330.13152790436));
#25938=CARTESIAN_POINT('Ctrl Pts',(14.4668496222053,0.575331616870021,330.113598662909));
#25939=CARTESIAN_POINT('Ctrl Pts',(14.4590883672789,0.438978651988007,330.101379703876));
#25940=CARTESIAN_POINT('Ctrl Pts',(14.4513146968741,0.302407566799698,330.08914119849));
#25941=CARTESIAN_POINT('Ctrl Pts',(14.4435410264693,0.165468987748349,330.08263124771));
#25942=CARTESIAN_POINT('Ctrl Pts',(14.4357673560644,0.0286781504160663,
330.081833611376));
#25943=CARTESIAN_POINT('Ctrl Pts',(14.4283555518893,-0.101745040491597,
330.081073105206));
#25944=CARTESIAN_POINT('Ctrl Pts',(14.4209437477141,-0.23203364726224,330.085505055417));
#25945=CARTESIAN_POINT('Ctrl Pts',(14.413531943539,-0.361747144852734,330.095071655397));
#25946=CARTESIAN_POINT('Ctrl Pts',(14.4057568647607,-0.497818287390422,
330.105107142942));
#25947=CARTESIAN_POINT('Ctrl Pts',(14.3979817859823,-0.633686529610552,
330.120825049894));
#25948=CARTESIAN_POINT('Ctrl Pts',(14.390206707204,-0.768839017416416,330.142215563881));
#25949=CARTESIAN_POINT('Ctrl Pts',(14.3824411961551,-0.903825191481438,
330.163579755479));
#25950=CARTESIAN_POINT('Ctrl Pts',(14.3746756851063,-1.03809698125641,330.19060260439));
#25951=CARTESIAN_POINT('Ctrl Pts',(14.3669101740574,-1.17114411490555,330.223222370193));
#25952=CARTESIAN_POINT('Ctrl Pts',(14.3591523625353,-1.30405933193441,330.255809793404));
#25953=CARTESIAN_POINT('Ctrl Pts',(14.3513945510132,-1.43575193207844,330.293982997491));
#25954=CARTESIAN_POINT('Ctrl Pts',(14.3436367394911,-1.56571968642209,330.337628830085));
#25955=CARTESIAN_POINT('Ctrl Pts',(14.3358847659682,-1.69558963590908,330.381241817807));
#25956=CARTESIAN_POINT('Ctrl Pts',(14.3281327924454,-1.82373695415702,330.430319112775));
#25957=CARTESIAN_POINT('Ctrl Pts',(14.3203808189225,-1.94967282942241,330.484697250382));
#25958=CARTESIAN_POINT('Ctrl Pts',(14.312632128365,-2.0755553707702,330.539052358815));
#25959=CARTESIAN_POINT('Ctrl Pts',(14.3048834378075,-2.19922797375872,330.598703690293));
#25960=CARTESIAN_POINT('Ctrl Pts',(14.29713474725,-2.32022034285369,330.66343907882));
#25961=CARTESIAN_POINT('Ctrl Pts',(14.2893876688722,-2.44118753847572,330.728160998609));
#25962=CARTESIAN_POINT('Ctrl Pts',(14.2816405904945,-2.55947526497103,330.797964687164));
#25963=CARTESIAN_POINT('Ctrl Pts',(14.2738935121168,-2.67463680527738,330.872591488312));
#25964=CARTESIAN_POINT('Ctrl Pts',(14.2661463688111,-2.78979931074804,330.947218914903));
#25965=CARTESIAN_POINT('Ctrl Pts',(14.2583992255054,-2.90183524974824,331.026669322147));
#25966=CARTESIAN_POINT('Ctrl Pts',(14.2506520821997,-3.01032627501437,331.11064031228));
#25967=CARTESIAN_POINT('Ctrl Pts',(14.2429031971717,-3.11884169136691,331.194630180875));
#25968=CARTESIAN_POINT('Ctrl Pts',(14.2351543121436,-3.22381029905678,331.283142415532));
#25969=CARTESIAN_POINT('Ctrl Pts',(14.2274054271156,-3.32484658471488,331.375834130367));
#25970=CARTESIAN_POINT('Ctrl Pts',(14.219648317341,-3.42599011133021,331.468624229146));
#25971=CARTESIAN_POINT('Ctrl Pts',(14.2118912075664,-3.52319268985944,331.565602405058));
#25972=CARTESIAN_POINT('Ctrl Pts',(14.2041340977918,-3.61610508764279,331.666388286314));
#25973=CARTESIAN_POINT('Ctrl Pts',(14.1963728428657,-3.70906713484093,331.767228024323));
#25974=CARTESIAN_POINT('Ctrl Pts',(14.1886115879396,-3.79773418066319,331.871879223957));
#25975=CARTESIAN_POINT('Ctrl Pts',(14.1808503330135,-3.8817977772239,331.979928961226));
#25976=CARTESIAN_POINT('Ctrl Pts',(14.1730766626089,-3.96599584814273,332.088151542862));
#25977=CARTESIAN_POINT('Ctrl Pts',(14.1653029922044,-4.04557552729667,332.199783207529));
#25978=CARTESIAN_POINT('Ctrl Pts',(14.1575293217998,-4.12027164784493,332.314381894151));
#25979=CARTESIAN_POINT('Ctrl Pts',(14.1501175176215,-4.19149064602285,332.423645984358));
#25980=CARTESIAN_POINT('Ctrl Pts',(14.1427057134433,-4.25827036565018,332.535606835987));
#25981=CARTESIAN_POINT('Ctrl Pts',(14.135293909265,-4.3204210241634,332.649862719655));
#25982=CARTESIAN_POINT('Ctrl Pts',(14.1271138568986,-4.38901372157135,332.775961452041));
#25983=CARTESIAN_POINT('Ctrl Pts',(14.1189338045322,-4.45216623723888,332.905220028662));
#25984=CARTESIAN_POINT('Ctrl Pts',(14.1107537521658,-4.50959184349229,333.0371539878));
#25985=CARTESIAN_POINT('Ctrl Pts',(14.102587857685,-4.56691805855238,333.168859598045));
#25986=CARTESIAN_POINT('Ctrl Pts',(14.0944219632042,-4.61853698427458,333.303231061453));
#25987=CARTESIAN_POINT('Ctrl Pts',(14.0862560687234,-4.66420741630333,333.439758916));
#25988=CARTESIAN_POINT('Ctrl Pts',(14.0781089270173,-4.70977296731469,333.575973237706));
#25989=CARTESIAN_POINT('Ctrl Pts',(14.0699617853112,-4.7494171610063,333.7143337624));
#25990=CARTESIAN_POINT('Ctrl Pts',(14.0618146436051,-4.78294686407446,333.854311404464));
#25991=CARTESIAN_POINT('Ctrl Pts',(14.0536786667445,-4.81643061802757,333.994097221127));
#25992=CARTESIAN_POINT('Ctrl Pts',(14.0455426898837,-4.84381649802361,334.13549541966));
#25993=CARTESIAN_POINT('Ctrl Pts',(14.037406713023,-4.86496063921135,334.277960498709));
#25994=CARTESIAN_POINT('Ctrl Pts',(14.0292854251914,-4.88606660589207,334.420168365413));
#25995=CARTESIAN_POINT('Ctrl Pts',(14.02116413736,-4.90095325625342,334.563438945091));
#25996=CARTESIAN_POINT('Ctrl Pts',(14.0130428495284,-4.90952752261186,334.707215835099));
#25997=CARTESIAN_POINT('Ctrl Pts',(14.0075406492106,-4.91533661743288,334.804625170454));
#25998=CARTESIAN_POINT('Ctrl Pts',(14.0020384488928,-4.91824929826728,334.902266623046));
#25999=CARTESIAN_POINT('Ctrl Pts',(13.996536248575,-4.91824999987318,334.999964680227));
#26000=CARTESIAN_POINT('',(17.4965362485264,-4.91824945026714,335.002325391798));
#26001=CARTESIAN_POINT('Ctrl Pts',(17.4965362484902,-4.91824945026684,335.002325392432));
#26002=CARTESIAN_POINT('Ctrl Pts',(17.4890742725109,-4.91818747571447,335.133402755509));
#26003=CARTESIAN_POINT('Ctrl Pts',(17.4816122965316,-4.91288593130427,335.264351668712));
#26004=CARTESIAN_POINT('Ctrl Pts',(17.4741503205523,-4.90237255421105,335.394875172957));
#26005=CARTESIAN_POINT('Ctrl Pts',(17.4663752417739,-4.89141803822839,335.530875413479));
#26006=CARTESIAN_POINT('Ctrl Pts',(17.4586001629954,-4.87478260324696,335.666634369524));
#26007=CARTESIAN_POINT('Ctrl Pts',(17.450825084217,-4.85247952611126,335.801639264988));
#26008=CARTESIAN_POINT('Ctrl Pts',(17.443059573168,-4.83020389433186,335.936478028334));
#26009=CARTESIAN_POINT('Ctrl Pts',(17.435294062119,-4.80227456054411,336.070564195434));
#26010=CARTESIAN_POINT('Ctrl Pts',(17.4275285510699,-4.76875671101047,336.203387923195));
#26011=CARTESIAN_POINT('Ctrl Pts',(17.4197707395477,-4.73527209452216,336.336079955845));
#26012=CARTESIAN_POINT('Ctrl Pts',(17.4120129280255,-4.6962100842725,336.467511663582));
#26013=CARTESIAN_POINT('Ctrl Pts',(17.4042551165033,-4.65168722296251,336.597181593379));
#26014=CARTESIAN_POINT('Ctrl Pts',(17.3965031429803,-4.60719786651756,336.726753942441));
#26015=CARTESIAN_POINT('Ctrl Pts',(17.3887511694572,-4.55725596512239,336.854566784288));
#26016=CARTESIAN_POINT('Ctrl Pts',(17.3809991959342,-4.5020282819259,336.980132422652));
#26017=CARTESIAN_POINT('Ctrl Pts',(17.3732505053766,-4.44682398768617,337.105644883894));
#26018=CARTESIAN_POINT('Ctrl Pts',(17.3655018148189,-4.38633852096908,337.228911677449));
#26019=CARTESIAN_POINT('Ctrl Pts',(17.3577531242613,-4.32078722010939,337.349463951849));
#26020=CARTESIAN_POINT('Ctrl Pts',(17.3500060458835,-4.25524955774524,337.469991144342));
#26021=CARTESIAN_POINT('Ctrl Pts',(17.3422589675056,-4.18464834430203,337.587804597887));
#26022=CARTESIAN_POINT('Ctrl Pts',(17.3345118891278,-4.10924524794454,337.702459353024));
#26023=CARTESIAN_POINT('Ctrl Pts',(17.3267647458219,-4.03384151963658,337.817115069077));
#26024=CARTESIAN_POINT('Ctrl Pts',(17.3190176025161,-3.95363604291983,337.928611707341));
#26025=CARTESIAN_POINT('Ctrl Pts',(17.3112704592103,-3.86893403488975,338.036532973009));
#26026=CARTESIAN_POINT('Ctrl Pts',(17.3035215741822,-3.78421298404988,338.144478501669));
#26027=CARTESIAN_POINT('Ctrl Pts',(17.2957726891541,-3.69499363156641,338.248846750803));
#26028=CARTESIAN_POINT('Ctrl Pts',(17.2880238041259,-3.60162145991608,338.349254532276));
#26029=CARTESIAN_POINT('Ctrl Pts',(17.2802666943512,-3.50815018207818,338.449768887606));
#26030=CARTESIAN_POINT('Ctrl Pts',(17.2725095845765,-3.41051754658914,338.546314091339));
#26031=CARTESIAN_POINT('Ctrl Pts',(17.2647524748018,-3.3091062758736,338.638543488468));
#26032=CARTESIAN_POINT('Ctrl Pts',(17.2569912198756,-3.20764081421757,338.730822170038));
#26033=CARTESIAN_POINT('Ctrl Pts',(17.2492299649494,-3.10239299370636,338.818780199107));
#26034=CARTESIAN_POINT('Ctrl Pts',(17.2414687100232,-2.99377781269178,338.902111924424));
#26035=CARTESIAN_POINT('Ctrl Pts',(17.2336950396186,-2.88498888278518,338.985576953344));
#26036=CARTESIAN_POINT('Ctrl Pts',(17.2259213692139,-2.77282214816773,339.064400665108));
#26037=CARTESIAN_POINT('Ctrl Pts',(17.2181476988092,-2.65772145121774,339.138320885364));
#26038=CARTESIAN_POINT('Ctrl Pts',(17.2107358946323,-2.54797871940428,339.208800101581));
#26039=CARTESIAN_POINT('Ctrl Pts',(17.2033240904553,-2.43556927819767,339.27482192201));
#26040=CARTESIAN_POINT('Ctrl Pts',(17.1959122862783,-2.32089612992976,339.336199282387));
#26041=CARTESIAN_POINT('Ctrl Pts',(17.1881372074999,-2.20060250906958,339.400584930031));
#26042=CARTESIAN_POINT('Ctrl Pts',(17.1803621287215,-2.07743751823178,339.460062798817));
#26043=CARTESIAN_POINT('Ctrl Pts',(17.172587049943,-1.95183954664401,339.514366560954));
#26044=CARTESIAN_POINT('Ctrl Pts',(17.164821538894,-1.82639613135625,339.568603498854));
#26045=CARTESIAN_POINT('Ctrl Pts',(17.157056027845,-1.69852604774229,339.617678845105));
#26046=CARTESIAN_POINT('Ctrl Pts',(17.149290516796,-1.56869330976127,339.661371510876));
#26047=CARTESIAN_POINT('Ctrl Pts',(17.1415327052739,-1.43898930131803,339.705020855242));
#26048=CARTESIAN_POINT('Ctrl Pts',(17.1337748937516,-1.30732687918569,339.743298016078));
#26049=CARTESIAN_POINT('Ctrl Pts',(17.1260170822294,-1.17419079385777,339.776029631621));
#26050=CARTESIAN_POINT('Ctrl Pts',(17.1182651087064,-1.04115489765623,339.808736615585));
#26051=CARTESIAN_POINT('Ctrl Pts',(17.1105131351835,-0.906647923669278,
339.835906267861));
#26052=CARTESIAN_POINT('Ctrl Pts',(17.1027611616605,-0.771170231202778,
339.857414902704));
#26053=CARTESIAN_POINT('Ctrl Pts',(17.0950124711029,-0.63574991361947,339.878914428627));
#26054=CARTESIAN_POINT('Ctrl Pts',(17.0872637805453,-0.499360080441308,
339.894757644304));
#26055=CARTESIAN_POINT('Ctrl Pts',(17.0795150899877,-0.362511530800745,
339.904871909901));
#26056=CARTESIAN_POINT('Ctrl Pts',(17.0717680116099,-0.22569145364373,339.914984071141));
#26057=CARTESIAN_POINT('Ctrl Pts',(17.0640209332321,-0.088413239427148,
339.919369624394));
#26058=CARTESIAN_POINT('Ctrl Pts',(17.0562738548543,0.0488073322865175,
339.918007818905));
#26059=CARTESIAN_POINT('Ctrl Pts',(17.0485267115485,0.186029054040741,339.916646002004));
#26060=CARTESIAN_POINT('Ctrl Pts',(17.0407795682426,0.323192741473425,339.909536734164));
#26061=CARTESIAN_POINT('Ctrl Pts',(17.0330324249368,0.459783152918351,339.896711397948));
#26062=CARTESIAN_POINT('Ctrl Pts',(17.0252835399088,0.596404272787481,339.883883178324));
#26063=CARTESIAN_POINT('Ctrl Pts',(17.0175346548807,0.732451471116397,339.865336369664));
#26064=CARTESIAN_POINT('Ctrl Pts',(17.0097857698526,0.867415556436818,339.841154130468));
#26065=CARTESIAN_POINT('Ctrl Pts',(17.0020286600779,1.00252289403202,339.816946223994));
#26066=CARTESIAN_POINT('Ctrl Pts',(16.9942715503032,1.13654443677542,339.787091007413));
#26067=CARTESIAN_POINT('Ctrl Pts',(16.9865144405285,1.26898156201064,339.751722725263));
#26068=CARTESIAN_POINT('Ctrl Pts',(16.9787531856023,1.40148945741097,339.716335543433));
#26069=CARTESIAN_POINT('Ctrl Pts',(16.9709919306761,1.53241087535465,339.675429542361));
#26070=CARTESIAN_POINT('Ctrl Pts',(16.96323067575,1.66126420776291,339.629188297586));
#26071=CARTESIAN_POINT('Ctrl Pts',(16.9554570053454,1.79032366350981,339.582873081889));
#26072=CARTESIAN_POINT('Ctrl Pts',(16.9476833349407,1.9173080605895,339.531205715116));
#26073=CARTESIAN_POINT('Ctrl Pts',(16.9399096645361,2.04175674241726,339.474417556207));
#26074=CARTESIAN_POINT('Ctrl Pts',(16.9324978603589,2.16041230816699,339.420272899757));
#26075=CARTESIAN_POINT('Ctrl Pts',(16.9250860561817,2.27676266417264,339.36147359786));
#26076=CARTESIAN_POINT('Ctrl Pts',(16.9176742520045,2.39043241641722,339.298257312568));
#26077=CARTESIAN_POINT('Ctrl Pts',(16.9098991732261,2.50967346182275,339.231942608822));
#26078=CARTESIAN_POINT('Ctrl Pts',(16.9021240944476,2.62634131433764,339.160557428056));
#26079=CARTESIAN_POINT('Ctrl Pts',(16.8943490156691,2.73997477567468,339.084326295874));
#26080=CARTESIAN_POINT('Ctrl Pts',(16.8865835046201,2.85346840380328,339.008188970953));
#26081=CARTESIAN_POINT('Ctrl Pts',(16.8788179935711,2.96393474887053,338.927217775453));
#26082=CARTESIAN_POINT('Ctrl Pts',(16.8710524825221,3.0709367879821,338.841683264758));
#26083=CARTESIAN_POINT('Ctrl Pts',(16.8632946709999,3.17783273426029,338.756233561779));
#26084=CARTESIAN_POINT('Ctrl Pts',(16.8555368594777,3.28127090681902,338.666229790184));
#26085=CARTESIAN_POINT('Ctrl Pts',(16.8477790479555,3.38084319574525,338.571985771008));
#26086=CARTESIAN_POINT('Ctrl Pts',(16.8400270744324,3.48034055336644,338.477812673445));
#26087=CARTESIAN_POINT('Ctrl Pts',(16.8322751009094,3.57597753523768,338.379405947279));
#26088=CARTESIAN_POINT('Ctrl Pts',(16.8245231273864,3.6673793582458,338.277119421872));
#26089=CARTESIAN_POINT('Ctrl Pts',(16.8167744368288,3.75874247252761,338.17487621487));
#26090=CARTESIAN_POINT('Ctrl Pts',(16.8090257462711,3.84587373537039,338.068756767487));
#26091=CARTESIAN_POINT('Ctrl Pts',(16.8012770557135,3.92843563966845,337.959151312029));
#26092=CARTESIAN_POINT('Ctrl Pts',(16.7935299773357,4.01098036627276,337.849568660902));
#26093=CARTESIAN_POINT('Ctrl Pts',(16.7857828989578,4.08895739029967,337.736501756372));
#26094=CARTESIAN_POINT('Ctrl Pts',(16.77803582058,4.16207014408058,337.620373099055));
#26095=CARTESIAN_POINT('Ctrl Pts',(16.7702886772742,4.2351835106167,337.504243468468));
#26096=CARTESIAN_POINT('Ctrl Pts',(16.7625415339684,4.30343231734124,337.385052364689));
#26097=CARTESIAN_POINT('Ctrl Pts',(16.7547943906626,4.36656412768936,337.263250048332));
#26098=CARTESIAN_POINT('Ctrl Pts',(16.7470455056345,4.42971013140886,337.141420348228));
#26099=CARTESIAN_POINT('Ctrl Pts',(16.7392966206063,4.48773666973072,337.016978614332));
#26100=CARTESIAN_POINT('Ctrl Pts',(16.7315477355782,4.5404381196899,336.890398038448));
#26101=CARTESIAN_POINT('Ctrl Pts',(16.7237906258035,4.59319550751257,336.763683108632));
#26102=CARTESIAN_POINT('Ctrl Pts',(16.7160335160287,4.64061636588967,336.634825163331));
#26103=CARTESIAN_POINT('Ctrl Pts',(16.708276406254,4.68254375058519,336.504316152395));
#26104=CARTESIAN_POINT('Ctrl Pts',(16.7005151513278,4.72449353993449,336.373737401616));
#26105=CARTESIAN_POINT('Ctrl Pts',(16.6927538964016,4.76094390246089,336.241506203815));
#26106=CARTESIAN_POINT('Ctrl Pts',(16.6849926414754,4.791788584984,336.108126896757));
#26107=CARTESIAN_POINT('Ctrl Pts',(16.6772189710708,4.8226826089469,335.974534226276));
#26108=CARTESIAN_POINT('Ctrl Pts',(16.6694453006661,4.84795296157558,335.839790160845));
#26109=CARTESIAN_POINT('Ctrl Pts',(16.6616716302614,4.86754490982744,335.70440727801));
#26110=CARTESIAN_POINT('Ctrl Pts',(16.6542598260844,4.88622484817441,335.575326500943));
#26111=CARTESIAN_POINT('Ctrl Pts',(16.6468480219074,4.89974311459746,335.445665328196));
#26112=CARTESIAN_POINT('Ctrl Pts',(16.6394362177304,4.90809641694306,335.315868049177));
#26113=CARTESIAN_POINT('Ctrl Pts',(16.631661138952,4.91685913951992,335.179709018866));
#26114=CARTESIAN_POINT('Ctrl Pts',(16.6238860601735,4.91996548747335,335.042969915293));
#26115=CARTESIAN_POINT('Ctrl Pts',(16.6161109813951,4.9173546883175,334.906160073626));
#26116=CARTESIAN_POINT('Ctrl Pts',(16.6083454703461,4.91474710191623,334.769518585179));
#26117=CARTESIAN_POINT('Ctrl Pts',(16.600579959297,4.90643637404882,334.632806918904));
#26118=CARTESIAN_POINT('Ctrl Pts',(16.592814448248,4.89241352234543,334.496538989721));
#26119=CARTESIAN_POINT('Ctrl Pts',(16.5850566367258,4.87840457434035,334.360406170586));
#26120=CARTESIAN_POINT('Ctrl Pts',(16.5772988252036,4.85869481311291,334.224716599299));
#26121=CARTESIAN_POINT('Ctrl Pts',(16.5695410136814,4.83332728577409,334.089983290762));
#26122=CARTESIAN_POINT('Ctrl Pts',(16.5617890401584,4.80797884830404,333.955351373313));
#26123=CARTESIAN_POINT('Ctrl Pts',(16.5540370666353,4.77698119139533,333.821674668827));
#26124=CARTESIAN_POINT('Ctrl Pts',(16.5462850931123,4.74042904105868,333.68945981779));
#26125=CARTESIAN_POINT('Ctrl Pts',(16.5385364025547,4.70389237057945,333.557300959821));
#26126=CARTESIAN_POINT('Ctrl Pts',(16.5307877119971,4.66180598923088,333.426603099921));
#26127=CARTESIAN_POINT('Ctrl Pts',(16.5230390214394,4.61431540722336,333.297861232108));
#26128=CARTESIAN_POINT('Ctrl Pts',(16.5152919430616,4.56683470602801,333.169146150116));
#26129=CARTESIAN_POINT('Ctrl Pts',(16.5075448646838,4.51395217585439,333.042386617226));
#26130=CARTESIAN_POINT('Ctrl Pts',(16.4997977863059,4.45586261669995,332.918060662844));
#26131=CARTESIAN_POINT('Ctrl Pts',(16.4920506430001,4.39777257069912,332.793733666492));
#26132=CARTESIAN_POINT('Ctrl Pts',(16.4843034996943,4.33447557413499,332.671840643454));
#26133=CARTESIAN_POINT('Ctrl Pts',(16.4765563563885,4.26621365285367,332.552837534877));
#26134=CARTESIAN_POINT('Ctrl Pts',(16.4688074713604,4.19793638484321,332.433807671876));
#26135=CARTESIAN_POINT('Ctrl Pts',(16.4610585863323,4.12469216540993,332.317669355183));
#26136=CARTESIAN_POINT('Ctrl Pts',(16.4533097013042,4.04676763725206,332.204851568773));
#26137=CARTESIAN_POINT('Ctrl Pts',(16.4455525915295,3.96876039919489,332.091914036399));
#26138=CARTESIAN_POINT('Ctrl Pts',(16.4377954817547,3.88606315140357,331.982304396841));
#26139=CARTESIAN_POINT('Ctrl Pts',(16.43003837198,3.79900465347133,331.876420850146));
#26140=CARTESIAN_POINT('Ctrl Pts',(16.4222771170538,3.71189963426132,331.770480722669));
#26141=CARTESIAN_POINT('Ctrl Pts',(16.4145158621276,3.62042898168615,331.668270946632));
#26142=CARTESIAN_POINT('Ctrl Pts',(16.4067546072014,3.52495930443916,331.570153798704));
#26143=CARTESIAN_POINT('Ctrl Pts',(16.3989809367968,3.42933690682208,331.471879695315));
#26144=CARTESIAN_POINT('Ctrl Pts',(16.3912072663921,3.32970298538194,331.377711571252));
#26145=CARTESIAN_POINT('Ctrl Pts',(16.3834335959875,3.22645895832361,331.287972837821));
#26146=CARTESIAN_POINT('Ctrl Pts',(16.3760217918105,3.1280209655656,331.202411464023));
#26147=CARTESIAN_POINT('Ctrl Pts',(16.3686099876335,3.02630162884219,331.120876564858));
#26148=CARTESIAN_POINT('Ctrl Pts',(16.3611981834565,2.92167277902398,331.043611339263));
#26149=CARTESIAN_POINT('Ctrl Pts',(16.3534231046781,2.81191575760143,330.962559114799));
#26150=CARTESIAN_POINT('Ctrl Pts',(16.3456480258997,2.69860995132663,330.885949545503));
#26151=CARTESIAN_POINT('Ctrl Pts',(16.3378729471213,2.58215078352836,330.814109366739));
#26152=CARTESIAN_POINT('Ctrl Pts',(16.3301074360723,2.46583492615005,330.742357591888));
#26153=CARTESIAN_POINT('Ctrl Pts',(16.3223419250233,2.3463737576461,330.675363733119));
#26154=CARTESIAN_POINT('Ctrl Pts',(16.3145764139743,2.22419457915933,330.613413452747));
#26155=CARTESIAN_POINT('Ctrl Pts',(16.3068186024521,2.102136541684,330.551524596259));
#26156=CARTESIAN_POINT('Ctrl Pts',(16.2990607909299,1.97736620363373,330.494669542076));
#26157=CARTESIAN_POINT('Ctrl Pts',(16.2913029794077,1.85033826544513,330.443089712763));
#26158=CARTESIAN_POINT('Ctrl Pts',(16.2835510058847,1.7234059198083,330.391548698907));
#26159=CARTESIAN_POINT('Ctrl Pts',(16.2757990323618,1.59421971634065,330.345275154742));
#26160=CARTESIAN_POINT('Ctrl Pts',(16.2680470588388,1.46325696151485,330.304463595384));
#26161=CARTESIAN_POINT('Ctrl Pts',(16.2602983682811,1.33234966949331,330.263669319744));
#26162=CARTESIAN_POINT('Ctrl Pts',(16.2525496777236,1.1996676949233,330.22833254426));
#26163=CARTESIAN_POINT('Ctrl Pts',(16.2448009871659,1.06570603275893,330.198598775957));
#26164=CARTESIAN_POINT('Ctrl Pts',(16.2370539087881,0.931772242437241,330.168871194013));
#26165=CARTESIAN_POINT('Ctrl Pts',(16.2293068304103,0.796559675458909,330.144744385128));
#26166=CARTESIAN_POINT('Ctrl Pts',(16.2215597520325,0.660575734404991,330.126313226969));
#26167=CARTESIAN_POINT('Ctrl Pts',(16.2138126087267,0.524590653674855,330.10788191434));
#26168=CARTESIAN_POINT('Ctrl Pts',(16.2060654654209,0.387834573307152,330.095146400147));
#26169=CARTESIAN_POINT('Ctrl Pts',(16.1983183221151,0.25082187801229,330.088149895609));
#26170=CARTESIAN_POINT('Ctrl Pts',(16.190569437087,0.113778379354477,330.081151818108));
#26171=CARTESIAN_POINT('Ctrl Pts',(16.1828205520589,-0.0235214587427138,
330.079895337648));
#26172=CARTESIAN_POINT('Ctrl Pts',(16.1750716670308,-0.160561775691114,
330.084371558113));
#26173=CARTESIAN_POINT('Ctrl Pts',(16.1673145572561,-0.297747548647628,
330.088852529685));
#26174=CARTESIAN_POINT('Ctrl Pts',(16.1595574474814,-0.434672858918308,
330.099078344256));
#26175=CARTESIAN_POINT('Ctrl Pts',(16.1518003377067,-0.570824940906885,
330.114988029765));
#26176=CARTESIAN_POINT('Ctrl Pts',(16.1440390827805,-0.70704977821487,330.130906216902));
#26177=CARTESIAN_POINT('Ctrl Pts',(16.1362778278544,-0.842500178127734,
330.152514265483));
#26178=CARTESIAN_POINT('Ctrl Pts',(16.1285165729282,-0.976673101465136,
330.179699935131));
#26179=CARTESIAN_POINT('Ctrl Pts',(16.1207429025236,-1.11106065775302,330.206929092991));
#26180=CARTESIAN_POINT('Ctrl Pts',(16.1129692321189,-1.24416627415039,330.23975360783));
#26181=CARTESIAN_POINT('Ctrl Pts',(16.1051955617142,-1.3755007567666,330.278010934931));
#26182=CARTESIAN_POINT('Ctrl Pts',(16.097783757537,-1.50072158762172,330.314487374251));
#26183=CARTESIAN_POINT('Ctrl Pts',(16.0903719533599,-1.62433219355919,330.35590212218));
#26184=CARTESIAN_POINT('Ctrl Pts',(16.0829601491827,-1.74592684438599,330.402074107105));
#26185=CARTESIAN_POINT('Ctrl Pts',(16.0751850704042,-1.87348121125986,330.45050911855));
#26186=CARTESIAN_POINT('Ctrl Pts',(16.0674099916258,-1.99922010573587,330.504332554518));
#26187=CARTESIAN_POINT('Ctrl Pts',(16.0596349128473,-2.12265478282301,330.563388710349));
#26188=CARTESIAN_POINT('Ctrl Pts',(16.0518694017983,-2.24593756568176,330.622372193821));
#26189=CARTESIAN_POINT('Ctrl Pts',(16.0441038907493,-2.36692142373041,330.686575417921));
#26190=CARTESIAN_POINT('Ctrl Pts',(16.0363383797003,-2.48513490026524,330.755793644274));
#26191=CARTESIAN_POINT('Ctrl Pts',(16.0285805681781,-2.60323116779383,330.824943240554));
#26192=CARTESIAN_POINT('Ctrl Pts',(16.0208227566559,-2.71856218504585,330.899097747518));
#26193=CARTESIAN_POINT('Ctrl Pts',(16.0130649451337,-2.83067887013833,330.978005445472));
#26194=CARTESIAN_POINT('Ctrl Pts',(16.0053129716106,-2.94271118387001,331.056853762881));
#26195=CARTESIAN_POINT('Ctrl Pts',(15.9975609980876,-3.05153366176024,331.140447927522));
#26196=CARTESIAN_POINT('Ctrl Pts',(15.9898090245646,-3.15672443397928,331.228491825487));
#26197=CARTESIAN_POINT('Ctrl Pts',(15.982060334007,-3.26187065784369,331.316498436809));
#26198=CARTESIAN_POINT('Ctrl Pts',(15.9743116434494,-3.36338793595524,331.408950783033));
#26199=CARTESIAN_POINT('Ctrl Pts',(15.9665629528917,-3.46088603817935,331.505511354542));
#26200=CARTESIAN_POINT('Ctrl Pts',(15.9588158745139,-3.55836385510897,331.602051835817));
#26201=CARTESIAN_POINT('Ctrl Pts',(15.951068796136,-3.65182388191053,331.70269856734));
#26202=CARTESIAN_POINT('Ctrl Pts',(15.9433217177582,-3.74091174927873,331.807076207203));
#26203=CARTESIAN_POINT('Ctrl Pts',(15.9355745744524,-3.83000036328894,331.911454721852));
#26204=CARTESIAN_POINT('Ctrl Pts',(15.9278274311466,-3.91471649102352,332.019563909902));
#26205=CARTESIAN_POINT('Ctrl Pts',(15.9200802878408,-3.99474543216421,332.130994598349));
#26206=CARTESIAN_POINT('Ctrl Pts',(15.9123314028127,-4.07479236550982,332.24245033878));
#26207=CARTESIAN_POINT('Ctrl Pts',(15.9045825177846,-4.15014978739144,332.357228748126));
#26208=CARTESIAN_POINT('Ctrl Pts',(15.8968336327565,-4.22054601697861,332.474891214014));
#26209=CARTESIAN_POINT('Ctrl Pts',(15.8890765229818,-4.29101696585138,332.592678568059));
#26210=CARTESIAN_POINT('Ctrl Pts',(15.8813194132071,-4.35651600238068,332.713355757661));
#26211=CARTESIAN_POINT('Ctrl Pts',(15.8735623034324,-4.4168169123865,332.836458591809));
#26212=CARTESIAN_POINT('Ctrl Pts',(15.8658010485062,-4.47715004527053,332.959627208176));
#26213=CARTESIAN_POINT('Ctrl Pts',(15.85803979358,-4.53227935976597,333.085223694128));
#26214=CARTESIAN_POINT('Ctrl Pts',(15.8502785386539,-4.58202701783645,333.212764293576));
#26215=CARTESIAN_POINT('Ctrl Pts',(15.8425048682492,-4.63185425594712,333.340508916418));
#26216=CARTESIAN_POINT('Ctrl Pts',(15.8347311978446,-4.67628250776983,333.47020349738));
#26217=CARTESIAN_POINT('Ctrl Pts',(15.8269575274399,-4.71518372974108,333.60134870061));
#26218=CARTESIAN_POINT('Ctrl Pts',(15.8195457232628,-4.75227409047033,333.726389063077));
#26219=CARTESIAN_POINT('Ctrl Pts',(15.8121339190857,-4.78434033703889,333.852747755207));
#26220=CARTESIAN_POINT('Ctrl Pts',(15.8047221149087,-4.81131517254095,333.979985601583));
#26221=CARTESIAN_POINT('Ctrl Pts',(15.7938135927537,-4.85101611224083,334.167251324341));
#26222=CARTESIAN_POINT('Ctrl Pts',(15.7829050705987,-4.87979520388835,334.356906926838));
#26223=CARTESIAN_POINT('Ctrl Pts',(15.7719965484437,-4.89742617354449,334.547893887255));
#26224=CARTESIAN_POINT('Ctrl Pts',(15.7635097817925,-4.91114296516664,334.696480629203));
#26225=CARTESIAN_POINT('Ctrl Pts',(15.7550230151414,-4.91811289450606,334.845873039927));
#26226=CARTESIAN_POINT('Ctrl Pts',(15.7465362484902,-4.91824799676507,334.99556098926));
#26227=CARTESIAN_POINT('',(19.2465362484902,-4.91524060940954,335.003192664787));
#26228=CARTESIAN_POINT('Ctrl Pts',(19.2465362484902,-4.91824896247744,335.003194618845));
#26229=CARTESIAN_POINT('Ctrl Pts',(19.2377820254298,-4.91814815424287,335.158393100778));
#26230=CARTESIAN_POINT('Ctrl Pts',(19.2290278023693,-4.91069724366754,335.313310701779));
#26231=CARTESIAN_POINT('Ctrl Pts',(19.2202735793088,-4.8960000081695,335.467297531027));
#26232=CARTESIAN_POINT('Ctrl Pts',(19.2114841097102,-4.88124359818296,335.621904347066));
#26233=CARTESIAN_POINT('Ctrl Pts',(19.2026946401115,-4.85918250561117,335.775572701174));
#26234=CARTESIAN_POINT('Ctrl Pts',(19.1939051705129,-4.82997157456934,335.927662466284));
#26235=CARTESIAN_POINT('Ctrl Pts',(19.1850664219562,-4.80059686979468,336.080604936449));
#26236=CARTESIAN_POINT('Ctrl Pts',(19.1762276733995,-4.76399202541037,336.231950888511));
#26237=CARTESIAN_POINT('Ctrl Pts',(19.1673889248429,-4.72036323075361,336.381069886809));
#26238=CARTESIAN_POINT('Ctrl Pts',(19.1594521252939,-4.68118653107344,336.514972055293));
#26239=CARTESIAN_POINT('Ctrl Pts',(19.1515153257449,-4.63634695919046,336.647078772111));
#26240=CARTESIAN_POINT('Ctrl Pts',(19.1435785261959,-4.58602598893983,336.776949265249));
#26241=CARTESIAN_POINT('Ctrl Pts',(19.1358034474176,-4.53673036222163,336.904173508333));
#26242=CARTESIAN_POINT('Ctrl Pts',(19.1280283686392,-4.48205869875328,337.029545917805));
#26243=CARTESIAN_POINT('Ctrl Pts',(19.1202532898608,-4.42217000146141,337.152578811722));
#26244=CARTESIAN_POINT('Ctrl Pts',(19.1124877788118,-4.36235500102435,337.27546030583));
#26245=CARTESIAN_POINT('Ctrl Pts',(19.1047222677628,-4.29733590994779,337.396007664526));
#26246=CARTESIAN_POINT('Ctrl Pts',(19.0969567567139,-4.2273206469613,337.513750825017));
#26247=CARTESIAN_POINT('Ctrl Pts',(19.0891989451918,-4.15737480431186,337.631377242822));
#26248=CARTESIAN_POINT('Ctrl Pts',(19.0814411336696,-4.08244284642495,337.746204661719));
#26249=CARTESIAN_POINT('Ctrl Pts',(19.0736833221475,-4.00277952111879,337.857785710618));
#26250=CARTESIAN_POINT('Ctrl Pts',(19.0659313486245,-3.92317614499119,337.969282791239));
#26251=CARTESIAN_POINT('Ctrl Pts',(19.0581793751016,-3.83884871465946,338.077538047691));
#26252=CARTESIAN_POINT('Ctrl Pts',(19.0504274015786,-3.75009618730341,338.182131620231));
#26253=CARTESIAN_POINT('Ctrl Pts',(19.042678711021,-3.66138124669539,338.28668089733));
#26254=CARTESIAN_POINT('Ctrl Pts',(19.0349300204635,-3.56824518875034,338.387571277386));
#26255=CARTESIAN_POINT('Ctrl Pts',(19.0271813299059,-3.47102815166506,338.484414819284));
#26256=CARTESIAN_POINT('Ctrl Pts',(19.0194342515281,-3.37383134139633,338.581238212076));
#26257=CARTESIAN_POINT('Ctrl Pts',(19.0116871731503,-3.27255551761854,338.674016165781));
#26258=CARTESIAN_POINT('Ctrl Pts',(19.0039400947726,-3.16757840768925,338.762396854884));
#26259=CARTESIAN_POINT('Ctrl Pts',(18.9961929514668,-3.06260041795096,338.850778284702));
#26260=CARTESIAN_POINT('Ctrl Pts',(18.9884458081611,-2.95392137920249,338.93476212467));
#26261=CARTESIAN_POINT('Ctrl Pts',(18.9806986648553,-2.84195258113796,339.014036445906));
#26262=CARTESIAN_POINT('Ctrl Pts',(18.9729497798273,-2.7299586101103,339.093328589693));
#26263=CARTESIAN_POINT('Ctrl Pts',(18.9652008947991,-2.61467372698004,339.167908882037));
#26264=CARTESIAN_POINT('Ctrl Pts',(18.9574520097711,-2.49653836950835,339.237508611445));
#26265=CARTESIAN_POINT('Ctrl Pts',(18.9496948999964,-2.37827762194752,339.307182214726));
#26266=CARTESIAN_POINT('Ctrl Pts',(18.9419377902218,-2.25716069358419,339.371864496226));
#26267=CARTESIAN_POINT('Ctrl Pts',(18.9341806804471,-2.13365329307323,339.431332382868));
#26268=CARTESIAN_POINT('Ctrl Pts',(18.926419425521,-2.01007989415652,339.490832047248));
#26269=CARTESIAN_POINT('Ctrl Pts',(18.9186581705949,-1.88411383655771,339.545111610003));
#26270=CARTESIAN_POINT('Ctrl Pts',(18.9108969156687,-1.75624006674755,339.593996505272));
#26271=CARTESIAN_POINT('Ctrl Pts',(18.9031232452641,-1.62816174057967,339.642959600442));
#26272=CARTESIAN_POINT('Ctrl Pts',(18.8953495748595,-1.49816997478634,339.686510659174));
#26273=CARTESIAN_POINT('Ctrl Pts',(18.8875759044549,-1.3667649588507,339.724525014195));
#26274=CARTESIAN_POINT('Ctrl Pts',(18.8801641002773,-1.24147687801078,339.760769791848));
#26275=CARTESIAN_POINT('Ctrl Pts',(18.8727522960996,-1.11490443906098,339.791981663734));
#26276=CARTESIAN_POINT('Ctrl Pts',(18.8653404919219,-0.987487262032757,
339.818096301427));
#26277=CARTESIAN_POINT('Ctrl Pts',(18.8575654131435,-0.853824989612378,
339.845490895302));
#26278=CARTESIAN_POINT('Ctrl Pts',(18.8497903343651,-0.718810681621633,
339.867362531755));
#26279=CARTESIAN_POINT('Ctrl Pts',(18.8420152555866,-0.582940485816961,
339.883581007058));
#26280=CARTESIAN_POINT('Ctrl Pts',(18.8342497445376,-0.447237486938147,
339.899779524494));
#26281=CARTESIAN_POINT('Ctrl Pts',(18.8264842334886,-0.310681080268791,
339.910338676482));
#26282=CARTESIAN_POINT('Ctrl Pts',(18.8187187224396,-0.173779068393592,
339.91517892837));
#26283=CARTESIAN_POINT('Ctrl Pts',(18.8109609109174,-0.0370127952616527,
339.920014381133));
#26284=CARTESIAN_POINT('Ctrl Pts',(18.8032030993952,0.100098013032427,339.919142204303));
#26285=CARTESIAN_POINT('Ctrl Pts',(18.795445287873,0.237039293933692,339.912534522589));
#26286=CARTESIAN_POINT('Ctrl Pts',(18.78769331435,0.373877522178236,339.905931813365));
#26287=CARTESIAN_POINT('Ctrl Pts',(18.779941340827,0.510546088113213,339.893602209103));
#26288=CARTESIAN_POINT('Ctrl Pts',(18.772189367304,0.646530139839806,339.875569899076));
#26289=CARTESIAN_POINT('Ctrl Pts',(18.7644406767464,0.782456602239759,339.857545225743));
#26290=CARTESIAN_POINT('Ctrl Pts',(18.7566919861888,0.917698740330531,339.833822701383));
#26291=CARTESIAN_POINT('Ctrl Pts',(18.7489432956312,1.0517462578595,339.804478418265));
#26292=CARTESIAN_POINT('Ctrl Pts',(18.7411962172533,1.18576588568286,339.775140240471));
#26293=CARTESIAN_POINT('Ctrl Pts',(18.7334491388756,1.31859100573686,339.740182713979));
#26294=CARTESIAN_POINT('Ctrl Pts',(18.7257020604978,1.44972135049144,339.699733084807));
#26295=CARTESIAN_POINT('Ctrl Pts',(18.717954917192,1.5808527942446,339.659283116628));
#26296=CARTESIAN_POINT('Ctrl Pts',(18.7102077738862,1.71028906085988,339.613341069176));
#26297=CARTESIAN_POINT('Ctrl Pts',(18.7024606305804,1.8375452702326,339.562084002114));
#26298=CARTESIAN_POINT('Ctrl Pts',(18.6947117455523,1.96483008950291,339.510815411375));
#26299=CARTESIAN_POINT('Ctrl Pts',(18.6869628605242,2.08993351374294,339.454229569258));
#26300=CARTESIAN_POINT('Ctrl Pts',(18.6792139754961,2.21239123158162,339.392551434067));
#26301=CARTESIAN_POINT('Ctrl Pts',(18.6714568657214,2.33497892730725,339.330807833065));
#26302=CARTESIAN_POINT('Ctrl Pts',(18.6636997559466,2.45491495738214,339.263961318076));
#26303=CARTESIAN_POINT('Ctrl Pts',(18.6559426461719,2.57175971322129,339.192282795799));
#26304=CARTESIAN_POINT('Ctrl Pts',(18.6481813912458,2.68866690716192,339.120565970812));
#26305=CARTESIAN_POINT('Ctrl Pts',(18.6404201363196,2.80247921118399,339.044012211576));
#26306=CARTESIAN_POINT('Ctrl Pts',(18.6326588813935,2.91278739676901,338.962934852319));
#26307=CARTESIAN_POINT('Ctrl Pts',(18.6248852109888,3.02327203950161,338.88172779571));
#26308=CARTESIAN_POINT('Ctrl Pts',(18.6171115405842,3.13024105730717,338.79598292344));
#26309=CARTESIAN_POINT('Ctrl Pts',(18.6093378701796,3.23331893358655,338.706053390901));
#26310=CARTESIAN_POINT('Ctrl Pts',(18.6019260660024,3.33159850992685,338.620310099737));
#26311=CARTESIAN_POINT('Ctrl Pts',(18.5945142618253,3.42634084830613,338.53076317034));
#26312=CARTESIAN_POINT('Ctrl Pts',(18.5871024576481,3.51725394995298,338.43774747677));
#26313=CARTESIAN_POINT('Ctrl Pts',(18.5793273788697,3.61262297352746,338.340172806979));
#26314=CARTESIAN_POINT('Ctrl Pts',(18.5715523000912,3.70407928840549,338.238472392464));
#26315=CARTESIAN_POINT('Ctrl Pts',(18.5637772213128,3.79124490947381,338.13299299375));
#26316=CARTESIAN_POINT('Ctrl Pts',(18.5560117102637,3.87830326769617,338.027643394151));
#26317=CARTESIAN_POINT('Ctrl Pts',(18.5482461992147,3.9610811911269,337.918524361504));
#26318=CARTESIAN_POINT('Ctrl Pts',(18.5404806881656,4.039236996263,337.806019877071));
#26319=CARTESIAN_POINT('Ctrl Pts',(18.5327228766434,4.11731530969082,337.693626941162));
#26320=CARTESIAN_POINT('Ctrl Pts',(18.5249650651211,4.19078040337237,337.577855552408));
#26321=CARTESIAN_POINT('Ctrl Pts',(18.5172072535989,4.25933064763511,337.45912291206));
#26322=CARTESIAN_POINT('Ctrl Pts',(18.5094552800758,4.32782930566519,337.340479621788));
#26323=CARTESIAN_POINT('Ctrl Pts',(18.5017033065528,4.39142028146919,337.218879852658));
#26324=CARTESIAN_POINT('Ctrl Pts',(18.4939513330297,4.44984530041762,337.094769644818));
#26325=CARTESIAN_POINT('Ctrl Pts',(18.4862026424721,4.50824557633576,336.970711997725));
#26326=CARTESIAN_POINT('Ctrl Pts',(18.4784539519145,4.56148408061635,336.84414637941));
#26327=CARTESIAN_POINT('Ctrl Pts',(18.4707052613568,4.60934865029003,336.715543086772));
#26328=CARTESIAN_POINT('Ctrl Pts',(18.4629581829789,4.65720326134028,336.586966551122));
#26329=CARTESIAN_POINT('Ctrl Pts',(18.455211104601,4.6996860254917,336.456353550521));
#26330=CARTESIAN_POINT('Ctrl Pts',(18.4474640262231,4.73663322317013,336.324193630728));
#26331=CARTESIAN_POINT('Ctrl Pts',(18.4397168829173,4.77358073050161,336.192032603308));
#26332=CARTESIAN_POINT('Ctrl Pts',(18.4319697396115,4.80499247358572,336.058325007279));
#26333=CARTESIAN_POINT('Ctrl Pts',(18.4242225963056,4.83075494922247,335.923574405807));
#26334=CARTESIAN_POINT('Ctrl Pts',(18.4164737112775,4.85652321681069,335.78879350954));
#26335=CARTESIAN_POINT('Ctrl Pts',(18.4087248262494,4.87663961625762,335.652969525067));
#26336=CARTESIAN_POINT('Ctrl Pts',(18.4009759412212,4.89104205427432,335.516614639572));
#26337=CARTESIAN_POINT('Ctrl Pts',(18.3932188314465,4.90545977918754,335.380115025593));
#26338=CARTESIAN_POINT('Ctrl Pts',(18.3854617216717,4.9141513864259,335.243083774266));
#26339=CARTESIAN_POINT('Ctrl Pts',(18.3777046118969,4.9171067897841,335.10603716499));
#26340=CARTESIAN_POINT('Ctrl Pts',(18.3699433569708,4.92006377241535,334.968917322388));
#26341=CARTESIAN_POINT('Ctrl Pts',(18.3621821020445,4.9172784513251,334.83178249608));
#26342=CARTESIAN_POINT('Ctrl Pts',(18.3544208471183,4.90879285891832,334.695146378187));
#26343=CARTESIAN_POINT('Ctrl Pts',(18.3466471767137,4.90029369232915,334.558291687035));
#26344=CARTESIAN_POINT('Ctrl Pts',(18.338873506309,4.8860760733654,334.421937687453));
#26345=CARTESIAN_POINT('Ctrl Pts',(18.3310998359043,4.86623376435236,334.286591272007));
#26346=CARTESIAN_POINT('Ctrl Pts',(18.3236880317275,4.84731511959862,334.157545264768));
#26347=CARTESIAN_POINT('Ctrl Pts',(18.3162762275508,4.82328371188101,334.029415429495));
#26348=CARTESIAN_POINT('Ctrl Pts',(18.308864423374,4.79426312665065,333.902628533751));
#26349=CARTESIAN_POINT('Ctrl Pts',(18.3010893445956,4.76382015608888,333.769627434562));
#26350=CARTESIAN_POINT('Ctrl Pts',(18.2933142658172,4.72779036758314,333.637683938384));
#26351=CARTESIAN_POINT('Ctrl Pts',(18.2855391870388,4.68626081002275,333.50730355298));
#26352=CARTESIAN_POINT('Ctrl Pts',(18.2777736759898,4.64478235722683,333.377083608942));
#26353=CARTESIAN_POINT('Ctrl Pts',(18.2700081649408,4.59781771888634,333.248423317326));
#26354=CARTESIAN_POINT('Ctrl Pts',(18.2622426538918,4.54550488848743,333.121817801374));
#26355=CARTESIAN_POINT('Ctrl Pts',(18.2544848423696,4.4932439264122,332.995337815159));
#26356=CARTESIAN_POINT('Ctrl Pts',(18.2467270308474,4.4356454733525,332.870908909159));
#26357=CARTESIAN_POINT('Ctrl Pts',(18.2389692193252,4.37289713361665,332.749010501733));
#26358=CARTESIAN_POINT('Ctrl Pts',(18.2312172458022,4.31019601399632,332.627203826725));
#26359=CARTESIAN_POINT('Ctrl Pts',(18.2234652722792,4.24235289977505,332.507924206048));
#26360=CARTESIAN_POINT('Ctrl Pts',(18.2157132987562,4.16960310840807,332.391630206268));
#26361=CARTESIAN_POINT('Ctrl Pts',(18.2079646081986,4.09688412662093,332.275385457065));
#26362=CARTESIAN_POINT('Ctrl Pts',(18.200215917641,4.01926280751208,332.162124144618));
#26363=CARTESIAN_POINT('Ctrl Pts',(18.1924672270834,3.93701982022087,332.052279185932));
#26364=CARTESIAN_POINT('Ctrl Pts',(18.1847201487056,3.85479394427009,331.942457081407));
#26365=CARTESIAN_POINT('Ctrl Pts',(18.1769730703277,3.7679485469018,331.836050229505));
#26366=CARTESIAN_POINT('Ctrl Pts',(18.1692259919499,3.67680669953446,331.733461226809));
#26367=CARTESIAN_POINT('Ctrl Pts',(18.1614788486441,3.58566408831078,331.630871364319));
#26368=CARTESIAN_POINT('Ctrl Pts',(18.1537317053383,3.49022521487238,331.532099707068));
#26369=CARTESIAN_POINT('Ctrl Pts',(18.1459845620325,3.39085211313526,331.437514209243));
#26370=CARTESIAN_POINT('Ctrl Pts',(18.1382356770045,3.29145667021513,331.34290744659));
#26371=CARTESIAN_POINT('Ctrl Pts',(18.1304867919763,3.18812552201458,331.252488985553));
#26372=CARTESIAN_POINT('Ctrl Pts',(18.1227379069483,3.08125577542158,331.16658821558));
#26373=CARTESIAN_POINT('Ctrl Pts',(18.1149807971735,2.97427259617522,331.080596269641));
#26374=CARTESIAN_POINT('Ctrl Pts',(18.1072236873988,2.86374362090279,330.999131838743));
#26375=CARTESIAN_POINT('Ctrl Pts',(18.0994665776241,2.75009754174042,330.922482792996));
#26376=CARTESIAN_POINT('Ctrl Pts',(18.0917053226979,2.63639073374697,330.84579278845));
#26377=CARTESIAN_POINT('Ctrl Pts',(18.0839440677718,2.51956383559806,330.773923501067));
#26378=CARTESIAN_POINT('Ctrl Pts',(18.0761828128456,2.40007156810452,330.707117573183));
#26379=CARTESIAN_POINT('Ctrl Pts',(18.068409142441,2.28038815192559,330.640204777586));
#26380=CARTESIAN_POINT('Ctrl Pts',(18.0606354720363,2.15803119526454,330.578371703528));
#26381=CARTESIAN_POINT('Ctrl Pts',(18.0528618016316,2.03347769506908,330.52181381292));
#26382=CARTESIAN_POINT('Ctrl Pts',(18.0454499974545,1.91472219027222,330.467888705726));
#26383=CARTESIAN_POINT('Ctrl Pts',(18.0380381932773,1.79397030461569,330.418758823205));
#26384=CARTESIAN_POINT('Ctrl Pts',(18.0306263891002,1.67164779522883,330.374551188133));
#26385=CARTESIAN_POINT('Ctrl Pts',(18.0228513103218,1.5433298952785,330.328176805177));
#26386=CARTESIAN_POINT('Ctrl Pts',(18.0150762315433,1.41287800850253,330.287072826296));
#26387=CARTESIAN_POINT('Ctrl Pts',(18.0073011527649,1.28076433431189,330.251439609476));
#26388=CARTESIAN_POINT('Ctrl Pts',(17.9995356417159,1.14881323440812,330.215850241598));
#26389=CARTESIAN_POINT('Ctrl Pts',(17.9917701306669,1.01520478970506,330.185718341606));
#26390=CARTESIAN_POINT('Ctrl Pts',(17.9840046196179,0.880430036092563,330.161195807429));
#26391=CARTESIAN_POINT('Ctrl Pts',(17.9762468080957,0.745788912040565,330.136697587416));
#26392=CARTESIAN_POINT('Ctrl Pts',(17.9684889965736,0.609984162461037,330.117797734637));
#26393=CARTESIAN_POINT('Ctrl Pts',(17.9607311850514,0.473520463938446,330.104597929411));
#26394=CARTESIAN_POINT('Ctrl Pts',(17.9529792115284,0.337159458676692,330.091408057456));
#26395=CARTESIAN_POINT('Ctrl Pts',(17.9452272380054,0.200140878988653,330.083909732563));
#26396=CARTESIAN_POINT('Ctrl Pts',(17.9374752644824,0.0629776870588596,
330.082153227943));
#26397=CARTESIAN_POINT('Ctrl Pts',(17.9297265739248,-0.0741274161777176,
330.080397467203));
#26398=CARTESIAN_POINT('Ctrl Pts',(17.9219778833672,-0.211376619818468,
330.084378695322));
#26399=CARTESIAN_POINT('Ctrl Pts',(17.9142291928096,-0.348253988541828,
330.094095167865));
#26400=CARTESIAN_POINT('Ctrl Pts',(17.9064821144318,-0.485102878785402,
330.103809618815));
#26401=CARTESIAN_POINT('Ctrl Pts',(17.898735036054,-0.621579698344404,330.119256913039));
#26402=CARTESIAN_POINT('Ctrl Pts',(17.8909879576762,-0.757171062679959,
330.140383241001));
#26403=CARTESIAN_POINT('Ctrl Pts',(17.8832408143704,-0.892763563401745,
330.161509746023));
#26404=CARTESIAN_POINT('Ctrl Pts',(17.8754936710645,-1.02747020788395,330.188315319542));
#26405=CARTESIAN_POINT('Ctrl Pts',(17.8677465277588,-1.16078565827567,330.220694640636));
#26406=CARTESIAN_POINT('Ctrl Pts',(17.8599976427307,-1.29413108081083,330.25308124129));
#26407=CARTESIAN_POINT('Ctrl Pts',(17.8522487577026,-1.42608430712066,330.291043990808));
#26408=CARTESIAN_POINT('Ctrl Pts',(17.8444998726745,-1.55615344927013,330.334427205066));
#26409=CARTESIAN_POINT('Ctrl Pts',(17.8367427628998,-1.68636064815112,330.377856466716));
#26410=CARTESIAN_POINT('Ctrl Pts',(17.8289856531251,-1.8146793967322,330.426717562068));
#26411=CARTESIAN_POINT('Ctrl Pts',(17.8212285433504,-1.94063562898163,330.480805777793));
#26412=CARTESIAN_POINT('Ctrl Pts',(17.8134672884243,-2.06665916821419,330.534922896532));
#26413=CARTESIAN_POINT('Ctrl Pts',(17.8057060334981,-2.19031732335299,330.594272532315));
#26414=CARTESIAN_POINT('Ctrl Pts',(17.797944778572,-2.31115997575782,330.658603608405));
#26415=CARTESIAN_POINT('Ctrl Pts',(17.7901711081674,-2.43219593702396,330.723037593251));
#26416=CARTESIAN_POINT('Ctrl Pts',(17.7823974377627,-2.55040705824079,330.792468744124));
#26417=CARTESIAN_POINT('Ctrl Pts',(17.7746237673581,-2.6653708408966,330.866601719771));
#26418=CARTESIAN_POINT('Ctrl Pts',(17.7672119631808,-2.77498303181388,330.937283787569));
#26419=CARTESIAN_POINT('Ctrl Pts',(17.7598001590035,-2.88164317223758,331.012239625843));
#26420=CARTESIAN_POINT('Ctrl Pts',(17.7523883548263,-2.98501404439358,331.091179945652));
#26421=CARTESIAN_POINT('Ctrl Pts',(17.7446981896833,-3.09226715832335,331.173084982705));
#26422=CARTESIAN_POINT('Ctrl Pts',(17.7370080245404,-3.19633425613697,331.259551070327));
#26423=CARTESIAN_POINT('Ctrl Pts',(17.7293178593975,-3.29679629098358,331.350299015226));
#26424=CARTESIAN_POINT('Ctrl Pts',(17.7216371958659,-3.39713419959996,331.440934836175));
#26425=CARTESIAN_POINT('Ctrl Pts',(17.7139565323343,-3.49387561020263,331.535841726835));
#26426=CARTESIAN_POINT('Ctrl Pts',(17.7062758688027,-3.58663160249314,331.634698110051));
#26427=CARTESIAN_POINT('Ctrl Pts',(17.6986027592911,-3.67929636820951,331.733457266888));
#26428=CARTESIAN_POINT('Ctrl Pts',(17.6909296497795,-3.76798324088064,331.836157899318));
#26429=CARTESIAN_POINT('Ctrl Pts',(17.6832565402679,-3.8523378461597,331.942439504843));
#26430=CARTESIAN_POINT('Ctrl Pts',(17.675476528112,-3.93786768950227,332.050201837921));
#26431=CARTESIAN_POINT('Ctrl Pts',(17.6676965159562,-4.01894332084126,332.161645408501));
#26432=CARTESIAN_POINT('Ctrl Pts',(17.6599165038003,-4.09523512542224,332.276356790986));
#26433=CARTESIAN_POINT('Ctrl Pts',(17.6522520831132,-4.17039342512254,332.389363850017));
#26434=CARTESIAN_POINT('Ctrl Pts',(17.6445876624261,-4.24090884870029,332.505541937));
#26435=CARTESIAN_POINT('Ctrl Pts',(17.636923241739,-4.30650827370955,332.62446436546));
#26436=CARTESIAN_POINT('Ctrl Pts',(17.6292600812692,-4.37209691257695,332.743367240178));
#26437=CARTESIAN_POINT('Ctrl Pts',(17.6215969207994,-4.43277096720742,332.865013208622));
#26438=CARTESIAN_POINT('Ctrl Pts',(17.6139337603296,-4.48830250834948,332.988949613748));
#26439=CARTESIAN_POINT('Ctrl Pts',(17.6062701133666,-4.54383757489307,333.112893886936));
#26440=CARTESIAN_POINT('Ctrl Pts',(17.5986064664036,-4.59422931560304,333.239128520474));
#26441=CARTESIAN_POINT('Ctrl Pts',(17.5909428194406,-4.6392975427444,333.367179932636));
#26442=CARTESIAN_POINT('Ctrl Pts',(17.5830756051977,-4.68556290441595,333.498632738127));
#26443=CARTESIAN_POINT('Ctrl Pts',(17.5752083909549,-4.72621782478933,333.631999771804));
#26444=CARTESIAN_POINT('Ctrl Pts',(17.567341176712,-4.76112199612357,333.766752092834));
#26445=CARTESIAN_POINT('Ctrl Pts',(17.559667529958,-4.79516737391469,333.898188924088));
#26446=CARTESIAN_POINT('Ctrl Pts',(17.5519938832039,-4.82374166199152,334.030943261726));
#26447=CARTESIAN_POINT('Ctrl Pts',(17.5443202364499,-4.84676671799636,334.164514845241));
#26448=CARTESIAN_POINT('Ctrl Pts',(17.5363562384626,-4.87066298343003,334.303140437005));
#26449=CARTESIAN_POINT('Ctrl Pts',(17.5283922404754,-4.88858176185565,334.442645856072));
#26450=CARTESIAN_POINT('Ctrl Pts',(17.5204282424881,-4.90049490263877,334.582468238679));
#26451=CARTESIAN_POINT('Ctrl Pts',(17.5124642445009,-4.9124080434219,334.722290621287));
#26452=CARTESIAN_POINT('Ctrl Pts',(17.5045002465137,-4.91831559428542,334.862429490414));
#26453=CARTESIAN_POINT('Ctrl Pts',(17.4965362485264,-4.91824945026714,335.002325391798));
#26454=CARTESIAN_POINT('',(20.9965362484902,-4.91588657005344,334.996283340543));
#26455=CARTESIAN_POINT('Ctrl Pts',(20.9965362484902,-4.91335673246954,334.996285253228));
#26456=CARTESIAN_POINT('Ctrl Pts',(20.93535974294,-4.90577737037676,336.078961636048));
#26457=CARTESIAN_POINT('Ctrl Pts',(20.7814372259651,-4.01911395901492,338.81429986906));
#26458=CARTESIAN_POINT('Ctrl Pts',(20.5347686975656,0.506096686042567,340.793816963868));
#26459=CARTESIAN_POINT('Ctrl Pts',(20.2565306632917,5.14602224722042,337.709779307904));
#26460=CARTESIAN_POINT('Ctrl Pts',(19.9782926290177,5.06351914728795,332.139017177353));
#26461=CARTESIAN_POINT('Ctrl Pts',(19.7000545947439,0.334299263309442,329.193736755108));
#26462=CARTESIAN_POINT('Ctrl Pts',(19.4561358012346,-4.08053706494637,331.282842392461));
#26463=CARTESIAN_POINT('Ctrl Pts',(19.3049630191501,-4.90617418397033,333.968623571676));
#26464=CARTESIAN_POINT('Ctrl Pts',(19.2465362484902,-4.91230824065646,335.003190760085));
#26465=CARTESIAN_POINT('',(22.7465362484346,-4.91824976548729,334.998481189866));
#26466=CARTESIAN_POINT('Ctrl Pts',(22.7465362484345,-4.91824976548729,334.998481189866));
#26467=CARTESIAN_POINT('Ctrl Pts',(22.7388226837815,-4.91829158424431,335.133899756872));
#26468=CARTESIAN_POINT('Ctrl Pts',(22.7311091191285,-4.91273627149401,335.269545225059));
#26469=CARTESIAN_POINT('Ctrl Pts',(22.7233955544755,-4.90155375923713,335.404912098866));
#26470=CARTESIAN_POINT('Ctrl Pts',(22.7156912571,-4.89038468194175,335.540116339386));
#26471=CARTESIAN_POINT('Ctrl Pts',(22.7079869597246,-4.87360188545452,335.675042258912));
#26472=CARTESIAN_POINT('Ctrl Pts',(22.7002826623491,-4.85122728219769,335.809182871149));
#26473=CARTESIAN_POINT('Ctrl Pts',(22.6925857063339,-4.82887399951244,335.943195661923));
#26474=CARTESIAN_POINT('Ctrl Pts',(22.6848887503186,-4.80093957597117,336.076424244487));
#26475=CARTESIAN_POINT('Ctrl Pts',(22.6771917943034,-4.76749780895062,336.208365716226));
#26476=CARTESIAN_POINT('Ctrl Pts',(22.6695002608708,-4.73407960198986,336.340214233877));
#26477=CARTESIAN_POINT('Ctrl Pts',(22.6618087274382,-4.69516186991169,336.470777061206));
#26478=CARTESIAN_POINT('Ctrl Pts',(22.6541171940056,-4.65086959118823,336.599560911082));
#26479=CARTESIAN_POINT('Ctrl Pts',(22.6464283535761,-4.6065928203277,336.728299670428));
#26480=CARTESIAN_POINT('Ctrl Pts',(22.6387395131467,-4.55694537205061,336.855260314972));
#26481=CARTESIAN_POINT('Ctrl Pts',(22.6310506727172,-4.50210216042523,336.979964444023));
#26482=CARTESIAN_POINT('Ctrl Pts',(22.623362963651,-4.44726701862451,337.104650223666));
#26483=CARTESIAN_POINT('Ctrl Pts',(22.6156752545848,-4.38723779378876,337.227079784249));
#26484=CARTESIAN_POINT('Ctrl Pts',(22.6079875455186,-4.3222374516481,337.346794936519));
#26485=CARTESIAN_POINT('Ctrl Pts',(22.6002992388898,-4.25723205705667,337.466519394199));
#26486=CARTESIAN_POINT('Ctrl Pts',(22.592610932261,-4.18725496639923,337.583528674518));
#26487=CARTESIAN_POINT('Ctrl Pts',(22.5849226256322,-4.11257474635776,337.697389852824));
#26488=CARTESIAN_POINT('Ctrl Pts',(22.5772319923915,-4.03787192681524,337.811285487455));
#26489=CARTESIAN_POINT('Ctrl Pts',(22.5695413591507,-3.95846336496409,337.922030792913));
#26490=CARTESIAN_POINT('Ctrl Pts',(22.56185072591,-3.87466023386913,338.029222859839));
#26491=CARTESIAN_POINT('Ctrl Pts',(22.5541517580921,-3.79076628272903,338.136531094124));
#26492=CARTESIAN_POINT('Ctrl Pts',(22.5464527902743,-3.70246849964301,338.240278088986));
#26493=CARTESIAN_POINT('Ctrl Pts',(22.5387538224564,-3.61011775775866,338.340094734826));
#26494=CARTESIAN_POINT('Ctrl Pts',(22.5310500850703,-3.51770980389792,338.439973217826));
#26495=CARTESIAN_POINT('Ctrl Pts',(22.5233463476842,-3.42124417273066,338.535916223746));
#26496=CARTESIAN_POINT('Ctrl Pts',(22.5156426102981,-3.32110679916533,338.627593236712));
#26497=CARTESIAN_POINT('Ctrl Pts',(22.5079277137406,-3.22082437261341,338.719403047494));
#26498=CARTESIAN_POINT('Ctrl Pts',(22.5002128171831,-3.11685988912234,338.80693427421));
#26499=CARTESIAN_POINT('Ctrl Pts',(22.4924979206257,-3.00963069273072,338.889897962142));
#26500=CARTESIAN_POINT('Ctrl Pts',(22.4891435929115,-2.96300895742366,338.925969398178));
#26501=CARTESIAN_POINT('Ctrl Pts',(22.4857892651973,-2.91577041472595,338.961177961164));
#26502=CARTESIAN_POINT('Ctrl Pts',(22.4824349374831,-2.86795086611008,338.995502583165));
#26503=CARTESIAN_POINT('Ctrl Pts',(22.4746598587047,-2.75710875725285,339.075064469431));
#26504=CARTESIAN_POINT('Ctrl Pts',(22.4668847799262,-2.64277821270163,339.15013615801));
#26505=CARTESIAN_POINT('Ctrl Pts',(22.4591097011478,-2.52535903425054,339.22039628597));
#26506=CARTESIAN_POINT('Ctrl Pts',(22.4513441900988,-2.40808434757379,339.29056995437));
#26507=CARTESIAN_POINT('Ctrl Pts',(22.4435786790498,-2.28772892162752,339.355943644326));
#26508=CARTESIAN_POINT('Ctrl Pts',(22.4358131680008,-2.16472387816742,339.416237492911));
#26509=CARTESIAN_POINT('Ctrl Pts',(22.4280553564786,-2.04184079456628,339.476471559969));
#26510=CARTESIAN_POINT('Ctrl Pts',(22.4202975449565,-1.91631367025211,339.531635637998));
#26511=CARTESIAN_POINT('Ctrl Pts',(22.4125397334343,-1.78860042604498,339.581494469979));
#26512=CARTESIAN_POINT('Ctrl Pts',(22.4047877599113,-1.66098329010396,339.631315781608));
#26513=CARTESIAN_POINT('Ctrl Pts',(22.3970357863883,-1.53118367145477,339.675839652223));
#26514=CARTESIAN_POINT('Ctrl Pts',(22.3892838128653,-1.3996814611181,339.714878033407));
#26515=CARTESIAN_POINT('Ctrl Pts',(22.3815351223077,-1.26823494204559,339.753899881813));
#26516=CARTESIAN_POINT('Ctrl Pts',(22.3737864317501,-1.13508763933206,339.78744075028));
#26517=CARTESIAN_POINT('Ctrl Pts',(22.3660377411925,-1.00073646871108,339.815361832998));
#26518=CARTESIAN_POINT('Ctrl Pts',(22.3582906628147,-0.866413250973457,
339.843277106501));
#26519=CARTESIAN_POINT('Ctrl Pts',(22.3505435844368,-0.73088704599748,339.86557484048));
#26520=CARTESIAN_POINT('Ctrl Pts',(22.342796506059,-0.594666491951997,339.882167021503));
#26521=CARTESIAN_POINT('Ctrl Pts',(22.3350493627532,-0.458444796246882,
339.898759341584));
#26522=CARTESIAN_POINT('Ctrl Pts',(22.3273022194474,-0.321529127871818,
339.909645966073));
#26523=CARTESIAN_POINT('Ctrl Pts',(22.3195550761416,-0.184434408416318,
339.914790637605));
#26524=CARTESIAN_POINT('Ctrl Pts',(22.3118061911135,-0.0473088671574665,
339.919936465769));
#26525=CARTESIAN_POINT('Ctrl Pts',(22.3040573060855,0.0899954147607131,
339.919337757548));
#26526=CARTESIAN_POINT('Ctrl Pts',(22.2963084210574,0.226962744033899,339.9130103781));
#26527=CARTESIAN_POINT('Ctrl Pts',(22.2885513112826,0.364075451845699,339.906676282706));
#26528=CARTESIAN_POINT('Ctrl Pts',(22.280794201508,0.500850101508433,339.89460138784));
#26529=CARTESIAN_POINT('Ctrl Pts',(22.2730370917332,0.636774798031272,339.876853588031));
#26530=CARTESIAN_POINT('Ctrl Pts',(22.2652758368071,0.772772128365996,339.859096304366));
#26531=CARTESIAN_POINT('Ctrl Pts',(22.2575145818808,0.90791821561975,339.835660142135));
#26532=CARTESIAN_POINT('Ctrl Pts',(22.2497533269547,1.04171158302198,339.806664128093));
#26533=CARTESIAN_POINT('Ctrl Pts',(22.24197965655,1.17571897620871,339.777621729878));
#26534=CARTESIAN_POINT('Ctrl Pts',(22.2342059861454,1.3083689470043,339.743001805863));
#26535=CARTESIAN_POINT('Ctrl Pts',(22.2264323157407,1.43917454233185,339.702973495482));
#26536=CARTESIAN_POINT('Ctrl Pts',(22.2190205115635,1.56389110572832,339.664808512579));
#26537=CARTESIAN_POINT('Ctrl Pts',(22.2116087073864,1.68693086912867,339.621727427768));
#26538=CARTESIAN_POINT('Ctrl Pts',(22.2041969032093,1.80789058585415,339.573916778001));
#26539=CARTESIAN_POINT('Ctrl Pts',(22.1964218244308,1.93477889861557,339.523762785869));
#26540=CARTESIAN_POINT('Ctrl Pts',(22.1886467456524,2.05977910106734,339.468245390123));
#26541=CARTESIAN_POINT('Ctrl Pts',(22.1808716668739,2.18240459657439,339.4075268847));
#26542=CARTESIAN_POINT('Ctrl Pts',(22.1731061558249,2.30487919360266,339.346883097263));
#26543=CARTESIAN_POINT('Ctrl Pts',(22.1653406447759,2.42498455114582,339.281051106691));
#26544=CARTESIAN_POINT('Ctrl Pts',(22.1575751337269,2.54225202177826,339.210242002577));
#26545=CARTESIAN_POINT('Ctrl Pts',(22.1498173222047,2.65940322137208,339.139503105896));
#26546=CARTESIAN_POINT('Ctrl Pts',(22.1420595106824,2.77372180117237,339.063797116992));
#26547=CARTESIAN_POINT('Ctrl Pts',(22.1343016991602,2.88476212130198,338.98338180018));
#26548=CARTESIAN_POINT('Ctrl Pts',(22.1265497256372,2.99571888006969,338.903026998443));
#26549=CARTESIAN_POINT('Ctrl Pts',(22.1187977521141,3.10340197429674,338.817970151135));
#26550=CARTESIAN_POINT('Ctrl Pts',(22.1110457785911,3.20739357349057,338.728513045067));
#26551=CARTESIAN_POINT('Ctrl Pts',(22.1032970880335,3.31134113217999,338.639093824136));
#26552=CARTESIAN_POINT('Ctrl Pts',(22.0955483974758,3.41160000952578,338.545278305213));
#26553=CARTESIAN_POINT('Ctrl Pts',(22.0877997069182,3.50778457114477,338.447409239551));
#26554=CARTESIAN_POINT('Ctrl Pts',(22.0800526285404,3.60394912076236,338.349560536365));
#26555=CARTESIAN_POINT('Ctrl Pts',(22.0723055501626,3.69604076697099,338.247660242575));
#26556=CARTESIAN_POINT('Ctrl Pts',(22.0645584717847,3.78371024409984,338.142088453751));
#26557=CARTESIAN_POINT('Ctrl Pts',(22.0568113284789,3.87138045598336,338.036515780133));
#26558=CARTESIAN_POINT('Ctrl Pts',(22.0490641851731,3.95462817514892,337.927271850814));
#26559=CARTESIAN_POINT('Ctrl Pts',(22.0413170418673,4.03314425838771,337.814770053403));
#26560=CARTESIAN_POINT('Ctrl Pts',(22.0335681568392,4.11167799370896,337.7022429632));
#26561=CARTESIAN_POINT('Ctrl Pts',(22.0258192718111,4.18547775265751,337.586456867904));
#26562=CARTESIAN_POINT('Ctrl Pts',(22.018070386783,4.25427780534426,337.467854010564));
#26563=CARTESIAN_POINT('Ctrl Pts',(22.0103132770083,4.32315088311768,337.349125266925));
#26564=CARTESIAN_POINT('Ctrl Pts',(22.0025561672335,4.38701345747788,337.227574127595));
#26565=CARTESIAN_POINT('Ctrl Pts',(21.9947990574588,4.44564560663194,337.103667797618));
#26566=CARTESIAN_POINT('Ctrl Pts',(21.9870378025326,4.50430908693178,336.97969525606));
#26567=CARTESIAN_POINT('Ctrl Pts',(21.9792765476065,4.55773642061718,336.853365375923));
#26568=CARTESIAN_POINT('Ctrl Pts',(21.9715152926804,4.60575632196914,336.725164271929));
#26569=CARTESIAN_POINT('Ctrl Pts',(21.9637416222757,4.65385303951368,336.596758087949));
#26570=CARTESIAN_POINT('Ctrl Pts',(21.955967951871,4.69652491747625,336.466475070168));
#26571=CARTESIAN_POINT('Ctrl Pts',(21.9481942814664,4.73365067056552,336.334816238871));
#26572=CARTESIAN_POINT('Ctrl Pts',(21.9407824772894,4.76904821091614,336.209286157848));
#26573=CARTESIAN_POINT('Ctrl Pts',(21.9333706731123,4.79940428359922,336.082505748886));
#26574=CARTESIAN_POINT('Ctrl Pts',(21.9259588689353,4.82465753160155,335.954915056568));
#26575=CARTESIAN_POINT('Ctrl Pts',(21.9181837901569,4.85114851651438,335.821070764345));
#26576=CARTESIAN_POINT('Ctrl Pts',(21.9104087113785,4.87210753607659,335.685911778915));
#26577=CARTESIAN_POINT('Ctrl Pts',(21.9026336326,4.88740774136202,335.549935116332));
#26578=CARTESIAN_POINT('Ctrl Pts',(21.894868121551,4.90268911877077,335.414125781688));
#26579=CARTESIAN_POINT('Ctrl Pts',(21.887102610502,4.91232549404534,335.277501156657));
#26580=CARTESIAN_POINT('Ctrl Pts',(21.879337099453,4.91624076491548,335.140569569549));
#26581=CARTESIAN_POINT('Ctrl Pts',(21.8715792879308,4.92015215378314,335.003773750509));
#26582=CARTESIAN_POINT('Ctrl Pts',(21.8638214764086,4.91835371572585,334.86667196327));
#26583=CARTESIAN_POINT('Ctrl Pts',(21.8560636648864,4.91082104894698,334.729778446975));
#26584=CARTESIAN_POINT('Ctrl Pts',(21.8483116913633,4.90329405073872,334.592987947391));
#26585=CARTESIAN_POINT('Ctrl Pts',(21.8405597178403,4.89004143437069,334.456405795499));
#26586=CARTESIAN_POINT('Ctrl Pts',(21.8328077443173,4.87109086675438,334.320546668032));
#26587=CARTESIAN_POINT('Ctrl Pts',(21.8250590537597,4.85214832471475,334.184745076987));
#26588=CARTESIAN_POINT('Ctrl Pts',(21.817310363202,4.82751268477103,334.049666287675));
#26589=CARTESIAN_POINT('Ctrl Pts',(21.8095616726444,4.79726348487193,333.915820070646));
#26590=CARTESIAN_POINT('Ctrl Pts',(21.8018145942665,4.76702057857156,333.782001701441));
#26591=CARTESIAN_POINT('Ctrl Pts',(21.7940675158888,4.73116652155738,333.649415775447));
#26592=CARTESIAN_POINT('Ctrl Pts',(21.7863204375109,4.68983193660753,333.518561689143));
#26593=CARTESIAN_POINT('Ctrl Pts',(21.7785732942051,4.64849700523404,333.387706506154));
#26594=CARTESIAN_POINT('Ctrl Pts',(21.7708261508993,4.60168157204609,333.258583564526));
#26595=CARTESIAN_POINT('Ctrl Pts',(21.7630790075935,4.54956596837533,333.131676537133));
#26596=CARTESIAN_POINT('Ctrl Pts',(21.7553301225654,4.49743864801056,333.004740978345));
#26597=CARTESIAN_POINT('Ctrl Pts',(21.7475812375373,4.44000893448496,332.880022686628));
#26598=CARTESIAN_POINT('Ctrl Pts',(21.7398323525093,4.3775049177217,332.757984443002));
#26599=CARTESIAN_POINT('Ctrl Pts',(21.7320752427345,4.314934558549,332.635816666722));
#26600=CARTESIAN_POINT('Ctrl Pts',(21.7243181329597,4.24727931572631,332.5163349694));
#26601=CARTESIAN_POINT('Ctrl Pts',(21.716561023185,4.17481305964195,332.399977119419));
#26602=CARTESIAN_POINT('Ctrl Pts',(21.7087997682588,4.10230807990751,332.283557091524));
#26603=CARTESIAN_POINT('Ctrl Pts',(21.7010385133327,4.02498718448782,332.170264559857));
#26604=CARTESIAN_POINT('Ctrl Pts',(21.6932772584065,3.94316646509159,332.060506626802));
#26605=CARTESIAN_POINT('Ctrl Pts',(21.6855035880019,3.86121485920964,331.950573116823));
#26606=CARTESIAN_POINT('Ctrl Pts',(21.6777299175972,3.77474929176875,331.844185807721));
#26607=CARTESIAN_POINT('Ctrl Pts',(21.6699562471925,3.68412544698488,331.741717821707));
#26608=CARTESIAN_POINT('Ctrl Pts',(21.6625444430155,3.59772016397853,331.644019745096));
#26609=CARTESIAN_POINT('Ctrl Pts',(21.6551326388384,3.50753522609962,331.549884522009));
#26610=CARTESIAN_POINT('Ctrl Pts',(21.6477208346613,3.41390747242586,331.459601882243));
#26611=CARTESIAN_POINT('Ctrl Pts',(21.6399457558829,3.31569074364166,331.364894221364));
#26612=CARTESIAN_POINT('Ctrl Pts',(21.6321706771044,3.21337479741648,331.274127052236));
#26613=CARTESIAN_POINT('Ctrl Pts',(21.6243955983259,3.1073089399203,331.187676008733));
#26614=CARTESIAN_POINT('Ctrl Pts',(21.6166300872769,3.0013736032144,331.101331348742));
#26615=CARTESIAN_POINT('Ctrl Pts',(21.6088645762279,2.89169783686368,331.019292491067));
#26616=CARTESIAN_POINT('Ctrl Pts',(21.6010990651789,2.77866792168339,330.941898517347));
#26617=CARTESIAN_POINT('Ctrl Pts',(21.5933412536567,2.66575007599316,330.864581279978));
#26618=CARTESIAN_POINT('Ctrl Pts',(21.5855834421345,2.54948502013865,330.791899980934));
#26619=CARTESIAN_POINT('Ctrl Pts',(21.5778256306123,2.43029198357238,330.724153424515));
#26620=CARTESIAN_POINT('Ctrl Pts',(21.5700736570893,2.31118864354578,330.656457849528));
#26621=CARTESIAN_POINT('Ctrl Pts',(21.5623216835663,2.18916204701557,330.593689817893));
#26622=CARTESIAN_POINT('Ctrl Pts',(21.5545697100433,2.06465996878092,330.536104585027));
#26623=CARTESIAN_POINT('Ctrl Pts',(21.5468210194857,1.94021061725066,330.478543739542));
#26624=CARTESIAN_POINT('Ctrl Pts',(21.5390723289281,1.81328822317247,330.426161491033));
#26625=CARTESIAN_POINT('Ctrl Pts',(21.5313236383705,1.68436450602539,330.379166820438));
#26626=CARTESIAN_POINT('Ctrl Pts',(21.5235765599926,1.55546761253445,330.332181927477));
#26627=CARTESIAN_POINT('Ctrl Pts',(21.5158294816148,1.42457059121446,330.290582516599));
#26628=CARTESIAN_POINT('Ctrl Pts',(21.5080824032369,1.29216408269702,330.254528996413));
#26629=CARTESIAN_POINT('Ctrl Pts',(21.5003352599311,1.15975646448497,330.218475174063));
#26630=CARTESIAN_POINT('Ctrl Pts',(21.4925881166253,1.02583971098499,330.187967437806));
#26631=CARTESIAN_POINT('Ctrl Pts',(21.4848409733195,0.890918140667847,330.163115886324));
#26632=CARTESIAN_POINT('Ctrl Pts',(21.4770920882914,0.75596623711778,330.138258747686));
#26633=CARTESIAN_POINT('Ctrl Pts',(21.4693432032633,0.620009451559208,330.119060395017));
#26634=CARTESIAN_POINT('Ctrl Pts',(21.4615943182352,0.483560378971694,330.105579459998));
#26635=CARTESIAN_POINT('Ctrl Pts',(21.4538372084605,0.346966477928753,330.092084216177));
#26636=CARTESIAN_POINT('Ctrl Pts',(21.4460800986857,0.209879635671917,330.084318550948));
#26637=CARTESIAN_POINT('Ctrl Pts',(21.438322988911,0.0728161879576935,330.082289062453));
#26638=CARTESIAN_POINT('Ctrl Pts',(21.4305617339849,-0.0643205020802697,
330.080258489464));
#26639=CARTESIAN_POINT('Ctrl Pts',(21.4228004790587,-0.201433382132718,
330.083970190382));
#26640=CARTESIAN_POINT('Ctrl Pts',(21.4150392241326,-0.338009055758815,
330.093378663405));
#26641=CARTESIAN_POINT('Ctrl Pts',(21.4072655537279,-0.474803205953177,
330.10280218692));
#26642=CARTESIAN_POINT('Ctrl Pts',(21.3994918833233,-0.611058043786753,
330.117940649785));
#26643=CARTESIAN_POINT('Ctrl Pts',(21.3917182129186,-0.746267321691431,
330.138696867395));
#26644=CARTESIAN_POINT('Ctrl Pts',(21.3843064087415,-0.875182575179624,
330.158486878082));
#26645=CARTESIAN_POINT('Ctrl Pts',(21.3768946045645,-1.00314713725636,330.183383345665));
#26646=CARTESIAN_POINT('Ctrl Pts',(21.3694828003874,-1.12973508500288,330.213259804396));
#26647=CARTESIAN_POINT('Ctrl Pts',(21.361707721609,-1.26252748515516,330.244600597366));
#26648=CARTESIAN_POINT('Ctrl Pts',(21.3539326428305,-1.39422456349755,330.281520935928));
#26649=CARTESIAN_POINT('Ctrl Pts',(21.3461575640521,-1.52432141188036,330.323930358112));
#26650=CARTESIAN_POINT('Ctrl Pts',(21.3383920530031,-1.65425816780887,330.366287592803));
#26651=CARTESIAN_POINT('Ctrl Pts',(21.3306265419541,-1.78259824381643,330.414120351281));
#26652=CARTESIAN_POINT('Ctrl Pts',(21.322861030905,-1.90884746020496,330.467287298298));
#26653=CARTESIAN_POINT('Ctrl Pts',(21.3151032193829,-2.03497150012728,330.520401530132));
#26654=CARTESIAN_POINT('Ctrl Pts',(21.3073454078607,-2.1590084480902,330.578839274642));
#26655=CARTESIAN_POINT('Ctrl Pts',(21.2995875963386,-2.28048016407282,330.642409692987));
#26656=CARTESIAN_POINT('Ctrl Pts',(21.2918356228156,-2.40186046873674,330.705932272577));
#26657=CARTESIAN_POINT('Ctrl Pts',(21.2840836492926,-2.52067903890204,330.774579657375));
#26658=CARTESIAN_POINT('Ctrl Pts',(21.2763316757697,-2.63647890820588,330.848113437353));
#26659=CARTESIAN_POINT('Ctrl Pts',(21.268582985212,-2.75222973619696,330.921616075733));
#26660=CARTESIAN_POINT('Ctrl Pts',(21.2608342946545,-2.86496407673566,331.000000784322));
#26661=CARTESIAN_POINT('Ctrl Pts',(21.2530856040969,-2.97425091881596,331.082983975726));
#26662=CARTESIAN_POINT('Ctrl Pts',(21.2453385257191,-3.08351502285583,331.165949901783));
#26663=CARTESIAN_POINT('Ctrl Pts',(21.2375914473412,-3.18933274405313,331.253512171376));
#26664=CARTESIAN_POINT('Ctrl Pts',(21.2298443689634,-3.2913036775886,331.345345000634));
#26665=CARTESIAN_POINT('Ctrl Pts',(21.2220972256576,-3.39327546573884,331.437178599539));
#26666=CARTESIAN_POINT('Ctrl Pts',(21.2143500823518,-3.49140011147154,331.533282567923));
#26667=CARTESIAN_POINT('Ctrl Pts',(21.206602939046,-3.58531211479375,331.633292394339));
#26668=CARTESIAN_POINT('Ctrl Pts',(21.1988540540179,-3.67924523152811,331.733324705088));
#26669=CARTESIAN_POINT('Ctrl Pts',(21.1911051689898,-3.76896355373146,331.837264336344));
#26670=CARTESIAN_POINT('Ctrl Pts',(21.1833562839617,-3.85414038221471,331.944711965022));
#26671=CARTESIAN_POINT('Ctrl Pts',(21.175599174187,-3.93940761826387,332.052273639723));
#26672=CARTESIAN_POINT('Ctrl Pts',(21.1678420644123,-4.02012348821465,332.163350442947));
#26673=CARTESIAN_POINT('Ctrl Pts',(21.1600849546375,-4.09600302464501,332.277511747574));
#26674=CARTESIAN_POINT('Ctrl Pts',(21.1523236997114,-4.17192310867353,332.391734056351));
#26675=CARTESIAN_POINT('Ctrl Pts',(21.1445624447852,-4.24300150711804,332.509043816707));
#26676=CARTESIAN_POINT('Ctrl Pts',(21.136801189859,-4.3089986551416,332.628984678985));
#26677=CARTESIAN_POINT('Ctrl Pts',(21.1290275194543,-4.37510137709339,332.749117407554));
#26678=CARTESIAN_POINT('Ctrl Pts',(21.1212538490497,-4.43610643175796,332.871889298458));
#26679=CARTESIAN_POINT('Ctrl Pts',(21.113480178645,-4.49182158413607,332.996822045152));
#26680=CARTESIAN_POINT('Ctrl Pts',(21.1060683744678,-4.54494318276729,333.115939142431));
#26681=CARTESIAN_POINT('Ctrl Pts',(21.0986565702907,-4.59325617917902,333.237020179856));
#26682=CARTESIAN_POINT('Ctrl Pts',(21.0912447661135,-4.63663642978742,333.359638551883));
#26683=CARTESIAN_POINT('Ctrl Pts',(21.0821717252757,-4.68973966564186,333.509739859241));
#26684=CARTESIAN_POINT('Ctrl Pts',(21.0730986844378,-4.7355897967023,333.662533588535));
#26685=CARTESIAN_POINT('Ctrl Pts',(21.0640256435999,-4.77394578823425,333.817365367706));
#26686=CARTESIAN_POINT('Ctrl Pts',(21.054991692469,-4.81213652927363,333.971530079576));
#26687=CARTESIAN_POINT('Ctrl Pts',(21.045957741338,-4.84289747739681,334.127715215526));
#26688=CARTESIAN_POINT('Ctrl Pts',(21.0369237902071,-4.86603740361971,334.285253157353));
#26689=CARTESIAN_POINT('Ctrl Pts',(21.0279628401055,-4.88899034206614,334.441518075698));
#26690=CARTESIAN_POINT('Ctrl Pts',(21.019001890004,-4.90444485114099,334.599113906424));
#26691=CARTESIAN_POINT('Ctrl Pts',(21.0100409399025,-4.91226154072782,334.757369379537));
#26692=CARTESIAN_POINT('Ctrl Pts',(21.0055393760983,-4.91618828136507,334.836869555467));
#26693=CARTESIAN_POINT('Ctrl Pts',(21.0010378122943,-4.91818830257432,334.916535897836));
#26694=CARTESIAN_POINT('Ctrl Pts',(20.9965362484902,-4.91824859433364,334.996281554732));
#26695=CARTESIAN_POINT('',(24.4965362484557,-4.91824791279987,335.004531085933));
#26696=CARTESIAN_POINT('Ctrl Pts',(24.4965362484557,-4.91824791279987,335.004531085932));
#26697=CARTESIAN_POINT('Ctrl Pts',(24.4864060560759,-4.91808312709539,335.183397026497));
#26698=CARTESIAN_POINT('Ctrl Pts',(24.4762758636962,-4.90815751266951,335.361829075815));
#26699=CARTESIAN_POINT('Ctrl Pts',(24.4661456713164,-4.88863305237369,335.538934079215));
#26700=CARTESIAN_POINT('Ctrl Pts',(24.455753395049,-4.86860346381701,335.720621065472));
#26701=CARTESIAN_POINT('Ctrl Pts',(24.4453611187817,-4.83847188859012,335.90091181959));
#26702=CARTESIAN_POINT('Ctrl Pts',(24.4349688425143,-4.79846090163957,336.07886794277));
#26703=CARTESIAN_POINT('Ctrl Pts',(24.4333462874764,-4.79221395181128,336.106652385441));
#26704=CARTESIAN_POINT('Ctrl Pts',(24.4317237324386,-4.78572626664462,336.134379960616));
#26705=CARTESIAN_POINT('Ctrl Pts',(24.4301011774008,-4.778998796945,336.162047142459));
#26706=CARTESIAN_POINT('Ctrl Pts',(24.4223260986224,-4.74676161196496,336.294624782907));
#26707=CARTESIAN_POINT('Ctrl Pts',(24.4145510198439,-4.7089524083983,336.426069432738));
#26708=CARTESIAN_POINT('Ctrl Pts',(24.4067759410655,-4.66566505716241,336.555876806458));
#26709=CARTESIAN_POINT('Ctrl Pts',(24.3990104300165,-4.62243097376797,336.685524443941));
#26710=CARTESIAN_POINT('Ctrl Pts',(24.3912449189675,-4.57373227824828,336.813538446878));
#26711=CARTESIAN_POINT('Ctrl Pts',(24.3834794079185,-4.51971364116093,336.939425601668));
#26712=CARTESIAN_POINT('Ctrl Pts',(24.3757215963963,-4.46574856370963,337.065187938977));
#26713=CARTESIAN_POINT('Ctrl Pts',(24.3679637848741,-4.40647419485819,337.188827267836));
#26714=CARTESIAN_POINT('Ctrl Pts',(24.3602059733519,-4.34208459926746,337.309866748387));
#26715=CARTESIAN_POINT('Ctrl Pts',(24.3524539998289,-4.27774345888933,337.430815142891));
#26716=CARTESIAN_POINT('Ctrl Pts',(24.3447020263059,-4.20829493659116,337.549167239647));
#26717=CARTESIAN_POINT('Ctrl Pts',(24.3369500527829,-4.13398052409446,337.66446769335));
#26718=CARTESIAN_POINT('Ctrl Pts',(24.3292013622253,-4.05969758379557,337.779719317243));
#26719=CARTESIAN_POINT('Ctrl Pts',(24.3214526716676,-3.98055306321583,337.891921540659));
#26720=CARTESIAN_POINT('Ctrl Pts',(24.31370398111,-3.89683345506705,338.000645278264));
#26721=CARTESIAN_POINT('Ctrl Pts',(24.3059569027322,-3.81313126548187,338.109346394988));
#26722=CARTESIAN_POINT('Ctrl Pts',(24.2982098243543,-3.72485612001893,338.214570155942));
#26723=CARTESIAN_POINT('Ctrl Pts',(24.2904627459765,-3.63233650013593,338.315918366347));
#26724=CARTESIAN_POINT('Ctrl Pts',(24.2827156026707,-3.53981610484941,338.417267426148));
#26725=CARTESIAN_POINT('Ctrl Pts',(24.2749684593649,-3.44305142772042,338.514740581938));
#26726=CARTESIAN_POINT('Ctrl Pts',(24.2672213160591,-3.34240944109033,338.607974804597));
#26727=CARTESIAN_POINT('Ctrl Pts',(24.259472431031,-3.24174482800509,338.70122998829));
#26728=CARTESIAN_POINT('Ctrl Pts',(24.2517235460029,-3.13720145751528,338.790244076901));
#26729=CARTESIAN_POINT('Ctrl Pts',(24.2439746609748,-3.02918085068011,338.874693076409));
#26730=CARTESIAN_POINT('Ctrl Pts',(24.2362175512001,-2.92104558965679,338.959231710958));
#26731=CARTESIAN_POINT('Ctrl Pts',(24.2284604414253,-2.80942602804438,339.039195336075));
#26732=CARTESIAN_POINT('Ctrl Pts',(24.2207033316506,-2.69475470829468,339.114301900034));
#26733=CARTESIAN_POINT('Ctrl Pts',(24.2129420767244,-2.58002211185827,339.189448598539));
#26734=CARTESIAN_POINT('Ctrl Pts',(24.2051808217983,-2.46223484333306,339.259732864015));
#26735=CARTESIAN_POINT('Ctrl Pts',(24.1974195668721,-2.34185086039195,339.324918220057));
#26736=CARTESIAN_POINT('Ctrl Pts',(24.1896458964675,-2.22127430231118,339.390207851425));
#26737=CARTESIAN_POINT('Ctrl Pts',(24.1818722260628,-2.09809308049226,339.450382102415));
#26738=CARTESIAN_POINT('Ctrl Pts',(24.1740985556581,-1.97278678925149,339.505251973714));
#26739=CARTESIAN_POINT('Ctrl Pts',(24.166686751481,-1.85331353601425,339.557567639304));
#26740=CARTESIAN_POINT('Ctrl Pts',(24.159274947304,-1.73190887298065,339.605061544593));
#26741=CARTESIAN_POINT('Ctrl Pts',(24.1518631431268,-1.60900023463661,339.647612430855));
#26742=CARTESIAN_POINT('Ctrl Pts',(24.1440880643483,-1.48006747780203,339.692248862805));
#26743=CARTESIAN_POINT('Ctrl Pts',(24.1363129855699,-1.34907213796948,339.731586539217));
#26744=CARTESIAN_POINT('Ctrl Pts',(24.1285379067915,-1.21648907850789,339.765431500334));
#26745=CARTESIAN_POINT('Ctrl Pts',(24.1207723957425,-1.08406917094163,339.79923481307));
#26746=CARTESIAN_POINT('Ctrl Pts',(24.1130068846935,-0.950065806337024,
339.827558763498));
#26747=CARTESIAN_POINT('Ctrl Pts',(24.1052413736444,-0.814972028073014,
339.850258101994));
#26748=CARTESIAN_POINT('Ctrl Pts',(24.0974835621223,-0.680012195683375,
339.87293493403));
#26749=CARTESIAN_POINT('Ctrl Pts',(24.0897257506001,-0.543964484168194,
339.889998187969));
#26750=CARTESIAN_POINT('Ctrl Pts',(24.0819679390779,-0.407334897859974,
339.901353011515));
#26751=CARTESIAN_POINT('Ctrl Pts',(24.0742159655549,-0.27080812964841,339.912699290196));
#26752=CARTESIAN_POINT('Ctrl Pts',(24.0664639920319,-0.133700746183982,
339.918345656773));
#26753=CARTESIAN_POINT('Ctrl Pts',(24.0587120185089,0.00347365792441432,
339.918248773314));
#26754=CARTESIAN_POINT('Ctrl Pts',(24.0509633279513,0.140589968591417,339.918151930884));
#26755=CARTESIAN_POINT('Ctrl Pts',(24.0432146373936,0.277772853389322,339.912316676307));
#26756=CARTESIAN_POINT('Ctrl Pts',(24.035465946836,0.414506447660042,339.90075172472));
#26757=CARTESIAN_POINT('Ctrl Pts',(24.0277188684582,0.551211593364265,339.889189179318));
#26758=CARTESIAN_POINT('Ctrl Pts',(24.0199717900804,0.687467245237846,339.871899341021));
#26759=CARTESIAN_POINT('Ctrl Pts',(24.0122247117026,0.822760792630141,339.848942950851));
#26760=CARTESIAN_POINT('Ctrl Pts',(24.0044775683968,0.958055473912675,339.825986368285));
#26761=CARTESIAN_POINT('Ctrl Pts',(23.9967304250909,1.09238764926478,339.79736320451));
#26762=CARTESIAN_POINT('Ctrl Pts',(23.9889832817851,1.22525344996556,339.763185598509));
#26763=CARTESIAN_POINT('Ctrl Pts',(23.981234396757,1.35814912171897,339.729000308658));
#26764=CARTESIAN_POINT('Ctrl Pts',(23.973485511729,1.48957738433362,339.689258189053));
#26765=CARTESIAN_POINT('Ctrl Pts',(23.9657366267009,1.61904849823985,339.644121555563));
#26766=CARTESIAN_POINT('Ctrl Pts',(23.9579795169262,1.74865703412442,339.598937013584));
#26767=CARTESIAN_POINT('Ctrl Pts',(23.9502224071514,1.87630390195221,339.548346648788));
#26768=CARTESIAN_POINT('Ctrl Pts',(23.9424652973767,2.00151784486931,339.492561560977));
#26769=CARTESIAN_POINT('Ctrl Pts',(23.9347040424505,2.12679869811386,339.436746663399));
#26770=CARTESIAN_POINT('Ctrl Pts',(23.9269427875244,2.24964368603234,339.375731685374));
#26771=CARTESIAN_POINT('Ctrl Pts',(23.9191815325982,2.3696061233979,339.309773762329));
#26772=CARTESIAN_POINT('Ctrl Pts',(23.9114078621936,2.48976046156758,339.243710328102));
#26773=CARTESIAN_POINT('Ctrl Pts',(23.9036341917889,2.60702270024926,339.172688350726));
#26774=CARTESIAN_POINT('Ctrl Pts',(23.8958605213843,2.72097436988642,339.097008852922));
#26775=CARTESIAN_POINT('Ctrl Pts',(23.8884487172072,2.82962156188694,339.024852253948));
#26776=CARTESIAN_POINT('Ctrl Pts',(23.88103691303,2.93525922944795,338.9484621601));
#26777=CARTESIAN_POINT('Ctrl Pts',(23.8736251088529,3.0375540941927,338.868132390102));
#26778=CARTESIAN_POINT('Ctrl Pts',(23.8658500300745,3.14486273497919,338.783865418786));
#26779=CARTESIAN_POINT('Ctrl Pts',(23.858074951296,3.24883172120144,338.694996516759));
#26780=CARTESIAN_POINT('Ctrl Pts',(23.8502998725176,3.34904097214365,338.601820044006));
#26781=CARTESIAN_POINT('Ctrl Pts',(23.8425343614686,3.44912690922296,338.508758230834));
#26782=CARTESIAN_POINT('Ctrl Pts',(23.8347688504196,3.54546203310141,338.411399657506));
#26783=CARTESIAN_POINT('Ctrl Pts',(23.8270033393706,3.63765738621025,338.310080331812));
#26784=CARTESIAN_POINT('Ctrl Pts',(23.8192455278484,3.72976132735801,338.208861464525));
#26785=CARTESIAN_POINT('Ctrl Pts',(23.8114877163261,3.81773340474025,338.103689947257));
#26786=CARTESIAN_POINT('Ctrl Pts',(23.8037299048039,3.90122002706017,337.994939959826));
#26787=CARTESIAN_POINT('Ctrl Pts',(23.7959779312809,3.98464382304916,337.88627181021));
#26788=CARTESIAN_POINT('Ctrl Pts',(23.788225957758,4.06358864557617,337.77403085934));
#26789=CARTESIAN_POINT('Ctrl Pts',(23.780473984235,4.13774011533684,337.658625547239));
#26790=CARTESIAN_POINT('Ctrl Pts',(23.7727252936773,4.21186018190613,337.543269109356));
#26791=CARTESIAN_POINT('Ctrl Pts',(23.7649766031197,4.28119072235909,337.424751303782));
#26792=CARTESIAN_POINT('Ctrl Pts',(23.7572279125621,4.3454599014739,337.303510648376));
#26793=CARTESIAN_POINT('Ctrl Pts',(23.7494808341843,4.40971570884922,337.182295218101));
#26794=CARTESIAN_POINT('Ctrl Pts',(23.7417337558065,4.46891206653934,337.05835840996));
#26795=CARTESIAN_POINT('Ctrl Pts',(23.7339866774286,4.52282264992869,336.932164159639));
#26796=CARTESIAN_POINT('Ctrl Pts',(23.7262395341228,4.57673368514065,336.805968851687));
#26797=CARTESIAN_POINT('Ctrl Pts',(23.718492390817,4.62535870413508,336.677516423267));
#26798=CARTESIAN_POINT('Ctrl Pts',(23.7107452475111,4.66851933469962,336.547291273173));
#26799=CARTESIAN_POINT('Ctrl Pts',(23.702996362483,4.71168966869018,336.4170368457));
#26800=CARTESIAN_POINT('Ctrl Pts',(23.6952474774549,4.74939304670637,336.285009274448));
#26801=CARTESIAN_POINT('Ctrl Pts',(23.6874985924268,4.7815009374426,336.151708230298));
#26802=CARTESIAN_POINT('Ctrl Pts',(23.6797414826521,4.81364290782583,336.018265699042));
#26803=CARTESIAN_POINT('Ctrl Pts',(23.6719843728774,4.84017743532795,335.883547375394));
#26804=CARTESIAN_POINT('Ctrl Pts',(23.6642272631027,4.86102701415203,335.74806378751));
#26805=CARTESIAN_POINT('Ctrl Pts',(23.6564660081765,4.88188773432438,335.612507801529));
#26806=CARTESIAN_POINT('Ctrl Pts',(23.6487047532503,4.89705740941223,335.476186124758));
#26807=CARTESIAN_POINT('Ctrl Pts',(23.6409434983242,4.90651054307436,335.339613535066));
#26808=CARTESIAN_POINT('Ctrl Pts',(23.6331698279195,4.91597879866959,335.20282247374));
#26809=CARTESIAN_POINT('Ctrl Pts',(23.6253961575148,4.91971222856349,335.065780088354));
#26810=CARTESIAN_POINT('Ctrl Pts',(23.6176224871101,4.91773751129472,334.929001179553));
#26811=CARTESIAN_POINT('Ctrl Pts',(23.6102106829331,4.91585471758991,334.798589361865));
#26812=CARTESIAN_POINT('Ctrl Pts',(23.6027988787561,4.90878326136743,334.668417330489));
#26813=CARTESIAN_POINT('Ctrl Pts',(23.595387074579,4.89658986500686,334.538924348494));
#26814=CARTESIAN_POINT('Ctrl Pts',(23.5876119958006,4.88379883396834,334.40308452971));
#26815=CARTESIAN_POINT('Ctrl Pts',(23.5798369170221,4.86533066250375,334.267562728932));
#26816=CARTESIAN_POINT('Ctrl Pts',(23.5720618382437,4.84120555442294,334.132871496072));
#26817=CARTESIAN_POINT('Ctrl Pts',(23.5642963271947,4.8171101338235,333.998346009349));
#26818=CARTESIAN_POINT('Ctrl Pts',(23.5565308161457,4.78737169569653,333.864649437998));
#26819=CARTESIAN_POINT('Ctrl Pts',(23.5487653050967,4.7520623089033,333.732290697833));
#26820=CARTESIAN_POINT('Ctrl Pts',(23.5410074935744,4.71678793146985,333.600063191744));
#26821=CARTESIAN_POINT('Ctrl Pts',(23.5332496820523,4.67595369777122,333.469171252337));
#26822=CARTESIAN_POINT('Ctrl Pts',(23.5254918705301,4.62968291506037,333.340114712247));
#26823=CARTESIAN_POINT('Ctrl Pts',(23.5177398970071,4.58344695258084,333.211155291297));
#26824=CARTESIAN_POINT('Ctrl Pts',(23.509987923484,4.53178271576097,333.084028886919));
#26825=CARTESIAN_POINT('Ctrl Pts',(23.502235949961,4.47486354184832,332.959220897712));
#26826=CARTESIAN_POINT('Ctrl Pts',(23.4944872594033,4.41796847323969,332.834465764762));
#26827=CARTESIAN_POINT('Ctrl Pts',(23.4867385688457,4.35582305569116,332.712027449047));
#26828=CARTESIAN_POINT('Ctrl Pts',(23.4789898782881,4.28864894258796,332.592371849778));
#26829=CARTESIAN_POINT('Ctrl Pts',(23.4712427999102,4.22148880562005,332.472741145857));
#26830=CARTESIAN_POINT('Ctrl Pts',(23.4634957215324,4.14930224541115,332.355892347399));
#26831=CARTESIAN_POINT('Ctrl Pts',(23.4557486431546,4.07235691813991,332.242266837822));
#26832=CARTESIAN_POINT('Ctrl Pts',(23.4480014998488,3.99541094599271,332.128640375953));
#26833=CARTESIAN_POINT('Ctrl Pts',(23.440254356543,3.91370634640223,332.018237580494));
#26834=CARTESIAN_POINT('Ctrl Pts',(23.4325072132372,3.82755393321118,331.911470584427));
#26835=CARTESIAN_POINT('Ctrl Pts',(23.4247583282091,3.74138215112858,331.804679584873));
#26836=CARTESIAN_POINT('Ctrl Pts',(23.417009443181,3.65076081104152,331.701526315387));
#26837=CARTESIAN_POINT('Ctrl Pts',(23.4092605581529,3.55604054119053,331.602389261274));
#26838=CARTESIAN_POINT('Ctrl Pts',(23.4015034483781,3.46121973426648,331.503146982066));
#26839=CARTESIAN_POINT('Ctrl Pts',(23.3937463386034,3.36229157720325,331.407929716738));
#26840=CARTESIAN_POINT('Ctrl Pts',(23.3859892288287,3.25964344118676,331.317078917649));
#26841=CARTESIAN_POINT('Ctrl Pts',(23.3782279739025,3.15694045328837,331.226179570797));
#26842=CARTESIAN_POINT('Ctrl Pts',(23.3704667189763,3.05051382862137,331.139651585947));
#26843=CARTESIAN_POINT('Ctrl Pts',(23.3627054640501,2.94078265734624,331.057794979361));
#26844=CARTESIAN_POINT('Ctrl Pts',(23.3549317936455,2.83087595195851,330.975807428881));
#26845=CARTESIAN_POINT('Ctrl Pts',(23.3471581232408,2.71765445955635,330.898506409812));
#26846=CARTESIAN_POINT('Ctrl Pts',(23.3393844528362,2.60156552427244,330.826148075768));
#26847=CARTESIAN_POINT('Ctrl Pts',(23.3319726486591,2.49088055685538,330.757158039582));
#26848=CARTESIAN_POINT('Ctrl Pts',(23.324560844482,2.37758934785036,330.692661022535));
#26849=CARTESIAN_POINT('Ctrl Pts',(23.3171490403049,2.26209739025036,330.632838626805));
#26850=CARTESIAN_POINT('Ctrl Pts',(23.3093739615264,2.14094482777552,330.570084157259));
#26851=CARTESIAN_POINT('Ctrl Pts',(23.301598882748,2.01698746698734,330.512275814005));
#26852=CARTESIAN_POINT('Ctrl Pts',(23.2938238039696,1.8906672554832,330.459673977395));
#26853=CARTESIAN_POINT('Ctrl Pts',(23.2860582929206,1.76450248904125,330.407136870694));
#26854=CARTESIAN_POINT('Ctrl Pts',(23.2782927818715,1.63598101463931,330.359793671491));
#26855=CARTESIAN_POINT('Ctrl Pts',(23.2705272708225,1.5055697910384,330.317859179092));
#26856=CARTESIAN_POINT('Ctrl Pts',(23.2627694593003,1.37528787054529,330.275966264864));
#26857=CARTESIAN_POINT('Ctrl Pts',(23.2550116477781,1.24312029931855,330.239471504151));
#26858=CARTESIAN_POINT('Ctrl Pts',(23.2472538362559,1.1095541259149,330.208541693371));
#26859=CARTESIAN_POINT('Ctrl Pts',(23.2395018627329,0.976088465292541,330.177635158255));
#26860=CARTESIAN_POINT('Ctrl Pts',(23.2317498892099,0.841226676692455,330.152285325285));
#26861=CARTESIAN_POINT('Ctrl Pts',(23.2239979156869,0.705470744880478,330.132609108504));
#26862=CARTESIAN_POINT('Ctrl Pts',(23.2162492251293,0.569772305786223,330.112941224613));
#26863=CARTESIAN_POINT('Ctrl Pts',(23.2085005345717,0.43318086265562,330.098942233901));
#26864=CARTESIAN_POINT('Ctrl Pts',(23.2007518440141,0.296208149440936,330.090677868106));
#26865=CARTESIAN_POINT('Ctrl Pts',(23.1930047656362,0.159263934543254,330.082415221781));
#26866=CARTESIAN_POINT('Ctrl Pts',(23.1852576872584,0.0219389972671578,
330.079884850665));
#26867=CARTESIAN_POINT('Ctrl Pts',(23.1775106088806,-0.115250649539025,
330.083100534861));
#26868=CARTESIAN_POINT('Ctrl Pts',(23.1697634655748,-0.252441446126399,
330.086316246008));
#26869=CARTESIAN_POINT('Ctrl Pts',(23.162016322269,-0.389496559215323,330.095278099361));
#26870=CARTESIAN_POINT('Ctrl Pts',(23.1542691789632,-0.525901218183885,
330.109947753734));
#26871=CARTESIAN_POINT('Ctrl Pts',(23.1465202939351,-0.662336543815736,
330.124620706156));
#26872=CARTESIAN_POINT('Ctrl Pts',(23.138771408907,-0.79812073577678,330.145003971305));
#26873=CARTESIAN_POINT('Ctrl Pts',(23.1310225238789,-0.932745772641469,
330.171007518527));
#26874=CARTESIAN_POINT('Ctrl Pts',(23.1232654141042,-1.06751370191141,330.197038666183));
#26875=CARTESIAN_POINT('Ctrl Pts',(23.1155083043294,-1.20111963398024,330.228701938163));
#26876=CARTESIAN_POINT('Ctrl Pts',(23.1077511945547,-1.33306680549895,330.265856365236));
#26877=CARTESIAN_POINT('Ctrl Pts',(23.0999899396285,-1.46508448536717,330.303030646447));
#26878=CARTESIAN_POINT('Ctrl Pts',(23.0922286847024,-1.59544126718632,330.345701808065));
#26879=CARTESIAN_POINT('Ctrl Pts',(23.0844674297762,-1.72365806714877,330.393679784247));
#26880=CARTESIAN_POINT('Ctrl Pts',(23.0766937593715,-1.85207997220541,330.441734509555));
#26881=CARTESIAN_POINT('Ctrl Pts',(23.0689200889668,-1.97835469447261,330.495112861041));
#26882=CARTESIAN_POINT('Ctrl Pts',(23.0611464185622,-2.10202474533145,330.553577276898));
#26883=CARTESIAN_POINT('Ctrl Pts',(23.0537346143851,-2.21993792556885,330.609320160132));
#26884=CARTESIAN_POINT('Ctrl Pts',(23.0463228102081,-2.33548321702727,330.669686117984));
#26885=CARTESIAN_POINT('Ctrl Pts',(23.0389110060311,-2.44828847103492,330.734432438104));
#26886=CARTESIAN_POINT('Ctrl Pts',(23.0311359272526,-2.56662264657159,330.802352168244));
#26887=CARTESIAN_POINT('Ctrl Pts',(23.0233608484742,-2.68231535629548,330.875307145868));
#26888=CARTESIAN_POINT('Ctrl Pts',(23.0155857696958,-2.79490847760867,330.953066634563));
#26889=CARTESIAN_POINT('Ctrl Pts',(23.0078202586468,-2.90736304591821,331.030730435256));
#26890=CARTESIAN_POINT('Ctrl Pts',(23.0000547475978,-3.01672529651027,331.113186763325));
#26891=CARTESIAN_POINT('Ctrl Pts',(22.9922892365487,-3.12256190188676,331.200159183415));
#26892=CARTESIAN_POINT('Ctrl Pts',(22.9845314250265,-3.22829356996095,331.287045370097));
#26893=CARTESIAN_POINT('Ctrl Pts',(22.9767736135044,-3.33050624939113,331.378438491322));
#26894=CARTESIAN_POINT('Ctrl Pts',(22.9690158019822,-3.42879610758851,331.474019240681));
#26895=CARTESIAN_POINT('Ctrl Pts',(22.9612638284591,-3.5270119995505,331.569528062496));
#26896=CARTESIAN_POINT('Ctrl Pts',(22.953511854936,-3.62131066708929,331.669217968486));
#26897=CARTESIAN_POINT('Ctrl Pts',(22.945759881413,-3.71132214193107,331.772730097852));
#26898=CARTESIAN_POINT('Ctrl Pts',(22.9380111908554,-3.80129549685981,331.876198389769));
#26899=CARTESIAN_POINT('Ctrl Pts',(22.9302625002978,-3.8869850142979,331.983485391212));
#26900=CARTESIAN_POINT('Ctrl Pts',(22.9225138097402,-3.96805849042088,332.094196345398));
#26901=CARTESIAN_POINT('Ctrl Pts',(22.9147667313624,-4.04911509853001,332.204884265245));
#26902=CARTESIAN_POINT('Ctrl Pts',(22.9070196529846,-4.12555734484776,332.318994405696));
#26903=CARTESIAN_POINT('Ctrl Pts',(22.8992725746067,-4.1970943972307,332.436100297743));
#26904=CARTESIAN_POINT('Ctrl Pts',(22.8915254313009,-4.26863204916294,332.553207171249));
#26905=CARTESIAN_POINT('Ctrl Pts',(22.8837782879951,-4.33526422139886,332.673309512869));
#26906=CARTESIAN_POINT('Ctrl Pts',(22.8760311446893,-4.39674458393906,332.795953692387));
#26907=CARTESIAN_POINT('Ctrl Pts',(22.8682822596612,-4.45823876857003,332.918625444921));
#26908=CARTESIAN_POINT('Ctrl Pts',(22.860533374633,-4.51457866361392,333.043839823133));
#26909=CARTESIAN_POINT('Ctrl Pts',(22.8527844896049,-4.565565058224,333.171120900217));
#26910=CARTESIAN_POINT('Ctrl Pts',(22.8450273798302,-4.61660557032018,333.298537074751));
#26911=CARTESIAN_POINT('Ctrl Pts',(22.8372702700555,-4.66228108555537,333.428023966692));
#26912=CARTESIAN_POINT('Ctrl Pts',(22.8295131602808,-4.70244132081064,333.559087550601));
#26913=CARTESIAN_POINT('Ctrl Pts',(22.8217519053546,-4.74262301641147,333.690221170699));
#26914=CARTESIAN_POINT('Ctrl Pts',(22.8139906504285,-4.77728346077039,333.822932783593));
#26915=CARTESIAN_POINT('Ctrl Pts',(22.8062293955024,-4.80632322457161,333.956716661954));
#26916=CARTESIAN_POINT('Ctrl Pts',(22.7984557250977,-4.83540944253091,334.090714550922));
#26917=CARTESIAN_POINT('Ctrl Pts',(22.790682054693,-4.85885694585041,334.225787747667));
#26918=CARTESIAN_POINT('Ctrl Pts',(22.7829083842883,-4.87661793197799,334.361422981927));
#26919=CARTESIAN_POINT('Ctrl Pts',(22.7754965801112,-4.89355213992822,334.4907443634));
#26920=CARTESIAN_POINT('Ctrl Pts',(22.7680847759342,-4.90531730531503,334.62057634763));
#26921=CARTESIAN_POINT('Ctrl Pts',(22.7606729717571,-4.91191613913101,334.75047464128));
#26922=CARTESIAN_POINT('Ctrl Pts',(22.7559607306682,-4.91611151384736,334.833060751504));
#26923=CARTESIAN_POINT('Ctrl Pts',(22.7512484895792,-4.91822421825937,334.915753557196));
#26924=CARTESIAN_POINT('Ctrl Pts',(22.7465362484902,-4.91824976548699,334.998481188888));
#26925=CARTESIAN_POINT('',(26.2465362485261,-4.91824994013874,334.999232650495));
#26926=CARTESIAN_POINT('Ctrl Pts',(26.2465362484902,-4.91824994013884,334.999232651133));
#26927=CARTESIAN_POINT('Ctrl Pts',(26.2385101248523,-4.91827217345382,335.141734979221));
#26928=CARTESIAN_POINT('Ctrl Pts',(26.2304840012145,-4.9120967350768,335.284149552615));
#26929=CARTESIAN_POINT('Ctrl Pts',(26.2224578775766,-4.89977251782948,335.425925270468));
#26930=CARTESIAN_POINT('Ctrl Pts',(26.2144242186472,-4.8874367300441,335.56783409384));
#26931=CARTESIAN_POINT('Ctrl Pts',(26.2063905597178,-4.86894068098241,335.709102518273));
#26932=CARTESIAN_POINT('Ctrl Pts',(26.1983569007885,-4.84438482869667,335.849187078325));
#26933=CARTESIAN_POINT('Ctrl Pts',(26.1901212743098,-4.8192116381157,335.992793387998));
#26934=CARTESIAN_POINT('Ctrl Pts',(26.1818856478311,-4.78767002512742,336.135155135803));
#26935=CARTESIAN_POINT('Ctrl Pts',(26.1736500213524,-4.74992278204833,336.275702405374));
#26936=CARTESIAN_POINT('Ctrl Pts',(26.1655921118387,-4.71299008847468,336.413216798911));
#26937=CARTESIAN_POINT('Ctrl Pts',(26.157534202325,-4.6701170328828,336.548993920819));
#26938=CARTESIAN_POINT('Ctrl Pts',(26.1494762928112,-4.62150526674811,336.682519578465));
#26939=CARTESIAN_POINT('Ctrl Pts',(26.1411518078501,-4.57128530393603,336.820462592979));
#26940=CARTESIAN_POINT('Ctrl Pts',(26.132827322889,-4.51494057631685,336.956002231368));
#26941=CARTESIAN_POINT('Ctrl Pts',(26.1245028379278,-4.45274510224256,337.088598601205));
#26942=CARTESIAN_POINT('Ctrl Pts',(26.1161783529667,-4.3905496281682,337.221194971042));
#26943=CARTESIAN_POINT('Ctrl Pts',(26.1078538680055,-4.32250365674387,337.350847748008));
#26944=CARTESIAN_POINT('Ctrl Pts',(26.0995293830443,-4.24893028952669,337.477049546788));
#26945=CARTESIAN_POINT('Ctrl Pts',(26.0917543042658,-4.18021267771288,337.594922175795));
#26946=CARTESIAN_POINT('Ctrl Pts',(26.0839792254874,-4.10647777830166,337.710119382585));
#26947=CARTESIAN_POINT('Ctrl Pts',(26.0762041467089,-4.02795941738535,337.822184613805));
#26948=CARTESIAN_POINT('Ctrl Pts',(26.0684386356599,-3.94953767831086,337.934111941623));
#26949=CARTESIAN_POINT('Ctrl Pts',(26.0606731246109,-3.86634441203466,338.042914645356));
#26950=CARTESIAN_POINT('Ctrl Pts',(26.0529076135618,-3.77865897503923,338.148161274912));
#26951=CARTESIAN_POINT('Ctrl Pts',(26.0451498020396,-3.69106047840993,338.253303552128));
#26952=CARTESIAN_POINT('Ctrl Pts',(26.0373919905174,-3.59897892336001,338.354896473452));
#26953=CARTESIAN_POINT('Ctrl Pts',(26.0296341789952,-3.50273633718802,338.452538372653));
#26954=CARTESIAN_POINT('Ctrl Pts',(26.0218822054721,-3.40656617661389,338.550106793229));
#26955=CARTESIAN_POINT('Ctrl Pts',(26.0141302319491,-3.30624149091604,338.643729832572));
#26956=CARTESIAN_POINT('Ctrl Pts',(26.006378258426,-3.20212363210602,338.733039955212));
#26957=CARTESIAN_POINT('Ctrl Pts',(25.9986295678684,-3.09804986727132,338.822312254962));
#26958=CARTESIAN_POINT('Ctrl Pts',(25.9908808773107,-2.99018642042605,338.907275016876));
#26959=CARTESIAN_POINT('Ctrl Pts',(25.9831321867531,-2.87893028361868,338.987598711576));
#26960=CARTESIAN_POINT('Ctrl Pts',(25.9753851083752,-2.7676972945798,339.06790569426));
#26961=CARTESIAN_POINT('Ctrl Pts',(25.9676380299974,-2.65307333633156,339.143575300916));
#26962=CARTESIAN_POINT('Ctrl Pts',(25.9598909516195,-2.53548683292859,339.214319587139));
#26963=CARTESIAN_POINT('Ctrl Pts',(25.9521438083137,-2.41789934403746,339.285064466268));
#26964=CARTESIAN_POINT('Ctrl Pts',(25.9443966650078,-2.29734959539829,339.350883741123));
#26965=CARTESIAN_POINT('Ctrl Pts',(25.936649521702,-2.17429287100784,339.411534151923));
#26966=CARTESIAN_POINT('Ctrl Pts',(25.9289006366739,-2.05120848085335,339.472198198223));
#26967=CARTESIAN_POINT('Ctrl Pts',(25.9211517516458,-1.92561634393892,339.52769089531));
#26968=CARTESIAN_POINT('Ctrl Pts',(25.9134028666177,-1.79799372202223,339.577816252109));
#26969=CARTESIAN_POINT('Ctrl Pts',(25.9056457568429,-1.67023564013588,339.627994812479));
#26970=CARTESIAN_POINT('Ctrl Pts',(25.8978886470682,-1.5404431324707,339.672794509247));
#26971=CARTESIAN_POINT('Ctrl Pts',(25.8901315372935,-1.40911122846013,339.712068400217));
#26972=CARTESIAN_POINT('Ctrl Pts',(25.8823702823673,-1.27770914487934,339.7513632779));
#26973=CARTESIAN_POINT('Ctrl Pts',(25.8746090274411,-1.14476640449553,339.78512636987));
#26974=CARTESIAN_POINT('Ctrl Pts',(25.8668477725149,-1.0107893948121,339.813261665631));
#26975=CARTESIAN_POINT('Ctrl Pts',(25.8590741021102,-0.876598065576192,
339.841441968696));
#26976=CARTESIAN_POINT('Ctrl Pts',(25.8513004317056,-0.741369546632563,
339.863976421327));
#26977=CARTESIAN_POINT('Ctrl Pts',(25.8435267613009,-0.605617419472553,
339.88082068957));
#26978=CARTESIAN_POINT('Ctrl Pts',(25.8361149571241,-0.476184586497428,
339.896880853072));
#26979=CARTESIAN_POINT('Ctrl Pts',(25.8287031529473,-0.346276082980034,
339.907768642485));
#26980=CARTESIAN_POINT('Ctrl Pts',(25.8212913487705,-0.216336173803566,
339.913489770255));
#26981=CARTESIAN_POINT('Ctrl Pts',(25.813516269992,-0.0800275226018157,
339.919491307541));
#26982=CARTESIAN_POINT('Ctrl Pts',(25.8057411912136,0.0567464511916358,
339.919825876169));
#26983=CARTESIAN_POINT('Ctrl Pts',(25.7979661124351,0.193475285405127,339.914443038274));
#26984=CARTESIAN_POINT('Ctrl Pts',(25.7902006013861,0.330035866083349,339.909066824303));
#26985=CARTESIAN_POINT('Ctrl Pts',(25.7824350903372,0.466551030866433,339.897987217929));
#26986=CARTESIAN_POINT('Ctrl Pts',(25.7746695792882,0.6025067883454,339.881205653576));
#26987=CARTESIAN_POINT('Ctrl Pts',(25.766911767766,0.738327745295094,339.864440728192));
#26988=CARTESIAN_POINT('Ctrl Pts',(25.7591539562437,0.873590013302157,339.841985143206));
#26989=CARTESIAN_POINT('Ctrl Pts',(25.7513961447216,1.00778155521446,339.813892333598));
#26990=CARTESIAN_POINT('Ctrl Pts',(25.7436441711986,1.14187211373546,339.785820664719));
#26991=CARTESIAN_POINT('Ctrl Pts',(25.7358921976756,1.27489316893825,339.75212029486));
#26992=CARTESIAN_POINT('Ctrl Pts',(25.7281402241526,1.4063401040965,339.712896198105));
#26993=CARTESIAN_POINT('Ctrl Pts',(25.720391533595,1.53773137140039,339.673688712777));
#26994=CARTESIAN_POINT('Ctrl Pts',(25.7126428430373,1.66754947078681,339.628962264794));
#26995=CARTESIAN_POINT('Ctrl Pts',(25.7048941524797,1.79530245879277,339.578872365982));
#26996=CARTESIAN_POINT('Ctrl Pts',(25.6971470741018,1.92302886672238,339.528792888792));
#26997=CARTESIAN_POINT('Ctrl Pts',(25.689399995724,2.04869065422893,339.473352322989));
#26998=CARTESIAN_POINT('Ctrl Pts',(25.6816529173462,2.17181383788041,339.412755116261));
#26999=CARTESIAN_POINT('Ctrl Pts',(25.6739057740404,2.29493805342277,339.352157401671));
#27000=CARTESIAN_POINT('Ctrl Pts',(25.6661586307346,2.41552327197314,339.286403132558));
#27001=CARTESIAN_POINT('Ctrl Pts',(25.6584114874287,2.5331185508954,339.215743525122));
#27002=CARTESIAN_POINT('Ctrl Pts',(25.6506626024006,2.65074026773281,339.145068031906));
#27003=CARTESIAN_POINT('Ctrl Pts',(25.6429137173726,2.7653703723578,339.069485207149));
#27004=CARTESIAN_POINT('Ctrl Pts',(25.6351648323445,2.87658577797066,338.989290328426));
#27005=CARTESIAN_POINT('Ctrl Pts',(25.6274077225698,2.98791922876426,338.909010330031));
#27006=CARTESIAN_POINT('Ctrl Pts',(25.619650612795,3.0958304229264,338.824108727861));
#27007=CARTESIAN_POINT('Ctrl Pts',(25.6118935030203,3.19992790479848,338.734922283876));
#27008=CARTESIAN_POINT('Ctrl Pts',(25.6041322480941,3.30408101303641,338.645688181506));
#27009=CARTESIAN_POINT('Ctrl Pts',(25.5963709931679,3.40441606245316,338.5521649413));
#27010=CARTESIAN_POINT('Ctrl Pts',(25.5886097382418,3.50057828043755,338.454726438523));
#27011=CARTESIAN_POINT('Ctrl Pts',(25.5808360678371,3.59689432663153,338.357132065896));
#27012=CARTESIAN_POINT('Ctrl Pts',(25.5730623974324,3.68902393961181,338.255610204689));
#27013=CARTESIAN_POINT('Ctrl Pts',(25.5652887270277,3.7766519095954,338.150568744886));
#27014=CARTESIAN_POINT('Ctrl Pts',(25.5578769228506,3.86020077649395,338.050416990308));
#27015=CARTESIAN_POINT('Ctrl Pts',(25.5504651186736,3.93965749629635,337.947066165813));
#27016=CARTESIAN_POINT('Ctrl Pts',(25.5430533144965,4.01478645550223,337.840892954551));
#27017=CARTESIAN_POINT('Ctrl Pts',(25.5352782357181,4.09359770879637,337.729515877931));
#27018=CARTESIAN_POINT('Ctrl Pts',(25.5275031569397,4.16789530000232,337.614680779707));
#27019=CARTESIAN_POINT('Ctrl Pts',(25.5197280781613,4.23736057446958,337.496789623583));
#27020=CARTESIAN_POINT('Ctrl Pts',(25.5119625671123,4.30674036749434,337.379043540032));
#27021=CARTESIAN_POINT('Ctrl Pts',(25.5041970560633,4.37129947902379,337.258249214786));
#27022=CARTESIAN_POINT('Ctrl Pts',(25.4964315450143,4.43076096505197,337.134839650436));
#27023=CARTESIAN_POINT('Ctrl Pts',(25.4886737334922,4.49016349484335,337.011552447028));
#27024=CARTESIAN_POINT('Ctrl Pts',(25.4809159219701,4.54447828892536,336.885655514631));
#27025=CARTESIAN_POINT('Ctrl Pts',(25.4731581104479,4.59347318922914,336.757608352942));
#27026=CARTESIAN_POINT('Ctrl Pts',(25.465406136925,4.64243121931652,336.629657550804));
#27027=CARTESIAN_POINT('Ctrl Pts',(25.457654163402,4.68607718505317,336.499560103748));
#27028=CARTESIAN_POINT('Ctrl Pts',(25.4499021898791,4.72422628431963,336.367797162244));
#27029=CARTESIAN_POINT('Ctrl Pts',(25.4421534993215,4.76235922742016,336.236090022424));
#27030=CARTESIAN_POINT('Ctrl Pts',(25.4344048087639,4.7949998256532,336.102719165696));
#27031=CARTESIAN_POINT('Ctrl Pts',(25.4266561182063,4.82201263339612,335.968182434187));
#27032=CARTESIAN_POINT('Ctrl Pts',(25.4189090398285,4.84901982089877,335.833673694169));
#27033=CARTESIAN_POINT('Ctrl Pts',(25.4111619614507,4.87040147003448,335.697999944844));
#27034=CARTESIAN_POINT('Ctrl Pts',(25.4034148830729,4.88607300559344,335.561670407366));
#27035=CARTESIAN_POINT('Ctrl Pts',(25.3956677397672,4.90174467249491,335.425339727317));
#27036=CARTESIAN_POINT('Ctrl Pts',(25.3879205964614,4.91170608572846,335.28835363647));
#27037=CARTESIAN_POINT('Ctrl Pts',(25.3801734531556,4.91592446741988,335.151227289609));
#27038=CARTESIAN_POINT('Ctrl Pts',(25.3724245681275,4.92014379749311,335.014070113833));
#27039=CARTESIAN_POINT('Ctrl Pts',(25.3646756830994,4.91861751475273,334.876773009909));
#27040=CARTESIAN_POINT('Ctrl Pts',(25.3569267980712,4.91136496786835,334.739851552195));
#27041=CARTESIAN_POINT('Ctrl Pts',(25.3491696882965,4.90410472305581,334.602784764631));
#27042=CARTESIAN_POINT('Ctrl Pts',(25.3414125785218,4.89110609359985,334.466094810689));
#27043=CARTESIAN_POINT('Ctrl Pts',(25.3336554687471,4.87244043069669,334.330293115003));
#27044=CARTESIAN_POINT('Ctrl Pts',(25.325894213821,4.85376479346011,334.194418851233));
#27045=CARTESIAN_POINT('Ctrl Pts',(25.3181329588949,4.82941615800395,334.059434175987));
#27046=CARTESIAN_POINT('Ctrl Pts',(25.3103717039687,4.79951693619806,333.92583975048));
#27047=CARTESIAN_POINT('Ctrl Pts',(25.3025980335641,4.76956988538138,333.792031617431));
#27048=CARTESIAN_POINT('Ctrl Pts',(25.2948243631595,4.73405460639817,333.659618555955));
#27049=CARTESIAN_POINT('Ctrl Pts',(25.2870506927548,4.69314352453913,333.529086365358));
#27050=CARTESIAN_POINT('Ctrl Pts',(25.2796388885774,4.65413686338139,333.404630479631));
#27051=CARTESIAN_POINT('Ctrl Pts',(25.2722270844,4.6102255404787,333.281884567405));
#27052=CARTESIAN_POINT('Ctrl Pts',(25.2648152802226,4.56159881274524,333.161250605966));
#27053=CARTESIAN_POINT('Ctrl Pts',(25.2570402014441,4.51058874423609,333.034704014731));
#27054=CARTESIAN_POINT('Ctrl Pts',(25.2492651226656,4.45422815003558,332.91008172433));
#27055=CARTESIAN_POINT('Ctrl Pts',(25.2414900438872,4.39268260768378,332.787869223881));
#27056=CARTESIAN_POINT('Ctrl Pts',(25.2337245328381,4.3312128010402,332.665807113695));
#27057=CARTESIAN_POINT('Ctrl Pts',(25.2259590217891,4.26457091555621,332.546149238934));
#27058=CARTESIAN_POINT('Ctrl Pts',(25.2181935107401,4.19297120205544,332.429362810268));
#27059=CARTESIAN_POINT('Ctrl Pts',(25.2104356992179,4.12144247987893,332.312692175686));
#27060=CARTESIAN_POINT('Ctrl Pts',(25.2026778876957,4.04496591519182,332.198887652501));
#27061=CARTESIAN_POINT('Ctrl Pts',(25.1949200761734,3.96380227704169,332.08839312904));
#27062=CARTESIAN_POINT('Ctrl Pts',(25.1871681026504,3.88269971710344,331.977981756213));
#27063=CARTESIAN_POINT('Ctrl Pts',(25.1794161291274,3.79691733483057,331.870875738886));
#27064=CARTESIAN_POINT('Ctrl Pts',(25.1716641556044,3.70675973288782,331.767490859233));
#27065=CARTESIAN_POINT('Ctrl Pts',(25.1639154650468,3.61664031274264,331.664149763138));
#27066=CARTESIAN_POINT('Ctrl Pts',(25.1561667744891,3.52214961459789,331.564526964333));
#27067=CARTESIAN_POINT('Ctrl Pts',(25.1484180839315,3.42363298712003,331.469005772873));
#27068=CARTESIAN_POINT('Ctrl Pts',(25.1406710055536,3.32513685684934,331.373504455395));
#27069=CARTESIAN_POINT('Ctrl Pts',(25.1329239271758,3.22261674379429,331.282103319761));
#27070=CARTESIAN_POINT('Ctrl Pts',(25.1251768487979,3.11645509438899,331.195149055856));
#27071=CARTESIAN_POINT('Ctrl Pts',(25.1174297054921,3.01029255524667,331.10819406319));
#27072=CARTESIAN_POINT('Ctrl Pts',(25.1096825621862,2.90048872126823,331.025686264266));
#27073=CARTESIAN_POINT('Ctrl Pts',(25.1019354188804,2.78745905911271,330.947932002511));
#27074=CARTESIAN_POINT('Ctrl Pts',(25.0941865338523,2.67440398548992,330.870160259948));
#27075=CARTESIAN_POINT('Ctrl Pts',(25.0864376488242,2.55812196252632,330.797144402628));
#27076=CARTESIAN_POINT('Ctrl Pts',(25.0786887637961,2.43905701837231,330.729147166709));
#27077=CARTESIAN_POINT('Ctrl Pts',(25.0709316540213,2.31986569745623,330.661077757821));
#27078=CARTESIAN_POINT('Ctrl Pts',(25.0631745442466,2.19788589477356,330.598037805299));
#27079=CARTESIAN_POINT('Ctrl Pts',(25.0554174344718,2.07358629043573,330.540244069614));
#27080=CARTESIAN_POINT('Ctrl Pts',(25.0476561795456,1.94922026436376,330.482419450804));
#27081=CARTESIAN_POINT('Ctrl Pts',(25.0398949246194,1.82253232740655,330.42984678462));
#27082=CARTESIAN_POINT('Ctrl Pts',(25.0321336696933,1.69400974034882,330.382694068821));
#27083=CARTESIAN_POINT('Ctrl Pts',(25.0243599992886,1.56528155903705,330.335465924043));
#27084=CARTESIAN_POINT('Ctrl Pts',(25.0165863288839,1.43471323540737,330.293675174401));
#27085=CARTESIAN_POINT('Ctrl Pts',(25.0088126584792,1.30280659767993,330.257439717669));
#27086=CARTESIAN_POINT('Ctrl Pts',(25.0014008543023,1.17704024567806,330.222891030167));
#27087=CARTESIAN_POINT('Ctrl Pts',(24.9939890501255,1.05005765297368,330.193392142141));
#27088=CARTESIAN_POINT('Ctrl Pts',(24.9865772459486,0.922299268618735,330.16900143639));
#27089=CARTESIAN_POINT('Ctrl Pts',(24.9788021671702,0.788279065269675,330.143415269492));
#27090=CARTESIAN_POINT('Ctrl Pts',(24.9710270883917,0.652981571079474,330.123369823394));
#27091=CARTESIAN_POINT('Ctrl Pts',(24.9632520096133,0.516904647714207,330.10898858643));
#27092=CARTESIAN_POINT('Ctrl Pts',(24.9554864985643,0.380995175665853,330.094625046493));
#27093=CARTESIAN_POINT('Ctrl Pts',(24.9477209875153,0.244308567844098,330.085911887738));
#27094=CARTESIAN_POINT('Ctrl Pts',(24.9399554764662,0.107353655083676,330.082921776579));
#27095=CARTESIAN_POINT('Ctrl Pts',(24.932197664944,-0.0294654664817331,
330.079934630124));
#27096=CARTESIAN_POINT('Ctrl Pts',(24.9244398534218,-0.1665519753169,330.082659247328));
#27097=CARTESIAN_POINT('Ctrl Pts',(24.9166820418996,-0.303391479163863,
330.091116555379));
#27098=CARTESIAN_POINT('Ctrl Pts',(24.9089300683766,-0.440128006944566,
330.099567499038));
#27099=CARTESIAN_POINT('Ctrl Pts',(24.9011780948535,-0.576617511161267,
330.113742522661));
#27100=CARTESIAN_POINT('Ctrl Pts',(24.8934261213305,-0.712345513734498,
330.133610482959));
#27101=CARTESIAN_POINT('Ctrl Pts',(24.8856774307729,-0.848016035417872,
330.153470029165));
#27102=CARTESIAN_POINT('Ctrl Pts',(24.8779287402153,-0.982925310932581,
330.179017660317));
#27103=CARTESIAN_POINT('Ctrl Pts',(24.8701800496577,-1.11656411869695,330.210170396419));
#27104=CARTESIAN_POINT('Ctrl Pts',(24.8624329712799,-1.25017512179138,330.241316650935));
#27105=CARTESIAN_POINT('Ctrl Pts',(24.854685892902,-1.38251580248019,330.278065602085));
#27106=CARTESIAN_POINT('Ctrl Pts',(24.8469388145242,-1.51308765813306,330.320283256296));
#27107=CARTESIAN_POINT('Ctrl Pts',(24.8391916712183,-1.64366060810384,330.362501264331));
#27108=CARTESIAN_POINT('Ctrl Pts',(24.8314445279125,-1.77246433155314,330.410187946591));
#27109=CARTESIAN_POINT('Ctrl Pts',(24.8236973846067,-1.89901638490937,330.463159708305));
#27110=CARTESIAN_POINT('Ctrl Pts',(24.8159484995787,-2.02559688985346,330.516143379196));
#27111=CARTESIAN_POINT('Ctrl Pts',(24.8081996145506,-2.14992435688523,330.574414343029));
#27112=CARTESIAN_POINT('Ctrl Pts',(24.8004507295225,-2.27153755645328,330.63774138867));
#27113=CARTESIAN_POINT('Ctrl Pts',(24.7926936197478,-2.39327983752818,330.701135650292));
#27114=CARTESIAN_POINT('Ctrl Pts',(24.784936509973,-2.51230174893353,330.769596533151));
#27115=CARTESIAN_POINT('Ctrl Pts',(24.7771794001983,-2.62816738246323,330.842847215671));
#27116=CARTESIAN_POINT('Ctrl Pts',(24.7694181452721,-2.74409493088274,330.916137041013));
#27117=CARTESIAN_POINT('Ctrl Pts',(24.761656890346,-2.85686251950509,330.994221543677));
#27118=CARTESIAN_POINT('Ctrl Pts',(24.7538956354198,-2.96606519066085,331.076781888902));
#27119=CARTESIAN_POINT('Ctrl Pts',(24.7461219650152,-3.07544255050139,331.159474303772));
#27120=CARTESIAN_POINT('Ctrl Pts',(24.7383482946105,-3.18124329536648,331.24665662008));
#27121=CARTESIAN_POINT('Ctrl Pts',(24.7305746242059,-3.28309671445723,331.337970641022));
#27122=CARTESIAN_POINT('Ctrl Pts',(24.7231628200288,-3.38020883238479,331.425033972319));
#27123=CARTESIAN_POINT('Ctrl Pts',(24.7157510158517,-3.47373264383196,331.515852802625));
#27124=CARTESIAN_POINT('Ctrl Pts',(24.7083392116747,-3.56338070120289,331.610088343217));
#27125=CARTESIAN_POINT('Ctrl Pts',(24.7006598905743,-3.65626445826493,331.707725161187));
#27126=CARTESIAN_POINT('Ctrl Pts',(24.6929805694739,-3.74529721302402,331.809355905759));
#27127=CARTESIAN_POINT('Ctrl Pts',(24.6853012483735,-3.83010939108351,331.91464019686));
#27128=CARTESIAN_POINT('Ctrl Pts',(24.6774360400451,-3.91697455019225,332.022473021194));
#27129=CARTESIAN_POINT('Ctrl Pts',(24.6695708317166,-3.99941184335112,332.134138294801));
#27130=CARTESIAN_POINT('Ctrl Pts',(24.6617056233881,-4.07706247657,332.249228358325));
#27131=CARTESIAN_POINT('Ctrl Pts',(24.6540451701267,-4.15269162988034,332.361322280781));
#27132=CARTESIAN_POINT('Ctrl Pts',(24.6463847168653,-4.22377999456111,332.476664540659));
#27133=CARTESIAN_POINT('Ctrl Pts',(24.6387242636039,-4.29003585261921,332.594843987235));
#27134=CARTESIAN_POINT('Ctrl Pts',(24.631068819397,-4.35624838697368,332.712946158057));
#27135=CARTESIAN_POINT('Ctrl Pts',(24.6234133751902,-4.4176345026729,332.833881477813));
#27136=CARTESIAN_POINT('Ctrl Pts',(24.6157579309833,-4.47394605442155,332.957210298483));
#27137=CARTESIAN_POINT('Ctrl Pts',(24.6081057372702,-4.53023369634304,333.080486753861));
#27138=CARTESIAN_POINT('Ctrl Pts',(24.600453543557,-4.58145089398798,333.206154324079));
#27139=CARTESIAN_POINT('Ctrl Pts',(24.5928013498439,-4.62739593893171,333.333749752631));
#27140=CARTESIAN_POINT('Ctrl Pts',(24.5847792580644,-4.67556191344435,333.467512994501));
#27141=CARTESIAN_POINT('Ctrl Pts',(24.576757166285,-4.71793310317526,333.603394707546));
#27142=CARTESIAN_POINT('Ctrl Pts',(24.5687350745055,-4.7543345560173,333.740839171527));
#27143=CARTESIAN_POINT('Ctrl Pts',(24.5610819356911,-4.78906182906563,333.871962273959));
#27144=CARTESIAN_POINT('Ctrl Pts',(24.5534287968767,-4.81835617095714,334.00450716053));
#27145=CARTESIAN_POINT('Ctrl Pts',(24.5457756580624,-4.84211746075958,334.137978214482));
#27146=CARTESIAN_POINT('Ctrl Pts',(24.5381208996189,-4.86588377914909,334.271477514831));
#27147=CARTESIAN_POINT('Ctrl Pts',(24.5304661411755,-4.88411465462634,334.405902975934));
#27148=CARTESIAN_POINT('Ctrl Pts',(24.5228113827321,-4.89676160564217,334.540751875335));
#27149=CARTESIAN_POINT('Ctrl Pts',(24.5151509942951,-4.90941785835635,334.67569995467));
#27150=CARTESIAN_POINT('Ctrl Pts',(24.507490605858,-4.91648196677551,334.811071693648));
#27151=CARTESIAN_POINT('Ctrl Pts',(24.499830217421,-4.91795751081103,334.94636247249));
#27152=CARTESIAN_POINT('Ctrl Pts',(24.4987322277773,-4.9181690055783,334.965754161993));
#27153=CARTESIAN_POINT('Ctrl Pts',(24.4976342381337,-4.91826577356416,334.985144192857));
#27154=CARTESIAN_POINT('Ctrl Pts',(24.4965362484901,-4.91824791280043,335.004531085324));
#27155=CARTESIAN_POINT('',(27.9965362484484,-4.91824819040164,334.995780982225));
#27156=CARTESIAN_POINT('Ctrl Pts',(27.9965362484484,-4.91824819040164,334.995780982225));
#27157=CARTESIAN_POINT('Ctrl Pts',(27.9888887221241,-4.91836378679145,335.130535506929));
#27158=CARTESIAN_POINT('Ctrl Pts',(27.9812411957999,-4.91293703731669,335.265481117084));
#27159=CARTESIAN_POINT('Ctrl Pts',(27.9735936694756,-4.90194754509121,335.400116642586));
#27160=CARTESIAN_POINT('Ctrl Pts',(27.965953003735,-4.89096791152174,335.534631386772));
#27161=CARTESIAN_POINT('Ctrl Pts',(27.9583123379943,-4.87443549378492,335.668836199799));
#27162=CARTESIAN_POINT('Ctrl Pts',(27.9506716722537,-4.8523819494007,335.802229692563));
#27163=CARTESIAN_POINT('Ctrl Pts',(27.9430355614214,-4.83034155202144,335.935543664101));
#27164=CARTESIAN_POINT('Ctrl Pts',(27.9353994505891,-4.80278663931256,336.068046880407));
#27165=CARTESIAN_POINT('Ctrl Pts',(27.9277633397567,-4.76980067974941,336.199243318915));
#27166=CARTESIAN_POINT('Ctrl Pts',(27.920129584571,-4.7368248959507,336.330399284929));
#27167=CARTESIAN_POINT('Ctrl Pts',(27.9124958293852,-4.69842149401602,336.460248883604));
#27168=CARTESIAN_POINT('Ctrl Pts',(27.9048620741995,-4.65472490221656,336.588307006591));
#27169=CARTESIAN_POINT('Ctrl Pts',(27.8972289078239,-4.61103168084217,336.716355252141));
#27170=CARTESIAN_POINT('Ctrl Pts',(27.8895957414484,-4.5620462117725,336.842611914903));
#27171=CARTESIAN_POINT('Ctrl Pts',(27.8819625750729,-4.50795240032874,336.966608303367));
#27172=CARTESIAN_POINT('Ctrl Pts',(27.8743282313581,-4.45385024545755,337.090623817029));
#27173=CARTESIAN_POINT('Ctrl Pts',(27.8666938876433,-4.39463834331634,337.212377993544));
#27174=CARTESIAN_POINT('Ctrl Pts',(27.8590595439285,-4.33054798471872,337.331423859908));
#27175=CARTESIAN_POINT('Ctrl Pts',(27.8514176237407,-4.26639402158833,337.450587869732));
#27176=CARTESIAN_POINT('Ctrl Pts',(27.8437757035531,-4.19735212412781,337.567037845476));
#27177=CARTESIAN_POINT('Ctrl Pts',(27.8361337833653,-4.12369881076348,337.68035280898));
#27178=CARTESIAN_POINT('Ctrl Pts',(27.8284880555331,-4.05000879907859,337.793724232523));
#27179=CARTESIAN_POINT('Ctrl Pts',(27.8208423277008,-3.97170303010984,337.903957204971));
#27180=CARTESIAN_POINT('Ctrl Pts',(27.8131965998685,-3.88909949679421,338.010662413246));
#27181=CARTESIAN_POINT('Ctrl Pts',(27.8055388590461,-3.80636617656312,338.11753527706));
#27182=CARTESIAN_POINT('Ctrl Pts',(27.7978811182238,-3.71932186260039,338.220868995746));
#27183=CARTESIAN_POINT('Ctrl Pts',(27.7902233774014,-3.62832316736817,338.320309331318));
#27184=CARTESIAN_POINT('Ctrl Pts',(27.7831347811636,-3.54408774812037,338.412358984731));
#27185=CARTESIAN_POINT('Ctrl Pts',(27.7760461849258,-3.45646448831866,338.501072716874));
#27186=CARTESIAN_POINT('Ctrl Pts',(27.768957588688,-3.36576112501035,338.586200651368));
#27187=CARTESIAN_POINT('Ctrl Pts',(27.7611825099096,-3.26627375522161,338.679572649819));
#27188=CARTESIAN_POINT('Ctrl Pts',(27.7534074311311,-3.16274078260526,338.768949131203));
#27189=CARTESIAN_POINT('Ctrl Pts',(27.7456323523527,-3.05551655667957,338.853959215451));
#27190=CARTESIAN_POINT('Ctrl Pts',(27.7378668413037,-2.94842427699026,338.938864689378));
#27191=CARTESIAN_POINT('Ctrl Pts',(27.7301013302547,-2.83765008527288,339.019414216642));
#27192=CARTESIAN_POINT('Ctrl Pts',(27.7223358192057,-2.7235848084545,339.095273965641));
#27193=CARTESIAN_POINT('Ctrl Pts',(27.7145780076835,-2.60963262769011,339.171058499478));
#27194=CARTESIAN_POINT('Ctrl Pts',(27.7068201961612,-2.4923961789912,339.24216229361));
#27195=CARTESIAN_POINT('Ctrl Pts',(27.699062384639,-2.37229869072276,339.308292235271));
#27196=CARTESIAN_POINT('Ctrl Pts',(27.691310411116,-2.25229157962292,339.374372412054));
#27197=CARTESIAN_POINT('Ctrl Pts',(27.6835584375931,-2.12942805546029,339.435485998811));
#27198=CARTESIAN_POINT('Ctrl Pts',(27.6758064640701,-2.00415930094692,339.491383813362));
#27199=CARTESIAN_POINT('Ctrl Pts',(27.6680577735124,-1.87894359782546,339.547257955155));
#27200=CARTESIAN_POINT('Ctrl Pts',(27.6603090829548,-1.75132504651622,339.597920559106));
#27201=CARTESIAN_POINT('Ctrl Pts',(27.6525603923972,-1.62177814700563,339.64316903681));
#27202=CARTESIAN_POINT('Ctrl Pts',(27.6448133140194,-1.49225820080949,339.688408100191));
#27203=CARTESIAN_POINT('Ctrl Pts',(27.6370662356415,-1.36081107322572,339.728235149112));
#27204=CARTESIAN_POINT('Ctrl Pts',(27.6293191572637,-1.22792952739986,339.762496418711));
#27205=CARTESIAN_POINT('Ctrl Pts',(27.6215720139579,-1.09504686789866,339.796757975453));
#27206=CARTESIAN_POINT('Ctrl Pts',(27.6138248706521,-0.960730144672856,
339.825453562243));
#27207=CARTESIAN_POINT('Ctrl Pts',(27.6060777273463,-0.82548511771542,339.848479904355));
#27208=CARTESIAN_POINT('Ctrl Pts',(27.5983288423182,-0.69020968480459,339.871511423277));
#27209=CARTESIAN_POINT('Ctrl Pts',(27.5905799572901,-0.554005918121751,
339.888871095683));
#27210=CARTESIAN_POINT('Ctrl Pts',(27.582831072262,-0.417387158036611,339.900507220973));
#27211=CARTESIAN_POINT('Ctrl Pts',(27.5750739624873,-0.280623389387794,
339.912155696966));
#27212=CARTESIAN_POINT('Ctrl Pts',(27.5673168527125,-0.143444137519326,
339.918068457172));
#27213=CARTESIAN_POINT('Ctrl Pts',(27.5595597429378,-0.00636578020518247,
339.918245880326));
#27214=CARTESIAN_POINT('Ctrl Pts',(27.5517984880116,0.1307858274001,339.918423398289));
#27215=CARTESIAN_POINT('Ctrl Pts',(27.5440372330855,0.267836042666445,339.912859488194));
#27216=CARTESIAN_POINT('Ctrl Pts',(27.5362759781593,0.40427213079559,339.90160658425));
#27217=CARTESIAN_POINT('Ctrl Pts',(27.5285023077547,0.540926472201139,339.890335679327));
#27218=CARTESIAN_POINT('Ctrl Pts',(27.52072863735,0.67696433526753,339.87335764342));
#27219=CARTESIAN_POINT('Ctrl Pts',(27.5129549669454,0.811880831709009,339.850776492233));
#27220=CARTESIAN_POINT('Ctrl Pts',(27.5055431627682,0.940516932782646,339.829246499067));
#27221=CARTESIAN_POINT('Ctrl Pts',(27.4981313585911,1.06813343529362,339.80262336002));
#27222=CARTESIAN_POINT('Ctrl Pts',(27.490719554414,1.19430616389448,339.771039283991));
#27223=CARTESIAN_POINT('Ctrl Pts',(27.4829444756356,1.32666299377277,339.737907178312));
#27224=CARTESIAN_POINT('Ctrl Pts',(27.4751693968572,1.45784921593568,339.699210835358));
#27225=CARTESIAN_POINT('Ctrl Pts',(27.4673943180787,1.58736119056331,339.655047530713));
#27226=CARTESIAN_POINT('Ctrl Pts',(27.4596288070297,1.71671379246137,339.610938571825));
#27227=CARTESIAN_POINT('Ctrl Pts',(27.4518632959807,1.84439587974724,339.56137616188));
#27228=CARTESIAN_POINT('Ctrl Pts',(27.4440977849317,1.96991522742806,339.506508300142));
#27229=CARTESIAN_POINT('Ctrl Pts',(27.4363399734095,2.09531012230978,339.451694840049));
#27230=CARTESIAN_POINT('Ctrl Pts',(27.4285821618873,2.21854618914502,339.391586552147));
#27231=CARTESIAN_POINT('Ctrl Pts',(27.4208243503651,2.33914791000277,339.326380718063));
#27232=CARTESIAN_POINT('Ctrl Pts',(27.4130723768421,2.45965887424075,339.261223953437));
#27233=CARTESIAN_POINT('Ctrl Pts',(27.4053204033192,2.57753909597758,339.190977463282));
#27234=CARTESIAN_POINT('Ctrl Pts',(27.3975684297962,2.6923348717475,339.115885809989));
#27235=CARTESIAN_POINT('Ctrl Pts',(27.3898197392386,2.80708203143853,339.040825958057));
#27236=CARTESIAN_POINT('Ctrl Pts',(27.3820710486809,2.91874701680486,338.960925237656));
#27237=CARTESIAN_POINT('Ctrl Pts',(27.3743223581233,3.02690268776494,338.876473033738));
#27238=CARTESIAN_POINT('Ctrl Pts',(27.3665752797455,3.13503585603434,338.792038400807));
#27239=CARTESIAN_POINT('Ctrl Pts',(27.3588282013677,3.23966085431551,338.703054408368));
#27240=CARTESIAN_POINT('Ctrl Pts',(27.3510811229899,3.3403817160414,338.609852220471));
#27241=CARTESIAN_POINT('Ctrl Pts',(27.3433339796841,3.44110342190513,338.516649251449));
#27242=CARTESIAN_POINT('Ctrl Pts',(27.3355868363783,3.53792063905991,338.419228281932));
#27243=CARTESIAN_POINT('Ctrl Pts',(27.3278396930725,3.63047282583165,338.317958728405));
#27244=CARTESIAN_POINT('Ctrl Pts',(27.3200908080444,3.72304582030016,338.216666407332));
#27245=CARTESIAN_POINT('Ctrl Pts',(27.3123419230162,3.81135161270188,338.111524068985));
#27246=CARTESIAN_POINT('Ctrl Pts',(27.3045930379881,3.89506892896896,338.002935414071));
#27247=CARTESIAN_POINT('Ctrl Pts',(27.2968359282134,3.97887510366026,337.894231502037));
#27248=CARTESIAN_POINT('Ctrl Pts',(27.2890788184387,4.0580828343907,337.782074276371));
#27249=CARTESIAN_POINT('Ctrl Pts',(27.281321708664,4.13241299800268,337.666898175116));
#27250=CARTESIAN_POINT('Ctrl Pts',(27.2735604537378,4.20678288127733,337.551660527436));
#27251=CARTESIAN_POINT('Ctrl Pts',(27.2657991988117,4.27626980599831,337.433401126571));
#27252=CARTESIAN_POINT('Ctrl Pts',(27.2580379438855,4.340640394989,337.312579517312));
#27253=CARTESIAN_POINT('Ctrl Pts',(27.2502642734809,4.40511395594383,337.191564632853));
#27254=CARTESIAN_POINT('Ctrl Pts',(27.2424906030762,4.46445465689536,337.067979702131));
#27255=CARTESIAN_POINT('Ctrl Pts',(27.2347169326716,4.51847674284651,336.942305585343));
#27256=CARTESIAN_POINT('Ctrl Pts',(27.2273051284944,4.56998408770003,336.822481628926));
#27257=CARTESIAN_POINT('Ctrl Pts',(27.2198933243173,4.6166567342375,336.700758881212));
#27258=CARTESIAN_POINT('Ctrl Pts',(27.2124815201402,4.65837631412361,336.577565586121));
#27259=CARTESIAN_POINT('Ctrl Pts',(27.2047064413617,4.70214069489594,336.448334220664));
#27260=CARTESIAN_POINT('Ctrl Pts',(27.1969313625833,4.74059250683218,336.317076116144));
#27261=CARTESIAN_POINT('Ctrl Pts',(27.1891562838048,4.77354100263976,336.184267435429));
#27262=CARTESIAN_POINT('Ctrl Pts',(27.1813907727558,4.80644895322569,336.05162218425));
#27263=CARTESIAN_POINT('Ctrl Pts',(27.1736252617068,4.83386696916201,335.917430529162));
#27264=CARTESIAN_POINT('Ctrl Pts',(27.1658597506578,4.85565313500078,335.782186483556));
#27265=CARTESIAN_POINT('Ctrl Pts',(27.1581019391356,4.87741769979264,335.647076532815));
#27266=CARTESIAN_POINT('Ctrl Pts',(27.1503441276133,4.89356146519102,335.51091665149));
#27267=CARTESIAN_POINT('Ctrl Pts',(27.1425863160911,4.90399299948555,335.374213473163));
#27268=CARTESIAN_POINT('Ctrl Pts',(27.1348343425681,4.91441668371969,335.237613168313));
#27269=CARTESIAN_POINT('Ctrl Pts',(27.1270823690452,4.91913666345235,335.100470768424));
#27270=CARTESIAN_POINT('Ctrl Pts',(27.1193303955222,4.91811307143793,334.963300149164));
#27271=CARTESIAN_POINT('Ctrl Pts',(27.1115817049646,4.91708991291533,334.826187621742));
#27272=CARTESIAN_POINT('Ctrl Pts',(27.1038330144069,4.91032802344049,334.689047288768));
#27273=CARTESIAN_POINT('Ctrl Pts',(27.0960843238493,4.89783960298501,334.552394944251));
#27274=CARTESIAN_POINT('Ctrl Pts',(27.0883372454715,4.88535378084973,334.415771031397));
#27275=CARTESIAN_POINT('Ctrl Pts',(27.0805901670936,4.86714383316806,334.279635294056));
#27276=CARTESIAN_POINT('Ctrl Pts',(27.0728430887158,4.84327396262556,334.144499920834));
#27277=CARTESIAN_POINT('Ctrl Pts',(27.06509594541,4.81940389203053,334.009363415047));
#27278=CARTESIAN_POINT('Ctrl Pts',(27.0573488021042,4.78987387195104,333.875227675017));
#27279=CARTESIAN_POINT('Ctrl Pts',(27.0496016587984,4.75479944280458,333.742595800387));
#27280=CARTESIAN_POINT('Ctrl Pts',(27.0418527737704,4.71971712818199,333.609934107296));
#27281=CARTESIAN_POINT('Ctrl Pts',(27.0341038887422,4.67908802400678,333.478777330199));
#27282=CARTESIAN_POINT('Ctrl Pts',(27.0263550037142,4.63307775098302,333.349614100931));
#27283=CARTESIAN_POINT('Ctrl Pts',(27.0185978939394,4.58701864217985,333.220313776476));
#27284=CARTESIAN_POINT('Ctrl Pts',(27.0108407841647,4.53556708638527,333.093011595494));
#27285=CARTESIAN_POINT('Ctrl Pts',(27.00308367439,4.47893736225992,332.968177377955));
#27286=CARTESIAN_POINT('Ctrl Pts',(26.9953224194638,4.4222773770207,332.843276453003));
#27287=CARTESIAN_POINT('Ctrl Pts',(26.9875611645377,4.36043388600542,332.720846468035));
#27288=CARTESIAN_POINT('Ctrl Pts',(26.9797999096115,4.29366703644942,332.601332360954));
#27289=CARTESIAN_POINT('Ctrl Pts',(26.9720262392068,4.22679338169339,332.48162707025));
#27290=CARTESIAN_POINT('Ctrl Pts',(26.9642525688022,4.15498083513406,332.364847311526));
#27291=CARTESIAN_POINT('Ctrl Pts',(26.9564788983975,4.07853323968209,332.251409511166));
#27292=CARTESIAN_POINT('Ctrl Pts',(26.9490670942204,4.00564429819054,332.143252267704));
#27293=CARTESIAN_POINT('Ctrl Pts',(26.9416552900433,3.9285422899142,332.038133080276));
#27294=CARTESIAN_POINT('Ctrl Pts',(26.9342434858662,3.84752327840411,331.936383234698));
#27295=CARTESIAN_POINT('Ctrl Pts',(26.9264684070877,3.76253328379668,331.829646326092));
#27296=CARTESIAN_POINT('Ctrl Pts',(26.9186933283094,3.67296402523994,331.726280085157));
#27297=CARTESIAN_POINT('Ctrl Pts',(26.9109182495309,3.57911269394363,331.626702594411));
#27298=CARTESIAN_POINT('Ctrl Pts',(26.9031527384819,3.48537685268535,331.527247640108));
#27299=CARTESIAN_POINT('Ctrl Pts',(26.8953872274328,3.3873696887367,331.431572441085));
#27300=CARTESIAN_POINT('Ctrl Pts',(26.8876217163838,3.28542982990655,331.340063676065));
#27301=CARTESIAN_POINT('Ctrl Pts',(26.8798639048616,3.18359104474328,331.248645642251));
#27302=CARTESIAN_POINT('Ctrl Pts',(26.8721060933393,3.07782761348009,331.161386080879));
#27303=CARTESIAN_POINT('Ctrl Pts',(26.8643482818171,2.96851609615829,331.078636047324));
#27304=CARTESIAN_POINT('Ctrl Pts',(26.8565963082941,2.85928683921914,330.995948285793));
#27305=CARTESIAN_POINT('Ctrl Pts',(26.8488443347711,2.74651512121259,330.917763532329));
#27306=CARTESIAN_POINT('Ctrl Pts',(26.841092361248,2.63061149669608,330.844393399761));
#27307=CARTESIAN_POINT('Ctrl Pts',(26.8333436706904,2.51475695743399,330.771054339488));
#27308=CARTESIAN_POINT('Ctrl Pts',(26.8255949801328,2.39577347928349,330.702526053323));
#27309=CARTESIAN_POINT('Ctrl Pts',(26.8178462895752,2.27410140653542,330.639077407785));
#27310=CARTESIAN_POINT('Ctrl Pts',(26.8100992111973,2.15245464867831,330.575641963267));
#27311=CARTESIAN_POINT('Ctrl Pts',(26.8023521328195,2.02812075524262,330.517284237823));
#27312=CARTESIAN_POINT('Ctrl Pts',(26.7946050544417,1.9015651803096,330.464227416687));
#27313=CARTESIAN_POINT('Ctrl Pts',(26.7868579111359,1.77500854471914,330.411170150884));
#27314=CARTESIAN_POINT('Ctrl Pts',(26.77911076783,1.64623055096989,330.363414029126));
#27315=CARTESIAN_POINT('Ctrl Pts',(26.7713636245242,1.51571679183518,330.321134147098));
#27316=CARTESIAN_POINT('Ctrl Pts',(26.7636147394962,1.38517369043689,330.278844759655));
#27317=CARTESIAN_POINT('Ctrl Pts',(26.7558658544681,1.25289441890203,330.242034182279));
#27318=CARTESIAN_POINT('Ctrl Pts',(26.74811696944,1.11937950503105,330.210827567709));
#27319=CARTESIAN_POINT('Ctrl Pts',(26.7403598596653,0.985722877050647,330.179587830116));
#27320=CARTESIAN_POINT('Ctrl Pts',(26.7326027498905,0.850828368059913,330.153964026328));
#27321=CARTESIAN_POINT('Ctrl Pts',(26.7248456401157,0.715207018173626,330.134030211391));
#27322=CARTESIAN_POINT('Ctrl Pts',(26.7170843851896,0.579513196574013,330.114085744461));
#27323=CARTESIAN_POINT('Ctrl Pts',(26.7093231302634,0.443092148718221,330.099837365532));
#27324=CARTESIAN_POINT('Ctrl Pts',(26.7015618753372,0.30645881297548,330.091307092672));
#27325=CARTESIAN_POINT('Ctrl Pts',(26.6937882049326,0.169606908424437,330.082763174156));
#27326=CARTESIAN_POINT('Ctrl Pts',(26.6860145345279,0.0325424283800611,
330.079955648345));
#27327=CARTESIAN_POINT('Ctrl Pts',(26.6782408641232,-0.104220018493641,
330.082854359464));
#27328=CARTESIAN_POINT('Ctrl Pts',(26.6708290599462,-0.234616140560568,
330.085618134883));
#27329=CARTESIAN_POINT('Ctrl Pts',(26.6634172557692,-0.364737428677432,
330.093568834486));
#27330=CARTESIAN_POINT('Ctrl Pts',(26.6560054515922,-0.494145080557771,
330.106636769883));
#27331=CARTESIAN_POINT('Ctrl Pts',(26.6482303728138,-0.629895386943907,
330.120345203721));
#27332=CARTESIAN_POINT('Ctrl Pts',(26.6404552940353,-0.765289329456113,
330.139728499994));
#27333=CARTESIAN_POINT('Ctrl Pts',(26.6326802152569,-0.899814506368985,
330.164762992714));
#27334=CARTESIAN_POINT('Ctrl Pts',(26.6249147042079,-1.03417414148737,330.189766678897));
#27335=CARTESIAN_POINT('Ctrl Pts',(26.6171491931589,-1.16766675754857,330.22040765392));
#27336=CARTESIAN_POINT('Ctrl Pts',(26.6093836821099,-1.29978393722895,330.256610412477));
#27337=CARTESIAN_POINT('Ctrl Pts',(26.6016258705877,-1.43177012234075,330.292777275894));
#27338=CARTESIAN_POINT('Ctrl Pts',(26.5938680590655,-1.56238321046072,330.334494845995));
#27339=CARTESIAN_POINT('Ctrl Pts',(26.5861102475433,-1.69112421338773,330.381636441618));
#27340=CARTESIAN_POINT('Ctrl Pts',(26.5783582740203,-1.81976833462812,330.428742561694));
#27341=CARTESIAN_POINT('Ctrl Pts',(26.5706063004973,-1.94654280926681,330.481264448906));
#27342=CARTESIAN_POINT('Ctrl Pts',(26.5628543269742,-2.07096342080095,330.539025490747));
#27343=CARTESIAN_POINT('Ctrl Pts',(26.5551056364166,-2.19533134013156,330.596762070752));
#27344=CARTESIAN_POINT('Ctrl Pts',(26.5473569458589,-2.31734702525195,330.659733228134));
#27345=CARTESIAN_POINT('Ctrl Pts',(26.5396082553013,-2.43654608500821,330.727714167084));
#27346=CARTESIAN_POINT('Ctrl Pts',(26.5318611769235,-2.55572034440467,330.795680962033));
#27347=CARTESIAN_POINT('Ctrl Pts',(26.5241140985457,-2.67207880475349,330.868655271766));
#27348=CARTESIAN_POINT('Ctrl Pts',(26.5163670201678,-2.78518190091799,330.946366464356));
#27349=CARTESIAN_POINT('Ctrl Pts',(26.5086198768621,-2.89828594499507,331.02407830824));
#27350=CARTESIAN_POINT('Ctrl Pts',(26.5008727335562,-3.00813424831016,331.106526892813));
#27351=CARTESIAN_POINT('Ctrl Pts',(26.4931255902504,-3.11431678705484,331.193398627073));
#27352=CARTESIAN_POINT('Ctrl Pts',(26.4853767052223,-3.22052319788898,331.280289891944));
#27353=CARTESIAN_POINT('Ctrl Pts',(26.4776278201942,-3.32306190173505,331.371606037824));
#27354=CARTESIAN_POINT('Ctrl Pts',(26.4698789351661,-3.42155679067098,331.466993887535));
#27355=CARTESIAN_POINT('Ctrl Pts',(26.4621218253913,-3.52015622309939,331.562482982896));
#27356=CARTESIAN_POINT('Ctrl Pts',(26.4543647156167,-3.61470298542498,331.66205214283));
#27357=CARTESIAN_POINT('Ctrl Pts',(26.4466076058419,-3.70485825004922,331.76531169824));
#27358=CARTESIAN_POINT('Ctrl Pts',(26.4388463509158,-3.7950616907642,331.868626432254));
#27359=CARTESIAN_POINT('Ctrl Pts',(26.4310850959895,-3.88086871341403,331.975635186401));
#27360=CARTESIAN_POINT('Ctrl Pts',(26.4233238410634,-3.96198213983656,332.08591685326));
#27361=CARTESIAN_POINT('Ctrl Pts',(26.4155501706587,-4.04322532130667,332.196374934845));
#27362=CARTESIAN_POINT('Ctrl Pts',(26.4077765002541,-4.1197596845675,332.310116066944));
#27363=CARTESIAN_POINT('Ctrl Pts',(26.4000028298494,-4.19133210397707,332.426691185133));
#27364=CARTESIAN_POINT('Ctrl Pts',(26.3925910256724,-4.25957281004351,332.537839703524));
#27365=CARTESIAN_POINT('Ctrl Pts',(26.3851792214953,-4.3233029924845,332.651564050485));
#27366=CARTESIAN_POINT('Ctrl Pts',(26.3777674173183,-4.38234379265973,332.767457515424));
#27367=CARTESIAN_POINT('Ctrl Pts',(26.3694807285346,-4.44835373098256,332.897030970559));
#27368=CARTESIAN_POINT('Ctrl Pts',(26.361194039751,-4.50868894522818,333.029682743206));
#27369=CARTESIAN_POINT('Ctrl Pts',(26.3529073509673,-4.56307101532043,333.164907094547));
#27370=CARTESIAN_POINT('Ctrl Pts',(26.3446366353416,-4.61734826026288,333.299870791727));
#27371=CARTESIAN_POINT('Ctrl Pts',(26.3363659197159,-4.66569511754526,333.437396894563));
#27372=CARTESIAN_POINT('Ctrl Pts',(26.3280952040902,-4.70787951244141,333.576956234392));
#27373=CARTESIAN_POINT('Ctrl Pts',(26.3198465163018,-4.7499515553925,333.716143878401));
#27374=CARTESIAN_POINT('Ctrl Pts',(26.3115978285134,-4.78589377748591,333.857353661482));
#27375=CARTESIAN_POINT('Ctrl Pts',(26.303349140725,-4.81552282204938,334.00003849433));
#27376=CARTESIAN_POINT('Ctrl Pts',(26.2951140627465,-4.84510298057505,334.142487906285));
#27377=CARTESIAN_POINT('Ctrl Pts',(26.2868789847679,-4.86839065493487,334.286407213762));
#27378=CARTESIAN_POINT('Ctrl Pts',(26.2786439067894,-4.88525214782621,334.431234218101));
#27379=CARTESIAN_POINT('Ctrl Pts',(26.2704270446483,-4.90207634341266,334.575740867832));
#27380=CARTESIAN_POINT('Ctrl Pts',(26.2622101825073,-4.91250266516355,334.721150901211));
#27381=CARTESIAN_POINT('Ctrl Pts',(26.2539933203662,-4.91644846050656,334.866892533332));
#27382=CARTESIAN_POINT('Ctrl Pts',(26.2515076297528,-4.91764210672796,334.910980970101));
#27383=CARTESIAN_POINT('Ctrl Pts',(26.2490219391395,-4.91824305447504,334.955099677308));
#27384=CARTESIAN_POINT('Ctrl Pts',(26.2465362485262,-4.91824994013874,334.999232650496));
#27385=CARTESIAN_POINT('',(29.7465362485277,-4.91824909912948,335.002976812401));
#27386=CARTESIAN_POINT('Ctrl Pts',(29.7465362484901,-4.91824909912908,335.002976813063));
#27387=CARTESIAN_POINT('Ctrl Pts',(29.7365654418619,-4.91814301649854,335.178245058349));
#27388=CARTESIAN_POINT('Ctrl Pts',(29.7265946352337,-4.90866871766501,335.353227704208));
#27389=CARTESIAN_POINT('Ctrl Pts',(29.7166238286055,-4.88991326132123,335.527191956743));
#27390=CARTESIAN_POINT('Ctrl Pts',(29.7088487498271,-4.87528805033922,335.662846555065));
#27391=CARTESIAN_POINT('Ctrl Pts',(29.7010736710487,-4.85499051391453,335.798106459909));
#27392=CARTESIAN_POINT('Ctrl Pts',(29.6932985922702,-4.82904777913399,335.932459441124));
#27393=CARTESIAN_POINT('Ctrl Pts',(29.6855330812212,-4.80313696854018,336.066647092442));
#27394=CARTESIAN_POINT('Ctrl Pts',(29.6777675701723,-4.77159485508092,336.199929660588));
#27395=CARTESIAN_POINT('Ctrl Pts',(29.6700020591232,-4.7345003770595,336.331799249934));
#27396=CARTESIAN_POINT('Ctrl Pts',(29.662244247601,-4.697442678321,336.463538090197));
#27397=CARTESIAN_POINT('Ctrl Pts',(29.6544864360789,-4.65484367581295,336.593866365828));
#27398=CARTESIAN_POINT('Ctrl Pts',(29.6467286245567,-4.60683341882943,336.722285955832));
#27399=CARTESIAN_POINT('Ctrl Pts',(29.6389766510337,-4.55885929108691,336.850608906022));
#27400=CARTESIAN_POINT('Ctrl Pts',(29.6312246775106,-4.50548215059201,336.977025664913));
#27401=CARTESIAN_POINT('Ctrl Pts',(29.6234727039876,-4.44688187704673,337.101053220195));
#27402=CARTESIAN_POINT('Ctrl Pts',(29.61572401343,-4.38830642075201,337.225028249734));
#27403=CARTESIAN_POINT('Ctrl Pts',(29.6079753228724,-4.32451239755108,337.346615735444));
#27404=CARTESIAN_POINT('Ctrl Pts',(29.6002266323148,-4.25572773541495,337.465352815424));
#27405=CARTESIAN_POINT('Ctrl Pts',(29.592479553937,-4.18695738450228,337.584065191163));
#27406=CARTESIAN_POINT('Ctrl Pts',(29.5847324755591,-4.11319865580338,337.699928002783));
#27407=CARTESIAN_POINT('Ctrl Pts',(29.5769853971813,-4.0347251446478,337.812503523491));
#27408=CARTESIAN_POINT('Ctrl Pts',(29.5692382538755,-3.95625097580862,337.925079987689));
#27409=CARTESIAN_POINT('Ctrl Pts',(29.5614911105697,-3.87306216921994,338.034368785366));
#27410=CARTESIAN_POINT('Ctrl Pts',(29.5537439672639,-3.78547507872997,338.139962020601));
#27411=CARTESIAN_POINT('Ctrl Pts',(29.5459950822359,-3.69786829680277,338.245578995436));
#27412=CARTESIAN_POINT('Ctrl Pts',(29.5382461972078,-3.60586151281525,338.347498453759));
#27413=CARTESIAN_POINT('Ctrl Pts',(29.5304973121797,-3.50981043676153,338.445346682193));
#27414=CARTESIAN_POINT('Ctrl Pts',(29.522740202405,-3.41365741110303,338.543298767749));
#27415=CARTESIAN_POINT('Ctrl Pts',(29.5149830926303,-3.31345179264932,338.637170711942));
#27416=CARTESIAN_POINT('Ctrl Pts',(29.5072259828555,-3.20958553062966,338.7266263274));
#27417=CARTESIAN_POINT('Ctrl Pts',(29.4994647279294,-3.10566376580051,338.816129745079));
#27418=CARTESIAN_POINT('Ctrl Pts',(29.4917034730033,-2.99807776607118,338.901211889283));
#27419=CARTESIAN_POINT('Ctrl Pts',(29.4839422180771,-2.88725063690228,338.981578433512));
#27420=CARTESIAN_POINT('Ctrl Pts',(29.4761685476724,-2.77624622044534,339.06207353802));
#27421=CARTESIAN_POINT('Ctrl Pts',(29.4683948772677,-2.66199063981317,339.137837752432));
#27422=CARTESIAN_POINT('Ctrl Pts',(29.4606212068631,-2.54493465922635,339.20862099063));
#27423=CARTESIAN_POINT('Ctrl Pts',(29.4532094026859,-2.43332766269678,339.276109252061));
#27424=CARTESIAN_POINT('Ctrl Pts',(29.4457975985088,-2.31917536817622,339.339069691241));
#27425=CARTESIAN_POINT('Ctrl Pts',(29.4383857943316,-2.2028856852926,339.397326201231));
#27426=CARTESIAN_POINT('Ctrl Pts',(29.4306107155532,-2.08089629864289,339.458438036312));
#27427=CARTESIAN_POINT('Ctrl Pts',(29.4228356367748,-1.95616919738411,339.514566300627));
#27428=CARTESIAN_POINT('Ctrl Pts',(29.4150605579963,-1.82914980680206,339.565456608793));
#27429=CARTESIAN_POINT('Ctrl Pts',(29.4072950469473,-1.70228672166639,339.616284293196));
#27430=CARTESIAN_POINT('Ctrl Pts',(29.3995295358983,-1.57313731917416,339.661886702443));
#27431=CARTESIAN_POINT('Ctrl Pts',(29.3917640248493,-1.442171417641,339.702055365969));
#27432=CARTESIAN_POINT('Ctrl Pts',(29.3840062133271,-1.31133536918059,339.742184202148));
#27433=CARTESIAN_POINT('Ctrl Pts',(29.3762484018049,-1.17868677718378,339.776889900308));
#27434=CARTESIAN_POINT('Ctrl Pts',(29.3684905902827,-1.04471489935553,339.806012259823));
#27435=CARTESIAN_POINT('Ctrl Pts',(29.3607386167597,-0.910843839614207,
339.835112703838));
#27436=CARTESIAN_POINT('Ctrl Pts',(29.3529866432367,-0.77565185657798,339.858638089672));
#27437=CARTESIAN_POINT('Ctrl Pts',(29.3452346697137,-0.639642468831033,
339.876478296329));
#27438=CARTESIAN_POINT('Ctrl Pts',(29.3374859791561,-0.503690681140176,
339.894310947647));
#27439=CARTESIAN_POINT('Ctrl Pts',(29.3297372885985,-0.366922563997023,
339.906463157758));
#27440=CARTESIAN_POINT('Ctrl Pts',(29.3219885980409,-0.229850692752224,
339.912876115021));
#27441=CARTESIAN_POINT('Ctrl Pts',(29.314241519663,-0.0928073404550829,
339.919287738014));
#27442=CARTESIAN_POINT('Ctrl Pts',(29.3064944412852,0.0445392500351959,
339.919962465052));
#27443=CARTESIAN_POINT('Ctrl Pts',(29.2987473629074,0.181672926787005,339.914893489199));
#27444=CARTESIAN_POINT('Ctrl Pts',(29.2910002196016,0.318807752850923,339.909824470863));
#27445=CARTESIAN_POINT('Ctrl Pts',(29.2832530762958,0.455729271009674,339.89901166806));
#27446=CARTESIAN_POINT('Ctrl Pts',(29.27550593299,0.591923275661444,339.882500373603));
#27447=CARTESIAN_POINT('Ctrl Pts',(29.2677570479619,0.728147899616939,339.865985367055));
#27448=CARTESIAN_POINT('Ctrl Pts',(29.2600081629338,0.863644296641082,339.843769366557));
#27449=CARTESIAN_POINT('Ctrl Pts',(29.2522592779057,0.99790570809472,339.81594925848));
#27450=CARTESIAN_POINT('Ctrl Pts',(29.2445021681309,1.13230962599766,339.788099621852));
#27451=CARTESIAN_POINT('Ctrl Pts',(29.2367450583561,1.26547555648274,339.754634074876));
#27452=CARTESIAN_POINT('Ctrl Pts',(29.2289879485814,1.39690868619675,339.71570028574));
#27453=CARTESIAN_POINT('Ctrl Pts',(29.2212266936553,1.52841204957296,339.676745691632));
#27454=CARTESIAN_POINT('Ctrl Pts',(29.2134654387291,1.65818039751886,339.632317159454));
#27455=CARTESIAN_POINT('Ctrl Pts',(29.2057041838029,1.78573725795884,339.582611210657));
#27456=CARTESIAN_POINT('Ctrl Pts',(29.1979305133983,1.91349816780484,339.53282574854));
#27457=CARTESIAN_POINT('Ctrl Pts',(29.1901568429936,2.03904016272585,339.477746157018));
#27458=CARTESIAN_POINT('Ctrl Pts',(29.182383172589,2.16190900558718,339.417616157393));
#27459=CARTESIAN_POINT('Ctrl Pts',(29.1749713684119,2.27905827425294,339.360285223717));
#27460=CARTESIAN_POINT('Ctrl Pts',(29.1675595642347,2.39377740738313,339.298363630232));
#27461=CARTESIAN_POINT('Ctrl Pts',(29.1601477600576,2.50569756959003,339.232099095278));
#27462=CARTESIAN_POINT('Ctrl Pts',(29.1523726812792,2.62310327233956,339.162586738073));
#27463=CARTESIAN_POINT('Ctrl Pts',(29.1445976025008,2.73779971857641,339.088075282148));
#27464=CARTESIAN_POINT('Ctrl Pts',(29.1368225237223,2.84933194502609,339.008801632602));
#27465=CARTESIAN_POINT('Ctrl Pts',(29.1290570126733,2.96072692397064,338.929625534329));
#27466=CARTESIAN_POINT('Ctrl Pts',(29.1212915016242,3.06896511507072,338.8456991268));
#27467=CARTESIAN_POINT('Ctrl Pts',(29.1135259905752,3.17361696533209,338.757304674878));
#27468=CARTESIAN_POINT('Ctrl Pts',(29.105768179053,3.27816505297931,338.668997866311));
#27469=CARTESIAN_POINT('Ctrl Pts',(29.0980103675308,3.37913357947951,338.576232080054));
#27470=CARTESIAN_POINT('Ctrl Pts',(29.0902525560086,3.47612306329126,338.479332049597));
#27471=CARTESIAN_POINT('Ctrl Pts',(29.0825005824856,3.57303955944059,338.382504939487));
#27472=CARTESIAN_POINT('Ctrl Pts',(29.0747486089626,3.66598269761639,338.281550052918));
#27473=CARTESIAN_POINT('Ctrl Pts',(29.0669966354396,3.75458739192506,338.176831216621));
#27474=CARTESIAN_POINT('Ctrl Pts',(29.059247944882,3.84315456209309,338.072156728813));
#27475=CARTESIAN_POINT('Ctrl Pts',(29.0514992543243,3.92738669077012,337.963721759472));
#27476=CARTESIAN_POINT('Ctrl Pts',(29.0437505637667,4.00695693805955,337.851925517793));
#27477=CARTESIAN_POINT('Ctrl Pts',(29.0360034853889,4.08651063009445,337.740152536255));
#27478=CARTESIAN_POINT('Ctrl Pts',(29.028256407011,4.16140414351533,337.625019991667));
#27479=CARTESIAN_POINT('Ctrl Pts',(29.0205093286332,4.23135243479777,337.506958243575));
#27480=CARTESIAN_POINT('Ctrl Pts',(29.0127621853274,4.30130131231427,337.388895506013));
#27481=CARTESIAN_POINT('Ctrl Pts',(29.0050150420216,4.36630468578707,337.267903852266));
#27482=CARTESIAN_POINT('Ctrl Pts',(28.9972678987158,4.42612237675188,337.144440199333));
#27483=CARTESIAN_POINT('Ctrl Pts',(28.9895190136877,4.48595351600351,337.02094878915));
#27484=CARTESIAN_POINT('Ctrl Pts',(28.9817701286596,4.54059648243839,336.894984625581));
#27485=CARTESIAN_POINT('Ctrl Pts',(28.9740212436315,4.58985851369572,336.76702628355));
#27486=CARTESIAN_POINT('Ctrl Pts',(28.9662641338568,4.63917283218208,336.638932125212));
#27487=CARTESIAN_POINT('Ctrl Pts',(28.9585070240821,4.68309466581821,336.508839925575));
#27488=CARTESIAN_POINT('Ctrl Pts',(28.9507499143074,4.72148042003775,336.377245695473));
#27489=CARTESIAN_POINT('Ctrl Pts',(28.9429886593812,4.75988668637704,336.245581145623));
#27490=CARTESIAN_POINT('Ctrl Pts',(28.935227404455,4.79275088500713,336.112413345279));
#27491=CARTESIAN_POINT('Ctrl Pts',(28.9274661495288,4.81998042862848,335.978249319007));
#27492=CARTESIAN_POINT('Ctrl Pts',(28.9196924791241,4.8472535306455,335.843870674018));
#27493=CARTESIAN_POINT('Ctrl Pts',(28.9119188087195,4.86887390411284,335.708493004729));
#27494=CARTESIAN_POINT('Ctrl Pts',(28.9041451383148,4.88480068569567,335.572630180419));
#27495=CARTESIAN_POINT('Ctrl Pts',(28.8967333341378,4.8999860717639,335.443091803269));
#27496=CARTESIAN_POINT('Ctrl Pts',(28.8893215299608,4.90999598828242,335.313112709501));
#27497=CARTESIAN_POINT('Ctrl Pts',(28.8819097257838,4.914839148895,335.183137115269));
#27498=CARTESIAN_POINT('Ctrl Pts',(28.8741346470054,4.91991968723628,335.046791029985));
#27499=CARTESIAN_POINT('Ctrl Pts',(28.8663595682269,4.91933024265626,334.910017917136));
#27500=CARTESIAN_POINT('Ctrl Pts',(28.8585844894485,4.91302382697354,334.773328567988));
#27501=CARTESIAN_POINT('Ctrl Pts',(28.8508189783995,4.9067251717368,334.636807423787));
#27502=CARTESIAN_POINT('Ctrl Pts',(28.8430534673505,4.89472356106533,334.500370224921));
#27503=CARTESIAN_POINT('Ctrl Pts',(28.8352879563015,4.87702390172891,334.364530941379));
#27504=CARTESIAN_POINT('Ctrl Pts',(28.8275301447793,4.85934179165624,334.228826342882));
#27505=CARTESIAN_POINT('Ctrl Pts',(28.8197723332571,4.83597292618353,334.093718865036));
#27506=CARTESIAN_POINT('Ctrl Pts',(28.8120145217349,4.80697419824712,333.959720172316));
#27507=CARTESIAN_POINT('Ctrl Pts',(28.8042625482119,4.77799729277312,333.825822317862));
#27508=CARTESIAN_POINT('Ctrl Pts',(28.7965105746889,4.74339904002279,333.693031968203));
#27509=CARTESIAN_POINT('Ctrl Pts',(28.7887586011659,4.70328782072906,333.561853019375));
#27510=CARTESIAN_POINT('Ctrl Pts',(28.7810099106083,4.66319358856045,333.430729624909));
#27511=CARTESIAN_POINT('Ctrl Pts',(28.7732612200507,4.61759114754874,333.301216646983));
#27512=CARTESIAN_POINT('Ctrl Pts',(28.765512529493,4.56663932940033,333.173804967241));
#27513=CARTESIAN_POINT('Ctrl Pts',(28.7577654511152,4.51569811220324,333.046419796563));
#27514=CARTESIAN_POINT('Ctrl Pts',(28.7500183727374,4.45940987671494,332.921135417163));
#27515=CARTESIAN_POINT('Ctrl Pts',(28.7422712943596,4.39798226805332,332.798424420469));
#27516=CARTESIAN_POINT('Ctrl Pts',(28.7345241510538,4.33655414456926,332.675712395338));
#27517=CARTESIAN_POINT('Ctrl Pts',(28.726777007748,4.26998673696837,332.555574145456));
#27518=CARTESIAN_POINT('Ctrl Pts',(28.7190298644422,4.19853430215554,332.438458906025));
#27519=CARTESIAN_POINT('Ctrl Pts',(28.7112809794141,4.12706580331839,332.321317336601));
#27520=CARTESIAN_POINT('Ctrl Pts',(28.703532094386,4.05071029539571,332.20720046364));
#27521=CARTESIAN_POINT('Ctrl Pts',(28.6957832093579,3.96976590747842,332.096529369475));
#27522=CARTESIAN_POINT('Ctrl Pts',(28.6880260995831,3.88873560435148,331.985740807867));
#27523=CARTESIAN_POINT('Ctrl Pts',(28.6802689898084,3.80310692269607,331.878405647019));
#27524=CARTESIAN_POINT('Ctrl Pts',(28.6725118800337,3.71321926134677,331.774913058588));
#27525=CARTESIAN_POINT('Ctrl Pts',(28.6647506251075,3.62328356690523,331.671365167028));
#27526=CARTESIAN_POINT('Ctrl Pts',(28.6569893701814,3.52908462621157,331.57166422334));
#27527=CARTESIAN_POINT('Ctrl Pts',(28.6492281152552,3.43099870274052,331.476162466246));
#27528=CARTESIAN_POINT('Ctrl Pts',(28.6414544448505,3.33275587375803,331.380507937465));
#27529=CARTESIAN_POINT('Ctrl Pts',(28.6336807744458,3.23061392815709,331.289066279344));
#27530=CARTESIAN_POINT('Ctrl Pts',(28.6259071040412,3.12498287608195,331.202149938887));
#27531=CARTESIAN_POINT('Ctrl Pts',(28.6184952998641,3.02426897489412,331.119279574989));
#27532=CARTESIAN_POINT('Ctrl Pts',(28.611083495687,2.92038372215826,331.040522876799));
#27533=CARTESIAN_POINT('Ctrl Pts',(28.6036716915099,2.81370538416739,330.966112907677));
#27534=CARTESIAN_POINT('Ctrl Pts',(28.5958966127315,2.7017984230533,330.888055884313));
#27535=CARTESIAN_POINT('Ctrl Pts',(28.588121533953,2.58646401224734,330.814535781434));
#27536=CARTESIAN_POINT('Ctrl Pts',(28.5803464551746,2.46810625902171,330.745868530866));
#27537=CARTESIAN_POINT('Ctrl Pts',(28.5725809441256,2.34989415254644,330.677285779721));
#27538=CARTESIAN_POINT('Ctrl Pts',(28.5648154330765,2.22866644107313,330.613544193107));
#27539=CARTESIAN_POINT('Ctrl Pts',(28.5570499220275,2.10485798826539,330.554917783467));
#27540=CARTESIAN_POINT('Ctrl Pts',(28.5492921105053,1.98117229189897,330.496349502084));
#27541=CARTESIAN_POINT('Ctrl Pts',(28.5415342989831,1.85491129737371,330.442886470885));
#27542=CARTESIAN_POINT('Ctrl Pts',(28.5337764874609,1.72653606229579,330.394757738393));
#27543=CARTESIAN_POINT('Ctrl Pts',(28.5260245139379,1.59825743365327,330.346665224299));
#27544=CARTESIAN_POINT('Ctrl Pts',(28.5182725404149,1.46786809585616,330.303899155449));
#27545=CARTESIAN_POINT('Ctrl Pts',(28.5105205668918,1.33585043686496,330.266641079231));
#27546=CARTESIAN_POINT('Ctrl Pts',(28.5027718763342,1.2038886874309,330.22939878183));
#27547=CARTESIAN_POINT('Ctrl Pts',(28.4950231857766,1.07030036375591,330.197659943553));
#27548=CARTESIAN_POINT('Ctrl Pts',(28.487274495219,0.935584211636791,330.171556643655));
#27549=CARTESIAN_POINT('Ctrl Pts',(28.4795274168411,0.80089608833811,330.145458774765));
#27550=CARTESIAN_POINT('Ctrl Pts',(28.4717803384633,0.665080986835005,330.124994186335));
#27551=CARTESIAN_POINT('Ctrl Pts',(28.4640332600854,0.528648688027829,330.110244011492));
#27552=CARTESIAN_POINT('Ctrl Pts',(28.4562861167796,0.392215245786766,330.095493713029));
#27553=CARTESIAN_POINT('Ctrl Pts',(28.4485389734738,0.25516498453403,330.086457965692));
#27554=CARTESIAN_POINT('Ctrl Pts',(28.440791830168,0.118013268734895,330.083166066369));
#27555=CARTESIAN_POINT('Ctrl Pts',(28.4330429451399,-0.0191692816817649,
330.079873426958));
#27556=CARTESIAN_POINT('Ctrl Pts',(28.4252940601118,-0.156452941347069,
330.082327214559));
#27557=CARTESIAN_POINT('Ctrl Pts',(28.4175451750837,-0.293322278384767,
330.090504597873));
#27558=CARTESIAN_POINT('Ctrl Pts',(28.409788065309,-0.430336889950923,330.098690660746));
#27559=CARTESIAN_POINT('Ctrl Pts',(28.4020309555342,-0.566935909620196,
330.112612431533));
#27560=CARTESIAN_POINT('Ctrl Pts',(28.3942738457595,-0.702608406458019,
330.132195105628));
#27561=CARTESIAN_POINT('Ctrl Pts',(28.3865125908333,-0.838353402340095,
330.151788244077));
#27562=CARTESIAN_POINT('Ctrl Pts',(28.3787513359072,-0.973170504857078,
330.177048241484));
#27563=CARTESIAN_POINT('Ctrl Pts',(28.370990080981,-1.10655989119709,330.20784930645));
#27564=CARTESIAN_POINT('Ctrl Pts',(28.3632164105763,-1.24016265708392,330.238699643081));
#27565=CARTESIAN_POINT('Ctrl Pts',(28.3554427401717,-1.3723327658881,330.27510865611));
#27566=CARTESIAN_POINT('Ctrl Pts',(28.347669069767,-1.50258559424392,330.316900642259));
#27567=CARTESIAN_POINT('Ctrl Pts',(28.3402572655899,-1.62677512210242,330.356747201399));
#27568=CARTESIAN_POINT('Ctrl Pts',(28.3328454614129,-1.74922158100058,330.40148675827));
#27569=CARTESIAN_POINT('Ctrl Pts',(28.3254336572358,-1.86952428139009,330.450927344635));
#27570=CARTESIAN_POINT('Ctrl Pts',(28.3176585784574,-1.99572337548938,330.502791161413));
#27571=CARTESIAN_POINT('Ctrl Pts',(28.3098834996789,-2.11996206605793,330.55999238176));
#27572=CARTESIAN_POINT('Ctrl Pts',(28.3021084209005,-2.24175599364902,330.622362152092));
#27573=CARTESIAN_POINT('Ctrl Pts',(28.2943429098514,-2.36340004605827,330.68465517245));
#27574=CARTESIAN_POINT('Ctrl Pts',(28.2865773988024,-2.48260497683239,330.752103911299));
#27575=CARTESIAN_POINT('Ctrl Pts',(28.2788118877534,-2.59890503337951,330.824490966364));
#27576=CARTESIAN_POINT('Ctrl Pts',(28.2710540762312,-2.71508977808188,330.896806249453));
#27577=CARTESIAN_POINT('Ctrl Pts',(28.263296264709,-2.82837505059285,330.97404989952));
#27578=CARTESIAN_POINT('Ctrl Pts',(28.2555384531868,-2.93831873439641,331.055958154685));
#27579=CARTESIAN_POINT('Ctrl Pts',(28.2477864796638,-3.04817968209153,331.137804771291));
#27580=CARTESIAN_POINT('Ctrl Pts',(28.2400345061408,-3.15470373418234,331.224308773408));
#27581=CARTESIAN_POINT('Ctrl Pts',(28.2322825326177,-3.25747717579205,331.315162756417));
#27582=CARTESIAN_POINT('Ctrl Pts',(28.2245338420601,-3.36020709278808,331.405978262711));
#27583=CARTESIAN_POINT('Ctrl Pts',(28.2167851515025,-3.45918926625015,331.501139827506));
#27584=CARTESIAN_POINT('Ctrl Pts',(28.2090364609448,-3.55404272794733,331.600299520483));
#27585=CARTESIAN_POINT('Ctrl Pts',(28.201289382567,-3.64887645458957,331.699438582459));
#27586=CARTESIAN_POINT('Ctrl Pts',(28.1935423041892,-3.73958290808541,331.802573835744));
#27587=CARTESIAN_POINT('Ctrl Pts',(28.1857952258113,-3.82581799015994,331.909320500494));
#27588=CARTESIAN_POINT('Ctrl Pts',(28.1780480825055,-3.91205379496752,332.016068059884));
#27589=CARTESIAN_POINT('Ctrl Pts',(28.1703009391997,-3.99381790797882,332.126426787055));
#27590=CARTESIAN_POINT('Ctrl Pts',(28.1625537958939,-4.0708067995312,332.239979155262));
#27591=CARTESIAN_POINT('Ctrl Pts',(28.1548049108658,-4.14781299982081,332.353557052451));
#27592=CARTESIAN_POINT('Ctrl Pts',(28.1470560258377,-4.22004162305708,332.470329695952));
#27593=CARTESIAN_POINT('Ctrl Pts',(28.1393071408096,-4.28723293880348,332.589851292775));
#27594=CARTESIAN_POINT('Ctrl Pts',(28.1315500310349,-4.35449557210673,332.709499751056));
#27595=CARTESIAN_POINT('Ctrl Pts',(28.1237929212601,-4.41671002563736,332.831902649912));
#27596=CARTESIAN_POINT('Ctrl Pts',(28.1160358114854,-4.47366271013816,332.956589855555));
#27597=CARTESIAN_POINT('Ctrl Pts',(28.1082745565592,-4.5306458283326,333.081343690054));
#27598=CARTESIAN_POINT('Ctrl Pts',(28.1005133016331,-4.58236142759018,333.208383901773));
#27599=CARTESIAN_POINT('Ctrl Pts',(28.0927520467069,-4.62864480577895,333.337222106102));
#27600=CARTESIAN_POINT('Ctrl Pts',(28.0849783763022,-4.67500222228903,333.466266409569));
#27601=CARTESIAN_POINT('Ctrl Pts',(28.0772047058975,-4.71590993627412,333.597114079887));
#27602=CARTESIAN_POINT('Ctrl Pts',(28.0694310354928,-4.75125344285673,333.729262503803));
#27603=CARTESIAN_POINT('Ctrl Pts',(28.0620192313158,-4.78495170070443,333.855259386791));
#27604=CARTESIAN_POINT('Ctrl Pts',(28.0546074271388,-4.81359205774079,333.982438367736));
#27605=CARTESIAN_POINT('Ctrl Pts',(28.0471956229618,-4.83711910804647,334.11035861322));
#27606=CARTESIAN_POINT('Ctrl Pts',(28.0354721385041,-4.87433258562982,334.312694100496));
#27607=CARTESIAN_POINT('Ctrl Pts',(28.0237486540465,-4.89885879954496,334.517429559264));
#27608=CARTESIAN_POINT('Ctrl Pts',(28.0120251695888,-4.91045911773521,334.723279354671));
#27609=CARTESIAN_POINT('Ctrl Pts',(28.0068621958893,-4.91556784952385,334.813934746725));
#27610=CARTESIAN_POINT('Ctrl Pts',(28.0016992221897,-4.91817014931963,334.904805934471));
#27611=CARTESIAN_POINT('Ctrl Pts',(27.9965362484901,-4.91824819040101,334.995780981491));
#27612=CARTESIAN_POINT('',(31.49653624844,-4.91824929754497,335.002628630519));
#27613=CARTESIAN_POINT('Ctrl Pts',(31.4965362484401,-4.91824929754497,335.002628630519));
#27614=CARTESIAN_POINT('Ctrl Pts',(31.4879704571182,-4.91816808857999,335.154573124847));
#27615=CARTESIAN_POINT('Ctrl Pts',(31.4794046657963,-4.91104154518577,335.30627050863));
#27616=CARTESIAN_POINT('Ctrl Pts',(31.4708388744744,-4.89696263499547,335.457099566788));
#27617=CARTESIAN_POINT('Ctrl Pts',(31.4622260458395,-4.88280641331326,335.608756872258));
#27618=CARTESIAN_POINT('Ctrl Pts',(31.4536132172045,-4.86162134728139,335.759536059089));
#27619=CARTESIAN_POINT('Ctrl Pts',(31.4450003885695,-4.8335521266272,335.908821710611));
#27620=CARTESIAN_POINT('Ctrl Pts',(31.4363631848292,-4.80540346747042,336.058529854398));
#27621=CARTESIAN_POINT('Ctrl Pts',(31.4277259810889,-4.77033175083558,336.206735782444));
#27622=CARTESIAN_POINT('Ctrl Pts',(31.4190887773486,-4.72853164846848,336.352838316996));
#27623=CARTESIAN_POINT('Ctrl Pts',(31.4104202046795,-4.6865797348817,336.499471472353));
#27624=CARTESIAN_POINT('Ctrl Pts',(31.4017516320105,-4.63785059343201,336.643985718313));
#27625=CARTESIAN_POINT('Ctrl Pts',(31.3930830593414,-4.5825882820768,336.785796096835));
#27626=CARTESIAN_POINT('Ctrl Pts',(31.3907393843106,-4.56764731033793,336.824136600622));
#27627=CARTESIAN_POINT('Ctrl Pts',(31.3883957092799,-4.55222904365927,336.862279597944));
#27628=CARTESIAN_POINT('Ctrl Pts',(31.3860520342491,-4.53633887755892,336.900213843347));
#27629=CARTESIAN_POINT('Ctrl Pts',(31.3782769554707,-4.48362367958517,337.026059680564));
#27630=CARTESIAN_POINT('Ctrl Pts',(31.3705018766923,-4.42558444376334,337.149909101025));
#27631=CARTESIAN_POINT('Ctrl Pts',(31.3627267979138,-4.36239329201938,337.271278897063));
#27632=CARTESIAN_POINT('Ctrl Pts',(31.3549612868648,-4.29927990101051,337.392499339841));
#27633=CARTESIAN_POINT('Ctrl Pts',(31.3471957758158,-4.23102738716775,337.511245886095));
#27634=CARTESIAN_POINT('Ctrl Pts',(31.3394302647668,-4.15785629429548,337.62705426257));
#27635=CARTESIAN_POINT('Ctrl Pts',(31.3316724532446,-4.08475775077477,337.742747814702));
#27636=CARTESIAN_POINT('Ctrl Pts',(31.3239146417224,-4.00675054074156,337.855508666182));
#27637=CARTESIAN_POINT('Ctrl Pts',(31.3161568302002,-3.92410140686709,337.964896492481));
#27638=CARTESIAN_POINT('Ctrl Pts',(31.3084048566772,-3.84151446908704,338.074202000971));
#27639=CARTESIAN_POINT('Ctrl Pts',(31.3006528831542,-3.75429279518361,338.18013922605));
#27640=CARTESIAN_POINT('Ctrl Pts',(31.2929009096312,-3.66274657769866,338.282296539019));
#27641=CARTESIAN_POINT('Ctrl Pts',(31.2851522190736,-3.57123913009104,338.384410588306));
#27642=CARTESIAN_POINT('Ctrl Pts',(31.2774035285159,-3.47541104183568,338.482747618863));
#27643=CARTESIAN_POINT('Ctrl Pts',(31.2696548379583,-3.37561280902233,338.57692902167));
#27644=CARTESIAN_POINT('Ctrl Pts',(31.2619077595805,-3.27583534006499,338.671090829249));
#27645=CARTESIAN_POINT('Ctrl Pts',(31.2541606812027,-3.17208965366063,338.76109846075));
#27646=CARTESIAN_POINT('Ctrl Pts',(31.2464136028248,-3.06476284550104,338.84661042521));
#27647=CARTESIAN_POINT('Ctrl Pts',(31.238666459519,-2.95743513783943,338.932123106343));
#27648=CARTESIAN_POINT('Ctrl Pts',(31.2309193162132,-2.84652655426544,339.013139801715));
#27649=CARTESIAN_POINT('Ctrl Pts',(31.2231721729074,-2.7324566625561,339.08935980928));
#27650=CARTESIAN_POINT('Ctrl Pts',(31.2154232878793,-2.61836112551333,339.16559695272));
#27651=CARTESIAN_POINT('Ctrl Pts',(31.2076744028513,-2.50110319099887,339.237035045346));
#27652=CARTESIAN_POINT('Ctrl Pts',(31.1999255178232,-2.38113039649116,339.303417374298));
#27653=CARTESIAN_POINT('Ctrl Pts',(31.1921684080485,-2.2610302616198,339.369870162138));
#27654=CARTESIAN_POINT('Ctrl Pts',(31.1844112982737,-2.13820985307904,339.431256277199));
#27655=CARTESIAN_POINT('Ctrl Pts',(31.176654188499,-2.01314073687532,339.487365311186));
#27656=CARTESIAN_POINT('Ctrl Pts',(31.1688929335728,-1.88800478773475,339.543504328046));
#27657=CARTESIAN_POINT('Ctrl Pts',(31.1611316786467,-1.76061809939056,339.594360500068));
#27658=CARTESIAN_POINT('Ctrl Pts',(31.1533704237205,-1.63147015798782,339.639772428266));
#27659=CARTESIAN_POINT('Ctrl Pts',(31.1455967533159,-1.50211562196822,339.685257000748));
#27660=CARTESIAN_POINT('Ctrl Pts',(31.1378230829112,-1.37099457687206,339.725279812042));
#27661=CARTESIAN_POINT('Ctrl Pts',(31.1300494125065,-1.23861039804341,339.759729755391));
#27662=CARTESIAN_POINT('Ctrl Pts',(31.1226376083294,-1.11238873458886,339.79257604559));
#27663=CARTESIAN_POINT('Ctrl Pts',(31.1152258041524,-0.985019169873967,
339.820356564486));
#27664=CARTESIAN_POINT('Ctrl Pts',(31.1078139999753,-0.856942901563595,
339.843018885567));
#27665=CARTESIAN_POINT('Ctrl Pts',(31.1000389211969,-0.722589233823908,
339.866791954512));
#27666=CARTESIAN_POINT('Ctrl Pts',(31.0922638424184,-0.587033253152717,
339.885007550787));
#27667=CARTESIAN_POINT('Ctrl Pts',(31.08448876364,-0.450774444236788,339.897548923995));
#27668=CARTESIAN_POINT('Ctrl Pts',(31.0767232525909,-0.314683310459706,
339.910074864245));
#27669=CARTESIAN_POINT('Ctrl Pts',(31.068957741542,-0.17789145479916,339.916940439105));
#27670=CARTESIAN_POINT('Ctrl Pts',(31.061192230493,-0.0409086434484924,
339.918079863665));
#27671=CARTESIAN_POINT('Ctrl Pts',(31.0534344189708,0.095938349045814,339.919218158483));
#27672=CARTESIAN_POINT('Ctrl Pts',(31.0456766074485,0.232975532103677,339.914641598307));
#27673=CARTESIAN_POINT('Ctrl Pts',(31.0379187959263,0.369688277670826,339.904336207873));
#27674=CARTESIAN_POINT('Ctrl Pts',(31.0301668224034,0.506298142561153,339.894038572571));
#27675=CARTESIAN_POINT('Ctrl Pts',(31.0224148488803,0.642583667729312,339.87802071736));
#27676=CARTESIAN_POINT('Ctrl Pts',(31.0146628753573,0.778030842837607,339.856320733857));
#27677=CARTESIAN_POINT('Ctrl Pts',(31.0069141847997,0.913420655987198,339.83462994031));
#27678=CARTESIAN_POINT('Ctrl Pts',(30.9991654942421,1.04797244008067,339.807261866306));
#27679=CARTESIAN_POINT('Ctrl Pts',(30.9914168036845,1.18117814117006,339.774306364418));
#27680=CARTESIAN_POINT('Ctrl Pts',(30.9836697253067,1.31435612770079,339.741357719197));
#27681=CARTESIAN_POINT('Ctrl Pts',(30.9759226469288,1.44618820909791,339.702824052225));
#27682=CARTESIAN_POINT('Ctrl Pts',(30.968175568551,1.57617773863676,339.658846080171));
#27683=CARTESIAN_POINT('Ctrl Pts',(30.9604284252452,1.70616835761289,339.61486773954));
#27684=CARTESIAN_POINT('Ctrl Pts',(30.9526812819394,1.83431602367146,339.565445128084));
#27685=CARTESIAN_POINT('Ctrl Pts',(30.9449341386336,1.96014081784816,339.510768342168));
#27686=CARTESIAN_POINT('Ctrl Pts',(30.9371852536055,2.08599390010994,339.456079263749));
#27687=CARTESIAN_POINT('Ctrl Pts',(30.9294363685774,2.20952271288873,339.396133816065));
#27688=CARTESIAN_POINT('Ctrl Pts',(30.9216874835493,2.33026919265421,339.331169420869));
#27689=CARTESIAN_POINT('Ctrl Pts',(30.9139303737746,2.45114383398085,339.266136071792));
#27690=CARTESIAN_POINT('Ctrl Pts',(30.9061732639998,2.56922989824594,339.196073319186));
#27691=CARTESIAN_POINT('Ctrl Pts',(30.8984161542251,2.68409525720108,339.121263848963));
#27692=CARTESIAN_POINT('Ctrl Pts',(30.8906548992989,2.79902199653145,339.046414402952));
#27693=CARTESIAN_POINT('Ctrl Pts',(30.8828936443728,2.91072428306379,338.966813411855));
#27694=CARTESIAN_POINT('Ctrl Pts',(30.8751323894466,3.01880150390626,338.882785152763));
#27695=CARTESIAN_POINT('Ctrl Pts',(30.867358719042,3.12705161307979,338.79862247584));
#27696=CARTESIAN_POINT('Ctrl Pts',(30.8595850486373,3.23166477017122,338.710018631373));
#27697=CARTESIAN_POINT('Ctrl Pts',(30.8518113782326,3.3322751378583,338.617336792187));
#27698=CARTESIAN_POINT('Ctrl Pts',(30.8443995740555,3.42820206872423,338.528969314913));
#27699=CARTESIAN_POINT('Ctrl Pts',(30.8369877698784,3.52049027966644,338.436895163454));
#27700=CARTESIAN_POINT('Ctrl Pts',(30.8295759657013,3.6088569267407,338.341456979345));
#27701=CARTESIAN_POINT('Ctrl Pts',(30.8218008869229,3.70155468641853,338.241341085538));
#27702=CARTESIAN_POINT('Ctrl Pts',(30.8140258081444,3.79022968928016,338.137206673786));
#27703=CARTESIAN_POINT('Ctrl Pts',(30.806250729366,3.87451345760266,338.029410591081));
#27704=CARTESIAN_POINT('Ctrl Pts',(30.798485218317,3.95869350938259,337.921747158319));
#27705=CARTESIAN_POINT('Ctrl Pts',(30.790719707268,4.03849283996574,337.810431325071));
#27706=CARTESIAN_POINT('Ctrl Pts',(30.782954196219,4.11358026568129,337.695856164616));
#27707=CARTESIAN_POINT('Ctrl Pts',(30.7751963846968,4.18859324199559,337.581394605766));
#27708=CARTESIAN_POINT('Ctrl Pts',(30.7674385731746,4.25890339785153,337.463680475659));
#27709=CARTESIAN_POINT('Ctrl Pts',(30.7596807616524,4.32422048638134,337.343138973185));
#27710=CARTESIAN_POINT('Ctrl Pts',(30.7519287881294,4.38948842173062,337.222688182015));
#27711=CARTESIAN_POINT('Ctrl Pts',(30.7441768146064,4.44977058328796,337.099414595818));
#27712=CARTESIAN_POINT('Ctrl Pts',(30.7364248410834,4.50482084261996,336.973771070412));
#27713=CARTESIAN_POINT('Ctrl Pts',(30.7286761505257,4.55984778813452,336.848180755114));
#27714=CARTESIAN_POINT('Ctrl Pts',(30.7209274599681,4.60964708178462,336.72022285411));
#27715=CARTESIAN_POINT('Ctrl Pts',(30.7131787694105,4.65401934537325,336.590373225187));
#27716=CARTESIAN_POINT('Ctrl Pts',(30.7054316910327,4.69838237694183,336.460550612564));
#27717=CARTESIAN_POINT('Ctrl Pts',(30.6976846126548,4.73732049807176,336.328837424542));
#27718=CARTESIAN_POINT('Ctrl Pts',(30.689937534277,4.77068327637423,336.195727451815));
#27719=CARTESIAN_POINT('Ctrl Pts',(30.6821903909712,4.80404633428892,336.062616363497));
#27720=CARTESIAN_POINT('Ctrl Pts',(30.6744432476654,4.83183386114659,335.92810884627));
#27721=CARTESIAN_POINT('Ctrl Pts',(30.6666961043596,4.85394600134562,335.79271134628));
#27722=CARTESIAN_POINT('Ctrl Pts',(30.6589472193315,4.87606311282318,335.657283406057));
#27723=CARTESIAN_POINT('Ctrl Pts',(30.6511983343034,4.89250223566147,335.520965470609));
#27724=CARTESIAN_POINT('Ctrl Pts',(30.6434494492753,4.90321513841902,335.384271217864));
#27725=CARTESIAN_POINT('Ctrl Pts',(30.6356923395006,4.91393941196226,335.247431876427));
#27726=CARTESIAN_POINT('Ctrl Pts',(30.6279352297258,4.91892529372301,335.110215810095));
#27727=CARTESIAN_POINT('Ctrl Pts',(30.6201781199511,4.91817665092632,334.973139382301));
#27728=CARTESIAN_POINT('Ctrl Pts',(30.6124168650249,4.91742760807885,334.835989705246));
#27729=CARTESIAN_POINT('Ctrl Pts',(30.6046556100988,4.9109379531716,334.698980205651));
#27730=CARTESIAN_POINT('Ctrl Pts',(30.5968943551726,4.89876358310378,334.562623252383));
#27731=CARTESIAN_POINT('Ctrl Pts',(30.5891206847679,4.88656973801147,334.426048172428));
#27732=CARTESIAN_POINT('Ctrl Pts',(30.5813470143632,4.86867305692279,334.290128112477));
#27733=CARTESIAN_POINT('Ctrl Pts',(30.5735733439585,4.84518096404822,334.155367246595));
#27734=CARTESIAN_POINT('Ctrl Pts',(30.5661615397815,4.82278243374894,334.026879531441));
#27735=CARTESIAN_POINT('Ctrl Pts',(30.5587497356045,4.79529776190851,333.89944579941));
#27736=CARTESIAN_POINT('Ctrl Pts',(30.5513379314274,4.76286202001619,333.773489323003));
#27737=CARTESIAN_POINT('Ctrl Pts',(30.543562852649,4.72883650579246,333.641359344482));
#27738=CARTESIAN_POINT('Ctrl Pts',(30.5357877738705,4.68925478955925,333.510437537347));
#27739=CARTESIAN_POINT('Ctrl Pts',(30.5280126950921,4.64421754712508,333.38122687276));
#27740=CARTESIAN_POINT('Ctrl Pts',(30.5202471840431,4.59923572588494,333.252175210121));
#27741=CARTESIAN_POINT('Ctrl Pts',(30.512481672994,4.54881186355072,333.124830865918));
#27742=CARTESIAN_POINT('Ctrl Pts',(30.504716161945,4.49309728134059,332.99968505407));
#27743=CARTESIAN_POINT('Ctrl Pts',(30.4969583504228,4.43743794030096,332.874663324659));
#27744=CARTESIAN_POINT('Ctrl Pts',(30.4892005389006,4.37649847670219,332.751836144362));
#27745=CARTESIAN_POINT('Ctrl Pts',(30.4814427273784,4.31047938012951,332.63167768748));
#27746=CARTESIAN_POINT('Ctrl Pts',(30.4736907538554,4.24450996502058,332.511609653648));
#27747=CARTESIAN_POINT('Ctrl Pts',(30.4659387803324,4.1734687130689,332.394206687002));
#27748=CARTESIAN_POINT('Ctrl Pts',(30.4581868068094,4.09760324617584,332.279920828463));
#27749=CARTESIAN_POINT('Ctrl Pts',(30.4504381162518,4.02176990835305,332.165683370053));
#27750=CARTESIAN_POINT('Ctrl Pts',(30.4426894256942,3.94111663481345,332.054560719145));
#27751=CARTESIAN_POINT('Ctrl Pts',(30.4349407351366,3.85593568953959,331.946978051072));
#27752=CARTESIAN_POINT('Ctrl Pts',(30.4271936567587,3.77077246687283,331.839417766472));
#27753=CARTESIAN_POINT('Ctrl Pts',(30.4194465783808,3.68108368870038,331.735396305966));
#27754=CARTESIAN_POINT('Ctrl Pts',(30.411699500003,3.58720318655211,331.635307389836));
#27755=CARTESIAN_POINT('Ctrl Pts',(30.4039523566972,3.49332189759481,331.535217634865));
#27756=CARTESIAN_POINT('Ctrl Pts',(30.3962052133914,3.39524908199738,331.439060775098));
#27757=CARTESIAN_POINT('Ctrl Pts',(30.3884580700856,3.2933565835326,331.347194848311));
#27758=CARTESIAN_POINT('Ctrl Pts',(30.3807091850575,3.19144117747106,331.255308268114));
#27759=CARTESIAN_POINT('Ctrl Pts',(30.3729603000294,3.08570466998124,331.167714802213));
#27760=CARTESIAN_POINT('Ctrl Pts',(30.3652114150013,2.97655292299249,331.08473299006));
#27761=CARTESIAN_POINT('Ctrl Pts',(30.3574543052266,2.86728532121158,331.001663100154));
#27762=CARTESIAN_POINT('Ctrl Pts',(30.3496971954519,2.75459555036754,330.923214878864));
#27763=CARTESIAN_POINT('Ctrl Pts',(30.3419400856772,2.63891992426349,330.84966450804));
#27764=CARTESIAN_POINT('Ctrl Pts',(30.334178830751,2.52318248480367,330.776074834249));
#27765=CARTESIAN_POINT('Ctrl Pts',(30.3264175758248,2.40445634897829,330.707388421677));
#27766=CARTESIAN_POINT('Ctrl Pts',(30.3186563208987,2.28320262771825,330.643835537623));
#27767=CARTESIAN_POINT('Ctrl Pts',(30.310882650494,2.16175494002051,330.580180989665));
#27768=CARTESIAN_POINT('Ctrl Pts',(30.3031089800893,2.0377719408323,330.521676547071));
#27769=CARTESIAN_POINT('Ctrl Pts',(30.2953353096846,1.91173573428443,330.468504712045));
#27770=CARTESIAN_POINT('Ctrl Pts',(30.2879235055076,1.79156654347443,330.417808038732));
#27771=CARTESIAN_POINT('Ctrl Pts',(30.2805117013306,1.66953126652681,330.371958781094));
#27772=CARTESIAN_POINT('Ctrl Pts',(30.2730998971535,1.54605893725225,330.331072411673));
#27773=CARTESIAN_POINT('Ctrl Pts',(30.2653248183751,1.41653486131422,330.288182079492));
#27774=CARTESIAN_POINT('Ctrl Pts',(30.2575497395966,1.28501998274813,330.250617886979));
#27775=CARTESIAN_POINT('Ctrl Pts',(30.2497746608182,1.15199174219043,330.218567360254));
#27776=CARTESIAN_POINT('Ctrl Pts',(30.2420091497692,1.01912720135174,330.186556273744));
#27777=CARTESIAN_POINT('Ctrl Pts',(30.2342436387202,0.884753380309309,330.160045443661));
#27778=CARTESIAN_POINT('Ctrl Pts',(30.2264781276712,0.749365239921871,330.139173444804));
#27779=CARTESIAN_POINT('Ctrl Pts',(30.218720316149,0.614111337269706,330.118322140595));
#27780=CARTESIAN_POINT('Ctrl Pts',(30.2109625046267,0.477845500495644,330.10309860054));
#27781=CARTESIAN_POINT('Ctrl Pts',(30.2032046931045,0.341074969304791,330.093590831594));
#27782=CARTESIAN_POINT('Ctrl Pts',(30.1954527195815,0.204407362275902,330.084090217546));
#27783=CARTESIAN_POINT('Ctrl Pts',(30.1877007460585,0.0672362051638616,
330.080296840078));
#27784=CARTESIAN_POINT('Ctrl Pts',(30.1799487725355,-0.0699243687591812,
330.082247093931));
#27785=CARTESIAN_POINT('Ctrl Pts',(30.1722000819779,-0.207026855097548,
330.084196521849));
#27786=CARTESIAN_POINT('Ctrl Pts',(30.1644513914202,-0.344118377139885,
330.091884737608));
#27787=CARTESIAN_POINT('Ctrl Pts',(30.1567027008626,-0.480683235067083,
330.105296056959));
#27788=CARTESIAN_POINT('Ctrl Pts',(30.1489556224848,-0.617219679534977,
330.118704585972));
#27789=CARTESIAN_POINT('Ctrl Pts',(30.1412085441069,-0.753229289085119,
330.137833811933));
#27790=CARTESIAN_POINT('Ctrl Pts',(30.1334614657291,-0.888200320536573,
330.162616073424));
#27791=CARTESIAN_POINT('Ctrl Pts',(30.1257143224233,-1.02317248317527,330.187398542613));
#27792=CARTESIAN_POINT('Ctrl Pts',(30.1179671791175,-1.15710566590641,330.217834071242));
#27793=CARTESIAN_POINT('Ctrl Pts',(30.1102200358117,-1.28949756112466,330.253803722732));
#27794=CARTESIAN_POINT('Ctrl Pts',(30.1024711507836,-1.42191922085154,330.289781460963));
#27795=CARTESIAN_POINT('Ctrl Pts',(30.0947222657555,-1.55279852641434,330.33129569539));
#27796=CARTESIAN_POINT('Ctrl Pts',(30.0869733807274,-1.68164797601495,330.378177508032));
#27797=CARTESIAN_POINT('Ctrl Pts',(30.0792162709527,-1.81063418775281,330.425109081514));
#27798=CARTESIAN_POINT('Ctrl Pts',(30.071459161178,-1.93758587179635,330.477419480049));
#27799=CARTESIAN_POINT('Ctrl Pts',(30.0637020514033,-2.06203466650152,330.534891255899));
#27800=CARTESIAN_POINT('Ctrl Pts',(30.0559407964771,-2.18654996266339,330.592393742828));
#27801=CARTESIAN_POINT('Ctrl Pts',(30.0481795415509,-2.30855935695502,330.655062924287));
#27802=CARTESIAN_POINT('Ctrl Pts',(30.0404182866247,-2.42761967910912,330.722635653103));
#27803=CARTESIAN_POINT('Ctrl Pts',(30.0326446162201,-2.54687045897701,330.790316476264));
#27804=CARTESIAN_POINT('Ctrl Pts',(30.0248709458154,-2.66316240789581,330.862916314471));
#27805=CARTESIAN_POINT('Ctrl Pts',(30.0170972754107,-2.77608116165939,330.94012851849));
#27806=CARTESIAN_POINT('Ctrl Pts',(30.0096854712336,-2.8837435202689,331.013746475836));
#27807=CARTESIAN_POINT('Ctrl Pts',(30.0022736670566,-2.98833942990736,331.091556879592));
#27808=CARTESIAN_POINT('Ctrl Pts',(29.9948618628795,-3.08953961243817,331.173261434893));
#27809=CARTESIAN_POINT('Ctrl Pts',(29.9871879224333,-3.1943189826596,331.25785566817));
#27810=CARTESIAN_POINT('Ctrl Pts',(29.9795139819871,-3.29580784769039,331.346907308451));
#27811=CARTESIAN_POINT('Ctrl Pts',(29.971840041541,-3.39359577220477,331.440127699288));
#27812=CARTESIAN_POINT('Ctrl Pts',(29.9641755913701,-3.49126276350013,331.533232805524));
#27813=CARTESIAN_POINT('Ctrl Pts',(29.9565111411992,-3.58523762853864,331.630496135086));
#27814=CARTESIAN_POINT('Ctrl Pts',(29.9488466910283,-3.67514112279571,331.731587420469));
#27815=CARTESIAN_POINT('Ctrl Pts',(29.941189771001,-3.76495628896586,331.832579386021));
#27816=CARTESIAN_POINT('Ctrl Pts',(29.9335328509736,-3.8507077755645,331.93739152815));
#27817=CARTESIAN_POINT('Ctrl Pts',(29.9258759309463,-3.93205187648206,332.045655554416));
#27818=CARTESIAN_POINT('Ctrl Pts',(29.9182246515771,-4.01333605327071,332.153839825328));
#27819=CARTESIAN_POINT('Ctrl Pts',(29.910573372208,-4.09021906416721,332.265470600495));
#27820=CARTESIAN_POINT('Ctrl Pts',(29.9029220928388,-4.16239667494011,332.380145617988));
#27821=CARTESIAN_POINT('Ctrl Pts',(29.895273816448,-4.23454595740404,332.494775627766));
#27822=CARTESIAN_POINT('Ctrl Pts',(29.8876255400571,-4.30199329779169,332.612447164746));
#27823=CARTESIAN_POINT('Ctrl Pts',(29.8799772636663,-4.36447731831841,332.732728335557));
#27824=CARTESIAN_POINT('Ctrl Pts',(29.8723302316669,-4.42695117255783,332.852989936358));
#27825=CARTESIAN_POINT('Ctrl Pts',(29.8646831996675,-4.48446312793866,332.975859969888));
#27826=CARTESIAN_POINT('Ctrl Pts',(29.857036167668,-4.53679764761379,333.100881739568));
#27827=CARTESIAN_POINT('Ctrl Pts',(29.84938862272,-4.58913567779022,333.225911895474));
#27828=CARTESIAN_POINT('Ctrl Pts',(29.841741077772,-4.63629542740628,333.35309370338));
#27829=CARTESIAN_POINT('Ctrl Pts',(29.834093532824,-4.67810962638648,333.481950795919));
#27830=CARTESIAN_POINT('Ctrl Pts',(29.8264396786577,-4.71995832204658,333.610914195454));
#27831=CARTESIAN_POINT('Ctrl Pts',(29.8187858244914,-4.75645253434975,333.741555257285));
#27832=CARTESIAN_POINT('Ctrl Pts',(29.8111319703251,-4.78747492394016,333.873382533801));
#27833=CARTESIAN_POINT('Ctrl Pts',(29.8034748858929,-4.81851040635478,334.005265447275));
#27834=CARTESIAN_POINT('Ctrl Pts',(29.7958178014607,-4.844069390303,334.138335178013));
#27835=CARTESIAN_POINT('Ctrl Pts',(29.7881607170285,-4.86408598944587,334.272091661144));
#27836=CARTESIAN_POINT('Ctrl Pts',(29.7804931283228,-4.88413004810485,334.406031636399));
#27837=CARTESIAN_POINT('Ctrl Pts',(29.772825539617,-4.89861649109298,334.540659846392));
#27838=CARTESIAN_POINT('Ctrl Pts',(29.7651579509112,-4.90753143194119,334.675472178374));
#27839=CARTESIAN_POINT('Ctrl Pts',(29.7589507167834,-4.91474844985958,334.784608406208));
#27840=CARTESIAN_POINT('Ctrl Pts',(29.7527434826556,-4.91831513988253,334.893865175375));
#27841=CARTESIAN_POINT('Ctrl Pts',(29.7465362485277,-4.91824909912948,335.002976812401));
#27842=CARTESIAN_POINT('',(33.2465372519956,-4.91612741639346,334.995890487429));
#27843=CARTESIAN_POINT('Ctrl Pts',(33.2465362484901,-4.91824829644928,334.995906471729));
#27844=CARTESIAN_POINT('Ctrl Pts',(33.2385755814652,-4.91836558057476,335.136819740692));
#27845=CARTESIAN_POINT('Ctrl Pts',(33.2306149144403,-4.91242204025201,335.27782646653));
#27846=CARTESIAN_POINT('Ctrl Pts',(33.2226542474154,-4.90042391361396,335.418364111009));
#27847=CARTESIAN_POINT('Ctrl Pts',(33.214938036397,-4.88879422521277,335.554586128265));
#27848=CARTESIAN_POINT('Ctrl Pts',(33.2072218253785,-4.87147638372207,335.690367031991));
#27849=CARTESIAN_POINT('Ctrl Pts',(33.1995056143601,-4.84852893196693,335.825197102746));
#27850=CARTESIAN_POINT('Ctrl Pts',(33.1917896841848,-4.82558231541894,335.960022266156));
#27851=CARTESIAN_POINT('Ctrl Pts',(33.1840737540096,-4.79700656195118,336.093896276925));
#27852=CARTESIAN_POINT('Ctrl Pts',(33.1763578238343,-4.76291165079966,336.226317931524));
#27853=CARTESIAN_POINT('Ctrl Pts',(33.1686404726742,-4.72881046064511,336.358763973222));
#27854=CARTESIAN_POINT('Ctrl Pts',(33.1609231215142,-4.6891881887503,336.489756745004));
#27855=CARTESIAN_POINT('Ctrl Pts',(33.1532057703542,-4.64420504520035,336.618808994488));
#27856=CARTESIAN_POINT('Ctrl Pts',(33.1454852957562,-4.59920369565548,336.747913475195));
#27857=CARTESIAN_POINT('Ctrl Pts',(33.1377648211582,-4.54883728704591,336.875075499219));
#27858=CARTESIAN_POINT('Ctrl Pts',(33.1300443465603,-4.49331446627497,336.999827034937));
#27859=CARTESIAN_POINT('Ctrl Pts',(33.1223148311214,-4.43772662709326,337.124724657371));
#27860=CARTESIAN_POINT('Ctrl Pts',(33.1145853156826,-4.37697048298475,337.247205797077));
#27861=CARTESIAN_POINT('Ctrl Pts',(33.1068558002437,-4.31130118631532,337.366825963897));
#27862=CARTESIAN_POINT('Ctrl Pts',(33.099120859815,-4.24558579939964,337.486530086587));
#27863=CARTESIAN_POINT('Ctrl Pts',(33.0913859193863,-4.1749505960538,337.603368901739));
#27864=CARTESIAN_POINT('Ctrl Pts',(33.0836509789576,-4.09969386809841,337.716927170606));
#27865=CARTESIAN_POINT('Ctrl Pts',(33.0759049469835,-4.02432922549006,337.830648276757));
#27866=CARTESIAN_POINT('Ctrl Pts',(33.0681589150093,-3.94433006251908,337.941079131096));
#27867=CARTESIAN_POINT('Ctrl Pts',(33.0604128830352,-3.86003489097701,338.047837545366));
#27868=CARTESIAN_POINT('Ctrl Pts',(33.0587686686544,-3.84214194478911,338.070498660192));
#27869=CARTESIAN_POINT('Ctrl Pts',(33.0571244542736,-3.82405556599331,338.092994440948));
#27870=CARTESIAN_POINT('Ctrl Pts',(33.0554802398928,-3.80577919883156,338.115321452473));
#27871=CARTESIAN_POINT('Ctrl Pts',(33.0477051611144,-3.71935482733553,338.220900308566));
#27872=CARTESIAN_POINT('Ctrl Pts',(33.0399300823359,-3.62839715136282,338.323046933694));
#27873=CARTESIAN_POINT('Ctrl Pts',(33.0321550035575,-3.53320898375705,338.421347298887));
#27874=CARTESIAN_POINT('Ctrl Pts',(33.0243894925085,-3.43813795125148,338.519526699222));
#27875=CARTESIAN_POINT('Ctrl Pts',(33.0166239814595,-3.33884705464954,338.613868978955));
#27876=CARTESIAN_POINT('Ctrl Pts',(33.0088584704104,-3.23568011531128,338.7039920699));
#27877=CARTESIAN_POINT('Ctrl Pts',(33.0011006588883,-3.13261546629395,338.794025803537));
#27878=CARTESIAN_POINT('Ctrl Pts',(32.9933428473661,-3.02568271501763,338.879848417969));
#27879=CARTESIAN_POINT('Ctrl Pts',(32.9855850358439,-2.9152631303013,338.961113977609));
#27880=CARTESIAN_POINT('Ctrl Pts',(32.9778330623208,-2.80492663982333,339.042318382338));
#27881=CARTESIAN_POINT('Ctrl Pts',(32.9700810887978,-2.691108852294,339.11897232743));
#27882=CARTESIAN_POINT('Ctrl Pts',(32.9623291152747,-2.57422449503257,339.190769775551));
#27883=CARTESIAN_POINT('Ctrl Pts',(32.9545804247171,-2.45738963836647,339.26253681741));
#27884=CARTESIAN_POINT('Ctrl Pts',(32.9468317341594,-2.33749112734454,339.32945124883));
#27885=CARTESIAN_POINT('Ctrl Pts',(32.9390830436018,-2.21497289874997,339.391250177376));
#27886=CARTESIAN_POINT('Ctrl Pts',(32.931335965224,-2.09248016109599,339.453036248139));
#27887=CARTESIAN_POINT('Ctrl Pts',(32.9235888868462,-1.96736913879282,339.50970875712));
#27888=CARTESIAN_POINT('Ctrl Pts',(32.9158418084683,-1.84010825891691,339.561050828259));
#27889=CARTESIAN_POINT('Ctrl Pts',(32.9080946651625,-1.71284631247242,339.612393329695));
#27890=CARTESIAN_POINT('Ctrl Pts',(32.9003475218567,-1.58343483500336,339.658405157943));
#27891=CARTESIAN_POINT('Ctrl Pts',(32.8926003785509,-1.4523617406965,339.698917794201));
#27892=CARTESIAN_POINT('Ctrl Pts',(32.8848514935228,-1.32125917837545,339.739439538561));
#27893=CARTESIAN_POINT('Ctrl Pts',(32.8771026084947,-1.18849462923059,339.77445951536));
#27894=CARTESIAN_POINT('Ctrl Pts',(32.8693537234666,-1.05457026632765,339.803859345971));
#27895=CARTESIAN_POINT('Ctrl Pts',(32.8615966136919,-0.920503754722047,
339.833290381867));
#27896=CARTESIAN_POINT('Ctrl Pts',(32.8538395039171,-0.785275352630049,
339.857089271423));
#27897=CARTESIAN_POINT('Ctrl Pts',(32.8460823941423,-0.649397054085376,
339.875188871074));
#27898=CARTESIAN_POINT('Ctrl Pts',(32.8383211392162,-0.5134461465226,339.893298142572));
#27899=CARTESIAN_POINT('Ctrl Pts',(32.8305598842901,-0.376845039588008,
339.905702020367));
#27900=CARTESIAN_POINT('Ctrl Pts',(32.8227986293639,-0.240108922136284,
339.91238544579));
#27901=CARTESIAN_POINT('Ctrl Pts',(32.8150249589592,-0.103154071458833,
339.919079562516));
#27902=CARTESIAN_POINT('Ctrl Pts',(32.8072512885546,0.0339358302430315,
339.920034938019));
#27903=CARTESIAN_POINT('Ctrl Pts',(32.7994776181499,0.170646628716568,339.915288678258));
#27904=CARTESIAN_POINT('Ctrl Pts',(32.7920658139729,0.300993506628775,339.91076335803));
#27905=CARTESIAN_POINT('Ctrl Pts',(32.7846540097959,0.430995494545105,339.90105530039));
#27906=CARTESIAN_POINT('Ctrl Pts',(32.7772422056189,0.560214771800575,339.886240116077));
#27907=CARTESIAN_POINT('Ctrl Pts',(32.7694671268405,0.695767470760528,339.870698795448));
#27908=CARTESIAN_POINT('Ctrl Pts',(32.761692048062,0.830887164652608,339.849487945254));
#27909=CARTESIAN_POINT('Ctrl Pts',(32.7539169692836,0.965061818276978,339.822638152444));
#27910=CARTESIAN_POINT('Ctrl Pts',(32.7461514582346,1.09907136144809,339.795821400012));
#27911=CARTESIAN_POINT('Ctrl Pts',(32.7383859471855,1.23213779864149,339.763379587704));
#27912=CARTESIAN_POINT('Ctrl Pts',(32.7306204361365,1.36375377910245,339.725395083216));
#27913=CARTESIAN_POINT('Ctrl Pts',(32.7228626246143,1.4952392619355,339.687448240475));
#27914=CARTESIAN_POINT('Ctrl Pts',(32.7151048130922,1.62527677687213,339.643969749787));
#27915=CARTESIAN_POINT('Ctrl Pts',(32.70734700157,1.75336909286239,339.595093022638));
#27916=CARTESIAN_POINT('Ctrl Pts',(32.6995950280469,1.88136501532299,339.546253076776));
#27917=CARTESIAN_POINT('Ctrl Pts',(32.6918430545239,2.00741828878591,339.492023119139));
#27918=CARTESIAN_POINT('Ctrl Pts',(32.6840910810008,2.13104712717919,339.432586288415));
#27919=CARTESIAN_POINT('Ctrl Pts',(32.6763423904432,2.25462360868584,339.373174629224));
#27920=CARTESIAN_POINT('Ctrl Pts',(32.6685936998856,2.37577734571228,339.308560651773));
#27921=CARTESIAN_POINT('Ctrl Pts',(32.6608450093279,2.49404702673606,339.238975405794));
#27922=CARTESIAN_POINT('Ctrl Pts',(32.6530979309501,2.61229210076489,339.169404637607));
#27923=CARTESIAN_POINT('Ctrl Pts',(32.6453508525723,2.72765397565889,339.094864856303));
#27924=CARTESIAN_POINT('Ctrl Pts',(32.6376037741945,2.83969678294388,339.015632608125));
#27925=CARTESIAN_POINT('Ctrl Pts',(32.6298566308887,2.9517405292552,338.936399695905));
#27926=CARTESIAN_POINT('Ctrl Pts',(32.6221094875828,3.06046483333505,338.852474464051));
#27927=CARTESIAN_POINT('Ctrl Pts',(32.6143623442771,3.16546394576596,338.764176014821));
#27928=CARTESIAN_POINT('Ctrl Pts',(32.606613459249,3.27048666422669,338.675857714225));
#27929=CARTESIAN_POINT('Ctrl Pts',(32.5988645742209,3.37178222540607,338.583164491334));
#27930=CARTESIAN_POINT('Ctrl Pts',(32.5911156891928,3.46897932753056,338.486454572724));
#27931=CARTESIAN_POINT('Ctrl Pts',(32.583358579418,3.56627959566361,338.389642005207));
#27932=CARTESIAN_POINT('Ctrl Pts',(32.5756014696433,3.65947243739439,338.288804501635));
#27933=CARTESIAN_POINT('Ctrl Pts',(32.5678443598686,3.7482243209166,338.184336273478));
#27934=CARTESIAN_POINT('Ctrl Pts',(32.5600831049424,3.83702363060768,338.079812220841));
#27935=CARTESIAN_POINT('Ctrl Pts',(32.5523218500163,3.92137701320233,337.971653885771));
#27936=CARTESIAN_POINT('Ctrl Pts',(32.5445605950901,4.00099300729565,337.86028635246));
#27937=CARTESIAN_POINT('Ctrl Pts',(32.5367869246854,4.08073636103262,337.748740667391));
#27938=CARTESIAN_POINT('Ctrl Pts',(32.5290132542807,4.15572696870276,337.633975852869));
#27939=CARTESIAN_POINT('Ctrl Pts',(32.5212395838761,4.22571779513056,337.516444352339));
#27940=CARTESIAN_POINT('Ctrl Pts',(32.513827779699,4.29245053174894,337.404383971435));
#27941=CARTESIAN_POINT('Ctrl Pts',(32.506415975522,4.35463835414161,337.289808939287));
#27942=CARTESIAN_POINT('Ctrl Pts',(32.4990041713449,4.41210791510817,337.173128345943));
#27943=CARTESIAN_POINT('Ctrl Pts',(32.4912290925665,4.47239423045099,337.050728889144));
#27944=CARTESIAN_POINT('Ctrl Pts',(32.4834540137881,4.52767859354105,336.92562544778));
#27945=CARTESIAN_POINT('Ctrl Pts',(32.4756789350097,4.57770963396754,336.798265155527));
#27946=CARTESIAN_POINT('Ctrl Pts',(32.4679134239606,4.62767910801365,336.67106158822));
#27947=CARTESIAN_POINT('Ctrl Pts',(32.4601479129116,4.6724079804435,336.541607056186));
#27948=CARTESIAN_POINT('Ctrl Pts',(32.4523824018626,4.71169095940682,336.410372775384));
#27949=CARTESIAN_POINT('Ctrl Pts',(32.4446245903404,4.7509349891821,336.279268613754));
#27950=CARTESIAN_POINT('Ctrl Pts',(32.4368667788182,4.78474375967213,336.146388587108));
#27951=CARTESIAN_POINT('Ctrl Pts',(32.4291089672961,4.8129603791914,336.012223024256));
#27952=CARTESIAN_POINT('Ctrl Pts',(32.4213569937731,4.84115576480965,335.878158425245));
#27953=CARTESIAN_POINT('Ctrl Pts',(32.4136050202501,4.86376729569296,335.74281059657));
#27954=CARTESIAN_POINT('Ctrl Pts',(32.4058530467271,4.88068825498377,335.60668378927));
#27955=CARTESIAN_POINT('Ctrl Pts',(32.3981043561695,4.89760204823829,335.470614631755));
#27956=CARTESIAN_POINT('Ctrl Pts',(32.3903556656119,4.90883001502641,335.33376753884));
#27957=CARTESIAN_POINT('Ctrl Pts',(32.3826069750543,4.91431680786163,335.196655471494));
#27958=CARTESIAN_POINT('Ctrl Pts',(32.3748598966765,4.91980245912377,335.05957193146));
#27959=CARTESIAN_POINT('Ctrl Pts',(32.3671128182986,4.91954929675717,334.922223916969));
#27960=CARTESIAN_POINT('Ctrl Pts',(32.3593657399208,4.91355400095527,334.78512761416));
#27961=CARTESIAN_POINT('Ctrl Pts',(32.351618596615,4.90755865490702,334.648030162352));
#27962=CARTESIAN_POINT('Ctrl Pts',(32.3438714533092,4.89582109651214,334.511184816935));
#27963=CARTESIAN_POINT('Ctrl Pts',(32.3361243100034,4.8783900913741,334.375105465792));
#27964=CARTESIAN_POINT('Ctrl Pts',(32.3283754249753,4.86095516737602,334.238995521121));
#27965=CARTESIAN_POINT('Ctrl Pts',(32.3206265399472,4.83782429921578,334.103652301037));
#27966=CARTESIAN_POINT('Ctrl Pts',(32.3128776549191,4.80909779456918,333.969581898077));
#27967=CARTESIAN_POINT('Ctrl Pts',(32.3051205451444,4.78034079931375,333.835369191407));
#27968=CARTESIAN_POINT('Ctrl Pts',(32.2973634353697,4.74597638535125,333.702432383376));
#27969=CARTESIAN_POINT('Ctrl Pts',(32.289606325595,4.7061555603185,333.571265278443));
#27970=CARTESIAN_POINT('Ctrl Pts',(32.2818450706688,4.6663134563101,333.440028082003));
#27971=CARTESIAN_POINT('Ctrl Pts',(32.2740838157427,4.62100926041166,333.310562841749));
#27972=CARTESIAN_POINT('Ctrl Pts',(32.2663225608165,4.57044270849739,333.183344691241));
#27973=CARTESIAN_POINT('Ctrl Pts',(32.2585488904119,4.51979526657965,333.055923033153));
#27974=CARTESIAN_POINT('Ctrl Pts',(32.2507752200072,4.46386880641896,332.930756004967));
#27975=CARTESIAN_POINT('Ctrl Pts',(32.2430015496026,4.40291011245137,332.808296186942));
#27976=CARTESIAN_POINT('Ctrl Pts',(32.2355897454254,4.34478906035313,332.691536902907));
#27977=CARTESIAN_POINT('Ctrl Pts',(32.2281779412482,4.28209387050131,332.577238712127));
#27978=CARTESIAN_POINT('Ctrl Pts',(32.2207661370711,4.21507474732732,332.465768768059));
#27979=CARTESIAN_POINT('Ctrl Pts',(32.2129910582926,4.14477081728747,332.348835349982));
#27980=CARTESIAN_POINT('Ctrl Pts',(32.2052159795142,4.0694862055636,332.234644899063));
#27981=CARTESIAN_POINT('Ctrl Pts',(32.1974409007357,3.98946088544972,332.123650767732));
#27982=CARTESIAN_POINT('Ctrl Pts',(32.1896753896867,3.909534041587,332.012793221746));
#27983=CARTESIAN_POINT('Ctrl Pts',(32.1819098786377,3.82487832322155,331.905124483288));
#27984=CARTESIAN_POINT('Ctrl Pts',(32.1741443675887,3.73577889070845,331.801072188649));
#27985=CARTESIAN_POINT('Ctrl Pts',(32.1663865560664,3.6467678005419,331.697123062162));
#27986=CARTESIAN_POINT('Ctrl Pts',(32.1586287445442,3.55332201692302,331.596783538706));
#27987=CARTESIAN_POINT('Ctrl Pts',(32.150870933022,3.45576896471481,331.500450896899));
#27988=CARTESIAN_POINT('Ctrl Pts',(32.143118959499,3.35828932427225,331.40419074846));
#27989=CARTESIAN_POINT('Ctrl Pts',(32.1353669859759,3.25670884443015,331.311931753392));
#27990=CARTESIAN_POINT('Ctrl Pts',(32.1276150124529,3.15139381003039,331.224036531347));
#27991=CARTESIAN_POINT('Ctrl Pts',(32.1198663218953,3.04612337661021,331.136178532981));
#27992=CARTESIAN_POINT('Ctrl Pts',(32.1121176313377,2.93712183376301,331.05268088191));
#27993=CARTESIAN_POINT('Ctrl Pts',(32.1043689407801,2.82479058960962,330.97386771363));
#27994=CARTESIAN_POINT('Ctrl Pts',(32.0966218624023,2.7124827169098,330.895070943088));
#27995=CARTESIAN_POINT('Ctrl Pts',(32.0888747840245,2.59684684064964,330.820956941054));
#27996=CARTESIAN_POINT('Ctrl Pts',(32.0811277056466,2.47831523622769,330.751807837164));
#27997=CARTESIAN_POINT('Ctrl Pts',(32.0733805623408,2.35978263839706,330.682658153738));
#27998=CARTESIAN_POINT('Ctrl Pts',(32.065633419035,2.23835460162027,330.618473648413));
#27999=CARTESIAN_POINT('Ctrl Pts',(32.0578862757292,2.11448965504715,330.559491407372));
#28000=CARTESIAN_POINT('Ctrl Pts',(32.0501373907011,1.99059686100465,330.500495905872));
#28001=CARTESIAN_POINT('Ctrl Pts',(32.0423885056731,1.86426641980479,330.446705164004));
#28002=CARTESIAN_POINT('Ctrl Pts',(32.034639620645,1.73597819769921,330.398308706615));
#28003=CARTESIAN_POINT('Ctrl Pts',(32.0268825108703,1.6075538091487,330.349860880726));
#28004=CARTESIAN_POINT('Ctrl Pts',(32.0191254010956,1.47716785496841,330.306818914822));
#28005=CARTESIAN_POINT('Ctrl Pts',(32.0113682913208,1.34531730475887,330.269323049286));
#28006=CARTESIAN_POINT('Ctrl Pts',(32.0036070363947,1.2133962978306,330.231807147158));
#28007=CARTESIAN_POINT('Ctrl Pts',(31.9958457814685,1.0800095153258,330.199843341796));
#28008=CARTESIAN_POINT('Ctrl Pts',(31.9880845265423,0.945664595734111,330.173520793075));
#28009=CARTESIAN_POINT('Ctrl Pts',(31.9803108561376,0.811104768054161,330.147156136855));
#28010=CARTESIAN_POINT('Ctrl Pts',(31.9725371857329,0.675584127078492,330.126450829309));
#28011=CARTESIAN_POINT('Ctrl Pts',(31.9647635153282,0.539616806420292,330.111442261287));
#28012=CARTESIAN_POINT('Ctrl Pts',(31.9573517111512,0.40997879725149,330.097132345718));
#28013=CARTESIAN_POINT('Ctrl Pts',(31.9499399069741,0.279935045503705,330.088000758948));
#28014=CARTESIAN_POINT('Ctrl Pts',(31.9425281027971,0.149929698326431,330.084035786536));
#28015=CARTESIAN_POINT('Ctrl Pts',(31.9347530240187,0.0135524018171826,
330.079876479015));
#28016=CARTESIAN_POINT('Ctrl Pts',(31.9269779452402,-0.12321360774063,330.081389909902));
#28017=CARTESIAN_POINT('Ctrl Pts',(31.9192028664618,-0.259857233298094,
330.088619615546));
#28018=CARTESIAN_POINT('Ctrl Pts',(31.9114373554128,-0.396332710175151,
330.095840424577));
#28019=CARTESIAN_POINT('Ctrl Pts',(31.9036718443638,-0.532685716108326,
330.10876349179));
#28020=CARTESIAN_POINT('Ctrl Pts',(31.8959063333147,-0.668402325986071,
330.127380438294));
#28021=CARTESIAN_POINT('Ctrl Pts',(31.8881485217925,-0.803984372450086,
330.145978926042));
#28022=CARTESIAN_POINT('Ctrl Pts',(31.8803907102703,-0.938930893808257,
330.170260005443));
#28023=CARTESIAN_POINT('Ctrl Pts',(31.8726328987481,-1.07273062161303,330.2001633282));
#28024=CARTESIAN_POINT('Ctrl Pts',(31.8648809252251,-1.20642966088014,330.230044147759));
#28025=CARTESIAN_POINT('Ctrl Pts',(31.857128951702,-1.33898324442268,330.265538704331));
#28026=CARTESIAN_POINT('Ctrl Pts',(31.849376978179,-1.46988821989237,330.306535215481));
#28027=CARTESIAN_POINT('Ctrl Pts',(31.8416282876214,-1.60073775702633,330.347514364583));
#28028=CARTESIAN_POINT('Ctrl Pts',(31.8338795970637,-1.72993970249786,330.393990717321));
#28029=CARTESIAN_POINT('Ctrl Pts',(31.8261309065061,-1.85700425888646,330.445802129356));
#28030=CARTESIAN_POINT('Ctrl Pts',(31.8183838281283,-1.98404237843301,330.497602761595));
#28031=CARTESIAN_POINT('Ctrl Pts',(31.8106367497505,-2.10894363172539,330.554736097764));
#28032=CARTESIAN_POINT('Ctrl Pts',(31.8028896713726,-2.23123684091283,330.616991304794));
#28033=CARTESIAN_POINT('Ctrl Pts',(31.7951425280668,-2.35353107503499,330.679247033582));
#28034=CARTESIAN_POINT('Ctrl Pts',(31.787395384761,-2.47321687311857,330.746624541524));
#28035=CARTESIAN_POINT('Ctrl Pts',(31.7796482414552,-2.58984672790028,330.818866542613));
#28036=CARTESIAN_POINT('Ctrl Pts',(31.7718993564271,-2.70650280354979,330.891124785237));
#28037=CARTESIAN_POINT('Ctrl Pts',(31.764150471399,-2.82010123653514,330.968249491448));
#28038=CARTESIAN_POINT('Ctrl Pts',(31.7564015863709,-2.93022296820521,331.049939694245));
#28039=CARTESIAN_POINT('Ctrl Pts',(31.7486444765962,-3.04046158421874,331.131716603867));
#28040=CARTESIAN_POINT('Ctrl Pts',(31.7408873668215,-3.14721581295896,331.218068456901));
#28041=CARTESIAN_POINT('Ctrl Pts',(31.7331302570468,-3.2500987845288,331.308653233127));
#28042=CARTESIAN_POINT('Ctrl Pts',(31.7253690021206,-3.35303673346916,331.39928641496));
#28043=CARTESIAN_POINT('Ctrl Pts',(31.7176077471944,-3.45209902106075,331.494156756887));
#28044=CARTESIAN_POINT('Ctrl Pts',(31.7098464922682,-3.54693595854771,331.592885624394));
#28045=CARTESIAN_POINT('Ctrl Pts',(31.7020728218636,-3.64192460422749,331.691772425914));
#28046=CARTESIAN_POINT('Ctrl Pts',(31.6942991514589,-3.73267413407582,331.794529794133));
#28047=CARTESIAN_POINT('Ctrl Pts',(31.6865254810542,-3.81887487813061,331.900745617462));
#28048=CARTESIAN_POINT('Ctrl Pts',(31.6791136768772,-3.90106295681072,332.00201706866));
#28049=CARTESIAN_POINT('Ctrl Pts',(31.6717018727001,-3.97911603891936,332.106432008296));
#28050=CARTESIAN_POINT('Ctrl Pts',(31.664290068523,-4.0528036218724,332.213610604198));
#28051=CARTESIAN_POINT('Ctrl Pts',(31.6564069701454,-4.1311767752573,332.327604362707));
#28052=CARTESIAN_POINT('Ctrl Pts',(31.6485238717677,-4.2048548864954,332.44507877176));
#28053=CARTESIAN_POINT('Ctrl Pts',(31.6406407733901,-4.27351847197092,332.56561651907));
#28054=CARTESIAN_POINT('Ctrl Pts',(31.6327680418378,-4.34209176003261,332.685995750819));
#28055=CARTESIAN_POINT('Ctrl Pts',(31.6248953102855,-4.40566346273056,332.809429978934));
#28056=CARTESIAN_POINT('Ctrl Pts',(31.6170225787332,-4.46395620642664,332.935471470382));
#28057=CARTESIAN_POINT('Ctrl Pts',(31.609158664089,-4.5221836663311,333.061371804186));
#28058=CARTESIAN_POINT('Ctrl Pts',(31.6012947494448,-4.57514377911361,333.189873249273));
#28059=CARTESIAN_POINT('Ctrl Pts',(31.5934308348006,-4.62260422957602,333.320502099077));
#28060=CARTESIAN_POINT('Ctrl Pts',(31.5853562859414,-4.67133590374573,333.454629830351));
#28061=CARTESIAN_POINT('Ctrl Pts',(31.5772817370822,-4.71426893629634,333.591000198089));
#28062=CARTESIAN_POINT('Ctrl Pts',(31.5692071882229,-4.75120345817438,333.729075627139));
#28063=CARTESIAN_POINT('Ctrl Pts',(31.561357229452,-4.78711066228243,333.86331054778));
#28064=CARTESIAN_POINT('Ctrl Pts',(31.553507270681,-4.81734850360566,333.999156548042));
#28065=CARTESIAN_POINT('Ctrl Pts',(31.54565731191,-4.84178310468622,334.136102187944));
#28066=CARTESIAN_POINT('Ctrl Pts',(31.5374704680067,-4.86726632959515,334.27892492241));
#28067=CARTESIAN_POINT('Ctrl Pts',(31.5292836241034,-4.88643701749181,334.422943374421));
#28068=CARTESIAN_POINT('Ctrl Pts',(31.5210967802001,-4.89920217817375,334.567563785192));
#28069=CARTESIAN_POINT('Ctrl Pts',(31.5129099362968,-4.91196733885568,334.712184195962));
#28070=CARTESIAN_POINT('Ctrl Pts',(31.5047230923934,-4.91832691382983,334.857406103153));
#28071=CARTESIAN_POINT('Ctrl Pts',(31.4965362484901,-4.91824929754544,335.002628629631));
#28072=CARTESIAN_POINT('',(34.9965357556323,-4.92245962640078,334.9992848849));
#28073=CARTESIAN_POINT('Ctrl Pts',(34.9965353149058,-4.92622403178934,334.999292078765));
#28074=CARTESIAN_POINT('Ctrl Pts',(34.905993025116,-4.92295145947301,336.59090228179));
#28075=CARTESIAN_POINT('Ctrl Pts',(34.7227047239016,-3.21855768239145,339.818862479759));
#28076=CARTESIAN_POINT('Ctrl Pts',(34.4466704112626,2.283209725273,340.34896272345));
#28077=CARTESIAN_POINT('Ctrl Pts',(34.1684323769887,5.73363266215494,335.97463088495));
#28078=CARTESIAN_POINT('Ctrl Pts',(33.8901943427146,3.92238553325728,330.70589466886));
#28079=CARTESIAN_POINT('Ctrl Pts',(33.6119563084407,-1.48837690519751,329.377795534267));
#28080=CARTESIAN_POINT('Ctrl Pts',(33.3974042091434,-4.60743999916255,332.332160351074));
#28081=CARTESIAN_POINT('Ctrl Pts',(33.2755981212709,-4.91847296868088,334.481873404345));
#28082=CARTESIAN_POINT('Ctrl Pts',(33.2465380448228,-4.9144517986456,334.995877858909));
#28083=CARTESIAN_POINT('',(36.7465362484456,-4.9182479594994,335.004480109374));
#28084=CARTESIAN_POINT('Ctrl Pts',(36.7465362484457,-4.9182479594994,335.004480109374));
#28085=CARTESIAN_POINT('Ctrl Pts',(36.7368046369555,-4.91809128867769,335.17647277404));
#28086=CARTESIAN_POINT('Ctrl Pts',(36.7270730254652,-4.90890910186633,335.348063028799));
#28087=CARTESIAN_POINT('Ctrl Pts',(36.717341413975,-4.89084924610496,335.518436798824));
#28088=CARTESIAN_POINT('Ctrl Pts',(36.7074286083814,-4.87245313160836,335.69198277959));
#28089=CARTESIAN_POINT('Ctrl Pts',(36.6975158027879,-4.844845702818,335.864266712581));
#28090=CARTESIAN_POINT('Ctrl Pts',(36.6876029971943,-4.80823161056874,336.034452435653));
#28091=CARTESIAN_POINT('Ctrl Pts',(36.6825935599475,-4.78972867557836,336.120455806946));
#28092=CARTESIAN_POINT('Ctrl Pts',(36.6775841227008,-4.76892638705445,336.205923705473));
#28093=CARTESIAN_POINT('Ctrl Pts',(36.672574685454,-4.74585574177114,336.290750301491));
#28094=CARTESIAN_POINT('Ctrl Pts',(36.6647996066755,-4.71004810995311,336.422408496624));
#28095=CARTESIAN_POINT('Ctrl Pts',(36.6570245278971,-4.66870110703505,336.552783560165));
#28096=CARTESIAN_POINT('Ctrl Pts',(36.6492494491186,-4.62192219533737,336.681373927105));
#28097=CARTESIAN_POINT('Ctrl Pts',(36.6414839380696,-4.57520084806862,336.809806055412));
#28098=CARTESIAN_POINT('Ctrl Pts',(36.6337184270205,-4.52306102422823,336.936457493079));
#28099=CARTESIAN_POINT('Ctrl Pts',(36.6259529159715,-4.46566066806993,337.060839115543));
#28100=CARTESIAN_POINT('Ctrl Pts',(36.6181951044492,-4.40831722453184,337.185097413267));
#28101=CARTESIAN_POINT('Ctrl Pts',(36.610437292927,-4.34572379120724,337.307090021847));
#28102=CARTESIAN_POINT('Ctrl Pts',(36.6026794814048,-4.27808724600464,337.426345519103));
#28103=CARTESIAN_POINT('Ctrl Pts',(36.5949275078817,-4.21050159944728,337.545511272815));
#28104=CARTESIAN_POINT('Ctrl Pts',(36.5871755343587,-4.13788058703176,337.661943676432));
#28105=CARTESIAN_POINT('Ctrl Pts',(36.5794235608356,-4.06047791563382,337.775194075943));
#28106=CARTESIAN_POINT('Ctrl Pts',(36.571674870278,-3.98310802431316,337.888396513843));
#28107=CARTESIAN_POINT('Ctrl Pts',(36.5639261797204,-3.90096072176034,337.998419305849));
#28108=CARTESIAN_POINT('Ctrl Pts',(36.5561774891627,-3.81433398987333,338.104841264251));
#28109=CARTESIAN_POINT('Ctrl Pts',(36.5484304107849,-3.72772528140129,338.211241080676));
#28110=CARTESIAN_POINT('Ctrl Pts',(36.540683332407,-3.63663924397457,338.314041250724));
#28111=CARTESIAN_POINT('Ctrl Pts',(36.5329362540292,-3.54141499825141,338.412852600488));
#28112=CARTESIAN_POINT('Ctrl Pts',(36.5251891107233,-3.44618995445762,338.511664778387));
#28113=CARTESIAN_POINT('Ctrl Pts',(36.5174419674175,-3.34682690442515,338.606487787871));
#28114=CARTESIAN_POINT('Ctrl Pts',(36.5096948241117,-3.24370249547495,338.696968647872));
#28115=CARTESIAN_POINT('Ctrl Pts',(36.5019459390836,-3.14055490196794,338.787469849892));
#28116=CARTESIAN_POINT('Ctrl Pts',(36.4941970540554,-3.03364456058375,338.873626702144));
#28117=CARTESIAN_POINT('Ctrl Pts',(36.4864481690273,-2.92338160002829,338.955126177901));
#28118=CARTESIAN_POINT('Ctrl Pts',(36.4786910592525,-2.81300160522727,339.036712158044));
#28119=CARTESIAN_POINT('Ctrl Pts',(36.4709339494777,-2.69926219763536,339.113630654111));
#28120=CARTESIAN_POINT('Ctrl Pts',(36.463176839703,-2.58260338275419,339.185611404549));
#28121=CARTESIAN_POINT('Ctrl Pts',(36.4554155847768,-2.46588222913245,339.257630619198));
#28122=CARTESIAN_POINT('Ctrl Pts',(36.4476543298506,-2.34623890048053,339.324706639573));
#28123=CARTESIAN_POINT('Ctrl Pts',(36.4398930749244,-2.22413757680755,339.386615449516));
#28124=CARTESIAN_POINT('Ctrl Pts',(36.4321194045197,-2.10184093080958,339.448623293379));
#28125=CARTESIAN_POINT('Ctrl Pts',(36.424345734115,-1.97707878841167,339.50544724709));
#28126=CARTESIAN_POINT('Ctrl Pts',(36.4165720637103,-1.85033567554691,339.556911338867));
#28127=CARTESIAN_POINT('Ctrl Pts',(36.4091602595336,-1.7294924850843,339.605979764788));
#28128=CARTESIAN_POINT('Ctrl Pts',(36.4017484553568,-1.60684887281296,339.650176004598));
#28129=CARTESIAN_POINT('Ctrl Pts',(36.3943366511801,-1.48283539354448,339.68939039302));
#28130=CARTESIAN_POINT('Ctrl Pts',(36.3865615724017,-1.35274364423431,339.730526795435));
#28131=CARTESIAN_POINT('Ctrl Pts',(36.3787864936232,-1.22073323610408,339.766310646383));
#28132=CARTESIAN_POINT('Ctrl Pts',(36.3710114148448,-1.08728409989692,339.796560887616));
#28133=CARTESIAN_POINT('Ctrl Pts',(36.3632459037958,-0.953999181347643,
339.826773904003));
#28134=CARTESIAN_POINT('Ctrl Pts',(36.3554803927467,-0.819279434961304,
339.851466773961));
#28135=CARTESIAN_POINT('Ctrl Pts',(36.3477148816977,-0.683621648717045,
339.870507622816));
#28136=CARTESIAN_POINT('Ctrl Pts',(36.3399570701755,-0.548098367562711,
339.889529592614));
#28137=CARTESIAN_POINT('Ctrl Pts',(36.3321992586534,-0.411639282027383,
339.902910639596));
#28138=CARTESIAN_POINT('Ctrl Pts',(36.3244414471312,-0.274752774587812,
339.910569618217));
#28139=CARTESIAN_POINT('Ctrl Pts',(36.3166894736082,-0.137969278586197,
339.918222833214));
#28140=CARTESIAN_POINT('Ctrl Pts',(36.3089375000852,-0.000759389598527255,
339.920162529059));
#28141=CARTESIAN_POINT('Ctrl Pts',(36.3011855265622,0.136362314299225,339.916359260849));
#28142=CARTESIAN_POINT('Ctrl Pts',(36.2934368360046,0.273425947074154,339.912557603326));
#28143=CARTESIAN_POINT('Ctrl Pts',(36.2856881454469,0.41040107912774,339.903017829935));
#28144=CARTESIAN_POINT('Ctrl Pts',(36.2779394548893,0.546772269625293,339.887762591173));
#28145=CARTESIAN_POINT('Ctrl Pts',(36.2701923765115,0.683115086957668,339.872510526391));
#28146=CARTESIAN_POINT('Ctrl Pts',(36.2624452981337,0.818853824463417,339.851545404969));
#28147=CARTESIAN_POINT('Ctrl Pts',(36.2546982197558,0.953477699854415,339.824941796372));
#28148=CARTESIAN_POINT('Ctrl Pts',(36.24695107645,1.08810270352297,339.798337964812));
#28149=CARTESIAN_POINT('Ctrl Pts',(36.2392039331442,1.22161244298154,339.766095627597));
#28150=CARTESIAN_POINT('Ctrl Pts',(36.2314567898384,1.35350626344092,339.728340497186));
#28151=CARTESIAN_POINT('Ctrl Pts',(36.2237079048104,1.48542973643115,339.690576878619));
#28152=CARTESIAN_POINT('Ctrl Pts',(36.2159590197822,1.61573619180197,339.647298108151));
#28153=CARTESIAN_POINT('Ctrl Pts',(36.2082101347542,1.74394045452447,339.598679675034));
#28154=CARTESIAN_POINT('Ctrl Pts',(36.2004530249794,1.8722807945762,339.550009637811));
#28155=CARTESIAN_POINT('Ctrl Pts',(36.1926959152047,1.99851411871656,339.495988755248));
#28156=CARTESIAN_POINT('Ctrl Pts',(36.18493880543,2.12217504601478,339.436840783325));
#28157=CARTESIAN_POINT('Ctrl Pts',(36.1771775505038,2.24590205375872,339.377661204616));
#28158=CARTESIAN_POINT('Ctrl Pts',(36.1694162955776,2.3670535805621,339.313349260521));
#28159=CARTESIAN_POINT('Ctrl Pts',(36.1616550406515,2.4851900520218,339.244174061915));
#28160=CARTESIAN_POINT('Ctrl Pts',(36.1538813702468,2.60351550333524,339.174888205535));
#28161=CARTESIAN_POINT('Ctrl Pts',(36.1461076998422,2.71881593239847,339.100723760221));
#28162=CARTESIAN_POINT('Ctrl Pts',(36.1383340294375,2.83068115600148,339.021992945737));
#28163=CARTESIAN_POINT('Ctrl Pts',(36.1309222252604,2.93733902653271,338.946927069609));
#28164=CARTESIAN_POINT('Ctrl Pts',(36.1235104210833,3.04087408336792,338.867710560901));
#28165=CARTESIAN_POINT('Ctrl Pts',(36.1160986169062,3.14096110872323,338.784646136165));
#28166=CARTESIAN_POINT('Ctrl Pts',(36.1083235381278,3.2459536973347,338.697510476537));
#28167=CARTESIAN_POINT('Ctrl Pts',(36.1005484593493,3.3474835076065,338.605864803047));
#28168=CARTESIAN_POINT('Ctrl Pts',(36.0927733805709,3.445138565732,338.510014718688));
#28169=CARTESIAN_POINT('Ctrl Pts',(36.0850078695219,3.54267345309158,338.41428258396));
#28170=CARTESIAN_POINT('Ctrl Pts',(36.0772423584729,3.63634279922566,338.314356603915));
#28171=CARTESIAN_POINT('Ctrl Pts',(36.0694768474239,3.72576686742553,338.210583173209));
#28172=CARTESIAN_POINT('Ctrl Pts',(36.0617190359017,3.81510227140124,338.106912634163));
#28173=CARTESIAN_POINT('Ctrl Pts',(36.0539612243796,3.90020052048451,337.999402530236));
#28174=CARTESIAN_POINT('Ctrl Pts',(36.0462034128574,3.98071826272555,337.888436458589));
#28175=CARTESIAN_POINT('Ctrl Pts',(36.0384514393344,4.06117541281218,337.777553892429));
#28176=CARTESIAN_POINT('Ctrl Pts',(36.0306994658114,4.13705868846306,337.663220850256));
#28177=CARTESIAN_POINT('Ctrl Pts',(36.0229474922884,4.20806486110713,337.545854117426));
#28178=CARTESIAN_POINT('Ctrl Pts',(36.0151988017308,4.27904096259503,337.428537089476));
#28179=CARTESIAN_POINT('Ctrl Pts',(36.0074501111731,4.34514386721381,337.308189259922));
#28180=CARTESIAN_POINT('Ctrl Pts',(35.9997014206155,4.40611368763817,337.185256331442));
#28181=CARTESIAN_POINT('Ctrl Pts',(35.9919543422377,4.46707082278208,337.062348980184));
#28182=CARTESIAN_POINT('Ctrl Pts',(35.9842072638599,4.5228968244588,336.936857949777));
#28183=CARTESIAN_POINT('Ctrl Pts',(35.9764601854821,4.573377986117,336.809253121761));
#28184=CARTESIAN_POINT('Ctrl Pts',(35.9687130421763,4.62385957085595,336.681647224292));
#28185=CARTESIAN_POINT('Ctrl Pts',(35.9609658988705,4.66899608244052,336.551927857345));
#28186=CARTESIAN_POINT('Ctrl Pts',(35.9532187555647,4.70862230212363,336.420584062435));
#28187=CARTESIAN_POINT('Ctrl Pts',(35.9454698705367,4.74825743062217,336.289210738651));
#28188=CARTESIAN_POINT('Ctrl Pts',(35.9377209855086,4.78237968920694,336.156212634328));
#28189=CARTESIAN_POINT('Ctrl Pts',(35.9299721004805,4.8108740944889,336.022092710802));
#28190=CARTESIAN_POINT('Ctrl Pts',(35.9222149907058,4.83939874402706,335.887830431004));
#28191=CARTESIAN_POINT('Ctrl Pts',(35.9144578809311,4.86228352635401,335.752444336393));
#28192=CARTESIAN_POINT('Ctrl Pts',(35.9067007711564,4.87946475832095,335.61644686292));
#28193=CARTESIAN_POINT('Ctrl Pts',(35.8989395162302,4.89665517138892,335.480376716746));
#28194=CARTESIAN_POINT('Ctrl Pts',(35.891178261304,4.90813592839074,335.343694930034));
#28195=CARTESIAN_POINT('Ctrl Pts',(35.8834170063779,4.91389545147088,335.206916781615));
#28196=CARTESIAN_POINT('Ctrl Pts',(35.8756433359732,4.91966418791092,335.069919832734));
#28197=CARTESIAN_POINT('Ctrl Pts',(35.8678696655686,4.91969340172038,334.932826605193));
#28198=CARTESIAN_POINT('Ctrl Pts',(35.8600959951639,4.91402367148986,334.796150990836));
#28199=CARTESIAN_POINT('Ctrl Pts',(35.8526841909867,4.90861786856551,334.665837659206));
#28200=CARTESIAN_POINT('Ctrl Pts',(35.8452723868095,4.8980317764762,334.535904222782));
#28201=CARTESIAN_POINT('Ctrl Pts',(35.8378605826322,4.88234396202589,334.406787981436));
#28202=CARTESIAN_POINT('Ctrl Pts',(35.8300855038538,4.8658872410581,334.271343368485));
#28203=CARTESIAN_POINT('Ctrl Pts',(35.8223104250754,4.84376404516267,334.136370052431));
#28204=CARTESIAN_POINT('Ctrl Pts',(35.8145353462969,4.81600841975109,334.00237985015));
#28205=CARTESIAN_POINT('Ctrl Pts',(35.8067698352479,4.78828694940359,333.868554531344));
#28206=CARTESIAN_POINT('Ctrl Pts',(35.7990043241989,4.75494691889533,333.735710298277));
#28207=CARTESIAN_POINT('Ctrl Pts',(35.7912388131498,4.71607412156075,333.604353933676));
#28208=CARTESIAN_POINT('Ctrl Pts',(35.7834810016276,4.67723986671793,333.473127809293));
#28209=CARTESIAN_POINT('Ctrl Pts',(35.7757231901055,4.63288387221369,333.343386989984));
#28210=CARTESIAN_POINT('Ctrl Pts',(35.7679653785833,4.58314290564166,333.215627794162));
#28211=CARTESIAN_POINT('Ctrl Pts',(35.7602134050602,4.53343937072436,333.087964741187));
#28212=CARTESIAN_POINT('Ctrl Pts',(35.7524614315372,4.47835907100887,332.962280706245));
#28213=CARTESIAN_POINT('Ctrl Pts',(35.7447094580142,4.41808839581309,332.839056227182));
#28214=CARTESIAN_POINT('Ctrl Pts',(35.7369607674566,4.35784324528403,332.715883933759));
#28215=CARTESIAN_POINT('Ctrl Pts',(35.729212076899,4.2924122625766,332.595169474892));
#28216=CARTESIAN_POINT('Ctrl Pts',(35.7214633863413,4.22202960863737,332.477372590673));
#28217=CARTESIAN_POINT('Ctrl Pts',(35.7137163079635,4.15166159839713,332.359600215079));
#28218=CARTESIAN_POINT('Ctrl Pts',(35.7059692295857,4.07634416649656,332.244744542046));
#28219=CARTESIAN_POINT('Ctrl Pts',(35.6982221512078,3.99635679746895,332.133239561836));
#28220=CARTESIAN_POINT('Ctrl Pts',(35.690475007902,3.91636875807015,332.021733647106));
#28221=CARTESIAN_POINT('Ctrl Pts',(35.6827278645962,3.83171093131317,331.913578798818));
#28222=CARTESIAN_POINT('Ctrl Pts',(35.6749807212904,3.74270515329863,331.809178601367));
#28223=CARTESIAN_POINT('Ctrl Pts',(35.6672318362623,3.65367936489567,331.704754932536));
#28224=CARTESIAN_POINT('Ctrl Pts',(35.6594829512342,3.56030393363461,331.604087891646));
#28225=CARTESIAN_POINT('Ctrl Pts',(35.6517340662061,3.46293958632525,331.507546351924));
#28226=CARTESIAN_POINT('Ctrl Pts',(35.6439769564314,3.36547189549168,331.410902342014));
#28227=CARTESIAN_POINT('Ctrl Pts',(35.6362198466566,3.26400710904246,331.318392856083));
#28228=CARTESIAN_POINT('Ctrl Pts',(35.6284627368819,3.15894168269649,331.230348755147));
#28229=CARTESIAN_POINT('Ctrl Pts',(35.6207014819557,3.05382011274594,331.142257606259));
#28230=CARTESIAN_POINT('Ctrl Pts',(35.6129402270296,2.94509437870116,331.058636835176));
#28231=CARTESIAN_POINT('Ctrl Pts',(35.6051789721034,2.83319152408137,330.979775024906));
#28232=CARTESIAN_POINT('Ctrl Pts',(35.5974053016987,2.72110966136323,330.90078706144));
#28233=CARTESIAN_POINT('Ctrl Pts',(35.5896316312941,2.60584085083701,330.826573483094));
#28234=CARTESIAN_POINT('Ctrl Pts',(35.5818579608894,2.48783919452025,330.75737826283));
#28235=CARTESIAN_POINT('Ctrl Pts',(35.5744461567124,2.37533054369523,330.691404096716));
#28236=CARTESIAN_POINT('Ctrl Pts',(35.5670343525354,2.2603380031423,330.629991729373));
#28237=CARTESIAN_POINT('Ctrl Pts',(35.5596225483583,2.14327182465691,330.573311740349));
#28238=CARTESIAN_POINT('Ctrl Pts',(35.5518474695799,2.02046788404084,330.513853696222));
#28239=CARTESIAN_POINT('Ctrl Pts',(35.5440723908014,1.89499381231326,330.459415757544));
#28240=CARTESIAN_POINT('Ctrl Pts',(35.536297312023,1.76729843113215,330.410246268282));
#28241=CARTESIAN_POINT('Ctrl Pts',(35.528531800974,1.63976018724706,330.361137285208));
#28242=CARTESIAN_POINT('Ctrl Pts',(35.5207662899249,1.5100064339957,330.317283991028));
#28243=CARTESIAN_POINT('Ctrl Pts',(35.5130007788759,1.37850976347893,330.278888489509));
#28244=CARTESIAN_POINT('Ctrl Pts',(35.5052429673537,1.24714347229373,330.240531057241));
#28245=CARTESIAN_POINT('Ctrl Pts',(35.4974851558314,1.11403807566469,330.207620757459));
#28246=CARTESIAN_POINT('Ctrl Pts',(35.4897273443092,0.979684951126885,330.180311165746));
#28247=CARTESIAN_POINT('Ctrl Pts',(35.4819753707862,0.845432931576058,330.153022125367));
#28248=CARTESIAN_POINT('Ctrl Pts',(35.4742233972632,0.709935434559029,330.131325481429));
#28249=CARTESIAN_POINT('Ctrl Pts',(35.4664714237402,0.573697420556687,330.115324541779));
#28250=CARTESIAN_POINT('Ctrl Pts',(35.4587227331826,0.437517103434159,330.099330378537));
#28251=CARTESIAN_POINT('Ctrl Pts',(35.450974042625,0.300597280471339,330.089027167518));
#28252=CARTESIAN_POINT('Ctrl Pts',(35.4432253520673,0.163451274842229,330.084466789528));
#28253=CARTESIAN_POINT('Ctrl Pts',(35.4354782736895,0.0263338035848693,
330.079907360363));
#28254=CARTESIAN_POINT('Ctrl Pts',(35.4277311953116,-0.111009366321611,
330.08108840058));
#28255=CARTESIAN_POINT('Ctrl Pts',(35.4199841169338,-0.248062038090289,
330.088009742705));
#28256=CARTESIAN_POINT('Ctrl Pts',(35.412236973628,-0.385115858491988,330.094931142838));
#28257=CARTESIAN_POINT('Ctrl Pts',(35.4044898303222,-0.521878785522984,
330.107592921121));
#28258=CARTESIAN_POINT('Ctrl Pts',(35.3967426870164,-0.657837272474206,
330.125942841385));
#28259=CARTESIAN_POINT('Ctrl Pts',(35.3889938019883,-0.793826325779775,
330.144296887102));
#28260=CARTESIAN_POINT('Ctrl Pts',(35.3812449169602,-0.92901019183751,330.168341567228));
#28261=CARTESIAN_POINT('Ctrl Pts',(35.3734960319321,-1.0628834673078,330.197973157361));
#28262=CARTESIAN_POINT('Ctrl Pts',(35.3657389221574,-1.19689883725602,330.227636198771));
#28263=CARTESIAN_POINT('Ctrl Pts',(35.3579818123826,-1.32960045557487,330.262897911322));
#28264=CARTESIAN_POINT('Ctrl Pts',(35.3502247026078,-1.46049554923932,330.303603954823));
#28265=CARTESIAN_POINT('Ctrl Pts',(35.3424634476817,-1.59146058905669,330.344331750333));
#28266=CARTESIAN_POINT('Ctrl Pts',(35.3347021927555,-1.72061681280448,330.390509542261));
#28267=CARTESIAN_POINT('Ctrl Pts',(35.3269409378293,-1.84749044712313,330.441934389427));
#28268=CARTESIAN_POINT('Ctrl Pts',(35.3191672674246,-1.97456703790849,330.493441499589));
#28269=CARTESIAN_POINT('Ctrl Pts',(35.31139359702,-2.09935338671523,330.550212275896));
#28270=CARTESIAN_POINT('Ctrl Pts',(35.3036199266153,-2.22139859081782,330.611996882042));
#28271=CARTESIAN_POINT('Ctrl Pts',(35.2962081224383,-2.33776256130557,330.670905399906));
#28272=CARTESIAN_POINT('Ctrl Pts',(35.2887963182613,-2.45163459314333,330.734371324704));
#28273=CARTESIAN_POINT('Ctrl Pts',(35.2813845140843,-2.56264923156155,330.802141977332));
#28274=CARTESIAN_POINT('Ctrl Pts',(35.2736094353059,-2.67910502810576,330.873234271524));
#28275=CARTESIAN_POINT('Ctrl Pts',(35.2658343565274,-2.79278427203539,330.949288603045));
#28276=CARTESIAN_POINT('Ctrl Pts',(35.258059277749,-2.90323524245689,331.030061941358));
#28277=CARTESIAN_POINT('Ctrl Pts',(35.2502937666999,-3.01355029592763,331.110735882935));
#28278=CARTESIAN_POINT('Ctrl Pts',(35.2425282556509,-3.12064466772559,331.196117048437));
#28279=CARTESIAN_POINT('Ctrl Pts',(35.2347627446019,-3.22409265777899,331.285917395028));
#28280=CARTESIAN_POINT('Ctrl Pts',(35.2270049330797,-3.327438078849,331.375628704314));
#28281=CARTESIAN_POINT('Ctrl Pts',(35.2192471215575,-3.42714401974859,331.469750220413));
#28282=CARTESIAN_POINT('Ctrl Pts',(35.2114893100353,-3.52281542291247,331.567951842035));
#28283=CARTESIAN_POINT('Ctrl Pts',(35.2037373365123,-3.61841483031169,331.666079563823));
#28284=CARTESIAN_POINT('Ctrl Pts',(35.1959853629892,-3.70998547155759,331.768281000789));
#28285=CARTESIAN_POINT('Ctrl Pts',(35.1882333894662,-3.79716720978638,331.874187426696));
#28286=CARTESIAN_POINT('Ctrl Pts',(35.1804846989086,-3.88431202649716,331.980049001169));
#28287=CARTESIAN_POINT('Ctrl Pts',(35.1727360083509,-3.96707138911558,332.089612142674));
#28288=CARTESIAN_POINT('Ctrl Pts',(35.1649873177933,-4.04512388134036,332.202473262485));
#28289=CARTESIAN_POINT('Ctrl Pts',(35.1572402394155,-4.12316013409223,332.315310900597));
#28290=CARTESIAN_POINT('Ctrl Pts',(35.1494931610376,-4.19649124216299,332.431444830889));
#28291=CARTESIAN_POINT('Ctrl Pts',(35.1417460826597,-4.2648380026844,332.55044088184));
#28292=CARTESIAN_POINT('Ctrl Pts',(35.1339989393539,-4.33318533601741,332.669437930093));
#28293=CARTESIAN_POINT('Ctrl Pts',(35.1262517960481,-4.39654804380354,332.791296807904));
#28294=CARTESIAN_POINT('Ctrl Pts',(35.1185046527423,-4.45469214296026,332.915557394902));
#28295=CARTESIAN_POINT('Ctrl Pts',(35.1107557677142,-4.5128493141449,333.039845918318));
#28296=CARTESIAN_POINT('Ctrl Pts',(35.1030068826861,-4.56578537642855,333.166536871407));
#28297=CARTESIAN_POINT('Ctrl Pts',(35.095257997658,-4.61331405112678,333.295149118493));
#28298=CARTESIAN_POINT('Ctrl Pts',(35.0875008878833,-4.6608931732514,333.423897875946));
#28299=CARTESIAN_POINT('Ctrl Pts',(35.0797437781085,-4.70305330698094,333.554571633834));
#28300=CARTESIAN_POINT('Ctrl Pts',(35.0719866683338,-4.73965757251598,333.686672486471));
#28301=CARTESIAN_POINT('Ctrl Pts',(35.0642254134076,-4.77628139820017,333.818843929581));
#28302=CARTESIAN_POINT('Ctrl Pts',(35.0564641584814,-4.80734335145991,333.952443606451));
#28303=CARTESIAN_POINT('Ctrl Pts',(35.0487029035552,-4.8327577039145,334.086963287838));
#28304=CARTESIAN_POINT('Ctrl Pts',(35.0409292331506,-4.8582127110505,334.221698156876));
#28305=CARTESIAN_POINT('Ctrl Pts',(35.0331555627459,-4.87800200768101,334.357355584354));
#28306=CARTESIAN_POINT('Ctrl Pts',(35.0253818923412,-4.89209167714841,334.49342119579));
#28307=CARTESIAN_POINT('Ctrl Pts',(35.0179700881642,-4.90552546911202,334.623152920274));
#28308=CARTESIAN_POINT('Ctrl Pts',(35.0105582839873,-4.91377830936601,334.753255394781));
#28309=CARTESIAN_POINT('Ctrl Pts',(35.0031464798104,-4.91686491261461,334.883284561436));
#28310=CARTESIAN_POINT('Ctrl Pts',(35.0009430693703,-4.91778251022781,334.921940146024));
#28311=CARTESIAN_POINT('Ctrl Pts',(34.9987396589303,-4.91824426091572,334.960606594331));
#28312=CARTESIAN_POINT('Ctrl Pts',(34.9965362484902,-4.91824994683472,334.999276840106));
#28313=CARTESIAN_POINT('',(38.4965362485229,-4.91824977738391,334.998520215163));
#28314=CARTESIAN_POINT('Ctrl Pts',(38.4965362484901,-4.91824977738408,334.998520215746));
#28315=CARTESIAN_POINT('Ctrl Pts',(38.4885838555402,-4.91829224990027,335.139682985052));
#28316=CARTESIAN_POINT('Ctrl Pts',(38.4806314625904,-4.91225292694631,335.280790264135));
#28317=CARTESIAN_POINT('Ctrl Pts',(38.4726790696405,-4.90017238107107,335.421300009837));
#28318=CARTESIAN_POINT('Ctrl Pts',(38.4647215384514,-4.88808402965417,335.561900542385));
#28319=CARTESIAN_POINT('Ctrl Pts',(38.4567640072624,-4.86994670554018,335.701902412536));
#28320=CARTESIAN_POINT('Ctrl Pts',(38.4488064760733,-4.84585267460449,335.840770431526));
#28321=CARTESIAN_POINT('Ctrl Pts',(38.4408425052537,-4.82173914557912,335.979750829433));
#28322=CARTESIAN_POINT('Ctrl Pts',(38.4328785344342,-4.79165936241612,336.117595192121));
#28323=CARTESIAN_POINT('Ctrl Pts',(38.4249145636146,-4.75575631911382,336.253780242191));
#28324=CARTESIAN_POINT('Ctrl Pts',(38.4169371080535,-4.71979248411985,336.390195883287));
#28325=CARTESIAN_POINT('Ctrl Pts',(38.4089596524924,-4.67798578106659,336.524946249112));
#28326=CARTESIAN_POINT('Ctrl Pts',(38.4009821969313,-4.63052889546794,336.657523819056));
#28327=CARTESIAN_POINT('Ctrl Pts',(38.3929971971094,-4.58302713000514,336.790226767292));
#28328=CARTESIAN_POINT('Ctrl Pts',(38.3850121972875,-4.52986466195102,336.920752488628));
#28329=CARTESIAN_POINT('Ctrl Pts',(38.3770271974656,-4.47128147023148,337.048615404722));
#28330=CARTESIAN_POINT('Ctrl Pts',(38.3690276478814,-4.4125915319209,337.176711304544));
#28331=CARTESIAN_POINT('Ctrl Pts',(38.3610280982973,-4.34846129757621,337.302134383415));
#28332=CARTESIAN_POINT('Ctrl Pts',(38.3530285487132,-4.27917616809477,337.424424547168));
#28333=CARTESIAN_POINT('Ctrl Pts',(38.349353329508,-4.24734462110284,337.480608105217));
#28334=CARTESIAN_POINT('Ctrl Pts',(38.3456781103028,-4.21442560091628,337.536130803463));
#28335=CARTESIAN_POINT('Ctrl Pts',(38.3420028910976,-4.18044970707607,337.590950271446));
#28336=CARTESIAN_POINT('Ctrl Pts',(38.3342278123192,-4.10857229339569,337.706923131395));
#28337=CARTESIAN_POINT('Ctrl Pts',(38.3264527335408,-4.03175171321087,337.820085979996));
#28338=CARTESIAN_POINT('Ctrl Pts',(38.3186776547624,-3.95023404320812,337.929988748507));
#28339=CARTESIAN_POINT('Ctrl Pts',(38.3109121437134,-3.86881668588808,338.039756274665));
#28340=CARTESIAN_POINT('Ctrl Pts',(38.3031466326644,-3.78271397006088,338.146271391997));
#28341=CARTESIAN_POINT('Ctrl Pts',(38.2953811216154,-3.69221680789574,338.249110356081));
#28342=CARTESIAN_POINT('Ctrl Pts',(38.2876233100932,-3.60180937393031,338.351847355032));
#28343=CARTESIAN_POINT('Ctrl Pts',(38.279865498571,-3.50701642107217,338.45091516278));
#28344=CARTESIAN_POINT('Ctrl Pts',(38.2721076870488,-3.40817071197461,338.545920960842));
#28345=CARTESIAN_POINT('Ctrl Pts',(38.2643557135258,-3.30939938740772,338.640855264028));
#28346=CARTESIAN_POINT('Ctrl Pts',(38.2566037400028,-3.20658165780887,338.731733372152));
#28347=CARTESIAN_POINT('Ctrl Pts',(38.2488517664798,-3.10008867398177,338.818197647575));
#28348=CARTESIAN_POINT('Ctrl Pts',(38.2411030759222,-2.99364078999656,338.904625305327));
#28349=CARTESIAN_POINT('Ctrl Pts',(38.2333543853646,-2.88352105031383,338.986642602341));
#28350=CARTESIAN_POINT('Ctrl Pts',(38.225605694807,-2.7701352058464,339.063930856182));
#28351=CARTESIAN_POINT('Ctrl Pts',(38.2178586164292,-2.65677295225092,339.141203029556));
#28352=CARTESIAN_POINT('Ctrl Pts',(38.2101115380514,-2.54014626829974,339.21374789682));
#28353=CARTESIAN_POINT('Ctrl Pts',(38.2023644596735,-2.42069120181971,339.281289194616));
#28354=CARTESIAN_POINT('Ctrl Pts',(38.1946173163677,-2.30123513419133,339.348831058472));
#28355=CARTESIAN_POINT('Ctrl Pts',(38.1868701730619,-2.17895097700587,339.411369076835));
#28356=CARTESIAN_POINT('Ctrl Pts',(38.1791230297561,-2.0543004208578,339.468672380402));
#28357=CARTESIAN_POINT('Ctrl Pts',(38.1713741447281,-1.9296218406183,339.525988566968));
#28358=CARTESIAN_POINT('Ctrl Pts',(38.1636252597,-1.80257615783736,339.578067533656));
#28359=CARTESIAN_POINT('Ctrl Pts',(38.1558763746719,-1.67364575565692,339.624726256447));
#28360=CARTESIAN_POINT('Ctrl Pts',(38.1481192648972,-1.54457850541533,339.671434503289));
#28361=CARTESIAN_POINT('Ctrl Pts',(38.1403621551225,-1.41362290779365,339.712710880649));
#28362=CARTESIAN_POINT('Ctrl Pts',(38.1326050453478,-1.28127778183339,339.748421875558));
#28363=CARTESIAN_POINT('Ctrl Pts',(38.1248437904216,-1.14886193486967,339.784151953282));
#28364=CARTESIAN_POINT('Ctrl Pts',(38.1170825354954,-1.0150554611458,339.814310636767));
#28365=CARTESIAN_POINT('Ctrl Pts',(38.1093212805692,-0.880367157463933,
339.838815633041));
#28366=CARTESIAN_POINT('Ctrl Pts',(38.1015476101646,-0.745463396390805,
339.863359829322));
#28367=CARTESIAN_POINT('Ctrl Pts',(38.09377393976,-0.609675373838679,339.882232211851));
#28368=CARTESIAN_POINT('Ctrl Pts',(38.0860002693553,-0.473517681683084,
339.89540233971));
#28369=CARTESIAN_POINT('Ctrl Pts',(38.0785884651781,-0.343698162852952,
339.907959394948));
#28370=CARTESIAN_POINT('Ctrl Pts',(38.0711766610009,-0.213542903478925,
339.915333112026));
#28371=CARTESIAN_POINT('Ctrl Pts',(38.0637648568238,-0.083495851893928,
339.917541205238));
#28372=CARTESIAN_POINT('Ctrl Pts',(38.0559897780453,0.0529251930775802,
339.919857523677));
#28373=CARTESIAN_POINT('Ctrl Pts',(38.0482146992669,0.189658270591596,339.916496369565));
#28374=CARTESIAN_POINT('Ctrl Pts',(38.0404396204885,0.326191742027135,339.907421116017));
#28375=CARTESIAN_POINT('Ctrl Pts',(38.0326741094394,0.462557200333927,339.898357030147));
#28376=CARTESIAN_POINT('Ctrl Pts',(38.0249085983904,0.598723155006201,339.883592861312));
#28377=CARTESIAN_POINT('Ctrl Pts',(38.0171430873414,0.734175841051302,339.863143931339));
#28378=CARTESIAN_POINT('Ctrl Pts',(38.0093852758192,0.86949422536337,339.84271527654));
#28379=CARTESIAN_POINT('Ctrl Pts',(38.001627464297,1.00410036442694,339.816613135444));
#28380=CARTESIAN_POINT('Ctrl Pts',(37.9938696527748,1.13748385183549,339.784904758646));
#28381=CARTESIAN_POINT('Ctrl Pts',(37.9861176792518,1.27076696394048,339.753220243407));
#28382=CARTESIAN_POINT('Ctrl Pts',(37.9783657057288,1.40282887702735,339.715937979958));
#28383=CARTESIAN_POINT('Ctrl Pts',(37.9706137322058,1.53316799498063,339.67317653868));
#28384=CARTESIAN_POINT('Ctrl Pts',(37.9628650416482,1.6634519142399,339.630433206898));
#28385=CARTESIAN_POINT('Ctrl Pts',(37.9551163510905,1.79201411887373,339.582215434063));
#28386=CARTESIAN_POINT('Ctrl Pts',(37.9473676605329,1.91836704692088,339.528691967421));
#28387=CARTESIAN_POINT('Ctrl Pts',(37.9396205821551,2.04469368618603,339.475179636784));
#28388=CARTESIAN_POINT('Ctrl Pts',(37.9318735037772,2.16881160346916,339.416363960429));
#28389=CARTESIAN_POINT('Ctrl Pts',(37.9241264253994,2.29025251251831,339.352462118319));
#28390=CARTESIAN_POINT('Ctrl Pts',(37.9163792820936,2.41169443935891,339.288559740651));
#28391=CARTESIAN_POINT('Ctrl Pts',(37.9086321387878,2.53045896730672,339.219571294222));
#28392=CARTESIAN_POINT('Ctrl Pts',(37.900884995482,2.64610210616758,339.145760087877));
#28393=CARTESIAN_POINT('Ctrl Pts',(37.8931361104539,2.76177124406138,339.071932287206));
#28394=CARTESIAN_POINT('Ctrl Pts',(37.8853872254259,2.87431726703825,338.99327977932));
#28395=CARTESIAN_POINT('Ctrl Pts',(37.8776383403978,2.98332522109835,338.910109165696));
#28396=CARTESIAN_POINT('Ctrl Pts',(37.869881230623,3.09244887732715,338.826850273923));
#28397=CARTESIAN_POINT('Ctrl Pts',(37.8621241208483,3.19802665174555,338.739063934295));
#28398=CARTESIAN_POINT('Ctrl Pts',(37.8543670110736,3.29967633084447,338.647097362858));
#28399=CARTESIAN_POINT('Ctrl Pts',(37.8466057561474,3.4013803282817,338.555081647425));
#28400=CARTESIAN_POINT('Ctrl Pts',(37.8388445012213,3.4991517693778,338.458881523174));
#28401=CARTESIAN_POINT('Ctrl Pts',(37.8310832462951,3.59264611307092,338.358880314738));
#28402=CARTESIAN_POINT('Ctrl Pts',(37.8233095758905,3.68629001724434,338.25871913696));
#28403=CARTESIAN_POINT('Ctrl Pts',(37.8155359054858,3.77564289685556,338.154745020968));
#28404=CARTESIAN_POINT('Ctrl Pts',(37.8077622350811,3.86040067829626,338.047374224724));
#28405=CARTESIAN_POINT('Ctrl Pts',(37.800350430904,3.94121296461935,337.945001564876));
#28406=CARTESIAN_POINT('Ctrl Pts',(37.7929386267269,4.01784815977472,337.839541571944));
#28407=CARTESIAN_POINT('Ctrl Pts',(37.7855268225499,4.09008091417473,337.731377157773));
#28408=CARTESIAN_POINT('Ctrl Pts',(37.7777517437714,4.16585401103821,337.617911283458));
#28409=CARTESIAN_POINT('Ctrl Pts',(37.769976664993,4.2370216588236,337.501110608152));
#28410=CARTESIAN_POINT('Ctrl Pts',(37.7622015862146,4.30327618018612,337.381385558775));
#28411=CARTESIAN_POINT('Ctrl Pts',(37.7544360751655,4.36944917114231,337.261807838694));
#28412=CARTESIAN_POINT('Ctrl Pts',(37.7466705641164,4.43072087786297,337.139313243511));
#28413=CARTESIAN_POINT('Ctrl Pts',(37.7389050530674,4.48682615708263,337.014342100692));
#28414=CARTESIAN_POINT('Ctrl Pts',(37.7311472415452,4.54287580775426,336.889494867125));
#28415=CARTESIAN_POINT('Ctrl Pts',(37.7233894300231,4.59376906598802,336.762176326803));
#28416=CARTESIAN_POINT('Ctrl Pts',(37.7156316185009,4.63928627404983,336.632852084517));
#28417=CARTESIAN_POINT('Ctrl Pts',(37.7078796449779,4.68476922896933,336.503625162825));
#28418=CARTESIAN_POINT('Ctrl Pts',(37.7001276714549,4.72488405713468,336.372395910684));
#28419=CARTESIAN_POINT('Ctrl Pts',(37.6923756979318,4.75945902447026,336.239650296208));
#28420=CARTESIAN_POINT('Ctrl Pts',(37.6846270073742,4.79401934928656,336.106960899578));
#28421=CARTESIAN_POINT('Ctrl Pts',(37.6768783168166,4.82304438125378,335.972756795332));
#28422=CARTESIAN_POINT('Ctrl Pts',(37.669129626259,4.84641217577767,335.83753930354));
#28423=CARTESIAN_POINT('Ctrl Pts',(37.6613825478812,4.86977510843673,335.702349944877));
#28424=CARTESIAN_POINT('Ctrl Pts',(37.6536354695033,4.88748307833829,335.566148002975));
#28425=CARTESIAN_POINT('Ctrl Pts',(37.6458883911255,4.89946530018679,335.429444798275));
#28426=CARTESIAN_POINT('Ctrl Pts',(37.6381412478197,4.91144762245785,335.292740447871));
#28427=CARTESIAN_POINT('Ctrl Pts',(37.6303941045139,4.9177040668318,335.155535215671));
#28428=CARTESIAN_POINT('Ctrl Pts',(37.6226469612081,4.9182157867627,335.018344954025));
#28429=CARTESIAN_POINT('Ctrl Pts',(37.61489807618,4.9187276217391,334.881123849096));
#28430=CARTESIAN_POINT('Ctrl Pts',(37.6071491911519,4.91349216080239,334.743918112213));
#28431=CARTESIAN_POINT('Ctrl Pts',(37.5994003061238,4.90254267625575,334.607242606701));
#28432=CARTESIAN_POINT('Ctrl Pts',(37.591643196349,4.89158156981306,334.470422032394));
#28433=CARTESIAN_POINT('Ctrl Pts',(37.5838860865743,4.87489435576975,334.334133203931));
#28434=CARTESIAN_POINT('Ctrl Pts',(37.5761289767996,4.85256617784498,334.19888543133));
#28435=CARTESIAN_POINT('Ctrl Pts',(37.5683677218734,4.83022606845586,334.063565386644));
#28436=CARTESIAN_POINT('Ctrl Pts',(37.5606064669472,4.80223906853414,333.92928788877));
#28437=CARTESIAN_POINT('Ctrl Pts',(37.5528452120211,4.76874107300531,333.796550108591));
#28438=CARTESIAN_POINT('Ctrl Pts',(37.5450715416164,4.73518949160061,333.663599991223));
#28439=CARTESIAN_POINT('Ctrl Pts',(37.5372978712118,4.69610940949782,333.532194888302));
#28440=CARTESIAN_POINT('Ctrl Pts',(37.5295242008071,4.65168631521807,333.402815762877));
#28441=CARTESIAN_POINT('Ctrl Pts',(37.52211239663,4.60933112666469,333.279459266868));
#28442=CARTESIAN_POINT('Ctrl Pts',(37.5147005924529,4.56211927014286,333.157944642853));
#28443=CARTESIAN_POINT('Ctrl Pts',(37.5072887882759,4.51025079480062,333.03866860768));
#28444=CARTESIAN_POINT('Ctrl Pts',(37.4995137094974,4.45584009097361,332.913546498717));
#28445=CARTESIAN_POINT('Ctrl Pts',(37.491738630719,4.39613280909055,332.79049255797));
#28446=CARTESIAN_POINT('Ctrl Pts',(37.4839635519405,4.33130758404089,332.669987623438));
#28447=CARTESIAN_POINT('Ctrl Pts',(37.4761980408915,4.26656213055763,332.549630977901));
#28448=CARTESIAN_POINT('Ctrl Pts',(37.4684325298425,4.19671144843798,332.431817438354));
#28449=CARTESIAN_POINT('Ctrl Pts',(37.4606670187935,4.12198233420488,332.317008255882));
#28450=CARTESIAN_POINT('Ctrl Pts',(37.4529092072713,4.04732731410615,332.20231290705));
#28451=CARTESIAN_POINT('Ctrl Pts',(37.4451513957492,3.96780369961219,332.090616312736));
#28452=CARTESIAN_POINT('Ctrl Pts',(37.437393584227,3.88368415832176,331.982355153286));
#28453=CARTESIAN_POINT('Ctrl Pts',(37.429641610704,3.79962791965396,331.874175463791));
#28454=CARTESIAN_POINT('Ctrl Pts',(37.421889637181,3.7109828771849,331.769426370709));
#28455=CARTESIAN_POINT('Ctrl Pts',(37.414137663658,3.61806475670521,331.668515274118));
#28456=CARTESIAN_POINT('Ctrl Pts',(37.4063889731004,3.52518598710445,331.567646913435));
#28457=CARTESIAN_POINT('Ctrl Pts',(37.3986402825428,3.42803800297779,331.470613603394));
#28458=CARTESIAN_POINT('Ctrl Pts',(37.3908915919852,3.32697638385219,331.377789182862));
#28459=CARTESIAN_POINT('Ctrl Pts',(37.3831445136074,3.2259357914404,331.284984075226));
#28460=CARTESIAN_POINT('Ctrl Pts',(37.3753974352296,3.12098347135104,331.196386379524));
#28461=CARTESIAN_POINT('Ctrl Pts',(37.3676503568517,3.01251109786592,331.112332325451));
#28462=CARTESIAN_POINT('Ctrl Pts',(37.359903213546,2.90403781527843,331.028277566924));
#28463=CARTESIAN_POINT('Ctrl Pts',(37.3521560702402,2.79204472942191,330.948766765397));
#28464=CARTESIAN_POINT('Ctrl Pts',(37.3444089269344,2.67695543259566,330.874094926638));
#28465=CARTESIAN_POINT('Ctrl Pts',(37.3366600419063,2.56184026125144,330.799406300064));
#28466=CARTESIAN_POINT('Ctrl Pts',(37.3289111568782,2.44362782162743,330.729559013768));
#28467=CARTESIAN_POINT('Ctrl Pts',(37.3211622718501,2.32276907882828,330.664803710449));
#28468=CARTESIAN_POINT('Ctrl Pts',(37.3134051620754,2.20178205531099,330.599979675181));
#28469=CARTESIAN_POINT('Ctrl Pts',(37.3056480523006,2.07814346283076,330.540258604143));
#28470=CARTESIAN_POINT('Ctrl Pts',(37.2978909425259,1.95232766720063,330.485844515041));
#28471=CARTESIAN_POINT('Ctrl Pts',(37.2901296875998,1.82644463963205,330.43140134879));
#28472=CARTESIAN_POINT('Ctrl Pts',(37.2823684326736,1.6983824554332,330.382270955159));
#28473=CARTESIAN_POINT('Ctrl Pts',(37.2746071777474,1.56863273674961,330.338608104901));
#28474=CARTESIAN_POINT('Ctrl Pts',(37.2668335073428,1.43867546080163,330.294875408312));
#28475=CARTESIAN_POINT('Ctrl Pts',(37.2590598369382,1.3070256315098,330.256627841875));
#28476=CARTESIAN_POINT('Ctrl Pts',(37.2512861665335,1.17418807944664,330.22396970104));
#28477=CARTESIAN_POINT('Ctrl Pts',(37.2438743623564,1.04753414738945,330.192831804517));
#28478=CARTESIAN_POINT('Ctrl Pts',(37.2364625581792,0.919800863073379,330.166774726325));
#28479=CARTESIAN_POINT('Ctrl Pts',(37.229050754002,0.791430092231746,330.145844927116));
#28480=CARTESIAN_POINT('Ctrl Pts',(37.2212756752235,0.656767487515261,330.1238892961));
#28481=CARTESIAN_POINT('Ctrl Pts',(37.2135005964451,0.520977767269429,330.107506875063));
#28482=CARTESIAN_POINT('Ctrl Pts',(37.2057255176667,0.384561948016524,330.096807655146));
#28483=CARTESIAN_POINT('Ctrl Pts',(37.1979600066176,0.248313997113864,330.0861216013));
#28484=CARTESIAN_POINT('Ctrl Pts',(37.1901944955686,0.111441866140478,330.081104863705));
#28485=CARTESIAN_POINT('Ctrl Pts',(37.1824289845195,-0.0255438364138864,
330.081816333755));
#28486=CARTESIAN_POINT('Ctrl Pts',(37.1746711729973,-0.162393717245253,
330.08252709838));
#28487=CARTESIAN_POINT('Ctrl Pts',(37.1669133614751,-0.299356557213057,
330.088954766037));
#28488=CARTESIAN_POINT('Ctrl Pts',(37.1591555499529,-0.43591758641646,330.101106357518));
#28489=CARTESIAN_POINT('Ctrl Pts',(37.1514035764298,-0.572375849115903,
330.11324880454));
#28490=CARTESIAN_POINT('Ctrl Pts',(37.1436516029067,-0.708432515145981,
330.131106567143));
#28491=CARTESIAN_POINT('Ctrl Pts',(37.1358996293836,-0.843574135747758,
330.154634612333));
#28492=CARTESIAN_POINT('Ctrl Pts',(37.128150938826,-0.978658523791689,330.178152693382));
#28493=CARTESIAN_POINT('Ctrl Pts',(37.1204022482683,-1.11282825288142,330.207336213962));
#28494=CARTESIAN_POINT('Ctrl Pts',(37.1126535577107,-1.24557652945232,330.242088465327));
#28495=CARTESIAN_POINT('Ctrl Pts',(37.1049064793328,-1.37829718663572,330.276833486195));
#28496=CARTESIAN_POINT('Ctrl Pts',(37.097159400955,-1.50959660166403,330.317144834339));
#28497=CARTESIAN_POINT('Ctrl Pts',(37.0894123225771,-1.63898007438538,330.36287509568));
#28498=CARTESIAN_POINT('Ctrl Pts',(37.0816651792713,-1.76836463146502,330.408605740284));
#28499=CARTESIAN_POINT('Ctrl Pts',(37.0739180359655,-1.89583284567782,330.459755258414));
#28500=CARTESIAN_POINT('Ctrl Pts',(37.0661708926596,-2.02090741028011,330.516127086817));
#28501=CARTESIAN_POINT('Ctrl Pts',(37.0584220076315,-2.14601009429959,330.572511588804));
#28502=CARTESIAN_POINT('Ctrl Pts',(37.0506731226034,-2.26871770158075,330.634120576785));
#28503=CARTESIAN_POINT('Ctrl Pts',(37.0429242375753,-2.38857541823775,330.700710461729));
#28504=CARTESIAN_POINT('Ctrl Pts',(37.0351671278005,-2.5085603531134,330.767371025864));
#28505=CARTESIAN_POINT('Ctrl Pts',(37.0274100180258,-2.62568901261414,330.839022857662));
#28506=CARTESIAN_POINT('Ctrl Pts',(37.0196529082511,-2.73953312733801,330.915377458477));
#28507=CARTESIAN_POINT('Ctrl Pts',(37.0118916533249,-2.85343807671698,330.99177286075));
#28508=CARTESIAN_POINT('Ctrl Pts',(37.0041303983987,-2.96405466894857,331.072875808435));
#28509=CARTESIAN_POINT('Ctrl Pts',(36.9963691434725,-3.07098670905383,331.158356641317));
#28510=CARTESIAN_POINT('Ctrl Pts',(36.9885954730679,-3.17808980557404,331.243974215673));
#28511=CARTESIAN_POINT('Ctrl Pts',(36.9808218026632,-3.28149627686227,331.333983412907));
#28512=CARTESIAN_POINT('Ctrl Pts',(36.9730481322585,-3.3808452258597,331.428016150473));
#28513=CARTESIAN_POINT('Ctrl Pts',(36.9656363280817,-3.4755694573765,331.51767164148));
#28514=CARTESIAN_POINT('Ctrl Pts',(36.9582245239048,-3.56660521980601,331.610984305163));
#28515=CARTESIAN_POINT('Ctrl Pts',(36.9508127197279,-3.65367432449124,331.707607709726));
#28516=CARTESIAN_POINT('Ctrl Pts',(36.9431146196332,-3.74410664933728,331.807963388596));
#28517=CARTESIAN_POINT('Ctrl Pts',(36.9354165195386,-3.83055911254457,331.912223196463));
#28518=CARTESIAN_POINT('Ctrl Pts',(36.9277184194439,-3.91267054438507,332.020034853626));
#28519=CARTESIAN_POINT('Ctrl Pts',(36.9200324550669,-3.99465253115025,332.127676550435));
#28520=CARTESIAN_POINT('Ctrl Pts',(36.9123464906898,-4.07230687213663,332.238858633726));
#28521=CARTESIAN_POINT('Ctrl Pts',(36.9046605263127,-4.14531014326032,332.353193078692));
#28522=CARTESIAN_POINT('Ctrl Pts',(36.8969815399504,-4.21824713540066,332.467423720491));
#28523=CARTESIAN_POINT('Ctrl Pts',(36.8893025535881,-4.28654124039229,332.584800699224));
#28524=CARTESIAN_POINT('Ctrl Pts',(36.8816235672258,-4.34991004158561,332.704903990546));
#28525=CARTESIAN_POINT('Ctrl Pts',(36.8739498084355,-4.41323570362541,332.824925519956));
#28526=CARTESIAN_POINT('Ctrl Pts',(36.8662760496453,-4.47164254473121,332.947669319001));
#28527=CARTESIAN_POINT('Ctrl Pts',(36.858602290855,-4.52489241493673,333.072687960981));
#28528=CARTESIAN_POINT('Ctrl Pts',(36.8509320135999,-4.57811812601729,333.197649882804));
#28529=CARTESIAN_POINT('Ctrl Pts',(36.8432617363449,-4.62619136494713,333.324884227468));
#28530=CARTESIAN_POINT('Ctrl Pts',(36.8355914590898,-4.66892097751543,333.453921098968));
#28531=CARTESIAN_POINT('Ctrl Pts',(36.8279210331352,-4.71165141845951,333.582960472036));
#28532=CARTESIAN_POINT('Ctrl Pts',(36.8202506071806,-4.74903788801809,333.713802066858));
#28533=CARTESIAN_POINT('Ctrl Pts',(36.812580181226,-4.7809382931974,333.845958363343));
#28534=CARTESIAN_POINT('Ctrl Pts',(36.8049099796634,-4.8128377651567,333.978110793704));
#28535=CARTESIAN_POINT('Ctrl Pts',(36.7972397781009,-4.83925140398853,334.11157745941));
#28536=CARTESIAN_POINT('Ctrl Pts',(36.7895695765383,-4.8600879060864,334.245859026698));
#28537=CARTESIAN_POINT('Ctrl Pts',(36.7818942818184,-4.88093824401132,334.380229759458));
#28538=CARTESIAN_POINT('Ctrl Pts',(36.7742189870985,-4.89620398947651,334.51541607898));
#28539=CARTESIAN_POINT('Ctrl Pts',(36.7665436923787,-4.90584553525493,334.65091169209));
#28540=CARTESIAN_POINT('Ctrl Pts',(36.7598745444158,-4.91422318037912,334.768645319935));
#28541=CARTESIAN_POINT('Ctrl Pts',(36.753205396453,-4.9183553271965,334.886612216886));
#28542=CARTESIAN_POINT('Ctrl Pts',(36.7465362484902,-4.91824795950011,335.004480108586));
#28543=CARTESIAN_POINT('',(40.2465362484602,-4.9182484758457,334.996128005489));
#28544=CARTESIAN_POINT('Ctrl Pts',(40.2465362484602,-4.91824847584569,334.996128005489));
#28545=CARTESIAN_POINT('Ctrl Pts',(40.2388859593559,-4.91835450293067,335.130804732851));
#28546=CARTESIAN_POINT('Ctrl Pts',(40.2312356702516,-4.91292458102749,335.265686434657));
#28547=CARTESIAN_POINT('Ctrl Pts',(40.2235853811473,-4.9019348286901,335.400272404463));
#28548=CARTESIAN_POINT('Ctrl Pts',(40.2159425957197,-4.89095585549429,335.534726367544));
#28549=CARTESIAN_POINT('Ctrl Pts',(40.2082998102923,-4.8744279304713,335.668884776161));
#28550=CARTESIAN_POINT('Ctrl Pts',(40.2006570248647,-4.85237921080569,335.802246257106));
#28551=CARTESIAN_POINT('Ctrl Pts',(40.1927726111929,-4.82963341630109,335.939823988893));
#28552=CARTESIAN_POINT('Ctrl Pts',(40.1848881975211,-4.80101195311241,336.076553133484));
#28553=CARTESIAN_POINT('Ctrl Pts',(40.1770037838493,-4.76660375329278,336.21188766872));
#28554=CARTESIAN_POINT('Ctrl Pts',(40.1693694278661,-4.73328682484401,336.342930008939));
#28555=CARTESIAN_POINT('Ctrl Pts',(40.1617350718829,-4.69454475515893,336.472664437365));
#28556=CARTESIAN_POINT('Ctrl Pts',(40.1541007158997,-4.65051021783986,336.600605440534));
#28557=CARTESIAN_POINT('Ctrl Pts',(40.146467469993,-4.60648208338,336.728527840391));
#28558=CARTESIAN_POINT('Ctrl Pts',(40.1388342240864,-4.55716314256936,336.854656952013));
#28559=CARTESIAN_POINT('Ctrl Pts',(40.1312009781797,-4.50273562993134,336.978523416451));
#28560=CARTESIAN_POINT('Ctrl Pts',(40.1235670762017,-4.44830343929241,337.102400527112));
#28561=CARTESIAN_POINT('Ctrl Pts',(40.1159331742237,-4.38876196647831,337.224014234624));
#28562=CARTESIAN_POINT('Ctrl Pts',(40.1082992722457,-4.32434094842294,337.342916649028));
#28563=CARTESIAN_POINT('Ctrl Pts',(40.1006629477018,-4.25989948680445,337.461856796288));
#28564=CARTESIAN_POINT('Ctrl Pts',(40.093026623158,-4.19057559340086,337.578083585273));
#28565=CARTESIAN_POINT('Ctrl Pts',(40.0853902986142,-4.11664386547576,337.69117564409));
#28566=CARTESIAN_POINT('Ctrl Pts',(40.077745772101,-4.04263272948421,337.804389172023));
#28567=CARTESIAN_POINT('Ctrl Pts',(40.0701012455878,-3.96400410309239,337.914460912896));
#28568=CARTESIAN_POINT('Ctrl Pts',(40.0624567190746,-3.88107476123571,338.021000125819));
#28569=CARTESIAN_POINT('Ctrl Pts',(40.0548072650216,-3.79809196444868,338.127608012219));
#28570=CARTESIAN_POINT('Ctrl Pts',(40.0471578109686,-3.71080319463436,338.230678532065));
#28571=CARTESIAN_POINT('Ctrl Pts',(40.0395083569156,-3.61956312757054,338.329856727854));
#28572=CARTESIAN_POINT('Ctrl Pts',(40.0318483389941,-3.5281970583026,338.429171888373));
#28573=CARTESIAN_POINT('Ctrl Pts',(40.0241883210727,-3.43286908885909,338.524583717112));
#28574=CARTESIAN_POINT('Ctrl Pts',(40.0165283031512,-3.33396819129148,338.615776425881));
#28575=CARTESIAN_POINT('Ctrl Pts',(40.0148292343479,-3.31203098025658,338.636003883329));
#28576=CARTESIAN_POINT('Ctrl Pts',(40.0131301655446,-3.28991809917468,338.656023927734));
#28577=CARTESIAN_POINT('Ctrl Pts',(40.0114310967413,-3.26763398618968,338.675833401393));
#28578=CARTESIAN_POINT('Ctrl Pts',(40.0036560179629,-3.16566004986063,338.766483184359));
#28579=CARTESIAN_POINT('Ctrl Pts',(39.9958809391844,-3.05974994568657,338.853029597787));
#28580=CARTESIAN_POINT('Ctrl Pts',(39.988105860406,-2.95026791490481,338.935111471456));
#28581=CARTESIAN_POINT('Ctrl Pts',(39.980340349357,-2.84092060873189,339.017092338154));
#28582=CARTESIAN_POINT('Ctrl Pts',(39.972574838308,-2.7280104314527,339.094619364151));
#28583=CARTESIAN_POINT('Ctrl Pts',(39.964809327259,-2.61193708735453,339.167369399777));
#28584=CARTESIAN_POINT('Ctrl Pts',(39.9570515157368,-2.49597883031505,339.240047303532));
#28585=CARTESIAN_POINT('Ctrl Pts',(39.9492937042146,-2.37686397691438,339.307957436375));
#28586=CARTESIAN_POINT('Ctrl Pts',(39.9415358926924,-2.25502352083456,339.370818228088));
#28587=CARTESIAN_POINT('Ctrl Pts',(39.9337839191694,-2.13327475356172,339.433631715061));
#28588=CARTESIAN_POINT('Ctrl Pts',(39.9260319456464,-2.00880481219777,339.491403245704));
#28589=CARTESIAN_POINT('Ctrl Pts',(39.9182799721234,-1.88207144757164,339.543895919664));
#28590=CARTESIAN_POINT('Ctrl Pts',(39.9105312815658,-1.75539175460049,339.596366362945));
#28591=CARTESIAN_POINT('Ctrl Pts',(39.9027825910081,-1.62645090524884,339.643562246726));
#28592=CARTESIAN_POINT('Ctrl Pts',(39.8950339004505,-1.49572870015399,339.685293877446));
#28593=CARTESIAN_POINT('Ctrl Pts',(39.8872868220727,-1.3650336929059,339.727016825552));
#28594=CARTESIAN_POINT('Ctrl Pts',(39.8795397436949,-1.23255843924232,339.76327766314));
#28595=CARTESIAN_POINT('Ctrl Pts',(39.8717926653171,-1.09879967709113,339.793935995831));
#28596=CARTESIAN_POINT('Ctrl Pts',(39.8640455220113,-0.965039793912857,
339.824594585468));
#28597=CARTESIAN_POINT('Ctrl Pts',(39.8562983787055,-0.829996761785789,
339.849650489228));
#28598=CARTESIAN_POINT('Ctrl Pts',(39.8485512353997,-0.694178946508504,
339.869014135605));
#28599=CARTESIAN_POINT('Ctrl Pts',(39.8408023503716,-0.558330596502665,
339.888382135341));
#28600=CARTESIAN_POINT('Ctrl Pts',(39.8330534653435,-0.42170750361822,339.902055275995));
#28601=CARTESIAN_POINT('Ctrl Pts',(39.8253045803154,-0.284824217742129,
339.909995746178));
#28602=CARTESIAN_POINT('Ctrl Pts',(39.8175474705407,-0.14779564253214,339.917944644458));
#28603=CARTESIAN_POINT('Ctrl Pts',(39.809790360766,-0.0105067134865973,
339.920148694805));
#28604=CARTESIAN_POINT('Ctrl Pts',(39.8020332509913,0.126526390383609,339.916622228221));
#28605=CARTESIAN_POINT('Ctrl Pts',(39.7942719960651,0.263632720363148,339.913093877206));
#28606=CARTESIAN_POINT('Ctrl Pts',(39.7865107411389,0.400482562986988,339.903828933928));
#28607=CARTESIAN_POINT('Ctrl Pts',(39.7787494862127,0.536564787416517,339.888893667427));
#28608=CARTESIAN_POINT('Ctrl Pts',(39.7709758158081,0.67286469905604,339.873934509366));
#28609=CARTESIAN_POINT('Ctrl Pts',(39.7632021454034,0.808394152096627,339.853286961097));
#28610=CARTESIAN_POINT('Ctrl Pts',(39.7554284749988,0.942651253067361,339.827068642312));
#28611=CARTESIAN_POINT('Ctrl Pts',(39.7480166708216,1.07065865368825,339.802070792574));
#28612=CARTESIAN_POINT('Ctrl Pts',(39.7406048666445,1.19750921239909,339.772009205777));
#28613=CARTESIAN_POINT('Ctrl Pts',(39.7331930624674,1.32278248097241,339.737027503671));
#28614=CARTESIAN_POINT('Ctrl Pts',(39.7254179836889,1.45419576560766,339.700331244139));
#28615=CARTESIAN_POINT('Ctrl Pts',(39.7176429049105,1.58428852553508,339.658104408384));
#28616=CARTESIAN_POINT('Ctrl Pts',(39.7098678261321,1.71255993317724,339.610457844702));
#28617=CARTESIAN_POINT('Ctrl Pts',(39.702102315083,1.84067349468632,339.56286991315));
#28618=CARTESIAN_POINT('Ctrl Pts',(39.694336804034,1.96696980052449,339.50987565851));
#28619=CARTESIAN_POINT('Ctrl Pts',(39.686571292985,2.09096080431581,339.451636325815));
#28620=CARTESIAN_POINT('Ctrl Pts',(39.6788134814628,2.21482887066563,339.393454737588));
#28621=CARTESIAN_POINT('Ctrl Pts',(39.6710556699406,2.33639583215662,339.330038585723));
#28622=CARTESIAN_POINT('Ctrl Pts',(39.6632978584184,2.45519167497269,339.261597928201));
#28623=CARTESIAN_POINT('Ctrl Pts',(39.6555458848953,2.57389812015029,339.193208774443));
#28624=CARTESIAN_POINT('Ctrl Pts',(39.6477939113723,2.68983726012588,339.11980283546));
#28625=CARTESIAN_POINT('Ctrl Pts',(39.6400419378492,2.80256216509931,339.041636843317));
#28626=CARTESIAN_POINT('Ctrl Pts',(39.6322932472916,2.91523933100809,338.963503954517));
#28627=CARTESIAN_POINT('Ctrl Pts',(39.624544556734,3.02470464876855,338.880615244278));
#28628=CARTESIAN_POINT('Ctrl Pts',(39.6167958661763,3.13053895336149,338.793271533121));
#28629=CARTESIAN_POINT('Ctrl Pts',(39.6090487877985,3.23635123824341,338.705945994552));
#28630=CARTESIAN_POINT('Ctrl Pts',(39.6013017094207,3.33853371134819,338.614167547376));
#28631=CARTESIAN_POINT('Ctrl Pts',(39.5935546310429,3.43669949865113,338.518277933659));
#28632=CARTESIAN_POINT('Ctrl Pts',(39.5858074877371,3.53486610867779,338.422387516294));
#28633=CARTESIAN_POINT('Ctrl Pts',(39.5780603444313,3.6290156861453,338.322386136794));
#28634=CARTESIAN_POINT('Ctrl Pts',(39.5703132011255,3.71879780256008,338.218652818521));
#28635=CARTESIAN_POINT('Ctrl Pts',(39.5625643160974,3.80860010390089,338.114896178796));
#28636=CARTESIAN_POINT('Ctrl Pts',(39.5548154310692,3.89403273457162,338.007406226236));
#28637=CARTESIAN_POINT('Ctrl Pts',(39.5470665460411,3.97478544569988,337.896595194906));
#28638=CARTESIAN_POINT('Ctrl Pts',(39.5393094362664,4.05562386859006,337.785666547602));
#28639=CARTESIAN_POINT('Ctrl Pts',(39.5315523264916,4.13177221869177,337.671410096348));
#28640=CARTESIAN_POINT('Ctrl Pts',(39.5237952167169,4.20296321316905,337.554267662413));
#28641=CARTESIAN_POINT('Ctrl Pts',(39.5160339617907,4.27419224983758,337.437062631306));
#28642=CARTESIAN_POINT('Ctrl Pts',(39.5082727068645,4.34045846366295,337.316968886651));
#28643=CARTESIAN_POINT('Ctrl Pts',(39.5005114519383,4.40154097946671,337.194452111251));
#28644=CARTESIAN_POINT('Ctrl Pts',(39.4927377815337,4.46272120738893,337.071739348939));
#28645=CARTESIAN_POINT('Ctrl Pts',(39.484964111129,4.51870100727224,336.946596167359));
#28646=CARTESIAN_POINT('Ctrl Pts',(39.4771904407244,4.56930768466818,336.819508270202));
#28647=CARTESIAN_POINT('Ctrl Pts',(39.4697786365474,4.61755860905538,336.698336345234));
#28648=CARTESIAN_POINT('Ctrl Pts',(39.4623668323704,4.66092529538337,336.57539695463));
#28649=CARTESIAN_POINT('Ctrl Pts',(39.4549550281934,4.69930098958318,336.451121384241));
#28650=CARTESIAN_POINT('Ctrl Pts',(39.447179949415,4.73955759087155,336.320754697949));
#28651=CARTESIAN_POINT('Ctrl Pts',(39.4394048706366,4.77444880093273,336.188505556916));
#28652=CARTESIAN_POINT('Ctrl Pts',(39.4316297918581,4.80379680792477,336.054855104112));
#28653=CARTESIAN_POINT('Ctrl Pts',(39.4238642808091,4.83310870032582,335.921369116699));
#28654=CARTESIAN_POINT('Ctrl Pts',(39.4160987697601,4.85689087898534,335.786485626711));
#28655=CARTESIAN_POINT('Ctrl Pts',(39.4083332587111,4.8750148283944,335.650702301698));
#28656=CARTESIAN_POINT('Ctrl Pts',(39.400575447189,4.89312080785479,335.515053606247));
#28657=CARTESIAN_POINT('Ctrl Pts',(39.3928176356667,4.90557967120106,335.37850723622));
#28658=CARTESIAN_POINT('Ctrl Pts',(39.3850598241446,4.91231370922472,335.241572110689));
#28659=CARTESIAN_POINT('Ctrl Pts',(39.3773078506216,4.91904267967125,335.104740033182));
#28660=CARTESIAN_POINT('Ctrl Pts',(39.3695558770986,4.92005538076119,334.967520171308));
#28661=CARTESIAN_POINT('Ctrl Pts',(39.3618039035756,4.9153258446041,334.830427290324));
#28662=CARTESIAN_POINT('Ctrl Pts',(39.354055213018,4.91059831140839,334.693392468256));
#28663=CARTESIAN_POINT('Ctrl Pts',(39.3463065224604,4.90013339117445,334.556484909947));
#28664=CARTESIAN_POINT('Ctrl Pts',(39.3385578319027,4.88395721605244,334.420219891451));
#28665=CARTESIAN_POINT('Ctrl Pts',(39.3308107535249,4.86778440651878,334.28398322403));
#28666=CARTESIAN_POINT('Ctrl Pts',(39.323063675147,4.84590275170732,334.148389218415));
#28667=CARTESIAN_POINT('Ctrl Pts',(39.3153165967692,4.81839027007874,334.01394814147));
#28668=CARTESIAN_POINT('Ctrl Pts',(39.3075694534634,4.79087755786903,333.879505937779));
#28669=CARTESIAN_POINT('Ctrl Pts',(39.2998223101577,4.75773400308046,333.746217064967));
#28670=CARTESIAN_POINT('Ctrl Pts',(39.2920751668518,4.71908869758066,333.614581317122));
#28671=CARTESIAN_POINT('Ctrl Pts',(39.2843262818238,4.68043470379588,333.482915974767));
#28672=CARTESIAN_POINT('Ctrl Pts',(39.2765773967957,4.6362766080701,333.352904871909));
#28673=CARTESIAN_POINT('Ctrl Pts',(39.2688285117676,4.58679317335638,333.22503198695));
#28674=CARTESIAN_POINT('Ctrl Pts',(39.2610714019929,4.53725721641367,333.097023376389));
#28675=CARTESIAN_POINT('Ctrl Pts',(39.2533142922182,4.48238477063109,332.971157882427));
#28676=CARTESIAN_POINT('Ctrl Pts',(39.2455571824434,4.4224027308611,332.847899363744));
#28677=CARTESIAN_POINT('Ctrl Pts',(39.2377959275173,4.36238863860695,332.72457497965));
#28678=CARTESIAN_POINT('Ctrl Pts',(39.2300346725911,4.29725969729425,332.603860690506));
#28679=CARTESIAN_POINT('Ctrl Pts',(39.2222734176649,4.22728798129583,332.486194242649));
#28680=CARTESIAN_POINT('Ctrl Pts',(39.2144997472603,4.15720433335545,332.368339566822));
#28681=CARTESIAN_POINT('Ctrl Pts',(39.2067260768556,4.0822626439893,332.253542802556));
#28682=CARTESIAN_POINT('Ctrl Pts',(39.198952406451,4.00277789691776,332.142212014434));
#28683=CARTESIAN_POINT('Ctrl Pts',(39.1915406022738,3.92699318394469,332.036063701282));
#28684=CARTESIAN_POINT('Ctrl Pts',(39.1841287980967,3.84707902993871,331.933066171042));
#28685=CARTESIAN_POINT('Ctrl Pts',(39.1767169939195,3.76334034162273,331.83354258901));
#28686=CARTESIAN_POINT('Ctrl Pts',(39.1689419151411,3.67549737074852,331.729141059758));
#28687=CARTESIAN_POINT('Ctrl Pts',(39.1611668363626,3.58316788246391,331.628232698179));
#28688=CARTESIAN_POINT('Ctrl Pts',(39.1533917575842,3.48666025596526,331.531227404114));
#28689=CARTESIAN_POINT('Ctrl Pts',(39.1456262465352,3.39027138824499,331.434341481238));
#28690=CARTESIAN_POINT('Ctrl Pts',(39.1378607354862,3.28971488539471,331.341349343787));
#28691=CARTESIAN_POINT('Ctrl Pts',(39.1300952244372,3.18533969955816,331.252628379661));
#28692=CARTESIAN_POINT('Ctrl Pts',(39.122337412915,3.08106800202204,331.16399538263));
#28693=CARTESIAN_POINT('Ctrl Pts',(39.1145796013928,2.97298545222309,331.079625382793));
#28694=CARTESIAN_POINT('Ctrl Pts',(39.1068217898706,2.86147795815404,330.999859132793));
#28695=CARTESIAN_POINT('Ctrl Pts',(39.0990698163476,2.75005437701114,330.920152909427));
#28696=CARTESIAN_POINT('Ctrl Pts',(39.0913178428247,2.63521129837364,330.845043766542));
#28697=CARTESIAN_POINT('Ctrl Pts',(39.0835658693017,2.51736754661055,330.774832110108));
#28698=CARTESIAN_POINT('Ctrl Pts',(39.0758171787441,2.39957370174583,330.704650188353));
#28699=CARTESIAN_POINT('Ctrl Pts',(39.0680684881864,2.27878204635426,330.639361827482));
#28700=CARTESIAN_POINT('Ctrl Pts',(39.0603197976288,2.15544002866688,330.579223897852));
#28701=CARTESIAN_POINT('Ctrl Pts',(39.052572719251,2.03212367331644,330.519098480421));
#28702=CARTESIAN_POINT('Ctrl Pts',(39.0448256408732,1.90625836223653,330.464121533956));
#28703=CARTESIAN_POINT('Ctrl Pts',(39.0370785624954,1.77831540998343,330.414503585748));
#28704=CARTESIAN_POINT('Ctrl Pts',(39.0293314191896,1.65037138544551,330.364885221694));
#28705=CARTESIAN_POINT('Ctrl Pts',(39.0215842758838,1.52035004943253,330.320626086811));
#28706=CARTESIAN_POINT('Ctrl Pts',(39.013837132578,1.38874154847184,330.28188809225));
#28707=CARTESIAN_POINT('Ctrl Pts',(39.0060882475499,1.25710345912512,330.243141388567));
#28708=CARTESIAN_POINT('Ctrl Pts',(38.9983393625217,1.12387786967725,330.209918405542));
#28709=CARTESIAN_POINT('Ctrl Pts',(38.9905904774936,0.989568506783285,330.182330726079));
#28710=CARTESIAN_POINT('Ctrl Pts',(38.9828333677189,0.855116586544422,330.154713764768));
#28711=CARTESIAN_POINT('Ctrl Pts',(38.9750762579442,0.719578978456182,330.132744134136));
#28712=CARTESIAN_POINT('Ctrl Pts',(38.9673191481695,0.583468537002301,330.116482054008));
#28713=CARTESIAN_POINT('Ctrl Pts',(38.9595578932433,0.447285362480382,330.100211283944));
#28714=CARTESIAN_POINT('Ctrl Pts',(38.9517966383171,0.310529134170466,330.089654171718));
#28715=CARTESIAN_POINT('Ctrl Pts',(38.944035383391,0.17371519736055,330.084818813848));
#28716=CARTESIAN_POINT('Ctrl Pts',(38.9362617129863,0.0366824028394827,
330.07997572098));
#28717=CARTESIAN_POINT('Ctrl Pts',(38.9284880425817,-0.100407893582374,
330.080872670198));
#28718=CARTESIAN_POINT('Ctrl Pts',(38.920714372177,-0.237042085926806,330.087465612131));
#28719=CARTESIAN_POINT('Ctrl Pts',(38.9133025679999,-0.367315923746237,
330.09375165103));
#28720=CARTESIAN_POINT('Ctrl Pts',(38.9058907638227,-0.4971748784866,330.105215294418));
#28721=CARTESIAN_POINT('Ctrl Pts',(38.8984789596456,-0.626182191032283,
330.121775023009));
#28722=CARTESIAN_POINT('Ctrl Pts',(38.8907038808672,-0.761512536258101,
330.139146393228));
#28723=CARTESIAN_POINT('Ctrl Pts',(38.8829288020887,-0.8963333142709,330.16218092512));
#28724=CARTESIAN_POINT('Ctrl Pts',(38.8751537233103,-1.03013294987281,330.190841116361));
#28725=CARTESIAN_POINT('Ctrl Pts',(38.8673882122612,-1.16376793650519,330.219466039412));
#28726=CARTESIAN_POINT('Ctrl Pts',(38.8596227012122,-1.29638390241144,330.253702766475));
#28727=CARTESIAN_POINT('Ctrl Pts',(38.8518571901632,-1.42747465602692,330.293462082496));
#28728=CARTESIAN_POINT('Ctrl Pts',(38.844099378641,-1.55843543277844,330.333181977039));
#28729=CARTESIAN_POINT('Ctrl Pts',(38.8363415671188,-1.68787363506793,330.378413450944));
#28730=CARTESIAN_POINT('Ctrl Pts',(38.8285837555966,-1.81529387977036,330.429016386753));
#28731=CARTESIAN_POINT('Ctrl Pts',(38.8208317820736,-1.94261823669775,330.479581242249));
#28732=CARTESIAN_POINT('Ctrl Pts',(38.8130798085506,-2.06792729687868,330.535509370169));
#28733=CARTESIAN_POINT('Ctrl Pts',(38.8053278350276,-2.19074179262632,330.596611139072));
#28734=CARTESIAN_POINT('Ctrl Pts',(38.7975791444699,-2.31350427636192,330.657687031341));
#28735=CARTESIAN_POINT('Ctrl Pts',(38.7898304539123,-2.43377394764012,330.723932033024));
#28736=CARTESIAN_POINT('Ctrl Pts',(38.7820817633547,-2.55109265878631,330.795108882648));
#28737=CARTESIAN_POINT('Ctrl Pts',(38.7743346849768,-2.66838696079509,330.866270923334));
#28738=CARTESIAN_POINT('Ctrl Pts',(38.766587606599,-2.78273118993459,330.942362568331));
#28739=CARTESIAN_POINT('Ctrl Pts',(38.7588405282211,-2.89369325396463,331.023101407572));
#28740=CARTESIAN_POINT('Ctrl Pts',(38.7510933849153,-3.00465624796379,331.103840923481));
#28741=CARTESIAN_POINT('Ctrl Pts',(38.7433462416095,-3.11223670425458,331.189227481345));
#28742=CARTESIAN_POINT('Ctrl Pts',(38.7355990983037,-3.21603322188358,331.278936525905));
#28743=CARTESIAN_POINT('Ctrl Pts',(38.7278502132756,-3.31985307517255,331.368665738963));
#28744=CARTESIAN_POINT('Ctrl Pts',(38.7201013282475,-3.41988700131146,331.462719116923));
#28745=CARTESIAN_POINT('Ctrl Pts',(38.7123524432195,-3.51576857245959,331.560733449207));
#28746=CARTESIAN_POINT('Ctrl Pts',(38.7045953334447,-3.6117519132985,331.658851814916));
#28747=CARTESIAN_POINT('Ctrl Pts',(38.69683822367,-3.70357382128163,331.760939253373));
#28748=CARTESIAN_POINT('Ctrl Pts',(38.6890811138953,-3.79090612128399,331.866597082705));
#28749=CARTESIAN_POINT('Ctrl Pts',(38.6813198589691,-3.87828508887506,331.972311372203));
#28750=CARTESIAN_POINT('Ctrl Pts',(38.6735586040429,-3.96116943198058,332.081599542963));
#28751=CARTESIAN_POINT('Ctrl Pts',(38.6657973491168,-4.0392734591617,332.194032611627));
#28752=CARTESIAN_POINT('Ctrl Pts',(38.6580236787121,-4.11750242733227,332.306645536559));
#28753=CARTESIAN_POINT('Ctrl Pts',(38.6502500083074,-4.19093558923302,332.422413082202));
#28754=CARTESIAN_POINT('Ctrl Pts',(38.6424763379028,-4.2593320452533,332.540879508691));
#28755=CARTESIAN_POINT('Ctrl Pts',(38.6350645337257,-4.32454462979014,332.653831294523));
#28756=CARTESIAN_POINT('Ctrl Pts',(38.6276527295487,-4.38517873921408,332.769236095203));
#28757=CARTESIAN_POINT('Ctrl Pts',(38.6202409253717,-4.44106656941066,332.886682515909));
#28758=CARTESIAN_POINT('Ctrl Pts',(38.6118318156202,-4.50447446398924,333.019932102386));
#28759=CARTESIAN_POINT('Ctrl Pts',(38.6034227058687,-4.56194910346594,333.156179451567));
#28760=CARTESIAN_POINT('Ctrl Pts',(38.5950135961173,-4.61322019579876,333.294895168157));
#28761=CARTESIAN_POINT('Ctrl Pts',(38.5866322854229,-4.66432179480058,333.433152314668));
#28762=CARTESIAN_POINT('Ctrl Pts',(38.5782509747286,-4.7092606479371,333.573861283209));
#28763=CARTESIAN_POINT('Ctrl Pts',(38.5698696640342,-4.74781433414765,333.716472785266));
#28764=CARTESIAN_POINT('Ctrl Pts',(38.5615052133412,-4.78629046504147,333.858797407357));
#28765=CARTESIAN_POINT('Ctrl Pts',(38.5531407626483,-4.81840695593296,334.003016657154));
#28766=CARTESIAN_POINT('Ctrl Pts',(38.5447763119554,-4.84398994818294,334.148563305699));
#28767=CARTESIAN_POINT('Ctrl Pts',(38.5364387881212,-4.86949058360599,334.293641410141));
#28768=CARTESIAN_POINT('Ctrl Pts',(38.5281012642869,-4.88849961290795,334.440038108003));
#28769=CARTESIAN_POINT('Ctrl Pts',(38.5197637404527,-4.90089360764275,334.587174481086));
#28770=CARTESIAN_POINT('Ctrl Pts',(38.5120212431428,-4.91240307649727,334.723810129204));
#28771=CARTESIAN_POINT('Ctrl Pts',(38.5042787458329,-4.918208425872,334.861083299193));
#28772=CARTESIAN_POINT('Ctrl Pts',(38.4965362485229,-4.91824977738391,334.998520215163));
#28773=CARTESIAN_POINT('',(41.9965362485248,-4.91824873401151,335.003528865855));
#28774=CARTESIAN_POINT('Ctrl Pts',(41.9965362484901,-4.91824873401107,335.003528866466));
#28775=CARTESIAN_POINT('Ctrl Pts',(41.984056611213,-4.91809120867879,335.223074937012));
#28776=CARTESIAN_POINT('Ctrl Pts',(41.971576973936,-4.9032326330616,335.442100836012));
#28777=CARTESIAN_POINT('Ctrl Pts',(41.9590973366589,-4.87388334896147,335.659123784441));
#28778=CARTESIAN_POINT('Ctrl Pts',(41.9513222578805,-4.85559812232357,335.794333685443));
#28779=CARTESIAN_POINT('Ctrl Pts',(41.9435471791021,-4.8316533057367,335.928995772172));
#28780=CARTESIAN_POINT('Ctrl Pts',(41.9357721003236,-4.80208985672172,336.062598734457));
#28781=CARTESIAN_POINT('Ctrl Pts',(41.9280065892746,-4.77256278741286,336.196037289792));
#28782=CARTESIAN_POINT('Ctrl Pts',(41.9202410782257,-4.73743092636431,336.328418935924));
#28783=CARTESIAN_POINT('Ctrl Pts',(41.9124755671766,-4.69678690627934,336.459238095549));
#28784=CARTESIAN_POINT('Ctrl Pts',(41.9047177556544,-4.65618318485865,336.589927547597));
#28785=CARTESIAN_POINT('Ctrl Pts',(41.8969599441322,-4.61007829592562,336.719057225286));
#28786=CARTESIAN_POINT('Ctrl Pts',(41.88920213261,-4.55861570040531,336.846132703388));
#28787=CARTESIAN_POINT('Ctrl Pts',(41.881450159087,-4.5071918321201,336.973112553163));
#28788=CARTESIAN_POINT('Ctrl Pts',(41.873698185564,-4.45041842856548,337.098040919456));
#28789=CARTESIAN_POINT('Ctrl Pts',(41.865946212041,-4.38848835464824,337.220439826615));
#28790=CARTESIAN_POINT('Ctrl Pts',(41.8581975214834,-4.32658450815407,337.342786897763));
#28791=CARTESIAN_POINT('Ctrl Pts',(41.8504488309257,-4.2595285109275,337.462606292326));
#28792=CARTESIAN_POINT('Ctrl Pts',(41.8427001403681,-4.18756071414259,337.579441475954));
#28793=CARTESIAN_POINT('Ctrl Pts',(41.8349530619903,-4.11560789085889,337.696252351045));
#28794=CARTESIAN_POINT('Ctrl Pts',(41.8272059836125,-4.03874550560012,337.810079917602));
#28795=CARTESIAN_POINT('Ctrl Pts',(41.8194589052346,-3.95725888108104,337.920494001125));
#28796=CARTESIAN_POINT('Ctrl Pts',(41.8117117619288,-3.87577157362567,338.030909010023));
#28797=CARTESIAN_POINT('Ctrl Pts',(41.803964618623,-3.7896601817132,338.137910164327));
#28798=CARTESIAN_POINT('Ctrl Pts',(41.7962174753172,-3.69925196494271,338.241098264843));
#28799=CARTESIAN_POINT('Ctrl Pts',(41.7884685902891,-3.60882342248567,338.344309564235));
#28800=CARTESIAN_POINT('Ctrl Pts',(41.780719705261,-3.51409639043736,338.443705810059));
#28801=CARTESIAN_POINT('Ctrl Pts',(41.7729708202329,-3.41543654656948,338.538923036583));
#28802=CARTESIAN_POINT('Ctrl Pts',(41.7652137104582,-3.31667198412384,338.634241327655));
#28803=CARTESIAN_POINT('Ctrl Pts',(41.7574566006834,-3.21396655294616,338.725371466923));
#28804=CARTESIAN_POINT('Ctrl Pts',(41.7496994909087,-3.10772114286859,338.811987980132));
#28805=CARTESIAN_POINT('Ctrl Pts',(41.7419382359825,-3.00141895864101,338.898650778435));
#28806=CARTESIAN_POINT('Ctrl Pts',(41.7341769810564,-2.89157333909619,338.980794910708));
#28807=CARTESIAN_POINT('Ctrl Pts',(41.7264157261303,-2.77861518785151,339.058137590119));
#28808=CARTESIAN_POINT('Ctrl Pts',(41.7186420557256,-2.66547634037781,339.135603992612));
#28809=CARTESIAN_POINT('Ctrl Pts',(41.7108683853209,-2.5492153432678,339.208253386567));
#28810=CARTESIAN_POINT('Ctrl Pts',(41.7030947149162,-2.43028955343579,339.275847956717));
#28811=CARTESIAN_POINT('Ctrl Pts',(41.6956829107391,-2.31689978773155,339.340295983365));
#28812=CARTESIAN_POINT('Ctrl Pts',(41.688271106562,-2.20108799401771,339.400149067519));
#28813=CARTESIAN_POINT('Ctrl Pts',(41.6808593023848,-2.08326669136225,339.45524218816));
#28814=CARTESIAN_POINT('Ctrl Pts',(41.6730842236064,-1.95967061569291,339.513035586757));
#28815=CARTESIAN_POINT('Ctrl Pts',(41.665309144828,-1.83347247986494,339.565773261686));
#28816=CARTESIAN_POINT('Ctrl Pts',(41.6575340660495,-1.70512441997229,339.61321295573));
#28817=CARTESIAN_POINT('Ctrl Pts',(41.6497685550005,-1.57693430053855,339.66059427221));
#28818=CARTESIAN_POINT('Ctrl Pts',(41.6420030439515,-1.44659988418907,339.702690445528));
#28819=CARTESIAN_POINT('Ctrl Pts',(41.6342375329025,-1.3145964505342,339.739305775611));
#28820=CARTESIAN_POINT('Ctrl Pts',(41.6264797213803,-1.18272389866784,339.775884801489));
#28821=CARTESIAN_POINT('Ctrl Pts',(41.6187219098581,-1.04918599693886,339.806993694837));
#28822=CARTESIAN_POINT('Ctrl Pts',(41.6109640983359,-0.914476153007197,
339.832485533148));
#28823=CARTESIAN_POINT('Ctrl Pts',(41.6032121248129,-0.779867682505355,
339.857958188042));
#28824=CARTESIAN_POINT('Ctrl Pts',(41.5954601512899,-0.644089407738613,
339.877822129175));
#28825=CARTESIAN_POINT('Ctrl Pts',(41.5877081777669,-0.5076476388997,339.891980880709));
#28826=CARTESIAN_POINT('Ctrl Pts',(41.5799594872093,-0.371263653230711,
339.906133636003));
#28827=CARTESIAN_POINT('Ctrl Pts',(41.5722107966516,-0.234217120336566,
339.914585966991));
#28828=CARTESIAN_POINT('Ctrl Pts',(41.564462106094,-0.0970220175030706,
339.917292933172));
#28829=CARTESIAN_POINT('Ctrl Pts',(41.5567150277162,0.0401445407434038,
339.919999336145));
#28830=CARTESIAN_POINT('Ctrl Pts',(41.5489679493384,0.177459216891762,339.916962744282));
#28831=CARTESIAN_POINT('Ctrl Pts',(41.5412208709606,0.314405863535913,339.908190299436));
#28832=CARTESIAN_POINT('Ctrl Pts',(41.5334737276547,0.451353657924867,339.899417781068));
#28833=CARTESIAN_POINT('Ctrl Pts',(41.5257265843489,0.587933026582659,339.884909338821));
#28834=CARTESIAN_POINT('Ctrl Pts',(41.5179794410431,0.723631175445326,339.864724142685));
#28835=CARTESIAN_POINT('Ctrl Pts',(41.510230556015,0.859359832132442,339.844534408489));
#28836=CARTESIAN_POINT('Ctrl Pts',(41.5024816709869,0.994206488249092,339.818665438297));
#28837=CARTESIAN_POINT('Ctrl Pts',(41.4947327859589,1.12766718802091,339.787227775609));
#28838=CARTESIAN_POINT('Ctrl Pts',(41.4869756761841,1.26126954435873,339.75575674466));
#28839=CARTESIAN_POINT('Ctrl Pts',(41.4792185664094,1.39348262469229,339.718705303863));
#28840=CARTESIAN_POINT('Ctrl Pts',(41.4714614566346,1.5238157862847,339.676234437234));
#28841=CARTESIAN_POINT('Ctrl Pts',(41.4637002017085,1.65421859375134,339.633740875531));
#28842=CARTESIAN_POINT('Ctrl Pts',(41.4559389467823,1.78273911472399,339.585822254005));
#28843=CARTESIAN_POINT('Ctrl Pts',(41.4481776918562,1.90890636105059,339.532687896518));
#28844=CARTESIAN_POINT('Ctrl Pts',(41.4404040214515,2.03527543385351,339.479468541376));
#28845=CARTESIAN_POINT('Ctrl Pts',(41.4326303510468,2.15928335572751,339.421016944276));
#28846=CARTESIAN_POINT('Ctrl Pts',(41.4248566806422,2.28048264067236,339.35758901092));
#28847=CARTESIAN_POINT('Ctrl Pts',(41.4174448764651,2.39604006974384,339.297113663122));
#28848=CARTESIAN_POINT('Ctrl Pts',(41.410033072288,2.50904421197558,339.232114993257));
#28849=CARTESIAN_POINT('Ctrl Pts',(41.402621268111,2.61913305993308,339.162850595069));
#28850=CARTESIAN_POINT('Ctrl Pts',(41.3948461893325,2.73461769026715,339.090191342397));
#28851=CARTESIAN_POINT('Ctrl Pts',(41.3870711105541,2.84725897876825,339.012608019652));
#28852=CARTESIAN_POINT('Ctrl Pts',(41.3792960317757,2.95660852938928,338.930349738438));
#28853=CARTESIAN_POINT('Ctrl Pts',(41.3715305207267,3.06582351842659,338.848192681277));
#28854=CARTESIAN_POINT('Ctrl Pts',(41.3637650096776,3.1717545199259,338.761372344866));
#28855=CARTESIAN_POINT('Ctrl Pts',(41.3559994986286,3.2739797644531,338.670182497431));
#28856=CARTESIAN_POINT('Ctrl Pts',(41.3482416871065,3.37610365235279,338.579083064996));
#28857=CARTESIAN_POINT('Ctrl Pts',(41.3404838755843,3.47452880547699,338.483623001744));
#28858=CARTESIAN_POINT('Ctrl Pts',(41.3327260640621,3.5688646623577,338.384137716505));
#28859=CARTESIAN_POINT('Ctrl Pts',(41.324974090539,3.66312952851454,338.284727297098));
#28860=CARTESIAN_POINT('Ctrl Pts',(41.317222117016,3.75331095582416,338.181297967484));
#28861=CARTESIAN_POINT('Ctrl Pts',(41.309470143493,3.83905382219862,338.074223286094));
#28862=CARTESIAN_POINT('Ctrl Pts',(41.3017214529354,3.92476037641827,337.967193950895));
#28863=CARTESIAN_POINT('Ctrl Pts',(41.2939727623778,4.00603186454649,337.856522638917));
#28864=CARTESIAN_POINT('Ctrl Pts',(41.2862240718202,4.08255235255462,337.742617244741));
#28865=CARTESIAN_POINT('Ctrl Pts',(41.2784769934423,4.159056919836,337.628735549534));
#28866=CARTESIAN_POINT('Ctrl Pts',(41.2707299150645,4.23081223533374,337.511621434784));
#28867=CARTESIAN_POINT('Ctrl Pts',(41.2629828366867,4.29754498780668,337.391712804723));
#28868=CARTESIAN_POINT('Ctrl Pts',(41.2552356933809,4.36427829956437,337.271803169713));
#28869=CARTESIAN_POINT('Ctrl Pts',(41.247488550075,4.42598877425816,337.149099314222));
#28870=CARTESIAN_POINT('Ctrl Pts',(41.2397414067692,4.48244866690289,337.024064477995));
#28871=CARTESIAN_POINT('Ctrl Pts',(41.2319925217411,4.53892125293017,336.899001531282));
#28872=CARTESIAN_POINT('Ctrl Pts',(41.2242436367131,4.59014074713045,336.771606917195));
#28873=CARTESIAN_POINT('Ctrl Pts',(41.216494751685,4.63592738850247,336.642364244324));
#28874=CARTESIAN_POINT('Ctrl Pts',(41.2087376419103,4.6817626282887,336.512984391944));
#28875=CARTESIAN_POINT('Ctrl Pts',(41.2009805321356,4.72215336541781,336.381752931423));
#28876=CARTESIAN_POINT('Ctrl Pts',(41.1932234223609,4.75696945984595,336.249169572393));
#28877=CARTESIAN_POINT('Ctrl Pts',(41.1854621674347,4.79180415888178,336.116515365055));
#28878=CARTESIAN_POINT('Ctrl Pts',(41.1777009125085,4.82105819614543,335.982508201426));
#28879=CARTESIAN_POINT('Ctrl Pts',(41.1699396575823,4.84465271782552,335.847657422645));
#28880=CARTESIAN_POINT('Ctrl Pts',(41.1621659871777,4.86828498305086,335.712590926566));
#28881=CARTESIAN_POINT('Ctrl Pts',(41.154392316773,4.88623959013899,335.576678506327));
#28882=CARTESIAN_POINT('Ctrl Pts',(41.1466186463684,4.8984895753013,335.44043494771));
#28883=CARTESIAN_POINT('Ctrl Pts',(41.1392068421913,4.91016932070711,335.310533559526));
#28884=CARTESIAN_POINT('Ctrl Pts',(41.1317950380142,4.91666357807027,335.180331455599));
#28885=CARTESIAN_POINT('Ctrl Pts',(41.1243832338371,4.91799306046915,335.050272454458));
#28886=CARTESIAN_POINT('Ctrl Pts',(41.1166081550587,4.91938770476073,334.913838874246));
#28887=CARTESIAN_POINT('Ctrl Pts',(41.1088330762803,4.91510289806022,334.777131623981));
#28888=CARTESIAN_POINT('Ctrl Pts',(41.1010579975018,4.90510547080146,334.64066257805));
#28889=CARTESIAN_POINT('Ctrl Pts',(41.0932924864528,4.8951203460134,334.504361465968));
#28890=CARTESIAN_POINT('Ctrl Pts',(41.0855269754038,4.87943661612563,334.368298361086));
#28891=CARTESIAN_POINT('Ctrl Pts',(41.0777614643548,4.85807307346464,334.232986913164));
#28892=CARTESIAN_POINT('Ctrl Pts',(41.0700036528325,4.83673071281841,334.097809626936));
#28893=CARTESIAN_POINT('Ctrl Pts',(41.0622458413103,4.80971980706881,333.963382898143));
#28894=CARTESIAN_POINT('Ctrl Pts',(41.0544880297881,4.77711105343428,333.830216667217));
#28895=CARTESIAN_POINT('Ctrl Pts',(41.0467360562651,4.74452683892095,333.697150648104));
#28896=CARTESIAN_POINT('Ctrl Pts',(41.0389840827421,4.70635325400689,333.565343616915));
#28897=CARTESIAN_POINT('Ctrl Pts',(41.0312321092191,4.6627122550075,333.435296357292));
#28898=CARTESIAN_POINT('Ctrl Pts',(41.0234834186615,4.61908973799709,333.305304172762));
#28899=CARTESIAN_POINT('Ctrl Pts',(41.0157347281038,4.5700045362693,333.177070647314));
#28900=CARTESIAN_POINT('Ctrl Pts',(41.0079860375462,4.51562868704753,333.051082191776));
#28901=CARTESIAN_POINT('Ctrl Pts',(41.0002389591684,4.46126415117542,332.925119949189));
#28902=CARTESIAN_POINT('Ctrl Pts',(40.9924918807906,4.40161131209717,332.801402206056));
#28903=CARTESIAN_POINT('Ctrl Pts',(40.9847448024127,4.33689050842846,332.680395770739));
#28904=CARTESIAN_POINT('Ctrl Pts',(40.9769976591069,4.27216916233707,332.559388321272));
#28905=CARTESIAN_POINT('Ctrl Pts',(40.9692505158011,4.20237995128564,332.441092569615));
#28906=CARTESIAN_POINT('Ctrl Pts',(40.9615033724953,4.12778917757917,332.325950716991));
#28907=CARTESIAN_POINT('Ctrl Pts',(40.9537544874672,4.05318163428327,332.210782978035));
#28908=CARTESIAN_POINT('Ctrl Pts',(40.9460056024392,3.97377059273798,332.098770877057));
#28909=CARTESIAN_POINT('Ctrl Pts',(40.9382567174111,3.88986545073272,331.990327287279));
#28910=CARTESIAN_POINT('Ctrl Pts',(40.9304996076363,3.80587125094262,331.881768594354));
#28911=CARTESIAN_POINT('Ctrl Pts',(40.9227424978616,3.71737366157023,331.776786288456));
#28912=CARTESIAN_POINT('Ctrl Pts',(40.9149853880868,3.62472247286212,331.67576022868));
#28913=CARTESIAN_POINT('Ctrl Pts',(40.9072241331606,3.53202177432123,331.574680183807));
#28914=CARTESIAN_POINT('Ctrl Pts',(40.8994628782345,3.43516332966786,331.477560874196));
#28915=CARTESIAN_POINT('Ctrl Pts',(40.8917016233083,3.33453278241015,331.384744243413));
#28916=CARTESIAN_POINT('Ctrl Pts',(40.8839279529037,3.23374125907223,331.291779136271));
#28917=CARTESIAN_POINT('Ctrl Pts',(40.876154282499,3.12916587345923,331.203130714881));
#28918=CARTESIAN_POINT('Ctrl Pts',(40.8683806120943,3.02122492826498,331.119100233795));
#28919=CARTESIAN_POINT('Ctrl Pts',(40.8609688079173,2.91830866003876,331.03898139182));
#28920=CARTESIAN_POINT('Ctrl Pts',(40.8535570037402,2.81233334840604,330.963060402824));
#28921=CARTESIAN_POINT('Ctrl Pts',(40.8461451995631,2.70368341887178,330.891560024411));
#28922=CARTESIAN_POINT('Ctrl Pts',(40.8383701207846,2.58970823263953,330.816555199463));
#28923=CARTESIAN_POINT('Ctrl Pts',(40.8305950420063,2.47242943460294,330.746178247451));
#28924=CARTESIAN_POINT('Ctrl Pts',(40.8228199632278,2.35225952089809,330.680734065973));
#28925=CARTESIAN_POINT('Ctrl Pts',(40.8150544521788,2.23223748392244,330.615370417727));
#28926=CARTESIAN_POINT('Ctrl Pts',(40.8072889411298,2.10933175007412,330.554927647437));
#28927=CARTESIAN_POINT('Ctrl Pts',(40.7995234300808,1.98398442799957,330.499667917592));
#28928=CARTESIAN_POINT('Ctrl Pts',(40.7917656185586,1.85876138815972,330.444462977929));
#28929=CARTESIAN_POINT('Ctrl Pts',(40.7840078070364,1.73110193306239,330.394431008472));
#28930=CARTESIAN_POINT('Ctrl Pts',(40.7762499955142,1.60147314081859,330.34978851645));
#28931=CARTESIAN_POINT('Ctrl Pts',(40.7684980219912,1.4719418983519,330.305179619319));
#28932=CARTESIAN_POINT('Ctrl Pts',(40.7607460484682,1.34044463664878,330.265952253609));
#28933=CARTESIAN_POINT('Ctrl Pts',(40.7529940749452,1.20746847291735,330.232274866416));
#28934=CARTESIAN_POINT('Ctrl Pts',(40.7452453843876,1.0745486246702,330.198611741616));
#28935=CARTESIAN_POINT('Ctrl Pts',(40.73749669383,0.940151498215772,330.170494016278));
#28936=CARTESIAN_POINT('Ctrl Pts',(40.7297480032724,0.804779226008882,330.148040245438));
#28937=CARTESIAN_POINT('Ctrl Pts',(40.7220009248945,0.669435119133876,330.125591146294));
#28938=CARTESIAN_POINT('Ctrl Pts',(40.7142538465167,0.533116655427259,330.108803721581));
#28939=CARTESIAN_POINT('Ctrl Pts',(40.7065067681389,0.396335621866165,330.097745300646));
#28940=CARTESIAN_POINT('Ctrl Pts',(40.6987596248331,0.259553441948266,330.086686787031));
#28941=CARTESIAN_POINT('Ctrl Pts',(40.6910124815273,0.122309074046436,330.081357404461));
#28942=CARTESIAN_POINT('Ctrl Pts',(40.6832653382215,-0.0148815139388311,
330.081772514102));
#28943=CARTESIAN_POINT('Ctrl Pts',(40.6755164531934,-0.15210294528073,330.082187717069));
#28944=CARTESIAN_POINT('Ctrl Pts',(40.6677675681653,-0.289270181850473,
330.088349980973));
#28945=CARTESIAN_POINT('Ctrl Pts',(40.6600186831373,-0.425868596852595,
330.100222556002));
#28946=CARTESIAN_POINT('Ctrl Pts',(40.6522615733625,-0.562611998823912,
330.112107732704));
#28947=CARTESIAN_POINT('Ctrl Pts',(40.6445044635878,-0.698784983152917,
330.129715294016));
#28948=CARTESIAN_POINT('Ctrl Pts',(40.6367473538131,-0.833878826649021,
330.152956657408));
#28949=CARTESIAN_POINT('Ctrl Pts',(40.6289860988869,-0.969044859975534,
330.176210440241));
#28950=CARTESIAN_POINT('Ctrl Pts',(40.6212248439607,-1.10313022151564,330.205103941599));
#28951=CARTESIAN_POINT('Ctrl Pts',(40.6134635890346,-1.23563866979703,330.239497910913));
#28952=CARTESIAN_POINT('Ctrl Pts',(40.6056899186299,-1.36835908841126,330.273946899369));
#28953=CARTESIAN_POINT('Ctrl Pts',(40.5979162482253,-1.49949717887832,330.313913824689));
#28954=CARTESIAN_POINT('Ctrl Pts',(40.5901425778206,-1.62857324222994,330.359209953338));
#28955=CARTESIAN_POINT('Ctrl Pts',(40.5827307736435,-1.75164078377967,330.402397536302));
#28956=CARTESIAN_POINT('Ctrl Pts',(40.5753189694664,-1.87283368511698,330.450429233247));
#28957=CARTESIAN_POINT('Ctrl Pts',(40.5679071652892,-1.99175658992211,330.503102319487));
#28958=CARTESIAN_POINT('Ctrl Pts',(40.5601320865108,-2.11650826054398,330.558357070588));
#28959=CARTESIAN_POINT('Ctrl Pts',(40.5523570077323,-2.23915602799083,330.618894306929));
#28960=CARTESIAN_POINT('Ctrl Pts',(40.5445819289539,-2.35922027203999,330.684532149292));
#28961=CARTESIAN_POINT('Ctrl Pts',(40.5368164179049,-2.47913676939318,330.750089220111));
#28962=CARTESIAN_POINT('Ctrl Pts',(40.5290509068559,-2.59647572933525,330.820734222574));
#28963=CARTESIAN_POINT('Ctrl Pts',(40.5212853958069,-2.71077744347913,330.896237249252));
#28964=CARTESIAN_POINT('Ctrl Pts',(40.5135275842847,-2.82496582714058,330.97166541446));
#28965=CARTESIAN_POINT('Ctrl Pts',(40.5057697727625,-2.93612263389326,331.051941804239));
#28966=CARTESIAN_POINT('Ctrl Pts',(40.4980119612403,-3.04381303542199,331.136790807127));
#28967=CARTESIAN_POINT('Ctrl Pts',(40.4902599877173,-3.15142239650851,331.22157595845));
#28968=CARTESIAN_POINT('Ctrl Pts',(40.4825080141942,-3.2555702388323,331.310926632736));
#28969=CARTESIAN_POINT('Ctrl Pts',(40.4747560406712,-3.35585130456456,331.404524359121));
#28970=CARTESIAN_POINT('Ctrl Pts',(40.4670073501136,-3.45608990120594,331.498082446814));
#28971=CARTESIAN_POINT('Ctrl Pts',(40.459258659556,-3.55246469313828,331.595883743111));
#28972=CARTESIAN_POINT('Ctrl Pts',(40.4515099689984,-3.64460425221766,331.697570151053));
#28973=CARTESIAN_POINT('Ctrl Pts',(40.4437628906205,-3.73672464089221,331.799235402288));
#28974=CARTESIAN_POINT('Ctrl Pts',(40.4360158122427,-3.82461128714093,331.904783867871));
#28975=CARTESIAN_POINT('Ctrl Pts',(40.4282687338649,-3.90793061498021,332.013821610988));
#28976=CARTESIAN_POINT('Ctrl Pts',(40.420521590559,-3.99125064111571,332.122860267947));
#28977=CARTESIAN_POINT('Ctrl Pts',(40.4127744472533,-4.07000303516805,332.235387950187));
#28978=CARTESIAN_POINT('Ctrl Pts',(40.4050273039475,-4.14389565976784,332.350979082103));
#28979=CARTESIAN_POINT('Ctrl Pts',(40.3972784189194,-4.21780489699833,332.466596201359));
#28980=CARTESIAN_POINT('Ctrl Pts',(40.3895295338913,-4.28685198017761,332.585277811514));
#28981=CARTESIAN_POINT('Ctrl Pts',(40.3817806488632,-4.35078931891849,332.706571264485));
#28982=CARTESIAN_POINT('Ctrl Pts',(40.3740235390885,-4.41479452141131,332.827993459581));
#28983=CARTESIAN_POINT('Ctrl Pts',(40.3662664293137,-4.47367896288824,332.952032688973));
#28984=CARTESIAN_POINT('Ctrl Pts',(40.358509319539,-4.52724183497792,333.07821321939));
#28985=CARTESIAN_POINT('Ctrl Pts',(40.3507480646129,-4.58083332935387,333.204461176649));
#28986=CARTESIAN_POINT('Ctrl Pts',(40.3429868096867,-4.62909745059222,333.332852349247));
#28987=CARTESIAN_POINT('Ctrl Pts',(40.3352255547605,-4.67188275273112,333.462894080672));
#28988=CARTESIAN_POINT('Ctrl Pts',(40.3274518843559,-4.71473649740974,333.593143836487));
#28989=CARTESIAN_POINT('Ctrl Pts',(40.3196782139512,-4.75209380270447,333.725049051062));
#28990=CARTESIAN_POINT('Ctrl Pts',(40.3119045435466,-4.78385378603542,333.858104200754));
#28991=CARTESIAN_POINT('Ctrl Pts',(40.3044927393695,-4.81413533450118,333.984965601217));
#28992=CARTESIAN_POINT('Ctrl Pts',(40.2970809351924,-4.83932888878897,334.112872004763));
#28993=CARTESIAN_POINT('Ctrl Pts',(40.2896691310154,-4.85939097442342,334.241381241866));
#28994=CARTESIAN_POINT('Ctrl Pts',(40.2767540041779,-4.89434931579393,334.465309594172));
#28995=CARTESIAN_POINT('Ctrl Pts',(40.2638388773405,-4.91383529265973,334.691713748575));
#28996=CARTESIAN_POINT('Ctrl Pts',(40.2509237505031,-4.91758155532653,334.918915419392));
#28997=CARTESIAN_POINT('Ctrl Pts',(40.2494612498321,-4.91800577970565,334.944643590722));
#28998=CARTESIAN_POINT('Ctrl Pts',(40.2479987491611,-4.91822820671533,334.970381944723));
#28999=CARTESIAN_POINT('Ctrl Pts',(40.2465362484901,-4.91824847584528,334.996128004963));
#29000=CARTESIAN_POINT('',(43.746536248449,-4.91824959557186,335.001994531842));
#29001=CARTESIAN_POINT('Ctrl Pts',(43.746536248449,-4.91824959557186,335.001994531842));
#29002=CARTESIAN_POINT('Ctrl Pts',(43.7381122937764,-4.91818896959446,335.15149010897));
#29003=CARTESIAN_POINT('Ctrl Pts',(43.7296883391039,-4.91130806957054,335.300771189963));
#29004=CARTESIAN_POINT('Ctrl Pts',(43.7212643844313,-4.89769029334711,335.449235854484));
#29005=CARTESIAN_POINT('Ctrl Pts',(43.7128031364178,-4.88401223043045,335.598357780773));
#29006=CARTESIAN_POINT('Ctrl Pts',(43.7043418884044,-4.8635375947404,335.746655781512));
#29007=CARTESIAN_POINT('Ctrl Pts',(43.6958806403909,-4.83640146697991,335.893534505598));
#29008=CARTESIAN_POINT('Ctrl Pts',(43.6874004131535,-4.80920447081761,336.040742689851));
#29009=CARTESIAN_POINT('Ctrl Pts',(43.6789201859162,-4.77531618448029,336.186524973221));
#29010=CARTESIAN_POINT('Ctrl Pts',(43.6704399586788,-4.73492171806959,336.330300487203));
#29011=CARTESIAN_POINT('Ctrl Pts',(43.6619313036429,-4.69439183951448,336.47455797192));
#29012=CARTESIAN_POINT('Ctrl Pts',(43.6534226486069,-4.64731221462689,336.616794965942));
#29013=CARTESIAN_POINT('Ctrl Pts',(43.644913993571,-4.59391736527239,336.756447068246));
#29014=CARTESIAN_POINT('Ctrl Pts',(43.6394511764814,-4.55963623690208,336.846107994424));
#29015=CARTESIAN_POINT('Ctrl Pts',(43.6339883593919,-4.52275290818965,336.934703882329));
#29016=CARTESIAN_POINT('Ctrl Pts',(43.6285255423024,-4.48333932707077,337.022090883427));
#29017=CARTESIAN_POINT('Ctrl Pts',(43.620750463524,-4.42724305053108,337.146466422022));
#29018=CARTESIAN_POINT('Ctrl Pts',(43.6129753847455,-4.36587862266312,337.268702418503));
#29019=CARTESIAN_POINT('Ctrl Pts',(43.6052003059671,-4.29943115870852,337.388320492318));
#29020=CARTESIAN_POINT('Ctrl Pts',(43.5974347949181,-4.23306546258865,337.507791368478));
#29021=CARTESIAN_POINT('Ctrl Pts',(43.5896692838691,-4.16162936403315,337.624650393445));
#29022=CARTESIAN_POINT('Ctrl Pts',(43.5819037728201,-4.08535587087988,337.738439422512));
#29023=CARTESIAN_POINT('Ctrl Pts',(43.5741459612979,-4.00915800311708,337.852115629425));
#29024=CARTESIAN_POINT('Ctrl Pts',(43.5663881497757,-3.92813250187994,337.962727575402));
#29025=CARTESIAN_POINT('Ctrl Pts',(43.5586303382535,-3.84255790991696,338.069842304001));
#29026=CARTESIAN_POINT('Ctrl Pts',(43.5508783647305,-3.75704771554815,338.17687642537));
#29027=CARTESIAN_POINT('Ctrl Pts',(43.5431263912075,-3.66699548742562,338.28041826361));
#29028=CARTESIAN_POINT('Ctrl Pts',(43.5353744176845,-3.57272242695035,338.380064721639));
#29029=CARTESIAN_POINT('Ctrl Pts',(43.5276257271268,-3.47848929117216,338.479668979333));
#29030=CARTESIAN_POINT('Ctrl Pts',(43.5198770365692,-3.38003914637162,338.575380854595));
#29031=CARTESIAN_POINT('Ctrl Pts',(43.5121283460116,-3.27773259059881,338.666831346957));
#29032=CARTESIAN_POINT('Ctrl Pts',(43.5043812676337,-3.17544732055942,338.75826281228));
#29033=CARTESIAN_POINT('Ctrl Pts',(43.4966341892559,-3.06930752673133,338.845434397915));
#29034=CARTESIAN_POINT('Ctrl Pts',(43.4888871108781,-2.95970939048294,338.928015196812));
#29035=CARTESIAN_POINT('Ctrl Pts',(43.4811399675723,-2.8501103356966,339.010596687816));
#29036=CARTESIAN_POINT('Ctrl Pts',(43.4733928242664,-2.73705319285481,339.088587080121));
#29037=CARTESIAN_POINT('Ctrl Pts',(43.4656456809606,-2.62096550144872,339.16169711809));
#29038=CARTESIAN_POINT('Ctrl Pts',(43.4578967959325,-2.50485171106531,339.234823592747));
#29039=CARTESIAN_POINT('Ctrl Pts',(43.4501479109045,-2.38570634702689,339.30306732149));
#29040=CARTESIAN_POINT('Ctrl Pts',(43.4423990258764,-2.26398371973685,339.366183777541));
#29041=CARTESIAN_POINT('Ctrl Pts',(43.4346419161017,-2.14213189479224,339.429367226052));
#29042=CARTESIAN_POINT('Ctrl Pts',(43.4268848063269,-2.01769768965781,339.487412350472));
#29043=CARTESIAN_POINT('Ctrl Pts',(43.4191276965522,-1.89115818335365,339.540121560931));
#29044=CARTESIAN_POINT('Ctrl Pts',(43.411366441626,-1.76455105838336,339.592858937507));
#29045=CARTESIAN_POINT('Ctrl Pts',(43.4036051866998,-1.63583675717992,339.640254583571));
#29046=CARTESIAN_POINT('Ctrl Pts',(43.3958439317737,-1.50550894813942,339.682160384862));
#29047=CARTESIAN_POINT('Ctrl Pts',(43.388070261369,-1.3749726570782,339.724133221778));
#29048=CARTESIAN_POINT('Ctrl Pts',(43.3802965909643,-1.24281807739595,339.760598560937));
#29049=CARTESIAN_POINT('Ctrl Pts',(43.3725229205596,-1.1095514027325,339.791458937233));
#29050=CARTESIAN_POINT('Ctrl Pts',(43.3651111163826,-0.982488323837292,
339.820882755588));
#29051=CARTESIAN_POINT('Ctrl Pts',(43.3576993122056,-0.854414638729723,
339.845211636134));
#29052=CARTESIAN_POINT('Ctrl Pts',(43.3502875080285,-0.725772800545157,
339.864405092556));
#29053=CARTESIAN_POINT('Ctrl Pts',(43.3425124292501,-0.59082584266642,339.884539277453));
#29054=CARTESIAN_POINT('Ctrl Pts',(43.3347373504716,-0.454827172425125,
339.899085532502));
#29055=CARTESIAN_POINT('Ctrl Pts',(43.3269622716932,-0.318279246714153,
339.907940645893));
#29056=CARTESIAN_POINT('Ctrl Pts',(43.3191967606442,-0.181899351918835,
339.916784862503));
#29057=CARTESIAN_POINT('Ctrl Pts',(43.3114312495952,-0.0449719328149411,
339.919951846985));
#29058=CARTESIAN_POINT('Ctrl Pts',(43.3036657385462,0.0919916530273213,
339.91738961221));
#29059=CARTESIAN_POINT('Ctrl Pts',(43.295907927024,0.228819439075556,339.914829917899));
#29060=CARTESIAN_POINT('Ctrl Pts',(43.2881501155018,0.365682932211432,339.906552316185));
#29061=CARTESIAN_POINT('Ctrl Pts',(43.2803923039797,0.502067314663267,339.892556742037));
#29062=CARTESIAN_POINT('Ctrl Pts',(43.2726403304567,0.638349063542123,339.878571700001));
#29063=CARTESIAN_POINT('Ctrl Pts',(43.2648883569337,0.774152032119386,339.858877290094));
#29064=CARTESIAN_POINT('Ctrl Pts',(43.2571363834107,0.908963426949346,339.833525478465));
#29065=CARTESIAN_POINT('Ctrl Pts',(43.2493876928531,1.04371772907356,339.808184403343));
#29066=CARTESIAN_POINT('Ctrl Pts',(43.2416390022954,1.17748090932436,339.777190763889));
#29067=CARTESIAN_POINT('Ctrl Pts',(43.2338903117378,1.30974752703994,339.74064810737));
#29068=CARTESIAN_POINT('Ctrl Pts',(43.22614323336,1.44198662558099,339.704113053857));
#29069=CARTESIAN_POINT('Ctrl Pts',(43.2183961549822,1.57272940440545,339.662031383725));
#29070=CARTESIAN_POINT('Ctrl Pts',(43.2106490766044,1.70148320024599,339.614557181548));
#29071=CARTESIAN_POINT('Ctrl Pts',(43.2029019332986,1.83023807516717,339.567082581493));
#29072=CARTESIAN_POINT('Ctrl Pts',(43.1951547899927,1.95700356711716,339.514215494473));
#29073=CARTESIAN_POINT('Ctrl Pts',(43.1874076466869,2.0813050687093,339.456158914745));
#29074=CARTESIAN_POINT('Ctrl Pts',(43.1796587616589,2.20563451591783,339.398089282666));
#29075=CARTESIAN_POINT('Ctrl Pts',(43.1719098766308,2.32749851637457,339.334828001639));
#29076=CARTESIAN_POINT('Ctrl Pts',(43.1641609916027,2.44644558886834,339.266624783504));
#29077=CARTESIAN_POINT('Ctrl Pts',(43.156403881828,2.56551891301413,339.198349173768));
#29078=CARTESIAN_POINT('Ctrl Pts',(43.1486467720533,2.68166878490923,339.125121343435));
#29079=CARTESIAN_POINT('Ctrl Pts',(43.1408896622786,2.79447087218239,339.047235551216));
#29080=CARTESIAN_POINT('Ctrl Pts',(43.1331284073524,2.9073332372842,338.969308139319));
#29081=CARTESIAN_POINT('Ctrl Pts',(43.1253671524262,3.01684394120711,338.886718041085));
#29082=CARTESIAN_POINT('Ctrl Pts',(43.1176058975001,3.1226112792139,338.799800239674));
#29083=CARTESIAN_POINT('Ctrl Pts',(43.1098322270954,3.22854781049201,338.712743398107));
#29084=CARTESIAN_POINT('Ctrl Pts',(43.1020585566908,3.33072871823893,338.621345280058));
#29085=CARTESIAN_POINT('Ctrl Pts',(43.0942848862861,3.42879811154415,338.525978810596));
#29086=CARTESIAN_POINT('Ctrl Pts',(43.086873082109,3.52230235099808,338.43505167323));
#29087=CARTESIAN_POINT('Ctrl Pts',(43.0794612779318,3.61206904556232,338.340517532343));
#29088=CARTESIAN_POINT('Ctrl Pts',(43.0720494737546,3.69782471265276,338.24272654675));
#29089=CARTESIAN_POINT('Ctrl Pts',(43.0642743949762,3.7877835204393,338.140142533649));
#29090=CARTESIAN_POINT('Ctrl Pts',(43.0564993161978,3.87361246071081,338.03365016371));
#29091=CARTESIAN_POINT('Ctrl Pts',(43.0487242374193,3.95495283219749,337.923616109819));
#29092=CARTESIAN_POINT('Ctrl Pts',(43.0409587263703,4.03619310917867,337.813717459837));
#29093=CARTESIAN_POINT('Ctrl Pts',(43.0331932153213,4.11295557736482,337.700286108918));
#29094=CARTESIAN_POINT('Ctrl Pts',(43.0254277042723,4.18491979474793,337.583723935336));
#29095=CARTESIAN_POINT('Ctrl Pts',(43.0176698927501,4.25681265940003,337.467277333488));
#29096=CARTESIAN_POINT('Ctrl Pts',(43.0099120812278,4.32391653688576,337.347706416999));
#29097=CARTESIAN_POINT('Ctrl Pts',(43.0021542697056,4.38595277508063,337.225444071924));
#29098=CARTESIAN_POINT('Ctrl Pts',(42.9944022961826,4.44794232903888,337.103273733141));
#29099=CARTESIAN_POINT('Ctrl Pts',(42.9866503226596,4.5048716582562,336.97841634437));
#29100=CARTESIAN_POINT('Ctrl Pts',(42.9788983491366,4.55650696021847,336.851331246423));
#29101=CARTESIAN_POINT('Ctrl Pts',(42.971149658579,4.60812039459969,336.72429996909));
#29102=CARTESIAN_POINT('Ctrl Pts',(42.9634009680213,4.65444411412603,336.595043220382));
#29103=CARTESIAN_POINT('Ctrl Pts',(42.9556522774637,4.695291670959,336.4640420715));
#29104=CARTESIAN_POINT('Ctrl Pts',(42.9479051990858,4.7361307291166,336.333068178502));
#29105=CARTESIAN_POINT('Ctrl Pts',(42.940158120708,4.7714957745706,336.20035098016));
#29106=CARTESIAN_POINT('Ctrl Pts',(42.9324110423302,4.80124977196343,336.066388151529));
#29107=CARTESIAN_POINT('Ctrl Pts',(42.9246638990244,4.83100401872342,335.93242420016));
#29108=CARTESIAN_POINT('Ctrl Pts',(42.9169167557186,4.85514703887497,335.797214979257));
#29109=CARTESIAN_POINT('Ctrl Pts',(42.9091696124127,4.87359269732948,335.661269448135));
#29110=CARTESIAN_POINT('Ctrl Pts',(42.9014207273846,4.89204250275962,335.525293353572));
#29111=CARTESIAN_POINT('Ctrl Pts',(42.8936718423565,4.90479234512532,335.388581006637));
#29112=CARTESIAN_POINT('Ctrl Pts',(42.8859229573284,4.91180789005123,335.251647200919));
#29113=CARTESIAN_POINT('Ctrl Pts',(42.8781658475537,4.91883088134902,335.114568052245));
#29114=CARTESIAN_POINT('Ctrl Pts',(42.8704087377789,4.92010739693597,334.977267366215));
#29115=CARTESIAN_POINT('Ctrl Pts',(42.8626516280042,4.91565525464364,334.840261213244));
#29116=CARTESIAN_POINT('Ctrl Pts',(42.854890373078,4.91120073326881,334.703181848565));
#29117=CARTESIAN_POINT('Ctrl Pts',(42.8471291181519,4.90101148329646,334.566397720154));
#29118=CARTESIAN_POINT('Ctrl Pts',(42.8393678632257,4.88515722530405,334.430419499491));
#29119=CARTESIAN_POINT('Ctrl Pts',(42.831594192821,4.86927760566573,334.29422375799));
#29120=CARTESIAN_POINT('Ctrl Pts',(42.8238205224164,4.84771493062566,334.158836886633));
#29121=CARTESIAN_POINT('Ctrl Pts',(42.8160468520117,4.82059020783828,334.02475997283));
#29122=CARTESIAN_POINT('Ctrl Pts',(42.8086350478347,4.79472814742274,333.896924371624));
#29123=CARTESIAN_POINT('Ctrl Pts',(42.8012232436577,4.76381028079485,333.770279795078));
#29124=CARTESIAN_POINT('Ctrl Pts',(42.7938114394807,4.7279830668526,333.645245711557));
#29125=CARTESIAN_POINT('Ctrl Pts',(42.7860363607022,4.69039985443093,333.514083335144));
#29126=CARTESIAN_POINT('Ctrl Pts',(42.7782612819238,4.64729511307846,333.384278816285));
#29127=CARTESIAN_POINT('Ctrl Pts',(42.7704862031454,4.59878307200934,333.256332222268));
#29128=CARTESIAN_POINT('Ctrl Pts',(42.7627206920964,4.55033072809519,333.128543074681));
#29129=CARTESIAN_POINT('Ctrl Pts',(42.7549551810473,4.49648446132126,333.002607664856));
#29130=CARTESIAN_POINT('Ctrl Pts',(42.7471896699983,4.43740881014279,332.879012938708));
#29131=CARTESIAN_POINT('Ctrl Pts',(42.7394318584762,4.37839173264449,332.755540757091));
#29132=CARTESIAN_POINT('Ctrl Pts',(42.7316740469539,4.31415575656308,332.634404991025));
#29133=CARTESIAN_POINT('Ctrl Pts',(42.7239162354317,4.244914110363,332.516074224511));
#29134=CARTESIAN_POINT('Ctrl Pts',(42.7161642619087,4.17572457069747,332.39783250565));
#29135=CARTESIAN_POINT('Ctrl Pts',(42.7084122883858,4.10153705540764,332.282391920797));
#29136=CARTESIAN_POINT('Ctrl Pts',(42.7006603148628,4.02261131002727,332.170197655146));
#29137=CARTESIAN_POINT('Ctrl Pts',(42.6929116243052,3.94371898974692,332.058050903833));
#29138=CARTESIAN_POINT('Ctrl Pts',(42.6851629337476,3.86009265487649,331.949148056333));
#29139=CARTESIAN_POINT('Ctrl Pts',(42.67741424319,3.77203595083023,331.843906235844));
#29140=CARTESIAN_POINT('Ctrl Pts',(42.6696671648122,3.68399756771671,331.738686311795));
#29141=CARTESIAN_POINT('Ctrl Pts',(42.6619200864343,3.5915308995744,331.637126199258));
#29142=CARTESIAN_POINT('Ctrl Pts',(42.6541730080565,3.49498029428049,331.539610454719));
#29143=CARTESIAN_POINT('Ctrl Pts',(42.6464258647507,3.39842887979951,331.442093892904));
#29144=CARTESIAN_POINT('Ctrl Pts',(42.6386787214448,3.29779373490988,331.348622044455));
#29145=CARTESIAN_POINT('Ctrl Pts',(42.630931578139,3.19345624172046,331.259542769297));
#29146=CARTESIAN_POINT('Ctrl Pts',(42.6231826931109,3.08909529124744,331.170443467227));
#29147=CARTESIAN_POINT('Ctrl Pts',(42.6154338080829,2.98103063337027,331.085738957296));
#29148=CARTESIAN_POINT('Ctrl Pts',(42.6076849230548,2.86967658869894,331.005736696364));
#29149=CARTESIAN_POINT('Ctrl Pts',(42.59992781328,2.75820435169409,330.925649520205));
#29150=CARTESIAN_POINT('Ctrl Pts',(42.5921707035053,2.64343607146026,330.850274791492));
#29151=CARTESIAN_POINT('Ctrl Pts',(42.5844135937306,2.52581536487079,330.779876802144));
#29152=CARTESIAN_POINT('Ctrl Pts',(42.5766523388044,2.40813180553642,330.709441194361));
#29153=CARTESIAN_POINT('Ctrl Pts',(42.5688910838783,2.2875931259754,330.643987811486));
#29154=CARTESIAN_POINT('Ctrl Pts',(42.5611298289521,2.16466649053501,330.583734377638));
#29155=CARTESIAN_POINT('Ctrl Pts',(42.5533561585475,2.04154321253977,330.523384557933));
#29156=CARTESIAN_POINT('Ctrl Pts',(42.5455824881428,1.91602470333266,330.468251466804));
#29157=CARTESIAN_POINT('Ctrl Pts',(42.5378088177382,1.78859782219465,330.418504513487));
#29158=CARTESIAN_POINT('Ctrl Pts',(42.530397013561,1.66710269302973,330.371073292814));
#29159=CARTESIAN_POINT('Ctrl Pts',(42.5229852093839,1.54387313506706,330.328538139231));
#29160=CARTESIAN_POINT('Ctrl Pts',(42.5155734052068,1.4193411455178,330.291002890727));
#29161=CARTESIAN_POINT('Ctrl Pts',(42.5077983264283,1.28870547219991,330.251627927883));
#29162=CARTESIAN_POINT('Ctrl Pts',(42.5000232476499,1.1562236341376,330.217630951149));
#29163=CARTESIAN_POINT('Ctrl Pts',(42.4922481688714,1.02237796456516,330.189186517846));
#29164=CARTESIAN_POINT('Ctrl Pts',(42.4844826578224,0.888697000610158,330.16077708723));
#29165=CARTESIAN_POINT('Ctrl Pts',(42.4767171467734,0.753655923124875,330.137906685292));
#29166=CARTESIAN_POINT('Ctrl Pts',(42.4689516357244,0.617753256515989,330.120700462509));
#29167=CARTESIAN_POINT('Ctrl Pts',(42.4611938242022,0.481985337796808,330.103511299746));
#29168=CARTESIAN_POINT('Ctrl Pts',(42.45343601268,0.345357915276657,330.09197518866));
#29169=CARTESIAN_POINT('Ctrl Pts',(42.4456782011578,0.208380421394342,330.086166398576));
#29170=CARTESIAN_POINT('Ctrl Pts',(42.4379262276348,0.071506007420166,330.080361979792));
#29171=CARTESIAN_POINT('Ctrl Pts',(42.4301742541118,-0.0657175646012655,
330.080276319677));
#29172=CARTESIAN_POINT('Ctrl Pts',(42.4224222805888,-0.202775365730806,
330.085931907925));
#29173=CARTESIAN_POINT('Ctrl Pts',(42.4146735900312,-0.339775122800384,
330.091585101027));
#29174=CARTESIAN_POINT('Ctrl Pts',(42.4069248994735,-0.476608858879873,
330.102974690484));
#29175=CARTESIAN_POINT('Ctrl Pts',(42.3991762089159,-0.612761486217139,
330.120071063682));
#29176=CARTESIAN_POINT('Ctrl Pts',(42.3914291305381,-0.748885785863119,
330.137163879838));
#29177=CARTESIAN_POINT('Ctrl Pts',(42.3836820521602,-0.884328871053551,
330.159961069357));
#29178=CARTESIAN_POINT('Ctrl Pts',(42.3759349737824,-1.01858101364081,330.188381168344));
#29179=CARTESIAN_POINT('Ctrl Pts',(42.3681878304766,-1.15283428139015,330.216801505518));
#29180=CARTESIAN_POINT('Ctrl Pts',(42.3604406871708,-1.28589620422812,330.250844765203));
#29181=CARTESIAN_POINT('Ctrl Pts',(42.352693543865,-1.41726787158047,330.290378482013));
#29182=CARTESIAN_POINT('Ctrl Pts',(42.3449446588369,-1.54866907407275,330.329921086842));
#29183=CARTESIAN_POINT('Ctrl Pts',(42.3371957738088,-1.67837889069072,330.374956492442));
#29184=CARTESIAN_POINT('Ctrl Pts',(42.3294468887807,-1.80591456174752,330.425302670321));
#29185=CARTESIAN_POINT('Ctrl Pts',(42.321689779006,-1.93358560048344,330.475702286154));
#29186=CARTESIAN_POINT('Ctrl Pts',(42.3139326692312,-2.05907751974478,330.531423790769));
#29187=CARTESIAN_POINT('Ctrl Pts',(42.3061755594565,-2.18192800427329,330.592237160796));
#29188=CARTESIAN_POINT('Ctrl Pts',(42.2984143045303,-2.30484413617248,330.653083027543));
#29189=CARTESIAN_POINT('Ctrl Pts',(42.2906530496042,-2.42511567823696,330.719025993578));
#29190=CARTESIAN_POINT('Ctrl Pts',(42.2828917946781,-2.5423067321758,330.789791033448));
#29191=CARTESIAN_POINT('Ctrl Pts',(42.2751181242734,-2.65968525360861,330.86066927432));
#29192=CARTESIAN_POINT('Ctrl Pts',(42.2673444538687,-2.77397311373386,330.936384787387));
#29193=CARTESIAN_POINT('Ctrl Pts',(42.259570783464,-2.88476438522012,331.016619839349));
#29194=CARTESIAN_POINT('Ctrl Pts',(42.252158979287,-2.99039829636355,331.093119930339));
#29195=CARTESIAN_POINT('Ctrl Pts',(42.2447471751099,-3.09285359918245,331.173728082346));
#29196=CARTESIAN_POINT('Ctrl Pts',(42.2373353709328,-3.19180919561692,331.258137212393));
#29197=CARTESIAN_POINT('Ctrl Pts',(42.2296717060472,-3.2941274047213,331.345414651262));
#29198=CARTESIAN_POINT('Ctrl Pts',(42.2220080411616,-3.39304721518895,331.437049180769));
#29199=CARTESIAN_POINT('Ctrl Pts',(42.214344376276,-3.48816669397042,331.532742268366));
#29200=CARTESIAN_POINT('Ctrl Pts',(42.2066902036045,-3.58316835778084,331.62831683052));
#29201=CARTESIAN_POINT('Ctrl Pts',(42.199036030933,-3.67437876941371,331.727939671103));
#29202=CARTESIAN_POINT('Ctrl Pts',(42.1913818582615,-3.76142826102061,331.831271469549));
#29203=CARTESIAN_POINT('Ctrl Pts',(42.1837352099999,-3.84839217890307,331.934501688));
#29204=CARTESIAN_POINT('Ctrl Pts',(42.1760885617383,-3.93120305480914,332.041433305814));
#29205=CARTESIAN_POINT('Ctrl Pts',(42.1684419134768,-4.00952774931863,332.151689923842));
#29206=CARTESIAN_POINT('Ctrl Pts',(42.1608009633331,-4.0877940779504,332.26186438101));
#29207=CARTESIAN_POINT('Ctrl Pts',(42.1531600131894,-4.16158064466773,332.375358580815));
#29208=CARTESIAN_POINT('Ctrl Pts',(42.1455190630456,-4.23059468085973,332.491763227129));
#29209=CARTESIAN_POINT('Ctrl Pts',(42.1378811123916,-4.29958162527869,332.608122178271));
#29210=CARTESIAN_POINT('Ctrl Pts',(42.1302431617375,-4.36379955897432,332.727388958204));
#29211=CARTESIAN_POINT('Ctrl Pts',(42.1226052110834,-4.4229993518083,332.849125806468));
#29212=CARTESIAN_POINT('Ctrl Pts',(42.1149684949439,-4.48218957623682,332.970842978522));
#29213=CARTESIAN_POINT('Ctrl Pts',(42.1073317788044,-4.53636309716481,333.095029062353));
#29214=CARTESIAN_POINT('Ctrl Pts',(42.0996950626649,-4.58531728162552,333.221222754439));
#29215=CARTESIAN_POINT('Ctrl Pts',(42.0920578173362,-4.63427485838587,333.347425191167));
#29216=CARTESIAN_POINT('Ctrl Pts',(42.0844205720074,-4.67801223514881,333.47563513653));
#29217=CARTESIAN_POINT('Ctrl Pts',(42.0767833266787,-4.71637556484622,333.605372955295));
#29218=CARTESIAN_POINT('Ctrl Pts',(42.0691402362242,-4.75476825571721,333.735210068221));
#29219=CARTESIAN_POINT('Ctrl Pts',(42.0614971457696,-4.78777857274076,333.866577002474));
#29220=CARTESIAN_POINT('Ctrl Pts',(42.0538540553152,-4.81530301176027,333.998980535937));
#29221=CARTESIAN_POINT('Ctrl Pts',(42.0462076894455,-4.84283924626572,334.131440810394));
#29222=CARTESIAN_POINT('Ctrl Pts',(42.0385613235758,-4.86488485507018,334.264938171483));
#29223=CARTESIAN_POINT('Ctrl Pts',(42.0309149577061,-4.88138798731653,334.39897223044));
#29224=CARTESIAN_POINT('Ctrl Pts',(42.0232593186771,-4.89791113379928,334.533168839713));
#29225=CARTESIAN_POINT('Ctrl Pts',(42.0156036796482,-4.90887835139367,334.667903045344));
#29226=CARTESIAN_POINT('Ctrl Pts',(42.0079480406192,-4.91428985496865,334.802672141216));
#29227=CARTESIAN_POINT('Ctrl Pts',(42.0041441099211,-4.91697872058704,334.869636152843));
#29228=CARTESIAN_POINT('Ctrl Pts',(42.000340179223,-4.918296749457,334.936608808896));
#29229=CARTESIAN_POINT('Ctrl Pts',(41.9965362485248,-4.91824873401151,335.003528865855));
#29230=CARTESIAN_POINT('',(45.4965362485242,-4.91824806876705,334.995641494621));
#29231=CARTESIAN_POINT('Ctrl Pts',(45.4965362484901,-4.91824806876759,334.995641495223));
#29232=CARTESIAN_POINT('Ctrl Pts',(45.4888448922254,-4.91836861593767,335.131669999676));
#29233=CARTESIAN_POINT('Ctrl Pts',(45.4811535359606,-4.91284152150253,335.267811737524));
#29234=CARTESIAN_POINT('Ctrl Pts',(45.4734621796958,-4.90166545359971,335.403557732533));
#29235=CARTESIAN_POINT('Ctrl Pts',(45.4657736941497,-4.89049355704787,335.539253061763));
#29236=CARTESIAN_POINT('Ctrl Pts',(45.4580852086035,-4.87367691054027,335.674552546379));
#29237=CARTESIAN_POINT('Ctrl Pts',(45.4503967230574,-4.85126624931149,335.808949220156));
#29238=CARTESIAN_POINT('Ctrl Pts',(45.4427095113432,-4.82885930109164,335.943323627029));
#29239=CARTESIAN_POINT('Ctrl Pts',(45.435022299629,-4.80086024643141,336.07679512861));
#29240=CARTESIAN_POINT('Ctrl Pts',(45.4273350879148,-4.76737138886389,336.208864385753));
#29241=CARTESIAN_POINT('Ctrl Pts',(45.4196474224994,-4.7338805547756,336.340941437657));
#29242=CARTESIAN_POINT('Ctrl Pts',(45.411959757084,-4.69489937097439,336.471615695214));
#29243=CARTESIAN_POINT('Ctrl Pts',(45.4042720916686,-4.65058059448133,336.600400948742));
#29244=CARTESIAN_POINT('Ctrl Pts',(45.3965822449971,-4.60624924322079,336.729222743094));
#29245=CARTESIAN_POINT('Ctrl Pts',(45.3888923983255,-4.5565774161553,336.856154091651));
#29246=CARTESIAN_POINT('Ctrl Pts',(45.381202551654,-4.50176660731064,336.980727259317));
#29247=CARTESIAN_POINT('Ctrl Pts',(45.3735042940699,-4.44689584812681,337.105436681197));
#29248=CARTESIAN_POINT('Ctrl Pts',(45.3658060364859,-4.38687504434181,337.227782408036));
#29249=CARTESIAN_POINT('Ctrl Pts',(45.3581077789019,-4.32195257877653,337.347319528591));
#29250=CARTESIAN_POINT('Ctrl Pts',(45.3504048901709,-4.25699105690859,337.46692856074));
#29251=CARTESIAN_POINT('Ctrl Pts',(45.3427020014398,-4.18712220483497,337.583725281629));
#29252=CARTESIAN_POINT('Ctrl Pts',(45.3349991127089,-4.1126379799387,337.697293441297));
#29253=CARTESIAN_POINT('Ctrl Pts',(45.327284537618,-4.03804075205248,337.811033899753));
#29254=CARTESIAN_POINT('Ctrl Pts',(45.3195699625271,-3.95881440009591,337.9215356939));
#29255=CARTESIAN_POINT('Ctrl Pts',(45.3118553874362,-3.87529174763549,338.028414920913));
#29256=CARTESIAN_POINT('Ctrl Pts',(45.3072215076062,-3.82512256397624,338.092613595301));
#29257=CARTESIAN_POINT('Ctrl Pts',(45.3025876277762,-3.77340402202431,338.155505931274));
#29258=CARTESIAN_POINT('Ctrl Pts',(45.2979537479462,-3.72021445435332,338.217015305547));
#29259=CARTESIAN_POINT('Ctrl Pts',(45.2901786691677,-3.63096892058864,338.320220448564));
#29260=CARTESIAN_POINT('Ctrl Pts',(45.2824035903893,-3.53728447553205,338.419872124906));
#29261=CARTESIAN_POINT('Ctrl Pts',(45.2746285116109,-3.43947500843542,338.515564638696));
#29262=CARTESIAN_POINT('Ctrl Pts',(45.2668630005619,-3.34178590211491,338.611139396755));
#29263=CARTESIAN_POINT('Ctrl Pts',(45.2590974895128,-3.23998215046829,338.702764415412));
#29264=CARTESIAN_POINT('Ctrl Pts',(45.2513319784638,-3.13441777271877,338.790067055946));
#29265=CARTESIAN_POINT('Ctrl Pts',(45.2435741669416,-3.0289580623572,338.877283135657));
#29266=CARTESIAN_POINT('Ctrl Pts',(45.2358163554194,-2.91974544543276,338.960185118432));
#29267=CARTESIAN_POINT('Ctrl Pts',(45.2280585438972,-2.80717039866113,339.038437496778));
#29268=CARTESIAN_POINT('Ctrl Pts',(45.2203065703742,-2.69468006818201,339.116630987728));
#29269=CARTESIAN_POINT('Ctrl Pts',(45.2125545968513,-2.57883266402352,339.190181616588));
#29270=CARTESIAN_POINT('Ctrl Pts',(45.2048026233282,-2.46005103114451,339.258794663595));
#29271=CARTESIAN_POINT('Ctrl Pts',(45.1970539327706,-2.3413197023577,339.327378652935));
#29272=CARTESIAN_POINT('Ctrl Pts',(45.189305242213,-2.21965695414906,339.391029024307));
#29273=CARTESIAN_POINT('Ctrl Pts',(45.1815565516554,-2.09551366451193,339.449494976325));
#29274=CARTESIAN_POINT('Ctrl Pts',(45.1738094732776,-1.97139620392307,339.507948764014));
#29275=CARTESIAN_POINT('Ctrl Pts',(45.1660623948997,-1.84479958185818,339.56122011145));
#29276=CARTESIAN_POINT('Ctrl Pts',(45.1583153165219,-1.71619791431085,339.609104878544));
#29277=CARTESIAN_POINT('Ctrl Pts',(45.150568173216,-1.58759516895751,339.656990046958));
#29278=CARTESIAN_POINT('Ctrl Pts',(45.1428210299102,-1.45698771090967,339.699488408594));
#29279=CARTESIAN_POINT('Ctrl Pts',(45.1350738866044,-1.32486782955475,339.736444689502));
#29280=CARTESIAN_POINT('Ctrl Pts',(45.1273250015763,-1.19271824484533,339.773409278967));
#29281=CARTESIAN_POINT('Ctrl Pts',(45.1195761165482,-1.05905593656923,339.804829203077));
#29282=CARTESIAN_POINT('Ctrl Pts',(45.1118272315201,-0.924386093011183,
339.830599695022));
#29283=CARTESIAN_POINT('Ctrl Pts',(45.1040701217454,-0.789573309490155,
339.856397540034));
#29284=CARTESIAN_POINT('Ctrl Pts',(45.0963130119706,-0.653751238958404,
339.876533900998));
#29285=CARTESIAN_POINT('Ctrl Pts',(45.0885559021959,-0.517433502723694,
339.890955492821));
#29286=CARTESIAN_POINT('Ctrl Pts',(45.0807946472698,-0.381042922649615,
339.905384791082));
#29287=CARTESIAN_POINT('Ctrl Pts',(45.0730333923436,-0.244156538987243,
339.914093210447));
#29288=CARTESIAN_POINT('Ctrl Pts',(45.0652721374175,-0.107289759377202,
339.917079618029));
#29289=CARTESIAN_POINT('Ctrl Pts',(45.0574984670128,0.0297959624756219,
339.920070802889));
#29290=CARTESIAN_POINT('Ctrl Pts',(45.0497247966082,0.166861626608122,339.917321692697));
#29291=CARTESIAN_POINT('Ctrl Pts',(45.0419511262035,0.303394269079817,339.90888327219));
#29292=CARTESIAN_POINT('Ctrl Pts',(45.0345393220264,0.433571284197149,339.900837662188));
#29293=CARTESIAN_POINT('Ctrl Pts',(45.0271275178493,0.563263498892685,339.88762052584));
#29294=CARTESIAN_POINT('Ctrl Pts',(45.0197157136722,0.692035295334352,339.869319276091));
#29295=CARTESIAN_POINT('Ctrl Pts',(45.0119406348937,0.827118581110721,339.850121027575));
#29296=CARTESIAN_POINT('Ctrl Pts',(45.0041655561153,0.961615830554773,339.825267019137));
#29297=CARTESIAN_POINT('Ctrl Pts',(44.9963904773368,1.09501602186309,339.794801661629));
#29298=CARTESIAN_POINT('Ctrl Pts',(44.9886249662878,1.22825205574351,339.764373793683));
#29299=CARTESIAN_POINT('Ctrl Pts',(44.9808594552388,1.36039334018034,339.728348402073));
#29300=CARTESIAN_POINT('Ctrl Pts',(44.9730939441898,1.49093493520868,339.686821532923));
#29301=CARTESIAN_POINT('Ctrl Pts',(44.9653361326676,1.62134709786523,339.645335837785));
#29302=CARTESIAN_POINT('Ctrl Pts',(44.9575783211453,1.75016235745318,339.598359638059));
#29303=CARTESIAN_POINT('Ctrl Pts',(44.9498205096232,1.87688726920886,339.546039731589));
#29304=CARTESIAN_POINT('Ctrl Pts',(44.9420685361002,2.0035168164496,339.493759197507));
#29305=CARTESIAN_POINT('Ctrl Pts',(44.9343165625772,2.12805878710484,339.436143109465));
#29306=CARTESIAN_POINT('Ctrl Pts',(44.9265645890542,2.25003651936725,339.373387557033));
#29307=CARTESIAN_POINT('Ctrl Pts',(44.9188158984965,2.37196259398778,339.310658581615));
#29308=CARTESIAN_POINT('Ctrl Pts',(44.9110672079389,2.49132624325801,339.242794649292));
#29309=CARTESIAN_POINT('Ctrl Pts',(44.9033185173813,2.60767256698994,339.170039189968));
#29310=CARTESIAN_POINT('Ctrl Pts',(44.8955714390034,2.72399468389747,339.097298868025));
#29311=CARTESIAN_POINT('Ctrl Pts',(44.8878243606256,2.83730039276237,339.019669250516));
#29312=CARTESIAN_POINT('Ctrl Pts',(44.8800772822478,2.94716145646065,338.937438559781));
#29313=CARTESIAN_POINT('Ctrl Pts',(44.8723301389419,3.05702344090061,338.855207179874));
#29314=CARTESIAN_POINT('Ctrl Pts',(44.8645829956361,3.16344040966663,338.76837488405));
#29315=CARTESIAN_POINT('Ctrl Pts',(44.8568358523303,3.2660153835485,338.677271621314));
#29316=CARTESIAN_POINT('Ctrl Pts',(44.8490869673022,3.3686134184618,338.586147876632));
#29317=CARTESIAN_POINT('Ctrl Pts',(44.8413380822742,3.4673674475097,338.490751513853));
#29318=CARTESIAN_POINT('Ctrl Pts',(44.8335891972461,3.56191598367893,338.391450661253));
#29319=CARTESIAN_POINT('Ctrl Pts',(44.8258320874714,3.65656487464145,338.292044409701));
#29320=CARTESIAN_POINT('Ctrl Pts',(44.8180749776966,3.74699908599997,338.188725673296));
#29321=CARTESIAN_POINT('Ctrl Pts',(44.8103178679219,3.83289585922195,338.081897531531));
#29322=CARTESIAN_POINT('Ctrl Pts',(44.8025566129957,3.91883853293328,337.975012304223));
#29323=CARTESIAN_POINT('Ctrl Pts',(44.7947953580695,4.00023870530215,337.864614249265));
#29324=CARTESIAN_POINT('Ctrl Pts',(44.7870341031434,4.0768165070112,337.751136170869));
#29325=CARTESIAN_POINT('Ctrl Pts',(44.7792604327387,4.15351680824623,337.637476564529));
#29326=CARTESIAN_POINT('Ctrl Pts',(44.771486762334,4.225379118524,337.520727422123));
#29327=CARTESIAN_POINT('Ctrl Pts',(44.7637130919293,4.29216871777705,337.401347696739));
#29328=CARTESIAN_POINT('Ctrl Pts',(44.7563012877523,4.35584924511586,337.287525126294));
#29329=CARTESIAN_POINT('Ctrl Pts',(44.7488894835753,4.41491857229445,337.171311625219));
#29330=CARTESIAN_POINT('Ctrl Pts',(44.7414776793982,4.46921446891838,337.053120818001));
#29331=CARTESIAN_POINT('Ctrl Pts',(44.7337026006198,4.52617156917527,336.929137127249));
#29332=CARTESIAN_POINT('Ctrl Pts',(44.7259275218414,4.5780554823679,336.802585590731));
#29333=CARTESIAN_POINT('Ctrl Pts',(44.718152443063,4.62462701130763,336.673919970842));
#29334=CARTESIAN_POINT('Ctrl Pts',(44.710386932014,4.67114123101611,336.54541268219));
#29335=CARTESIAN_POINT('Ctrl Pts',(44.7026214209649,4.71235594191723,336.41479685046));
#29336=CARTESIAN_POINT('Ctrl Pts',(44.6948559099159,4.74807865925728,336.28254906651));
#29337=CARTESIAN_POINT('Ctrl Pts',(44.6870980983937,4.78376595741905,336.150432406623));
#29338=CARTESIAN_POINT('Ctrl Pts',(44.6793402868716,4.81397199725656,336.016687389517));
#29339=CARTESIAN_POINT('Ctrl Pts',(44.6715824753494,4.83855319293455,335.881808404158));
#29340=CARTESIAN_POINT('Ctrl Pts',(44.6638305018264,4.86311589048326,335.747030919512));
#29341=CARTESIAN_POINT('Ctrl Pts',(44.6560785283034,4.88206209940156,335.611121548152));
#29342=CARTESIAN_POINT('Ctrl Pts',(44.6483265547804,4.89529876653869,335.474587240478));
#29343=CARTESIAN_POINT('Ctrl Pts',(44.6405778642228,4.90852982793945,335.338110755165));
#29344=CARTESIAN_POINT('Ctrl Pts',(44.6328291736652,4.91605611914042,335.20101024817));
#29345=CARTESIAN_POINT('Ctrl Pts',(44.6250804831076,4.91783617294715,335.063799988657));
#29346=CARTESIAN_POINT('Ctrl Pts',(44.6173334047297,4.91961585639881,334.926618276883));
#29347=CARTESIAN_POINT('Ctrl Pts',(44.6095863263519,4.91565167542782,334.789327248607));
#29348=CARTESIAN_POINT('Ctrl Pts',(44.6018392479741,4.90595425866768,334.652442991208));
#29349=CARTESIAN_POINT('Ctrl Pts',(44.5940921046683,4.89625676063386,334.515557586587));
#29350=CARTESIAN_POINT('Ctrl Pts',(44.5863449613624,4.88082595859335,334.379079349539));
#29351=CARTESIAN_POINT('Ctrl Pts',(44.5785978180566,4.85972448547493,334.243520662691));
#29352=CARTESIAN_POINT('Ctrl Pts',(44.5708489330285,4.83861826829729,334.107931499372));
#29353=CARTESIAN_POINT('Ctrl Pts',(44.5631000480004,4.81183890326738,333.973262683779));
#29354=CARTESIAN_POINT('Ctrl Pts',(44.5553511629723,4.77950033593997,333.840017413385));
#29355=CARTESIAN_POINT('Ctrl Pts',(44.5475940531976,4.74712744412307,333.706630715085));
#29356=CARTESIAN_POINT('Ctrl Pts',(44.5398369434229,4.70918365535144,333.574670960727));
#29357=CARTESIAN_POINT('Ctrl Pts',(44.5320798336481,4.66583326460921,333.444627694291));
#29358=CARTESIAN_POINT('Ctrl Pts',(44.524318578722,4.62245970880426,333.314514936891));
#29359=CARTESIAN_POINT('Ctrl Pts',(44.5165573237958,4.57367393316091,333.186321073173));
#29360=CARTESIAN_POINT('Ctrl Pts',(44.5087960688696,4.51968843862668,333.060515666409));
#29361=CARTESIAN_POINT('Ctrl Pts',(44.5010223984649,4.46561658489511,332.934509011994));
#29362=CARTESIAN_POINT('Ctrl Pts',(44.4932487280603,4.40632855986221,332.810898802147));
#29363=CARTESIAN_POINT('Ctrl Pts',(44.4854750576557,4.34208328647498,332.690130783829));
#29364=CARTESIAN_POINT('Ctrl Pts',(44.4780632534785,4.28082864602001,332.574984545818));
#29365=CARTESIAN_POINT('Ctrl Pts',(44.4706514493014,4.21506803599211,332.462422094642));
#29366=CARTESIAN_POINT('Ctrl Pts',(44.4632396451243,4.14506148987295,332.352803689245));
#29367=CARTESIAN_POINT('Ctrl Pts',(44.4554645663458,4.07162371439012,332.237812559264));
#29368=CARTESIAN_POINT('Ctrl Pts',(44.4476894875674,3.99328118999983,332.12569797183));
#29369=CARTESIAN_POINT('Ctrl Pts',(44.4399144087889,3.91028605185769,332.016906629831));
#29370=CARTESIAN_POINT('Ctrl Pts',(44.4321488977399,3.82739304451675,331.908249162504));
#29371=CARTESIAN_POINT('Ctrl Pts',(44.4243833866909,3.73985905001655,331.802907111546));
#29372=CARTESIAN_POINT('Ctrl Pts',(44.4166178756419,3.64798067923199,331.701300252152));
#29373=CARTESIAN_POINT('Ctrl Pts',(44.4088600641197,3.55619340611961,331.599794136256));
#29374=CARTESIAN_POINT('Ctrl Pts',(44.4011022525975,3.46007058928822,331.502016129895));
#29375=CARTESIAN_POINT('Ctrl Pts',(44.3933444410753,3.35995026843267,331.4083545197));
#29376=CARTESIAN_POINT('Ctrl Pts',(44.3855924675523,3.25990529129357,331.314763392837));
#29377=CARTESIAN_POINT('Ctrl Pts',(44.3778404940293,3.15586908219602,331.225282762237));
#29378=CARTESIAN_POINT('Ctrl Pts',(44.3700885205063,3.04821759014883,331.14026521823));
#29379=CARTESIAN_POINT('Ctrl Pts',(44.3623398299486,2.94061168857243,331.055283679203));
#29380=CARTESIAN_POINT('Ctrl Pts',(44.354591139391,2.82939385535681,330.974761709206));
#29381=CARTESIAN_POINT('Ctrl Pts',(44.3468424488334,2.71497411013338,330.899012479438));
#29382=CARTESIAN_POINT('Ctrl Pts',(44.3390953704555,2.60057817089359,330.82327900993));
#29383=CARTESIAN_POINT('Ctrl Pts',(44.3313482920777,2.48298197045246,330.752316521123));
#29384=CARTESIAN_POINT('Ctrl Pts',(44.3236012136999,2.36262524946094,330.686395359666));
#29385=CARTESIAN_POINT('Ctrl Pts',(44.315854070394,2.24226751976384,330.620473645726));
#29386=CARTESIAN_POINT('Ctrl Pts',(44.3081069270882,2.11914956619075,330.559593531177));
#29387=CARTESIAN_POINT('Ctrl Pts',(44.3003597837824,1.99373615649516,330.503979626294));
#29388=CARTESIAN_POINT('Ctrl Pts',(44.2926108987543,1.86829455120333,330.448353218223));
#29389=CARTESIAN_POINT('Ctrl Pts',(44.2848620137263,1.7405568201209,330.397995534178));
#29390=CARTESIAN_POINT('Ctrl Pts',(44.2771131286982,1.6110077752169,330.353083063935));
#29391=CARTESIAN_POINT('Ctrl Pts',(44.2693560189235,1.48132122561779,330.308122923132));
#29392=CARTESIAN_POINT('Ctrl Pts',(44.2615989091487,1.3498198916223,330.268619669673));
#29393=CARTESIAN_POINT('Ctrl Pts',(44.253841799374,1.21700435064926,330.234700064739));
#29394=CARTESIAN_POINT('Ctrl Pts',(44.2460805444478,1.08411783729764,330.200762334252));
#29395=CARTESIAN_POINT('Ctrl Pts',(44.2383192895217,0.949916099873101,330.172414278369));
#29396=CARTESIAN_POINT('Ctrl Pts',(44.2305580345955,0.814909000605078,330.14973130814));
#29397=CARTESIAN_POINT('Ctrl Pts',(44.2227843641909,0.679685933976937,330.127012052552));
#29398=CARTESIAN_POINT('Ctrl Pts',(44.2150106937862,0.543655319116055,330.109976040355));
#29399=CARTESIAN_POINT('Ctrl Pts',(44.2072370233815,0.407332112217123,330.098646756981));
#29400=CARTESIAN_POINT('Ctrl Pts',(44.1998252192045,0.277354783397359,330.087844854473));
#29401=CARTESIAN_POINT('Ctrl Pts',(44.1924134150274,0.14711177736114,330.082230353223));
#29402=CARTESIAN_POINT('Ctrl Pts',(44.1850016108504,0.0170467625781974,
330.081779542316));
#29403=CARTESIAN_POINT('Ctrl Pts',(44.1772265320719,-0.119393126023619,
330.081306635823));
#29404=CARTESIAN_POINT('Ctrl Pts',(44.1694514532935,-0.256068309697689,
330.086514899553));
#29405=CARTESIAN_POINT('Ctrl Pts',(44.161676374515,-0.392466701654937,330.097434044238));
#29406=CARTESIAN_POINT('Ctrl Pts',(44.153910863466,-0.52869724670715,330.108339752222));
#29407=CARTESIAN_POINT('Ctrl Pts',(44.146145352417,-0.664651291855306,330.124942327354));
#29408=CARTESIAN_POINT('Ctrl Pts',(44.138379841368,-0.799815326017855,330.147219507667));
#29409=CARTESIAN_POINT('Ctrl Pts',(44.1306220298458,-0.934845344647104,
330.169474600092));
#29410=CARTESIAN_POINT('Ctrl Pts',(44.1228642183236,-1.06908652791168,330.197393037713));
#29411=CARTESIAN_POINT('Ctrl Pts',(44.1151064068014,-1.20202942462513,330.230900679915));
#29412=CARTESIAN_POINT('Ctrl Pts',(44.1073544332784,-1.33487227759277,330.264383106554));
#29413=CARTESIAN_POINT('Ctrl Pts',(44.0996024597554,-1.4664184111891,330.303446270684));
#29414=CARTESIAN_POINT('Ctrl Pts',(44.0918504862323,-1.59616787710212,330.347964835622));
#29415=CARTESIAN_POINT('Ctrl Pts',(44.0841017956747,-1.72586239403947,330.392464546922));
#29416=CARTESIAN_POINT('Ctrl Pts',(44.0763531051172,-1.85376138770215,330.442414937286));
#29417=CARTESIAN_POINT('Ctrl Pts',(44.0686044145595,-1.97937962059679,330.497640687366));
#29418=CARTESIAN_POINT('Ctrl Pts',(44.0608573361817,-2.10497171756873,330.552854947266));
#29419=CARTESIAN_POINT('Ctrl Pts',(44.0531102578039,-2.22828364005197,330.613342226502));
#29420=CARTESIAN_POINT('Ctrl Pts',(44.045363179426,-2.34885007888299,330.678879037862));
#29421=CARTESIAN_POINT('Ctrl Pts',(44.0376160361202,-2.46941752817672,330.744416398483));
#29422=CARTESIAN_POINT('Ctrl Pts',(44.0298688928144,-2.58723910450557,330.815003188966));
#29423=CARTESIAN_POINT('Ctrl Pts',(44.0221217495086,-2.70187441579872,330.890370125698));
#29424=CARTESIAN_POINT('Ctrl Pts',(44.0143728644805,-2.8165354995441,330.965754006519));
#29425=CARTESIAN_POINT('Ctrl Pts',(44.0066239794524,-2.92800856627114,331.045919957391));
#29426=CARTESIAN_POINT('Ctrl Pts',(43.9988750944243,-3.03588284238472,331.130555798333));
#29427=CARTESIAN_POINT('Ctrl Pts',(43.9911179846496,-3.14387161736908,331.215281472631));
#29428=CARTESIAN_POINT('Ctrl Pts',(43.9833608748749,-3.24825366333711,331.304486272703));
#29429=CARTESIAN_POINT('Ctrl Pts',(43.9756037651002,-3.34865149294404,331.397817850066));
#29430=CARTESIAN_POINT('Ctrl Pts',(43.967842510174,-3.44910297194108,331.49119930084));
#29431=CARTESIAN_POINT('Ctrl Pts',(43.9600812552479,-3.54556571752651,331.588711645259));
#29432=CARTESIAN_POINT('Ctrl Pts',(43.9523200003217,-3.63770039923142,331.689966938544));
#29433=CARTESIAN_POINT('Ctrl Pts',(43.944546329917,-3.72998246640044,331.791384207299));
#29434=CARTESIAN_POINT('Ctrl Pts',(43.9367726595124,-3.81792238363982,331.896556089696));
#29435=CARTESIAN_POINT('Ctrl Pts',(43.9289989891077,-3.90122172920631,332.005062257397));
#29436=CARTESIAN_POINT('Ctrl Pts',(43.9215871849306,-3.98064347019634,332.108517436887));
#29437=CARTESIAN_POINT('Ctrl Pts',(43.9141753807535,-4.05584678798625,332.21500323049));
#29438=CARTESIAN_POINT('Ctrl Pts',(43.9067635765764,-4.12661152712434,332.324133716587));
#29439=CARTESIAN_POINT('Ctrl Pts',(43.89881824557,-4.20247015244647,332.441119785595));
#29440=CARTESIAN_POINT('Ctrl Pts',(43.8908729145636,-4.27345962110023,332.561502301101));
#29441=CARTESIAN_POINT('Ctrl Pts',(43.8829275835573,-4.33926899970426,332.684848253201));
#29442=CARTESIAN_POINT('Ctrl Pts',(43.8749932764454,-4.40498706988476,332.808023066709));
#29443=CARTESIAN_POINT('Ctrl Pts',(43.8670589693336,-4.46553918750092,332.934152809086));
#29444=CARTESIAN_POINT('Ctrl Pts',(43.8591246622217,-4.5206574553238,333.062775378505));
#29445=CARTESIAN_POINT('Ctrl Pts',(43.8511999370428,-4.57570915910553,333.191242615793));
#29446=CARTESIAN_POINT('Ctrl Pts',(43.8432752118639,-4.62533993597997,333.322196349463));
#29447=CARTESIAN_POINT('Ctrl Pts',(43.8353504866849,-4.66932768418344,333.455149832437));
#29448=CARTESIAN_POINT('Ctrl Pts',(43.8274359625603,-4.71325880942557,333.58793217185));
#29449=CARTESIAN_POINT('Ctrl Pts',(43.8195214384357,-4.7515612687418,333.722708782192));
#29450=CARTESIAN_POINT('Ctrl Pts',(43.811606914311,-4.78406117279454,333.858973375657));
#29451=CARTESIAN_POINT('Ctrl Pts',(43.8036983779828,-4.81653648878549,333.995134877056));
#29452=CARTESIAN_POINT('Ctrl Pts',(43.7957898416545,-4.84321790503991,334.13278176346));
#29453=CARTESIAN_POINT('Ctrl Pts',(43.7878813053263,-4.86398132358368,334.271392597945));
#29454=CARTESIAN_POINT('Ctrl Pts',(43.7799779889375,-4.88473103746923,334.409911943925));
#29455=CARTESIAN_POINT('Ctrl Pts',(43.7720746725487,-4.89957048181482,334.549393607077));
#29456=CARTESIAN_POINT('Ctrl Pts',(43.7641713561599,-4.90842667497265,334.689306197492));
#29457=CARTESIAN_POINT('Ctrl Pts',(43.7582929869366,-4.91501377976932,334.793371102018));
#29458=CARTESIAN_POINT('Ctrl Pts',(43.7524146177133,-4.9182919013256,334.897674145527));
#29459=CARTESIAN_POINT('Ctrl Pts',(43.7465362484901,-4.91824959557215,335.001994531113));
#29460=CARTESIAN_POINT('',(47.246536248526,-4.91824999896793,335.000100756667));
#29461=CARTESIAN_POINT('Ctrl Pts',(47.2465362484901,-4.91824999896792,335.000100757296));
#29462=CARTESIAN_POINT('Ctrl Pts',(47.2462308282813,-4.91824988916758,335.005460423983));
#29463=CARTESIAN_POINT('Ctrl Pts',(47.2459254080725,-4.9182410183197,335.010820080069));
#29464=CARTESIAN_POINT('Ctrl Pts',(47.2456199878637,-4.91822338650565,335.016179707317));
#29465=CARTESIAN_POINT('Ctrl Pts',(47.2378449090853,-4.91777453361609,335.152619677169));
#29466=CARTESIAN_POINT('Ctrl Pts',(47.2300698303068,-4.91164305056294,335.289256556375));
#29467=CARTESIAN_POINT('Ctrl Pts',(47.2222947515284,-4.89980268680175,335.425578069113));
#29468=CARTESIAN_POINT('Ctrl Pts',(47.2145292404793,-4.88797689336197,335.561731829552));
#29469=CARTESIAN_POINT('Ctrl Pts',(47.2067637294303,-4.87045623072988,335.697570610002));
#29470=CARTESIAN_POINT('Ctrl Pts',(47.1989982183813,-4.84726642949793,335.832581061496));
#29471=CARTESIAN_POINT('Ctrl Pts',(47.1912404068591,-4.82409962102142,335.967457649735));
#29472=CARTESIAN_POINT('Ctrl Pts',(47.1834825953368,-4.79527492573058,336.101507160681));
#29473=CARTESIAN_POINT('Ctrl Pts',(47.1757247838146,-4.76086992425483,336.234220655647));
#29474=CARTESIAN_POINT('Ctrl Pts',(47.1679728102916,-4.7264908136338,336.366834279499));
#29475=CARTESIAN_POINT('Ctrl Pts',(47.1602208367686,-4.68653985313726,336.498113511716));
#29476=CARTESIAN_POINT('Ctrl Pts',(47.1524688632456,-4.64114575409418,336.627559262133));
#29477=CARTESIAN_POINT('Ctrl Pts',(47.1447201726879,-4.59577087947888,336.756950192198));
#29478=CARTESIAN_POINT('Ctrl Pts',(47.1369714821304,-4.54495758022238,336.884508816744));
#29479=CARTESIAN_POINT('Ctrl Pts',(47.1292227915727,-4.4888844497976,337.009751093759));
#29480=CARTESIAN_POINT('Ctrl Pts',(47.1214757131949,-4.43282298585593,337.134967313072));
#29481=CARTESIAN_POINT('Ctrl Pts',(47.113728634817,-4.37150402711232,337.25786778693));
#29482=CARTESIAN_POINT('Ctrl Pts',(47.1059815564392,-4.30515419917185,337.377988726603));
#29483=CARTESIAN_POINT('Ctrl Pts',(47.0982344131333,-4.23880381515596,337.498110673006));
#29484=CARTESIAN_POINT('Ctrl Pts',(47.0904872698275,-4.16742266683379,337.615452696611));
#29485=CARTESIAN_POINT('Ctrl Pts',(47.0827401265217,-4.09128300683433,337.729576234599));
#29486=CARTESIAN_POINT('Ctrl Pts',(47.0749912414936,-4.01512622902287,337.843725429982));
#29487=CARTESIAN_POINT('Ctrl Pts',(47.0672423564654,-3.93420902761155,337.954654374809));
#29488=CARTESIAN_POINT('Ctrl Pts',(47.0594934714373,-3.84884635052599,338.061954413858));
#29489=CARTESIAN_POINT('Ctrl Pts',(47.0517363616626,-3.7633930686129,338.169368342277));
#29490=CARTESIAN_POINT('Ctrl Pts',(47.0439792518879,-3.67348512916239,338.273145364301));
#29491=CARTESIAN_POINT('Ctrl Pts',(47.0362221421131,-3.57947742281258,338.372910381566));
#29492=CARTESIAN_POINT('Ctrl Pts',(47.0284608871869,-3.48541948175034,338.472728710066));
#29493=CARTESIAN_POINT('Ctrl Pts',(47.0206996322608,-3.38725768804384,338.56853048905));
#29494=CARTESIAN_POINT('Ctrl Pts',(47.0129383773346,-3.28538227003903,338.659979016636));
#29495=CARTESIAN_POINT('Ctrl Pts',(47.0051647069299,-3.18334388456646,338.751573832063));
#29496=CARTESIAN_POINT('Ctrl Pts',(46.9973910365252,-3.07758030544742,338.83880123156));
#29497=CARTESIAN_POINT('Ctrl Pts',(46.9896173661205,-2.96851386747844,338.921365639811));
#29498=CARTESIAN_POINT('Ctrl Pts',(46.9822055619436,-2.86452449843929,339.000086654992));
#29499=CARTESIAN_POINT('Ctrl Pts',(46.9747937577667,-2.7575330828981,339.074568869282));
#29500=CARTESIAN_POINT('Ctrl Pts',(46.9673819535897,-2.64792702097345,339.144594739429));
#29501=CARTESIAN_POINT('Ctrl Pts',(46.9596068748113,-2.53294883945196,339.218052786069));
#29502=CARTESIAN_POINT('Ctrl Pts',(46.9518317960329,-2.41472987540388,339.28683874672));
#29503=CARTESIAN_POINT('Ctrl Pts',(46.9440567172544,-2.29368670681961,339.350653324899));
#29504=CARTESIAN_POINT('Ctrl Pts',(46.9362912062054,-2.17279248956019,339.414389375178));
#29505=CARTESIAN_POINT('Ctrl Pts',(46.9285256951564,-2.04908132520099,339.473166034713));
#29506=CARTESIAN_POINT('Ctrl Pts',(46.9207601841074,-1.92299882414081,339.526727138326));
#29507=CARTESIAN_POINT('Ctrl Pts',(46.9130023725852,-1.79704133424759,339.580235135948));
#29508=CARTESIAN_POINT('Ctrl Pts',(46.905244561063,-1.66871754408978,339.628537716863));
#29509=CARTESIAN_POINT('Ctrl Pts',(46.8974867495408,-1.53849741439805,339.671424704348));
#29510=CARTESIAN_POINT('Ctrl Pts',(46.8897347760178,-1.40837527948344,339.714279418015));
#29511=CARTESIAN_POINT('Ctrl Pts',(46.8819828024948,-1.27636001528255,339.75172652837));
#29512=CARTESIAN_POINT('Ctrl Pts',(46.8742308289718,-1.142940970448,339.78360418519));
#29513=CARTESIAN_POINT('Ctrl Pts',(46.8664821384142,-1.00957842865815,339.815468341804));
#29514=CARTESIAN_POINT('Ctrl Pts',(46.8587334478566,-0.874813668039296,
339.84176764546));
#29515=CARTESIAN_POINT('Ctrl Pts',(46.8509847572989,-0.739150377022791,
339.862390336311));
#29516=CARTESIAN_POINT('Ctrl Pts',(46.8432376789211,-0.60351531188697,339.883008736439));
#29517=CARTESIAN_POINT('Ctrl Pts',(46.8354906005432,-0.46698247439608,339.897952814281));
#29518=CARTESIAN_POINT('Ctrl Pts',(46.8277435221654,-0.330064514506286,
339.90716216145));
#29519=CARTESIAN_POINT('Ctrl Pts',(46.8199963788596,-0.193145407112298,
339.916371585802));
#29520=CARTESIAN_POINT('Ctrl Pts',(46.8122492355538,-0.0558415608746182,
339.919846157384));
#29521=CARTESIAN_POINT('Ctrl Pts',(46.804502092248,0.0813308958569487,339.917577487735));
#29522=CARTESIAN_POINT('Ctrl Pts',(46.7967532072199,0.218534191869136,339.915308308041));
#29523=CARTESIAN_POINT('Ctrl Pts',(46.7890043221918,0.355605648851132,339.907293324229));
#29524=CARTESIAN_POINT('Ctrl Pts',(46.7812554371637,0.492031183513202,339.893576235939));
#29525=CARTESIAN_POINT('Ctrl Pts',(46.773498327389,0.628601521647209,339.87984458819));
#29526=CARTESIAN_POINT('Ctrl Pts',(46.7657412176142,0.764524178406057,339.860398785147));
#29527=CARTESIAN_POINT('Ctrl Pts',(46.7579841078395,0.899291673883825,339.835334274668));
#29528=CARTESIAN_POINT('Ctrl Pts',(46.7502228529133,1.03413118480224,339.810256370517));
#29529=CARTESIAN_POINT('Ctrl Pts',(46.7424615979872,1.16781392368806,339.779553863713));
#29530=CARTESIAN_POINT('Ctrl Pts',(46.734700343061,1.29984557579606,339.743372696888));
#29531=CARTESIAN_POINT('Ctrl Pts',(46.7269266726564,1.43208843551832,339.707133651988));
#29532=CARTESIAN_POINT('Ctrl Pts',(46.7191530022517,1.56267455804415,339.665398552915));
#29533=CARTESIAN_POINT('Ctrl Pts',(46.711379331847,1.69112683819248,339.618362597246));
#29534=CARTESIAN_POINT('Ctrl Pts',(46.7039675276699,1.81359963379623,339.57351617663));
#29535=CARTESIAN_POINT('Ctrl Pts',(46.6965557234929,1.93413251091924,339.52385141268));
#29536=CARTESIAN_POINT('Ctrl Pts',(46.6891439193158,2.05233288836629,339.469576353283));
#29537=CARTESIAN_POINT('Ctrl Pts',(46.6813688405373,2.17632661841252,339.412641111549));
#29538=CARTESIAN_POINT('Ctrl Pts',(46.6735937617589,2.29814526505762,339.350452292836));
#29539=CARTESIAN_POINT('Ctrl Pts',(46.6658186829804,2.41731170924942,339.283198239963));
#29540=CARTESIAN_POINT('Ctrl Pts',(46.6580531719314,2.53633151154506,339.216026947484));
#29541=CARTESIAN_POINT('Ctrl Pts',(46.6502876608825,2.65270526807261,339.143803013191));
#29542=CARTESIAN_POINT('Ctrl Pts',(46.6425221498335,2.76597641871267,339.066762534698));
#29543=CARTESIAN_POINT('Ctrl Pts',(46.6347643383113,2.87913526067709,338.989798442064));
#29544=CARTESIAN_POINT('Ctrl Pts',(46.6270065267891,2.98919729753012,338.908027527387));
#29545=CARTESIAN_POINT('Ctrl Pts',(46.619248715267,3.09573146446576,338.821731251987));
#29546=CARTESIAN_POINT('Ctrl Pts',(46.611496741744,3.20218546106231,338.735499917272));
#29547=CARTESIAN_POINT('Ctrl Pts',(46.603744768221,3.30511656955243,338.644750245312));
#29548=CARTESIAN_POINT('Ctrl Pts',(46.595992794698,3.40412387199562,338.549806153385));
#29549=CARTESIAN_POINT('Ctrl Pts',(46.5882441041404,3.50308924478751,338.454902270338));
#29550=CARTESIAN_POINT('Ctrl Pts',(46.5804954135828,3.59813383507359,338.355807770315));
#29551=CARTESIAN_POINT('Ctrl Pts',(46.5727467230251,3.68889108690309,338.252885735999));
#29552=CARTESIAN_POINT('Ctrl Pts',(46.5649996446473,3.77962945592833,338.149985115472));
#29553=CARTESIAN_POINT('Ctrl Pts',(46.5572525662695,3.86608200242266,338.043258837638));
#29554=CARTESIAN_POINT('Ctrl Pts',(46.5495054878917,3.94792050337689,337.933105310335));
#29555=CARTESIAN_POINT('Ctrl Pts',(46.5417583445859,4.02975969021658,337.82295085984));
#29556=CARTESIAN_POINT('Ctrl Pts',(46.5340112012801,4.1069845212793,337.709369416344));
#29557=CARTESIAN_POINT('Ctrl Pts',(46.5262640579743,4.17930863586297,337.592790463709));
#29558=CARTESIAN_POINT('Ctrl Pts',(46.5185151729462,4.251649010443,337.476185301651));
#29559=CARTESIAN_POINT('Ctrl Pts',(46.5107662879181,4.31908627009488,337.356581621544));
#29560=CARTESIAN_POINT('Ctrl Pts',(46.5030174028901,4.38137896281191,337.234435375375));
#29561=CARTESIAN_POINT('Ctrl Pts',(46.4952602931154,4.44373777363664,337.11215948192));
#29562=CARTESIAN_POINT('Ctrl Pts',(46.4875031833407,4.5009409318119,336.987335980242));
#29563=CARTESIAN_POINT('Ctrl Pts',(46.479746073566,4.55279407498322,336.860443273335));
#29564=CARTESIAN_POINT('Ctrl Pts',(46.4719848186398,4.60467492681631,336.733482759023));
#29565=CARTESIAN_POINT('Ctrl Pts',(46.4642235637137,4.65119993456036,336.604451203757));
#29566=CARTESIAN_POINT('Ctrl Pts',(46.4564623087875,4.6922243224165,336.473843265284));
#29567=CARTESIAN_POINT('Ctrl Pts',(46.4486886383829,4.7333143359234,336.343026396675));
#29568=CARTESIAN_POINT('Ctrl Pts',(46.4409149679782,4.76888604466275,336.210628483442));
#29569=CARTESIAN_POINT('Ctrl Pts',(46.4331412975735,4.79884540545156,336.077156366122));
#29570=CARTESIAN_POINT('Ctrl Pts',(46.4257294933963,4.82741015078846,335.949897407971));
#29571=CARTESIAN_POINT('Ctrl Pts',(46.4183176892191,4.85087324721813,335.821662286603));
#29572=CARTESIAN_POINT('Ctrl Pts',(46.4109058850419,4.8691971984371,335.692893718569));
#29573=CARTESIAN_POINT('Ctrl Pts',(46.4031308062634,4.88841926108922,335.557813819436));
#29574=CARTESIAN_POINT('Ctrl Pts',(46.395355727485,4.90204641634547,335.421719982386));
#29575=CARTESIAN_POINT('Ctrl Pts',(46.3875806487065,4.90997884920386,335.285115350114));
#29576=CARTESIAN_POINT('Ctrl Pts',(46.3798151376575,4.91790152069862,335.148678818539));
#29577=CARTESIAN_POINT('Ctrl Pts',(46.3720496266085,4.92014339070318,335.011733128895));
#29578=CARTESIAN_POINT('Ctrl Pts',(46.3642841155595,4.91665592786032,334.874789978293));
#29579=CARTESIAN_POINT('Ctrl Pts',(46.3565263040373,4.91317192284702,334.737982607223));
#29580=CARTESIAN_POINT('Ctrl Pts',(46.348768492515,4.90396989968825,334.601178158416));
#29581=CARTESIAN_POINT('Ctrl Pts',(46.3410106809928,4.88905327131267,334.464891438335));
#29582=CARTESIAN_POINT('Ctrl Pts',(46.3332587074698,4.87414786817297,334.328707278333));
#29583=CARTESIAN_POINT('Ctrl Pts',(46.3255067339468,4.85353646195163,334.193040458551));
#29584=CARTESIAN_POINT('Ctrl Pts',(46.3177547604238,4.8272744818967,334.058403409666));
#29585=CARTESIAN_POINT('Ctrl Pts',(46.3100060698661,4.80102362380593,333.923823379651));
#29586=CARTESIAN_POINT('Ctrl Pts',(46.3022573793085,4.76912702610943,333.790272635988));
#29587=CARTESIAN_POINT('Ctrl Pts',(46.2945086887509,4.73169164832267,333.65825590827));
#29588=CARTESIAN_POINT('Ctrl Pts',(46.286761610373,4.69426405927893,333.526266647734));
#29589=CARTESIAN_POINT('Ctrl Pts',(46.2790145319952,4.65130008889624,333.395811144114));
#29590=CARTESIAN_POINT('Ctrl Pts',(46.2712674536173,4.60295714652336,333.267381008482));
#29591=CARTESIAN_POINT('Ctrl Pts',(46.2635203103115,4.55461379899007,333.138949796482));
#29592=CARTESIAN_POINT('Ctrl Pts',(46.2557731670057,4.50089152724785,333.012544352144));
#29593=CARTESIAN_POINT('Ctrl Pts',(46.2480260236999,4.441996527232,332.888637900653));
#29594=CARTESIAN_POINT('Ctrl Pts',(46.2402771386717,4.38308828636985,332.764703592362));
#29595=CARTESIAN_POINT('Ctrl Pts',(46.2325282536437,4.31900517088127,332.643269747846));
#29596=CARTESIAN_POINT('Ctrl Pts',(46.2247793686155,4.24999993698532,332.524786151032));
#29597=CARTESIAN_POINT('Ctrl Pts',(46.2170222588408,4.18092146022106,332.406176794504));
#29598=CARTESIAN_POINT('Ctrl Pts',(46.2092651490661,4.10691062587209,332.290524279289));
#29599=CARTESIAN_POINT('Ctrl Pts',(46.2015080392913,4.02826455259932,332.178250940149));
#29600=CARTESIAN_POINT('Ctrl Pts',(46.1937467843651,3.94957645337966,332.065917605726));
#29601=CARTESIAN_POINT('Ctrl Pts',(46.185985529439,3.86624841708287,331.956967355762));
#29602=CARTESIAN_POINT('Ctrl Pts',(46.1782242745128,3.77861806547016,331.851789623008));
#29603=CARTESIAN_POINT('Ctrl Pts',(46.1704506041081,3.69084753385355,331.746443640158));
#29604=CARTESIAN_POINT('Ctrl Pts',(46.1626769337034,3.59876119673338,331.644882523549));
#29605=CARTESIAN_POINT('Ctrl Pts',(46.1549032632988,3.50273437496572,331.547459636596));
#29606=CARTESIAN_POINT('Ctrl Pts',(46.1474914591218,3.411177624856,331.454571808471));
#29607=CARTESIAN_POINT('Ctrl Pts',(46.1400796549449,3.31603920331488,331.365445807822));
#29608=CARTESIAN_POINT('Ctrl Pts',(46.1326678507679,3.21767110873487,331.280352745419));
#29609=CARTESIAN_POINT('Ctrl Pts',(46.1248927719895,3.11448170081422,331.191089018547));
#29610=CARTESIAN_POINT('Ctrl Pts',(46.1171176932111,3.00741192543951,331.105981468679));
#29611=CARTESIAN_POINT('Ctrl Pts',(46.1093426144327,2.89683087041296,331.025386311763));
#29612=CARTESIAN_POINT('Ctrl Pts',(46.1015771033837,2.78638589241456,330.944890332318));
#29613=CARTESIAN_POINT('Ctrl Pts',(46.0938115923347,2.67243854488297,330.868895925395));
#29614=CARTESIAN_POINT('Ctrl Pts',(46.0860460812857,2.55539286173332,330.797720810714));
#29615=CARTESIAN_POINT('Ctrl Pts',(46.0782882697635,2.4384632297192,330.726616266367));
#29616=CARTESIAN_POINT('Ctrl Pts',(46.0705304582413,2.31844170737988,330.660321706871));
#29617=CARTESIAN_POINT('Ctrl Pts',(46.0627726467191,2.19576305338438,330.599112853538));
#29618=CARTESIAN_POINT('Ctrl Pts',(46.0550206731961,2.07317671896638,330.537950061809));
#29619=CARTESIAN_POINT('Ctrl Pts',(46.0472686996731,1.94793758129912,330.481865532281));
#29620=CARTESIAN_POINT('Ctrl Pts',(46.0395167261501,1.82050655021642,330.43108995896));
#29621=CARTESIAN_POINT('Ctrl Pts',(46.0317680355924,1.69312948625113,330.380335889124));
#29622=CARTESIAN_POINT('Ctrl Pts',(46.0240193450349,1.56356273748543,330.334886448075));
#29623=CARTESIAN_POINT('Ctrl Pts',(46.0162706544773,1.4322886237324,330.294924829418));
#29624=CARTESIAN_POINT('Ctrl Pts',(46.0085235760994,1.30104182265517,330.25497152511));
#29625=CARTESIAN_POINT('Ctrl Pts',(46.0007764977216,1.16808873686888,330.220503885856));
#29626=CARTESIAN_POINT('Ctrl Pts',(45.9930294193438,1.03392795584425,330.191655581739));
#29627=CARTESIAN_POINT('Ctrl Pts',(45.985282276038,0.899766050423068,330.162807035845));
#29628=CARTESIAN_POINT('Ctrl Pts',(45.9775351327322,0.764396811714784,330.139578001193));
#29629=CARTESIAN_POINT('Ctrl Pts',(45.9697879894264,0.628329769325667,330.122051172524));
#29630=CARTESIAN_POINT('Ctrl Pts',(45.9620391043983,0.492232136176728,330.104520403451));
#29631=CARTESIAN_POINT('Ctrl Pts',(45.9542902193702,0.355436774766759,330.092694441278));
#29632=CARTESIAN_POINT('Ctrl Pts',(45.9465413343421,0.218458698889019,330.0866041418));
#29633=CARTESIAN_POINT('Ctrl Pts',(45.9387842245674,0.0813352330662,330.080507378014));
#29634=CARTESIAN_POINT('Ctrl Pts',(45.9310271147927,-0.0559709435225165,
330.080158455448));
#29635=CARTESIAN_POINT('Ctrl Pts',(45.923270005018,-0.192943892610512,330.085536070251));
#29636=CARTESIAN_POINT('Ctrl Pts',(45.9155087500918,-0.329990035662955,
330.09091655868));
#29637=CARTESIAN_POINT('Ctrl Pts',(45.9077474951657,-0.466702207010266,
330.102029650308));
#29638=CARTESIAN_POINT('Ctrl Pts',(45.8999862402395,-0.602570217838123,
330.1188021762));
#29639=CARTESIAN_POINT('Ctrl Pts',(45.8922125698349,-0.73865557320393,330.135601532666));
#29640=CARTESIAN_POINT('Ctrl Pts',(45.8844388994303,-0.873893683799842,
330.158078350353));
#29641=CARTESIAN_POINT('Ctrl Pts',(45.8766652290256,-1.00778429114064,330.186108239165));
#29642=CARTESIAN_POINT('Ctrl Pts',(45.8692534248484,-1.13544225849978,330.21283332991));
#29643=CARTESIAN_POINT('Ctrl Pts',(45.8618416206712,-1.26187507280759,330.244606065274));
#29644=CARTESIAN_POINT('Ctrl Pts',(45.854429816494,-1.38666426470488,330.281277155894));
#29645=CARTESIAN_POINT('Ctrl Pts',(45.8466547377155,-1.51756974662326,330.319745605902));
#29646=CARTESIAN_POINT('Ctrl Pts',(45.8388796589371,-1.64708010011546,330.363726285544));
#29647=CARTESIAN_POINT('Ctrl Pts',(45.8311045801586,-1.7746960410034,330.413101589903));
#29648=CARTESIAN_POINT('Ctrl Pts',(45.8233390691096,-1.90215494235157,330.462416134807));
#29649=CARTESIAN_POINT('Ctrl Pts',(45.8155735580605,-2.02772370845022,330.517111956162));
#29650=CARTESIAN_POINT('Ctrl Pts',(45.8078080470115,-2.15091651607223,330.577021229602));
#29651=CARTESIAN_POINT('Ctrl Pts',(45.8000502354893,-2.27398717766699,330.636871102824));
#29652=CARTESIAN_POINT('Ctrl Pts',(45.7922924239671,-2.39468621965149,330.701923971382));
#29653=CARTESIAN_POINT('Ctrl Pts',(45.7845346124448,-2.51254650922983,330.771963446059));
#29654=CARTESIAN_POINT('Ctrl Pts',(45.7767826389218,-2.63031810520262,330.841950213812));
#29655=CARTESIAN_POINT('Ctrl Pts',(45.7690306653988,-2.74525486620574,330.916915919479));
#29656=CARTESIAN_POINT('Ctrl Pts',(45.7612786918758,-2.85691337197112,330.996597815913));
#29657=CARTESIAN_POINT('Ctrl Pts',(45.7535300013181,-2.96852459029293,331.076245967016));
#29658=CARTESIAN_POINT('Ctrl Pts',(45.7457813107605,-3.0768599971882,331.160606109799));
#29659=CARTESIAN_POINT('Ctrl Pts',(45.7380326202029,-3.18150453031966,331.249371787813));
#29660=CARTESIAN_POINT('Ctrl Pts',(45.730285541825,-3.28612729128206,331.338118997385));
#29661=CARTESIAN_POINT('Ctrl Pts',(45.7225384634472,-3.38706040803083,331.431269666301));
#29662=CARTESIAN_POINT('Ctrl Pts',(45.7147913850693,-3.48392165917142,331.528476856586));
#29663=CARTESIAN_POINT('Ctrl Pts',(45.7070442417635,-3.58078372210252,331.625684861562));
#29664=CARTESIAN_POINT('Ctrl Pts',(45.6992970984577,-3.67357357546152,331.726949178837));
#29665=CARTESIAN_POINT('Ctrl Pts',(45.6915499551519,-3.76194594377021,331.831886084963));
#29666=CARTESIAN_POINT('Ctrl Pts',(45.6838010701237,-3.85033818006337,331.936846583134));
#29667=CARTESIAN_POINT('Ctrl Pts',(45.6760521850956,-3.93431070332546,332.04548101424));
#29668=CARTESIAN_POINT('Ctrl Pts',(45.6683033000675,-4.01355886274549,332.157372990036));
#29669=CARTESIAN_POINT('Ctrl Pts',(45.6605461902927,-4.09289113698077,332.269383729131));
#29670=CARTESIAN_POINT('Ctrl Pts',(45.652789080518,-4.16748880419008,332.384658600302));
#29671=CARTESIAN_POINT('Ctrl Pts',(45.6450319707433,-4.23709057543311,332.502752211318));
#29672=CARTESIAN_POINT('Ctrl Pts',(45.6372707158171,-4.30672953963721,332.620908927784));
#29673=CARTESIAN_POINT('Ctrl Pts',(45.6295094608909,-4.37136710425829,332.741887040846));
#29674=CARTESIAN_POINT('Ctrl Pts',(45.6217482059647,-4.43078870617346,332.865217925936));
#29675=CARTESIAN_POINT('Ctrl Pts',(45.61397453556,-4.49030536328627,332.988746100249));
#29676=CARTESIAN_POINT('Ctrl Pts',(45.6062008651553,-4.54458922937574,333.114634208398));
#29677=CARTESIAN_POINT('Ctrl Pts',(45.5984271947507,-4.59347418815556,333.242394257733));
#29678=CARTESIAN_POINT('Ctrl Pts',(45.5910153905738,-4.64008354034179,333.364207046031));
#29679=CARTESIAN_POINT('Ctrl Pts',(45.5836035863969,-4.68178521986609,333.487721147128));
#29680=CARTESIAN_POINT('Ctrl Pts',(45.57619178222,-4.71847830955698,333.612503872171));
#29681=CARTESIAN_POINT('Ctrl Pts',(45.5665478765862,-4.76622170454504,333.774865531535));
#29682=CARTESIAN_POINT('Ctrl Pts',(45.5569039709524,-4.80560894877283,333.939788460419));
#29683=CARTESIAN_POINT('Ctrl Pts',(45.5472600653186,-4.83640864842891,334.106504366042));
#29684=CARTESIAN_POINT('Ctrl Pts',(45.537753019719,-4.86677125878656,334.270854348002));
#29685=CARTESIAN_POINT('Ctrl Pts',(45.5282459741194,-4.88878833469871,334.436946835478));
#29686=CARTESIAN_POINT('Ctrl Pts',(45.5187389285197,-4.90228382780651,334.604024831427));
#29687=CARTESIAN_POINT('Ctrl Pts',(45.5113380351879,-4.91278958418529,334.734089046766));
#29688=CARTESIAN_POINT('Ctrl Pts',(45.503937141856,-4.91813207402702,334.864750086541));
#29689=CARTESIAN_POINT('Ctrl Pts',(45.4965362485241,-4.91824806876705,334.995641494621));
#29690=CARTESIAN_POINT('',(48.9965362484528,-4.91824811618257,335.004304668006));
#29691=CARTESIAN_POINT('Ctrl Pts',(48.9965362484528,-4.91824811618257,335.004304668006));
#29692=CARTESIAN_POINT('Ctrl Pts',(48.9871270537799,-4.91810243521494,335.170750754804));
#29693=CARTESIAN_POINT('Ctrl Pts',(48.977717859107,-4.90950360885218,335.336825553689));
#29694=CARTESIAN_POINT('Ctrl Pts',(48.9683086644341,-4.89258686062691,335.501773727611));
#29695=CARTESIAN_POINT('Ctrl Pts',(48.9587672542104,-4.8754324026652,335.669039710277));
#29696=CARTESIAN_POINT('Ctrl Pts',(48.9492258439866,-4.84972467282967,335.835147204582));
#29697=CARTESIAN_POINT('Ctrl Pts',(48.9396844337628,-4.81565367945835,335.999331127314));
#29698=CARTESIAN_POINT('Ctrl Pts',(48.9314723536777,-4.78632953139384,336.140640586876));
#29699=CARTESIAN_POINT('Ctrl Pts',(48.9232602735926,-4.75081098049385,336.280525521972));
#29700=CARTESIAN_POINT('Ctrl Pts',(48.9150481935074,-4.7092472580705,336.418510953379));
#29701=CARTESIAN_POINT('Ctrl Pts',(48.907273114729,-4.66989532618284,336.549153566254));
#29702=CARTESIAN_POINT('Ctrl Pts',(48.8994980359506,-4.62504071553603,336.678363843504));
#29703=CARTESIAN_POINT('Ctrl Pts',(48.8917229571721,-4.57480440138443,336.80564330685));
#29704=CARTESIAN_POINT('Ctrl Pts',(48.8839574461231,-4.52462990621563,336.932766144714));
#29705=CARTESIAN_POINT('Ctrl Pts',(48.8761919350741,-4.46908702660577,337.057962536106));
#29706=CARTESIAN_POINT('Ctrl Pts',(48.8684264240251,-4.40834686517368,337.180747802662));
#29707=CARTESIAN_POINT('Ctrl Pts',(48.8606686125029,-4.34766692778848,337.303411327267));
#29708=CARTESIAN_POINT('Ctrl Pts',(48.8529108009808,-4.28180013577821,337.423668136446));
#29709=CARTESIAN_POINT('Ctrl Pts',(48.8451529894586,-4.21096602923657,337.541052569924));
#29710=CARTESIAN_POINT('Ctrl Pts',(48.8374010159355,-4.14018522760629,337.658348667893));
#29711=CARTESIAN_POINT('Ctrl Pts',(48.8296490424125,-4.06444475300885,337.772776359314));
#29712=CARTESIAN_POINT('Ctrl Pts',(48.8218970688895,-3.98401034221723,337.88389400908));
#29713=CARTESIAN_POINT('Ctrl Pts',(48.8141483783318,-3.90360999544645,337.994964600455));
#29714=CARTESIAN_POINT('Ctrl Pts',(48.8063996877743,-3.8185198949626,338.1027276223));
#29715=CARTESIAN_POINT('Ctrl Pts',(48.7986509972167,-3.72904929426316,338.206770092079));
#29716=CARTESIAN_POINT('Ctrl Pts',(48.7909039188388,-3.63959730866947,338.310790914954));
#29717=CARTESIAN_POINT('Ctrl Pts',(48.783156840461,-3.54576689039424,338.411092429311));
#29718=CARTESIAN_POINT('Ctrl Pts',(48.7754097620831,-3.44790755166998,338.507294766289));
#29719=CARTESIAN_POINT('Ctrl Pts',(48.7676626187773,-3.35004739279028,338.603497909535));
#29720=CARTESIAN_POINT('Ctrl Pts',(48.7599154754716,-3.24815852485193,338.69560153286));
#29721=CARTESIAN_POINT('Ctrl Pts',(48.7521683321658,-3.1426269951272,338.78326296099));
#29722=CARTESIAN_POINT('Ctrl Pts',(48.7444194471377,-3.03707173967402,338.87094409727));
#29723=CARTESIAN_POINT('Ctrl Pts',(48.7366705621096,-2.92787249343328,338.954180801344));
#29724=CARTESIAN_POINT('Ctrl Pts',(48.7289216770815,-2.81544769328122,339.032671242353));
#29725=CARTESIAN_POINT('Ctrl Pts',(48.7211645673068,-2.70290356428479,339.111244993926));
#29726=CARTESIAN_POINT('Ctrl Pts',(48.713407457532,-2.58712736334224,339.185062194982));
#29727=CARTESIAN_POINT('Ctrl Pts',(48.7056503477573,-2.46856623771255,339.253864571484));
#29728=CARTESIAN_POINT('Ctrl Pts',(48.6978890928312,-2.34994175680825,339.322703713776));
#29729=CARTESIAN_POINT('Ctrl Pts',(48.690127837905,-2.22852973170751,339.386522510074));
#29730=CARTESIAN_POINT('Ctrl Pts',(48.6823665829789,-2.10480022581093,339.445109568045));
#29731=CARTESIAN_POINT('Ctrl Pts',(48.6745929125742,-1.98087279302818,339.503790346215));
#29732=CARTESIAN_POINT('Ctrl Pts',(48.6668192421695,-1.85462083149161,339.557222509742));
#29733=CARTESIAN_POINT('Ctrl Pts',(48.6590455717649,-1.72653344494976,339.605243242867));
#29734=CARTESIAN_POINT('Ctrl Pts',(48.6516337675877,-1.60440855706575,339.651028599312));
#29735=CARTESIAN_POINT('Ctrl Pts',(48.6442219634105,-1.48061555003002,339.691894901509));
#29736=CARTESIAN_POINT('Ctrl Pts',(48.6368101592333,-1.3555877845884,339.727744157711));
#29737=CARTESIAN_POINT('Ctrl Pts',(48.6290350804549,-1.22443203592577,339.765350492749));
#29738=CARTESIAN_POINT('Ctrl Pts',(48.6212600016764,-1.09150295362755,339.797554388829));
#29739=CARTESIAN_POINT('Ctrl Pts',(48.613484922898,-0.957285185365169,339.824187821425));
#29740=CARTESIAN_POINT('Ctrl Pts',(48.605719411849,-0.823232580611261,339.850788479886));
#29741=CARTESIAN_POINT('Ctrl Pts',(48.5979539007999,-0.68789482493425,339.871832238616));
#29742=CARTESIAN_POINT('Ctrl Pts',(48.5901883897509,-0.551772088158436,
339.887200694184));
#29743=CARTESIAN_POINT('Ctrl Pts',(48.5824305782287,-0.415784317472539,
339.902553911882));
#29744=CARTESIAN_POINT('Ctrl Pts',(48.5746727667066,-0.27901350047548,339.912242981055));
#29745=CARTESIAN_POINT('Ctrl Pts',(48.5669149551844,-0.141970026566872,
339.916200522157));
#29746=CARTESIAN_POINT('Ctrl Pts',(48.5591629816614,-0.00502968221827982,
339.920155085084));
#29747=CARTESIAN_POINT('Ctrl Pts',(48.5514110081383,0.132182521496973,339.91838669383));
#29748=CARTESIAN_POINT('Ctrl Pts',(48.5436590346153,0.26915139878126,339.91087981802));
#29749=CARTESIAN_POINT('Ctrl Pts',(48.5359103440577,0.406062269664699,339.903376121376));
#29750=CARTESIAN_POINT('Ctrl Pts',(48.5281616535001,0.542729629597855,339.890138795123));
#29751=CARTESIAN_POINT('Ctrl Pts',(48.5204129629425,0.678638837944847,339.871204408576));
#29752=CARTESIAN_POINT('Ctrl Pts',(48.5126658845646,0.814519769245907,339.852273961487));
#29753=CARTESIAN_POINT('Ctrl Pts',(48.5049188061868,0.949642475824041,339.827648865693));
#29754=CARTESIAN_POINT('Ctrl Pts',(48.497171727809,1.08349837672737,339.79741746465));
#29755=CARTESIAN_POINT('Ctrl Pts',(48.4894245845032,1.21735539947198,339.767185810239));
#29756=CARTESIAN_POINT('Ctrl Pts',(48.4816774411973,1.34994521409406,339.731347842972));
#29757=CARTESIAN_POINT('Ctrl Pts',(48.4739302978915,1.48077074531474,339.690042756982));
#29758=CARTESIAN_POINT('Ctrl Pts',(48.4661814128635,1.61162568889215,339.648728384732));
#29759=CARTESIAN_POINT('Ctrl Pts',(48.4584325278354,1.74071518711738,339.6019445656));
#29760=CARTESIAN_POINT('Ctrl Pts',(48.4506836428073,1.86755898377751,339.549879834085));
#29761=CARTESIAN_POINT('Ctrl Pts',(48.4429265330326,1.99453741375413,339.497759840525));
#29762=CARTESIAN_POINT('Ctrl Pts',(48.4351694232578,2.1192650185099,339.440347886297));
#29763=CARTESIAN_POINT('Ctrl Pts',(48.4274123134831,2.24128263285874,339.377880220169));
#29764=CARTESIAN_POINT('Ctrl Pts',(48.4196510585569,2.36336544951923,339.315379173317));
#29765=CARTESIAN_POINT('Ctrl Pts',(48.4118898036308,2.48273505024341,339.247817223797));
#29766=CARTESIAN_POINT('Ctrl Pts',(48.4041285487046,2.5989592924295,339.175475261428));
#29767=CARTESIAN_POINT('Ctrl Pts',(48.3963548782999,2.71536945552577,339.103017575495));
#29768=CARTESIAN_POINT('Ctrl Pts',(48.3885812078953,2.82862388248384,339.025764817192));
#29769=CARTESIAN_POINT('Ctrl Pts',(48.3808075374907,2.9383209759564,338.944040175347));
#29770=CARTESIAN_POINT('Ctrl Pts',(48.3733957333136,3.04291164333591,338.866119835243));
#29771=CARTESIAN_POINT('Ctrl Pts',(48.3659839291365,3.14426848804456,338.784134755646));
#29772=CARTESIAN_POINT('Ctrl Pts',(48.3585721249594,3.24207459036566,338.698396329898));
#29773=CARTESIAN_POINT('Ctrl Pts',(48.350797046181,3.34467446111122,338.608455608502));
#29774=CARTESIAN_POINT('Ctrl Pts',(48.3430219674025,3.44369095826579,338.514100083308));
#29775=CARTESIAN_POINT('Ctrl Pts',(48.3352468886241,3.53872051575556,338.415646377169));
#29776=CARTESIAN_POINT('Ctrl Pts',(48.3274813775751,3.63363313332503,338.317313824584));
#29777=CARTESIAN_POINT('Ctrl Pts',(48.3197158665261,3.72456830426629,338.21489340387));
#29778=CARTESIAN_POINT('Ctrl Pts',(48.3119503554771,3.81115579001483,338.108741643613));
#29779=CARTESIAN_POINT('Ctrl Pts',(48.3041925439548,3.8976574240191,338.002695133136));
#29780=CARTESIAN_POINT('Ctrl Pts',(48.2964347324327,3.9798197059786,337.892924946534));
#29781=CARTESIAN_POINT('Ctrl Pts',(48.2886769209105,4.0573097740065,337.779823818203));
#29782=CARTESIAN_POINT('Ctrl Pts',(48.2809249473874,4.13474152830081,337.666807802059));
#29783=CARTESIAN_POINT('Ctrl Pts',(48.2731729738644,4.20750784703314,337.550466154683));
#29784=CARTESIAN_POINT('Ctrl Pts',(48.2654210003414,4.27531687378358,337.431223702427));
#29785=CARTESIAN_POINT('Ctrl Pts',(48.2576723097838,4.34309718337099,337.31203174942));
#29786=CARTESIAN_POINT('Ctrl Pts',(48.2499236192262,4.40592418374961,337.189941773988));
#29787=CARTESIAN_POINT('Ctrl Pts',(48.2421749286685,4.46355012526062,337.065406338178));
#29788=CARTESIAN_POINT('Ctrl Pts',(48.2344278502907,4.52116407721321,336.940896813006));
#29789=CARTESIAN_POINT('Ctrl Pts',(48.2266807719128,4.57357895867524,336.813943194006));
#29790=CARTESIAN_POINT('Ctrl Pts',(48.218933693535,4.62059383720838,336.685020965464));
#29791=CARTESIAN_POINT('Ctrl Pts',(48.2111865502292,4.66760910977145,336.556097656429));
#29792=CARTESIAN_POINT('Ctrl Pts',(48.2034394069234,4.7092241552209,336.425206072164));
#29793=CARTESIAN_POINT('Ctrl Pts',(48.1956922636176,4.74528702891783,336.292839539805));
#29794=CARTESIAN_POINT('Ctrl Pts',(48.1879433785895,4.78135801031437,336.160443248641));
#29795=CARTESIAN_POINT('Ctrl Pts',(48.1801944935614,4.81187423336076,336.026571726592));
#29796=CARTESIAN_POINT('Ctrl Pts',(48.1724456085333,4.83673434654541,335.89173085819));
#29797=CARTESIAN_POINT('Ctrl Pts',(48.1646884987586,4.86162084651107,335.756746868297));
#29798=CARTESIAN_POINT('Ctrl Pts',(48.1569313889838,4.88083917317195,335.620791861781));
#29799=CARTESIAN_POINT('Ctrl Pts',(48.1491742792091,4.89433951252887,335.484379808207));
#29800=CARTESIAN_POINT('Ctrl Pts',(48.1414130242829,4.90784706603548,335.347894860394));
#29801=CARTESIAN_POINT('Ctrl Pts',(48.1336517693567,4.91563052169075,335.210952768916));
#29802=CARTESIAN_POINT('Ctrl Pts',(48.1258905144306,4.91769222857898,335.074068937308));
#29803=CARTESIAN_POINT('Ctrl Pts',(48.1181168440259,4.91975723352632,334.936966136179));
#29804=CARTESIAN_POINT('Ctrl Pts',(48.1103431736212,4.91608220991886,334.799922172092));
#29805=CARTESIAN_POINT('Ctrl Pts',(48.1025695032166,4.90672160676861,334.663449652845));
#29806=CARTESIAN_POINT('Ctrl Pts',(48.0951576990396,4.89779674194713,334.533329962204));
#29807=CARTESIAN_POINT('Ctrl Pts',(48.0877458948625,4.88370374396625,334.403729998264));
#29808=CARTESIAN_POINT('Ctrl Pts',(48.0803340906855,4.8645329666847,334.275084778379));
#29809=CARTESIAN_POINT('Ctrl Pts',(48.0725590119071,4.84442257250159,334.140134273052));
#29810=CARTESIAN_POINT('Ctrl Pts',(48.0647839331287,4.81866050655486,334.00580799937));
#29811=CARTESIAN_POINT('Ctrl Pts',(48.0570088543503,4.78729463099764,333.872616667446));
#29812=CARTESIAN_POINT('Ctrl Pts',(48.0492433433013,4.75596735314714,333.739589235935));
#29813=CARTESIAN_POINT('Ctrl Pts',(48.0414778322522,4.71905007518084,333.607694344144));
#29814=CARTESIAN_POINT('Ctrl Pts',(48.0337123212032,4.67664225225996,333.477436271653));
#29815=CARTESIAN_POINT('Ctrl Pts',(48.025954509681,4.63427647681895,333.347307350421));
#29816=CARTESIAN_POINT('Ctrl Pts',(48.0181966981588,4.5864311103,333.218812388084));
#29817=CARTESIAN_POINT('Ctrl Pts',(48.0104388866366,4.53325628076957,333.09244382642));
#29818=CARTESIAN_POINT('Ctrl Pts',(48.0026869131136,4.48012146698467,332.966170361107));
#29819=CARTESIAN_POINT('Ctrl Pts',(47.9949349395906,4.42166532406268,332.842020470206));
#29820=CARTESIAN_POINT('Ctrl Pts',(47.9871829660676,4.35808715729016,332.720469479923));
#29821=CARTESIAN_POINT('Ctrl Pts',(47.97943427551,4.29453591590902,332.598969966557));
#29822=CARTESIAN_POINT('Ctrl Pts',(47.9716855849524,4.22586714581079,332.480067510356));
#29823=CARTESIAN_POINT('Ctrl Pts',(47.9639368943948,4.15232734451882,332.364215356585));
#29824=CARTESIAN_POINT('Ctrl Pts',(47.9561898160169,4.07880284379672,332.248387306823));
#29825=CARTESIAN_POINT('Ctrl Pts',(47.9484427376391,4.0004095370675,332.135608626941));
#29826=CARTESIAN_POINT('Ctrl Pts',(47.9406956592613,3.91743853313924,332.026305597144));
#29827=CARTESIAN_POINT('Ctrl Pts',(47.9329485159555,3.8344668338341,331.917001651283));
#29828=CARTESIAN_POINT('Ctrl Pts',(47.9252013726497,3.74691759713921,331.811173724943));
#29829=CARTESIAN_POINT('Ctrl Pts',(47.9174542293439,3.65512344640808,331.709216559234));
#29830=CARTESIAN_POINT('Ctrl Pts',(47.9097053443158,3.56330865840308,331.607236471391));
#29831=CARTESIAN_POINT('Ctrl Pts',(47.9019564592877,3.46724731879979,331.509129166269));
#29832=CARTESIAN_POINT('Ctrl Pts',(47.8942075742596,3.36730998957424,331.415253635665));
#29833=CARTESIAN_POINT('Ctrl Pts',(47.8864504644849,3.26726658583476,331.321278464603));
#29834=CARTESIAN_POINT('Ctrl Pts',(47.8786933547102,3.16333925968627,331.231544308586));
#29835=CARTESIAN_POINT('Ctrl Pts',(47.8709362449354,3.05593326188828,331.146371195693));
#29836=CARTESIAN_POINT('Ctrl Pts',(47.8631749900093,2.94846986975925,331.061152569012));
#29837=CARTESIAN_POINT('Ctrl Pts',(47.8554137350832,2.83752441797451,330.980500071664));
#29838=CARTESIAN_POINT('Ctrl Pts',(47.847652480157,2.72353159158441,330.904690642681));
#29839=CARTESIAN_POINT('Ctrl Pts',(47.8398788097523,2.60935641382235,330.828759943318));
#29840=CARTESIAN_POINT('Ctrl Pts',(47.8321051393476,2.49212445457095,330.757687996525));
#29841=CARTESIAN_POINT('Ctrl Pts',(47.824331468943,2.37229624214689,330.691706416457));
#29842=CARTESIAN_POINT('Ctrl Pts',(47.8169196647658,2.2580460618388,330.628796294815));
#29843=CARTESIAN_POINT('Ctrl Pts',(47.8095078605886,2.14143615740147,330.570513420545));
#29844=CARTESIAN_POINT('Ctrl Pts',(47.8020960564115,2.02288123986652,330.517017226009));
#29845=CARTESIAN_POINT('Ctrl Pts',(47.794320977633,1.89851559266764,330.460899023624));
#29846=CARTESIAN_POINT('Ctrl Pts',(47.7865458988546,1.77161643129144,330.409871240158));
#29847=CARTESIAN_POINT('Ctrl Pts',(47.7787708200762,1.64263912372649,330.364170001855));
#29848=CARTESIAN_POINT('Ctrl Pts',(47.7710053090272,1.51382053094959,330.318525001835));
#29849=CARTESIAN_POINT('Ctrl Pts',(47.7632397979782,1.38292924516727,330.278193634396));
#29850=CARTESIAN_POINT('Ctrl Pts',(47.7554742869292,1.25044314673299,330.243365160191));
#29851=CARTESIAN_POINT('Ctrl Pts',(47.747716475407,1.11808840865112,330.208571218518));
#29852=CARTESIAN_POINT('Ctrl Pts',(47.7399586638847,0.984142380311724,330.1792694108));
#29853=CARTESIAN_POINT('Ctrl Pts',(47.7322008523626,0.849100409423858,330.155599979645));
#29854=CARTESIAN_POINT('Ctrl Pts',(47.7244488788395,0.714160061901511,330.131948360487));
#29855=CARTESIAN_POINT('Ctrl Pts',(47.7166969053165,0.578125796873363,330.113920748492));
#29856=CARTESIAN_POINT('Ctrl Pts',(47.7089449317935,0.441505181812714,330.101606769875));
#29857=CARTESIAN_POINT('Ctrl Pts',(47.7011962412359,0.304942425663562,330.089298006236));
#29858=CARTESIAN_POINT('Ctrl Pts',(47.6934475506783,0.167794201858067,330.082698098324));
#29859=CARTESIAN_POINT('Ctrl Pts',(47.6856988601207,0.0305750479628804,
330.081845038132));
#29860=CARTESIAN_POINT('Ctrl Pts',(47.6779517817429,-0.106615556341168,
330.080992155428));
#29861=CARTESIAN_POINT('Ctrl Pts',(47.670204703365,-0.243876670759664,330.085883744581));
#29862=CARTESIAN_POINT('Ctrl Pts',(47.6624576249872,-0.380692291494497,
330.096505690663));
#29863=CARTESIAN_POINT('Ctrl Pts',(47.6547104816814,-0.517509058875916,
330.107127725768));
#29864=CARTESIAN_POINT('Ctrl Pts',(47.6469633383756,-0.653879935425003,
330.123480183338));
#29865=CARTESIAN_POINT('Ctrl Pts',(47.6392161950698,-0.789292973337843,
330.145496970365));
#29866=CARTESIAN_POINT('Ctrl Pts',(47.6314673100417,-0.9247364549766,330.167518707232));
#29867=CARTESIAN_POINT('Ctrl Pts',(47.6237184250137,-1.05922128373901,330.195207244886));
#29868=CARTESIAN_POINT('Ctrl Pts',(47.6159695399856,-1.19224504341742,330.228445240915));
#29869=CARTESIAN_POINT('Ctrl Pts',(47.6082124302108,-1.32540999588875,330.261718516096));
#29870=CARTESIAN_POINT('Ctrl Pts',(47.6004553204361,-1.45711040160517,330.300552921081));
#29871=CARTESIAN_POINT('Ctrl Pts',(47.5926982106614,-1.58685783768899,330.344780857418));
#29872=CARTESIAN_POINT('Ctrl Pts',(47.5849369557352,-1.71667460665414,330.389032427749));
#29873=CARTESIAN_POINT('Ctrl Pts',(47.577175700809,-1.84453596232846,330.438683130918));
#29874=CARTESIAN_POINT('Ctrl Pts',(47.5694144458829,-1.96997378775028,330.493517298593));
#29875=CARTESIAN_POINT('Ctrl Pts',(47.5616407754782,-2.09561227281259,330.548439183066));
#29876=CARTESIAN_POINT('Ctrl Pts',(47.5538671050736,-2.21881912904405,330.608560930118));
#29877=CARTESIAN_POINT('Ctrl Pts',(47.5460934346689,-2.33915036886212,330.673620611371));
#29878=CARTESIAN_POINT('Ctrl Pts',(47.5386816304918,-2.45388016051664,330.73565174881));
#29879=CARTESIAN_POINT('Ctrl Pts',(47.5312698263147,-2.56599578326613,330.802171297675));
#29880=CARTESIAN_POINT('Ctrl Pts',(47.5238580221376,-2.67513874309868,330.872916796614));
#29881=CARTESIAN_POINT('Ctrl Pts',(47.516087547911,-2.78956331991435,330.947085792856));
#29882=CARTESIAN_POINT('Ctrl Pts',(47.5083170736843,-2.90108290454413,331.026134975483));
#29883=CARTESIAN_POINT('Ctrl Pts',(47.5005465994576,-3.00925281587577,331.109809702258));
#29884=CARTESIAN_POINT('Ctrl Pts',(47.4927856906637,-3.11728957033832,331.193381425671));
#29885=CARTESIAN_POINT('Ctrl Pts',(47.4850247818698,-3.22198454916022,331.281567126827));
#29886=CARTESIAN_POINT('Ctrl Pts',(47.477263873076,-3.32292027247217,331.37406785429));
#29887=CARTESIAN_POINT('Ctrl Pts',(47.4695106565121,-3.42375595327387,331.466476899595));
#29888=CARTESIAN_POINT('Ctrl Pts',(47.4617574399482,-3.52083950663695,331.563192197508));
#29889=CARTESIAN_POINT('Ctrl Pts',(47.4540042233843,-3.6137852015038,331.663873566561));
#29890=CARTESIAN_POINT('Ctrl Pts',(47.4462568325578,-3.70666105732902,331.764479284016));
#29891=CARTESIAN_POINT('Ctrl Pts',(47.4385094417314,-3.79540497875993,331.869044854578));
#29892=CARTESIAN_POINT('Ctrl Pts',(47.4307620509049,-3.87966717411193,331.977192417533));
#29893=CARTESIAN_POINT('Ctrl Pts',(47.4230179225773,-3.96389388586381,332.085294438536));
#29894=CARTESIAN_POINT('Ctrl Pts',(47.4152737942498,-4.04364238505329,332.196975143799));
#29895=CARTESIAN_POINT('Ctrl Pts',(47.4075296659222,-4.1186025216092,332.311822860842));
#29896=CARTESIAN_POINT('Ctrl Pts',(47.399787129472,-4.19354724941406,332.426646969871));
#29897=CARTESIAN_POINT('Ctrl Pts',(47.3920445930219,-4.26370535857375,332.544636468245));
#29898=CARTESIAN_POINT('Ctrl Pts',(47.3843020565717,-4.32880972192682,332.665350250283));
#29899=CARTESIAN_POINT('Ctrl Pts',(47.3765594304384,-4.39391483939484,332.78606543057));
#29900=CARTESIAN_POINT('Ctrl Pts',(47.368816804305,-4.45396590860242,332.909504612914));
#29901=CARTESIAN_POINT('Ctrl Pts',(47.3610741781717,-4.5087417087322,333.035201978208));
#29902=CARTESIAN_POINT('Ctrl Pts',(47.3533297810897,-4.56353003757391,333.1609280939));
#29903=CARTESIAN_POINT('Ctrl Pts',(47.3455853840077,-4.61304054009972,333.288913061565));
#29904=CARTESIAN_POINT('Ctrl Pts',(47.3378409869257,-4.65710025417135,333.418671354494));
#29905=CARTESIAN_POINT('Ctrl Pts',(47.3300883647611,-4.70120676269058,333.548567459658));
#29906=CARTESIAN_POINT('Ctrl Pts',(47.3223357425966,-4.73985079285584,333.68024028102));
#29907=CARTESIAN_POINT('Ctrl Pts',(47.3145831204321,-4.77290922257903,333.81318888802));
#29908=CARTESIAN_POINT('Ctrl Pts',(47.3068263182969,-4.8059854763705,333.946209176738));
#29909=CARTESIAN_POINT('Ctrl Pts',(47.2990695161617,-4.83347005073907,334.080506238446));
#29910=CARTESIAN_POINT('Ctrl Pts',(47.2913127140265,-4.85529123749409,334.215570231561));
#29911=CARTESIAN_POINT('Ctrl Pts',(47.283543580039,-4.87714711581998,334.350848950948));
#29912=CARTESIAN_POINT('Ctrl Pts',(47.2757744460515,-4.89332156925475,334.486896649303));
#29913=CARTESIAN_POINT('Ctrl Pts',(47.2680053120641,-4.90379484877796,334.623198800959));
#29914=CARTESIAN_POINT('Ctrl Pts',(47.2608489575514,-4.91344206316505,334.748750312836));
#29915=CARTESIAN_POINT('Ctrl Pts',(47.2536926030387,-4.91825257170291,334.874517465928));
#29916=CARTESIAN_POINT('Ctrl Pts',(47.246536248526,-4.91824999896793,335.000100756667));
#29917=CARTESIAN_POINT('',(50.7465362485347,-4.9182495281824,334.997845694185));
#29918=CARTESIAN_POINT('Ctrl Pts',(50.7465362484901,-4.91824952818275,334.997845694977));
#29919=CARTESIAN_POINT('Ctrl Pts',(50.7386479016619,-4.91831084118688,335.137822462629));
#29920=CARTESIAN_POINT('Ctrl Pts',(50.7307595548337,-4.91239204902384,335.277775344747));
#29921=CARTESIAN_POINT('Ctrl Pts',(50.7228712080056,-4.90052569889815,335.417170153461));
#29922=CARTESIAN_POINT('Ctrl Pts',(50.7149796963707,-4.88865458798989,335.556620887407));
#29923=CARTESIAN_POINT('Ctrl Pts',(50.707088184736,-4.87083119616067,335.69551273247));
#29924=CARTESIAN_POINT('Ctrl Pts',(50.6991966731011,-4.84713987443125,335.833317526636));
#29925=CARTESIAN_POINT('Ctrl Pts',(50.6913005484341,-4.82343470379245,335.971202875451));
#29926=CARTESIAN_POINT('Ctrl Pts',(50.683404423767,-4.79385483167211,336.107999542287));
#29927=CARTESIAN_POINT('Ctrl Pts',(50.6755082991,-4.75853551509368,336.243190578348));
#29928=CARTESIAN_POINT('Ctrl Pts',(50.6676003404927,-4.72316326537386,336.378584225526));
#29929=CARTESIAN_POINT('Ctrl Pts',(50.6596923818854,-4.68203447918535,336.512367074974));
#29930=CARTESIAN_POINT('Ctrl Pts',(50.6517844232781,-4.63533431358539,336.64403736691));
#29931=CARTESIAN_POINT('Ctrl Pts',(50.6438702478799,-4.58859743494991,336.775811170602));
#29932=CARTESIAN_POINT('Ctrl Pts',(50.6359560724817,-4.53628058314284,336.905468762458));
#29933=CARTESIAN_POINT('Ctrl Pts',(50.6280418970835,-4.47861646679156,337.032529853627));
#29934=CARTESIAN_POINT('Ctrl Pts',(50.6201131041793,-4.42084584464198,337.159825627017));
#29935=CARTESIAN_POINT('Ctrl Pts',(50.612184311275,-4.35770838602701,337.28451498402));
#29936=CARTESIAN_POINT('Ctrl Pts',(50.6042555183708,-4.28948260207043,337.406142570388));
#29937=CARTESIAN_POINT('Ctrl Pts',(50.5976624786309,-4.23275072493055,337.50727971952));
#29938=CARTESIAN_POINT('Ctrl Pts',(50.5910694388909,-4.1725014178184,337.606300241126));
#29939=CARTESIAN_POINT('Ctrl Pts',(50.584476399151,-4.10891655614067,337.702959081668));
#29940=CARTESIAN_POINT('Ctrl Pts',(50.5767013203726,-4.03393182555143,337.816947489064));
#29941=CARTESIAN_POINT('Ctrl Pts',(50.5689262415942,-3.95408165905571,337.927993347852));
#29942=CARTESIAN_POINT('Ctrl Pts',(50.5611511628157,-3.86962420424877,338.035653402546));
#29943=CARTESIAN_POINT('Ctrl Pts',(50.5533856517667,-3.78527067971686,338.143180974689));
#29944=CARTESIAN_POINT('Ctrl Pts',(50.5456201407177,-3.69632138662564,338.247330728178));
#29945=CARTESIAN_POINT('Ctrl Pts',(50.5378546296687,-3.60307858040679,338.347686933677));
#29946=CARTESIAN_POINT('Ctrl Pts',(50.5300968181464,-3.50992822470139,338.447943635707));
#29947=CARTESIAN_POINT('Ctrl Pts',(50.5223390066242,-3.41249309194134,338.544413990468));
#29948=CARTESIAN_POINT('Ctrl Pts',(50.514581195102,-3.31111643715103,338.636714314065));
#29949=CARTESIAN_POINT('Ctrl Pts',(50.506829221579,-3.20981607150857,338.728945178742));
#29950=CARTESIAN_POINT('Ctrl Pts',(50.499077248056,-3.10458037561479,338.817011996363));
#29951=CARTESIAN_POINT('Ctrl Pts',(50.491325274533,-2.99579002805088,338.900567288271));
#29952=CARTESIAN_POINT('Ctrl Pts',(50.4835765839753,-2.8870457532639,338.984087194464));
#29953=CARTESIAN_POINT('Ctrl Pts',(50.4758278934177,-2.77475013028511,339.063099137468));
#29954=CARTESIAN_POINT('Ctrl Pts',(50.4680792028601,-2.65931737261189,339.137295514491));
#29955=CARTESIAN_POINT('Ctrl Pts',(50.4603321244822,-2.54390863168793,339.211476454338));
#29956=CARTESIAN_POINT('Ctrl Pts',(50.4525850461044,-2.42536438295216,339.280843609877));
#29957=CARTESIAN_POINT('Ctrl Pts',(50.4448379677266,-2.30412797960113,339.345132600522));
#29958=CARTESIAN_POINT('Ctrl Pts',(50.4370908244207,-2.18289056017243,339.409422129971));
#29959=CARTESIAN_POINT('Ctrl Pts',(50.429343681115,-2.05896128645139,339.468633226518));
#29960=CARTESIAN_POINT('Ctrl Pts',(50.4215965378092,-1.93280791850323,339.522547579923));
#29961=CARTESIAN_POINT('Ctrl Pts',(50.4138476527811,-1.80662618859973,339.57647405442));
#29962=CARTESIAN_POINT('Ctrl Pts',(50.406098767753,-1.6782197288339,339.625101262596));
#29963=CARTESIAN_POINT('Ctrl Pts',(50.3983498827249,-1.54807569149528,339.668259281135));
#29964=CARTESIAN_POINT('Ctrl Pts',(50.3905927729502,-1.41779351793071,339.71146310804));
#29965=CARTESIAN_POINT('Ctrl Pts',(50.3828356631754,-1.2857704542579,339.74918602594));
#29966=CARTESIAN_POINT('Ctrl Pts',(50.3750785534007,-1.15250874488829,339.781308048584));
#29967=CARTESIAN_POINT('Ctrl Pts',(50.3673172984745,-1.019175824722,339.813447236211));
#29968=CARTESIAN_POINT('Ctrl Pts',(50.3595560435484,-0.884603323275451,
339.83997948931));
#29969=CARTESIAN_POINT('Ctrl Pts',(50.3517947886222,-0.749302075125627,
339.860836292523));
#29970=CARTESIAN_POINT('Ctrl Pts',(50.3440211182175,-0.613784389073338,
339.881726459825));
#29971=CARTESIAN_POINT('Ctrl Pts',(50.3362474478128,-0.477536015459398,
339.896922991618));
#29972=CARTESIAN_POINT('Ctrl Pts',(50.3284737774082,-0.34107218078802,339.906409362252));
#29973=CARTESIAN_POINT('Ctrl Pts',(50.3210619732311,-0.210960770451982,
339.91545414005));
#29974=CARTESIAN_POINT('Ctrl Pts',(50.313650169054,-0.080653794728576,339.919308400497));
#29975=CARTESIAN_POINT('Ctrl Pts',(50.3062383648769,0.0494054387711424,
339.918001846799));
#29976=CARTESIAN_POINT('Ctrl Pts',(50.2984632860985,0.185839262731332,339.916631255013));
#29977=CARTESIAN_POINT('Ctrl Pts',(50.29068820732,0.322431601338373,339.909576832478));
#29978=CARTESIAN_POINT('Ctrl Pts',(50.2829131285416,0.458670013120958,339.896815790038));
#29979=CARTESIAN_POINT('Ctrl Pts',(50.2751476174925,0.594740774864668,339.884070450872));
#29980=CARTESIAN_POINT('Ctrl Pts',(50.2673821064435,0.730458090912218,339.865632500386));
#29981=CARTESIAN_POINT('Ctrl Pts',(50.2596165953945,0.865308797838984,339.841531136622));
#29982=CARTESIAN_POINT('Ctrl Pts',(50.2518587838723,1.00002579989732,339.817453669431));
#29983=CARTESIAN_POINT('Ctrl Pts',(50.24410097235,1.13387752048345,339.787724032034));
#29984=CARTESIAN_POINT('Ctrl Pts',(50.2363431608278,1.26635555663571,339.752423241535));
#29985=CARTESIAN_POINT('Ctrl Pts',(50.2285911873048,1.39873389886383,339.717149016));
#29986=CARTESIAN_POINT('Ctrl Pts',(50.2208392137819,1.52974023809469,339.676312082505));
#29987=CARTESIAN_POINT('Ctrl Pts',(50.2130872402589,1.65887636508962,339.630044521152));
#29988=CARTESIAN_POINT('Ctrl Pts',(50.2053385497013,1.78795780285853,339.583796554138));
#29989=CARTESIAN_POINT('Ctrl Pts',(50.1975898591436,1.91517023649173,339.532122665117));
#29990=CARTESIAN_POINT('Ctrl Pts',(50.189841168586,2.04003084154797,339.475204713534));
#29991=CARTESIAN_POINT('Ctrl Pts',(50.1820940902081,2.16486546831238,339.418298604206));
#29992=CARTESIAN_POINT('Ctrl Pts',(50.1743470118303,2.2873488843468,339.356150764562));
#29993=CARTESIAN_POINT('Ctrl Pts',(50.1665999334525,2.40701884252234,339.288990948258));
#29994=CARTESIAN_POINT('Ctrl Pts',(50.1588527901467,2.52668980364707,339.221830569091));
#29995=CARTESIAN_POINT('Ctrl Pts',(50.1511056468409,2.64354691901748,339.149658320778));
#29996=CARTESIAN_POINT('Ctrl Pts',(50.1433585035352,2.75715347508346,339.072749412539));
#29997=CARTESIAN_POINT('Ctrl Pts',(50.1356096185071,2.87078557231525,338.995823213544));
#29998=CARTESIAN_POINT('Ctrl Pts',(50.1278607334789,2.98116533242721,338.914158454669));
#29999=CARTESIAN_POINT('Ctrl Pts',(50.1201118484508,3.08788623721916,338.828072837407));
#30000=CARTESIAN_POINT('Ctrl Pts',(50.1123547386761,3.1947204166823,338.741895847982));
#30001=CARTESIAN_POINT('Ctrl Pts',(50.1045976289014,3.29788767836247,338.651288872566));
#30002=CARTESIAN_POINT('Ctrl Pts',(50.0968405191267,3.39701532999277,338.556609327758));
#30003=CARTESIAN_POINT('Ctrl Pts',(50.0890792642005,3.49619595227048,338.461879189228));
#30004=CARTESIAN_POINT('Ctrl Pts',(50.0813180092743,3.5913323922436,338.363072426356));
#30005=CARTESIAN_POINT('Ctrl Pts',(50.0735567543482,3.68209059198383,338.260581533243));
#30006=CARTESIAN_POINT('Ctrl Pts',(50.0657830839435,3.77299397526568,338.157926688103));
#30007=CARTESIAN_POINT('Ctrl Pts',(50.0580094135389,3.85950487594716,338.05157623933));
#30008=CARTESIAN_POINT('Ctrl Pts',(50.0502357431342,3.9413305786295,337.941954508904));
#30009=CARTESIAN_POINT('Ctrl Pts',(50.0428239389572,4.01934727516536,337.837435696404));
#30010=CARTESIAN_POINT('Ctrl Pts',(50.0354121347801,4.09310498657809,337.729943542026));
#30011=CARTESIAN_POINT('Ctrl Pts',(50.0280003306031,4.16238879174328,337.619866906709));
#30012=CARTESIAN_POINT('Ctrl Pts',(50.0202252518246,4.23506840258589,337.504395087593));
#30013=CARTESIAN_POINT('Ctrl Pts',(50.0124501730462,4.30305414026398,337.385714123173));
#30014=CARTESIAN_POINT('Ctrl Pts',(50.0046750942678,4.36604952940482,337.264242603893));
#30015=CARTESIAN_POINT('Ctrl Pts',(49.9969095832188,4.42896739870875,337.142920563051));
#30016=CARTESIAN_POINT('Ctrl Pts',(49.9891440721698,4.4869069599596,337.018815143608));
#30017=CARTESIAN_POINT('Ctrl Pts',(49.9813785611207,4.53961506424028,336.892373676371));
#30018=CARTESIAN_POINT('Ctrl Pts',(49.9736207495985,4.59227090828222,336.766057576217));
#30019=CARTESIAN_POINT('Ctrl Pts',(49.9658629380764,4.63970546836064,336.637410396094));
#30020=CARTESIAN_POINT('Ctrl Pts',(49.9581051265542,4.68171174747052,336.506903505901));
#30021=CARTESIAN_POINT('Ctrl Pts',(49.9503531530312,4.72368641552299,336.376494826282));
#30022=CARTESIAN_POINT('Ctrl Pts',(49.9426011795082,4.76024081422956,336.244229592789));
#30023=CARTESIAN_POINT('Ctrl Pts',(49.9348492059852,4.79121640295882,336.110598236321));
#30024=CARTESIAN_POINT('Ctrl Pts',(49.9271005154276,4.82217887350806,335.97702347281));
#30025=CARTESIAN_POINT('Ctrl Pts',(49.91935182487,4.84756714510293,335.842084117013));
#30026=CARTESIAN_POINT('Ctrl Pts',(49.9116031343124,4.86727286322162,335.706284600884));
#30027=CARTESIAN_POINT('Ctrl Pts',(49.9038560559346,4.88697448140102,335.570513338979));
#30028=CARTESIAN_POINT('Ctrl Pts',(49.8961089775568,4.90099584169176,335.433882659294));
#30029=CARTESIAN_POINT('Ctrl Pts',(49.8883618991789,4.90928000040002,335.296905608186));
#30030=CARTESIAN_POINT('Ctrl Pts',(49.8806147558731,4.91756422853751,335.159927409079));
#30031=CARTESIAN_POINT('Ctrl Pts',(49.8728676125673,4.92011113559047,335.022603222922));
#30032=CARTESIAN_POINT('Ctrl Pts',(49.8651204692615,4.91691582010293,334.885449222956));
#30033=CARTESIAN_POINT('Ctrl Pts',(49.8573715842335,4.91371978624064,334.748264387859));
#30034=CARTESIAN_POINT('Ctrl Pts',(49.8496226992053,4.90477897004681,334.611250205781));
#30035=CARTESIAN_POINT('Ctrl Pts',(49.8418738141772,4.89014054316272,334.474920453059));
#30036=CARTESIAN_POINT('Ctrl Pts',(49.8341167044025,4.8754865789011,334.338445998528));
#30037=CARTESIAN_POINT('Ctrl Pts',(49.8263595946278,4.85512296529114,334.20265781378));
#30038=CARTESIAN_POINT('Ctrl Pts',(49.8186024848531,4.82914857640288,334.068062722322));
#30039=CARTESIAN_POINT('Ctrl Pts',(49.8108412299269,4.80316030763167,333.93339570755));
#30040=CARTESIAN_POINT('Ctrl Pts',(49.8030799750008,4.77155537937993,333.799923436608));
#30041=CARTESIAN_POINT('Ctrl Pts',(49.7953187200746,4.73448307039813,333.668139227016));
#30042=CARTESIAN_POINT('Ctrl Pts',(49.78754504967,4.69735145780381,333.536144205637));
#30043=CARTESIAN_POINT('Ctrl Pts',(49.7797713792653,4.65473510889653,333.405843013406));
#30044=CARTESIAN_POINT('Ctrl Pts',(49.7719977088606,4.60683243998393,333.277711425918));
#30045=CARTESIAN_POINT('Ctrl Pts',(49.7645859046835,4.56115965183345,333.155544394654));
#30046=CARTESIAN_POINT('Ctrl Pts',(49.7571741005063,4.51068173583416,333.035349788941));
#30047=CARTESIAN_POINT('Ctrl Pts',(49.7497622963291,4.45560938729194,332.917518775505));
#30048=CARTESIAN_POINT('Ctrl Pts',(49.7419872175507,4.39783777889631,332.7939125131));
#30049=CARTESIAN_POINT('Ctrl Pts',(49.7342121387723,4.33482740764643,332.672516776115));
#30050=CARTESIAN_POINT('Ctrl Pts',(49.7264370599938,4.26676983534172,332.553807400322));
#30051=CARTESIAN_POINT('Ctrl Pts',(49.7186715489448,4.1987960122124,332.435244103974));
#30052=CARTESIAN_POINT('Ctrl Pts',(49.7109060378958,4.12578753849365,332.319360927203));
#30053=CARTESIAN_POINT('Ctrl Pts',(49.7031405268468,4.04798359080069,332.206612824704));
#30054=CARTESIAN_POINT('Ctrl Pts',(49.6953827153246,3.97025678594811,332.093976512276));
#30055=CARTESIAN_POINT('Ctrl Pts',(49.6876249038024,3.88774418986797,331.984469407796));
#30056=CARTESIAN_POINT('Ctrl Pts',(49.6798670922801,3.80073016960812,331.87852066476));
#30057=CARTESIAN_POINT('Ctrl Pts',(49.6721151187571,3.7137816301583,331.772651651514));
#30058=CARTESIAN_POINT('Ctrl Pts',(49.6643631452341,3.62233865618957,331.670335970566));
#30059=CARTESIAN_POINT('Ctrl Pts',(49.6566111717111,3.52672786607519,331.571972342418));
#30060=CARTESIAN_POINT('Ctrl Pts',(49.6488624811535,3.43115756718693,331.473650371324));
#30061=CARTESIAN_POINT('Ctrl Pts',(49.6411137905959,3.33142323463103,331.379277403864));
#30062=CARTESIAN_POINT('Ctrl Pts',(49.6333651000382,3.22789041915044,331.289217534743));
#30063=CARTESIAN_POINT('Ctrl Pts',(49.6256180216604,3.12437914453698,331.19917640333));
#30064=CARTESIAN_POINT('Ctrl Pts',(49.6178709432826,3.01707125370011,331.113446841685));
#30065=CARTESIAN_POINT('Ctrl Pts',(49.6101238649048,2.90636736276843,331.032354373796));
#30066=CARTESIAN_POINT('Ctrl Pts',(49.602376721599,2.79566254403151,330.951261226275));
#30067=CARTESIAN_POINT('Ctrl Pts',(49.5946295782931,2.68156198375639,330.874805481008));
#30068=CARTESIAN_POINT('Ctrl Pts',(49.5868824349873,2.56449709057508,330.803270590694));
#30069=CARTESIAN_POINT('Ctrl Pts',(49.5791335499592,2.44740587872018,330.731719617818));
#30070=CARTESIAN_POINT('Ctrl Pts',(49.5713846649311,2.32734934127482,330.665091905105));
#30071=CARTESIAN_POINT('Ctrl Pts',(49.563635779903,2.2047850510028,330.603625818771));
#30072=CARTESIAN_POINT('Ctrl Pts',(49.5558786701283,2.08209066972701,330.542094491699));
#30073=CARTESIAN_POINT('Ctrl Pts',(49.5481215603535,1.9568835684702,330.48573591053));
#30074=CARTESIAN_POINT('Ctrl Pts',(49.5403644505788,1.82964345236461,330.434741201233));
#30075=CARTESIAN_POINT('Ctrl Pts',(49.5326031956526,1.70233534320933,330.383719241993));
#30076=CARTESIAN_POINT('Ctrl Pts',(49.5248419407265,1.57299242290108,330.338066995978));
#30077=CARTESIAN_POINT('Ctrl Pts',(49.5170806858003,1.4421103159632,330.297925893917));
#30078=CARTESIAN_POINT('Ctrl Pts',(49.5093070153956,1.31101884030859,330.257720579175));
#30079=CARTESIAN_POINT('Ctrl Pts',(49.501533344991,1.17838363618827,330.223044124354));
#30080=CARTESIAN_POINT('Ctrl Pts',(49.4937596745863,1.04471216789936,330.193987146423));
#30081=CARTESIAN_POINT('Ctrl Pts',(49.4863478704093,0.91726313861926,330.166282777806));
#30082=CARTESIAN_POINT('Ctrl Pts',(49.4789360662322,0.78887243366812,330.143686536353));
#30083=CARTESIAN_POINT('Ctrl Pts',(49.4715242620551,0.659983012809761,330.126232926647));
#30084=CARTESIAN_POINT('Ctrl Pts',(49.4637491832767,0.524776337492697,330.107923863537));
#30085=CARTESIAN_POINT('Ctrl Pts',(49.4559741044982,0.388593544978953,330.09521643002));
#30086=CARTESIAN_POINT('Ctrl Pts',(49.4481990257198,0.251938440804253,330.088207039731));
#30087=CARTESIAN_POINT('Ctrl Pts',(49.4404335146707,0.115451499434481,330.081206274944));
#30088=CARTESIAN_POINT('Ctrl Pts',(49.4326680036217,-0.0215062105264285,
330.079889621736));
#30089=CARTESIAN_POINT('Ctrl Pts',(49.4249024925726,-0.158422675780561,
330.084302153478));
#30090=CARTESIAN_POINT('Ctrl Pts',(49.4171446810504,-0.295203387959936,
330.088710310183));
#30091=CARTESIAN_POINT('Ctrl Pts',(49.4093868695282,-0.431942548659525,
330.098836334805));
#30092=CARTESIAN_POINT('Ctrl Pts',(49.4016290580061,-0.568125386221159,
330.11467333661));
#30093=CARTESIAN_POINT('Ctrl Pts',(49.3938770844831,-0.704205741878459,
330.130498420569));
#30094=CARTESIAN_POINT('Ctrl Pts',(49.3861251109601,-0.839730221007358,
330.152025882396));
#30095=CARTESIAN_POINT('Ctrl Pts',(49.3783731374371,-0.974186779090219,
330.179196832275));
#30096=CARTESIAN_POINT('Ctrl Pts',(49.3706244468795,-1.10858639474154,330.206356275241));
#30097=CARTESIAN_POINT('Ctrl Pts',(49.3628757563218,-1.24191860653802,330.239154375414));
#30098=CARTESIAN_POINT('Ctrl Pts',(49.3551270657642,-1.37367941899319,330.277480765912));
#30099=CARTESIAN_POINT('Ctrl Pts',(49.3473799873864,-1.50541281751075,330.315799182284));
#30100=CARTESIAN_POINT('Ctrl Pts',(49.3396329090086,-1.63557509191617,330.359643492034));
#30101=CARTESIAN_POINT('Ctrl Pts',(49.3318858306307,-1.76367570576659,330.408852968224));
#30102=CARTESIAN_POINT('Ctrl Pts',(49.324138687325,-1.89177739322301,330.458062856836));
#30103=CARTESIAN_POINT('Ctrl Pts',(49.3163915440191,-2.01781702078277,330.512637861406));
#30104=CARTESIAN_POINT('Ctrl Pts',(49.3086444007133,-2.14132276705989,330.572368593732));
#30105=CARTESIAN_POINT('Ctrl Pts',(49.3008955156853,-2.26485628005096,330.632112754795));
#30106=CARTESIAN_POINT('Ctrl Pts',(49.2931466306572,-2.38585442636517,330.69701477998));
#30107=CARTESIAN_POINT('Ctrl Pts',(49.2853977456291,-2.50386913988776,330.766818880225));
#30108=CARTESIAN_POINT('Ctrl Pts',(49.2776406358544,-2.62200911544685,330.836697071264));
#30109=CARTESIAN_POINT('Ctrl Pts',(49.2698835260797,-2.73715899558075,330.911487531762));
#30110=CARTESIAN_POINT('Ctrl Pts',(49.2621264163049,-2.84889846241441,330.990890296668));
#30111=CARTESIAN_POINT('Ctrl Pts',(49.2543651613788,-2.96069763924648,331.070335491872));
#30112=CARTESIAN_POINT('Ctrl Pts',(49.2466039064526,-3.0690824627426,331.154397663125));
#30113=CARTESIAN_POINT('Ctrl Pts',(49.2388426515264,-3.1736657899163,331.242736565475));
#30114=CARTESIAN_POINT('Ctrl Pts',(49.2310689811218,-3.27841641632978,331.33121678128));
#30115=CARTESIAN_POINT('Ctrl Pts',(49.2232953107171,-3.37935310653415,331.423987134635));
#30116=CARTESIAN_POINT('Ctrl Pts',(49.2155216403125,-3.47612504073809,331.520669926027));
#30117=CARTESIAN_POINT('Ctrl Pts',(49.2081098361354,-3.56839221812225,331.612852110219));
#30118=CARTESIAN_POINT('Ctrl Pts',(49.2006980319584,-3.65687345713565,331.708590470285));
#30119=CARTESIAN_POINT('Ctrl Pts',(49.1932862277814,-3.74130003119369,331.80753118432));
#30120=CARTESIAN_POINT('Ctrl Pts',(49.1855629235076,-3.82927484875019,331.910630135843));
#30121=CARTESIAN_POINT('Ctrl Pts',(49.1778396192339,-3.91313527088013,332.017544756288));
#30122=CARTESIAN_POINT('Ctrl Pts',(49.1701163149601,-3.99252856049073,332.127910385074));
#30123=CARTESIAN_POINT('Ctrl Pts',(49.1624054455346,-4.07179402352995,332.238098320506));
#30124=CARTESIAN_POINT('Ctrl Pts',(49.1546945761091,-4.14660644630111,332.351725881446));
#30125=CARTESIAN_POINT('Ctrl Pts',(49.1469837066835,-4.21665188104645,332.468393795124));
#30126=CARTESIAN_POINT('Ctrl Pts',(49.1392800286901,-4.28663198891882,332.584952900141));
#30127=CARTESIAN_POINT('Ctrl Pts',(49.1315763506966,-4.35185374767205,332.704546381286));
#30128=CARTESIAN_POINT('Ctrl Pts',(49.1238726727032,-4.41204511106492,332.826744147499));
#30129=CARTESIAN_POINT('Ctrl Pts',(49.1161744546254,-4.47219381434558,332.948855307095));
#30130=CARTESIAN_POINT('Ctrl Pts',(49.1084762365477,-4.5273190398065,333.073566725879));
#30131=CARTESIAN_POINT('Ctrl Pts',(49.1007780184699,-4.57719374991476,333.200422149991));
#30132=CARTESIAN_POINT('Ctrl Pts',(49.0930835331751,-4.62704427631365,333.327216063276));
#30133=CARTESIAN_POINT('Ctrl Pts',(49.0853890478803,-4.67164920880391,333.456151544821));
#30134=CARTESIAN_POINT('Ctrl Pts',(49.0776945625855,-4.71082909366054,333.586751149719));
#30135=CARTESIAN_POINT('Ctrl Pts',(49.0700007301838,-4.75000565402211,333.717339672967));
#30136=CARTESIAN_POINT('Ctrl Pts',(49.0623068977822,-4.78375796038099,333.849591661466));
#30137=CARTESIAN_POINT('Ctrl Pts',(49.0546130653805,-4.81195608938995,333.983013443411));
#30138=CARTESIAN_POINT('Ctrl Pts',(49.0469196794052,-4.84015258223297,334.116427483701));
#30139=CARTESIAN_POINT('Ctrl Pts',(49.0392262934298,-4.86279546241927,334.25101079316));
#30140=CARTESIAN_POINT('Ctrl Pts',(49.0315329074544,-4.87980586329072,334.38625917596));
#30141=CARTESIAN_POINT('Ctrl Pts',(49.0238358959717,-4.89682428031193,334.521571294547));
#30142=CARTESIAN_POINT('Ctrl Pts',(49.0161388844889,-4.90820487232326,334.657548718119));
#30143=CARTESIAN_POINT('Ctrl Pts',(49.0084418730062,-4.91392062046323,334.793681803308));
#30144=CARTESIAN_POINT('Ctrl Pts',(49.0044733315008,-4.91686763227146,334.863871356752));
#30145=CARTESIAN_POINT('Ctrl Pts',(49.0005047899955,-4.91830956042976,334.934102250792));
#30146=CARTESIAN_POINT('Ctrl Pts',(48.9965362484901,-4.91824811618314,335.004304667347));
#30147=CARTESIAN_POINT('',(52.4965362484542,-4.91824882173218,334.996595586683));
#30148=CARTESIAN_POINT('Ctrl Pts',(52.4965362484542,-4.91824882173218,334.996595586683));
#30149=CARTESIAN_POINT('Ctrl Pts',(52.4888775572962,-4.91834206568241,335.131302188295));
#30150=CARTESIAN_POINT('Ctrl Pts',(52.4812188661381,-4.91289690048249,335.266224549053));
#30151=CARTESIAN_POINT('Ctrl Pts',(52.47356017498,-4.9018866689054,335.400861756354));
#30152=CARTESIAN_POINT('Ctrl Pts',(52.4659095597492,-4.8908880473839,335.535356991577));
#30153=CARTESIAN_POINT('Ctrl Pts',(52.4582589445185,-4.87433606304535,335.669567273004));
#30154=CARTESIAN_POINT('Ctrl Pts',(52.4506083292877,-4.85225607951328,335.802990660797));
#30155=CARTESIAN_POINT('Ctrl Pts',(52.4429638300524,-4.8301937469903,335.9363073883));
#30156=CARTESIAN_POINT('Ctrl Pts',(52.4353193308171,-4.8026122716787,336.068838077947));
#30157=CARTESIAN_POINT('Ctrl Pts',(52.4276748315818,-4.76958887882669,336.200085409241));
#30158=CARTESIAN_POINT('Ctrl Pts',(52.4200339012011,-4.73658090303234,336.331271467374));
#30159=CARTESIAN_POINT('Ctrl Pts',(52.4123929708203,-4.69813615873357,336.46117496852));
#30160=CARTESIAN_POINT('Ctrl Pts',(52.4047520404396,-4.65438298141709,336.589308693991));
#30161=CARTESIAN_POINT('Ctrl Pts',(52.3971128016806,-4.61063949059459,336.717414052001));
#30162=CARTESIAN_POINT('Ctrl Pts',(52.3894735629215,-4.56159003326485,336.843750032233));
#30163=CARTESIAN_POINT('Ctrl Pts',(52.3818343241625,-4.50741267909441,336.967845014944));
#30164=CARTESIAN_POINT('Ctrl Pts',(52.3741950142381,-4.45323482022019,337.091941153695));
#30165=CARTESIAN_POINT('Ctrl Pts',(52.3665557043138,-4.39392913095153,337.213795884254));
#30166=CARTESIAN_POINT('Ctrl Pts',(52.3589163943894,-4.3297214253522,337.332958516851));
#30167=CARTESIAN_POINT('Ctrl Pts',(52.3512752506671,-4.26549830684867,337.452149754148));
#30168=CARTESIAN_POINT('Ctrl Pts',(52.3436341069449,-4.19637102359047,337.568647254121));
#30169=CARTESIAN_POINT('Ctrl Pts',(52.3359929632226,-4.12261055905108,337.682026331135));
#30170=CARTESIAN_POINT('Ctrl Pts',(52.3283438794186,-4.04877344837884,337.795523222859));
#30171=CARTESIAN_POINT('Ctrl Pts',(52.3206947956146,-3.97029376465579,337.905894884365));
#30172=CARTESIAN_POINT('Ctrl Pts',(52.3130457118107,-3.88748507880771,338.012746724261));
#30173=CARTESIAN_POINT('Ctrl Pts',(52.305392237099,-3.8046288571621,338.119659901775));
#30174=CARTESIAN_POINT('Ctrl Pts',(52.2977387623873,-3.71743894559341,338.223048928115));
#30175=CARTESIAN_POINT('Ctrl Pts',(52.2900852876756,-3.62626726704912,338.322554554921));
#30176=CARTESIAN_POINT('Ctrl Pts',(52.282420522707,-3.53496109382011,338.422206970491));
#30177=CARTESIAN_POINT('Ctrl Pts',(52.2747557577385,-3.43966171024998,338.517964264827));
#30178=CARTESIAN_POINT('Ctrl Pts',(52.2670909927699,-3.34075603402147,338.609505808784));
#30179=CARTESIAN_POINT('Ctrl Pts',(52.2626955301115,-3.28403724246679,338.662001539548));
#30180=CARTESIAN_POINT('Ctrl Pts',(52.2583000674531,-3.22613307481586,338.713111638871));
#30181=CARTESIAN_POINT('Ctrl Pts',(52.2539046047947,-3.16712081781979,338.762782054256));
#30182=CARTESIAN_POINT('Ctrl Pts',(52.2461295260163,-3.0627347764188,338.850643429176));
#30183=CARTESIAN_POINT('Ctrl Pts',(52.2383544472378,-2.95452487634904,338.934296578371));
#30184=CARTESIAN_POINT('Ctrl Pts',(52.2305793684594,-2.84286498459752,339.013390305197));
#30185=CARTESIAN_POINT('Ctrl Pts',(52.2228138574103,-2.73134249745118,339.092386702157));
#30186=CARTESIAN_POINT('Ctrl Pts',(52.2150483463614,-2.61637878173231,339.166834616576));
#30187=CARTESIAN_POINT('Ctrl Pts',(52.2072828353123,-2.49838212722402,339.236421816683));
#30188=CARTESIAN_POINT('Ctrl Pts',(52.1995250237901,-2.38050246674245,339.305940020878));
#30189=CARTESIAN_POINT('Ctrl Pts',(52.1917672122679,-2.25959618642276,339.370606904387));
#30190=CARTESIAN_POINT('Ctrl Pts',(52.1840094007457,-2.13610173055205,339.430152645139));
#30191=CARTESIAN_POINT('Ctrl Pts',(52.1762574272226,-2.01270020817519,339.489653575833));
#30192=CARTESIAN_POINT('Ctrl Pts',(52.1685054536996,-1.8867147376829,339.544040865534));
#30193=CARTESIAN_POINT('Ctrl Pts',(52.1607534801766,-1.75860930377084,339.5930900687));
#30194=CARTESIAN_POINT('Ctrl Pts',(52.1530047896189,-1.63055812258654,339.6421184995));
#30195=CARTESIAN_POINT('Ctrl Pts',(52.1452560990614,-1.50038912792764,339.685813200631));
#30196=CARTESIAN_POINT('Ctrl Pts',(52.1375074085038,-1.36858707073141,339.723997511888));
#30197=CARTESIAN_POINT('Ctrl Pts',(52.1297603301259,-1.23681243605401,339.762173878581));
#30198=CARTESIAN_POINT('Ctrl Pts',(52.122013251748,-1.10340578987091,339.794842027137));
#30199=CARTESIAN_POINT('Ctrl Pts',(52.1142661733702,-0.968867482173869,
339.821875036175));
#30200=CARTESIAN_POINT('Ctrl Pts',(52.1065190300644,-0.834328046916041,
339.848908271776));
#30201=CARTESIAN_POINT('Ctrl Pts',(52.0987718867586,-0.698657314441851,
339.87030619666));
#30202=CARTESIAN_POINT('Ctrl Pts',(52.0910247434527,-0.562365885146263,
339.885993007949));
#30203=CARTESIAN_POINT('Ctrl Pts',(52.0832758584246,-0.426043814644006,
339.901683345966));
#30204=CARTESIAN_POINT('Ctrl Pts',(52.0755269733965,-0.289101157874568,
339.911659970726));
#30205=CARTESIAN_POINT('Ctrl Pts',(52.0677780883684,-0.152053298517322,
339.915898987663));
#30206=CARTESIAN_POINT('Ctrl Pts',(52.0600209785937,-0.0148599751461849,
339.920142503937));
#30207=CARTESIAN_POINT('Ctrl Pts',(52.0522638688189,0.122438382565781,339.918636235025));
#30208=CARTESIAN_POINT('Ctrl Pts',(52.0445067590442,0.25932617128518,339.911408453732));
#30209=CARTESIAN_POINT('Ctrl Pts',(52.036745504118,0.396287108462141,339.904176810143));
#30210=CARTESIAN_POINT('Ctrl Pts',(52.0289842491918,0.53283665055394,339.891217598954));
#30211=CARTESIAN_POINT('Ctrl Pts',(52.0212229942656,0.668465643909878,339.872610875641));
#30212=CARTESIAN_POINT('Ctrl Pts',(52.013449323861,0.804311599453707,339.853974387634));
#30213=CARTESIAN_POINT('Ctrl Pts',(52.0056756534563,0.939233678728462,339.829672403864));
#30214=CARTESIAN_POINT('Ctrl Pts',(51.9979019830517,1.07273334956113,339.799836062121));
#30215=CARTESIAN_POINT('Ctrl Pts',(51.9904901788746,1.20001857859784,339.771388609265));
#30216=CARTESIAN_POINT('Ctrl Pts',(51.9830783746975,1.32601056710423,339.73791052572));
#30217=CARTESIAN_POINT('Ctrl Pts',(51.9756665705205,1.45029290098457,339.69955674121));
#30218=CARTESIAN_POINT('Ctrl Pts',(51.967891491742,1.5806666822669,339.659323123471));
#30219=CARTESIAN_POINT('Ctrl Pts',(51.9601164129636,1.70957098609738,339.613596628992));
#30220=CARTESIAN_POINT('Ctrl Pts',(51.9523413341851,1.83650816284588,339.562501597841));
#30221=CARTESIAN_POINT('Ctrl Pts',(51.9445758231361,1.96328913531692,339.511469442379));
#30222=CARTESIAN_POINT('Ctrl Pts',(51.9368103120871,2.08810743802025,339.4550820395));
#30223=CARTESIAN_POINT('Ctrl Pts',(51.9290448010381,2.21047955956878,339.393513762267));
#30224=CARTESIAN_POINT('Ctrl Pts',(51.9212869895159,2.33273034880319,339.332006530159));
#30225=CARTESIAN_POINT('Ctrl Pts',(51.9135291779937,2.45253943663542,339.265328820867));
#30226=CARTESIAN_POINT('Ctrl Pts',(51.9057713664715,2.56944265656888,339.193703315341));
#30227=CARTESIAN_POINT('Ctrl Pts',(51.8980193929485,2.68625790312165,339.12213171028));
#30228=CARTESIAN_POINT('Ctrl Pts',(51.8902674194254,2.80017130246058,339.04561992356));
#30229=CARTESIAN_POINT('Ctrl Pts',(51.8825154459024,2.91074302479976,338.96443666945));
#30230=CARTESIAN_POINT('Ctrl Pts',(51.8747667553448,3.02126791994889,338.883287796496));
#30231=CARTESIAN_POINT('Ctrl Pts',(51.8670180647872,3.12845363842076,338.797471621837));
#30232=CARTESIAN_POINT('Ctrl Pts',(51.8592693742296,3.23188929633324,338.707300181904));
#30233=CARTESIAN_POINT('Ctrl Pts',(51.8515222958517,3.33530343359317,338.617147502892));
#30234=CARTESIAN_POINT('Ctrl Pts',(51.8437752174739,3.43496876777921,338.522641617692));
#30235=CARTESIAN_POINT('Ctrl Pts',(51.8360281390961,3.53050779990477,338.424134596845));
#30236=CARTESIAN_POINT('Ctrl Pts',(51.8282809957903,3.62604763273911,338.325626750415));
#30237=CARTESIAN_POINT('Ctrl Pts',(51.8205338524845,3.71746082240527,338.223117982037));
#30238=CARTESIAN_POINT('Ctrl Pts',(51.8127867091787,3.8044073094734,338.11699664519));
#30239=CARTESIAN_POINT('Ctrl Pts',(51.8050378241506,3.89137334395804,338.010851450013));
#30240=CARTESIAN_POINT('Ctrl Pts',(51.7972889391225,3.97387042990715,337.901092372509));
#30241=CARTESIAN_POINT('Ctrl Pts',(51.7895400540944,4.05159957018778,337.788139879087));
#30242=CARTESIAN_POINT('Ctrl Pts',(51.7817829443197,4.12941121298095,337.675067496721));
#30243=CARTESIAN_POINT('Ctrl Pts',(51.774025834545,4.2024445788538,337.558795250051));
#30244=CARTESIAN_POINT('Ctrl Pts',(51.7662687247703,4.27044442046223,337.439772020957));
#30245=CARTESIAN_POINT('Ctrl Pts',(51.7585074698441,4.33848059901175,337.320685189654));
#30246=CARTESIAN_POINT('Ctrl Pts',(51.7507462149179,4.40147771428681,337.198844793779));
#30247=CARTESIAN_POINT('Ctrl Pts',(51.7429849599917,4.45922755439041,337.07472231411));
#30248=CARTESIAN_POINT('Ctrl Pts',(51.7352112895871,4.51706977541754,336.950401278925));
#30249=CARTESIAN_POINT('Ctrl Pts',(51.7274376191824,4.56964779772785,336.823791226161));
#30250=CARTESIAN_POINT('Ctrl Pts',(51.7196639487778,4.61680211352313,336.695382348342));
#30251=CARTESIAN_POINT('Ctrl Pts',(51.7122521446007,4.66176138457331,336.572950934679));
#30252=CARTESIAN_POINT('Ctrl Pts',(51.7048403404237,4.70179044429626,336.448884671644));
#30253=CARTESIAN_POINT('Ctrl Pts',(51.6974285362466,4.73679423084125,336.323617572099));
#30254=CARTESIAN_POINT('Ctrl Pts',(51.6896534574682,4.77351365723589,336.192210758853));
#30255=CARTESIAN_POINT('Ctrl Pts',(51.6818783786898,4.80481878782615,336.059067149761));
#30256=CARTESIAN_POINT('Ctrl Pts',(51.6741032999113,4.83054487605908,335.924672516559));
#30257=CARTESIAN_POINT('Ctrl Pts',(51.6663377888623,4.85623930670258,335.79044326451));
#30258=CARTESIAN_POINT('Ctrl Pts',(51.6585722778133,4.87636828231503,335.654966431679));
#30259=CARTESIAN_POINT('Ctrl Pts',(51.6508067667643,4.89081678116865,335.518742976376));
#30260=CARTESIAN_POINT('Ctrl Pts',(51.6430489552421,4.90525095429364,335.382654587025));
#30261=CARTESIAN_POINT('Ctrl Pts',(51.6352911437199,4.91401581811348,335.245821434588));
#30262=CARTESIAN_POINT('Ctrl Pts',(51.6275333321977,4.91704744266493,335.108754352015));
#30263=CARTESIAN_POINT('Ctrl Pts',(51.6197813586747,4.92007678582278,334.971790416768));
#30264=CARTESIAN_POINT('Ctrl Pts',(51.6120293851516,4.91738146879444,334.834593290988));
#30265=CARTESIAN_POINT('Ctrl Pts',(51.6042774116286,4.90894944200643,334.697678253636));
#30266=CARTESIAN_POINT('Ctrl Pts',(51.596528721071,4.9005209861868,334.560821199883));
#30267=CARTESIAN_POINT('Ctrl Pts',(51.5887800305134,4.88636067668862,334.424246386274));
#30268=CARTESIAN_POINT('Ctrl Pts',(51.5810313399558,4.86650855875888,334.288468194649));
#30269=CARTESIAN_POINT('Ctrl Pts',(51.573284261578,4.84666057122808,334.15271825281));
#30270=CARTESIAN_POINT('Ctrl Pts',(51.5655371832001,4.82112318729248,334.017764989798));
#30271=CARTESIAN_POINT('Ctrl Pts',(51.5577901048223,4.78998818421876,333.884116378136));
#30272=CARTESIAN_POINT('Ctrl Pts',(51.5500429615165,4.75885292020376,333.75046664637));
#30273=CARTESIAN_POINT('Ctrl Pts',(51.5422958182107,4.72212003216232,333.618121968443));
#30274=CARTESIAN_POINT('Ctrl Pts',(51.5345486749049,4.6799320691492,333.487578467937));
#30275=CARTESIAN_POINT('Ctrl Pts',(51.5267997898768,4.63773462138643,333.35700561848));
#30276=CARTESIAN_POINT('Ctrl Pts',(51.5190509048487,4.59007977839495,333.228235124096));
#30277=CARTESIAN_POINT('Ctrl Pts',(51.5113020198206,4.53715931484396,333.101745956352));
#30278=CARTESIAN_POINT('Ctrl Pts',(51.5035449100459,4.48418268096593,332.975122531699));
#30279=CARTESIAN_POINT('Ctrl Pts',(51.4957878002712,4.42592941310896,332.850785631865));
#30280=CARTESIAN_POINT('Ctrl Pts',(51.4880306904965,4.36263885663847,332.729192815528));
#30281=CARTESIAN_POINT('Ctrl Pts',(51.4802694355703,4.29931447971815,332.607535023879));
#30282=CARTESIAN_POINT('Ctrl Pts',(51.4725081806441,4.23094764532456,332.48862457625));
#30283=CARTESIAN_POINT('Ctrl Pts',(51.4647469257179,4.15782215629907,332.372891707773));
#30284=CARTESIAN_POINT('Ctrl Pts',(51.4569732553133,4.08457969032283,332.256973704423));
#30285=CARTESIAN_POINT('Ctrl Pts',(51.4491995849086,4.00656358064499,332.144243759326));
#30286=CARTESIAN_POINT('Ctrl Pts',(51.441425914504,3.92409972179423,332.035101277292));
#30287=CARTESIAN_POINT('Ctrl Pts',(51.4340141103269,3.84547457541285,331.931039404056));
#30288=CARTESIAN_POINT('Ctrl Pts',(51.4266023061498,3.76280662907251,331.830238739903));
#30289=CARTESIAN_POINT('Ctrl Pts',(51.4191905019727,3.6764094100248,331.733014093636));
#30290=CARTESIAN_POINT('Ctrl Pts',(51.4114154231943,3.58577760590738,331.631024177838));
#30291=CARTESIAN_POINT('Ctrl Pts',(51.4036403444159,3.4907553069779,331.532647379));
#30292=CARTESIAN_POINT('Ctrl Pts',(51.3958652656375,3.39166185524052,331.438285114975));
#30293=CARTESIAN_POINT('Ctrl Pts',(51.3880997545885,3.29269034430423,331.344038969724));
#30294=CARTESIAN_POINT('Ctrl Pts',(51.3803342435395,3.18965792900957,331.253797796795));
#30295=CARTESIAN_POINT('Ctrl Pts',(51.3725687324905,3.08292363102994,331.167929417699));
#30296=CARTESIAN_POINT('Ctrl Pts',(51.3648109209683,2.97629516041743,331.082146177351));
#30297=CARTESIAN_POINT('Ctrl Pts',(51.3570531094461,2.86597241406727,331.000727346107));
#30298=CARTESIAN_POINT('Ctrl Pts',(51.349295297924,2.75235036613324,330.924003125057));
#30299=CARTESIAN_POINT('Ctrl Pts',(51.341543324401,2.6388138223936,330.847336641416));
#30300=CARTESIAN_POINT('Ctrl Pts',(51.333791350878,2.52198324165249,330.775357953879));
#30301=CARTESIAN_POINT('Ctrl Pts',(51.326039377355,2.40228541226457,330.7083560422));
#30302=CARTESIAN_POINT('Ctrl Pts',(51.3182906867974,2.28263827497823,330.64138250587));
#30303=CARTESIAN_POINT('Ctrl Pts',(51.3105419962398,2.16012664453082,330.579381743919));
#30304=CARTESIAN_POINT('Ctrl Pts',(51.3027933056822,2.03520474636636,330.522598442973));
#30305=CARTESIAN_POINT('Ctrl Pts',(51.2950462273044,1.91030883924635,330.465826956267));
#30306=CARTESIAN_POINT('Ctrl Pts',(51.2872991489266,1.78300401749595,330.414270933002));
#30307=CARTESIAN_POINT('Ctrl Pts',(51.2795520705488,1.65376711199213,330.368128088797));
#30308=CARTESIAN_POINT('Ctrl Pts',(51.2718049272429,1.52452912335803,330.32198485787));
#30309=CARTESIAN_POINT('Ctrl Pts',(51.2640577839371,1.39335938678749,330.281255027923));
#30310=CARTESIAN_POINT('Ctrl Pts',(51.2563106406313,1.26075224465636,330.246087207353));
#30311=CARTESIAN_POINT('Ctrl Pts',(51.2485617556032,1.12811528962479,330.21091148031));
#30312=CARTESIAN_POINT('Ctrl Pts',(51.2408128705751,0.994040663721647,330.181300351092));
#30313=CARTESIAN_POINT('Ctrl Pts',(51.233063985547,0.859034924634935,330.157351751288));
#30314=CARTESIAN_POINT('Ctrl Pts',(51.2253068757723,0.723885889061702,330.133377732192));
#30315=CARTESIAN_POINT('Ctrl Pts',(51.2175497659976,0.587804151570398,330.115078316962));
#30316=CARTESIAN_POINT('Ctrl Pts',(51.2097926562228,0.451304006526837,330.102499846228));
#30317=CARTESIAN_POINT('Ctrl Pts',(51.2020314012967,0.314730920170378,330.089914653963));
#30318=CARTESIAN_POINT('Ctrl Pts',(51.1942701463705,0.177739370938527,330.083056517255));
#30319=CARTESIAN_POINT('Ctrl Pts',(51.1865088914444,0.0408447347324409,
330.081919605156));
#30320=CARTESIAN_POINT('Ctrl Pts',(51.1787352210397,-0.0962688882778101,
330.080780874369));
#30321=CARTESIAN_POINT('Ctrl Pts',(51.1709615506351,-0.233284897608335,
330.085381643663));
#30322=CARTESIAN_POINT('Ctrl Pts',(51.1631878802304,-0.369691065002353,
330.095664002237));
#30323=CARTESIAN_POINT('Ctrl Pts',(51.1557760760532,-0.499747492488417,
330.105467714545));
#30324=CARTESIAN_POINT('Ctrl Pts',(51.148364271876,-0.629249290714439,330.120435930953));
#30325=CARTESIAN_POINT('Ctrl Pts',(51.1409524676988,-0.757762062657612,
330.14047536081));
#30326=CARTESIAN_POINT('Ctrl Pts',(51.1331773889204,-0.892573628372065,
330.161496982818));
#30327=CARTESIAN_POINT('Ctrl Pts',(51.125402310142,-1.02672279562088,330.18816593049));
#30328=CARTESIAN_POINT('Ctrl Pts',(51.1176272313635,-1.15969918928645,330.220430892552));
#30329=CARTESIAN_POINT('Ctrl Pts',(51.1098617203145,-1.29251194703411,330.252656150525));
#30330=CARTESIAN_POINT('Ctrl Pts',(51.1020962092655,-1.42415442647661,330.290463629938));
#30331=CARTESIAN_POINT('Ctrl Pts',(51.0943306982164,-1.55412303142994,330.33375047113));
#30332=CARTESIAN_POINT('Ctrl Pts',(51.0865728866942,-1.68396277213262,330.376994393293));
#30333=CARTESIAN_POINT('Ctrl Pts',(51.078815075172,-1.81213157268847,330.425706742934));
#30334=CARTESIAN_POINT('Ctrl Pts',(51.0710572636498,-1.93813801677779,330.479734068617));
#30335=CARTESIAN_POINT('Ctrl Pts',(51.0633052901268,-2.06404963702264,330.533720737024));
#30336=CARTESIAN_POINT('Ctrl Pts',(51.0555533166038,-2.1878017819479,330.593014266879));
#30337=CARTESIAN_POINT('Ctrl Pts',(51.0478013430807,-2.30892048264449,330.657412146274));
#30338=CARTESIAN_POINT('Ctrl Pts',(51.0400526525231,-2.42998788949892,330.72178275313));
#30339=CARTESIAN_POINT('Ctrl Pts',(51.0323039619654,-2.54842372590289,330.791253226949));
#30340=CARTESIAN_POINT('Ctrl Pts',(51.0245552714078,-2.66377642220092,330.865574013841));
#30341=CARTESIAN_POINT('Ctrl Pts',(51.0168081930299,-2.77910511840727,330.939879337672));
#30342=CARTESIAN_POINT('Ctrl Pts',(51.0090611146521,-2.89135162206878,331.019032755739));
#30343=CARTESIAN_POINT('Ctrl Pts',(51.0013140362742,-3.00009162935601,331.102740286051));
#30344=CARTESIAN_POINT('Ctrl Pts',(50.9935668929684,-3.10883254798894,331.186448517913));
#30345=CARTESIAN_POINT('Ctrl Pts',(50.9858197496626,-3.21406660189955,331.274710699717));
#30346=CARTESIAN_POINT('Ctrl Pts',(50.9780726063568,-3.31540130609275,331.367191548945));
#30347=CARTESIAN_POINT('Ctrl Pts',(50.9703237213287,-3.4167587924785,331.45969318983));
#30348=CARTESIAN_POINT('Ctrl Pts',(50.9625748363006,-3.51421489603983,331.556415122003));
#30349=CARTESIAN_POINT('Ctrl Pts',(50.9548259512726,-3.60741313658341,331.656984366697));
#30350=CARTESIAN_POINT('Ctrl Pts',(50.9470688414978,-3.70071029870273,331.757660356628));
#30351=CARTESIAN_POINT('Ctrl Pts',(50.9393117317231,-3.78974030389571,331.862191529259));
#30352=CARTESIAN_POINT('Ctrl Pts',(50.9315546219484,-3.87418586914465,331.970170481063));
#30353=CARTESIAN_POINT('Ctrl Pts',(50.9237933670222,-3.95867655940367,332.078207133367));
#30354=CARTESIAN_POINT('Ctrl Pts',(50.916032112096,-4.03857770073597,332.18969491841));
#30355=CARTESIAN_POINT('Ctrl Pts',(50.9082708571698,-4.11361529703815,332.304197290143));
#30356=CARTESIAN_POINT('Ctrl Pts',(50.9004971867652,-4.18877292903972,332.418882828354));
#30357=CARTESIAN_POINT('Ctrl Pts',(50.8927235163605,-4.25905126861334,332.536592253965));
#30358=CARTESIAN_POINT('Ctrl Pts',(50.8849498459559,-4.3242218180849,332.656863484451));
#30359=CARTESIAN_POINT('Ctrl Pts',(50.8775380417789,-4.38635866279863,332.771536060221));
#30360=CARTESIAN_POINT('Ctrl Pts',(50.8701262376019,-4.44385242411905,332.88853704592));
#30361=CARTESIAN_POINT('Ctrl Pts',(50.8627144334249,-4.49654647498829,333.007450662902));
#30362=CARTESIAN_POINT('Ctrl Pts',(50.8541643290833,-4.55733324462683,333.144626957438));
#30363=CARTESIAN_POINT('Ctrl Pts',(50.8456142247417,-4.61189867345044,333.28472172135));
#30364=CARTESIAN_POINT('Ctrl Pts',(50.8370641204001,-4.65998033764655,333.42717886737));
#30365=CARTESIAN_POINT('Ctrl Pts',(50.8285467284448,-4.70787804315518,333.569090977564));
#30366=CARTESIAN_POINT('Ctrl Pts',(50.8200293364895,-4.74934137372882,333.713347197521));
#30367=CARTESIAN_POINT('Ctrl Pts',(50.8115119445342,-4.7841566456173,333.859373745394));
#30368=CARTESIAN_POINT('Ctrl Pts',(50.8030154818032,-4.81888636823912,334.005041471883));
#30369=CARTESIAN_POINT('Ctrl Pts',(50.7945190190723,-4.84700053829952,334.152470602505));
#30370=CARTESIAN_POINT('Ctrl Pts',(50.7860225563413,-4.86833456063157,334.301071056358));
#30371=CARTESIAN_POINT('Ctrl Pts',(50.7775592787733,-4.88958525734558,334.449091112176));
#30372=CARTESIAN_POINT('Ctrl Pts',(50.7690960012053,-4.90410856744097,334.598273112415));
#30373=CARTESIAN_POINT('Ctrl Pts',(50.7606327236373,-4.91179067866555,334.748017080987));
#30374=CARTESIAN_POINT('Ctrl Pts',(50.7559338986031,-4.91605579891569,334.831155168164));
#30375=CARTESIAN_POINT('Ctrl Pts',(50.7512350735689,-4.91821300605794,334.914466203605));
#30376=CARTESIAN_POINT('Ctrl Pts',(50.7465362485347,-4.9182495281824,334.997845694185));
#30377=CARTESIAN_POINT('',(54.2465362485459,-4.9182483994059,335.00396790137));
#30378=CARTESIAN_POINT('Ctrl Pts',(54.24653624849,-4.91824839940511,335.003967902354));
#30379=CARTESIAN_POINT('Ctrl Pts',(54.2339556148914,-4.91806968276805,335.225488679793));
#30380=CARTESIAN_POINT('Ctrl Pts',(54.2213749812928,-4.90292221337486,335.446423007763));
#30381=CARTESIAN_POINT('Ctrl Pts',(54.2087943476942,-4.87305733668216,335.665203168895));
#30382=CARTESIAN_POINT('Ctrl Pts',(54.2063865133669,-4.86734143416276,335.707075971086));
#30383=CARTESIAN_POINT('Ctrl Pts',(54.2039786790395,-4.86108652521291,335.748869975681));
#30384=CARTESIAN_POINT('Ctrl Pts',(54.2015708447122,-4.85429452218873,335.790574319307));
#30385=CARTESIAN_POINT('Ctrl Pts',(54.1937957659337,-4.83236263178532,335.925240792587));
#30386=CARTESIAN_POINT('Ctrl Pts',(54.1860206871553,-4.80478801956478,336.059206730811));
#30387=CARTESIAN_POINT('Ctrl Pts',(54.1782456083769,-4.77162544357483,336.191962117154));
#30388=CARTESIAN_POINT('Ctrl Pts',(54.1704800973278,-4.73850367624587,336.324554139541));
#30389=CARTESIAN_POINT('Ctrl Pts',(54.1627145862788,-4.69980772092743,336.45593819845));
#30390=CARTESIAN_POINT('Ctrl Pts',(54.1549490752298,-4.65564383708228,336.585611404077));
#30391=CARTESIAN_POINT('Ctrl Pts',(54.1471912637076,-4.61152374185654,336.715156038343));
#30392=CARTESIAN_POINT('Ctrl Pts',(54.1394334521854,-4.56194663233361,336.842992827472));
#30393=CARTESIAN_POINT('Ctrl Pts',(54.1316756406632,-4.50706927631419,336.968631403032));
#30394=CARTESIAN_POINT('Ctrl Pts',(54.1239236671402,-4.4522332172455,337.09417543158));
#30395=CARTESIAN_POINT('Ctrl Pts',(54.1161716936172,-4.39210500662631,337.217524182461));
#30396=CARTESIAN_POINT('Ctrl Pts',(54.1084197200942,-4.32689035373806,337.338205065692));
#30397=CARTESIAN_POINT('Ctrl Pts',(54.1006710295365,-4.26170331929394,337.458834840498));
#30398=CARTESIAN_POINT('Ctrl Pts',(54.0929223389789,-4.19143431239677,337.576798651674));
#30399=CARTESIAN_POINT('Ctrl Pts',(54.0851736484213,-4.11633593191898,337.691646625784));
#30400=CARTESIAN_POINT('Ctrl Pts',(54.0774265700435,-4.04125317628654,337.806470704813));
#30401=CARTESIAN_POINT('Ctrl Pts',(54.0696794916656,-3.96134325945718,337.918179909305));
#30402=CARTESIAN_POINT('Ctrl Pts',(54.0619324132877,-3.87690302318793,338.02635193117));
#30403=CARTESIAN_POINT('Ctrl Pts',(54.0541852699819,-3.79246207922818,338.134524859621));
#30404=CARTESIAN_POINT('Ctrl Pts',(54.0464381266761,-3.70349098061472,338.239160238203));
#30405=CARTESIAN_POINT('Ctrl Pts',(54.0386909833703,-3.61032765373224,338.339867855948));
#30406=CARTESIAN_POINT('Ctrl Pts',(54.0309420983422,-3.51714338175602,338.440598114904));
#30407=CARTESIAN_POINT('Ctrl Pts',(54.0231932133141,-3.41976527141893,338.537398568993));
#30408=CARTESIAN_POINT('Ctrl Pts',(54.015444328286,-3.31856870125198,338.629915265894));
#30409=CARTESIAN_POINT('Ctrl Pts',(54.0076872185113,-3.21726471999983,338.722530160973));
#30410=CARTESIAN_POINT('Ctrl Pts',(53.9999301087365,-3.11213447170504,338.810851951998));
#30411=CARTESIAN_POINT('Ctrl Pts',(53.9921729989618,-3.00358749407249,338.894566115494));
#30412=CARTESIAN_POINT('Ctrl Pts',(53.9844117440357,-2.89498251240583,338.978325013161));
#30413=CARTESIAN_POINT('Ctrl Pts',(53.9766504891095,-2.78295748242483,339.057471151778));
#30414=CARTESIAN_POINT('Ctrl Pts',(53.9688892341833,-2.66795079125739,339.131733490671));
#30415=CARTESIAN_POINT('Ctrl Pts',(53.9611155637787,-2.55276012686466,339.206114625104));
#30416=CARTESIAN_POINT('Ctrl Pts',(53.953341893374,-2.43457860717126,339.275596149943));
#30417=CARTESIAN_POINT('Ctrl Pts',(53.9455682229694,-2.31386984782282,339.339952694424));
#30418=CARTESIAN_POINT('Ctrl Pts',(53.9381564187923,-2.19878011026379,339.401313426276));
#30419=CARTESIAN_POINT('Ctrl Pts',(53.9307446146153,-2.08139338324387,339.458015450623));
#30420=CARTESIAN_POINT('Ctrl Pts',(53.9233328104383,-1.96212649404924,339.509904952862));
#30421=CARTESIAN_POINT('Ctrl Pts',(53.9155577316598,-1.83701397933638,339.564337714178));
#30422=CARTESIAN_POINT('Ctrl Pts',(53.9077826528814,-1.70943695894224,339.61364629062));
#30423=CARTESIAN_POINT('Ctrl Pts',(53.900007574103,-1.57985394961869,339.65760073003));
#30424=CARTESIAN_POINT('Ctrl Pts',(53.892242063054,-1.45043040043768,339.701501080704));
#30425=CARTESIAN_POINT('Ctrl Pts',(53.884476552005,-1.31900614054945,339.740060279425));
#30426=CARTESIAN_POINT('Ctrl Pts',(53.8767110409559,-1.18606156380943,339.773095539517));
#30427=CARTESIAN_POINT('Ctrl Pts',(53.8689532294337,-1.0532488020043,339.806098045051));
#30428=CARTESIAN_POINT('Ctrl Pts',(53.8611954179115,-0.918919100050427,
339.833587417843));
#30429=CARTESIAN_POINT('Ctrl Pts',(53.8534376063893,-0.783569655275992,
339.855430120785));
#30430=CARTESIAN_POINT('Ctrl Pts',(53.8456856328663,-0.648322065251018,
339.877256386401));
#30431=CARTESIAN_POINT('Ctrl Pts',(53.8379336593433,-0.512056644183368,
339.893444378163));
#30432=CARTESIAN_POINT('Ctrl Pts',(53.8301816858203,-0.375282124166118,
339.90391133584));
#30433=CARTESIAN_POINT('Ctrl Pts',(53.8224329952626,-0.238565528239298,
339.914373860754));
#30434=CARTESIAN_POINT('Ctrl Pts',(53.814684304705,-0.101340651107091,339.91912014072));
#30435=CARTESIAN_POINT('Ctrl Pts',(53.8069356141474,0.0358775033162497,
339.918119139189));
#30436=CARTESIAN_POINT('Ctrl Pts',(53.7991885357696,0.173067108356401,339.917118345924));
#30437=CARTESIAN_POINT('Ctrl Pts',(53.7914414573917,0.310249602851338,339.910372652482));
#30438=CARTESIAN_POINT('Ctrl Pts',(53.7836943790139,0.446909220811845,339.897903144291));
#30439=CARTESIAN_POINT('Ctrl Pts',(53.7759472357081,0.583569984111577,339.885433531593));
#30440=CARTESIAN_POINT('Ctrl Pts',(53.7682000924023,0.719707472878996,339.867240043981));
#30441=CARTESIAN_POINT('Ctrl Pts',(53.7604529490965,0.854810679030702,339.843395685417));
#30442=CARTESIAN_POINT('Ctrl Pts',(53.7527040640684,0.989944259251474,339.819545966135));
#30443=CARTESIAN_POINT('Ctrl Pts',(53.7449551790403,1.12404270930034,339.790042915798));
#30444=CARTESIAN_POINT('Ctrl Pts',(53.7372062940122,1.25660524425672,339.755010654311));
#30445=CARTESIAN_POINT('Ctrl Pts',(53.7294491842374,1.38930848245733,339.719941209219));
#30446=CARTESIAN_POINT('Ctrl Pts',(53.7216920744627,1.52047217051797,339.679330929599));
#30447=CARTESIAN_POINT('Ctrl Pts',(53.713934964688,1.64961019458591,339.633353997745));
#30448=CARTESIAN_POINT('Ctrl Pts',(53.7061737097618,1.77881722588479,339.587352497288));
#30449=CARTESIAN_POINT('Ctrl Pts',(53.6984124548357,1.90599607407346,339.535978776638));
#30450=CARTESIAN_POINT('Ctrl Pts',(53.6906511999095,2.03068157883941,339.479454809222));
#30451=CARTESIAN_POINT('Ctrl Pts',(53.6828775295048,2.15556653977817,339.42284042188));
#30452=CARTESIAN_POINT('Ctrl Pts',(53.6751038591001,2.27794983789881,339.361059500617));
#30453=CARTESIAN_POINT('Ctrl Pts',(53.6673301886955,2.39739106509028,339.294379948668));
#30454=CARTESIAN_POINT('Ctrl Pts',(53.6599183845184,2.51127227442001,339.230804345906));
#30455=CARTESIAN_POINT('Ctrl Pts',(53.6525065803413,2.62247891001836,339.162776061754));
#30456=CARTESIAN_POINT('Ctrl Pts',(53.6450947761642,2.73065605674223,339.090562377263));
#30457=CARTESIAN_POINT('Ctrl Pts',(53.6373196973858,2.84413528767021,339.014809284981));
#30458=CARTESIAN_POINT('Ctrl Pts',(53.6295446186073,2.95463916765595,338.934210746834));
#30459=CARTESIAN_POINT('Ctrl Pts',(53.6217695398289,3.06172619529895,338.849027899031));
#30460=CARTESIAN_POINT('Ctrl Pts',(53.6140040287799,3.16868144553693,338.763949874146));
#30461=CARTESIAN_POINT('Ctrl Pts',(53.6062385177309,3.27222790651429,338.674299005147));
#30462=CARTESIAN_POINT('Ctrl Pts',(53.5984730066818,3.37195190033349,338.580380349116));
#30463=CARTESIAN_POINT('Ctrl Pts',(53.5907151951596,3.47157701752247,338.486554813706));
#30464=CARTESIAN_POINT('Ctrl Pts',(53.5829573836375,3.56738692712724,338.388470178493));
#30465=CARTESIAN_POINT('Ctrl Pts',(53.5751995721153,3.6590002729416,338.286472282724));
#30466=CARTESIAN_POINT('Ctrl Pts',(53.5674475985922,3.75054467680788,338.184551143607));
#30467=CARTESIAN_POINT('Ctrl Pts',(53.5596956250692,3.8378985426843,338.078722895145));
#30468=CARTESIAN_POINT('Ctrl Pts',(53.5519436515462,3.92071697159911,337.969370554699));
#30469=CARTESIAN_POINT('Ctrl Pts',(53.5441949609886,4.00350032686016,337.860064525034));
#30470=CARTESIAN_POINT('Ctrl Pts',(53.536446270431,4.08175182991898,337.747237682721));
#30471=CARTESIAN_POINT('Ctrl Pts',(53.5286975798734,4.15516668331015,337.631306309879));
#30472=CARTESIAN_POINT('Ctrl Pts',(53.5209505014955,4.2285662621279,337.515399057528));
#30473=CARTESIAN_POINT('Ctrl Pts',(53.5132034231177,4.29713098390071,337.396388889458));
#30474=CARTESIAN_POINT('Ctrl Pts',(53.5054563447398,4.36059946924277,337.274720934827));
#30475=CARTESIAN_POINT('Ctrl Pts',(53.497709201434,4.42406848651186,337.153051960502));
#30476=CARTESIAN_POINT('Ctrl Pts',(53.4899620581282,4.48244100137742,337.028725501742));
#30477=CARTESIAN_POINT('Ctrl Pts',(53.4822149148224,4.53550186863297,336.902210782781));
#30478=CARTESIAN_POINT('Ctrl Pts',(53.4744660297943,4.58857466509797,336.775667620625));
#30479=CARTESIAN_POINT('Ctrl Pts',(53.4667171447662,4.63633328653853,336.646935579692));
#30480=CARTESIAN_POINT('Ctrl Pts',(53.4589682597381,4.67861110457458,336.516502949107));
#30481=CARTESIAN_POINT('Ctrl Pts',(53.4512111499634,4.72093379672353,336.385931875981));
#30482=CARTESIAN_POINT('Ctrl Pts',(53.4434540401886,4.75776394398962,336.253656979917));
#30483=CARTESIAN_POINT('Ctrl Pts',(53.4356969304139,4.78898495587991,336.120181304457));
#30484=CARTESIAN_POINT('Ctrl Pts',(53.4279356754877,4.82022265128067,335.986634303864));
#30485=CARTESIAN_POINT('Ctrl Pts',(53.4201744205615,4.84584516585099,335.851885629113));
#30486=CARTESIAN_POINT('Ctrl Pts',(53.4124131656354,4.86578743684675,335.716446565994));
#30487=CARTESIAN_POINT('Ctrl Pts',(53.4046394952307,4.88576160897694,335.580790844513));
#30488=CARTESIAN_POINT('Ctrl Pts',(53.396865824826,4.90003733921393,335.444442916706));
#30489=CARTESIAN_POINT('Ctrl Pts',(53.3890921544213,4.90860158300433,335.307918108963));
#30490=CARTESIAN_POINT('Ctrl Pts',(53.3816803502443,4.91676715918579,335.177748563867));
#30491=CARTESIAN_POINT('Ctrl Pts',(53.3742685460673,4.91974101528029,335.047418523487));
#30492=CARTESIAN_POINT('Ctrl Pts',(53.3668567418903,4.91755584867608,334.917371084651));
#30493=CARTESIAN_POINT('Ctrl Pts',(53.3590816631118,4.9152635805473,334.780949633446));
#30494=CARTESIAN_POINT('Ctrl Pts',(53.3513065843334,4.90728654049637,334.644408069534));
#30495=CARTESIAN_POINT('Ctrl Pts',(53.343531505555,4.89360540179282,334.508258976651));
#30496=CARTESIAN_POINT('Ctrl Pts',(53.335765994506,4.87994109860143,334.372277423895));
#30497=CARTESIAN_POINT('Ctrl Pts',(53.328000483457,4.86058670177242,334.236687766411));
#30498=CARTESIAN_POINT('Ctrl Pts',(53.320234972408,4.83557487546681,334.102002958661));
#30499=CARTESIAN_POINT('Ctrl Pts',(53.3124771608858,4.81058784845981,333.96745169129));
#30500=CARTESIAN_POINT('Ctrl Pts',(53.3047193493636,4.77995462582332,333.833803870079));
#30501=CARTESIAN_POINT('Ctrl Pts',(53.2969615378414,4.74375965743472,333.70156733906));
#30502=CARTESIAN_POINT('Ctrl Pts',(53.2892095643184,4.70759192690765,333.569430320225));
#30503=CARTESIAN_POINT('Ctrl Pts',(53.2814575907954,4.66587088421923,333.43870285313));
#30504=CARTESIAN_POINT('Ctrl Pts',(53.2737056172724,4.61873197221471,333.309882243351));
#30505=CARTESIAN_POINT('Ctrl Pts',(53.2659569267148,4.57161302356745,333.181116189176));
#30506=CARTESIAN_POINT('Ctrl Pts',(53.2582082361572,4.5190809031863,333.054255752452));
#30507=CARTESIAN_POINT('Ctrl Pts',(53.2504595455995,4.46132072818991,332.929782518013));
#30508=CARTESIAN_POINT('Ctrl Pts',(53.2427124672217,4.4035725706803,332.80533518127));
#30509=CARTESIAN_POINT('Ctrl Pts',(53.2349653888439,4.34059868657379,332.683274413223));
#30510=CARTESIAN_POINT('Ctrl Pts',(53.227218310466,4.27263194709239,332.564060898301));
#30511=CARTESIAN_POINT('Ctrl Pts',(53.2194711671602,4.20466463798429,332.444846384256));
#30512=CARTESIAN_POINT('Ctrl Pts',(53.2117240238545,4.13170458363291,332.328479510497));
#30513=CARTESIAN_POINT('Ctrl Pts',(53.2039768805487,4.05402993728916,332.215395121375));
#30514=CARTESIAN_POINT('Ctrl Pts',(53.1962279955206,3.97633782803589,332.102285308481));
#30515=CARTESIAN_POINT('Ctrl Pts',(53.1884791104925,3.89392923888849,331.992459770835));
#30516=CARTESIAN_POINT('Ctrl Pts',(53.1807302254644,3.80712461041235,331.886322871059));
#30517=CARTESIAN_POINT('Ctrl Pts',(53.1729731156896,3.72022784660662,331.780073316481));
#30518=CARTESIAN_POINT('Ctrl Pts',(53.1652160059149,3.62892597054433,331.677520523715));
#30519=CARTESIAN_POINT('Ctrl Pts',(53.1574588961402,3.53357890846681,331.579034761922));
#30520=CARTESIAN_POINT('Ctrl Pts',(53.149697641214,3.43818089596792,331.480496372486));
#30521=CARTESIAN_POINT('Ctrl Pts',(53.1419363862878,3.33873367348651,331.386029613567));
#30522=CARTESIAN_POINT('Ctrl Pts',(53.1341751313617,3.23563198296683,331.295965883891));
#30523=CARTESIAN_POINT('Ctrl Pts',(53.126401460957,3.13236536334307,331.205758081599));
#30524=CARTESIAN_POINT('Ctrl Pts',(53.1186277905524,3.02543289876756,331.119967628105));
#30525=CARTESIAN_POINT('Ctrl Pts',(53.1108541201477,2.91526087903867,331.038884365529));
#30526=CARTESIAN_POINT('Ctrl Pts',(53.1034423159706,2.81021739333343,330.961575548334));
#30527=CARTESIAN_POINT('Ctrl Pts',(53.0960305117935,2.70222940607966,330.888545706113));
#30528=CARTESIAN_POINT('Ctrl Pts',(53.0886187076163,2.59168722128641,330.820007128054));
#30529=CARTESIAN_POINT('Ctrl Pts',(53.0808436288379,2.47572703472884,330.748109270118));
#30530=CARTESIAN_POINT('Ctrl Pts',(53.0730685500595,2.35658948655505,330.680926858294));
#30531=CARTESIAN_POINT('Ctrl Pts',(53.0652934712811,2.23469516055991,330.618753533312));
#30532=CARTESIAN_POINT('Ctrl Pts',(53.057527960232,2.11295083329308,330.556656716564));
#30533=CARTESIAN_POINT('Ctrl Pts',(53.049762449183,1.98845682295723,330.499556897968));
#30534=CARTESIAN_POINT('Ctrl Pts',(53.041996938134,1.86166216035348,330.447704198626));
#30535=CARTESIAN_POINT('Ctrl Pts',(53.0342391266118,1.73499321502695,330.395902911386));
#30536=CARTESIAN_POINT('Ctrl Pts',(53.0264813150896,1.60602851641711,330.349338537065));
#30537=CARTESIAN_POINT('Ctrl Pts',(53.0187235035675,1.47524082207895,330.308214883504));
#30538=CARTESIAN_POINT('Ctrl Pts',(53.0109715300445,1.34455154962829,330.267122176797));
#30539=CARTESIAN_POINT('Ctrl Pts',(53.0032195565214,1.21204238344852,330.231462158087));
#30540=CARTESIAN_POINT('Ctrl Pts',(52.9954675829984,1.07820481430193,330.20139005118));
#30541=CARTESIAN_POINT('Ctrl Pts',(52.9877188924408,0.944423925445244,330.171330679827));
#30542=CARTESIAN_POINT('Ctrl Pts',(52.9799702018832,0.809316133124911,330.146854599018));
#30543=CARTESIAN_POINT('Ctrl Pts',(52.9722215113256,0.673386589796168,330.128066753004));
#30544=CARTESIAN_POINT('Ctrl Pts',(52.9644744329477,0.537485327744312,330.109282815959));
#30545=CARTESIAN_POINT('Ctrl Pts',(52.9567273545699,0.400763041709971,330.096184813157));
#30546=CARTESIAN_POINT('Ctrl Pts',(52.9489802761921,0.263733151039706,330.088826220999));
#30547=CARTESIAN_POINT('Ctrl Pts',(52.9412331328863,0.126702111927065,330.08146756717));
#30548=CARTESIAN_POINT('Ctrl Pts',(52.9334859895805,-0.0106361466516469,
330.079848440888));
#30549=CARTESIAN_POINT('Ctrl Pts',(52.9257388462747,-0.14776543012098,330.08397025638));
#30550=CARTESIAN_POINT('Ctrl Pts',(52.9179899612466,-0.284925543164574,
330.088092998543));
#30551=CARTESIAN_POINT('Ctrl Pts',(52.9102410762185,-0.421876196988287,
330.097959239058));
#30552=CARTESIAN_POINT('Ctrl Pts',(52.9024921911904,-0.558103945658428,
330.113518336437));
#30553=CARTESIAN_POINT('Ctrl Pts',(52.8947350814157,-0.694476287868504,
330.129093948402));
#30554=CARTESIAN_POINT('Ctrl Pts',(52.8869779716409,-0.83012380321036,330.150374443179));
#30555=CARTESIAN_POINT('Ctrl Pts',(52.8792208618662,-0.964540347707559,
330.177257525003));
#30556=CARTESIAN_POINT('Ctrl Pts',(52.87145960694,-1.09902872010824,330.204154972285));
#30557=CARTESIAN_POINT('Ctrl Pts',(52.8636983520138,-1.2322844314088,330.23666087953));
#30558=CARTESIAN_POINT('Ctrl Pts',(52.8559370970877,-1.36381518383249,330.274622638683));
#30559=CARTESIAN_POINT('Ctrl Pts',(52.848163426683,-1.49555634259439,330.312645124279));
#30560=CARTESIAN_POINT('Ctrl Pts',(52.8403897562784,-1.62556665756216,330.356140778003));
#30561=CARTESIAN_POINT('Ctrl Pts',(52.8326160858738,-1.7533717044416,330.404907973874));
#30562=CARTESIAN_POINT('Ctrl Pts',(52.8252042816966,-1.87522739564112,330.451405045045));
#30563=CARTESIAN_POINT('Ctrl Pts',(52.8177924775195,-1.99507824424029,330.502693809272));
#30564=CARTESIAN_POINT('Ctrl Pts',(52.8103806733424,-2.11253451583751,330.558560933448));
#30565=CARTESIAN_POINT('Ctrl Pts',(52.802605594564,-2.23574766918971,330.617166271799));
#30566=CARTESIAN_POINT('Ctrl Pts',(52.7948305157855,-2.35671495599475,330.680995319783));
#30567=CARTESIAN_POINT('Ctrl Pts',(52.7870554370071,-2.47496184547317,330.749853305361));
#30568=CARTESIAN_POINT('Ctrl Pts',(52.779289925958,-2.59306322462612,330.818626556804));
#30569=CARTESIAN_POINT('Ctrl Pts',(52.771524414909,-2.7084505327123,330.89241623783));
#30570=CARTESIAN_POINT('Ctrl Pts',(52.76375890386,-2.82067044122897,330.970980103738));
#30571=CARTESIAN_POINT('Ctrl Pts',(52.7560010923378,-2.93277908337955,331.049466073344));
#30572=CARTESIAN_POINT('Ctrl Pts',(52.7482432808156,-3.04172625756441,331.132716584938));
#30573=CARTESIAN_POINT('Ctrl Pts',(52.7404854692934,-3.14708474118129,331.220444378723));
#30574=CARTESIAN_POINT('Ctrl Pts',(52.7327334957704,-3.25236393919822,331.308106154562));
#30575=CARTESIAN_POINT('Ctrl Pts',(52.7249815222474,-3.35405952289839,331.400238257067));
#30576=CARTESIAN_POINT('Ctrl Pts',(52.7172295487243,-3.45177498742063,331.496511381677));
#30577=CARTESIAN_POINT('Ctrl Pts',(52.7094808581667,-3.54944906938555,331.592743734562));
#30578=CARTESIAN_POINT('Ctrl Pts',(52.701732167609,-3.64314610682035,331.693113347759));
#30579=CARTESIAN_POINT('Ctrl Pts',(52.6939834770514,-3.7325044828853,331.79725221915));
#30580=CARTESIAN_POINT('Ctrl Pts',(52.6862363986735,-3.82184426719377,331.901369423578));
#30581=CARTESIAN_POINT('Ctrl Pts',(52.6784893202957,-3.90684693127986,332.009254029867));
#30582=CARTESIAN_POINT('Ctrl Pts',(52.6707422419179,-3.98718966502875,332.120503231884));
#30583=CARTESIAN_POINT('Ctrl Pts',(52.6629950986121,-4.06753307212707,332.231753366277));
#30584=CARTESIAN_POINT('Ctrl Pts',(52.6552479553063,-4.14321624214478,332.346367835763));
#30585=CARTESIAN_POINT('Ctrl Pts',(52.6475008120004,-4.21395864332476,332.463913326629));
#30586=CARTESIAN_POINT('Ctrl Pts',(52.6397519269723,-4.28471694889842,332.581485244218));
#30587=CARTESIAN_POINT('Ctrl Pts',(52.6320030419442,-4.35053207377265,332.7019891596));
#30588=CARTESIAN_POINT('Ctrl Pts',(52.6242541569161,-4.41116874840035,332.824965900121));
#30589=CARTESIAN_POINT('Ctrl Pts',(52.6164970471414,-4.47186978342102,332.948073169425));
#30590=CARTESIAN_POINT('Ctrl Pts',(52.6087399373666,-4.52738121536722,333.073658155788));
#30591=CARTESIAN_POINT('Ctrl Pts',(52.6009828275918,-4.57751516338388,333.201239873832));
#30592=CARTESIAN_POINT('Ctrl Pts',(52.5932215726657,-4.62767590137936,333.328889767468));
#30593=CARTESIAN_POINT('Ctrl Pts',(52.5854603177395,-4.67245330208958,333.458538149585));
#30594=CARTESIAN_POINT('Ctrl Pts',(52.5776990628133,-4.71170928630875,333.589688451507));
#30595=CARTESIAN_POINT('Ctrl Pts',(52.5699253924086,-4.75102806730916,333.72104855117));
#30596=CARTESIAN_POINT('Ctrl Pts',(52.562151722004,-4.78480768557222,333.853914992686));
#30597=CARTESIAN_POINT('Ctrl Pts',(52.5543780515994,-4.81296095448017,333.987779711155));
#30598=CARTESIAN_POINT('Ctrl Pts',(52.5469662474224,-4.83980368194676,334.115412994772));
#30599=CARTESIAN_POINT('Ctrl Pts',(52.5395544432454,-4.86153203712724,334.243953423534));
#30600=CARTESIAN_POINT('Ctrl Pts',(52.5321426390684,-4.87811450873532,334.372957814684));
#30601=CARTESIAN_POINT('Ctrl Pts',(52.5202738422089,-4.90466863540197,334.579537329735));
#30602=CARTESIAN_POINT('Ctrl Pts',(52.5084050453495,-4.91810432005569,334.787838599102));
#30603=CARTESIAN_POINT('Ctrl Pts',(52.4965362484901,-4.91824882173174,334.996595586053));
#30604=CARTESIAN_POINT('',(55.9965362484619,-4.9182498257703,335.001309125831));
#30605=CARTESIAN_POINT('Ctrl Pts',(55.9965362484619,-4.9182498257703,335.001309125831));
#30606=CARTESIAN_POINT('Ctrl Pts',(55.9882359763961,-4.9182106052105,335.148656696918));
#30607=CARTESIAN_POINT('Ctrl Pts',(55.9799357043303,-4.91154550858833,335.295822679162));
#30608=CARTESIAN_POINT('Ctrl Pts',(55.9716354322645,-4.89832862073287,335.442221421699));
#30609=CARTESIAN_POINT('Ctrl Pts',(55.9632490671054,-4.8849746430628,335.59013865911));
#30610=CARTESIAN_POINT('Ctrl Pts',(55.9548627019463,-4.86493227844111,335.737272344221));
#30611=CARTESIAN_POINT('Ctrl Pts',(55.9464763367872,-4.83833005884191,335.883031881761));
#30612=CARTESIAN_POINT('Ctrl Pts',(55.9381312631354,-4.81185881919924,336.028073750694));
#30613=CARTESIAN_POINT('Ctrl Pts',(55.9297861894837,-4.77889233825748,336.17175470877));
#30614=CARTESIAN_POINT('Ctrl Pts',(55.9214411158319,-4.739606898083,336.313510378392));
#30615=CARTESIAN_POINT('Ctrl Pts',(55.9130341049192,-4.70002988078658,336.456318160706));
#30616=CARTESIAN_POINT('Ctrl Pts',(55.9046270940064,-4.6540398562618,336.597171677283));
#30617=CARTESIAN_POINT('Ctrl Pts',(55.8962200830937,-4.60186564622711,336.735515956877));
#30618=CARTESIAN_POINT('Ctrl Pts',(55.887813072181,-4.54969143619245,336.873860236471));
#30619=CARTESIAN_POINT('Ctrl Pts',(55.8794060612684,-4.49133322060517,337.009695028739));
#30620=CARTESIAN_POINT('Ctrl Pts',(55.8709990503557,-4.42706603779988,337.142491390755));
#30621=CARTESIAN_POINT('Ctrl Pts',(55.8632239715773,-4.36762964425063,337.265305811586));
#30622=CARTESIAN_POINT('Ctrl Pts',(55.8554488927988,-4.30298483270222,337.385839127243));
#30623=CARTESIAN_POINT('Ctrl Pts',(55.8476738140204,-4.23332957654058,337.503618133599));
#30624=CARTESIAN_POINT('Ctrl Pts',(55.8399083029714,-4.16376003560613,337.62125220539));
#30625=CARTESIAN_POINT('Ctrl Pts',(55.8321427919224,-4.08919251504711,337.736138378496));
#30626=CARTESIAN_POINT('Ctrl Pts',(55.8243772808734,-4.00987231659231,337.847824971294));
#30627=CARTESIAN_POINT('Ctrl Pts',(55.8166194693512,-3.93063076434522,337.959400826511));
#30628=CARTESIAN_POINT('Ctrl Pts',(55.8088616578289,-3.84664613680464,338.067783098033));
#30629=CARTESIAN_POINT('Ctrl Pts',(55.8011038463067,-3.75820857340413,338.172546513653));
#30630=CARTESIAN_POINT('Ctrl Pts',(55.7933518727837,-3.66983756207446,338.27723109148));
#30631=CARTESIAN_POINT('Ctrl Pts',(55.7855998992607,-3.57702053595824,338.37830193653));
#30632=CARTESIAN_POINT('Ctrl Pts',(55.7778479257377,-3.48008947077399,338.475364777676));
#30633=CARTESIAN_POINT('Ctrl Pts',(55.7700992351801,-3.38319945595352,338.57238651265));
#30634=CARTESIAN_POINT('Ctrl Pts',(55.7623505446224,-3.28219914300021,338.665403343712));
#30635=CARTESIAN_POINT('Ctrl Pts',(55.7546018540648,-3.17745896861545,338.75405614839));
#30636=CARTESIAN_POINT('Ctrl Pts',(55.7468547756869,-3.07274058629877,338.842690508112));
#30637=CARTESIAN_POINT('Ctrl Pts',(55.7391076973091,-2.9642841884288,338.926962395102));
#30638=CARTESIAN_POINT('Ctrl Pts',(55.7313606189313,-2.85249475275847,339.006551727856));
#30639=CARTESIAN_POINT('Ctrl Pts',(55.7236134756255,-2.740704380185,339.086141727645));
#30640=CARTESIAN_POINT('Ctrl Pts',(55.7158663323197,-2.62558123251232,339.161048868221));
#30641=CARTESIAN_POINT('Ctrl Pts',(55.7081191890139,-2.50756050875593,339.230995551573));
#30642=CARTESIAN_POINT('Ctrl Pts',(55.7003703039858,-2.38951325143526,339.300957960423));
#30643=CARTESIAN_POINT('Ctrl Pts',(55.6926214189576,-2.26856745793434,339.365957493646));
#30644=CARTESIAN_POINT('Ctrl Pts',(55.6848725339295,-2.14518387984355,339.4257619891));
#30645=CARTESIAN_POINT('Ctrl Pts',(55.6771154241548,-2.02166934114818,339.485629961663));
#30646=CARTESIAN_POINT('Ctrl Pts',(55.6693583143801,-1.89571220139915,339.540291710836));
#30647=CARTESIAN_POINT('Ctrl Pts',(55.6616012046053,-1.76779470426661,339.589562609451));
#30648=CARTESIAN_POINT('Ctrl Pts',(55.6538399496792,-1.63980885211362,339.638859836858));
#30649=CARTESIAN_POINT('Ctrl Pts',(55.646078694753,-1.5098609253601,339.682760348615));
#30650=CARTESIAN_POINT('Ctrl Pts',(55.6383174398268,-1.37844841417604,339.721129423343));
#30651=CARTESIAN_POINT('Ctrl Pts',(55.6305437694222,-1.24682568580134,339.759559876086));
#30652=CARTESIAN_POINT('Ctrl Pts',(55.6227700990175,-1.11373407093708,339.792441116084));
#30653=CARTESIAN_POINT('Ctrl Pts',(55.6149964286128,-0.979682211895785,
339.81968939105));
#30654=CARTESIAN_POINT('Ctrl Pts',(55.6075846244358,-0.851870499145784,
339.845669252259));
#30655=CARTESIAN_POINT('Ctrl Pts',(55.6001728202589,-0.723186213177062,
339.866528729482));
#30656=CARTESIAN_POINT('Ctrl Pts',(55.5927610160819,-0.594072739515768,
339.882239306165));
#30657=CARTESIAN_POINT('Ctrl Pts',(55.5849859373034,-0.458631029899123,
339.898719905011));
#30658=CARTESIAN_POINT('Ctrl Pts',(55.577210858525,-0.322288976450269,339.909586197146));
#30659=CARTESIAN_POINT('Ctrl Pts',(55.5694357797466,-0.185551641373691,
339.914748584707));
#30660=CARTESIAN_POINT('Ctrl Pts',(55.5616702686976,-0.0489825702929563,
339.919904619622));
#30661=CARTESIAN_POINT('Ctrl Pts',(55.5539047576486,0.0879804277186762,
339.919370701191));
#30662=CARTESIAN_POINT('Ctrl Pts',(55.5461392465996,0.224824777107929,339.913108678026));
#30663=CARTESIAN_POINT('Ctrl Pts',(55.5383814350773,0.361533444926443,339.906852863676));
#30664=CARTESIAN_POINT('Ctrl Pts',(55.5306236235551,0.498123310283324,339.894880264738));
#30665=CARTESIAN_POINT('Ctrl Pts',(55.5228658120329,0.634079741609925,339.877204726458));
#30666=CARTESIAN_POINT('Ctrl Pts',(55.5151138385099,0.769933861410248,339.85954248958));
#30667=CARTESIAN_POINT('Ctrl Pts',(55.5073618649869,0.905155109935398,339.836185905855));
#30668=CARTESIAN_POINT('Ctrl Pts',(55.4996098914638,1.03923228507392,339.807200778016));
#30669=CARTESIAN_POINT('Ctrl Pts',(55.4918612009062,1.17325267844926,339.778227925397));
#30670=CARTESIAN_POINT('Ctrl Pts',(55.4841125103486,1.30612958085206,339.743631352079));
#30671=CARTESIAN_POINT('Ctrl Pts',(55.476363819791,1.43736053397991,339.703528224414));
#30672=CARTESIAN_POINT('Ctrl Pts',(55.4686167414132,1.56856418341191,339.663433440539));
#30673=CARTESIAN_POINT('Ctrl Pts',(55.4608696630353,1.69812219115844,339.617834495325));
#30674=CARTESIAN_POINT('Ctrl Pts',(55.4531225846575,1.82554623715271,339.566898728735));
#30675=CARTESIAN_POINT('Ctrl Pts',(55.4453754413517,1.95297135108313,339.515962535254));
#30676=CARTESIAN_POINT('Ctrl Pts',(55.4376282980458,2.0782621046381,339.459689576268));
#30677=CARTESIAN_POINT('Ctrl Pts',(55.42988115474,2.20094954856742,339.398295595701));
#30678=CARTESIAN_POINT('Ctrl Pts',(55.4221322697119,2.32366457523886,339.336887812463));
#30679=CARTESIAN_POINT('Ctrl Pts',(55.4143833846839,2.44377477816129,339.270356891542));
#30680=CARTESIAN_POINT('Ctrl Pts',(55.4066344996558,2.56083558811472,339.198964652524));
#30681=CARTESIAN_POINT('Ctrl Pts',(55.398877389881,2.67802064762139,339.127496637045));
#30682=CARTESIAN_POINT('Ctrl Pts',(55.3911202801063,2.79214951439594,339.051157200021));
#30683=CARTESIAN_POINT('Ctrl Pts',(55.3833631703315,2.90280596179214,338.970251958086));
#30684=CARTESIAN_POINT('Ctrl Pts',(55.3756019154054,3.01352154045571,338.889303482976));
#30685=CARTESIAN_POINT('Ctrl Pts',(55.3678406604792,3.12076069694579,338.803784584974));
#30686=CARTESIAN_POINT('Ctrl Pts',(55.360079405553,3.22414092070293,338.714040708709));
#30687=CARTESIAN_POINT('Ctrl Pts',(55.3523057351483,3.32768651912647,338.624153271489));
#30688=CARTESIAN_POINT('Ctrl Pts',(55.3445320647436,3.42736056492973,338.530027618853));
#30689=CARTESIAN_POINT('Ctrl Pts',(55.336758394339,3.52281737348578,338.432046155804));
#30690=CARTESIAN_POINT('Ctrl Pts',(55.3293465901619,3.61383064463764,338.338625753433));
#30691=CARTESIAN_POINT('Ctrl Pts',(55.3219347859849,3.70101027509299,338.241700652043));
#30692=CARTESIAN_POINT('Ctrl Pts',(55.3145229818078,3.78409234332512,338.141628272041));
#30693=CARTESIAN_POINT('Ctrl Pts',(55.3067479030294,3.87124651121026,338.036651046595));
#30694=CARTESIAN_POINT('Ctrl Pts',(55.2989728242509,3.95416671651489,337.927878479301));
#30695=CARTESIAN_POINT('Ctrl Pts',(55.2911977454725,4.03250429634635,337.815686801199));
#30696=CARTESIAN_POINT('Ctrl Pts',(55.2834322344235,4.11074547679861,337.7036331821));
#30697=CARTESIAN_POINT('Ctrl Pts',(55.2756667233745,4.18441503055797,337.588169141195));
#30698=CARTESIAN_POINT('Ctrl Pts',(55.2679012123255,4.25320349126631,337.469705068299));
#30699=CARTESIAN_POINT('Ctrl Pts',(55.2601434008033,4.32192374801559,337.351358452875));
#30700=CARTESIAN_POINT('Ctrl Pts',(55.2523855892811,4.38577234781364,337.230018060807));
#30701=CARTESIAN_POINT('Ctrl Pts',(55.2446277777589,4.44448243675132,337.106124149216));
#30702=CARTESIAN_POINT('Ctrl Pts',(55.2368758042359,4.50314834448523,336.982323471722));
#30703=CARTESIAN_POINT('Ctrl Pts',(55.2291238307129,4.5566832715103,336.855973451364));
#30704=CARTESIAN_POINT('Ctrl Pts',(55.2213718571899,4.60486591195454,336.727539578539));
#30705=CARTESIAN_POINT('Ctrl Pts',(55.2136231666322,4.65302814702194,336.599160097536));
#30706=CARTESIAN_POINT('Ctrl Pts',(55.2058744760746,4.69584246679902,336.468698884528));
#30707=CARTESIAN_POINT('Ctrl Pts',(55.198125785517,4.73313548995022,336.336641872857));
#30708=CARTESIAN_POINT('Ctrl Pts',(55.1903787071392,4.77042075397648,336.204612336749));
#30709=CARTESIAN_POINT('Ctrl Pts',(55.1826316287614,4.80218690016365,336.070988038314));
#30710=CARTESIAN_POINT('Ctrl Pts',(55.1748845503835,4.82831039024877,335.936270173569));
#30711=CARTESIAN_POINT('Ctrl Pts',(55.1671374070777,4.85443409927388,335.801551179759));
#30712=CARTESIAN_POINT('Ctrl Pts',(55.1593902637719,4.87491498346233,335.665738985085));
#30713=CARTESIAN_POINT('Ctrl Pts',(55.1516431204661,4.88968069113446,335.529344690393));
#30714=CARTESIAN_POINT('Ctrl Pts',(55.143894235438,4.90444971845117,335.392919731367));
#30715=CARTESIAN_POINT('Ctrl Pts',(55.1361453504099,4.91350097039693,335.255912800437));
#30716=CARTESIAN_POINT('Ctrl Pts',(55.1283964653818,4.91681403473352,335.118839430946));
#30717=CARTESIAN_POINT('Ctrl Pts',(55.1206393556071,4.92013061559083,334.981620570364));
#30718=CARTESIAN_POINT('Ctrl Pts',(55.1128822458324,4.91769683289119,334.844335521731));
#30719=CARTESIAN_POINT('Ctrl Pts',(55.1051251360576,4.90954444206203,334.707499685611));
#30720=CARTESIAN_POINT('Ctrl Pts',(55.0973638811315,4.90138769485587,334.570590728795));
#30721=CARTESIAN_POINT('Ctrl Pts',(55.0896026262053,4.88750629001892,334.434131851474));
#30722=CARTESIAN_POINT('Ctrl Pts',(55.0818413712792,4.86798372089684,334.298631654846));
#30723=CARTESIAN_POINT('Ctrl Pts',(55.0740677008745,4.84842992202655,334.162914702064));
#30724=CARTESIAN_POINT('Ctrl Pts',(55.0662940304698,4.82321699812177,334.028159878925));
#30725=CARTESIAN_POINT('Ctrl Pts',(55.0585203600652,4.79247945192098,333.894864820298));
#30726=CARTESIAN_POINT('Ctrl Pts',(55.0511085558881,4.76317274589082,333.767774678718));
#30727=CARTESIAN_POINT('Ctrl Pts',(55.043696751711,4.72884426073161,333.642011733649));
#30728=CARTESIAN_POINT('Ctrl Pts',(55.0362849475339,4.68965173580566,333.517991343023));
#30729=CARTESIAN_POINT('Ctrl Pts',(55.0285098687555,4.64853826848464,333.387892343615));
#30730=CARTESIAN_POINT('Ctrl Pts',(55.020734789977,4.60194197713734,333.259299896418));
#30731=CARTESIAN_POINT('Ctrl Pts',(55.0129597111986,4.54999056097327,333.132710799701));
#30732=CARTESIAN_POINT('Ctrl Pts',(55.0051942001496,4.49810307433418,333.006277478926));
#30733=CARTESIAN_POINT('Ctrl Pts',(54.9974286891007,4.44087372171737,332.88184296164));
#30734=CARTESIAN_POINT('Ctrl Pts',(54.9896631780516,4.37848013866901,332.759889570182));
#30735=CARTESIAN_POINT('Ctrl Pts',(54.9819053665294,4.31614841903985,332.638057095866));
#30736=CARTESIAN_POINT('Ctrl Pts',(54.9741475550072,4.24866283564847,332.518701197487));
#30737=CARTESIAN_POINT('Ctrl Pts',(54.966389743485,4.17624920013888,332.402284526581));
#30738=CARTESIAN_POINT('Ctrl Pts',(54.958637769962,4.10389005818644,332.285955462912));
#30739=CARTESIAN_POINT('Ctrl Pts',(54.950885796439,4.02661045135484,332.172561554681));
#30740=CARTESIAN_POINT('Ctrl Pts',(54.943133822916,3.9446820591438,332.06254080628));
#30741=CARTESIAN_POINT('Ctrl Pts',(54.9353851323583,3.86278836365551,331.952566651732));
#30742=CARTESIAN_POINT('Ctrl Pts',(54.9276364418008,3.77625003148594,331.845963128607));
#30743=CARTESIAN_POINT('Ctrl Pts',(54.9198877512432,3.6853818677589,331.743139003382));
#30744=CARTESIAN_POINT('Ctrl Pts',(54.9121406728653,3.59453260991228,331.640336271575));
#30745=CARTESIAN_POINT('Ctrl Pts',(54.9043935944875,3.49935557105182,331.541311666301));
#30746=CARTESIAN_POINT('Ctrl Pts',(54.8966465161097,3.4002053639589,331.446440299445));
#30747=CARTESIAN_POINT('Ctrl Pts',(54.8888993728038,3.30105432589182,331.351568137476));
#30748=CARTESIAN_POINT('Ctrl Pts',(54.881152229498,3.19793033559151,331.260849553582));
#30749=CARTESIAN_POINT('Ctrl Pts',(54.8734050861922,3.09122403501736,331.174621975826));
#30750=CARTESIAN_POINT('Ctrl Pts',(54.8656562011641,2.98449374460147,331.088375012281));
#30751=CARTESIAN_POINT('Ctrl Pts',(54.8579073161361,2.8741798452564,331.006621309638));
#30752=CARTESIAN_POINT('Ctrl Pts',(54.850158431108,2.7607048137354,330.929657017656));
#30753=CARTESIAN_POINT('Ctrl Pts',(54.8424013213333,2.64710933864345,330.852611034979));
#30754=CARTESIAN_POINT('Ctrl Pts',(54.8346442115585,2.53034635293069,330.780364837544));
#30755=CARTESIAN_POINT('Ctrl Pts',(54.8268871017838,2.41086645261118,330.713170634353));
#30756=CARTESIAN_POINT('Ctrl Pts',(54.8191258468576,2.29132270605309,330.645940524728));
#30757=CARTESIAN_POINT('Ctrl Pts',(54.8113645919315,2.16905950021886,330.583767965675));
#30758=CARTESIAN_POINT('Ctrl Pts',(54.8036033370053,2.0445497117483,330.52685797915));
#30759=CARTESIAN_POINT('Ctrl Pts',(54.7958296666006,1.91984074819393,330.469856955195));
#30760=CARTESIAN_POINT('Ctrl Pts',(54.788055996196,1.79287838270644,330.41813547377));
#30761=CARTESIAN_POINT('Ctrl Pts',(54.7802823257913,1.6641538742119,330.371849727435));
#30762=CARTESIAN_POINT('Ctrl Pts',(54.7728705216142,1.54142152255667,330.327718593727));
#30763=CARTESIAN_POINT('Ctrl Pts',(54.7654587174371,1.41708766592525,330.28852860341));
#30764=CARTESIAN_POINT('Ctrl Pts',(54.75804691326,1.29158694948444,330.2543718841));
#30765=CARTESIAN_POINT('Ctrl Pts',(54.7502718344816,1.1599350690839,330.218541042229));
#30766=CARTESIAN_POINT('Ctrl Pts',(54.7424967557031,1.02658300989388,330.1881361059));
#30767=CARTESIAN_POINT('Ctrl Pts',(54.7347216769247,0.892017645546317,330.163318536172));
#30768=CARTESIAN_POINT('Ctrl Pts',(54.7269561658757,0.757617872446341,330.138531506045));
#30769=CARTESIAN_POINT('Ctrl Pts',(54.7191906548266,0.622008145645764,330.11931823224));
#30770=CARTESIAN_POINT('Ctrl Pts',(54.7114251437776,0.485690189076216,330.105790349532));
#30771=CARTESIAN_POINT('Ctrl Pts',(54.7036673322554,0.349507392157486,330.092275879759));
#30772=CARTESIAN_POINT('Ctrl Pts',(54.6959095207333,0.212618149369224,330.084435621322));
#30773=CARTESIAN_POINT('Ctrl Pts',(54.6881517092111,0.0755337138958797,
330.082330051685));
#30774=CARTESIAN_POINT('Ctrl Pts',(54.6803997356881,-0.0614475611925734,
330.080226066555));
#30775=CARTESIAN_POINT('Ctrl Pts',(54.6726477621651,-0.198623347336834,
330.083848186343));
#30776=CARTESIAN_POINT('Ctrl Pts',(54.664895788642,-0.335478295932384,330.09320497927));
#30777=CARTESIAN_POINT('Ctrl Pts',(54.6571470980844,-0.472275286375859,
330.10255780959));
#30778=CARTESIAN_POINT('Ctrl Pts',(54.6493984075268,-0.608751320363877,
330.117640456054));
#30779=CARTESIAN_POINT('Ctrl Pts',(54.6416497169692,-0.744392298328861,
330.138409399313));
#30780=CARTESIAN_POINT('Ctrl Pts',(54.6339026385913,-0.880005055055391,
330.15917402142));
#30781=CARTESIAN_POINT('Ctrl Pts',(54.6261555602135,-1.01478271521205,330.185622527967));
#30782=CARTESIAN_POINT('Ctrl Pts',(54.6184084818356,-1.14821793788851,330.217659712065));
#30783=CARTESIAN_POINT('Ctrl Pts',(54.6106613385298,-1.28165427888065,330.249697164665));
#30784=CARTESIAN_POINT('Ctrl Pts',(54.6029141952241,-1.41374777987883,330.287323296986));
#30785=CARTESIAN_POINT('Ctrl Pts',(54.5951670519183,-1.54400329164488,330.330392211557));
#30786=CARTESIAN_POINT('Ctrl Pts',(54.5874181668902,-1.67428808761519,330.373470808934));
#30787=CARTESIAN_POINT('Ctrl Pts',(54.5796692818621,-1.80273370105262,330.421994500811));
#30788=CARTESIAN_POINT('Ctrl Pts',(54.571920396834,-1.92886246689311,330.475768281099));
#30789=CARTESIAN_POINT('Ctrl Pts',(54.5641632870593,-2.05512510710899,330.529599137433));
#30790=CARTESIAN_POINT('Ctrl Pts',(54.5564061772845,-2.1790656272652,330.58869106023));
#30791=CARTESIAN_POINT('Ctrl Pts',(54.5486490675098,-2.30022809607237,330.652801618451));
#30792=CARTESIAN_POINT('Ctrl Pts',(54.5408878125836,-2.42145531022877,330.716946435305));
#30793=CARTESIAN_POINT('Ctrl Pts',(54.5331265576575,-2.53990117766808,330.786115034298));
#30794=CARTESIAN_POINT('Ctrl Pts',(54.5253653027313,-2.65513739036905,330.86002071252));
#30795=CARTESIAN_POINT('Ctrl Pts',(54.5175916323266,-2.77055794345502,330.934044615741));
#30796=CARTESIAN_POINT('Ctrl Pts',(54.509817961922,-2.88275826167886,331.012820516126));
#30797=CARTESIAN_POINT('Ctrl Pts',(54.5020442915173,-2.99134115099241,331.096019828319));
#30798=CARTESIAN_POINT('Ctrl Pts',(54.4946324873402,-3.09486948068459,331.175346192512));
#30799=CARTESIAN_POINT('Ctrl Pts',(54.4872206831632,-3.19510936372162,331.258693232618));
#30800=CARTESIAN_POINT('Ctrl Pts',(54.4798088789861,-3.29174811658647,331.345745301782));
#30801=CARTESIAN_POINT('Ctrl Pts',(54.4721496015553,-3.39161354760378,331.435703958638));
#30802=CARTESIAN_POINT('Ctrl Pts',(54.4644903241245,-3.4879690371342,331.529922246825));
#30803=CARTESIAN_POINT('Ctrl Pts',(54.4568310466937,-3.58042108453715,331.628091353565));
#30804=CARTESIAN_POINT('Ctrl Pts',(54.449181280803,-3.672758321977,331.726138550712));
#30805=CARTESIAN_POINT('Ctrl Pts',(54.4415315149124,-3.7612014832035,331.828126518954));
#30806=CARTESIAN_POINT('Ctrl Pts',(54.4338817490217,-3.84539041192421,331.933706530291));
#30807=CARTESIAN_POINT('Ctrl Pts',(54.4260756865019,-3.93129945155538,332.041443705665));
#30808=CARTESIAN_POINT('Ctrl Pts',(54.418269623982,-4.01277819006488,332.152921045607));
#30809=CARTESIAN_POINT('Ctrl Pts',(54.4104635614622,-4.08948322967486,332.267728055865));
#30810=CARTESIAN_POINT('Ctrl Pts',(54.4028272154001,-4.16452057733722,332.380038975546));
#30811=CARTESIAN_POINT('Ctrl Pts',(54.3951908693379,-4.23498942841753,332.495535914817));
#30812=CARTESIAN_POINT('Ctrl Pts',(54.3875545232757,-4.30060931046474,332.613801638328));
#30813=CARTESIAN_POINT('Ctrl Pts',(54.3799211644284,-4.36620352307743,332.732021098205));
#30814=CARTESIAN_POINT('Ctrl Pts',(54.372287805581,-4.42695234296321,332.853006836397));
#30815=CARTESIAN_POINT('Ctrl Pts',(54.3646544467337,-4.48261975490676,332.976314452436));
#30816=CARTESIAN_POINT('Ctrl Pts',(54.3570223074505,-4.5382782729964,333.099602367902));
#30817=CARTESIAN_POINT('Ctrl Pts',(54.3493901681673,-4.58885683266491,333.225211055429));
#30818=CARTESIAN_POINT('Ctrl Pts',(54.3417580288841,-4.63416658944166,333.352673959472));
#30819=CARTESIAN_POINT('Ctrl Pts',(54.3338228805226,-4.68127522162277,333.4851973604));
#30820=CARTESIAN_POINT('Ctrl Pts',(54.325887732161,-4.72268787865864,333.61972481477));
#30821=CARTESIAN_POINT('Ctrl Pts',(54.3179525837995,-4.75824888827521,333.755712822646));
#30822=CARTESIAN_POINT('Ctrl Pts',(54.3103144412865,-4.79247887957251,333.886610915144));
#30823=CARTESIAN_POINT('Ctrl Pts',(54.3026762987735,-4.82128732478986,334.018861780984));
#30824=CARTESIAN_POINT('Ctrl Pts',(54.2950381562605,-4.84458745902484,334.151969685472));
#30825=CARTESIAN_POINT('Ctrl Pts',(54.2873966328377,-4.86789790671672,334.285136508187));
#30826=CARTESIAN_POINT('Ctrl Pts',(54.2797551094148,-4.88569513531771,334.419160725621));
#30827=CARTESIAN_POINT('Ctrl Pts',(54.2721135859919,-4.89794422320548,334.553541212576));
#30828=CARTESIAN_POINT('Ctrl Pts',(54.2644640690337,-4.91020612444362,334.688062270346));
#30829=CARTESIAN_POINT('Ctrl Pts',(54.2568145520755,-4.91690828641832,334.822939939611));
#30830=CARTESIAN_POINT('Ctrl Pts',(54.2491650351173,-4.91806785985879,334.957672841768));
#30831=CARTESIAN_POINT('Ctrl Pts',(54.2482887729268,-4.91820069051574,334.973106672246));
#30832=CARTESIAN_POINT('Ctrl Pts',(54.2474125107363,-4.91826084731576,334.988538608389));
#30833=CARTESIAN_POINT('Ctrl Pts',(54.2465362485458,-4.9182483994059,335.00396790137));
#30834=CARTESIAN_POINT('',(57.746536723243,-4.91737005110712,334.995488220275));
#30835=CARTESIAN_POINT('Ctrl Pts',(57.7465362484901,-4.91824793749837,334.995495802735));
#30836=CARTESIAN_POINT('Ctrl Pts',(57.7388648584507,-4.91837207600807,335.131045809413));
#30837=CARTESIAN_POINT('Ctrl Pts',(57.7311934684114,-4.91288823446128,335.266732526264));
#30838=CARTESIAN_POINT('Ctrl Pts',(57.7235220783721,-4.90178935935022,335.402049921106));
#30839=CARTESIAN_POINT('Ctrl Pts',(57.7158548430756,-4.89069649527138,335.537294029491));
#30840=CARTESIAN_POINT('Ctrl Pts',(57.7081876077791,-4.87399467829062,335.672168816094));
#30841=CARTESIAN_POINT('Ctrl Pts',(57.7005203724827,-4.85172892970453,335.806169619353));
#30842=CARTESIAN_POINT('Ctrl Pts',(57.6928552568424,-4.82946933662675,335.940133377235));
#30843=CARTESIAN_POINT('Ctrl Pts',(57.6851901412021,-4.80164893564545,336.073223237912));
#30844=CARTESIAN_POINT('Ctrl Pts',(57.6775250255618,-4.76836440272733,336.204941486257));
#30845=CARTESIAN_POINT('Ctrl Pts',(57.6698602841005,-4.73508149462132,336.336653304666));
#30846=CARTESIAN_POINT('Ctrl Pts',(57.6621955426392,-4.6963350830001,336.466993256056));
#30847=CARTESIAN_POINT('Ctrl Pts',(57.6545308011779,-4.65227245534205,336.595476124474));
#30848=CARTESIAN_POINT('Ctrl Pts',(57.6468646889625,-4.60820194757135,336.723981970628));
#30849=CARTESIAN_POINT('Ctrl Pts',(57.6391985767472,-4.55881346291096,336.850629695007));
#30850=CARTESIAN_POINT('Ctrl Pts',(57.6315324645318,-4.50430324539716,336.974951983215));
#30851=CARTESIAN_POINT('Ctrl Pts',(57.6238584954147,-4.44973716104893,337.099401687768));
#30852=CARTESIAN_POINT('Ctrl Pts',(57.6161845262976,-4.39003902030269,337.221520828921));
#30853=CARTESIAN_POINT('Ctrl Pts',(57.6085105571805,-4.32545224267202,337.340864361484));
#30854=CARTESIAN_POINT('Ctrl Pts',(57.600832649253,-4.26083231465094,337.460269149381));
#30855=CARTESIAN_POINT('Ctrl Pts',(57.5931547413254,-4.19131895732629,337.576895148148));
#30856=CARTESIAN_POINT('Ctrl Pts',(57.5854768333979,-4.11719949279303,337.69032551916));
#30857=CARTESIAN_POINT('Ctrl Pts',(57.5777866395038,-4.04296142443203,337.803937398178));
#30858=CARTESIAN_POINT('Ctrl Pts',(57.5700964456096,-3.9641027559769,337.914343107769));
#30859=CARTESIAN_POINT('Ctrl Pts',(57.5624062517154,-3.88095219500436,338.021157579901));
#30860=CARTESIAN_POINT('Ctrl Pts',(57.5550799198101,-3.801735907849,338.122918118828));
#30861=CARTESIAN_POINT('Ctrl Pts',(57.5477535879048,-3.71862476919697,338.221419264264));
#30862=CARTESIAN_POINT('Ctrl Pts',(57.5404272559994,-3.63193320562401,338.316360090881));
#30863=CARTESIAN_POINT('Ctrl Pts',(57.532652177221,-3.5399316767669,338.417116160326));
#30864=CARTESIAN_POINT('Ctrl Pts',(57.5248770984425,-3.44358887110002,338.514200122131));
#30865=CARTESIAN_POINT('Ctrl Pts',(57.5171020196641,-3.34322952508125,338.60721490975));
#30866=CARTESIAN_POINT('Ctrl Pts',(57.5093365086151,-3.24299367762721,338.700115236752));
#30867=CARTESIAN_POINT('Ctrl Pts',(57.5015709975661,-3.13875140813542,338.788956089653));
#30868=CARTESIAN_POINT('Ctrl Pts',(57.4938054865171,-3.03086667518702,338.873374531302));
#30869=CARTESIAN_POINT('Ctrl Pts',(57.4860476749949,-2.92308891026529,338.95770927182));
#30870=CARTESIAN_POINT('Ctrl Pts',(57.4782898634727,-2.81167617485285,339.037630087828));
#30871=CARTESIAN_POINT('Ctrl Pts',(57.4705320519505,-2.69702786843564,339.112812144918));
#30872=CARTESIAN_POINT('Ctrl Pts',(57.4627800784275,-2.58246583850456,339.187937625125));
#30873=CARTESIAN_POINT('Ctrl Pts',(57.4550281049045,-2.46467340960457,339.258331231013));
#30874=CARTESIAN_POINT('Ctrl Pts',(57.4472761313815,-2.3440812355723,339.323709775591));
#30875=CARTESIAN_POINT('Ctrl Pts',(57.4395274408238,-2.22354013239741,339.389060632316));
#30876=CARTESIAN_POINT('Ctrl Pts',(57.4317787502662,-2.10020198526002,339.449400466076));
#30877=CARTESIAN_POINT('Ctrl Pts',(57.4240300597086,-1.97452428413207,339.504490749671));
#30878=CARTESIAN_POINT('Ctrl Pts',(57.4162829813308,-1.8488727312996,339.559569571273));
#30879=CARTESIAN_POINT('Ctrl Pts',(57.408535902953,-1.72088295045042,339.609400858372));
#30880=CARTESIAN_POINT('Ctrl Pts',(57.4007888245751,-1.59103440029527,339.653793355917));
#30881=CARTESIAN_POINT('Ctrl Pts',(57.3930416812693,-1.46118476188429,339.698186225513));
#30882=CARTESIAN_POINT('Ctrl Pts',(57.3852945379635,-1.3294766929521,339.737140088191));
#30883=CARTESIAN_POINT('Ctrl Pts',(57.3775473946577,-1.19640649861654,339.770513028236));
#30884=CARTESIAN_POINT('Ctrl Pts',(57.3697985096296,-1.06330638727604,339.803893471226));
#30885=CARTESIAN_POINT('Ctrl Pts',(57.3620496246015,-0.928843920218223,
339.831690399787));
#30886=CARTESIAN_POINT('Ctrl Pts',(57.3543007395734,-0.793526932057894,
339.853812735428));
#30887=CARTESIAN_POINT('Ctrl Pts',(57.3465436297987,-0.658066317048245,
339.875958551944));
#30888=CARTESIAN_POINT('Ctrl Pts',(57.3387865200239,-0.521749755485907,
339.892417680725));
#30889=CARTESIAN_POINT('Ctrl Pts',(57.3310294102492,-0.385092120905921,
339.90315073406));
#30890=CARTESIAN_POINT('Ctrl Pts',(57.3232681553231,-0.248361460855573,
339.913889522796));
#30891=CARTESIAN_POINT('Ctrl Pts',(57.3155069003969,-0.11128975503674,339.918896124835));
#30892=CARTESIAN_POINT('Ctrl Pts',(57.3077456454707,0.0256077464752018,
339.918183333897));
#30893=CARTESIAN_POINT('Ctrl Pts',(57.2999719750661,0.162724239374864,339.917469402726));
#30894=CARTESIAN_POINT('Ctrl Pts',(57.2921983046614,0.299665580455625,339.911017814241));
#30895=CARTESIAN_POINT('Ctrl Pts',(57.2844246342567,0.43592037065603,339.898893394732));
#30896=CARTESIAN_POINT('Ctrl Pts',(57.2770128300797,0.565832467591508,339.887333369868));
#30897=CARTESIAN_POINT('Ctrl Pts',(57.2696010259026,0.695120207681032,339.870616805978));
#30898=CARTESIAN_POINT('Ctrl Pts',(57.2621892217255,0.823350494014021,339.848842854384));
#30899=CARTESIAN_POINT('Ctrl Pts',(57.2544141429471,0.957865728658688,339.82600169656));
#30900=CARTESIAN_POINT('Ctrl Pts',(57.2466390641686,1.0916423236309,339.7975226783));
#30901=CARTESIAN_POINT('Ctrl Pts',(57.2388639853902,1.22417064367228,339.763464001929));
#30902=CARTESIAN_POINT('Ctrl Pts',(57.2310984743412,1.3565358791786,339.729447236927));
#30903=CARTESIAN_POINT('Ctrl Pts',(57.2233329632922,1.48765552116257,339.689864571792));
#30904=CARTESIAN_POINT('Ctrl Pts',(57.2155674522432,1.61702740915682,339.644825660941));
#30905=CARTESIAN_POINT('Ctrl Pts',(57.2078096407209,1.74627102454782,339.599831406301));
#30906=CARTESIAN_POINT('Ctrl Pts',(57.2000518291988,1.87376996775819,339.549391799604));
#30907=CARTESIAN_POINT('Ctrl Pts',(57.1922940176765,1.99903494062448,339.493666917859));
#30908=CARTESIAN_POINT('Ctrl Pts',(57.1845420441536,2.12420564762537,339.437983970856));
#30909=CARTESIAN_POINT('Ctrl Pts',(57.1767900706306,2.24714537480343,339.377023823733));
#30910=CARTESIAN_POINT('Ctrl Pts',(57.1690380971076,2.36738293267486,339.31099537376));
#30911=CARTESIAN_POINT('Ctrl Pts',(57.16128940655,2.48756956986963,339.244994886874));
#30912=CARTESIAN_POINT('Ctrl Pts',(57.1535407159924,2.60505597192953,339.173930553989));
#30913=CARTESIAN_POINT('Ctrl Pts',(57.1457920254348,2.71939398216957,339.098058007427));
#30914=CARTESIAN_POINT('Ctrl Pts',(57.138044947057,2.8337082034316,339.022201246783));
#30915=CARTESIAN_POINT('Ctrl Pts',(57.1302978686791,2.94487501032733,338.941538478293));
#30916=CARTESIAN_POINT('Ctrl Pts',(57.1225507903013,3.05247410978212,338.856369389933));
#30917=CARTESIAN_POINT('Ctrl Pts',(57.1148036469955,3.16007411102093,338.771199587773));
#30918=CARTESIAN_POINT('Ctrl Pts',(57.1070565036897,3.26410603869727,338.681523633007));
#30919=CARTESIAN_POINT('Ctrl Pts',(57.0993093603839,3.3641819736827,338.587682080459));
#30920=CARTESIAN_POINT('Ctrl Pts',(57.0915604753558,3.46428040786298,338.493819430338));
#30921=CARTESIAN_POINT('Ctrl Pts',(57.0838115903277,3.56042079449067,338.39578958619));
#30922=CARTESIAN_POINT('Ctrl Pts',(57.0760627052996,3.65225172527092,338.293970309179));
#30923=CARTESIAN_POINT('Ctrl Pts',(57.0683055955249,3.74418012634996,338.192042960136));
#30924=CARTESIAN_POINT('Ctrl Pts',(57.0605484857502,3.83178967218643,338.08631843434));
#30925=CARTESIAN_POINT('Ctrl Pts',(57.0527913759754,3.9147686132002,337.977208384981));
#30926=CARTESIAN_POINT('Ctrl Pts',(57.0450301210493,3.99779189550695,337.8680400307));
#30927=CARTESIAN_POINT('Ctrl Pts',(57.0372688661231,4.07617941916421,337.755482868623));
#30928=CARTESIAN_POINT('Ctrl Pts',(57.0295076111969,4.14966311130294,337.639977106945));
#30929=CARTESIAN_POINT('Ctrl Pts',(57.0217339407923,4.22326435340077,337.524286573691));
#30930=CARTESIAN_POINT('Ctrl Pts',(57.0139602703876,4.29194589235666,337.40563835374));
#30931=CARTESIAN_POINT('Ctrl Pts',(57.006186599983,4.35548549460405,337.284497574696));
#30932=CARTESIAN_POINT('Ctrl Pts',(56.9987747958058,4.41606731308076,337.168995928061));
#30933=CARTESIAN_POINT('Ctrl Pts',(56.9913629916286,4.47197501256549,337.051228817268));
#30934=CARTESIAN_POINT('Ctrl Pts',(56.9839511874514,4.52305759793053,336.931614099219));
#30935=CARTESIAN_POINT('Ctrl Pts',(56.976176108673,4.57664389297102,336.806136707526));
#30936=CARTESIAN_POINT('Ctrl Pts',(56.9684010298945,4.62508947058191,336.678229483909));
#30937=CARTESIAN_POINT('Ctrl Pts',(56.9606259511161,4.66816748145873,336.548352488147));
#30938=CARTESIAN_POINT('Ctrl Pts',(56.9528604400671,4.7111924821006,336.418635314297));
#30939=CARTESIAN_POINT('Ctrl Pts',(56.945094929018,4.74886293645054,336.28695355868));
#30940=CARTESIAN_POINT('Ctrl Pts',(56.937329417969,4.78099930740395,336.153788839044));
#30941=CARTESIAN_POINT('Ctrl Pts',(56.9295716064468,4.81310381505205,336.020756152615));
#30942=CARTESIAN_POINT('Ctrl Pts',(56.9218137949246,4.83968506775702,335.886243805791));
#30943=CARTESIAN_POINT('Ctrl Pts',(56.9140559834024,4.86061289038045,335.750749886692));
#30944=CARTESIAN_POINT('Ctrl Pts',(56.9063040098794,4.88152496415359,335.615357931064));
#30945=CARTESIAN_POINT('Ctrl Pts',(56.8985520363564,4.89679201656638,335.478986258175));
#30946=CARTESIAN_POINT('Ctrl Pts',(56.8908000628334,4.90633472612238,335.342144147613));
#30947=CARTESIAN_POINT('Ctrl Pts',(56.8830513722758,4.91587339433525,335.205359989765));
#30948=CARTESIAN_POINT('Ctrl Pts',(56.8753026817182,4.91969251424371,335.068106179615));
#30949=CARTESIAN_POINT('Ctrl Pts',(56.8675539911605,4.91776452922478,334.930897919));
#30950=CARTESIAN_POINT('Ctrl Pts',(56.8598069127827,4.91583694533923,334.793718205708));
#30951=CARTESIAN_POINT('Ctrl Pts',(56.8520598344048,4.90816464041253,334.656584413691));
#30952=CARTESIAN_POINT('Ctrl Pts',(56.844312756027,4.89477218375724,334.52001215472));
#30953=CARTESIAN_POINT('Ctrl Pts',(56.8365656127212,4.88137961486029,334.383438751142));
#30954=CARTESIAN_POINT('Ctrl Pts',(56.8288184694154,4.86226683676075,334.247427279006));
#30955=CARTESIAN_POINT('Ctrl Pts',(56.8210713261096,4.8375103039781,334.112488241539));
#30956=CARTESIAN_POINT('Ctrl Pts',(56.8133224410815,4.81274820540122,333.977518866912));
#30957=CARTESIAN_POINT('Ctrl Pts',(56.8055735560533,4.78233989782012,333.843622791111));
#30958=CARTESIAN_POINT('Ctrl Pts',(56.7978246710252,4.74641288146532,333.711299949111));
#30959=CARTESIAN_POINT('Ctrl Pts',(56.7900675612505,4.71044773180424,333.57883665828));
#30960=CARTESIAN_POINT('Ctrl Pts',(56.7823104514757,4.66895227481521,333.447950314738));
#30961=CARTESIAN_POINT('Ctrl Pts',(56.774553341701,4.62210397286131,333.31912584452));
#30962=CARTESIAN_POINT('Ctrl Pts',(56.7667920867748,4.57523063667273,333.190232534624));
#30963=CARTESIAN_POINT('Ctrl Pts',(56.7590308318486,4.52299890470561,333.063403654727));
#30964=CARTESIAN_POINT('Ctrl Pts',(56.7512695769224,4.46563388781244,332.939102854939));
#30965=CARTESIAN_POINT('Ctrl Pts',(56.7434959065178,4.40817710558753,332.81460321438));
#30966=CARTESIAN_POINT('Ctrl Pts',(56.7357222361131,4.34557080785631,332.692640083167));
#30967=CARTESIAN_POINT('Ctrl Pts',(56.7279485657084,4.27808586701096,332.573652049482));
#30968=CARTESIAN_POINT('Ctrl Pts',(56.7205367615314,4.21374236639908,332.460202937395));
#30969=CARTESIAN_POINT('Ctrl Pts',(56.7131249573545,4.14496435465852,332.349458419038));
#30970=CARTESIAN_POINT('Ctrl Pts',(56.7057131531776,4.07202150444447,332.241771595781));
#30971=CARTESIAN_POINT('Ctrl Pts',(56.6979380743991,3.99550350785452,332.128806720532));
#30972=CARTESIAN_POINT('Ctrl Pts',(56.6901629956207,3.91416027658614,332.018849862764));
#30973=CARTESIAN_POINT('Ctrl Pts',(56.6823879168423,3.82825592354718,331.912340749641));
#30974=CARTESIAN_POINT('Ctrl Pts',(56.6746224057933,3.74245728128369,331.805962702763));
#30975=CARTESIAN_POINT('Ctrl Pts',(56.6668568947443,3.65210892805783,331.703024260175));
#30976=CARTESIAN_POINT('Ctrl Pts',(56.6590913836953,3.55751870867872,331.603937029456));
#30977=CARTESIAN_POINT('Ctrl Pts',(56.6513335721731,3.46302227577733,331.504948044014));
#30978=CARTESIAN_POINT('Ctrl Pts',(56.6435757606508,3.3642926147085,331.409802952345));
#30979=CARTESIAN_POINT('Ctrl Pts',(56.6358179491286,3.26167813316202,331.318880765562));
#30980=CARTESIAN_POINT('Ctrl Pts',(56.6280659756056,3.15914087226707,331.228027000607));
#30981=CARTESIAN_POINT('Ctrl Pts',(56.6203140020826,3.05272490125626,331.141390073319));
#30982=CARTESIAN_POINT('Ctrl Pts',(56.6125620285596,2.94281555878699,331.059312287245));
#30983=CARTESIAN_POINT('Ctrl Pts',(56.604813338002,2.83295276298965,330.977269261161));
#30984=CARTESIAN_POINT('Ctrl Pts',(56.5970646474443,2.71959985077697,330.899781769459));
#30985=CARTESIAN_POINT('Ctrl Pts',(56.5893159568867,2.60317515389412,330.827151790366));
#30986=CARTESIAN_POINT('Ctrl Pts',(56.5815688785089,2.48677468014185,330.754536922546));
#30987=CARTESIAN_POINT('Ctrl Pts',(56.5738218001311,2.36730402438114,330.686777763845));
#30988=CARTESIAN_POINT('Ctrl Pts',(56.5660747217533,2.24521007141623,330.624132680518));
#30989=CARTESIAN_POINT('Ctrl Pts',(56.5583275784475,2.12311509518648,330.561487072165));
#30990=CARTESIAN_POINT('Ctrl Pts',(56.5505804351417,1.99839712566912,330.503955803113));
#30991=CARTESIAN_POINT('Ctrl Pts',(56.5428332918359,1.87152682984747,330.451750843713));
#30992=CARTESIAN_POINT('Ctrl Pts',(56.5350844068078,1.74462801088971,330.399534147531));
#30993=CARTESIAN_POINT('Ctrl Pts',(56.5273355217797,1.61557626414142,330.352646292538));
#30994=CARTESIAN_POINT('Ctrl Pts',(56.5195866367516,1.48486099327881,330.311250604571));
#30995=CARTESIAN_POINT('Ctrl Pts',(56.5118295269769,1.35400697987717,330.269810978793));
#30996=CARTESIAN_POINT('Ctrl Pts',(56.5040724172021,1.22148628846988,330.233875283094));
#30997=CARTESIAN_POINT('Ctrl Pts',(56.4963153074274,1.08780273877196,330.20355670689));
#30998=CARTESIAN_POINT('Ctrl Pts',(56.4885540525012,0.954047752859172,330.173221929408));
#30999=CARTESIAN_POINT('Ctrl Pts',(56.4807927975751,0.819129054755004,330.148510322783));
#31000=CARTESIAN_POINT('Ctrl Pts',(56.4730315426489,0.683558358126731,330.129483494173));
#31001=CARTESIAN_POINT('Ctrl Pts',(56.4652578722443,0.547770792566609,330.110426228838));
#31002=CARTESIAN_POINT('Ctrl Pts',(56.4574842018396,0.41132953350921,330.097071951704));
#31003=CARTESIAN_POINT('Ctrl Pts',(56.4497105314349,0.274749983709251,330.08943022563));
#31004=CARTESIAN_POINT('Ctrl Pts',(56.4422987272578,0.144528244811165,330.082144223744));
#31005=CARTESIAN_POINT('Ctrl Pts',(56.4348869230807,0.0141810880569334,
330.080050907729));
#31006=CARTESIAN_POINT('Ctrl Pts',(56.4274751189036,-0.115848620730662,
330.083114587508));
#31007=CARTESIAN_POINT('Ctrl Pts',(56.4197000401252,-0.252251472883883,
330.08632842736));
#31008=CARTESIAN_POINT('Ctrl Pts',(56.4119249613468,-0.38873603032035,330.095227720854));
#31009=CARTESIAN_POINT('Ctrl Pts',(56.4041498825684,-0.524789590437118,
330.109828331411));
#31010=CARTESIAN_POINT('Ctrl Pts',(56.3963843715194,-0.660675727986569,
330.124410974988));
#31011=CARTESIAN_POINT('Ctrl Pts',(56.3886188604704,-0.796131538572317,
330.144680934822));
#31012=CARTESIAN_POINT('Ctrl Pts',(56.3808533494214,-0.930644300109056,
330.170602082125));
#31013=CARTESIAN_POINT('Ctrl Pts',(56.3730955378992,-1.06502369185111,330.196497528535));
#31014=CARTESIAN_POINT('Ctrl Pts',(56.365337726377,-1.19846151397801,330.228032938307));
#31015=CARTESIAN_POINT('Ctrl Pts',(56.3575799148549,-1.33045050456621,330.26512043264));
#31016=CARTESIAN_POINT('Ctrl Pts',(56.3498279413318,-1.46234016925374,330.302180017459));
#31017=CARTESIAN_POINT('Ctrl Pts',(56.3420759678088,-1.59278279778895,330.344783265186));
#31018=CARTESIAN_POINT('Ctrl Pts',(56.3343239942858,-1.7212820109589,330.392791376414));
#31019=CARTESIAN_POINT('Ctrl Pts',(56.3265753037282,-1.84972680463568,330.440779156178));
#31020=CARTESIAN_POINT('Ctrl Pts',(56.3188266131706,-1.97622945451844,330.494167110345));
#31021=CARTESIAN_POINT('Ctrl Pts',(56.311077922613,-2.10030963736182,330.552766872571));
#31022=CARTESIAN_POINT('Ctrl Pts',(56.3033308442351,-2.22436400428681,330.611354442627));
#31023=CARTESIAN_POINT('Ctrl Pts',(56.2955837658573,-2.34599655347423,330.675151497058));
#31024=CARTESIAN_POINT('Ctrl Pts',(56.2878366874794,-2.46474818421698,330.743922057704));
#31025=CARTESIAN_POINT('Ctrl Pts',(56.2800895441736,-2.58350081021221,330.812693194713));
#31026=CARTESIAN_POINT('Ctrl Pts',(56.2723424008679,-2.6993721313554,330.886437725194));
#31027=CARTESIAN_POINT('Ctrl Pts',(56.2645952575621,-2.81192919234291,330.964874564558));
#31028=CARTESIAN_POINT('Ctrl Pts',(56.256846372534,-2.92451155854755,331.043329038189));
#31029=CARTESIAN_POINT('Ctrl Pts',(56.249097487506,-3.03377786127287,331.126477696467));
#31030=CARTESIAN_POINT('Ctrl Pts',(56.2413486024779,-3.13932591192704,331.21399737438));
#31031=CARTESIAN_POINT('Ctrl Pts',(56.2335914927032,-3.24498599237297,331.301609946583));
#31032=CARTESIAN_POINT('Ctrl Pts',(56.2258343829284,-3.34691963569661,331.39360255626));
#31033=CARTESIAN_POINT('Ctrl Pts',(56.2180772731537,-3.44475901274711,331.489612783951));
#31034=CARTESIAN_POINT('Ctrl Pts',(56.2103160182276,-3.5426506720322,331.585674316438));
#31035=CARTESIAN_POINT('Ctrl Pts',(56.2025547633014,-3.63644343841991,331.685757459741));
#31036=CARTESIAN_POINT('Ctrl Pts',(56.1947935083752,-3.7258085875077,331.789465242089));
#31037=CARTESIAN_POINT('Ctrl Pts',(56.1870198379706,-3.81531669171012,331.893338923091));
#31038=CARTESIAN_POINT('Ctrl Pts',(56.1792461675659,-3.90038278252682,332.000848523054));
#31039=CARTESIAN_POINT('Ctrl Pts',(56.1714724971613,-3.98071990434125,332.111565803817));
#31040=CARTESIAN_POINT('Ctrl Pts',(56.1640606929841,-4.05731731380821,332.217129168524));
#31041=CARTESIAN_POINT('Ctrl Pts',(56.1566488888069,-4.12961595374309,332.325608060064));
#31042=CARTESIAN_POINT('Ctrl Pts',(56.1492370846297,-4.1974061765844,332.43661074917));
#31043=CARTESIAN_POINT('Ctrl Pts',(56.1412198285504,-4.27073401461147,332.556680972664));
#31044=CARTESIAN_POINT('Ctrl Pts',(56.1332025724711,-4.33900642600092,332.680064084548));
#31045=CARTESIAN_POINT('Ctrl Pts',(56.1251853163918,-4.40192101234788,332.806310308282));
#31046=CARTESIAN_POINT('Ctrl Pts',(56.1171799294359,-4.46474245697842,332.932369631161));
#31047=CARTESIAN_POINT('Ctrl Pts',(56.10917454248,-4.52222171530947,333.061283306954));
#31048=CARTESIAN_POINT('Ctrl Pts',(56.1011691555242,-4.57410032287582,333.192573846939));
#31049=CARTESIAN_POINT('Ctrl Pts',(56.0931743527628,-4.62591033996967,333.323690803234));
#31050=CARTESIAN_POINT('Ctrl Pts',(56.0851795500014,-4.67213432462472,333.457178033807));
#31051=CARTESIAN_POINT('Ctrl Pts',(56.0771847472401,-4.71256030916059,333.59253476241));
#31052=CARTESIAN_POINT('Ctrl Pts',(56.069201958957,-4.75292554208981,333.727688078806));
#31053=CARTESIAN_POINT('Ctrl Pts',(56.0612191706739,-4.7875100435083,333.864704951177));
#31054=CARTESIAN_POINT('Ctrl Pts',(56.0532363823908,-4.8161506074193,334.003066507156));
#31055=CARTESIAN_POINT('Ctrl Pts',(56.0452607064753,-4.84476565365275,334.141304788132));
#31056=CARTESIAN_POINT('Ctrl Pts',(56.0372850305599,-4.86744723670225,334.280885017952));
#31057=CARTESIAN_POINT('Ctrl Pts',(56.0293093546443,-4.88408227987325,334.421274377681));
#31058=CARTESIAN_POINT('Ctrl Pts',(56.0213410202696,-4.90070201063064,334.561534510217));
#31059=CARTESIAN_POINT('Ctrl Pts',(56.0133726858949,-4.91128625380656,334.702601933746));
#31060=CARTESIAN_POINT('Ctrl Pts',(56.0054043515202,-4.91577326859276,334.843935159985));
#31061=CARTESIAN_POINT('Ctrl Pts',(56.0024483171769,-4.91743782848488,334.896365925434));
#31062=CARTESIAN_POINT('Ctrl Pts',(55.9994922828334,-4.91826379365925,334.94883319718));
#31063=CARTESIAN_POINT('Ctrl Pts',(55.9965362484901,-4.91824982577043,335.00130912533));
#31064=CARTESIAN_POINT('',(59.4965362854383,-4.92235223384019,335.000920754802));
#31065=CARTESIAN_POINT('Ctrl Pts',(59.4965362484901,-4.92614409942434,335.000922113078));
#31066=CARTESIAN_POINT('Ctrl Pts',(59.4937219976324,-4.9262713585574,335.050394967013));
#31067=CARTESIAN_POINT('Ctrl Pts',(59.39816173535,-4.90316042549208,336.730165617781));
#31068=CARTESIAN_POINT('Ctrl Pts',(59.209855461643,-2.99763204210603,339.983838982809));
#31069=CARTESIAN_POINT('Ctrl Pts',(58.9316174273691,2.56882582411236,340.217813982101));
#31070=CARTESIAN_POINT('Ctrl Pts',(58.6533793930951,5.77791014734984,335.663478104826));
#31071=CARTESIAN_POINT('Ctrl Pts',(58.3751413588212,3.68469161017836,330.500278163674));
#31072=CARTESIAN_POINT('Ctrl Pts',(58.0969033245472,-1.78991403169479,329.466406535932));
#31073=CARTESIAN_POINT('Ctrl Pts',(57.887368524017,-4.6757280257409,332.512021663937));
#31074=CARTESIAN_POINT('Ctrl Pts',(57.7705797349114,-4.92074476144685,334.570768816846));
#31075=CARTESIAN_POINT('Ctrl Pts',(57.7465369572303,-4.91693737480017,334.995484483173));
#31076=CARTESIAN_POINT('',(61.246536248442,-4.91824836367761,335.004011942491));
#31077=CARTESIAN_POINT('Ctrl Pts',(61.2465362484419,-4.91824836367761,335.004011942491));
#31078=CARTESIAN_POINT('Ctrl Pts',(61.2373935566682,-4.91811632314456,335.165880697366));
#31079=CARTESIAN_POINT('Ctrl Pts',(61.2282508648945,-4.9099893496518,335.327409458201));
#31080=CARTESIAN_POINT('Ctrl Pts',(61.2191081731208,-4.89399104746928,335.48788798898));
#31081=CARTESIAN_POINT('Ctrl Pts',(61.2099024893427,-4.87788251898293,335.649472196791));
#31082=CARTESIAN_POINT('Ctrl Pts',(61.2006968055647,-4.85379392770351,335.809991592536));
#31083=CARTESIAN_POINT('Ctrl Pts',(61.1914911217866,-4.82190030170716,335.968741731782));
#31084=CARTESIAN_POINT('Ctrl Pts',(61.1822161920626,-4.78976676911054,336.128686003242));
#31085=CARTESIAN_POINT('Ctrl Pts',(61.1729412623387,-4.74971040607306,336.286834244761));
#31086=CARTESIAN_POINT('Ctrl Pts',(61.1636663326148,-4.70195835134677,336.442487686152));
#31087=CARTESIAN_POINT('Ctrl Pts',(61.1616181222634,-4.6914131228975,336.476861099145));
#31088=CARTESIAN_POINT('Ctrl Pts',(61.159569911912,-4.68049277986775,336.511112932837));
#31089=CARTESIAN_POINT('Ctrl Pts',(61.1575217015606,-4.66920007739127,336.545235807179));
#31090=CARTESIAN_POINT('Ctrl Pts',(61.1497466227822,-4.62633258025302,336.674767442432));
#31091=CARTESIAN_POINT('Ctrl Pts',(61.1419715440037,-4.57800311475789,336.802718583922));
#31092=CARTESIAN_POINT('Ctrl Pts',(61.1341964652253,-4.52434608075795,336.928594204085));
#31093=CARTESIAN_POINT('Ctrl Pts',(61.1264309541762,-4.47075507515425,337.054314926284));
#31094=CARTESIAN_POINT('Ctrl Pts',(61.1186654431272,-4.4118496972396,337.177964852875));
#31095=CARTESIAN_POINT('Ctrl Pts',(61.1108999320782,-4.34781408305863,337.2990641056));
#31096=CARTESIAN_POINT('Ctrl Pts',(61.103142120556,-4.28384196037555,337.420043288062));
#31097=CARTESIAN_POINT('Ctrl Pts',(61.0953843090337,-4.21474990567511,337.538476486199));
#31098=CARTESIAN_POINT('Ctrl Pts',(61.0876264975115,-4.14076996092782,337.653904141671));
#31099=CARTESIAN_POINT('Ctrl Pts',(61.0798745239885,-4.06684568843509,337.769244934172));
#31100=CARTESIAN_POINT('Ctrl Pts',(61.0721225504655,-3.98804105742427,337.881584358183));
#31101=CARTESIAN_POINT('Ctrl Pts',(61.0643705769425,-3.90463364052436,337.990488119987));
#31102=CARTESIAN_POINT('Ctrl Pts',(61.0566218863849,-3.82126154671502,338.099345760984));
#31103=CARTESIAN_POINT('Ctrl Pts',(61.0488731958272,-3.73329078117446,338.204770324002));
#31104=CARTESIAN_POINT('Ctrl Pts',(61.0411245052696,-3.64104164318245,338.306357333246));
#31105=CARTESIAN_POINT('Ctrl Pts',(61.0333774268918,-3.54881169839407,338.407923206465));
#31106=CARTESIAN_POINT('Ctrl Pts',(61.0256303485139,-3.45230541433311,338.505652824865));
#31107=CARTESIAN_POINT('Ctrl Pts',(61.0178832701361,-3.35188243959219,338.599175902016));
#31108=CARTESIAN_POINT('Ctrl Pts',(61.0101361268303,-3.25145862321008,338.692699762981));
#31109=CARTESIAN_POINT('Ctrl Pts',(61.0023889835245,-3.14711833671667,338.78201674599));
#31110=CARTESIAN_POINT('Ctrl Pts',(60.9946418402186,-3.03925674544342,338.866794731787));
#31111=CARTESIAN_POINT('Ctrl Pts',(60.9868929551905,-2.93137090459449,338.951591777475));
#31112=CARTESIAN_POINT('Ctrl Pts',(60.9791440701625,-2.81996249089327,339.031847553848));
#31113=CARTESIAN_POINT('Ctrl Pts',(60.9713951851344,-2.70545794384329,339.107271646312));
#31114=CARTESIAN_POINT('Ctrl Pts',(60.9636380753596,-2.59083186048403,339.182775794686));
#31115=CARTESIAN_POINT('Ctrl Pts',(60.9558809655849,-2.4731034060855,339.253437799337));
#31116=CARTESIAN_POINT('Ctrl Pts',(60.9481238558101,-2.35272654315668,339.31901156234));
#31117=CARTESIAN_POINT('Ctrl Pts',(60.940362600884,-2.23228535468121,339.384620365865));
#31118=CARTESIAN_POINT('Ctrl Pts',(60.9326013459578,-2.10919328831053,339.445135337539));
#31119=CARTESIAN_POINT('Ctrl Pts',(60.9248400910316,-1.98392594759599,339.50035786321));
#31120=CARTESIAN_POINT('Ctrl Pts',(60.917066420627,-1.85845821996083,339.555668726925));
#31121=CARTESIAN_POINT('Ctrl Pts',(60.9092927502223,-1.73080862859112,339.605670084048));
#31122=CARTESIAN_POINT('Ctrl Pts',(60.9015190798176,-1.6014704979069,339.650212393734));
#31123=CARTESIAN_POINT('Ctrl Pts',(60.8941072756407,-1.47815308832491,339.692681248186));
#31124=CARTESIAN_POINT('Ctrl Pts',(60.8866954714637,-1.35330108031076,339.730187772153));
#31125=CARTESIAN_POINT('Ctrl Pts',(60.8792836672867,-1.22735032410398,339.76264571897));
#31126=CARTESIAN_POINT('Ctrl Pts',(60.8715085885083,-1.09522634614551,339.796694526447));
#31127=CARTESIAN_POINT('Ctrl Pts',(60.8637335097299,-0.961475654625873,
339.825294952343));
#31128=CARTESIAN_POINT('Ctrl Pts',(60.8559584309514,-0.826587260254591,
339.848292128542));
#31129=CARTESIAN_POINT('Ctrl Pts',(60.8481929199024,-0.691864854639906,
339.871261005252));
#31130=CARTESIAN_POINT('Ctrl Pts',(60.8404274088534,-0.556007913434547,
339.888640286582));
#31131=CARTESIAN_POINT('Ctrl Pts',(60.8326618978044,-0.419519623083472,
339.9003251268));
#31132=CARTESIAN_POINT('Ctrl Pts',(60.8249040862822,-0.283166661269655,
339.911998381465));
#31133=CARTESIAN_POINT('Ctrl Pts',(60.81714627476,-0.146183982995693,339.91798839786));
#31134=CARTESIAN_POINT('Ctrl Pts',(60.8093884632378,-0.00908361189721485,
339.918241611643));
#31135=CARTESIAN_POINT('Ctrl Pts',(60.8016364897148,0.127913586824123,339.918494634874));
#31136=CARTESIAN_POINT('Ctrl Pts',(60.7938845161918,0.265027912780756,339.913019447802));
#31137=CARTESIAN_POINT('Ctrl Pts',(60.7861325426688,0.401743948642575,339.90181444592));
#31138=CARTESIAN_POINT('Ctrl Pts',(60.7783838521111,0.538402085182131,339.890614189363));
#31139=CARTESIAN_POINT('Ctrl Pts',(60.7706351615535,0.674661878354404,339.873688976156));
#31140=CARTESIAN_POINT('Ctrl Pts',(60.7628864709959,0.810009863513417,339.851089267733));
#31141=CARTESIAN_POINT('Ctrl Pts',(60.755139392618,0.945329688393576,339.828494261368));
#31142=CARTESIAN_POINT('Ctrl Pts',(60.7473923142402,1.07973769731095,339.80022717247));
#31143=CARTESIAN_POINT('Ctrl Pts',(60.7396452358624,1.21272788201621,339.76639005398));
#31144=CARTESIAN_POINT('Ctrl Pts',(60.7318980925566,1.34571918130723,339.732552651902));
#31145=CARTESIAN_POINT('Ctrl Pts',(60.7241509492508,1.4772922538798,339.693145223501));
#31146=CARTESIAN_POINT('Ctrl Pts',(60.716403805945,1.60695396693021,339.648320342948));
#31147=CARTESIAN_POINT('Ctrl Pts',(60.7086549209169,1.73664483068643,339.60348538481));
#31148=CARTESIAN_POINT('Ctrl Pts',(60.7009060358888,1.8644231104876,339.553230678606));
#31149=CARTESIAN_POINT('Ctrl Pts',(60.6931571508607,1.9898138196204,339.49775766641));
#31150=CARTESIAN_POINT('Ctrl Pts',(60.685400041086,2.11533761974757,339.442225774585));
#31151=CARTESIAN_POINT('Ctrl Pts',(60.6776429313112,2.23846842889919,339.381464670957));
#31152=CARTESIAN_POINT('Ctrl Pts',(60.6698858215365,2.35875363291676,339.315722924575));
#31153=CARTESIAN_POINT('Ctrl Pts',(60.6621245666103,2.47910311350138,339.249946047906));
#31154=CARTESIAN_POINT('Ctrl Pts',(60.6543633116841,2.59660362434685,339.179183426762));
#31155=CARTESIAN_POINT('Ctrl Pts',(60.646602056758,2.71083077020372,339.103727524802));
#31156=CARTESIAN_POINT('Ctrl Pts',(60.6388283863533,2.82524064226742,339.02815091799));
#31157=CARTESIAN_POINT('Ctrl Pts',(60.6310547159486,2.93636636862656,338.947866256739));
#31158=CARTESIAN_POINT('Ctrl Pts',(60.623281045544,3.0438152310433,338.863207462947));
#31159=CARTESIAN_POINT('Ctrl Pts',(60.6158692413669,3.14626232306398,338.782489556373));
#31160=CARTESIAN_POINT('Ctrl Pts',(60.6084574371898,3.24536694477937,338.697795771474));
#31161=CARTESIAN_POINT('Ctrl Pts',(60.6010456330127,3.3408207059551,338.609445950996));
#31162=CARTESIAN_POINT('Ctrl Pts',(60.5932705542342,3.44095294030791,338.516765842636));
#31163=CARTESIAN_POINT('Ctrl Pts',(60.5854954754558,3.53738382240136,338.419769364235));
#31164=CARTESIAN_POINT('Ctrl Pts',(60.5777203966774,3.62971848857881,338.31878392731));
#31165=CARTESIAN_POINT('Ctrl Pts',(60.5699548856283,3.72193953107127,338.217922759393));
#31166=CARTESIAN_POINT('Ctrl Pts',(60.5621893745793,3.81007412586831,338.113082685504));
#31167=CARTESIAN_POINT('Ctrl Pts',(60.5544238635303,3.89376180289814,338.004630107816));
#31168=CARTESIAN_POINT('Ctrl Pts',(60.5466660520081,3.97736650335248,337.896285061174));
#31169=CARTESIAN_POINT('Ctrl Pts',(60.5389082404859,4.05653282320891,337.784334946195));
#31170=CARTESIAN_POINT('Ctrl Pts',(60.5311504289637,4.13093863369961,337.669181347737));
#31171=CARTESIAN_POINT('Ctrl Pts',(60.5233984554407,4.20528845145833,337.554114406014));
#31172=CARTESIAN_POINT('Ctrl Pts',(60.5156464819177,4.27488467923452,337.43584910622));
#31173=CARTESIAN_POINT('Ctrl Pts',(60.5078945083947,4.33944704587327,337.314818005495));
#31174=CARTESIAN_POINT('Ctrl Pts',(60.5001458178371,4.40398207031145,337.193838161512));
#31175=CARTESIAN_POINT('Ctrl Pts',(60.4923971272795,4.46348729011247,337.070095190423));
#31176=CARTESIAN_POINT('Ctrl Pts',(60.4846484367219,4.51772727419102,336.944048183181));
#31177=CARTESIAN_POINT('Ctrl Pts',(60.476901358344,4.57195597318787,336.818027401072));
#31178=CARTESIAN_POINT('Ctrl Pts',(60.4691542799662,4.62092146103723,336.689703895137));
#31179=CARTESIAN_POINT('Ctrl Pts',(60.4614072015883,4.66443572613481,336.559558405209));
#31180=CARTESIAN_POINT('Ctrl Pts',(60.4536600582825,4.70795035592381,336.429411824536));
#31181=CARTESIAN_POINT('Ctrl Pts',(60.4459129149767,4.74601354789115,336.297443600116));
#31182=CARTESIAN_POINT('Ctrl Pts',(60.4381657716709,4.7784867424562,336.164150984482));
#31183=CARTESIAN_POINT('Ctrl Pts',(60.4304168866428,4.8109672376848,336.030828401838));
#31184=CARTESIAN_POINT('Ctrl Pts',(60.4226680016147,4.83785514221687,335.896181215182));
#31185=CARTESIAN_POINT('Ctrl Pts',(60.4149191165866,4.85906281042534,335.760717862838));
#31186=CARTESIAN_POINT('Ctrl Pts',(60.4071620068119,4.88029298867198,335.625110728293));
#31187=CARTESIAN_POINT('Ctrl Pts',(60.3994048970371,4.89583082642603,335.488686084352));
#31188=CARTESIAN_POINT('Ctrl Pts',(60.3916477872624,4.90564041521214,335.351959058894));
#31189=CARTESIAN_POINT('Ctrl Pts',(60.3838865323362,4.91545524592883,335.215158970884));
#31190=CARTESIAN_POINT('Ctrl Pts',(60.3761252774101,4.91953571675091,335.078056569892));
#31191=CARTESIAN_POINT('Ctrl Pts',(60.3683640224839,4.91789810198718,334.941167007802));
#31192=CARTESIAN_POINT('Ctrl Pts',(60.3605903520792,4.91625786757352,334.804058467026));
#31193=CARTESIAN_POINT('Ctrl Pts',(60.3528166816745,4.90888129005536,334.667163836031));
#31194=CARTESIAN_POINT('Ctrl Pts',(60.3450430112699,4.89583664910739,334.530994064263));
#31195=CARTESIAN_POINT('Ctrl Pts',(60.3376312070928,4.88339923933396,334.401163028131));
#31196=CARTESIAN_POINT('Ctrl Pts',(60.3302194029158,4.86580962618219,334.27199117069));
#31197=CARTESIAN_POINT('Ctrl Pts',(60.3228075987387,4.84316988458913,334.143910909129));
#31198=CARTESIAN_POINT('Ctrl Pts',(60.3150325199603,4.81942050182019,334.009553052417));
#31199=CARTESIAN_POINT('Ctrl Pts',(60.3072574411819,4.7900383773079,333.875971906282));
#31200=CARTESIAN_POINT('Ctrl Pts',(60.2994823624034,4.75508515499803,333.743676701156));
#31201=CARTESIAN_POINT('Ctrl Pts',(60.2917168513544,4.72017494485344,333.611544293703));
#31202=CARTESIAN_POINT('Ctrl Pts',(60.2839513403054,4.67970737646155,333.480695052965));
#31203=CARTESIAN_POINT('Ctrl Pts',(60.2761858292564,4.6337954941881,333.351630387158));
#31204=CARTESIAN_POINT('Ctrl Pts',(60.2684280177342,4.58792913367964,333.222693689342));
#31205=CARTESIAN_POINT('Ctrl Pts',(60.260670206212,4.5366293318795,333.095538411124));
#31206=CARTESIAN_POINT('Ctrl Pts',(60.2529123946898,4.48005946770334,332.970652758067));
#31207=CARTESIAN_POINT('Ctrl Pts',(60.2451604211668,4.42353217414386,332.845861085424));
#31208=CARTESIAN_POINT('Ctrl Pts',(60.2374084476438,4.36174287274813,332.723335992936));
#31209=CARTESIAN_POINT('Ctrl Pts',(60.2296564741208,4.29490363923846,332.603547248086));
#31210=CARTESIAN_POINT('Ctrl Pts',(60.2219077835632,4.22809271218391,332.48380923384));
#31211=CARTESIAN_POINT('Ctrl Pts',(60.2141590930056,4.15623629669805,332.366805602995));
#31212=CARTESIAN_POINT('Ctrl Pts',(60.2064104024479,4.07959304688827,332.25298277503));
#31213=CARTESIAN_POINT('Ctrl Pts',(60.1986633240701,4.00296574334676,332.139183628855));
#31214=CARTESIAN_POINT('Ctrl Pts',(60.1909162456923,3.92155380465824,332.028564293227));
#31215=CARTESIAN_POINT('Ctrl Pts',(60.1831691673145,3.83565975133767,331.921543027023));
#31216=CARTESIAN_POINT('Ctrl Pts',(60.1754220240087,3.74976497814225,331.814520863879));
#31217=CARTESIAN_POINT('Ctrl Pts',(60.1676748807029,3.65938826004781,331.711097135142));
#31218=CARTESIAN_POINT('Ctrl Pts',(60.1599277373971,3.5648727647788,331.611657450399));
#31219=CARTESIAN_POINT('Ctrl Pts',(60.152178852369,3.47033602041984,331.512195409503));
#31220=CARTESIAN_POINT('Ctrl Pts',(60.1444299673409,3.37165891655857,331.4167194782));
#31221=CARTESIAN_POINT('Ctrl Pts',(60.1366810823128,3.26922157975248,331.325578504719));
#31222=CARTESIAN_POINT('Ctrl Pts',(60.128923972538,3.16667551489865,331.234340793268));
#31223=CARTESIAN_POINT('Ctrl Pts',(60.1211668627633,3.06036153688643,331.147447491134));
#31224=CARTESIAN_POINT('Ctrl Pts',(60.1134097529886,2.95069339560144,331.065207559775));
#31225=CARTESIAN_POINT('Ctrl Pts',(60.1056484980624,2.84096665116833,330.982923682026));
#31226=CARTESIAN_POINT('Ctrl Pts',(60.0978872431363,2.72788249412141,330.905298350947));
#31227=CARTESIAN_POINT('Ctrl Pts',(60.0901259882101,2.61188293363476,330.832596659371));
#31228=CARTESIAN_POINT('Ctrl Pts',(60.0823523178054,2.4956978116555,330.759778668781));
#31229=CARTESIAN_POINT('Ctrl Pts',(60.0745786474008,2.37658830657052,330.691900250345));
#31230=CARTESIAN_POINT('Ctrl Pts',(60.0668049769961,2.25502103671737,330.62918049029));
#31231=CARTESIAN_POINT('Ctrl Pts',(60.059393172819,2.13911275252312,330.569380350154));
#31232=CARTESIAN_POINT('Ctrl Pts',(60.051981368642,2.02097063287131,330.51426952717));
#31233=CARTESIAN_POINT('Ctrl Pts',(60.0445695644649,1.90101354520732,330.463996190099));
#31234=CARTESIAN_POINT('Ctrl Pts',(60.0367944856864,1.77517700334329,330.411258807021));
#31235=CARTESIAN_POINT('Ctrl Pts',(60.029019406908,1.64694541421068,330.363678439306));
#31236=CARTESIAN_POINT('Ctrl Pts',(60.0212443281296,1.51678035961847,330.321478823049));
#31237=CARTESIAN_POINT('Ctrl Pts',(60.0134788170806,1.38677548141265,330.279331136107));
#31238=CARTESIAN_POINT('Ctrl Pts',(60.0057133060316,1.25484224004473,330.242551145415));
#31239=CARTESIAN_POINT('Ctrl Pts',(59.9979477949825,1.12146345517206,330.211315130308));
#31240=CARTESIAN_POINT('Ctrl Pts',(59.9901899834603,0.988216915753007,330.180110085802));
#31241=CARTESIAN_POINT('Ctrl Pts',(59.9824321719381,0.853528063224444,330.154438166357));
#31242=CARTESIAN_POINT('Ctrl Pts',(59.9746743604159,0.717895853766025,330.134426179201));
#31243=CARTESIAN_POINT('Ctrl Pts',(59.9669223868929,0.582365711846368,330.1144292517));
#31244=CARTESIAN_POINT('Ctrl Pts',(59.9591704133699,0.445894011160946,330.100083835427));
#31245=CARTESIAN_POINT('Ctrl Pts',(59.9514184398469,0.308990555549207,330.091465809523));
#31246=CARTESIAN_POINT('Ctrl Pts',(59.9436697492893,0.172145078632198,330.082851433358));
#31247=CARTESIAN_POINT('Ctrl Pts',(59.9359210587316,0.0348685997518534,
330.079959647812));
#31248=CARTESIAN_POINT('Ctrl Pts',(59.928172368174,-0.10232350484836,330.082814528325));
#31249=CARTESIAN_POINT('Ctrl Pts',(59.9204252897962,-0.239487065485361,
330.085668814856));
#31250=CARTESIAN_POINT('Ctrl Pts',(59.9126782114184,-0.376565896215581,
330.094267381102));
#31251=CARTESIAN_POINT('Ctrl Pts',(59.9049311330405,-0.513044563016202,
330.108582174987));
#31252=CARTESIAN_POINT('Ctrl Pts',(59.8971839897347,-0.64952437363941,330.122897088843));
#31253=CARTESIAN_POINT('Ctrl Pts',(59.8894368464289,-0.785403621558577,
330.14292828512));
#31254=CARTESIAN_POINT('Ctrl Pts',(59.8816897031231,-0.92017233169974,330.168595862229));
#31255=CARTESIAN_POINT('Ctrl Pts',(59.873940818095,-1.05497134070807,330.194269209954));
#31256=CARTESIAN_POINT('Ctrl Pts',(59.8661919330669,-1.18865893122083,330.225581386939));
#31257=CARTESIAN_POINT('Ctrl Pts',(59.8584430480389,-1.32073604102711,330.262401518445));
#31258=CARTESIAN_POINT('Ctrl Pts',(59.8506859382641,-1.45295333884254,330.29926073122));
#31259=CARTESIAN_POINT('Ctrl Pts',(59.8429288284894,-1.583556364191,330.341639471718));
#31260=CARTESIAN_POINT('Ctrl Pts',(59.8351717187147,-1.71206140098901,330.389357005607));
#31261=CARTESIAN_POINT('Ctrl Pts',(59.8274104637885,-1.84063510676971,330.43710003822));
#31262=CARTESIAN_POINT('Ctrl Pts',(59.8196492088623,-1.96710822988306,330.490187397639));
#31263=CARTESIAN_POINT('Ctrl Pts',(59.8118879539362,-2.09101865158471,330.54839084586));
#31264=CARTESIAN_POINT('Ctrl Pts',(59.8041142835315,-2.21512728957886,330.60668740063));
#31265=CARTESIAN_POINT('Ctrl Pts',(59.7963406131268,-2.33666468746766,330.670116217467));
#31266=CARTESIAN_POINT('Ctrl Pts',(59.7885669427222,-2.45519409701178,330.738403467185));
#31267=CARTESIAN_POINT('Ctrl Pts',(59.7811551385451,-2.5682059340255,330.803511929));
#31268=CARTESIAN_POINT('Ctrl Pts',(59.773743334368,-2.67848328074788,330.873036529292));
#31269=CARTESIAN_POINT('Ctrl Pts',(59.7663315301909,-2.78567486569737,330.946705216109));
#31270=CARTESIAN_POINT('Ctrl Pts',(59.7585951336949,-2.89756079554421,331.023600147076));
#31271=CARTESIAN_POINT('Ctrl Pts',(59.7508587371989,-3.00644595196727,331.105258833066));
#31272=CARTESIAN_POINT('Ctrl Pts',(59.743122340703,-3.11189487609635,331.191418460552));
#31273=CARTESIAN_POINT('Ctrl Pts',(59.7353954868895,-3.21721373119349,331.277471811948));
#31274=CARTESIAN_POINT('Ctrl Pts',(59.7276686330761,-3.31910448276863,331.368014812905));
#31275=CARTESIAN_POINT('Ctrl Pts',(59.7199417792626,-3.41715987418023,331.462740968378));
#31276=CARTESIAN_POINT('Ctrl Pts',(59.7122225605611,-3.51511837442402,331.557373522391));
#31277=CARTESIAN_POINT('Ctrl Pts',(59.7045033418596,-3.60924877267888,331.65618073379));
#31278=CARTESIAN_POINT('Ctrl Pts',(59.6967841231581,-3.69917653089978,331.758815639964));
#31279=CARTESIAN_POINT('Ctrl Pts',(59.6890706390703,-3.78903748171775,331.861374298586));
#31280=CARTESIAN_POINT('Ctrl Pts',(59.6813571549825,-3.87470174650037,331.967754696837));
#31281=CARTESIAN_POINT('Ctrl Pts',(59.6736436708947,-3.95583164723709,332.077573090526));
#31282=CARTESIAN_POINT('Ctrl Pts',(59.6659333188321,-4.03692860554529,332.187346892954));
#31283=CARTESIAN_POINT('Ctrl Pts',(59.6582229667696,-4.11349462648461,332.300555597711));
#31284=CARTESIAN_POINT('Ctrl Pts',(59.650512614707,-4.18523252934497,332.416782677007));
#31285=CARTESIAN_POINT('Ctrl Pts',(59.6428037123741,-4.25695694377249,332.532987902846));
#31286=CARTESIAN_POINT('Ctrl Pts',(59.6350948100412,-4.32385483805942,332.65221003839));
#31287=CARTESIAN_POINT('Ctrl Pts',(59.6273859077083,-4.38567282591597,332.774004284253));
#31288=CARTESIAN_POINT('Ctrl Pts',(59.6196767431305,-4.44749291672514,332.89580267337));
#31289=CARTESIAN_POINT('Ctrl Pts',(59.6119675785526,-4.5042325784646,333.020172994421));
#31290=CARTESIAN_POINT('Ctrl Pts',(59.6042584139747,-4.55568499706754,333.14664701959));
#31291=CARTESIAN_POINT('Ctrl Pts',(59.5965472753277,-4.60715059098092,333.273153430692));
#31292=CARTESIAN_POINT('Ctrl Pts',(59.5888361366806,-4.65332609961916,333.401764251546));
#31293=CARTESIAN_POINT('Ctrl Pts',(59.5811249980335,-4.69405350941549,333.531992945097));
#31294=CARTESIAN_POINT('Ctrl Pts',(59.5734057227792,-4.73482389379036,333.662359052819));
#31295=CARTESIAN_POINT('Ctrl Pts',(59.565686447525,-4.77013458171241,333.794346064602));
#31296=CARTESIAN_POINT('Ctrl Pts',(59.5579671722708,-4.79987784009613,333.927453598834));
#31297=CARTESIAN_POINT('Ctrl Pts',(59.5502434732637,-4.82963814371007,334.060637414169));
#31298=CARTESIAN_POINT('Ctrl Pts',(59.5425197742566,-4.85382459290499,334.194942642628));
#31299=CARTESIAN_POINT('Ctrl Pts',(59.5347960752495,-4.8723810982895,334.329861584797));
#31300=CARTESIAN_POINT('Ctrl Pts',(59.5270608342684,-4.89096533374258,334.464982144212));
#31301=CARTESIAN_POINT('Ctrl Pts',(59.5193255932873,-4.90390278545122,334.600717856209));
#31302=CARTESIAN_POINT('Ctrl Pts',(59.5115903523062,-4.91118941666391,334.736558211082));
#31303=CARTESIAN_POINT('Ctrl Pts',(59.5065723433413,-4.91591640330058,334.824680626429));
#31304=CARTESIAN_POINT('Ctrl Pts',(59.5015543343764,-4.91826637593461,334.912847083949));
#31305=CARTESIAN_POINT('Ctrl Pts',(59.4965363254115,-4.91824991408677,335.000919285319));
#31306=CARTESIAN_POINT('',(62.9965362485424,-4.91824921808336,334.997226676644));
#31307=CARTESIAN_POINT('Ctrl Pts',(62.99653624849,-4.91824921808388,334.997226677573));
#31308=CARTESIAN_POINT('Ctrl Pts',(62.9887031285403,-4.91832755861146,335.136156877207));
#31309=CARTESIAN_POINT('Ctrl Pts',(62.9808700085906,-4.91251482706172,335.275093926432));
#31310=CARTESIAN_POINT('Ctrl Pts',(62.9730368886409,-4.90083586450775,335.413510449269));
#31311=CARTESIAN_POINT('Ctrl Pts',(62.9652022573993,-4.88915464865987,335.551953677655));
#31312=CARTESIAN_POINT('Ctrl Pts',(62.9573676261577,-4.87160497907927,335.6898758022));
#31313=CARTESIAN_POINT('Ctrl Pts',(62.9495329949161,-4.84826359170246,335.826754623738));
#31314=CARTESIAN_POINT('Ctrl Pts',(62.9416953021712,-4.82491308331758,335.963686932793));
#31315=CARTESIAN_POINT('Ctrl Pts',(62.9338576094262,-4.79576641330961,336.099574753729));
#31316=CARTESIAN_POINT('Ctrl Pts',(62.9260199166813,-4.76095139074702,336.233906364942));
#31317=CARTESIAN_POINT('Ctrl Pts',(62.9181776104982,-4.7261158752969,336.368317046694));
#31318=CARTESIAN_POINT('Ctrl Pts',(62.9103353043151,-4.68560545705694,336.501169328344));
#31319=CARTESIAN_POINT('Ctrl Pts',(62.9024929981319,-4.63959764255931,336.631967149687));
#31320=CARTESIAN_POINT('Ctrl Pts',(62.8946398519426,-4.59352623388616,336.76294576596));
#31321=CARTESIAN_POINT('Ctrl Pts',(62.8867867057531,-4.54194238104062,336.891863894192));
#31322=CARTESIAN_POINT('Ctrl Pts',(62.8789335595638,-4.48507179021934,337.018245302008));
#31323=CARTESIAN_POINT('Ctrl Pts',(62.8710739677352,-4.42815452163348,337.144730440092));
#31324=CARTESIAN_POINT('Ctrl Pts',(62.8632143759067,-4.36594203687394,337.268674371339));
#31325=CARTESIAN_POINT('Ctrl Pts',(62.8553547840781,-4.29870536434282,337.389626592811));
#31326=CARTESIAN_POINT('Ctrl Pts',(62.8474829775086,-4.23136419802172,337.510766788429));
#31327=CARTESIAN_POINT('Ctrl Pts',(62.8396111709391,-4.15898345072758,337.628905669596));
#31328=CARTESIAN_POINT('Ctrl Pts',(62.8317393643696,-4.0818770102074,337.743622265553));
#31329=CARTESIAN_POINT('Ctrl Pts',(62.8301428786478,-4.06623900763951,337.766888005874));
#31330=CARTESIAN_POINT('Ctrl Pts',(62.828546392926,-4.05040675680743,337.790013092481));
#31331=CARTESIAN_POINT('Ctrl Pts',(62.8269499072042,-4.03438307029467,337.812994188515));
#31332=CARTESIAN_POINT('Ctrl Pts',(62.8191748284258,-3.95634577672058,337.924914908911));
#31333=CARTESIAN_POINT('Ctrl Pts',(62.8113997496473,-3.87352433058407,338.033762692091));
#31334=CARTESIAN_POINT('Ctrl Pts',(62.8036246708689,-3.78618876188953,338.13910141949));
#31335=CARTESIAN_POINT('Ctrl Pts',(62.7958591598199,-3.69896066517238,338.244310520878));
#31336=CARTESIAN_POINT('Ctrl Pts',(62.7880936487709,-3.60722974567853,338.34601886027));
#31337=CARTESIAN_POINT('Ctrl Pts',(62.7803281377219,-3.51130938139486,338.443819026986));
#31338=CARTESIAN_POINT('Ctrl Pts',(62.7725703261997,-3.41548412243165,338.541522224551));
#31339=CARTESIAN_POINT('Ctrl Pts',(62.7648125146775,-3.31547795700033,338.635324683576));
#31340=CARTESIAN_POINT('Ctrl Pts',(62.7570547031553,-3.21164438185126,338.724852134921));
#31341=CARTESIAN_POINT('Ctrl Pts',(62.7493027296323,-3.10788894476045,338.814312214019));
#31342=CARTESIAN_POINT('Ctrl Pts',(62.7415507561093,-3.00031212578102,338.899503434659));
#31343=CARTESIAN_POINT('Ctrl Pts',(62.7337987825863,-2.88930385329977,338.980088730896));
#31344=CARTESIAN_POINT('Ctrl Pts',(62.7260500920286,-2.77834259288751,339.060639899213));
#31345=CARTESIAN_POINT('Ctrl Pts',(62.7183014014711,-2.66395308498706,339.136588793607));
#31346=CARTESIAN_POINT('Ctrl Pts',(62.7105527109134,-2.54655770322131,339.207639115545));
#31347=CARTESIAN_POINT('Ctrl Pts',(62.7028056325356,-2.42918674654533,339.27867465487));
#31348=CARTESIAN_POINT('Ctrl Pts',(62.6950585541577,-2.30881149415232,339.344813446718));
#31349=CARTESIAN_POINT('Ctrl Pts',(62.6873114757799,-2.18588228087157,339.40580318633));
#31350=CARTESIAN_POINT('Ctrl Pts',(62.6795643324741,-2.0629520373257,339.466793437093));
#31351=CARTESIAN_POINT('Ctrl Pts',(62.6718171891683,-1.93746814034687,339.522634375824));
#31352=CARTESIAN_POINT('Ctrl Pts',(62.6640700458625,-1.80990407791222,339.573120410754));
#31353=CARTESIAN_POINT('Ctrl Pts',(62.6563211608344,-1.68231133636815,339.623617796016));
#31354=CARTESIAN_POINT('Ctrl Pts',(62.6485722758063,-1.55263786214078,339.668757738046));
#31355=CARTESIAN_POINT('Ctrl Pts',(62.6408233907782,-1.42137522094821,339.708383538304));
#31356=CARTESIAN_POINT('Ctrl Pts',(62.6330662810034,-1.28997325623171,339.748051397796));
#31357=CARTESIAN_POINT('Ctrl Pts',(62.6253091712287,-1.15697912987852,339.782193310924));
#31358=CARTESIAN_POINT('Ctrl Pts',(62.617552061454,-1.02289814493059,339.810702905771));
#31359=CARTESIAN_POINT('Ctrl Pts',(62.6097908065278,-0.888745511391657,
339.839227735234));
#31360=CARTESIAN_POINT('Ctrl Pts',(62.6020295516016,-0.753505247195832,
339.86211418407));
#31361=CARTESIAN_POINT('Ctrl Pts',(62.5942682966754,-0.617689851683025,
339.879307564566));
#31362=CARTESIAN_POINT('Ctrl Pts',(62.5864946262708,-0.48165719579944,339.896528448866));
#31363=CARTESIAN_POINT('Ctrl Pts',(62.5787209558661,-0.345047959820318,
339.908038033402));
#31364=CARTESIAN_POINT('Ctrl Pts',(62.5709472854614,-0.20837762865966,339.913833719854));
#31365=CARTESIAN_POINT('Ctrl Pts',(62.5635354812844,-0.0780693342963419,
339.919359615707));
#31366=CARTESIAN_POINT('Ctrl Pts',(62.5561236771073,0.0522942074957861,
339.919691605138));
#31367=CARTESIAN_POINT('Ctrl Pts',(62.5487118729303,0.182270653531195,339.914871358577));
#31368=CARTESIAN_POINT('Ctrl Pts',(62.5409367941519,0.318617632367615,339.909814857374));
#31369=CARTESIAN_POINT('Ctrl Pts',(62.5331617153734,0.454969492207677,339.899072317563));
#31370=CARTESIAN_POINT('Ctrl Pts',(62.525386636595,0.590813362915036,339.882634804355));
#31371=CARTESIAN_POINT('Ctrl Pts',(62.517621125546,0.726490069091153,339.866217518554));
#31372=CARTESIAN_POINT('Ctrl Pts',(62.509855614497,0.861659645595877,339.844119249827));
#31373=CARTESIAN_POINT('Ctrl Pts',(62.502090103448,0.995809905285056,339.816383051112));
#31374=CARTESIAN_POINT('Ctrl Pts',(62.4943322919258,1.12982715460091,339.788674352918));
#31375=CARTESIAN_POINT('Ctrl Pts',(62.4865744804036,1.26282671805026,339.755338927832));
#31376=CARTESIAN_POINT('Ctrl Pts',(62.4788166688814,1.39430256735267,339.716471500303));
#31377=CARTESIAN_POINT('Ctrl Pts',(62.4710646953584,1.52567947690887,339.677633321747));
#31378=CARTESIAN_POINT('Ctrl Pts',(62.4633127218354,1.65553458132659,339.633271537376));
#31379=CARTESIAN_POINT('Ctrl Pts',(62.4555607483124,1.78337342203687,339.583531640566));
#31380=CARTESIAN_POINT('Ctrl Pts',(62.4478120577548,1.91115812292272,339.533812808632));
#31381=CARTESIAN_POINT('Ctrl Pts',(62.4400633671972,2.03692789491125,339.478720535749));
#31382=CARTESIAN_POINT('Ctrl Pts',(62.4323146766396,2.16020500364008,339.418449660769));
#31383=CARTESIAN_POINT('Ctrl Pts',(62.4245675982617,2.28345646353665,339.358191325648));
#31384=CARTESIAN_POINT('Ctrl Pts',(62.4168205198839,2.40421594081165,339.292756703129));
#31385=CARTESIAN_POINT('Ctrl Pts',(62.4090734415061,2.52202756499258,339.222387952796));
#31386=CARTESIAN_POINT('Ctrl Pts',(62.4013262982003,2.63984017654832,339.152018612705));
#31387=CARTESIAN_POINT('Ctrl Pts',(62.3935791548944,2.75470455016115,339.076715262754));
#31388=CARTESIAN_POINT('Ctrl Pts',(62.3858320115886,2.86619156781367,338.996764811581));
#31389=CARTESIAN_POINT('Ctrl Pts',(62.3780831265606,2.97770365011463,338.91679638585));
#31390=CARTESIAN_POINT('Ctrl Pts',(62.3703342415325,3.0858365479526,338.832179007672));
#31391=CARTESIAN_POINT('Ctrl Pts',(62.3625853565044,3.19019247576707,338.743241246575));
#31392=CARTESIAN_POINT('Ctrl Pts',(62.3548282467297,3.29465916804167,338.654209086019));
#31393=CARTESIAN_POINT('Ctrl Pts',(62.347071136955,3.39534058414771,338.56084763612));
#31394=CARTESIAN_POINT('Ctrl Pts',(62.3393140271802,3.49187382520074,338.463524253037));
#31395=CARTESIAN_POINT('Ctrl Pts',(62.3315527722541,3.58845865053107,338.366148863451));
#31396=CARTESIAN_POINT('Ctrl Pts',(62.3237915173279,3.68089062065925,338.264807610753));
#31397=CARTESIAN_POINT('Ctrl Pts',(62.3160302624018,3.76884640471999,338.159901871915));
#31398=CARTESIAN_POINT('Ctrl Pts',(62.3082565919971,3.85694288937075,338.054828318082));
#31399=CARTESIAN_POINT('Ctrl Pts',(62.3004829215924,3.94054864077809,337.946179193729));
#31400=CARTESIAN_POINT('Ctrl Pts',(62.2927092511878,4.01938251549385,337.834386575018));
#31401=CARTESIAN_POINT('Ctrl Pts',(62.2852974470106,4.09454665437628,337.727797929602));
#31402=CARTESIAN_POINT('Ctrl Pts',(62.2778856428334,4.16537302409506,337.618352104653));
#31403=CARTESIAN_POINT('Ctrl Pts',(62.2704738386562,4.23165728892461,337.506443626254));
#31404=CARTESIAN_POINT('Ctrl Pts',(62.2626987598778,4.30119034302321,337.389050179972));
#31405=CARTESIAN_POINT('Ctrl Pts',(62.2549236810993,4.36594452734166,337.268575587395));
#31406=CARTESIAN_POINT('Ctrl Pts',(62.2471486023209,4.42563478496584,337.145446296834));
#31407=CARTESIAN_POINT('Ctrl Pts',(62.2393830912719,4.48525158992794,337.022468524705));
#31408=CARTESIAN_POINT('Ctrl Pts',(62.2316175802228,4.53981669818476,336.896842902899));
#31409=CARTESIAN_POINT('Ctrl Pts',(62.2238520691738,4.58908914001719,336.769023438928));
#31410=CARTESIAN_POINT('Ctrl Pts',(62.2160942576517,4.63831272807992,336.641330708328));
#31411=CARTESIAN_POINT('Ctrl Pts',(62.2083364461295,4.68225395324022,336.511448826702));
#31412=CARTESIAN_POINT('Ctrl Pts',(62.2005786346073,4.72071863037156,336.379854584861));
#31413=CARTESIAN_POINT('Ctrl Pts',(62.1928266610843,4.7591543616135,336.248359371861));
#31414=CARTESIAN_POINT('Ctrl Pts',(62.1850746875613,4.79212163880366,336.115154737217));
#31415=CARTESIAN_POINT('Ctrl Pts',(62.1773227140384,4.81947523052142,335.980735216504));
#31416=CARTESIAN_POINT('Ctrl Pts',(62.1695740234807,4.84681723797698,335.846372622536));
#31417=CARTESIAN_POINT('Ctrl Pts',(62.1618253329231,4.86855021065845,335.71079654804));
#31418=CARTESIAN_POINT('Ctrl Pts',(62.1540766423655,4.88457946323702,335.574514168514));
#31419=CARTESIAN_POINT('Ctrl Pts',(62.1463295639876,4.9006053807957,335.438260143676));
#31420=CARTESIAN_POINT('Ctrl Pts',(62.1385824856098,4.91092989306442,335.301300494062));
#31421=CARTESIAN_POINT('Ctrl Pts',(62.1308354072319,4.91550993953144,335.164149617324));
#31422=CARTESIAN_POINT('Ctrl Pts',(62.1230882639261,4.92009002438368,335.026997591129));
#31423=CARTESIAN_POINT('Ctrl Pts',(62.1153411206204,4.9189255343614,334.88965472527));
#31424=CARTESIAN_POINT('Ctrl Pts',(62.1075939773145,4.91202551667773,334.752637136969));
#31425=CARTESIAN_POINT('Ctrl Pts',(62.0998450922865,4.90512394772362,334.615588744206));
#31426=CARTESIAN_POINT('Ctrl Pts',(62.0920962072584,4.89248430486528,334.478866164824));
#31427=CARTESIAN_POINT('Ctrl Pts',(62.0843473222303,4.8741676246373,334.342981713011));
#31428=CARTESIAN_POINT('Ctrl Pts',(62.0765902124555,4.8558315028956,334.206953032037));
#31429=CARTESIAN_POINT('Ctrl Pts',(62.0688331026808,4.83180635924938,334.07176464367));
#31430=CARTESIAN_POINT('Ctrl Pts',(62.0610759929061,4.80220472592158,333.937920514822));
#31431=CARTESIAN_POINT('Ctrl Pts',(62.0533147379799,4.77258727442745,333.80400486395));
#31432=CARTESIAN_POINT('Ctrl Pts',(62.0455534830537,4.73738749579509,333.671435281525));
#31433=CARTESIAN_POINT('Ctrl Pts',(62.0377922281276,4.69676794359653,333.540700871478));
#31434=CARTESIAN_POINT('Ctrl Pts',(62.0300185577229,4.65608341335234,333.409757328981));
#31435=CARTESIAN_POINT('Ctrl Pts',(62.0222448873183,4.60996191614014,333.2806551935));
#31436=CARTESIAN_POINT('Ctrl Pts',(62.0144712169136,4.55861465117034,333.153864705761));
#31437=CARTESIAN_POINT('Ctrl Pts',(62.0070594127365,4.50965761373842,333.03297634573));
#31438=CARTESIAN_POINT('Ctrl Pts',(61.9996476085594,4.45595049728665,332.914189524542));
#31439=CARTESIAN_POINT('Ctrl Pts',(61.9922358043824,4.39771448942881,332.797889573167));
#31440=CARTESIAN_POINT('Ctrl Pts',(61.9844607256039,4.33662416134957,332.675889414735));
#31441=CARTESIAN_POINT('Ctrl Pts',(61.9766856468255,4.27035671096763,332.556240524797));
#31442=CARTESIAN_POINT('Ctrl Pts',(61.9689105680471,4.19911648711376,332.439413389446));
#31443=CARTESIAN_POINT('Ctrl Pts',(61.9611450569981,4.12796392889081,332.322730017322));
#31444=CARTESIAN_POINT('Ctrl Pts',(61.9533795459491,4.05185097443223,332.208861821338));
#31445=CARTESIAN_POINT('Ctrl Pts',(61.9456140349,3.97102900579846,332.098257127586));
#31446=CARTESIAN_POINT('Ctrl Pts',(61.9378562233779,3.89028717238233,331.98776209871));
#31447=CARTESIAN_POINT('Ctrl Pts',(61.9300984118557,3.8048458454959,331.880524446259));
#31448=CARTESIAN_POINT('Ctrl Pts',(61.9223406003336,3.71500088399098,331.776965483516));
#31449=CARTESIAN_POINT('Ctrl Pts',(61.9145886268106,3.62522353366838,331.673484452176));
#31450=CARTESIAN_POINT('Ctrl Pts',(61.9068366532876,3.53104939994974,331.573676894374));
#31451=CARTESIAN_POINT('Ctrl Pts',(61.8990846797646,3.43281575529389,331.477932559887));
#31452=CARTESIAN_POINT('Ctrl Pts',(61.891335989207,3.3346237126448,331.382228773181));
#31453=CARTESIAN_POINT('Ctrl Pts',(61.8835872986494,3.23237585776785,331.290585059537));
#31454=CARTESIAN_POINT('Ctrl Pts',(61.8758386080918,3.12644744569646,331.203355503632));
#31455=CARTESIAN_POINT('Ctrl Pts',(61.8680915297139,3.02054107291607,331.116144096565));
#31456=CARTESIAN_POINT('Ctrl Pts',(61.8603444513361,2.91095596765934,331.033345268786));
#31457=CARTESIAN_POINT('Ctrl Pts',(61.8525973729583,2.79810139537135,330.955273600882));
#31458=CARTESIAN_POINT('Ctrl Pts',(61.8448502296525,2.68524587725349,330.877201278663));
#31459=CARTESIAN_POINT('Ctrl Pts',(61.8371030863468,2.56912115890212,330.803856417718));
#31460=CARTESIAN_POINT('Ctrl Pts',(61.829355943041,2.45016615026692,330.735510710696));
#31461=CARTESIAN_POINT('Ctrl Pts',(61.8216070580129,2.33118439802006,330.667149638109));
#31462=CARTESIAN_POINT('Ctrl Pts',(61.8138581729848,2.20937142815575,330.603790150599));
#31463=CARTESIAN_POINT('Ctrl Pts',(61.8061092879567,2.08519108697685,330.545658163848));
#31464=CARTESIAN_POINT('Ctrl Pts',(61.798352178182,1.96087893950071,330.487464475206));
#31465=CARTESIAN_POINT('Ctrl Pts',(61.7905950684072,1.83419475581605,330.434509536998));
#31466=CARTESIAN_POINT('Ctrl Pts',(61.7828379586325,1.70562323009318,330.386971443892));
#31467=CARTESIAN_POINT('Ctrl Pts',(61.7750767037064,1.57698299985807,330.339407947949));
#31468=CARTESIAN_POINT('Ctrl Pts',(61.7673154487802,1.44645378976839,330.297267184864));
#31469=CARTESIAN_POINT('Ctrl Pts',(61.7595541938541,1.31453486481976,330.260677142073));
#31470=CARTESIAN_POINT('Ctrl Pts',(61.7517805234494,1.18240491258339,330.224028567137));
#31471=CARTESIAN_POINT('Ctrl Pts',(61.7440068530448,1.04888118399147,330.192948544714));
#31472=CARTESIAN_POINT('Ctrl Pts',(61.7362331826401,0.914473406514856,330.16751394712));
#31473=CARTESIAN_POINT('Ctrl Pts',(61.7288213784629,0.786322343413962,330.143263336163));
#31474=CARTESIAN_POINT('Ctrl Pts',(61.7214095742857,0.657367968842301,330.124144431247));
#31475=CARTESIAN_POINT('Ctrl Pts',(61.7139977701084,0.528054013144585,330.110179755686));
#31476=CARTESIAN_POINT('Ctrl Pts',(61.70622269133,0.392401995274051,330.095530629778));
#31477=CARTESIAN_POINT('Ctrl Pts',(61.6984476125515,0.255925571301257,330.086507462761));
#31478=CARTESIAN_POINT('Ctrl Pts',(61.6906725337731,0.119130967896039,330.083193020365));
#31479=CARTESIAN_POINT('Ctrl Pts',(61.6829070227241,-0.0174953010410114,
330.079882656601));
#31480=CARTESIAN_POINT('Ctrl Pts',(61.6751415116751,-0.154438583333955,
330.082267049201));
#31481=CARTESIAN_POINT('Ctrl Pts',(61.667376000626,-0.291185834749258,330.090377420601));
#31482=CARTESIAN_POINT('Ctrl Pts',(61.6596181891038,-0.427797500866653,
330.098479750545));
#31483=CARTESIAN_POINT('Ctrl Pts',(61.6518603775816,-0.56421313522898,330.112296738098));
#31484=CARTESIAN_POINT('Ctrl Pts',(61.6441025660594,-0.699918340307498,
330.131807586033));
#31485=CARTESIAN_POINT('Ctrl Pts',(61.6363505925364,-0.83552142291629,330.151303751437));
#31486=CARTESIAN_POINT('Ctrl Pts',(61.6285986190133,-0.970414755039212,
330.176485193116));
#31487=CARTESIAN_POINT('Ctrl Pts',(61.6208466454903,-1.1040880702953,330.20727920743));
#31488=CARTESIAN_POINT('Ctrl Pts',(61.6130979549326,-1.23770477482239,330.238060180461));
#31489=CARTESIAN_POINT('Ctrl Pts',(61.605349264375,-1.37010211001328,330.274448911022));
#31490=CARTESIAN_POINT('Ctrl Pts',(61.5976005738174,-1.50077924647777,330.316321454685));
#31491=CARTESIAN_POINT('Ctrl Pts',(61.5898534954396,-1.6314291944724,330.358185286416));
#31492=CARTESIAN_POINT('Ctrl Pts',(61.5821064170618,-1.76035928363424,330.405530542616));
#31493=CARTESIAN_POINT('Ctrl Pts',(61.5743593386839,-1.88708349941958,330.458183300846));
#31494=CARTESIAN_POINT('Ctrl Pts',(61.5666121953782,-2.01380877727573,330.510836500356));
#31495=CARTESIAN_POINT('Ctrl Pts',(61.5588650520723,-2.13832778392347,330.568797140646));
#31496=CARTESIAN_POINT('Ctrl Pts',(61.5511179087665,-2.26017452785904,330.631843161456));
#31497=CARTESIAN_POINT('Ctrl Pts',(61.5433690237384,-2.3820486655297,330.694903356351));
#31498=CARTESIAN_POINT('Ctrl Pts',(61.5356201387103,-2.50124899791215,330.763051027218));
#31499=CARTESIAN_POINT('Ctrl Pts',(61.5278712536822,-2.61733453384105,330.836018371743));
#31500=CARTESIAN_POINT('Ctrl Pts',(61.5201141439075,-2.73354328415734,330.909063164562));
#31501=CARTESIAN_POINT('Ctrl Pts',(61.5123570341327,-2.84663030236878,330.986937641693));
#31502=CARTESIAN_POINT('Ctrl Pts',(61.504599924358,-2.95618352904371,331.069330590712));
#31503=CARTESIAN_POINT('Ctrl Pts',(61.4968386694318,-3.06579529745992,331.151767567889));
#31504=CARTESIAN_POINT('Ctrl Pts',(61.4890774145057,-3.17186920951577,331.23872758043));
#31505=CARTESIAN_POINT('Ctrl Pts',(61.4813161595796,-3.27402745690945,331.329860047096));
#31506=CARTESIAN_POINT('Ctrl Pts',(61.4735424891749,-3.37634912420559,331.421138296008));
#31507=CARTESIAN_POINT('Ctrl Pts',(61.4657688187702,-3.47474232925547,331.516602064481));
#31508=CARTESIAN_POINT('Ctrl Pts',(61.4579951483656,-3.56886658570419,331.61586431183));
#31509=CARTESIAN_POINT('Ctrl Pts',(61.4505833441886,-3.65860933536932,331.710505877684));
#31510=CARTESIAN_POINT('Ctrl Pts',(61.4431715400116,-3.74447144187631,331.808600025886));
#31511=CARTESIAN_POINT('Ctrl Pts',(61.4357597358346,-3.82619383693742,331.909785802783));
#31512=CARTESIAN_POINT('Ctrl Pts',(61.4278754238619,-3.91312609289425,332.017422245031));
#31513=CARTESIAN_POINT('Ctrl Pts',(61.4199911118892,-3.99566014173165,332.1289122848));
#31514=CARTESIAN_POINT('Ctrl Pts',(61.4121067999165,-4.07343455458442,332.243858858473));
#31515=CARTESIAN_POINT('Ctrl Pts',(61.4043645082339,-4.14980801517776,332.356734896912));
#31516=CARTESIAN_POINT('Ctrl Pts',(61.3966222165512,-4.22159159652285,332.472943674719));
#31517=CARTESIAN_POINT('Ctrl Pts',(61.3888799248686,-4.28848152717237,332.592073661093));
#31518=CARTESIAN_POINT('Ctrl Pts',(61.381145075822,-4.35530715678206,332.711089128258));
#31519=CARTESIAN_POINT('Ctrl Pts',(61.3734102267753,-4.41724830220632,332.833019877969));
#31520=CARTESIAN_POINT('Ctrl Pts',(61.3656753777287,-4.47404401241101,332.957424851441));
#31521=CARTESIAN_POINT('Ctrl Pts',(61.3579462672387,-4.53079758534822,333.081737527703));
#31522=CARTESIAN_POINT('Ctrl Pts',(61.3502171567488,-4.58241315598515,333.208520419483));
#31523=CARTESIAN_POINT('Ctrl Pts',(61.3424880462589,-4.62867553359679,333.337307645058));
#31524=CARTESIAN_POINT('Ctrl Pts',(61.3344920631115,-4.67653527013741,333.470541668124));
#31525=CARTESIAN_POINT('Ctrl Pts',(61.326496079964,-4.71866527595313,333.605920551521));
#31526=CARTESIAN_POINT('Ctrl Pts',(61.3185000968166,-4.75488129027722,333.742905342517));
#31527=CARTESIAN_POINT('Ctrl Pts',(61.3107765708199,-4.78986327097582,333.875222479123));
#31528=CARTESIAN_POINT('Ctrl Pts',(61.3030530448233,-4.81932759969248,334.009037463177));
#31529=CARTESIAN_POINT('Ctrl Pts',(61.2953295188266,-4.84315901522016,334.143849419908));
#31530=CARTESIAN_POINT('Ctrl Pts',(61.2876066690408,-4.86698834425729,334.278649573568));
#31531=CARTESIAN_POINT('Ctrl Pts',(61.2798838192551,-4.88518567836036,334.41444613842));
#31532=CARTESIAN_POINT('Ctrl Pts',(61.2721609694693,-4.89768709330298,334.550729259139));
#31533=CARTESIAN_POINT('Ctrl Pts',(61.264435857073,-4.91019217086169,334.687052307559));
#31534=CARTESIAN_POINT('Ctrl Pts',(61.2567107446767,-4.91699796774325,334.823861804713));
#31535=CARTESIAN_POINT('Ctrl Pts',(61.2489856322803,-4.91809253490547,334.960644179502));
#31536=CARTESIAN_POINT('Ctrl Pts',(61.2481691710169,-4.91820821887774,334.975100604834));
#31537=CARTESIAN_POINT('Ctrl Pts',(61.2473527097534,-4.91826015516819,334.989556727422));
#31538=CARTESIAN_POINT('Ctrl Pts',(61.24653624849,-4.9182483636783,335.00401194164));
#31539=CARTESIAN_POINT('',(64.7465362484525,-4.91824918766967,334.997173255123));
#31540=CARTESIAN_POINT('Ctrl Pts',(64.7465362484525,-4.91824918766967,334.997173255123));
#31541=CARTESIAN_POINT('Ctrl Pts',(64.7388635417342,-4.91832669084382,335.132020911997));
#31542=CARTESIAN_POINT('Ctrl Pts',(64.731190835016,-4.91285417304389,335.267091728814));
#31543=CARTESIAN_POINT('Ctrl Pts',(64.7235181282978,-4.9018029748704,335.40188388628));
#31544=CARTESIAN_POINT('Ctrl Pts',(64.715853995146,-4.89076412542671,335.536525425515));
#31545=CARTESIAN_POINT('Ctrl Pts',(64.7081898619942,-4.87415902608872,335.670888527897));
#31546=CARTESIAN_POINT('Ctrl Pts',(64.7005257288424,-4.85201102103137,335.804470082906));
#31547=CARTESIAN_POINT('Ctrl Pts',(64.6928682158542,-4.82988214708956,335.937936252164));
#31548=CARTESIAN_POINT('Ctrl Pts',(64.685210702866,-4.80221995721399,336.070621822914));
#31549=CARTESIAN_POINT('Ctrl Pts',(64.6775531898779,-4.76909967332192,336.202028023143));
#31550=CARTESIAN_POINT('Ctrl Pts',(64.6698999197036,-4.73599774045353,336.333361414869));
#31551=CARTESIAN_POINT('Ctrl Pts',(64.6622466495294,-4.69744382577316,336.463416457486));
#31552=CARTESIAN_POINT('Ctrl Pts',(64.6545933793552,-4.65356430540468,336.591704218115));
#31553=CARTESIAN_POINT('Ctrl Pts',(64.6469422691734,-4.60969716921042,336.719955771921));
#31554=CARTESIAN_POINT('Ctrl Pts',(64.6392911589915,-4.56050754533228,336.846440655695));
#31555=CARTESIAN_POINT('Ctrl Pts',(64.6316400488097,-4.50617163613448,336.970685223012));
#31556=CARTESIAN_POINT('Ctrl Pts',(64.6239893429186,-4.45183859808905,337.094923225148));
#31557=CARTESIAN_POINT('Ctrl Pts',(64.6163386370275,-4.39235997645717,337.216920778271));
#31558=CARTESIAN_POINT('Ctrl Pts',(64.6086879311364,-4.32795985513916,337.33622485108));
#31559=CARTESIAN_POINT('Ctrl Pts',(64.6010358743879,-4.26354836292587,337.455549988975));
#31560=CARTESIAN_POINT('Ctrl Pts',(64.5933838176395,-4.19421383407427,337.572180347593));
#31561=CARTESIAN_POINT('Ctrl Pts',(64.585731760891,-4.12022570570791,337.685688588896));
#31562=CARTESIAN_POINT('Ctrl Pts',(64.5780719696904,-4.04616279252726,337.799311560668));
#31563=CARTESIAN_POINT('Ctrl Pts',(64.5704121784898,-3.96743710541301,337.909805775638));
#31564=CARTESIAN_POINT('Ctrl Pts',(64.5627523872891,-3.88436093284001,338.016773641811));
#31565=CARTESIAN_POINT('Ctrl Pts',(64.5550886535452,-3.80124200043196,338.123796565026));
#31566=CARTESIAN_POINT('Ctrl Pts',(64.5474249198012,-3.71376838271351,338.227289218797));
#31567=CARTESIAN_POINT('Ctrl Pts',(64.5397611860573,-3.62229101222018,338.326889070181));
#31568=CARTESIAN_POINT('Ctrl Pts',(64.5320854558956,-3.53067044771968,338.426644830089));
#31569=CARTESIAN_POINT('Ctrl Pts',(64.524409725734,-3.43503389460652,338.522495331051));
#31570=CARTESIAN_POINT('Ctrl Pts',(64.5167339955724,-3.33576779431985,338.614116252264));
#31571=CARTESIAN_POINT('Ctrl Pts',(64.5099487013309,-3.24801722408502,338.695108535215));
#31572=CARTESIAN_POINT('Ctrl Pts',(64.5031634070894,-3.15743100405289,338.77279611708));
#31573=CARTESIAN_POINT('Ctrl Pts',(64.4963781128479,-3.06429501471525,338.846983119964));
#31574=CARTESIAN_POINT('Ctrl Pts',(64.4886030340694,-2.9575730910322,338.931991930376));
#31575=CARTESIAN_POINT('Ctrl Pts',(64.480827955291,-2.84714241004196,339.012690731727));
#31576=CARTESIAN_POINT('Ctrl Pts',(64.4730528765125,-2.7333861914832,339.088738557393));
#31577=CARTESIAN_POINT('Ctrl Pts',(64.4652873654635,-2.61976995719346,339.164692801367));
#31578=CARTESIAN_POINT('Ctrl Pts',(64.4575218544145,-2.50283664965343,339.236007242268));
#31579=CARTESIAN_POINT('Ctrl Pts',(64.4497563433655,-2.38300284600843,339.302380794213));
#31580=CARTESIAN_POINT('Ctrl Pts',(64.4419985318433,-2.26328785792879,339.368688536589));
#31581=CARTESIAN_POINT('Ctrl Pts',(64.4342407203211,-2.14067843657487,339.430064950941));
#31582=CARTESIAN_POINT('Ctrl Pts',(64.4264829087989,-2.01562015668641,339.486252160374));
#31583=CARTESIAN_POINT('Ctrl Pts',(64.4187309352759,-1.89065598711913,339.54239708715));
#31584=CARTESIAN_POINT('Ctrl Pts',(64.4109789617528,-1.76324698221357,339.593360422256));
#31585=CARTESIAN_POINT('Ctrl Pts',(64.4032269882298,-1.63386302173005,339.638930338852));
#31586=CARTESIAN_POINT('Ctrl Pts',(64.3954782976722,-1.50453385543096,339.684480956562));
#31587=CARTESIAN_POINT('Ctrl Pts',(64.3877296071146,-1.37323176499267,339.724642569129));
#31588=CARTESIAN_POINT('Ctrl Pts',(64.379980916557,-1.24044609768678,339.759251678703));
#31589=CARTESIAN_POINT('Ctrl Pts',(64.3722338381791,-1.10768805754793,339.793853587562));
#31590=CARTESIAN_POINT('Ctrl Pts',(64.3644867598013,-0.973447432509595,
339.822905192771));
#31591=CARTESIAN_POINT('Ctrl Pts',(64.3567396814234,-0.838227819271319,
339.846293138627));
#31592=CARTESIAN_POINT('Ctrl Pts',(64.3489925381176,-0.703007072762353,
339.869681280496));
#31593=CARTESIAN_POINT('Ctrl Pts',(64.3412453948118,-0.566807706843793,
339.887405601719));
#31594=CARTESIAN_POINT('Ctrl Pts',(64.333498251506,-0.430142183666102,339.899404123394));
#31595=CARTESIAN_POINT('Ctrl Pts',(64.3257493664779,-0.293445935177217,
339.911405342592));
#31596=CARTESIAN_POINT('Ctrl Pts',(64.3180004814498,-0.156283710185274,
339.917678166518));
#31597=CARTESIAN_POINT('Ctrl Pts',(64.3102515964217,-0.0191713498283948,
339.918212634875));
#31598=CARTESIAN_POINT('Ctrl Pts',(64.3024944866469,0.118086543004216,339.918747670522));
#31599=CARTESIAN_POINT('Ctrl Pts',(64.2947373768722,0.255294073986738,339.91353218223));
#31600=CARTESIAN_POINT('Ctrl Pts',(64.2869802670974,0.391936591957358,339.902608363961));
#31601=CARTESIAN_POINT('Ctrl Pts',(64.2792190121713,0.528652127320508,339.891678708354));
#31602=CARTESIAN_POINT('Ctrl Pts',(64.2714577572451,0.664801660270137,339.875034692081));
#31603=CARTESIAN_POINT('Ctrl Pts',(64.263696502319,0.799878386127947,339.852770098604));
#31604=CARTESIAN_POINT('Ctrl Pts',(64.2559228319143,0.935171190725635,339.830469889034));
#31605=CARTESIAN_POINT('Ctrl Pts',(64.2481491615096,1.06938737599947,339.802531215094));
#31606=CARTESIAN_POINT('Ctrl Pts',(64.240375491105,1.20203213510304,339.769098636921));
#31607=CARTESIAN_POINT('Ctrl Pts',(64.232963686928,1.32850224875641,339.737222353305));
#31608=CARTESIAN_POINT('Ctrl Pts',(64.225551882751,1.45354366758471,339.700352218741));
#31609=CARTESIAN_POINT('Ctrl Pts',(64.218140078574,1.5767443156899,339.658654357799));
#31610=CARTESIAN_POINT('Ctrl Pts',(64.2103649997955,1.70598339455634,339.61491276048));
#31611=CARTESIAN_POINT('Ctrl Pts',(64.2025899210171,1.83360511624078,339.565719996807));
#31612=CARTESIAN_POINT('Ctrl Pts',(64.1948148422386,1.95911537244465,339.511213807829));
#31613=CARTESIAN_POINT('Ctrl Pts',(64.1870493311896,2.08447118028754,339.456774692187));
#31614=CARTESIAN_POINT('Ctrl Pts',(64.1792838201406,2.20772033740928,339.397035315208));
#31615=CARTESIAN_POINT('Ctrl Pts',(64.1715183090916,2.32838422047214,339.332183050652));
#31616=CARTESIAN_POINT('Ctrl Pts',(64.1637604975694,2.44892846494381,339.267395087305));
#31617=CARTESIAN_POINT('Ctrl Pts',(64.1560026860472,2.56689219440278,339.197504508715));
#31618=CARTESIAN_POINT('Ctrl Pts',(64.148244874525,2.68181742860675,339.122746456201));
#31619=CARTESIAN_POINT('Ctrl Pts',(64.140492901002,2.79665617792788,339.048044661492));
#31620=CARTESIAN_POINT('Ctrl Pts',(64.132740927479,2.90846065695497,338.968482896016));
#31621=CARTESIAN_POINT('Ctrl Pts',(64.1249889539559,3.01679845708052,338.884341660032));
#31622=CARTESIAN_POINT('Ctrl Pts',(64.1172402633983,3.12509037608303,338.80023605791));
#31623=CARTESIAN_POINT('Ctrl Pts',(64.1094915728406,3.22991822814946,338.711555081886));
#31624=CARTESIAN_POINT('Ctrl Pts',(64.101742882283,3.33087971056249,338.618621756451));
#31625=CARTESIAN_POINT('Ctrl Pts',(64.0939958039052,3.431820187096,338.525707766571));
#31626=CARTESIAN_POINT('Ctrl Pts',(64.0862487255273,3.52889560663854,338.428543451637));
#31627=CARTESIAN_POINT('Ctrl Pts',(64.0785016471495,3.62173812089176,338.327490953583));
#31628=CARTESIAN_POINT('Ctrl Pts',(64.0707545038437,3.71458141325461,338.226437608613));
#31629=CARTESIAN_POINT('Ctrl Pts',(64.0630073605378,3.80319146511906,338.121496303361));
#31630=CARTESIAN_POINT('Ctrl Pts',(64.055260217232,3.88723883443075,338.013064437843));
#31631=CARTESIAN_POINT('Ctrl Pts',(64.0475113322039,3.9713050993756,337.90460819454));
#31632=CARTESIAN_POINT('Ctrl Pts',(64.0397624471758,4.05080640115004,337.792660138277));
#31633=CARTESIAN_POINT('Ctrl Pts',(64.0320135621476,4.12545521268858,337.677648660784));
#31634=CARTESIAN_POINT('Ctrl Pts',(64.0242564523729,4.20018325724675,337.562515108922));
#31635=CARTESIAN_POINT('Ctrl Pts',(64.0164993425982,4.27004830985525,337.444311968944));
#31636=CARTESIAN_POINT('Ctrl Pts',(64.0087422328234,4.33480734504369,337.323494855569));
#31637=CARTESIAN_POINT('Ctrl Pts',(64.0009809778973,4.39960098538997,337.202613181391));
#31638=CARTESIAN_POINT('Ctrl Pts',(63.9932197229711,4.45928300155939,337.079115102272));
#31639=CARTESIAN_POINT('Ctrl Pts',(63.9854584680449,4.51365799697293,336.95347755269));
#31640=CARTESIAN_POINT('Ctrl Pts',(63.9776847976402,4.56811997465828,336.827639023974));
#31641=CARTESIAN_POINT('Ctrl Pts',(63.9699111272355,4.61725782687195,336.69965455081));
#31642=CARTESIAN_POINT('Ctrl Pts',(63.9621374568309,4.66092534893875,336.570018456618));
#31643=CARTESIAN_POINT('Ctrl Pts',(63.9547256526539,4.70256013734701,336.4464169538));
#31644=CARTESIAN_POINT('Ctrl Pts',(63.9473138484769,4.73922234120536,336.321314411645));
#31645=CARTESIAN_POINT('Ctrl Pts',(63.9399020442999,4.77082866029556,336.195147253104));
#31646=CARTESIAN_POINT('Ctrl Pts',(63.9321269655215,4.80398409923516,336.062796266289));
#31647=CARTESIAN_POINT('Ctrl Pts',(63.924351886743,4.83168029131735,335.928855410731));
#31648=CARTESIAN_POINT('Ctrl Pts',(63.9165768079646,4.85376567557622,335.793814732225));
#31649=CARTESIAN_POINT('Ctrl Pts',(63.9088112969156,4.87582388236372,335.658940229872));
#31650=CARTESIAN_POINT('Ctrl Pts',(63.9010457858666,4.89228495673134,335.522968979514));
#31651=CARTESIAN_POINT('Ctrl Pts',(63.8932802748176,4.90304745472148,335.386404864422));
#31652=CARTESIAN_POINT('Ctrl Pts',(63.8855224632954,4.91379928166351,335.249976153048));
#31653=CARTESIAN_POINT('Ctrl Pts',(63.8777646517732,4.91886374584472,335.112956133905));
#31654=CARTESIAN_POINT('Ctrl Pts',(63.8700068402511,4.91819074322881,334.97585718081));
#31655=CARTESIAN_POINT('Ctrl Pts',(63.862254866728,4.91751824706871,334.838861399024));
#31656=CARTESIAN_POINT('Ctrl Pts',(63.854502893205,4.91111688004535,334.701787190814));
#31657=CARTESIAN_POINT('Ctrl Pts',(63.846750919682,4.89898851970082,334.565149972589));
#31658=CARTESIAN_POINT('Ctrl Pts',(63.8390022291243,4.88686529572412,334.428570620307));
#31659=CARTESIAN_POINT('Ctrl Pts',(63.8312535385667,4.86901993683374,334.29242827846));
#31660=CARTESIAN_POINT('Ctrl Pts',(63.8235048480091,4.84550637213241,334.157236059075));
#31661=CARTESIAN_POINT('Ctrl Pts',(63.8157577696313,4.8219976996246,334.022071967559));
#31662=CARTESIAN_POINT('Ctrl Pts',(63.8080106912535,4.79282323398786,333.887857990155));
#31663=CARTESIAN_POINT('Ctrl Pts',(63.8002636128756,4.75808844427899,333.755099434124));
#31664=CARTESIAN_POINT('Ctrl Pts',(63.7925164695698,4.72335336345914,333.622339765448));
#31665=CARTESIAN_POINT('Ctrl Pts',(63.784769326264,4.6830579645558,333.49103592062));
#31666=CARTESIAN_POINT('Ctrl Pts',(63.7770221829582,4.6373581497214,333.361679990444));
#31667=CARTESIAN_POINT('Ctrl Pts',(63.7692732979302,4.59164806059842,333.232294978308));
#31668=CARTESIAN_POINT('Ctrl Pts',(63.7615244129021,4.54053126795435,333.104859120739));
#31669=CARTESIAN_POINT('Ctrl Pts',(63.753775527874,4.48421241814045,332.979846032726));
#31670=CARTESIAN_POINT('Ctrl Pts',(63.7460184180992,4.42783379091744,332.854700254529));
#31671=CARTESIAN_POINT('Ctrl Pts',(63.7382613083245,4.36624223757976,332.731982739749));
#31672=CARTESIAN_POINT('Ctrl Pts',(63.7305041985498,4.29968937923557,332.612144412954));
#31673=CARTESIAN_POINT('Ctrl Pts',(63.7227429436236,4.23310095717178,332.492242048388));
#31674=CARTESIAN_POINT('Ctrl Pts',(63.7149816886975,4.16154615122746,332.375222270802));
#31675=CARTESIAN_POINT('Ctrl Pts',(63.7072204337713,4.08532028547939,332.261507489959));
#31676=CARTESIAN_POINT('Ctrl Pts',(63.6994467633666,4.00897248318813,332.147610802527));
#31677=CARTESIAN_POINT('Ctrl Pts',(63.691673092962,3.92793892063876,332.037029992114));
#31678=CARTESIAN_POINT('Ctrl Pts',(63.6838994225573,3.84255616519977,331.930155512117));
#31679=CARTESIAN_POINT('Ctrl Pts',(63.6764876183802,3.76114799756813,331.828256064876));
#31680=CARTESIAN_POINT('Ctrl Pts',(63.6690758142031,3.67578662310787,331.729725871554));
#31681=CARTESIAN_POINT('Ctrl Pts',(63.661664010026,3.58679396066131,331.634871154582));
#31682=CARTESIAN_POINT('Ctrl Pts',(63.6538889312476,3.49343950273298,331.535367325374));
#31683=CARTESIAN_POINT('Ctrl Pts',(63.6461138524692,3.39579377853452,331.439593924113));
#31684=CARTESIAN_POINT('Ctrl Pts',(63.6383387736907,3.29418685969407,331.347943593546));
#31685=CARTESIAN_POINT('Ctrl Pts',(63.6305732626417,3.19270497463588,331.256406044547));
#31686=CARTESIAN_POINT('Ctrl Pts',(63.6228077515927,3.08727188126725,331.168981730332));
#31687=CARTESIAN_POINT('Ctrl Pts',(63.6150422405437,2.9782564086333,331.086028637441));
#31688=CARTESIAN_POINT('Ctrl Pts',(63.6072844290216,2.86934902515838,331.003157792783));
#31689=CARTESIAN_POINT('Ctrl Pts',(63.5995266174994,2.75686664003477,330.924749582242));
#31690=CARTESIAN_POINT('Ctrl Pts',(63.5917688059772,2.64121300516677,330.851123414244));
#31691=CARTESIAN_POINT('Ctrl Pts',(63.5840168324542,2.52564640332603,330.777552652271));
#31692=CARTESIAN_POINT('Ctrl Pts',(63.5762648589312,2.40691363028603,330.708756978989));
#31693=CARTESIAN_POINT('Ctrl Pts',(63.5685128854082,2.28544912674577,330.645013736927));
#31694=CARTESIAN_POINT('Ctrl Pts',(63.5607641948506,2.16403606349503,330.581297490165));
#31695=CARTESIAN_POINT('Ctrl Pts',(63.553015504293,2.03989391610473,330.522629600151));
#31696=CARTESIAN_POINT('Ctrl Pts',(63.5452668137354,1.91348335555601,330.469242391111));
#31697=CARTESIAN_POINT('Ctrl Pts',(63.5375197353576,1.7870990957803,330.415866289725));
#31698=CARTESIAN_POINT('Ctrl Pts',(63.5297726569797,1.65844772146513,330.367768835919));
#31699=CARTESIAN_POINT('Ctrl Pts',(63.5220255786019,1.52801123162574,330.325134789267));
#31700=CARTESIAN_POINT('Ctrl Pts',(63.5142784352961,1.39757364860275,330.2825003853));
#31701=CARTESIAN_POINT('Ctrl Pts',(63.5065312919903,1.26535129174619,330.245329601253));
#31702=CARTESIAN_POINT('Ctrl Pts',(63.4987841486845,1.13184233831114,330.213757634249));
#31703=CARTESIAN_POINT('Ctrl Pts',(63.4910352636564,0.99830336922879,330.182178569198));
#31704=CARTESIAN_POINT('Ctrl Pts',(63.4832863786283,0.863477608293114,330.156200915862));
#31705=CARTESIAN_POINT('Ctrl Pts',(63.4755374936002,0.727874074336119,330.135908883007));
#31706=CARTESIAN_POINT('Ctrl Pts',(63.4677803838255,0.59212660938732,330.115595311979));
#31707=CARTESIAN_POINT('Ctrl Pts',(63.4600232740507,0.455600109511585,330.100979474401));
#31708=CARTESIAN_POINT('Ctrl Pts',(63.452266164276,0.318809933418614,330.092093797875));
#31709=CARTESIAN_POINT('Ctrl Pts',(63.4445049093499,0.18194666102924,330.083203373128));
#31710=CARTESIAN_POINT('Ctrl Pts',(63.4367436544237,0.0448198222391019,
330.080049219756));
#31711=CARTESIAN_POINT('Ctrl Pts',(63.4289823994975,-0.0920555527655096,
330.082611583604));
#31712=CARTESIAN_POINT('Ctrl Pts',(63.4212087290929,-0.229149883762641,
330.085178046399));
#31713=CARTESIAN_POINT('Ctrl Pts',(63.4134350586882,-0.36599155677716,330.093479276283));
#31714=CARTESIAN_POINT('Ctrl Pts',(63.4056613882835,-0.502070095303246,
330.10744354331));
#31715=CARTESIAN_POINT('Ctrl Pts',(63.3982495841064,-0.631814145122987,
330.120757770347));
#31716=CARTESIAN_POINT('Ctrl Pts',(63.3908377799293,-0.760864224492547,
330.139219629968));
#31717=CARTESIAN_POINT('Ctrl Pts',(63.3834259757521,-0.888788615679096,
330.162724128278));
#31718=CARTESIAN_POINT('Ctrl Pts',(63.3756508969737,-1.02298296234413,330.187380652067));
#31719=CARTESIAN_POINT('Ctrl Pts',(63.3678758181953,-1.1563625629749,330.217664541827));
#31720=CARTESIAN_POINT('Ctrl Pts',(63.3601007394168,-1.28841861521052,330.253510714804));
#31721=CARTESIAN_POINT('Ctrl Pts',(63.3523352283678,-1.42031216406704,330.289312776784));
#31722=CARTESIAN_POINT('Ctrl Pts',(63.3445697173188,-1.55088503157779,330.330663401486));
#31723=CARTESIAN_POINT('Ctrl Pts',(63.3368042062697,-1.67963658466572,330.377446159756));
#31724=CARTESIAN_POINT('Ctrl Pts',(63.3290463947475,-1.80826048021356,330.424182532785));
#31725=CARTESIAN_POINT('Ctrl Pts',(63.3212885832253,-1.9350662900519,330.476340188357));
#31726=CARTESIAN_POINT('Ctrl Pts',(63.3135307717031,-2.05956692349905,330.533752453107));
#31727=CARTESIAN_POINT('Ctrl Pts',(63.3057787981801,-2.18397386627105,330.591121513307));
#31728=CARTESIAN_POINT('Ctrl Pts',(63.2980268246572,-2.3060787320014,330.653737148901));
#31729=CARTESIAN_POINT('Ctrl Pts',(63.2902748511342,-2.42541319665132,330.721384115393));
#31730=CARTESIAN_POINT('Ctrl Pts',(63.2825261605766,-2.54469712308501,330.789002433355));
#31731=CARTESIAN_POINT('Ctrl Pts',(63.2747774700189,-2.66121264265049,330.861647651902));
#31732=CARTESIAN_POINT('Ctrl Pts',(63.2670287794613,-2.77451509344808,330.93905810695));
#31733=CARTESIAN_POINT('Ctrl Pts',(63.2592817010835,-2.88779397072437,331.016452456106));
#31734=CARTESIAN_POINT('Ctrl Pts',(63.2515346227056,-2.99786078640036,331.098609849338));
#31735=CARTESIAN_POINT('Ctrl Pts',(63.2437875443278,-3.10429933488433,331.1852249474));
#31736=CARTESIAN_POINT('Ctrl Pts',(63.236040401022,-3.21073877542587,331.27184077138));
#31737=CARTESIAN_POINT('Ctrl Pts',(63.2282932577162,-3.31354958494718,331.362914127994));
#31738=CARTESIAN_POINT('Ctrl Pts',(63.2205461144104,-3.41234848100445,331.458099252282));
#31739=CARTESIAN_POINT('Ctrl Pts',(63.2127972293822,-3.51116958915165,331.553305776207));
#31740=CARTESIAN_POINT('Ctrl Pts',(63.2050483443541,-3.60597670759358,331.652625636142));
#31741=CARTESIAN_POINT('Ctrl Pts',(63.1972994593259,-3.69642356408649,331.755676357487));
#31742=CARTESIAN_POINT('Ctrl Pts',(63.1895423495512,-3.78696642180693,331.858836457932));
#31743=CARTESIAN_POINT('Ctrl Pts',(63.1817852397765,-3.87313951441264,331.965735035974));
#31744=CARTESIAN_POINT('Ctrl Pts',(63.1740281300017,-3.95463668267359,332.075956263913));
#31745=CARTESIAN_POINT('Ctrl Pts',(63.1662668750755,-4.03617740041542,332.186236390551));
#31746=CARTESIAN_POINT('Ctrl Pts',(63.1585056201494,-4.1130369960825,332.299842381388));
#31747=CARTESIAN_POINT('Ctrl Pts',(63.1507443652232,-4.18495336897915,332.416330446444));
#31748=CARTESIAN_POINT('Ctrl Pts',(63.1429706948185,-4.25698478463489,332.533004854441));
#31749=CARTESIAN_POINT('Ctrl Pts',(63.1351970244139,-4.3240569845687,332.652570208483));
#31750=CARTESIAN_POINT('Ctrl Pts',(63.1274233540092,-4.38595403989221,332.774558420795));
#31751=CARTESIAN_POINT('Ctrl Pts',(63.1200115498322,-4.44496977239846,332.890868052475));
#31752=CARTESIAN_POINT('Ctrl Pts',(63.1125997456551,-4.49928120361495,333.009379788961));
#31753=CARTESIAN_POINT('Ctrl Pts',(63.1051879414781,-4.54874299790963,333.129673771379));
#31754=CARTESIAN_POINT('Ctrl Pts',(63.0961336337335,-4.6091658445539,333.27662567548));
#31755=CARTESIAN_POINT('Ctrl Pts',(63.0870793259888,-4.6625195439318,333.426645313086));
#31756=CARTESIAN_POINT('Ctrl Pts',(63.0780250182441,-4.70851907182097,333.579073818667));
#31757=CARTESIAN_POINT('Ctrl Pts',(63.0693519322519,-4.75258183975855,333.725084488269));
#31758=CARTESIAN_POINT('Ctrl Pts',(63.0606788462596,-4.78989686999387,333.87330508545));
#31759=CARTESIAN_POINT('Ctrl Pts',(63.0520057602673,-4.8202607883652,334.02313307219));
#31760=CARTESIAN_POINT('Ctrl Pts',(63.0433595919639,-4.85053046963215,334.17249605453));
#31761=CARTESIAN_POINT('Ctrl Pts',(63.0347134236606,-4.87389200367215,334.323456262872));
#31762=CARTESIAN_POINT('Ctrl Pts',(63.0260672553572,-4.8901916756631,334.475396875938));
#31763=CARTESIAN_POINT('Ctrl Pts',(63.0174618850766,-4.90641443562036,334.626620538285));
#31764=CARTESIAN_POINT('Ctrl Pts',(63.0088565147959,-4.91564172524436,334.778815161151));
#31765=CARTESIAN_POINT('Ctrl Pts',(63.0002511445153,-4.91777094463565,334.93135600101));
#31766=CARTESIAN_POINT('Ctrl Pts',(62.9990128458577,-4.91807733581093,334.953306377469));
#31767=CARTESIAN_POINT('Ctrl Pts',(62.9977745472,-4.91823683361801,334.975263897979));
#31768=CARTESIAN_POINT('Ctrl Pts',(62.9965362485424,-4.91824921808336,334.997226676644));
#31769=CARTESIAN_POINT('',(66.4965362485266,-4.91824813384112,335.00428444493));
#31770=CARTESIAN_POINT('Ctrl Pts',(66.49653624849,-4.91824813384056,335.004284445576));
#31771=CARTESIAN_POINT('Ctrl Pts',(66.4850389575283,-4.91807160973532,335.20692194809));
#31772=CARTESIAN_POINT('Ctrl Pts',(66.4735416665666,-4.90536856690133,335.409034498468));
#31773=CARTESIAN_POINT('Ctrl Pts',(66.4620443756049,-4.8803514912982,335.609386891788));
#31774=CARTESIAN_POINT('Ctrl Pts',(66.4560443679917,-4.86729601200498,335.713943338107));
#31775=CARTESIAN_POINT('Ctrl Pts',(66.4500443603786,-4.85088762851043,335.818021062282));
#31776=CARTESIAN_POINT('Ctrl Pts',(66.4440443527654,-4.83116108478416,335.921447576028));
#31777=CARTESIAN_POINT('Ctrl Pts',(66.4362692739869,-4.80559854530318,336.055472287993));
#31778=CARTESIAN_POINT('Ctrl Pts',(66.4284941952085,-4.77441427245794,336.188644255654));
#31779=CARTESIAN_POINT('Ctrl Pts',(66.4207191164301,-4.7376767848386,336.320455127939));
#31780=CARTESIAN_POINT('Ctrl Pts',(66.412953605381,-4.70098450503661,336.452103798555));
#31781=CARTESIAN_POINT('Ctrl Pts',(66.405188094332,-4.65875271127288,336.582394333471));
#31782=CARTESIAN_POINT('Ctrl Pts',(66.397422583283,-4.61110121217894,336.710826897597));
#31783=CARTESIAN_POINT('Ctrl Pts',(66.3896647717608,-4.56349695968512,336.839132120462));
#31784=CARTESIAN_POINT('Ctrl Pts',(66.3819069602386,-4.51048383082645,336.965582674482));
#31785=CARTESIAN_POINT('Ctrl Pts',(66.3741491487164,-4.45223178580728,337.08969260609));
#31786=CARTESIAN_POINT('Ctrl Pts',(66.3663971751934,-4.39402357729927,337.213709141038));
#31787=CARTESIAN_POINT('Ctrl Pts',(66.3586452016703,-4.3305844652939,337.335388207126));
#31788=CARTESIAN_POINT('Ctrl Pts',(66.3508932281473,-4.26213285323817,337.454262945132));
#31789=CARTESIAN_POINT('Ctrl Pts',(66.3431445375897,-4.19371023048078,337.573087339616));
#31790=CARTESIAN_POINT('Ctrl Pts',(66.3353958470321,-4.12027952441099,337.689109430114));
#31791=CARTESIAN_POINT('Ctrl Pts',(66.3276471564745,-4.04210539715163,337.801886332601));
#31792=CARTESIAN_POINT('Ctrl Pts',(66.3199000780966,-3.96394753467243,337.914639770912));
#31793=CARTESIAN_POINT('Ctrl Pts',(66.3121529997188,-3.88104843657232,338.024149043168));
#31794=CARTESIAN_POINT('Ctrl Pts',(66.3044059213409,-3.79371624689646,338.13000001606));
#31795=CARTESIAN_POINT('Ctrl Pts',(66.2966587780351,-3.70638332529279,338.235851876084));
#31796=CARTESIAN_POINT('Ctrl Pts',(66.2889116347293,-3.61461748676222,338.338045074088));
#31797=CARTESIAN_POINT('Ctrl Pts',(66.2811644914235,-3.51876707772084,338.436198672261));
#31798=CARTESIAN_POINT('Ctrl Pts',(66.2734156063954,-3.4228951194726,338.534374337447));
#31799=CARTESIAN_POINT('Ctrl Pts',(66.2656667213674,-3.32293703643878,338.628508316014));
#31800=CARTESIAN_POINT('Ctrl Pts',(66.2579178363393,-3.21927763380795,338.718256927508));
#31801=CARTESIAN_POINT('Ctrl Pts',(66.2501607265645,-3.11550820601595,338.808100799107));
#31802=CARTESIAN_POINT('Ctrl Pts',(66.2424036167898,-3.00802990681466,338.89354974923));
#31803=CARTESIAN_POINT('Ctrl Pts',(66.2346465070151,-2.89726062273687,338.974300434849));
#31804=CARTESIAN_POINT('Ctrl Pts',(66.2268852520889,-2.7864321470953,339.055094271052));
#31805=CARTESIAN_POINT('Ctrl Pts',(66.2191239971627,-2.67230950746492,339.131184623423));
#31806=CARTESIAN_POINT('Ctrl Pts',(66.2113627422365,-2.55533825437342,339.202312395365));
#31807=CARTESIAN_POINT('Ctrl Pts',(66.2035890718318,-2.43817988539798,339.273553948561));
#31808=CARTESIAN_POINT('Ctrl Pts',(66.1958154014272,-2.31816413938298,339.339816868807));
#31809=CARTESIAN_POINT('Ctrl Pts',(66.1880417310225,-2.19576055217275,339.400888394407));
#31810=CARTESIAN_POINT('Ctrl Pts',(66.1806299268455,-2.07905488139724,339.459117025796));
#31811=CARTESIAN_POINT('Ctrl Pts',(66.1732181226685,-1.96017893697345,339.512626586462));
#31812=CARTESIAN_POINT('Ctrl Pts',(66.1658063184915,-1.83955355003807,339.561274580536));
#31813=CARTESIAN_POINT('Ctrl Pts',(66.158031239713,-1.71301595356296,339.612306957714));
#31814=CARTESIAN_POINT('Ctrl Pts',(66.1502561609346,-1.5841532054684,339.658150430498));
#31815=CARTESIAN_POINT('Ctrl Pts',(66.1424810821562,-1.45342986835477,339.698587519699));
#31816=CARTESIAN_POINT('Ctrl Pts',(66.1347155711072,-1.32286739462962,339.738974848488));
#31817=CARTESIAN_POINT('Ctrl Pts',(66.1269500600581,-1.19044925732672,339.773968916648));
#31818=CARTESIAN_POINT('Ctrl Pts',(66.1191845490091,-1.05666061376249,339.803399984368));
#31819=CARTESIAN_POINT('Ctrl Pts',(66.1114267374869,-0.92300462202786,339.832801871098));
#31820=CARTESIAN_POINT('Ctrl Pts',(66.1036689259647,-0.787981207529575,
339.856651650567));
#31821=CARTESIAN_POINT('Ctrl Pts',(66.0959111144425,-0.65209099421004,339.874829268576));
#31822=CARTESIAN_POINT('Ctrl Pts',(66.0881591409195,-0.51630304258554,339.892993207352));
#31823=CARTESIAN_POINT('Ctrl Pts',(66.0804071673965,-0.379649976361819,
339.905493429256));
#31824=CARTESIAN_POINT('Ctrl Pts',(66.0726551938735,-0.242642578055625,
339.912260950094));
#31825=CARTESIAN_POINT('Ctrl Pts',(66.0649065033159,-0.105693202463863,
339.919025604882));
#31826=CARTESIAN_POINT('Ctrl Pts',(66.0571578127583,0.0316098171660805,
339.920062368087));
#31827=CARTESIAN_POINT('Ctrl Pts',(66.0494091222006,0.168750826347874,339.915354129776));
#31828=CARTESIAN_POINT('Ctrl Pts',(66.0416620438228,0.305863302197189,339.910646871053));
#31829=CARTESIAN_POINT('Ctrl Pts',(66.033914965445,0.442813444246325,339.900197001745));
#31830=CARTESIAN_POINT('Ctrl Pts',(66.0261678870671,0.579086244535765,339.884039535455));
#31831=CARTESIAN_POINT('Ctrl Pts',(66.0184207437613,0.715360186922433,339.86788193375));
#31832=CARTESIAN_POINT('Ctrl Pts',(66.0106736004556,0.850956388071212,339.846016685676));
#31833=CARTESIAN_POINT('Ctrl Pts',(66.0029264571498,0.98536599901788,339.818530575858));
#31834=CARTESIAN_POINT('Ctrl Pts',(65.9951775721216,1.11980582809887,339.791038286579));
#31835=CARTESIAN_POINT('Ctrl Pts',(65.9874286870936,1.25305815325959,339.757922699253));
#31836=CARTESIAN_POINT('Ctrl Pts',(65.9796798020655,1.38462572610689,339.719321419558));
#31837=CARTESIAN_POINT('Ctrl Pts',(65.9719226922907,1.51633294613527,339.680679168067));
#31838=CARTESIAN_POINT('Ctrl Pts',(65.964165582516,1.64635146606899,339.636539703291));
#31839=CARTESIAN_POINT('Ctrl Pts',(65.9564084727413,1.7742000559003,339.587090278613));
#31840=CARTESIAN_POINT('Ctrl Pts',(65.9486472178151,1.90211696393022,339.537614429743));
#31841=CARTESIAN_POINT('Ctrl Pts',(65.9408859628889,2.027861273215,339.48282312311));
#31842=CARTESIAN_POINT('Ctrl Pts',(65.9331247079628,2.15097399094221,339.422950819621));
#31843=CARTESIAN_POINT('Ctrl Pts',(65.9253510375581,2.27428364889544,339.36298273996));
#31844=CARTESIAN_POINT('Ctrl Pts',(65.9175773671534,2.39495295885802,339.297917607023));
#31845=CARTESIAN_POINT('Ctrl Pts',(65.9098036967488,2.51254891219449,339.228035125957));
#31846=CARTESIAN_POINT('Ctrl Pts',(65.9023918925717,2.62467074561071,339.161405691199));
#31847=CARTESIAN_POINT('Ctrl Pts',(65.8949800883947,2.73399867138034,339.09039746708));
#31848=CARTESIAN_POINT('Ctrl Pts',(65.8875682842176,2.84018512581103,339.01528722679));
#31849=CARTESIAN_POINT('Ctrl Pts',(65.8797932054392,2.95157609468705,338.936495609881));
#31850=CARTESIAN_POINT('Ctrl Pts',(65.8720181266607,3.05986187611574,338.852940709464));
#31851=CARTESIAN_POINT('Ctrl Pts',(65.8642430478823,3.16460818572794,338.764895495671));
#31852=CARTESIAN_POINT('Ctrl Pts',(65.8564775368333,3.26922559833768,338.676958627119));
#31853=CARTESIAN_POINT('Ctrl Pts',(65.8487120257843,3.37031190906547,338.584542688685));
#31854=CARTESIAN_POINT('Ctrl Pts',(65.8409465147353,3.46746183361833,338.487963803554));
#31855=CARTESIAN_POINT('Ctrl Pts',(65.8331887032131,3.56451543373815,338.391480676668));
#31856=CARTESIAN_POINT('Ctrl Pts',(65.8254308916908,3.65764013933336,338.290843090989));
#31857=CARTESIAN_POINT('Ctrl Pts',(65.8176730801686,3.74646407792625,338.186407063655));
#31858=CARTESIAN_POINT('Ctrl Pts',(65.8099211066456,3.83522117368845,338.082049627743));
#31859=CARTESIAN_POINT('Ctrl Pts',(65.8021691331226,3.91968369225314,337.973899736325));
#31860=CARTESIAN_POINT('Ctrl Pts',(65.7944171595996,3.99951720961025,337.86234958601));
#31861=CARTESIAN_POINT('Ctrl Pts',(65.786668469042,4.07931691742543,337.75084667725));
#31862=CARTESIAN_POINT('Ctrl Pts',(65.7789197784844,4.15449129609051,337.635946690871));
#31863=CARTESIAN_POINT('Ctrl Pts',(65.7711710879267,4.22474690726673,337.518073992567));
#31864=CARTESIAN_POINT('Ctrl Pts',(65.7634240095489,4.29498790117625,337.400225818661));
#31865=CARTESIAN_POINT('Ctrl Pts',(65.7556769311711,4.3603119631969,337.279406498613));
#31866=CARTESIAN_POINT('Ctrl Pts',(65.7479298527933,4.42046983665772,337.156068061472));
#31867=CARTESIAN_POINT('Ctrl Pts',(65.7401827094875,4.48062821429947,337.032728590636));
#31868=CARTESIAN_POINT('Ctrl Pts',(65.7324355661817,4.5356201456691,336.906870311911));
#31869=CARTESIAN_POINT('Ctrl Pts',(65.7246884228759,4.58524324243812,336.778968091388));
#31870=CARTESIAN_POINT('Ctrl Pts',(65.7169395378478,4.63487749553275,336.65103711573));
#31871=CARTESIAN_POINT('Ctrl Pts',(65.7091906528196,4.67914037082135,336.521061648214));
#31872=CARTESIAN_POINT('Ctrl Pts',(65.7014417677916,4.71787849421724,336.389534301952));
#31873=CARTESIAN_POINT('Ctrl Pts',(65.6936846580168,4.75665773465756,336.257867351206));
#31874=CARTESIAN_POINT('Ctrl Pts',(65.6859275482421,4.78990039865099,336.124645606858));
#31875=CARTESIAN_POINT('Ctrl Pts',(65.6781704384674,4.81750353038996,335.990375079038));
#31876=CARTESIAN_POINT('Ctrl Pts',(65.6704091835412,4.84512141235998,335.856032801341));
#31877=CARTESIAN_POINT('Ctrl Pts',(65.662647928615,4.86709369465182,335.720641009083));
#31878=CARTESIAN_POINT('Ctrl Pts',(65.6548866736888,4.88336915309756,335.584712559362));
#31879=CARTESIAN_POINT('Ctrl Pts',(65.6471130032842,4.89967064697264,335.44856666842));
#31880=CARTESIAN_POINT('Ctrl Pts',(65.6393393328796,4.91025707620642,335.311882794437));
#31881=CARTESIAN_POINT('Ctrl Pts',(65.6315656624749,4.91512932500585,335.175176428116));
#31882=CARTESIAN_POINT('Ctrl Pts',(65.6241538582978,4.9197747694515,335.044833776037));
#31883=CARTESIAN_POINT('Ctrl Pts',(65.6167420541206,4.91922605276479,334.914470966325));
#31884=CARTESIAN_POINT('Ctrl Pts',(65.6093302499435,4.91352783276819,334.784530050559));
#31885=CARTESIAN_POINT('Ctrl Pts',(65.6015551711651,4.90755032603547,334.648220343437));
#31886=CARTESIAN_POINT('Ctrl Pts',(65.5937800923866,4.89588687747655,334.511944168663));
#31887=CARTESIAN_POINT('Ctrl Pts',(65.5860050136082,4.87853201730905,334.376214445029));
#31888=CARTESIAN_POINT('Ctrl Pts',(65.5782395025592,4.86119851340186,334.240651745461));
#31889=CARTESIAN_POINT('Ctrl Pts',(65.5704739915102,4.83818758223108,334.105634543076));
#31890=CARTESIAN_POINT('Ctrl Pts',(65.5627084804612,4.80954573594088,333.971674722477));
#31891=CARTESIAN_POINT('Ctrl Pts',(65.554950668939,4.78093228812467,333.83784772343));
#31892=CARTESIAN_POINT('Ctrl Pts',(65.5471928574167,4.74669911701042,333.705076399572));
#31893=CARTESIAN_POINT('Ctrl Pts',(65.5394350458945,4.70694436346909,333.573866127705));
#31894=CARTESIAN_POINT('Ctrl Pts',(65.5316830723715,4.66721952664052,333.442754595729));
#31895=CARTESIAN_POINT('Ctrl Pts',(65.5239310988486,4.62198149092398,333.313202150053));
#31896=CARTESIAN_POINT('Ctrl Pts',(65.5161791253256,4.57137908679407,333.185702255052));
#31897=CARTESIAN_POINT('Ctrl Pts',(65.5084304347679,4.52079811281232,333.058256356333));
#31898=CARTESIAN_POINT('Ctrl Pts',(65.5006817442103,4.46485743278348,332.932861641949));
#31899=CARTESIAN_POINT('Ctrl Pts',(65.4929330536526,4.40375510854871,332.809994519087));
#31900=CARTESIAN_POINT('Ctrl Pts',(65.4851859752748,4.34266549716282,332.687152959755));
#31901=CARTESIAN_POINT('Ctrl Pts',(65.477438896897,4.27641655161998,332.566838295685));
#31902=CARTESIAN_POINT('Ctrl Pts',(65.4696918185192,4.20525350570571,332.449504750985));
#31903=CARTESIAN_POINT('Ctrl Pts',(65.4619446752134,4.13408986337662,332.332170222917));
#31904=CARTESIAN_POINT('Ctrl Pts',(65.4541975319075,4.05801224122849,332.217817198262));
#31905=CARTESIAN_POINT('Ctrl Pts',(65.4464503886017,3.97731044035036,332.106872846973));
#31906=CARTESIAN_POINT('Ctrl Pts',(65.4387015035736,3.89659049599416,331.995903553039));
#31907=CARTESIAN_POINT('Ctrl Pts',(65.4309526185455,3.81124453407735,331.888344773439));
#31908=CARTESIAN_POINT('Ctrl Pts',(65.4232037335174,3.72160380395527,331.784592064934));
#31909=CARTESIAN_POINT('Ctrl Pts',(65.4154466237427,3.63186792823594,331.680729232232));
#31910=CARTESIAN_POINT('Ctrl Pts',(65.407689513968,3.53782843420305,331.58068083675));
#31911=CARTESIAN_POINT('Ctrl Pts',(65.3999324041932,3.43985512127422,331.484807287339));
#31912=CARTESIAN_POINT('Ctrl Pts',(65.3921711492671,3.34182945453953,331.388882506169));
#31913=CARTESIAN_POINT('Ctrl Pts',(65.3844098943409,3.23986607068938,331.297137277661));
#31914=CARTESIAN_POINT('Ctrl Pts',(65.3766486394147,3.13436852186318,331.209892213716));
#31915=CARTESIAN_POINT('Ctrl Pts',(65.36887496901,3.02870221134042,331.122507586101));
#31916=CARTESIAN_POINT('Ctrl Pts',(65.3611012986054,2.91949074999282,331.039637744775));
#31917=CARTESIAN_POINT('Ctrl Pts',(65.3533276282007,2.80716810344607,330.961560907789));
#31918=CARTESIAN_POINT('Ctrl Pts',(65.3459158240237,2.70007410312047,330.88711856635));
#31919=CARTESIAN_POINT('Ctrl Pts',(65.3385040198467,2.59015229318238,330.817033197368));
#31920=CARTESIAN_POINT('Ctrl Pts',(65.3310922156697,2.47779857114452,330.751506466601));
#31921=CARTESIAN_POINT('Ctrl Pts',(65.3233171368912,2.35993805850395,330.682768075564));
#31922=CARTESIAN_POINT('Ctrl Pts',(65.3155420581128,2.23902875454784,330.618829260591));
#31923=CARTESIAN_POINT('Ctrl Pts',(65.3077669793344,2.11549902361918,330.559972191127));
#31924=CARTESIAN_POINT('Ctrl Pts',(65.3000014682854,1.9921213038887,330.501187549034));
#31925=CARTESIAN_POINT('Ctrl Pts',(65.2922359572364,1.86612992271413,330.447472376476));
#31926=CARTESIAN_POINT('Ctrl Pts',(65.2844704461873,1.73798050516856,330.39906457053));
#31927=CARTESIAN_POINT('Ctrl Pts',(65.2767126346652,1.60995814814376,330.350704761064));
#31928=CARTESIAN_POINT('Ctrl Pts',(65.2689548231429,1.47978237617114,330.30764198323));
#31929=CARTESIAN_POINT('Ctrl Pts',(65.2611970116207,1.34793128104159,330.270067196662));
#31930=CARTESIAN_POINT('Ctrl Pts',(65.2534450380977,1.21617940804218,330.232520686313));
#31931=CARTESIAN_POINT('Ctrl Pts',(65.2456930645747,1.08275509570918,330.200454053585));
#31932=CARTESIAN_POINT('Ctrl Pts',(65.2379410910517,0.948153849472003,330.174009185646));
#31933=CARTESIAN_POINT('Ctrl Pts',(65.2301924004941,0.813609606942613,330.147575517123));
#31934=CARTESIAN_POINT('Ctrl Pts',(65.2224437099365,0.677889804599434,330.126758953301));
#31935=CARTESIAN_POINT('Ctrl Pts',(65.2146950193789,0.541502246035292,330.111650751016));
#31936=CARTESIAN_POINT('Ctrl Pts',(65.206947941001,0.40514306404184,330.096545692119));
#31937=CARTESIAN_POINT('Ctrl Pts',(65.1992008626232,0.26811679042755,330.087146675403));
#31938=CARTESIAN_POINT('Ctrl Pts',(65.1914537842454,0.130938102009095,330.083493285274));
#31939=CARTESIAN_POINT('Ctrl Pts',(65.1837066409396,-0.00624173609880257,
330.079839864527));
#31940=CARTESIAN_POINT('Ctrl Pts',(65.1759594976338,-0.143573600822953,
330.08193217682));
#31941=CARTESIAN_POINT('Ctrl Pts',(65.168212354328,-0.280541447838741,330.089757688408));
#31942=CARTESIAN_POINT('Ctrl Pts',(65.1604634692999,-0.417540088134261,
330.097584959337));
#31943=CARTESIAN_POINT('Ctrl Pts',(65.1527145842718,-0.554174157709508,
330.111147972126));
#31944=CARTESIAN_POINT('Ctrl Pts',(65.1449656992437,-0.689931766411287,
330.130382230586));
#31945=CARTESIAN_POINT('Ctrl Pts',(65.137208589469,-0.825833469641766,330.149636904486));
#31946=CARTESIAN_POINT('Ctrl Pts',(65.1294514796943,-0.960856466047415,
330.174574793691));
#31947=CARTESIAN_POINT('Ctrl Pts',(65.1216943699196,-1.09449756045277,330.205079963893));
#31948=CARTESIAN_POINT('Ctrl Pts',(65.1139331149934,-1.22821006838595,330.235601435082));
#31949=CARTESIAN_POINT('Ctrl Pts',(65.1061718600672,-1.36053882599565,330.271696012369));
#31950=CARTESIAN_POINT('Ctrl Pts',(65.098410605141,-1.49099583867701,330.313197841646));
#31951=CARTESIAN_POINT('Ctrl Pts',(65.0906369347364,-1.62166154006283,330.354766060325));
#31952=CARTESIAN_POINT('Ctrl Pts',(65.0828632643318,-1.75044914587142,330.401758681885));
#31953=CARTESIAN_POINT('Ctrl Pts',(65.0750895939271,-1.87688985290771,330.453961335123));
#31954=CARTESIAN_POINT('Ctrl Pts',(65.06767778975,-1.99744471461211,330.503733942295));
#31955=CARTESIAN_POINT('Ctrl Pts',(65.0602659855729,-2.11586599526626,330.558242322697));
#31956=CARTESIAN_POINT('Ctrl Pts',(65.0528541813957,-2.23176986697115,330.61726269058));
#31957=CARTESIAN_POINT('Ctrl Pts',(65.0450791026173,-2.35335453268751,330.679175822505));
#31958=CARTESIAN_POINT('Ctrl Pts',(65.0373040238389,-2.47255300841858,330.746250074098));
#31959=CARTESIAN_POINT('Ctrl Pts',(65.0295289450605,-2.58889619933093,330.818277922723));
#31960=CARTESIAN_POINT('Ctrl Pts',(65.0217634340115,-2.70509622254001,330.890217136494));
#31961=CARTESIAN_POINT('Ctrl Pts',(65.0139979229625,-2.81844762284406,330.967097614784));
#31962=CARTESIAN_POINT('Ctrl Pts',(65.0062324119135,-2.9285037826456,331.048664952509));
#31963=CARTESIAN_POINT('Ctrl Pts',(64.9984746003913,-3.03845082144427,331.130151415981));
#31964=CARTESIAN_POINT('Ctrl Pts',(64.9907167888692,-3.14510880972732,331.216315259783));
#31965=CARTESIAN_POINT('Ctrl Pts',(64.982958977347,-3.24805844256378,331.306857785545));
#31966=CARTESIAN_POINT('Ctrl Pts',(64.975207003824,-3.35093060253687,331.397332175185));
#31967=CARTESIAN_POINT('Ctrl Pts',(64.9674550303009,-3.45009966939793,331.492178430956));
#31968=CARTESIAN_POINT('Ctrl Pts',(64.9597030567779,-3.54517818078163,331.59105665506));
#31969=CARTESIAN_POINT('Ctrl Pts',(64.9519543662203,-3.64021642635931,331.689893004177));
#31970=CARTESIAN_POINT('Ctrl Pts',(64.9442056756627,-3.73116729162761,331.792757644285));
#31971=CARTESIAN_POINT('Ctrl Pts',(64.9364569851051,-3.81767923510401,331.899272936817));
#31972=CARTESIAN_POINT('Ctrl Pts',(64.9287099067273,-3.90417317904801,332.005766067953));
#31973=CARTESIAN_POINT('Ctrl Pts',(64.9209628283495,-3.98622979194255,332.115908037502));
#31974=CARTESIAN_POINT('Ctrl Pts',(64.9132157499717,-4.06353726525788,332.229287464142));
#31975=CARTESIAN_POINT('Ctrl Pts',(64.9054686066659,-4.14084538648424,332.342667841011));
#31976=CARTESIAN_POINT('Ctrl Pts',(64.89772146336,-4.21340406854225,332.459285406143));
#31977=CARTESIAN_POINT('Ctrl Pts',(64.8899743200543,-4.28094459013163,332.578699424127));
#31978=CARTESIAN_POINT('Ctrl Pts',(64.8822254350262,-4.3485002962641,332.698140288918));
#31979=CARTESIAN_POINT('Ctrl Pts',(64.8744765499981,-4.41103540456437,332.820378517449));
#31980=CARTESIAN_POINT('Ctrl Pts',(64.86672766497,-4.46832713811948,332.944948747781));
#31981=CARTESIAN_POINT('Ctrl Pts',(64.8589705551953,-4.5256796817126,333.069651198244));
#31982=CARTESIAN_POINT('Ctrl Pts',(64.8512134454206,-4.57777756962596,333.196690239295));
#31983=CARTESIAN_POINT('Ctrl Pts',(64.8434563356459,-4.62444598571164,333.325579984671));
#31984=CARTESIAN_POINT('Ctrl Pts',(64.8356950807197,-4.67113933990671,333.454538604605));
#31985=CARTESIAN_POINT('Ctrl Pts',(64.8279338257936,-4.71239732358709,333.585349526865));
#31986=CARTESIAN_POINT('Ctrl Pts',(64.8201725708674,-4.7480953251286,333.717512633204));
#31987=CARTESIAN_POINT('Ctrl Pts',(64.8123989004627,-4.78385043183862,333.849887157441));
#31988=CARTESIAN_POINT('Ctrl Pts',(64.8046252300581,-4.81402769715993,333.98361780669));
#31989=CARTESIAN_POINT('Ctrl Pts',(64.7968515596534,-4.83855369410069,334.118194345786));
#31990=CARTESIAN_POINT('Ctrl Pts',(64.7894397554763,-4.86193799998361,334.246506314611));
#31991=CARTESIAN_POINT('Ctrl Pts',(64.7820279512991,-4.88018528999157,334.375586908248));
#31992=CARTESIAN_POINT('Ctrl Pts',(64.7746161471219,-4.89327603903691,334.504992254316));
#31993=CARTESIAN_POINT('Ctrl Pts',(64.7652561809112,-4.90980763725605,334.668411259691));
#31994=CARTESIAN_POINT('Ctrl Pts',(64.7558962147006,-4.91815464120901,334.832672048007));
#31995=CARTESIAN_POINT('Ctrl Pts',(64.7465362484901,-4.91824918766929,334.997173254461));
#31996=CARTESIAN_POINT('',(68.2465362484391,-4.91824996458591,335.000590212407));
#31997=CARTESIAN_POINT('Ctrl Pts',(68.2465362484391,-4.91824996458591,335.000590212407));
#31998=CARTESIAN_POINT('Ctrl Pts',(68.2383441378392,-4.91823250944352,335.146044209075));
#31999=CARTESIAN_POINT('Ctrl Pts',(68.2301520272394,-4.9117582215266,335.291349637273));
#32000=CARTESIAN_POINT('Ctrl Pts',(68.2219599166395,-4.89889212011513,335.435934694621));
#32001=CARTESIAN_POINT('Ctrl Pts',(68.2137541776497,-4.88600461466552,335.580760283577));
#32002=CARTESIAN_POINT('Ctrl Pts',(68.2055484386599,-4.86670409518988,335.724862792216));
#32003=CARTESIAN_POINT('Ctrl Pts',(68.19734269967,-4.84110687754105,335.867679239538));
#32004=CARTESIAN_POINT('Ctrl Pts',(68.1891149144263,-4.81544088817531,336.01087938998));
#32005=CARTESIAN_POINT('Ctrl Pts',(68.1808871291826,-4.78344442544275,336.15278625445));
#32006=CARTESIAN_POINT('Ctrl Pts',(68.1726593439388,-4.74528454118827,336.292848670827));
#32007=CARTESIAN_POINT('Ctrl Pts',(68.164419561526,-4.70706901491457,336.433115316222));
#32008=CARTESIAN_POINT('Ctrl Pts',(68.1561797791132,-4.66267222273283,336.571531841512));
#32009=CARTESIAN_POINT('Ctrl Pts',(68.1479399967003,-4.61230994494546,336.70756552854));
#32010=CARTESIAN_POINT('Ctrl Pts',(68.1396810005123,-4.56183023086696,336.843916423056));
#32011=CARTESIAN_POINT('Ctrl Pts',(68.1314220043242,-4.50535734070595,336.977873075394));
#32012=CARTESIAN_POINT('Ctrl Pts',(68.1231630081361,-4.44315446345079,337.108924246249));
#32013=CARTESIAN_POINT('Ctrl Pts',(68.1199328582271,-4.41882649262576,337.160179255693));
#32014=CARTESIAN_POINT('Ctrl Pts',(68.1167027083181,-4.39362251811818,337.210990123609));
#32015=CARTESIAN_POINT('Ctrl Pts',(68.113472558409,-4.36756010055526,337.261327448765));
#32016=CARTESIAN_POINT('Ctrl Pts',(68.1056974796306,-4.30482699050945,337.382491072622));
#32017=CARTESIAN_POINT('Ctrl Pts',(68.0979224008521,-4.23694899898551,337.501233693909));
#32018=CARTESIAN_POINT('Ctrl Pts',(68.0901473220737,-4.16413681295339,337.61708763046));
#32019=CARTESIAN_POINT('Ctrl Pts',(68.0823818110247,-4.09141422695164,337.732799001366));
#32020=CARTESIAN_POINT('Ctrl Pts',(68.0746162999757,-4.01376973366603,337.845628432614));
#32021=CARTESIAN_POINT('Ctrl Pts',(68.0668507889267,-3.93146074959675,337.955131035484));
#32022=CARTESIAN_POINT('Ctrl Pts',(68.0590929774045,-3.84923337512486,338.064525066204));
#32023=CARTESIAN_POINT('Ctrl Pts',(68.0513351658823,-3.76235094693859,338.170598522431));
#32024=CARTESIAN_POINT('Ctrl Pts',(68.0435773543601,-3.67111498929645,338.272934126722));
#32025=CARTESIAN_POINT('Ctrl Pts',(68.0358253808371,-3.57994768960564,338.375192720226));
#32026=CARTESIAN_POINT('Ctrl Pts',(68.0280734073141,-3.48443364057982,338.473718770054));
#32027=CARTESIAN_POINT('Ctrl Pts',(68.0203214337911,-3.38491534984609,338.568127118935));
#32028=CARTESIAN_POINT('Ctrl Pts',(68.0125727432335,-3.28543920516764,338.662495485823));
#32029=CARTESIAN_POINT('Ctrl Pts',(68.0048240526758,-3.1819624745896,338.752749351704));
#32030=CARTESIAN_POINT('Ctrl Pts',(67.9970753621182,-3.07486516297142,338.838539734332));
#32031=CARTESIAN_POINT('Ctrl Pts',(67.9893282837404,-2.96779013384341,338.924312267555));
#32032=CARTESIAN_POINT('Ctrl Pts',(67.9815812053626,-2.85709632690015,339.005622920487));
#32033=CARTESIAN_POINT('Ctrl Pts',(67.9738341269847,-2.74319722056397,339.082162670888));
#32034=CARTESIAN_POINT('Ctrl Pts',(67.9660869836789,-2.62929715964365,339.158703062766));
#32035=CARTESIAN_POINT('Ctrl Pts',(67.9583398403731,-2.51219207017602,339.230472254346));
#32036=CARTESIAN_POINT('Ctrl Pts',(67.9505926970673,-2.39232449291819,339.297204507943));
#32037=CARTESIAN_POINT('Ctrl Pts',(67.9428438120392,-2.27242996688413,339.363951764367));
#32038=CARTESIAN_POINT('Ctrl Pts',(67.9350949270111,-2.14977205865853,339.425659639345));
#32039=CARTESIAN_POINT('Ctrl Pts',(67.927346041983,-2.02481762457754,339.4821085049));
#32040=CARTESIAN_POINT('Ctrl Pts',(67.9195889322083,-1.89973056256911,339.538617285865));
#32041=CARTESIAN_POINT('Ctrl Pts',(67.9118318224336,-1.77234246223286,339.589855745728));
#32042=CARTESIAN_POINT('Ctrl Pts',(67.9040747126588,-1.64314037975421,339.635652354839));
#32043=CARTESIAN_POINT('Ctrl Pts',(67.8963134577327,-1.51386925581384,339.681473436193));
#32044=CARTESIAN_POINT('Ctrl Pts',(67.8885522028065,-1.38278259161438,339.721846757448));
#32045=CARTESIAN_POINT('Ctrl Pts',(67.8807909478804,-1.2503813358319,339.756651088476));
#32046=CARTESIAN_POINT('Ctrl Pts',(67.8730172774757,-1.11776828118954,339.791511095092));
#32047=CARTESIAN_POINT('Ctrl Pts',(67.865243607071,-0.983836814771475,339.820784226016));
#32048=CARTESIAN_POINT('Ctrl Pts',(67.8574699366664,-0.849097656151765,
339.844400502933));
#32049=CARTESIAN_POINT('Ctrl Pts',(67.8500581324893,-0.720630637782078,
339.866917436478));
#32050=CARTESIAN_POINT('Ctrl Pts',(67.8426463283122,-0.591429716341078,
339.884292278768));
#32051=CARTESIAN_POINT('Ctrl Pts',(67.8352345241351,-0.461938885985191,
339.896508503834));
#32052=CARTESIAN_POINT('Ctrl Pts',(67.8274594453566,-0.326101324300288,
339.90932348248));
#32053=CARTESIAN_POINT('Ctrl Pts',(67.8196843665782,-0.189515444745477,
339.916501877123));
#32054=CARTESIAN_POINT('Ctrl Pts',(67.8119092877997,-0.0526885460399227,
339.917967769274));
#32055=CARTESIAN_POINT('Ctrl Pts',(67.8041437767507,0.0839699784559471,
339.919431857551));
#32056=CARTESIAN_POINT('Ctrl Pts',(67.7963782657017,0.220868544859206,339.915197426074));
#32057=CARTESIAN_POINT('Ctrl Pts',(67.7886127546527,0.357493733916682,339.905240187056));
#32058=CARTESIAN_POINT('Ctrl Pts',(67.7808549431305,0.493983458701527,339.89529282067));
#32059=CARTESIAN_POINT('Ctrl Pts',(67.7730971316083,0.630199958225146,339.87963396691));
#32060=CARTESIAN_POINT('Ctrl Pts',(67.7653393200861,0.765629162906398,339.858291371193));
#32061=CARTESIAN_POINT('Ctrl Pts',(67.7575873465631,0.900956452816237,339.836964836455));
#32062=CARTESIAN_POINT('Ctrl Pts',(67.7498353730401,1.03549724260055,339.809963133912));
#32063=CARTESIAN_POINT('Ctrl Pts',(67.7420833995171,1.16874229476243,339.777365854834));
#32064=CARTESIAN_POINT('Ctrl Pts',(67.7343347089595,1.30193091756562,339.744782380723));
#32065=CARTESIAN_POINT('Ctrl Pts',(67.7265860184018,1.43382451527536,339.706608135994));
#32066=CARTESIAN_POINT('Ctrl Pts',(67.7188373278442,1.56392397884424,339.662973820524));
#32067=CARTESIAN_POINT('Ctrl Pts',(67.7110902494664,1.69399637413319,339.619348583539));
#32068=CARTESIAN_POINT('Ctrl Pts',(67.7033431710885,1.822275007417,339.570265659637));
#32069=CARTESIAN_POINT('Ctrl Pts',(67.6955960927107,1.94827625840118,339.51590552198));
#32070=CARTESIAN_POINT('Ctrl Pts',(67.6878489494049,2.07427856539712,339.461544928733));
#32071=CARTESIAN_POINT('Ctrl Pts',(67.6801018060991,2.19800309312541,339.401907188351));
#32072=CARTESIAN_POINT('Ctrl Pts',(67.6723546627933,2.3189868928995,339.33722063689));
#32073=CARTESIAN_POINT('Ctrl Pts',(67.6646057777652,2.43999789240033,339.272519542518));
#32074=CARTESIAN_POINT('Ctrl Pts',(67.6568568927371,2.55826659319983,339.202767562647));
#32075=CARTESIAN_POINT('Ctrl Pts',(67.649108007709,2.67335566269407,339.128238433429));
#32076=CARTESIAN_POINT('Ctrl Pts',(67.6413508979342,2.78856688891576,339.053630198224));
#32077=CARTESIAN_POINT('Ctrl Pts',(67.6335937881595,2.90059141355886,338.974234897639));
#32078=CARTESIAN_POINT('Ctrl Pts',(67.6258366783848,3.00902141963126,338.890369283076));
#32079=CARTESIAN_POINT('Ctrl Pts',(67.6180754234586,3.11750936723192,338.80645885341));
#32080=CARTESIAN_POINT('Ctrl Pts',(67.6103141685325,3.22239867015139,338.718073601625));
#32081=CARTESIAN_POINT('Ctrl Pts',(67.6025529136063,3.3233162913176,338.625569181572));
#32082=CARTESIAN_POINT('Ctrl Pts',(67.5947792432016,3.4243953477887,338.532916784594));
#32083=CARTESIAN_POINT('Ctrl Pts',(67.587005572797,3.52148974956198,338.436132328015));
#32084=CARTESIAN_POINT('Ctrl Pts',(67.5792319023923,3.61426427071333,338.33560741754));
#32085=CARTESIAN_POINT('Ctrl Pts',(67.5718200982153,3.70272011558394,338.239761965832));
#32086=CARTESIAN_POINT('Ctrl Pts',(67.5644082940383,3.78724902327938,338.140516678744));
#32087=CARTESIAN_POINT('Ctrl Pts',(67.5569964898613,3.86759682604606,338.038235977283));
#32088=CARTESIAN_POINT('Ctrl Pts',(67.5492214110828,3.95188271397092,337.930942193964));
#32089=CARTESIAN_POINT('Ctrl Pts',(67.5414463323044,4.03183363589342,337.819968855152));
#32090=CARTESIAN_POINT('Ctrl Pts',(67.533671253526,4.10711122189202,337.705701475313));
#32091=CARTESIAN_POINT('Ctrl Pts',(67.525905742477,4.18229617402865,337.591574708759));
#32092=CARTESIAN_POINT('Ctrl Pts',(67.518140231428,4.2528190197808,337.474162289823));
#32093=CARTESIAN_POINT('Ctrl Pts',(67.510374720379,4.3183814944129,337.353882820196));
#32094=CARTESIAN_POINT('Ctrl Pts',(67.5026169088568,4.38387896366047,337.233722608012));
#32095=CARTESIAN_POINT('Ctrl Pts',(67.4948590973346,4.44442566346064,337.110701343238));
#32096=CARTESIAN_POINT('Ctrl Pts',(67.4871012858124,4.49976673297661,336.985266332585));
#32097=CARTESIAN_POINT('Ctrl Pts',(67.4793493122893,4.55506615658283,336.859925715756));
#32098=CARTESIAN_POINT('Ctrl Pts',(67.4715973387663,4.60516759015947,336.732175324721));
#32099=CARTESIAN_POINT('Ctrl Pts',(67.4638453652433,4.64986238607439,336.602486459559));
#32100=CARTESIAN_POINT('Ctrl Pts',(67.4560966746857,4.6945382537167,336.472852517708));
#32101=CARTESIAN_POINT('Ctrl Pts',(67.4483479841281,4.73381191068625,336.341282103307));
#32102=CARTESIAN_POINT('Ctrl Pts',(67.4405992935705,4.76752316875362,336.208265657005));
#32103=CARTESIAN_POINT('Ctrl Pts',(67.4328522151926,4.80122741291215,336.075276885885));
#32104=CARTESIAN_POINT('Ctrl Pts',(67.4251051368148,4.82937146416139,335.940843059952));
#32105=CARTESIAN_POINT('Ctrl Pts',(67.417358058437,4.85184537154071,335.80546853021));
#32106=CARTESIAN_POINT('Ctrl Pts',(67.4096109151312,4.87431946727301,335.6700928659));
#32107=CARTESIAN_POINT('Ctrl Pts',(67.4018637718254,4.89112326033665,335.533776867653));
#32108=CARTESIAN_POINT('Ctrl Pts',(67.3941166285196,4.9021982352922,335.397033404638));
#32109=CARTESIAN_POINT('Ctrl Pts',(67.3863677434915,4.91327570013724,335.260259198788));
#32110=CARTESIAN_POINT('Ctrl Pts',(67.3786188584634,4.91862175243003,335.123057726458));
#32111=CARTESIAN_POINT('Ctrl Pts',(67.3708699734353,4.91822991697447,334.985944884303));
#32112=CARTESIAN_POINT('Ctrl Pts',(67.3631128636606,4.91783766562072,334.84868650916));
#32113=CARTESIAN_POINT('Ctrl Pts',(67.3553557538858,4.911695361785,334.711517343602));
#32114=CARTESIAN_POINT('Ctrl Pts',(67.3475986441111,4.8998486753028,334.574951741995));
#32115=CARTESIAN_POINT('Ctrl Pts',(67.339837389185,4.88799565833015,334.438313164097));
#32116=CARTESIAN_POINT('Ctrl Pts',(67.3320761342588,4.87043223484404,334.302279180271));
#32117=CARTESIAN_POINT('Ctrl Pts',(67.3243148793326,4.84725560999143,334.167355950056));
#32118=CARTESIAN_POINT('Ctrl Pts',(67.316541208928,4.82404191009229,334.032216886645));
#32119=CARTESIAN_POINT('Ctrl Pts',(67.3087675385233,4.79519714782457,333.898192509829));
#32120=CARTESIAN_POINT('Ctrl Pts',(67.3009938681187,4.76086922279677,333.765776638559));
#32121=CARTESIAN_POINT('Ctrl Pts',(67.2935820639415,4.72813927093746,333.639524757952));
#32122=CARTESIAN_POINT('Ctrl Pts',(67.2861702597643,4.69042523394044,333.514735276587));
#32123=CARTESIAN_POINT('Ctrl Pts',(67.2787584555871,4.64789601645093,333.391819138666));
#32124=CARTESIAN_POINT('Ctrl Pts',(67.2709833768087,4.60328231532474,333.26287851468));
#32125=CARTESIAN_POINT('Ctrl Pts',(67.2632082980302,4.55322849864028,333.135592037477));
#32126=CARTESIAN_POINT('Ctrl Pts',(67.2554332192518,4.4978756423563,333.010452873542));
#32127=CARTESIAN_POINT('Ctrl Pts',(67.2476677082028,4.44259090128592,332.885467701315));
#32128=CARTESIAN_POINT('Ctrl Pts',(67.2399021971538,4.38202025175566,332.762624938774));
#32129=CARTESIAN_POINT('Ctrl Pts',(67.2321366861048,4.31635429669298,332.642401932491));
#32130=CARTESIAN_POINT('Ctrl Pts',(67.2243788745826,4.25075344961588,332.52229812767));
#32131=CARTESIAN_POINT('Ctrl Pts',(67.2166210630604,4.18006753695382,332.404809250772));
#32132=CARTESIAN_POINT('Ctrl Pts',(67.2088632515382,4.10453478864253,332.290391683043));
#32133=CARTESIAN_POINT('Ctrl Pts',(67.2011112780151,4.02905888111973,332.176060218162));
#32134=CARTESIAN_POINT('Ctrl Pts',(67.1933593044921,3.94874361239123,332.064795786895));
#32135=CARTESIAN_POINT('Ctrl Pts',(67.1856073309691,3.86387239754204,331.957028893004));
#32136=CARTESIAN_POINT('Ctrl Pts',(67.1778586404115,3.77903712570267,331.849307638456));
#32137=CARTESIAN_POINT('Ctrl Pts',(67.1701099498539,3.68964998660911,331.745081281703));
#32138=CARTESIAN_POINT('Ctrl Pts',(67.1623612592962,3.5960367152237,331.644749934019));
#32139=CARTESIAN_POINT('Ctrl Pts',(67.1546141809184,3.50244292086127,331.544439461111));
#32140=CARTESIAN_POINT('Ctrl Pts',(67.1468671025406,3.40462500964993,331.448022670965));
#32141=CARTESIAN_POINT('Ctrl Pts',(67.1391200241627,3.30294760033661,331.355864956957));
#32142=CARTESIAN_POINT('Ctrl Pts',(67.1313728808569,3.20126933886874,331.26370647058));
#32143=CARTESIAN_POINT('Ctrl Pts',(67.1236257375511,3.09573180439669,331.175807394038));
#32144=CARTESIAN_POINT('Ctrl Pts',(67.1158785942453,2.98673461348322,331.092494477148));
#32145=CARTESIAN_POINT('Ctrl Pts',(67.1081297092172,2.87771291768715,331.009162829745));
#32146=CARTESIAN_POINT('Ctrl Pts',(67.1003808241891,2.76523032819159,330.930419631022));
#32147=CARTESIAN_POINT('Ctrl Pts',(67.092631939161,2.64971716940016,330.856549507393));
#32148=CARTESIAN_POINT('Ctrl Pts',(67.0848748293863,2.53408140374851,330.782600977251));
#32149=CARTESIAN_POINT('Ctrl Pts',(67.0771177196115,2.41540897300358,330.713536065338));
#32150=CARTESIAN_POINT('Ctrl Pts',(67.0693606098368,2.29415712329452,330.649594713577));
#32151=CARTESIAN_POINT('Ctrl Pts',(67.0615993549106,2.17284048047385,330.585619193602));
#32152=CARTESIAN_POINT('Ctrl Pts',(67.0538380999844,2.04894202507939,330.526772856834));
#32153=CARTESIAN_POINT('Ctrl Pts',(67.0460768450583,1.92294000074851,330.473247873362));
#32154=CARTESIAN_POINT('Ctrl Pts',(67.0383031746536,1.79673641424266,330.41963726736));
#32155=CARTESIAN_POINT('Ctrl Pts',(67.030529504249,1.66842290051878,330.371365162715));
#32156=CARTESIAN_POINT('Ctrl Pts',(67.0227558338443,1.53849475943024,330.32857442126));
#32157=CARTESIAN_POINT('Ctrl Pts',(67.0153440296673,1.41461480456986,330.287775599115));
#32158=CARTESIAN_POINT('Ctrl Pts',(67.0079322254903,1.28926743797538,330.251959388634));
#32159=CARTESIAN_POINT('Ctrl Pts',(67.0005204213133,1.16288963539091,330.221206139788));
#32160=CARTESIAN_POINT('Ctrl Pts',(66.9927453425348,1.03031768024012,330.188945582606));
#32161=CARTESIAN_POINT('Ctrl Pts',(66.9849702637564,0.896192773727019,330.162154888396));
#32162=CARTESIAN_POINT('Ctrl Pts',(66.977195184978,0.761005974365572,330.140982304058));
#32163=CARTESIAN_POINT('Ctrl Pts',(66.969429673929,0.625985530967246,330.119835773932));
#32164=CARTESIAN_POINT('Ctrl Pts',(66.9616641628799,0.48990617720738,330.104293657813));
#32165=CARTESIAN_POINT('Ctrl Pts',(66.9538986518309,0.353272470183254,330.094453993253));
#32166=CARTESIAN_POINT('Ctrl Pts',(66.9461408403087,0.216774235877347,330.084624084749));
#32167=CARTESIAN_POINT('Ctrl Pts',(66.9383830287865,0.0797231294808181,
330.080485403925));
#32168=CARTESIAN_POINT('Ctrl Pts',(66.9306252172643,-0.0573681483938241,
330.082084592223));
#32169=CARTESIAN_POINT('Ctrl Pts',(66.9228732437413,-0.194356260734451,
330.083682577082));
#32170=CARTESIAN_POINT('Ctrl Pts',(66.9151212702183,-0.33138409510728,330.091009831896));
#32171=CARTESIAN_POINT('Ctrl Pts',(66.9073692966953,-0.46793625955047,330.104060997163));
#32172=CARTESIAN_POINT('Ctrl Pts',(66.8996206061377,-0.604430594070853,
330.117106635254));
#32173=CARTESIAN_POINT('Ctrl Pts',(66.8918719155801,-0.740449271033134,
330.135871325362));
#32174=CARTESIAN_POINT('Ctrl Pts',(66.8841232250225,-0.875479554450303,
330.160297673179));
#32175=CARTESIAN_POINT('Ctrl Pts',(66.8763761466446,-1.01048174368921,330.18471893889));
#32176=CARTESIAN_POINT('Ctrl Pts',(66.8686290682668,-1.14449556403225,330.214799449738));
#32177=CARTESIAN_POINT('Ctrl Pts',(66.860881989889,-1.27701643226724,330.250430325364));
#32178=CARTESIAN_POINT('Ctrl Pts',(66.8531348465832,-1.40953841115466,330.286061499611));
#32179=CARTESIAN_POINT('Ctrl Pts',(66.8453877032774,-1.54056703550862,330.327243029928));
#32180=CARTESIAN_POINT('Ctrl Pts',(66.8376405599716,-1.66961127898546,330.373815693297));
#32181=CARTESIAN_POINT('Ctrl Pts',(66.8298916749435,-1.79868453434784,330.420398827189));
#32182=CARTESIAN_POINT('Ctrl Pts',(66.8221427899154,-1.92577215349164,330.472375373294));
#32183=CARTESIAN_POINT('Ctrl Pts',(66.8143939048873,-2.05040191476713,330.529537490324));
#32184=CARTESIAN_POINT('Ctrl Pts',(66.8066367951126,-2.17516395935908,330.586760279816));
#32185=CARTESIAN_POINT('Ctrl Pts',(66.7988796853378,-2.29746257892062,330.649179471814));
#32186=CARTESIAN_POINT('Ctrl Pts',(66.7911225755631,-2.41684855905274,330.716540404637));
#32187=CARTESIAN_POINT('Ctrl Pts',(66.7833613206369,-2.53629833523533,330.783937332989));
#32188=CARTESIAN_POINT('Ctrl Pts',(66.7756000657108,-2.65283203876058,330.856281057961));
#32189=CARTESIAN_POINT('Ctrl Pts',(66.7678388107846,-2.76602926462784,330.933273408536));
#32190=CARTESIAN_POINT('Ctrl Pts',(66.76006514038,-2.87940756916561,331.01038892178));
#32191=CARTESIAN_POINT('Ctrl Pts',(66.7522914699753,-2.98943841670535,331.092167687243));
#32192=CARTESIAN_POINT('Ctrl Pts',(66.7445177995706,-3.09573363651364,331.178270507446));
#32193=CARTESIAN_POINT('Ctrl Pts',(66.7371059953935,-3.19708078826693,331.260365220653));
#32194=CARTESIAN_POINT('Ctrl Pts',(66.7296941912164,-3.29503205626142,331.346390288768));
#32195=CARTESIAN_POINT('Ctrl Pts',(66.7222823870393,-3.38928339984472,331.436021731543));
#32196=CARTESIAN_POINT('Ctrl Pts',(66.7146216124402,-3.48670074676993,331.528663990255));
#32197=CARTESIAN_POINT('Ctrl Pts',(66.706960837841,-3.58049266797326,331.625470871143));
#32198=CARTESIAN_POINT('Ctrl Pts',(66.6993000632418,-3.67027405721862,331.726122878389));
#32199=CARTESIAN_POINT('Ctrl Pts',(66.6916488412757,-3.75994349320634,331.826649377218));
#32200=CARTESIAN_POINT('Ctrl Pts',(66.6839976193096,-3.84561207674849,331.931011169319));
#32201=CARTESIAN_POINT('Ctrl Pts',(66.6763463973436,-3.9269291249062,332.038849765638));
#32202=CARTESIAN_POINT('Ctrl Pts',(66.6687038397904,-4.00815408784147,332.146566243147));
#32203=CARTESIAN_POINT('Ctrl Pts',(66.6610612822372,-4.0850370824608,332.257751368257));
#32204=CARTESIAN_POINT('Ctrl Pts',(66.6534187246839,-4.15726603818599,332.372011767483));
#32205=CARTESIAN_POINT('Ctrl Pts',(66.6457810204546,-4.22944912569078,332.486199606874));
#32206=CARTESIAN_POINT('Ctrl Pts',(66.6381433162252,-4.29698383526736,332.603458498373));
#32207=CARTESIAN_POINT('Ctrl Pts',(66.6305056119959,-4.35960007431012,332.723364268361));
#32208=CARTESIAN_POINT('Ctrl Pts',(66.6228709912686,-4.4221910338584,332.843221629864));
#32209=CARTESIAN_POINT('Ctrl Pts',(66.6152363705412,-4.4798672853151,332.96572338788));
#32210=CARTESIAN_POINT('Ctrl Pts',(66.6076017498139,-4.53240385282728,333.090419318966));
#32211=CARTESIAN_POINT('Ctrl Pts',(66.5999684456413,-4.58493136065385,333.215093746822));
#32212=CARTESIAN_POINT('Ctrl Pts',(66.5923351414687,-4.6323207920059,333.341961223155));
#32213=CARTESIAN_POINT('Ctrl Pts',(66.584701837296,-4.67439487409207,333.47055054887));
#32214=CARTESIAN_POINT('Ctrl Pts',(66.5770649754741,-4.71648856561941,333.599199806132));
#32215=CARTESIAN_POINT('Ctrl Pts',(66.5694281136522,-4.75326182912498,333.729572133486));
#32216=CARTESIAN_POINT('Ctrl Pts',(66.5617912518302,-4.78458694957643,333.861180091304));
#32217=CARTESIAN_POINT('Ctrl Pts',(66.5541527205776,-4.8159189177513,333.99281681884));
#32218=CARTESIAN_POINT('Ctrl Pts',(66.546514189325,-4.84180028910966,334.125689319563));
#32219=CARTESIAN_POINT('Ctrl Pts',(66.5388756580723,-4.86215453878236,334.259300125896));
#32220=CARTESIAN_POINT('Ctrl Pts',(66.5312289651637,-4.88253053666523,334.393053693369));
#32221=CARTESIAN_POINT('Ctrl Pts',(66.5235822722552,-4.89736756682387,334.527546741511));
#32222=CARTESIAN_POINT('Ctrl Pts',(66.5159355793466,-4.90664099949656,334.66227649688));
#32223=CARTESIAN_POINT('Ctrl Pts',(66.5094691357399,-4.91448309936048,334.776211027226));
#32224=CARTESIAN_POINT('Ctrl Pts',(66.5030026921332,-4.91834741662029,334.89031464222));
#32225=CARTESIAN_POINT('Ctrl Pts',(66.4965362485266,-4.91824813384112,335.00428444493));
#32226=CARTESIAN_POINT('',(69.9965362484408,-4.9182479192268,334.995475895536));
#32227=CARTESIAN_POINT('Ctrl Pts',(69.9965362484408,-4.9182479192268,334.995475895536));
#32228=CARTESIAN_POINT('Ctrl Pts',(69.9888786876184,-4.91837226176216,335.130651248063));
#32229=CARTESIAN_POINT('Ctrl Pts',(69.9812211267961,-4.91291958376056,335.265984642031));
#32230=CARTESIAN_POINT('Ctrl Pts',(69.9735635659737,-4.90187762434903,335.400972341199));
#32231=CARTESIAN_POINT('Ctrl Pts',(69.9656192825603,-4.89042222007096,335.541014394325));
#32232=CARTESIAN_POINT('Ctrl Pts',(69.9576749991469,-4.87295076806222,335.680683923758));
#32233=CARTESIAN_POINT('Ctrl Pts',(69.9497307157336,-4.84950892526431,335.819418236484));
#32234=CARTESIAN_POINT('Ctrl Pts',(69.9420814518508,-4.82693762057524,335.953000500913));
#32235=CARTESIAN_POINT('Ctrl Pts',(69.934432187968,-4.79883150560313,336.085715334998));
#32236=CARTESIAN_POINT('Ctrl Pts',(69.9267829240852,-4.76528407550447,336.217066449395));
#32237=CARTESIAN_POINT('Ctrl Pts',(69.919134721278,-4.73174129897208,336.348399343287));
#32238=CARTESIAN_POINT('Ctrl Pts',(69.9114865184707,-4.69275880747613,336.478368504336));
#32239=CARTESIAN_POINT('Ctrl Pts',(69.9038383156634,-4.64848079770478,336.606489755918));
#32240=CARTESIAN_POINT('Ctrl Pts',(69.8961894173898,-4.6041987616455,336.734622657822));
#32241=CARTESIAN_POINT('Ctrl Pts',(69.8885405191162,-4.55462038131386,336.860906936359));
#32242=CARTESIAN_POINT('Ctrl Pts',(69.8808916208425,-4.49993893860682,336.984875968747));
#32243=CARTESIAN_POINT('Ctrl Pts',(69.873240270243,-4.44523996439255,337.108884747051));
#32244=CARTESIAN_POINT('Ctrl Pts',(69.8655889196436,-4.38543483662483,337.230576435766));
#32245=CARTESIAN_POINT('Ctrl Pts',(69.8579375690441,-4.3207637078602,337.349507191591));
#32246=CARTESIAN_POINT('Ctrl Pts',(69.8502779279927,-4.25602250612296,337.468566812209));
#32247=CARTESIAN_POINT('Ctrl Pts',(69.8426182869414,-4.18640497263787,337.584859176312));
#32248=CARTESIAN_POINT('Ctrl Pts',(69.83495864589,-4.11219581219732,337.697967506225));
#32249=CARTESIAN_POINT('Ctrl Pts',(69.827294070046,-4.03793884183712,337.811148707199));
#32250=CARTESIAN_POINT('Ctrl Pts',(69.8196294942019,-3.95908458950933,337.921141465313));
#32251=CARTESIAN_POINT('Ctrl Pts',(69.8119649183578,-3.87595847820086,338.027561549789));
#32252=CARTESIAN_POINT('Ctrl Pts',(69.8042896202234,-3.79271607835604,338.134130509699));
#32253=CARTESIAN_POINT('Ctrl Pts',(69.7966143220889,-3.70519015408199,338.237116518811));
#32254=CARTESIAN_POINT('Ctrl Pts',(69.7889390239544,-3.61374357270736,338.336171526348));
#32255=CARTESIAN_POINT('Ctrl Pts',(69.7869262706539,-3.58976282234917,338.362147493648));
#32256=CARTESIAN_POINT('Ctrl Pts',(69.7849135173533,-3.56551263235681,338.387853344704));
#32257=CARTESIAN_POINT('Ctrl Pts',(69.7829007640527,-3.54099991569648,338.413283266818));
#32258=CARTESIAN_POINT('Ctrl Pts',(69.7751256852743,-3.44630957135392,338.511516690511));
#32259=CARTESIAN_POINT('Ctrl Pts',(69.7673506064958,-3.34737875468833,338.605962046973));
#32260=CARTESIAN_POINT('Ctrl Pts',(69.7595755277174,-3.24454281224072,338.696231188932));
#32261=CARTESIAN_POINT('Ctrl Pts',(69.7518100166684,-3.14183341596715,338.786389248966));
#32262=CARTESIAN_POINT('Ctrl Pts',(69.7440445056194,-3.03522874643746,338.872381064435));
#32263=CARTESIAN_POINT('Ctrl Pts',(69.7362789945704,-2.92510243582782,338.95385366477));
#32264=CARTESIAN_POINT('Ctrl Pts',(69.7285211830482,-2.81508531577622,339.035245484784));
#32265=CARTESIAN_POINT('Ctrl Pts',(69.720763371526,-2.70155381556513,339.112126775767));
#32266=CARTESIAN_POINT('Ctrl Pts',(69.7130055600039,-2.58491596580884,339.184183613587));
#32267=CARTESIAN_POINT('Ctrl Pts',(69.7052535864809,-2.46836588973304,339.256186226351));
#32268=CARTESIAN_POINT('Ctrl Pts',(69.6975016129579,-2.34871444823933,339.323371407786));
#32269=CARTESIAN_POINT('Ctrl Pts',(69.6897496394349,-2.22639978957823,339.385467710458));
#32270=CARTESIAN_POINT('Ctrl Pts',(69.6820009488772,-2.1041369312476,339.447537715308));
#32271=CARTESIAN_POINT('Ctrl Pts',(69.6742522583196,-1.97921344681806,339.50452295125));
#32272=CARTESIAN_POINT('Ctrl Pts',(69.666503567762,-1.85209310418054,339.556197339443));
#32273=CARTESIAN_POINT('Ctrl Pts',(69.6587564893841,-1.72499920999185,339.607860976347));
#32274=CARTESIAN_POINT('Ctrl Pts',(69.6510094110063,-1.59570972862215,339.654215816257));
#32275=CARTESIAN_POINT('Ctrl Pts',(69.6432623326285,-1.46470911139812,339.695083628807));
#32276=CARTESIAN_POINT('Ctrl Pts',(69.6355151893227,-1.33370739626284,339.735951783868));
#32277=CARTESIAN_POINT('Ctrl Pts',(69.6277680460169,-1.20099488980739,339.771332703439));
#32278=CARTESIAN_POINT('Ctrl Pts',(69.620020902711,-1.0670715504776,339.801097933667));
#32279=CARTESIAN_POINT('Ctrl Pts',(69.6122720176829,-0.933118102338027,
339.830869855751));
#32280=CARTESIAN_POINT('Ctrl Pts',(69.6045231326549,-0.797953661124003,
339.855023491418));
#32281=CARTESIAN_POINT('Ctrl Pts',(69.5967742476268,-0.662088336959024,
339.873481517002));
#32282=CARTESIAN_POINT('Ctrl Pts',(69.5890171378521,-0.526078803935131,
339.891959134126));
#32283=CARTESIAN_POINT('Ctrl Pts',(69.5812600280773,-0.389367289829594,
339.904729012253));
#32284=CARTESIAN_POINT('Ctrl Pts',(69.5735029183026,-0.252469544443574,
339.911765689813));
#32285=CARTESIAN_POINT('Ctrl Pts',(69.5657416633764,-0.115498645279374,
339.91880612755));
#32286=CARTESIAN_POINT('Ctrl Pts',(69.5579804084502,0.0216582928015551,
339.920107256437));
#32287=CARTESIAN_POINT('Ctrl Pts',(69.550219153524,0.158486553525184,339.91569578746));
#32288=CARTESIAN_POINT('Ctrl Pts',(69.5424454831194,0.295533694873559,339.91127726157));
#32289=CARTESIAN_POINT('Ctrl Pts',(69.5346718127147,0.432250718200474,339.901127905749));
#32290=CARTESIAN_POINT('Ctrl Pts',(69.5268981423101,0.568128162747628,339.885326340501));
#32291=CARTESIAN_POINT('Ctrl Pts',(69.5194863381329,0.697680479561715,339.870260341916));
#32292=CARTESIAN_POINT('Ctrl Pts',(69.5120745339558,0.826469339011665,339.850056556936));
#32293=CARTESIAN_POINT('Ctrl Pts',(69.5046627297787,0.954064481356156,339.824825802857));
#32294=CARTESIAN_POINT('Ctrl Pts',(69.4968876510003,1.08791344171287,339.798358414362));
#32295=CARTESIAN_POINT('Ctrl Pts',(69.4891125722218,1.22087169841239,339.766275181687));
#32296=CARTESIAN_POINT('Ctrl Pts',(69.4813374934434,1.35243137487755,339.728648056131));
#32297=CARTESIAN_POINT('Ctrl Pts',(69.4735719823944,1.48382915878506,339.691067233148));
#32298=CARTESIAN_POINT('Ctrl Pts',(69.4658064713453,1.61383141462508,339.647956197789));
#32299=CARTESIAN_POINT('Ctrl Pts',(69.4580409602963,1.74193912810579,339.599438132693));
#32300=CARTESIAN_POINT('Ctrl Pts',(69.4502831487741,1.86991982241595,339.550968173401));
#32301=CARTESIAN_POINT('Ctrl Pts',(69.4425253372519,1.99600934939483,339.497101990783));
#32302=CARTESIAN_POINT('Ctrl Pts',(69.4347675257296,2.11972291476512,339.438012824127));
#32303=CARTESIAN_POINT('Ctrl Pts',(69.4270155522066,2.24334338175396,339.378968123944));
#32304=CARTESIAN_POINT('Ctrl Pts',(69.4192635786836,2.36459109474623,339.3147084309));
#32305=CARTESIAN_POINT('Ctrl Pts',(69.4115116051606,2.48300068064472,339.245455297423));
#32306=CARTESIAN_POINT('Ctrl Pts',(69.403762914603,2.60136012001328,339.17623149269));
#32307=CARTESIAN_POINT('Ctrl Pts',(69.3960142240453,2.71688348617671,339.102018650488));
#32308=CARTESIAN_POINT('Ctrl Pts',(69.3882655334877,2.82912969319749,339.023084418897));
#32309=CARTESIAN_POINT('Ctrl Pts',(69.3805184551099,2.94135254645741,338.944166610232));
#32310=CARTESIAN_POINT('Ctrl Pts',(69.372771376732,3.05029927727239,338.860529590793));
#32311=CARTESIAN_POINT('Ctrl Pts',(69.3650242983542,3.15555784351558,338.772484295359));
#32312=CARTESIAN_POINT('Ctrl Pts',(69.3572771550484,3.26081729192708,338.68443826202));
#32313=CARTESIAN_POINT('Ctrl Pts',(69.3495300117426,3.36238821429832,338.591984129781));
#32314=CARTESIAN_POINT('Ctrl Pts',(69.3417828684368,3.4598920348416,338.495472810614));
#32315=CARTESIAN_POINT('Ctrl Pts',(69.3340339834087,3.55741777631341,338.398939793654));
#32316=CARTESIAN_POINT('Ctrl Pts',(69.3262850983806,3.65087431871563,338.298348049624));
#32317=CARTESIAN_POINT('Ctrl Pts',(69.3185362133525,3.73992058907056,338.19408469674));
#32318=CARTESIAN_POINT('Ctrl Pts',(69.3107791035777,3.82906137405711,338.089710677654));
#32319=CARTESIAN_POINT('Ctrl Pts',(69.303021993803,3.91378228179486,337.98165756262));
#32320=CARTESIAN_POINT('Ctrl Pts',(69.2952648840283,3.99378279929591,337.870345277932));
#32321=CARTESIAN_POINT('Ctrl Pts',(69.2875036291021,4.07382606651549,337.758973511518));
#32322=CARTESIAN_POINT('Ctrl Pts',(69.279742374176,4.14914370281404,337.644339431671));
#32323=CARTESIAN_POINT('Ctrl Pts',(69.2719811192498,4.21947962751796,337.526890329132));
#32324=CARTESIAN_POINT('Ctrl Pts',(69.2642074488451,4.28992806677902,337.409253346306));
#32325=CARTESIAN_POINT('Ctrl Pts',(69.2564337784405,4.35537868308554,337.288792685855));
#32326=CARTESIAN_POINT('Ctrl Pts',(69.2486601080358,4.41562189164699,337.165979310268));
#32327=CARTESIAN_POINT('Ctrl Pts',(69.2412483038588,4.47306076435524,337.048882926863));
#32328=CARTESIAN_POINT('Ctrl Pts',(69.2338364996819,4.52576601228643,336.929648200018));
#32329=CARTESIAN_POINT('Ctrl Pts',(69.2264246955049,4.57359798583643,336.808696913928));
#32330=CARTESIAN_POINT('Ctrl Pts',(69.2186496167265,4.62377434689503,336.681817445009));
#32331=CARTESIAN_POINT('Ctrl Pts',(69.210874537948,4.66874621391566,336.552647932275));
#32332=CARTESIAN_POINT('Ctrl Pts',(69.2030994591696,4.70829925112364,336.42165439695));
#32333=CARTESIAN_POINT('Ctrl Pts',(69.1953339481206,4.74780361580127,336.290822057511));
#32334=CARTESIAN_POINT('Ctrl Pts',(69.1875684370716,4.78190230659738,336.158170532155));
#32335=CARTESIAN_POINT('Ctrl Pts',(69.1798029260226,4.81042886515467,336.024186113842));
#32336=CARTESIAN_POINT('Ctrl Pts',(69.1720451145004,4.83892713954608,335.89033454147));
#32337=CARTESIAN_POINT('Ctrl Pts',(69.1642873029782,4.86186419546177,335.755153085976));
#32338=CARTESIAN_POINT('Ctrl Pts',(69.156529491456,4.87912336351415,335.619143170931));
#32339=CARTESIAN_POINT('Ctrl Pts',(69.1487775179329,4.89636954349531,335.483235607659));
#32340=CARTESIAN_POINT('Ctrl Pts',(69.1410255444099,4.90794629138625,335.34650121197));
#32341=CARTESIAN_POINT('Ctrl Pts',(69.1332735708869,4.91378807526547,335.209451220762));
#32342=CARTESIAN_POINT('Ctrl Pts',(69.1255248803293,4.91962738514574,335.072459270307));
#32343=CARTESIAN_POINT('Ctrl Pts',(69.1177761897716,4.91973654503682,334.93515237987));
#32344=CARTESIAN_POINT('Ctrl Pts',(69.110027499214,4.91410192900904,334.798046307759));
#32345=CARTESIAN_POINT('Ctrl Pts',(69.1022804208362,4.9084684853102,334.660968761712));
#32346=CARTESIAN_POINT('Ctrl Pts',(69.0945333424584,4.89709365875272,334.524092341184));
#32347=CARTESIAN_POINT('Ctrl Pts',(69.0867862640806,4.88001594138767,334.38793180584));
#32348=CARTESIAN_POINT('Ctrl Pts',(69.0790391207748,4.86293808089493,334.25177012934));
#32349=CARTESIAN_POINT('Ctrl Pts',(69.071291977469,4.84015728290615,334.116324737826));
#32350=CARTESIAN_POINT('Ctrl Pts',(69.0635448341632,4.81176376770433,333.982103882359));
#32351=CARTESIAN_POINT('Ctrl Pts',(69.0557959491351,4.78336386903753,333.847852851195));
#32352=CARTESIAN_POINT('Ctrl Pts',(69.048047064107,4.74934882308201,333.714827286234));
#32353=CARTESIAN_POINT('Ctrl Pts',(69.040298179079,4.70985959164327,333.583523494898));
#32354=CARTESIAN_POINT('Ctrl Pts',(69.0325410693042,4.67032844592617,333.452080336361));
#32355=CARTESIAN_POINT('Ctrl Pts',(69.0247839595295,4.62531162074379,333.322362976972));
#32356=CARTESIAN_POINT('Ctrl Pts',(69.0170268497548,4.57499961625492,333.194851370727));
#32357=CARTESIAN_POINT('Ctrl Pts',(69.0092655948286,4.52466072663955,333.067271626356));
#32358=CARTESIAN_POINT('Ctrl Pts',(69.0015043399025,4.46902117801145,332.941900340854));
#32359=CARTESIAN_POINT('Ctrl Pts',(68.9937430849763,4.40831852675184,332.819194912608));
#32360=CARTESIAN_POINT('Ctrl Pts',(68.9859694145717,4.34751877103316,332.696293195665));
#32361=CARTESIAN_POINT('Ctrl Pts',(68.978195744167,4.2816399157845,332.576066200685));
#32362=CARTESIAN_POINT('Ctrl Pts',(68.9704220737623,4.21096458505192,332.458945036813));
#32363=CARTESIAN_POINT('Ctrl Pts',(68.9630102695851,4.1435792079672,332.347275891294));
#32364=CARTESIAN_POINT('Ctrl Pts',(68.9555984654079,4.07183401628188,332.238430171505));
#32365=CARTESIAN_POINT('Ctrl Pts',(68.9481866612307,3.99600812490951,332.132753563407));
#32366=CARTESIAN_POINT('Ctrl Pts',(68.9404115824522,3.91646578072868,332.021897429953));
#32367=CARTESIAN_POINT('Ctrl Pts',(68.9326365036738,3.83218123948952,331.914178592456));
#32368=CARTESIAN_POINT('Ctrl Pts',(68.9248614248954,3.74343039899669,331.81002948127));
#32369=CARTESIAN_POINT('Ctrl Pts',(68.9170959138464,3.6547887720633,331.706008532195));
#32370=CARTESIAN_POINT('Ctrl Pts',(68.9093304027974,3.56169203256781,331.605548863728));
#32371=CARTESIAN_POINT('Ctrl Pts',(68.9015648917484,3.46445903446503,331.509053615277));
#32372=CARTESIAN_POINT('Ctrl Pts',(68.8938070802262,3.36732244316268,331.412654042144));
#32373=CARTESIAN_POINT('Ctrl Pts',(68.8860492687039,3.26605803035187,331.320211340206));
#32374=CARTESIAN_POINT('Ctrl Pts',(68.8782914571817,3.16102431730964,331.232094968304));
#32375=CARTESIAN_POINT('Ctrl Pts',(68.8705394836587,3.05606964546772,331.144044906767));
#32376=CARTESIAN_POINT('Ctrl Pts',(68.8627875101358,2.94735161759048,331.060314945162));
#32377=CARTESIAN_POINT('Ctrl Pts',(68.8550355366128,2.83526468060926,330.9812368503));
#32378=CARTESIAN_POINT('Ctrl Pts',(68.8472868460552,2.7232252125121,330.902192245057));
#32379=CARTESIAN_POINT('Ctrl Pts',(68.8395381554975,2.60781999170988,330.827795813093));
#32380=CARTESIAN_POINT('Ctrl Pts',(68.8317894649399,2.48947535659532,330.758338119156));
#32381=CARTESIAN_POINT('Ctrl Pts',(68.8240423865621,2.37115534407044,330.688894876473));
#32382=CARTESIAN_POINT('Ctrl Pts',(68.8162953081842,2.2498974705799,330.624388525681));
#32383=CARTESIAN_POINT('Ctrl Pts',(68.8085482298064,2.12615543876557,330.565065263986));
#32384=CARTESIAN_POINT('Ctrl Pts',(68.8008010865006,2.00241236987407,330.505741505104));
#32385=CARTESIAN_POINT('Ctrl Pts',(68.7930539431948,1.87618545359561,330.451601090937));
#32386=CARTESIAN_POINT('Ctrl Pts',(68.785306799889,1.74795091246184,330.402843197135));
#32387=CARTESIAN_POINT('Ctrl Pts',(68.7775579148609,1.61968754148019,330.354074341524));
#32388=CARTESIAN_POINT('Ctrl Pts',(68.7698090298327,1.48941601277807,330.310690553141));
#32389=CARTESIAN_POINT('Ctrl Pts',(68.7620601448046,1.35762996437586,330.272841874622));
#32390=CARTESIAN_POINT('Ctrl Pts',(68.7543030350299,1.22570403690073,330.234953023124));
#32391=CARTESIAN_POINT('Ctrl Pts',(68.7465459252551,1.0922607548206,330.202611125466));
#32392=CARTESIAN_POINT('Ctrl Pts',(68.7387888154804,0.957806812257021,330.175915716647));
#32393=CARTESIAN_POINT('Ctrl Pts',(68.7310275605542,0.823281021805727,330.149206042655));
#32394=CARTESIAN_POINT('Ctrl Pts',(68.7232663056281,0.687743880788366,330.128148929726));
#32395=CARTESIAN_POINT('Ctrl Pts',(68.7155050507019,0.551708580656278,330.112792136145));
#32396=CARTESIAN_POINT('Ctrl Pts',(68.7077313802973,0.415455668377595,330.097410776698));
#32397=CARTESIAN_POINT('Ctrl Pts',(68.6999577098926,0.278703394664759,330.087747985933));
#32398=CARTESIAN_POINT('Ctrl Pts',(68.6921840394879,0.141967232484869,330.083799397156));
#32399=CARTESIAN_POINT('Ctrl Pts',(68.6847722353109,0.0115961715527522,
330.080034616137));
#32400=CARTESIAN_POINT('Ctrl Pts',(68.6773604311339,-0.118759956294964,
330.081464013898));
#32401=CARTESIAN_POINT('Ctrl Pts',(68.6699486269569,-0.248659411263507,
330.088039947262));
#32402=CARTESIAN_POINT('Ctrl Pts',(68.6621735481784,-0.384925625472301,
330.09493818671));
#32403=CARTESIAN_POINT('Ctrl Pts',(68.6543984694,-0.521119895514062,330.107522011695));
#32404=CARTESIAN_POINT('Ctrl Pts',(68.6466233906216,-0.656729277347898,
330.125793426744));
#32405=CARTESIAN_POINT('Ctrl Pts',(68.6388578795725,-0.792171783203887,
330.144042357653));
#32406=CARTESIAN_POINT('Ctrl Pts',(68.6310923685235,-0.927030449261685,
330.167964901045));
#32407=CARTESIAN_POINT('Ctrl Pts',(68.6233268574745,-1.06079371682242,330.197511087691));
#32408=CARTESIAN_POINT('Ctrl Pts',(68.6155690459523,-1.19442435771365,330.227027979207));
#32409=CARTESIAN_POINT('Ctrl Pts',(68.6078112344301,-1.3269613822743,330.262157333941));
#32410=CARTESIAN_POINT('Ctrl Pts',(68.6000534229079,-1.45790008824687,330.302797599082));
#32411=CARTESIAN_POINT('Ctrl Pts',(68.5923014493849,-1.58874025869097,330.343407281134));
#32412=CARTESIAN_POINT('Ctrl Pts',(68.5845494758619,-1.71798413282898,330.389519503525));
#32413=CARTESIAN_POINT('Ctrl Pts',(68.5767975023389,-1.84513926300358,330.440982105472));
#32414=CARTESIAN_POINT('Ctrl Pts',(68.5690488117812,-1.97224054290524,330.492422912977));
#32415=CARTESIAN_POINT('Ctrl Pts',(68.5613001212236,-2.09725447664881,330.54920944701));
#32416=CARTESIAN_POINT('Ctrl Pts',(68.553551430666,-2.21970600596944,330.611140431779));
#32417=CARTESIAN_POINT('Ctrl Pts',(68.5458043522882,-2.34213205822649,330.67305853129));
#32418=CARTESIAN_POINT('Ctrl Pts',(68.5380572739103,-2.46199641791078,330.740118776244));
#32419=CARTESIAN_POINT('Ctrl Pts',(68.5303101955325,-2.57884652800746,330.812072869846));
#32420=CARTESIAN_POINT('Ctrl Pts',(68.5225630522267,-2.69569761742069,330.884027566492));
#32421=CARTESIAN_POINT('Ctrl Pts',(68.5148159089209,-2.80953407402629,330.960875988641));
#32422=CARTESIAN_POINT('Ctrl Pts',(68.507068765615,-2.91993069543224,331.042325455981));
#32423=CARTESIAN_POINT('Ctrl Pts',(68.4993198805869,-3.03035213634224,331.123793234891));
#32424=CARTESIAN_POINT('Ctrl Pts',(68.4915709955589,-3.13733188870471,331.209863885342));
#32425=CARTESIAN_POINT('Ctrl Pts',(68.4838221105308,-3.2404766426096,331.300203493271));
#32426=CARTESIAN_POINT('Ctrl Pts',(68.4760650007561,-3.3437308754219,331.390638988594));
#32427=CARTESIAN_POINT('Ctrl Pts',(68.4683078909813,-3.44314168405402,331.485352234782));
#32428=CARTESIAN_POINT('Ctrl Pts',(68.4605507812066,-3.53835116613823,331.583971006038));
#32429=CARTESIAN_POINT('Ctrl Pts',(68.4527895262805,-3.63361152512546,331.682642476012));
#32430=CARTESIAN_POINT('Ctrl Pts',(68.4450282713543,-3.72466582474512,331.785223337389));
#32431=CARTESIAN_POINT('Ctrl Pts',(68.4372670164281,-3.81119618669597,331.891307881276));
#32432=CARTESIAN_POINT('Ctrl Pts',(68.4294933460235,-3.89786496902588,331.997562125861));
#32433=CARTESIAN_POINT('Ctrl Pts',(68.4217196756188,-3.97999511807655,332.107330939774));
#32434=CARTESIAN_POINT('Ctrl Pts',(68.4139460052141,-4.05731135389337,332.220178487732));
#32435=CARTESIAN_POINT('Ctrl Pts',(68.406534201037,-4.13102850033182,332.327772955183));
#32436=CARTESIAN_POINT('Ctrl Pts',(68.3991223968599,-4.20036966987215,332.438165733265));
#32437=CARTESIAN_POINT('Ctrl Pts',(68.3917105926828,-4.26513587592794,332.550959571103));
#32438=CARTESIAN_POINT('Ctrl Pts',(68.3836106157741,-4.33591550811773,332.674226114593));
#32439=CARTESIAN_POINT('Ctrl Pts',(68.3755106388654,-4.401439174065,332.800722637179));
#32440=CARTESIAN_POINT('Ctrl Pts',(68.3674106619567,-4.46141296734486,332.929981305083));
#32441=CARTESIAN_POINT('Ctrl Pts',(68.359323648681,-4.52129077538237,333.059033100552));
#32442=CARTESIAN_POINT('Ctrl Pts',(68.3512366354052,-4.57563626180767,333.19083792405));
#32443=CARTESIAN_POINT('Ctrl Pts',(68.3431496221295,-4.62420032361822,333.324901665708));
#32444=CARTESIAN_POINT('Ctrl Pts',(68.3350791102444,-4.67266529142197,333.458691852955));
#32445=CARTESIAN_POINT('Ctrl Pts',(68.3270085983591,-4.71537223973322,333.594731445541));
#32446=CARTESIAN_POINT('Ctrl Pts',(68.3189380864739,-4.75211955942271,333.732505323304));
#32447=CARTESIAN_POINT('Ctrl Pts',(68.3108772009443,-4.78882304759698,333.870114866965));
#32448=CARTESIAN_POINT('Ctrl Pts',(68.3028163154146,-4.81958097740674,334.009454244478));
#32449=CARTESIAN_POINT('Ctrl Pts',(68.294755429885,-4.84424064846224,334.149990822234));
#32450=CARTESIAN_POINT('Ctrl Pts',(68.2867065378168,-4.86886362940282,334.290318301371));
#32451=CARTESIAN_POINT('Ctrl Pts',(68.2786576457488,-4.88740638320064,334.431839091039));
#32452=CARTESIAN_POINT('Ctrl Pts',(68.2706087536806,-4.89976675740206,334.574008467739));
#32453=CARTESIAN_POINT('Ctrl Pts',(68.2625845852838,-4.91208916441178,334.715741144718));
#32454=CARTESIAN_POINT('Ctrl Pts',(68.2545604168869,-4.91826706186341,334.858118091645));
#32455=CARTESIAN_POINT('Ctrl Pts',(68.24653624849,-4.91824996458602,335.000590211503));
#32456=CARTESIAN_POINT('',(71.7465372896154,-4.92216623067323,335.00168803465));
#32457=CARTESIAN_POINT('Ctrl Pts',(71.7465362484899,-4.91824970447095,335.001704984294));
#32458=CARTESIAN_POINT('Ctrl Pts',(71.7412131669834,-4.91821730456371,335.095166745058));
#32459=CARTESIAN_POINT('Ctrl Pts',(71.7358900854768,-4.91552100689044,335.18857910669));
#32460=CARTESIAN_POINT('Ctrl Pts',(71.7305670039701,-4.9101680900388,335.281837524231));
#32461=CARTESIAN_POINT('Ctrl Pts',(71.7227919251917,-4.9023494327133,335.418054026315));
#32462=CARTESIAN_POINT('Ctrl Pts',(71.7150168464133,-4.88884580562974,335.554160175694));
#32463=CARTESIAN_POINT('Ctrl Pts',(71.7072417676348,-4.86965866961016,335.689643026493));
#32464=CARTESIAN_POINT('Ctrl Pts',(71.6994762565858,-4.85049514458297,335.824959157019));
#32465=CARTESIAN_POINT('Ctrl Pts',(71.6917107455368,-4.82566208079924,335.959653131777));
#32466=CARTESIAN_POINT('Ctrl Pts',(71.6839452344878,-4.79521290228959,336.093213741322));
#32467=CARTESIAN_POINT('Ctrl Pts',(71.6761874229656,-4.76479391422907,336.226641925134));
#32468=CARTESIAN_POINT('Ctrl Pts',(71.6684296114434,-4.72876997918441,336.358938601386));
#32469=CARTESIAN_POINT('Ctrl Pts',(71.6606717999212,-4.68724605727273,336.4895997654));
#32470=CARTESIAN_POINT('Ctrl Pts',(71.6529198263981,-4.64575338342915,336.620162602745));
#32471=CARTESIAN_POINT('Ctrl Pts',(71.6451678528751,-4.59876907893377,336.749092006634));
#32472=CARTESIAN_POINT('Ctrl Pts',(71.6374158793521,-4.54644862793027,336.875896568602));
#32473=CARTESIAN_POINT('Ctrl Pts',(71.6296671887945,-4.49415033466883,337.002647428762));
#32474=CARTESIAN_POINT('Ctrl Pts',(71.6219184982369,-4.43652053837923,337.127274876208));
#32475=CARTESIAN_POINT('Ctrl Pts',(71.6141698076792,-4.37376371961623,337.249305223279));
#32476=CARTESIAN_POINT('Ctrl Pts',(71.6064227293014,-4.31101995793353,337.371310180916));
#32477=CARTESIAN_POINT('Ctrl Pts',(71.5986756509236,-4.2431514742083,337.490718765585));
#32478=CARTESIAN_POINT('Ctrl Pts',(71.5909285725458,-4.17040961691579,337.607080108021));
#32479=CARTESIAN_POINT('Ctrl Pts',(71.58318142924,-4.09766714997654,337.723442425676));
#32480=CARTESIAN_POINT('Ctrl Pts',(71.5754342859342,-4.02005143520023,337.836757118717));
#32481=CARTESIAN_POINT('Ctrl Pts',(71.5676871426284,-3.9378580187657,337.94660097172));
#32482=CARTESIAN_POINT('Ctrl Pts',(71.5599382576003,-3.85564612350614,338.056469519954));
#32483=CARTESIAN_POINT('Ctrl Pts',(71.5521893725722,-3.76885471279912,338.162865362505));
#32484=CARTESIAN_POINT('Ctrl Pts',(71.5444404875441,-3.67782035017689,338.265397454266));
#32485=CARTESIAN_POINT('Ctrl Pts',(71.5366833777694,-3.58668936274155,338.368038374648));
#32486=CARTESIAN_POINT('Ctrl Pts',(71.5289262679946,-3.49130668712623,338.466807059305));
#32487=CARTESIAN_POINT('Ctrl Pts',(71.5211691582199,-3.3920469585192,338.561348128687));
#32488=CARTESIAN_POINT('Ctrl Pts',(71.5134079032938,-3.29273418868691,338.655939717793));
#32489=CARTESIAN_POINT('Ctrl Pts',(71.5056466483676,-3.18954053159051,338.746298932791));
#32490=CARTESIAN_POINT('Ctrl Pts',(71.4978853934414,-3.08287383435791,338.832110643488));
#32491=CARTESIAN_POINT('Ctrl Pts',(71.4901117230368,-2.97603650517234,338.918059624955));
#32492=CARTESIAN_POINT('Ctrl Pts',(71.4823380526321,-2.86571534856039,338.999446333297));
#32493=CARTESIAN_POINT('Ctrl Pts',(71.4745643822274,-2.75234804957195,339.075998439219));
#32494=CARTESIAN_POINT('Ctrl Pts',(71.4671525780504,-2.64425802562663,339.148987026193));
#32495=CARTESIAN_POINT('Ctrl Pts',(71.4597407738734,-2.53339931774793,339.217580831547));
#32496=CARTESIAN_POINT('Ctrl Pts',(71.4523289696963,-2.42017051204073,339.28158355695));
#32497=CARTESIAN_POINT('Ctrl Pts',(71.4445538909179,-2.30139202527402,339.34872324658));
#32498=CARTESIAN_POINT('Ctrl Pts',(71.4367788121394,-2.17962987311048,339.411022605677));
#32499=CARTESIAN_POINT('Ctrl Pts',(71.429003733361,-2.05531619321631,339.46820527823));
#32500=CARTESIAN_POINT('Ctrl Pts',(71.421238222312,-1.93115548921944,339.525317583864));
#32501=CARTESIAN_POINT('Ctrl Pts',(71.413472711263,-1.80444985654074,339.577325569219));
#32502=CARTESIAN_POINT('Ctrl Pts',(71.405707200214,-1.67565809291909,339.623997514936));
#32503=CARTESIAN_POINT('Ctrl Pts',(71.3979493886918,-1.54699402670612,339.670623185283));
#32504=CARTESIAN_POINT('Ctrl Pts',(71.3901915771696,-1.41624831091442,339.711923212469));
#32505=CARTESIAN_POINT('Ctrl Pts',(71.3824337656474,-1.28390157377272,339.747713113844));
#32506=CARTESIAN_POINT('Ctrl Pts',(71.3746817921244,-1.15165443174776,339.783476082183));
#32507=CARTESIAN_POINT('Ctrl Pts',(71.3669298186014,-1.0178090423085,339.813737076578));
#32508=CARTESIAN_POINT('Ctrl Pts',(71.3591778450784,-0.882862782708903,
339.838360917646));
#32509=CARTESIAN_POINT('Ctrl Pts',(71.3514291545208,-0.747973672930176,
339.862974330503));
#32510=CARTESIAN_POINT('Ctrl Pts',(71.3436804639632,-0.611985003993076,
339.88195526826));
#32511=CARTESIAN_POINT('Ctrl Pts',(71.3359317734056,-0.475405766120146,
339.895219343404));
#32512=CARTESIAN_POINT('Ctrl Pts',(71.3281846950277,-0.338854944698388,
339.908480658847));
#32513=CARTESIAN_POINT('Ctrl Pts',(71.3204376166499,-0.201714187543178,
339.916027439799));
#32514=CARTESIAN_POINT('Ctrl Pts',(71.3126905382721,-0.0644986593213518,
339.917827059327));
#32515=CARTESIAN_POINT('Ctrl Pts',(71.3049433949663,0.0727180188987628,
339.919626693937));
#32516=CARTESIAN_POINT('Ctrl Pts',(71.2971962516605,0.210009078594723,339.915679065923));
#32517=CARTESIAN_POINT('Ctrl Pts',(71.2894491083546,0.346858691890955,339.906003680223));
#32518=CARTESIAN_POINT('Ctrl Pts',(71.2817002233266,0.483739071885563,339.89632611929));
#32519=CARTESIAN_POINT('Ctrl Pts',(71.2739513382984,0.620177418166119,339.88091826581));
#32520=CARTESIAN_POINT('Ctrl Pts',(71.2662024532703,0.755662758719872,339.85985152629));
#32521=CARTESIAN_POINT('Ctrl Pts',(71.2584453434956,0.891291904813915,339.838762426315));
#32522=CARTESIAN_POINT('Ctrl Pts',(71.2506882337209,1.02596563771167,339.812002502104));
#32523=CARTESIAN_POINT('Ctrl Pts',(71.2429311239462,1.15918237457085,339.779694476113));
#32524=CARTESIAN_POINT('Ctrl Pts',(71.23516986902,1.29247029819477,339.747369185745));
#32525=CARTESIAN_POINT('Ctrl Pts',(71.2274086140938,1.42429929892198,339.709489994));
#32526=CARTESIAN_POINT('Ctrl Pts',(71.2196473591676,1.55418366756549,339.666229333195));
#32527=CARTESIAN_POINT('Ctrl Pts',(71.211873688763,1.68427580886961,339.622899469433));
#32528=CARTESIAN_POINT('Ctrl Pts',(71.2041000183583,1.81241673629315,339.574171073091));
#32529=CARTESIAN_POINT('Ctrl Pts',(71.1963263479537,1.93814058582717,339.52026482986));
#32530=CARTESIAN_POINT('Ctrl Pts',(71.1889145437766,2.05801195991865,339.46886793522));
#32531=CARTESIAN_POINT('Ctrl Pts',(71.1815027395994,2.17568596213188,339.412764526687));
#32532=CARTESIAN_POINT('Ctrl Pts',(71.1740909354223,2.29078182319854,339.352183555527));
#32533=CARTESIAN_POINT('Ctrl Pts',(71.1663158566439,2.41151887526843,339.288633330511));
#32534=CARTESIAN_POINT('Ctrl Pts',(71.1585407778654,2.5298002226781,339.219954697018));
#32535=CARTESIAN_POINT('Ctrl Pts',(71.150765699087,2.64515961727508,339.146361496739));
#32536=CARTESIAN_POINT('Ctrl Pts',(71.143000188038,2.7603770547928,339.072858857577));
#32537=CARTESIAN_POINT('Ctrl Pts',(71.135234676989,2.87267936742943,338.994453893005));
#32538=CARTESIAN_POINT('Ctrl Pts',(71.12746916594,2.98162341565095,338.911407019187));
#32539=CARTESIAN_POINT('Ctrl Pts',(71.1197113544178,3.0904594455314,338.828442486586));
#32540=CARTESIAN_POINT('Ctrl Pts',(71.1119535428956,3.19594352849189,338.740845439344));
#32541=CARTESIAN_POINT('Ctrl Pts',(71.1041957313734,3.29766043362354,338.648920213846));
#32542=CARTESIAN_POINT('Ctrl Pts',(71.0964437578504,3.39930079355852,338.557064164995));
#32543=CARTESIAN_POINT('Ctrl Pts',(71.0886917843274,3.4971793296083,338.460886681992));
#32544=CARTESIAN_POINT('Ctrl Pts',(71.0809398108044,3.59091320717331,338.36073286666));
#32545=CARTESIAN_POINT('Ctrl Pts',(71.0731911202468,3.68460738838553,338.260621466528));
#32546=CARTESIAN_POINT('Ctrl Pts',(71.0654424296892,3.77416013567615,338.156537368174));
#32547=CARTESIAN_POINT('Ctrl Pts',(71.0576937391316,3.85922504196941,338.048862925409));
#32548=CARTESIAN_POINT('Ctrl Pts',(71.0499466607537,3.94427224979843,337.941210885212));
#32549=CARTESIAN_POINT('Ctrl Pts',(71.0421995823759,4.02483323173668,337.829970292958));
#32550=CARTESIAN_POINT('Ctrl Pts',(71.0344525039981,4.10060176593665,337.7155567053));
#32551=CARTESIAN_POINT('Ctrl Pts',(71.0267053606923,4.17637093514987,337.601142158745));
#32552=CARTESIAN_POINT('Ctrl Pts',(71.0189582173865,4.2473473606952,337.483554889638));
#32553=CARTESIAN_POINT('Ctrl Pts',(71.0112110740806,4.31326830062813,337.363239223882));
#32554=CARTESIAN_POINT('Ctrl Pts',(71.0034621890526,4.37920406098791,337.242896508611));
#32555=CARTESIAN_POINT('Ctrl Pts',(70.9957133040245,4.44008188628708,337.119824518819));
#32556=CARTESIAN_POINT('Ctrl Pts',(70.9879644189964,4.49568530750658,336.99449158393));
#32557=CARTESIAN_POINT('Ctrl Pts',(70.9802073092217,4.55134774677189,336.86902561937));
#32558=CARTESIAN_POINT('Ctrl Pts',(70.9724501994469,4.60172444005301,336.741294273764));
#32559=CARTESIAN_POINT('Ctrl Pts',(70.9646930896722,4.64664715202462,336.611785750986));
#32560=CARTESIAN_POINT('Ctrl Pts',(70.956931834746,4.69159386925713,336.482208022995));
#32561=CARTESIAN_POINT('Ctrl Pts',(70.9491705798199,4.73108068544076,336.350851599674));
#32562=CARTESIAN_POINT('Ctrl Pts',(70.9414093248937,4.76498975748128,336.218218237262));
#32563=CARTESIAN_POINT('Ctrl Pts',(70.9336356544891,4.79895307298612,336.085372704696));
#32564=CARTESIAN_POINT('Ctrl Pts',(70.9258619840844,4.82732073348177,335.951246533764));
#32565=CARTESIAN_POINT('Ctrl Pts',(70.9180883136798,4.85002621252508,335.816350905138));
#32566=CARTESIAN_POINT('Ctrl Pts',(70.9106765095027,4.8716747460562,335.687734700479));
#32567=CARTESIAN_POINT('Ctrl Pts',(70.9032647053256,4.88817634763701,335.558419347984));
#32568=CARTESIAN_POINT('Ctrl Pts',(70.8958529011486,4.89951749117312,335.428848943322));
#32569=CARTESIAN_POINT('Ctrl Pts',(70.8880778223701,4.91141449793752,335.292927907157));
#32570=CARTESIAN_POINT('Ctrl Pts',(70.8803027435917,4.91766999390518,335.156296649336));
#32571=CARTESIAN_POINT('Ctrl Pts',(70.8725276648133,4.91821148948509,335.019462969887));
#32572=CARTESIAN_POINT('Ctrl Pts',(70.8647621537643,4.91875231872022,334.882797672991));
#32573=CARTESIAN_POINT('Ctrl Pts',(70.8569966427153,4.91359313658753,334.745930837224));
#32574=CARTESIAN_POINT('Ctrl Pts',(70.8492311316662,4.90271312436751,334.609376034203));
#32575=CARTESIAN_POINT('Ctrl Pts',(70.841473320144,4.89184389971127,334.472956625668));
#32576=CARTESIAN_POINT('Ctrl Pts',(70.8337155086218,4.87526516385015,334.336849021322));
#32577=CARTESIAN_POINT('Ctrl Pts',(70.8259576970996,4.85300813447139,334.201567091576));
#32578=CARTESIAN_POINT('Ctrl Pts',(70.8182057235766,4.83076785421308,334.066386965772));
#32579=CARTESIAN_POINT('Ctrl Pts',(70.8104537500536,4.80285784902508,333.932031661945));
#32580=CARTESIAN_POINT('Ctrl Pts',(70.8027017765306,4.76936114862362,333.799009868276));
#32581=CARTESIAN_POINT('Ctrl Pts',(70.7949530859729,4.73587863409464,333.666044409414));
#32582=CARTESIAN_POINT('Ctrl Pts',(70.7872043954153,4.69681422534648,333.53441171573));
#32583=CARTESIAN_POINT('Ctrl Pts',(70.7794557048577,4.65230199111062,333.404610001909));
#32584=CARTESIAN_POINT('Ctrl Pts',(70.7717086264798,4.60779901801685,333.274835294419));
#32585=CARTESIAN_POINT('Ctrl Pts',(70.763961548102,4.55785060069146,333.146891178562));
#32586=CARTESIAN_POINT('Ctrl Pts',(70.7562144697241,4.50264047537589,333.02126004437));
#32587=CARTESIAN_POINT('Ctrl Pts',(70.7484673264183,4.44742988734638,332.895627857268));
#32588=CARTESIAN_POINT('Ctrl Pts',(70.7407201831125,4.38695766062848,332.772309048342));
#32589=CARTESIAN_POINT('Ctrl Pts',(70.7329730398067,4.32145525361317,332.651765013139));
#32590=CARTESIAN_POINT('Ctrl Pts',(70.7252241547786,4.25593812026611,332.531193877078));
#32591=CARTESIAN_POINT('Ctrl Pts',(70.7174752697505,4.18538874286202,332.413399099466));
#32592=CARTESIAN_POINT('Ctrl Pts',(70.7097263847224,4.11008380579922,332.298816153645));
#32593=CARTESIAN_POINT('Ctrl Pts',(70.7019692749477,4.03469893929813,332.184111588302));
#32594=CARTESIAN_POINT('Ctrl Pts',(70.694212165173,3.95454864509715,332.072625991852));
#32595=CARTESIAN_POINT('Ctrl Pts',(70.6864550553982,3.86995242246284,331.964765032098));
#32596=CARTESIAN_POINT('Ctrl Pts',(70.678693800472,3.78531099431202,331.856846434897));
#32597=CARTESIAN_POINT('Ctrl Pts',(70.6709325455458,3.69621915756468,331.752556630864));
#32598=CARTESIAN_POINT('Ctrl Pts',(70.6631712906197,3.60303507808759,331.652266245866));
#32599=CARTESIAN_POINT('Ctrl Pts',(70.655397620215,3.50970193445195,331.551815428936));
#32600=CARTESIAN_POINT('Ctrl Pts',(70.6476239498103,3.4122637446887,331.455377090778));
#32601=CARTESIAN_POINT('Ctrl Pts',(70.6398502794056,3.31111437025545,331.363283804091));
#32602=CARTESIAN_POINT('Ctrl Pts',(70.6324384752286,3.21467352353712,331.275477482056));
#32603=CARTESIAN_POINT('Ctrl Pts',(70.6250266710515,3.11485944827854,331.191620975891));
#32604=CARTESIAN_POINT('Ctrl Pts',(70.6176148668744,3.01203827425644,331.111965985628));
#32605=CARTESIAN_POINT('Ctrl Pts',(70.6098397880959,2.90417752820712,331.028406867012));
#32606=CARTESIAN_POINT('Ctrl Pts',(70.6020647093175,2.79266659641416,330.949207473491));
#32607=CARTESIAN_POINT('Ctrl Pts',(70.5942896305391,2.67789327047571,330.874703562841));
#32608=CARTESIAN_POINT('Ctrl Pts',(70.58652411949,2.56326118042166,330.800291333995));
#32609=CARTESIAN_POINT('Ctrl Pts',(70.578758608441,2.44537500881328,330.730563302066));
#32610=CARTESIAN_POINT('Ctrl Pts',(70.570993097392,2.32465536277718,330.66581489703));
#32611=CARTESIAN_POINT('Ctrl Pts',(70.5632352858698,2.20405541062159,330.601130690225));
#32612=CARTESIAN_POINT('Ctrl Pts',(70.5554774743476,2.08062791713669,330.541416468338));
#32613=CARTESIAN_POINT('Ctrl Pts',(70.5477196628254,1.95482190059504,330.486924064515));
#32614=CARTESIAN_POINT('Ctrl Pts',(70.5399676893024,1.82911055707046,330.432472667954));
#32615=CARTESIAN_POINT('Ctrl Pts',(70.5322157157794,1.70102461045468,330.383235422544));
#32616=CARTESIAN_POINT('Ctrl Pts',(70.5244637422564,1.57103675963464,330.339417787188));
#32617=CARTESIAN_POINT('Ctrl Pts',(70.5167150516988,1.4411039587466,330.295618708628));
#32618=CARTESIAN_POINT('Ctrl Pts',(70.5089663611411,1.30927122527812,330.257234799712));
#32619=CARTESIAN_POINT('Ctrl Pts',(70.5012176705835,1.1760300708719,330.224422931739));
#32620=CARTESIAN_POINT('Ctrl Pts',(70.4934705922057,1.0428166384007,330.191617890549));
#32621=CARTESIAN_POINT('Ctrl Pts',(70.4857235138278,0.908195747153761,330.164382677758));
#32622=CARTESIAN_POINT('Ctrl Pts',(70.47797643545,0.77267247942467,330.142823834568));
#32623=CARTESIAN_POINT('Ctrl Pts',(70.4702292921442,0.637148075880062,330.121264810694));
#32624=CARTESIAN_POINT('Ctrl Pts',(70.4624821488384,0.500721666789251,330.105382312718));
#32625=CARTESIAN_POINT('Ctrl Pts',(70.4547350055326,0.363906504929608,330.095231389946));
#32626=CARTESIAN_POINT('Ctrl Pts',(70.4469861205045,0.227060584117003,330.085078185031));
#32627=CARTESIAN_POINT('Ctrl Pts',(70.4392372354764,0.0898261263462719,
330.080659148367));
#32628=CARTESIAN_POINT('Ctrl Pts',(70.4314883504483,-0.0472809397553424,
330.081977269752));
#32629=CARTESIAN_POINT('Ctrl Pts',(70.4237312406736,-0.184533532713591,
330.083296790205));
#32630=CARTESIAN_POINT('Ctrl Pts',(70.4159741308988,-0.321658072424833,
330.090365629248));
#32631=CARTESIAN_POINT('Ctrl Pts',(70.4082170211241,-0.458140524791754,
330.10313464326));
#32632=CARTESIAN_POINT('Ctrl Pts',(70.4004557661979,-0.594695909017264,
330.115910480624));
#32633=CARTESIAN_POINT('Ctrl Pts',(70.3926945112718,-0.730608135105816,
330.134392509726));
#32634=CARTESIAN_POINT('Ctrl Pts',(70.3849332563456,-0.865371711759068,
330.15848010817));
#32635=CARTESIAN_POINT('Ctrl Pts',(70.3771595859409,-1.00035086621562,330.182606238921));
#32636=CARTESIAN_POINT('Ctrl Pts',(70.3693859155363,-1.13417731767726,330.212355773038));
#32637=CARTESIAN_POINT('Ctrl Pts',(70.3616122451316,-1.26635825763189,330.247577478188));
#32638=CARTESIAN_POINT('Ctrl Pts',(70.3542004409546,-1.39238614302976,330.281159604489));
#32639=CARTESIAN_POINT('Ctrl Pts',(70.3467886367776,-1.51691799151516,330.319715822643));
#32640=CARTESIAN_POINT('Ctrl Pts',(70.3393768326005,-1.63954400933231,330.363074455637));
#32641=CARTESIAN_POINT('Ctrl Pts',(70.3316017538221,-1.76818029356765,330.408558224394));
#32642=CARTESIAN_POINT('Ctrl Pts',(70.3238266750437,-1.89512571691326,330.459470809625));
#32643=CARTESIAN_POINT('Ctrl Pts',(70.3160515962652,-2.01988807720766,330.515667806902));
#32644=CARTESIAN_POINT('Ctrl Pts',(70.3082860852162,-2.14449690947495,330.571795650196));
#32645=CARTESIAN_POINT('Ctrl Pts',(70.3005205741672,-2.26692767087084,330.633194807822));
#32646=CARTESIAN_POINT('Ctrl Pts',(70.2927550631182,-2.38670431337455,330.699671456386));
#32647=CARTESIAN_POINT('Ctrl Pts',(70.284997251596,-2.50636219698866,330.76608219316));
#32648=CARTESIAN_POINT('Ctrl Pts',(70.2772394400738,-2.62337085911305,330.837560213777));
#32649=CARTESIAN_POINT('Ctrl Pts',(70.2694816285516,-2.73727553833108,330.913864210559));
#32650=CARTESIAN_POINT('Ctrl Pts',(70.2617296550286,-2.85109450066557,330.990110786162));
#32651=CARTESIAN_POINT('Ctrl Pts',(70.2539776815056,-2.96181380604507,331.071175892541));
#32652=CARTESIAN_POINT('Ctrl Pts',(70.2462257079826,-3.06900487520345,331.156773212719));
#32653=CARTESIAN_POINT('Ctrl Pts',(70.238477017425,-3.17615054888047,331.24233428238));
#32654=CARTESIAN_POINT('Ctrl Pts',(70.2307283268674,-3.2797706534131,331.332423504899));
#32655=CARTESIAN_POINT('Ctrl Pts',(70.2229796363098,-3.37946728722723,331.426712449709));
#32656=CARTESIAN_POINT('Ctrl Pts',(70.2152325579319,-3.479143178324,331.520981776918));
#32657=CARTESIAN_POINT('Ctrl Pts',(70.2074854795541,-3.5748969385962,331.619448819981));
#32658=CARTESIAN_POINT('Ctrl Pts',(70.1997384011763,-3.66636564626394,331.72174649998));
#32659=CARTESIAN_POINT('Ctrl Pts',(70.1919912578705,-3.75783512052749,331.824045037332));
#32660=CARTESIAN_POINT('Ctrl Pts',(70.1842441145647,-3.8450192100189,331.930173984273));
#32661=CARTESIAN_POINT('Ctrl Pts',(70.1764969712589,-3.92759387207261,332.039731525933));
#32662=CARTESIAN_POINT('Ctrl Pts',(70.1687480862308,-4.01018709866346,332.149313698453));
#32663=CARTESIAN_POINT('Ctrl Pts',(70.1609992012027,-4.08816860048186,332.262325687458));
#32664=CARTESIAN_POINT('Ctrl Pts',(70.1532503161746,-4.16125666475779,332.378335255509));
#32665=CARTESIAN_POINT('Ctrl Pts',(70.1454932063999,-4.23442230546034,332.494467957314));
#32666=CARTESIAN_POINT('Ctrl Pts',(70.1377360966252,-4.30268392454371,332.613604262597));
#32667=CARTESIAN_POINT('Ctrl Pts',(70.1299789868505,-4.36580467458381,332.735285314685));
#32668=CARTESIAN_POINT('Ctrl Pts',(70.1222177319243,-4.42895915433449,332.857031389236));
#32669=CARTESIAN_POINT('Ctrl Pts',(70.1144564769981,-4.48696712594403,332.98132456616));
#32670=CARTESIAN_POINT('Ctrl Pts',(70.106695222072,-4.53963965458598,333.107685314486));
#32671=CARTESIAN_POINT('Ctrl Pts',(70.0989215516673,-4.59239644210783,333.234248198829));
#32672=CARTESIAN_POINT('Ctrl Pts',(70.0911478812627,-4.63980059603682,333.362884896864));
#32673=CARTESIAN_POINT('Ctrl Pts',(70.083374210858,-4.68171260390408,333.493099154906));
#32674=CARTESIAN_POINT('Ctrl Pts',(70.0759624066808,-4.72167359772205,333.61725190791));
#32675=CARTESIAN_POINT('Ctrl Pts',(70.0685506025037,-4.75664218016783,333.742838378072));
#32676=CARTESIAN_POINT('Ctrl Pts',(70.0611387983266,-4.78654095518772,333.869421056799));
#32677=CARTESIAN_POINT('Ctrl Pts',(70.0503717066871,-4.82997475927267,334.053307094428));
#32678=CARTESIAN_POINT('Ctrl Pts',(70.0396046150477,-4.8628271733437,334.239780564964));
#32679=CARTESIAN_POINT('Ctrl Pts',(70.0288375234083,-4.88485179693977,334.427805990564));
#32680=CARTESIAN_POINT('Ctrl Pts',(70.0180704317688,-4.90687642053583,334.615831416164));
#32681=CARTESIAN_POINT('Ctrl Pts',(70.0073033401294,-4.91807308447629,334.805409443769));
#32682=CARTESIAN_POINT('Ctrl Pts',(69.99653624849,-4.91824791922601,334.995475894668));
#32683=CARTESIAN_POINT('',(73.4965351039332,-4.91545634990101,335.003629922274));
#32684=CARTESIAN_POINT('Ctrl Pts',(73.4965341419554,-4.91310945567289,335.003645225589));
#32685=CARTESIAN_POINT('Ctrl Pts',(73.4643544978415,-4.91696488633254,335.573219306921));
#32686=CARTESIAN_POINT('Ctrl Pts',(73.339428842303,-4.56197822582132,337.779717770033));
#32687=CARTESIAN_POINT('Ctrl Pts',(73.12175717534,-1.29865199811852,340.669034472837));
#32688=CARTESIAN_POINT('Ctrl Pts',(72.8435191410659,4.06443691893726,339.159904013125));
#32689=CARTESIAN_POINT('Ctrl Pts',(72.5652811067921,5.6976520664749,333.83329104065));
#32690=CARTESIAN_POINT('Ctrl Pts',(72.287043072518,2.10221600981517,329.577349659575));
#32691=CARTESIAN_POINT('Ctrl Pts',(72.0141287743647,-3.31668618667384,330.283911562685));
#32692=CARTESIAN_POINT('Ctrl Pts',(71.8339604876357,-4.91872723309669,333.464419225402));
#32693=CARTESIAN_POINT('Ctrl Pts',(71.7465382123315,-4.92563732181515,335.001673012725));
#32694=CARTESIAN_POINT('',(75.2465362485451,-4.91824887921523,334.996679668969));
#32695=CARTESIAN_POINT('Ctrl Pts',(75.24653624849,-4.91824887921589,334.996679669946));
#32696=CARTESIAN_POINT('Ctrl Pts',(75.2387502416897,-4.918342051693,335.134691681902));
#32697=CARTESIAN_POINT('Ctrl Pts',(75.2309642348894,-4.91262172361729,335.272740197146));
#32698=CARTESIAN_POINT('Ctrl Pts',(75.2231782280891,-4.90110537645683,335.410303730626));
#32699=CARTESIAN_POINT('Ctrl Pts',(75.215392118815,-4.88958887772644,335.54786907462));
#32700=CARTESIAN_POINT('Ctrl Pts',(75.2076060095409,-4.87227623934469,335.684949040227));
#32701=CARTESIAN_POINT('Ctrl Pts',(75.1998199002667,-4.84923690881224,335.821026470166));
#32702=CARTESIAN_POINT('Ctrl Pts',(75.1920320670668,-4.82619247713191,335.957134029066));
#32703=CARTESIAN_POINT('Ctrl Pts',(75.184244233867,-4.7974188931302,336.092238230602));
#32704=CARTESIAN_POINT('Ctrl Pts',(75.1764564006671,-4.76303683020181,336.225831642862));
#32705=CARTESIAN_POINT('Ctrl Pts',(75.1686652213274,-4.72863999459062,336.3594824552));
#32706=CARTESIAN_POINT('Ctrl Pts',(75.1608740419877,-4.68862997852826,336.49162081324));
#32707=CARTESIAN_POINT('Ctrl Pts',(75.153082862648,-4.6431773670528,336.621754297231));
#32708=CARTESIAN_POINT('Ctrl Pts',(75.1452818525729,-4.59766740449111,336.752051980735));
#32709=CARTESIAN_POINT('Ctrl Pts',(75.1374808424978,-4.5467012589998,336.880339374289));
#32710=CARTESIAN_POINT('Ctrl Pts',(75.1296798324227,-4.49049797789784,337.00614330819));
#32711=CARTESIAN_POINT('Ctrl Pts',(75.1218733667279,-4.43425539115167,337.132035222803));
#32712=CARTESIAN_POINT('Ctrl Pts',(75.1140669010331,-4.3727685424437,337.255439873238));
#32713=CARTESIAN_POINT('Ctrl Pts',(75.1062604353383,-4.30630210015476,337.37590935953));
#32714=CARTESIAN_POINT('Ctrl Pts',(75.0984414107914,-4.23972872827054,337.496572654201));
#32715=CARTESIAN_POINT('Ctrl Pts',(75.0906223862445,-4.16815996133327,337.614291024703));
#32716=CARTESIAN_POINT('Ctrl Pts',(75.0828033616977,-4.09190377840686,337.728645548758));
#32717=CARTESIAN_POINT('Ctrl Pts',(75.0783433795509,-4.04840714882195,337.793873523505));
#32718=CARTESIAN_POINT('Ctrl Pts',(75.0738833974042,-4.00338618302853,337.858007640782));
#32719=CARTESIAN_POINT('Ctrl Pts',(75.0694234152574,-3.95690367396601,337.920975244239));
#32720=CARTESIAN_POINT('Ctrl Pts',(75.061648336479,-3.87587080031553,338.030746553014));
#32721=CARTESIAN_POINT('Ctrl Pts',(75.0538732577005,-3.79013855083957,338.137316779828));
#32722=CARTESIAN_POINT('Ctrl Pts',(75.0460981789221,-3.6999886407755,338.240257261489));
#32723=CARTESIAN_POINT('Ctrl Pts',(75.0383326678731,-3.6099496659151,338.343071068334));
#32724=CARTESIAN_POINT('Ctrl Pts',(75.0305671568241,-3.51550410202622,338.442263726101));
#32725=CARTESIAN_POINT('Ctrl Pts',(75.0228016457751,-3.41697622082204,338.537436440254));
#32726=CARTESIAN_POINT('Ctrl Pts',(75.0150438342529,-3.31854603029906,338.632514790384));
#32727=CARTESIAN_POINT('Ctrl Pts',(75.0072860227307,-3.21604185679651,338.723580859026));
#32728=CARTESIAN_POINT('Ctrl Pts',(74.9995282112085,-3.10982718066701,338.810270065085));
#32729=CARTESIAN_POINT('Ctrl Pts',(74.9917762376856,-3.00369243445,338.896894034767));
#32730=CARTESIAN_POINT('Ctrl Pts',(74.9840242641626,-2.89385304508389,338.979147451715));
#32731=CARTESIAN_POINT('Ctrl Pts',(74.9762722906396,-2.78070790603495,339.056703908817));
#32732=CARTESIAN_POINT('Ctrl Pts',(74.968523600082,-2.66761068401903,339.134227520715));
#32733=CARTESIAN_POINT('Ctrl Pts',(74.9607749095244,-2.55121081852823,339.207057908543));
#32734=CARTESIAN_POINT('Ctrl Pts',(74.9530262189668,-2.43193853489333,339.274910294381));
#32735=CARTESIAN_POINT('Ctrl Pts',(74.945279140589,-2.31269106685314,339.342748562963));
#32736=CARTESIAN_POINT('Ctrl Pts',(74.9375320622111,-2.19057270893039,339.40561069651));
#32737=CARTESIAN_POINT('Ctrl Pts',(74.9297849838333,-2.06604044875218,339.463256650319));
#32738=CARTESIAN_POINT('Ctrl Pts',(74.9220378405275,-1.94150714487402,339.520903087257));
#32739=CARTESIAN_POINT('Ctrl Pts',(74.9142906972217,-1.81456025310254,339.573333093063));
#32740=CARTESIAN_POINT('Ctrl Pts',(74.9065435539159,-1.6856786435854,339.620353944565));
#32741=CARTESIAN_POINT('Ctrl Pts',(74.8987946688878,-1.55676805874611,339.667385367353));
#32742=CARTESIAN_POINT('Ctrl Pts',(74.8910457838597,-1.4259222577556,339.709005082006));
#32743=CARTESIAN_POINT('Ctrl Pts',(74.8832968988316,-1.29363686081873,339.745069729185));
#32744=CARTESIAN_POINT('Ctrl Pts',(74.8755397890569,-1.16121105479461,339.781172655754));
#32745=CARTESIAN_POINT('Ctrl Pts',(74.8677826792822,-1.02734297820329,339.811708633652));
#32746=CARTESIAN_POINT('Ctrl Pts',(74.8600255695074,-0.892540623744539,
339.836584982967));
#32747=CARTESIAN_POINT('Ctrl Pts',(74.8522643145813,-0.757666235217709,
339.861474625409));
#32748=CARTESIAN_POINT('Ctrl Pts',(74.8445030596551,-0.621856960846329,
339.880698558274));
#32749=CARTESIAN_POINT('Ctrl Pts',(74.836741804729,-0.485626590505696,339.894215961428));
#32750=CARTESIAN_POINT('Ctrl Pts',(74.8289681343243,-0.349178295969892,
339.907754988021));
#32751=CARTESIAN_POINT('Ctrl Pts',(74.8211944639196,-0.212307949824023,
339.91556922099));
#32752=CARTESIAN_POINT('Ctrl Pts',(74.813420793515,-0.0755309189842747,
339.917669991244));
#32753=CARTESIAN_POINT('Ctrl Pts',(74.8060089893378,0.0548791081639752,
339.919672970137));
#32754=CARTESIAN_POINT('Ctrl Pts',(74.7985971851607,0.185204024440773,339.916482446133));
#32755=CARTESIAN_POINT('Ctrl Pts',(74.7911853809836,0.315002774085483,339.908152026457));
#32756=CARTESIAN_POINT('Ctrl Pts',(74.7834103022051,0.451163347100028,339.899413308099));
#32757=CARTESIAN_POINT('Ctrl Pts',(74.7756352234267,0.587175163910888,339.884990495225));
#32758=CARTESIAN_POINT('Ctrl Pts',(74.7678601446483,0.722525300214955,339.864888513938));
#32759=CARTESIAN_POINT('Ctrl Pts',(74.7600946335993,0.85770887955958,339.84481126942));
#32760=CARTESIAN_POINT('Ctrl Pts',(74.7523291225502,0.992232015564157,339.819068818629));
#32761=CARTESIAN_POINT('Ctrl Pts',(74.7445636115012,1.12558387136455,339.787718037962));
#32762=CARTESIAN_POINT('Ctrl Pts',(74.736805799979,1.2588035084115,339.756398341685));
#32763=CARTESIAN_POINT('Ctrl Pts',(74.7290479884569,1.39085379831284,339.719481470468));
#32764=CARTESIAN_POINT('Ctrl Pts',(74.7212901769347,1.5212314569717,339.677075786944));
#32765=CARTESIAN_POINT('Ctrl Pts',(74.7135382034117,1.65151100230764,339.634702015042));
#32766=CARTESIAN_POINT('Ctrl Pts',(74.7057862298887,1.78012005158749,339.586847772814));
#32767=CARTESIAN_POINT('Ctrl Pts',(74.6980342563657,1.90656825796609,339.533671860668));
#32768=CARTESIAN_POINT('Ctrl Pts',(74.6902855658081,2.03296291345448,339.480518468553));
#32769=CARTESIAN_POINT('Ctrl Pts',(74.6825368752504,2.15719818658698,339.42204804024));
#32770=CARTESIAN_POINT('Ctrl Pts',(74.6747881846928,2.27880178192222,339.358468251715));
#32771=CARTESIAN_POINT('Ctrl Pts',(74.667041106315,2.40038007661387,339.294901691496));
#32772=CARTESIAN_POINT('Ctrl Pts',(74.6592940279371,2.51932743644053,339.226228066529));
#32773=CARTESIAN_POINT('Ctrl Pts',(74.6515469495593,2.63519470046314,339.152701765496));
#32774=CARTESIAN_POINT('Ctrl Pts',(74.6437998062535,2.75106293556487,339.079174848242));
#32775=CARTESIAN_POINT('Ctrl Pts',(74.6360526629477,2.86385069334135,339.000795383233));
#32776=CARTESIAN_POINT('Ctrl Pts',(74.6283055196419,2.97313676465028,338.917861769025));
#32777=CARTESIAN_POINT('Ctrl Pts',(74.6205566346138,3.0824474057881,338.834909509579));
#32778=CARTESIAN_POINT('Ctrl Pts',(74.6128077495857,3.18825448260362,338.747401299791));
#32779=CARTESIAN_POINT('Ctrl Pts',(74.6050588645576,3.29016923263935,338.6556763373));
#32780=CARTESIAN_POINT('Ctrl Pts',(74.5973017547829,3.39219215604403,338.563854016985));
#32781=CARTESIAN_POINT('Ctrl Pts',(74.5895446450081,3.49031420890693,338.467806265224));
#32782=CARTESIAN_POINT('Ctrl Pts',(74.5817875352334,3.58418255071518,338.367910109497));
#32783=CARTESIAN_POINT('Ctrl Pts',(74.5740262803072,3.67810105276383,338.267960572458));
#32784=CARTESIAN_POINT('Ctrl Pts',(74.5662650253811,3.76776105913171,338.164158829418));
#32785=CARTESIAN_POINT('Ctrl Pts',(74.5585037704549,3.85285020211303,338.056914847126));
#32786=CARTESIAN_POINT('Ctrl Pts',(74.5507301000503,3.93807545999268,337.949499309413));
#32787=CARTESIAN_POINT('Ctrl Pts',(74.5429564296456,4.0187150131237,337.838630845178));
#32788=CARTESIAN_POINT('Ctrl Pts',(74.535182759241,4.09449949529976,337.724748969261));
#32789=CARTESIAN_POINT('Ctrl Pts',(74.5277709550638,4.16675619159799,337.616168322067));
#32790=CARTESIAN_POINT('Ctrl Pts',(74.5203591508867,4.23459950213563,337.504848743999));
#32791=CARTESIAN_POINT('Ctrl Pts',(74.5129473467096,4.29783582579211,337.391190138203));
#32792=CARTESIAN_POINT('Ctrl Pts',(74.5051722679312,4.36417155004215,337.271960785565));
#32793=CARTESIAN_POINT('Ctrl Pts',(74.4973971891527,4.42564689743183,337.149780535497));
#32794=CARTESIAN_POINT('Ctrl Pts',(74.4896221103743,4.48198843765453,337.025083382785));
#32795=CARTESIAN_POINT('Ctrl Pts',(74.4818565993253,4.5382606460251,336.900539677858));
#32796=CARTESIAN_POINT('Ctrl Pts',(74.4740910882763,4.58941145779213,336.773485585642));
#32797=CARTESIAN_POINT('Ctrl Pts',(74.4663255772273,4.6352122583908,336.644381458836));
#32798=CARTESIAN_POINT('Ctrl Pts',(74.4585677657051,4.68096764736237,336.515405339147));
#32799=CARTESIAN_POINT('Ctrl Pts',(74.4508099541829,4.72138345167913,336.384383595895));
#32800=CARTESIAN_POINT('Ctrl Pts',(74.4430521426607,4.75627843988719,336.251798092651));
#32801=CARTESIAN_POINT('Ctrl Pts',(74.4353001691377,4.79114716850988,336.119312364203));
#32802=CARTESIAN_POINT('Ctrl Pts',(74.4275481956148,4.82050325144547,335.985265594564));
#32803=CARTESIAN_POINT('Ctrl Pts',(74.4197962220918,4.84421487253223,335.850156062872));
#32804=CARTESIAN_POINT('Ctrl Pts',(74.4120475315342,4.86791645173343,335.715103750146));
#32805=CARTESIAN_POINT('Ctrl Pts',(74.4042988409766,4.88597825606357,335.578989954733));
#32806=CARTESIAN_POINT('Ctrl Pts',(74.396550150419,4.89831933852613,335.442324225338));
#32807=CARTESIAN_POINT('Ctrl Pts',(74.3888030720411,4.91065785332343,335.30568693039));
#32808=CARTESIAN_POINT('Ctrl Pts',(74.3810559936633,4.91727797860126,335.16849831892));
#32809=CARTESIAN_POINT('Ctrl Pts',(74.3733089152854,4.91815056847279,335.031273764256));
#32810=CARTESIAN_POINT('Ctrl Pts',(74.3655617719796,4.91902316565747,334.894048059519));
#32811=CARTESIAN_POINT('Ctrl Pts',(74.3578146286739,4.91414812887192,334.756786801854));
#32812=CARTESIAN_POINT('Ctrl Pts',(74.3500674853681,4.90354844739205,334.620005675596));
#32813=CARTESIAN_POINT('Ctrl Pts',(74.34231860034,4.89294638287878,334.483193798038));
#32814=CARTESIAN_POINT('Ctrl Pts',(74.3345697153119,4.87661714283574,334.346862656312));
#32815=CARTESIAN_POINT('Ctrl Pts',(74.3268208302838,4.85463558412194,334.21152272837));
#32816=CARTESIAN_POINT('Ctrl Pts',(74.3190637205091,4.83263069395455,334.07603914923));
#32817=CARTESIAN_POINT('Ctrl Pts',(74.3113066107343,4.80496156345587,333.941549271938));
#32818=CARTESIAN_POINT('Ctrl Pts',(74.3035495009596,4.77175430083064,333.808553838814));
#32819=CARTESIAN_POINT('Ctrl Pts',(74.2957882460335,4.73852929330609,333.675487337183));
#32820=CARTESIAN_POINT('Ctrl Pts',(74.2880269911073,4.69976036720641,333.543917245715));
#32821=CARTESIAN_POINT('Ctrl Pts',(74.2802657361812,4.65562323222839,333.414328097608));
#32822=CARTESIAN_POINT('Ctrl Pts',(74.2724920657765,4.61141549221861,333.284531649097));
#32823=CARTESIAN_POINT('Ctrl Pts',(74.2647183953719,4.56182252466442,333.156722840871));
#32824=CARTESIAN_POINT('Ctrl Pts',(74.2569447249672,4.50706815746109,333.031366035419));
#32825=CARTESIAN_POINT('Ctrl Pts',(74.2495329207901,4.45486261922376,332.911844619419));
#32826=CARTESIAN_POINT('Ctrl Pts',(74.2421211166129,4.3979655193077,332.794552321006));
#32827=CARTESIAN_POINT('Ctrl Pts',(74.2347093124358,4.33660837612317,332.679868354029));
#32828=CARTESIAN_POINT('Ctrl Pts',(74.2269342336573,4.27224393657805,332.559563384205));
#32829=CARTESIAN_POINT('Ctrl Pts',(74.2191591548789,4.20276779562158,332.441748709052));
#32830=CARTESIAN_POINT('Ctrl Pts',(74.2113840761004,4.12839693990018,332.326889121431));
#32831=CARTESIAN_POINT('Ctrl Pts',(74.2036185650514,4.05411760225148,332.212170875845));
#32832=CARTESIAN_POINT('Ctrl Pts',(74.1958530540023,3.97495574480711,332.100400807315));
#32833=CARTESIAN_POINT('Ctrl Pts',(74.1880875429533,3.89117477151336,331.992020285966));
#32834=CARTESIAN_POINT('Ctrl Pts',(74.1803297314311,3.80747686729844,331.88374722422));
#32835=CARTESIAN_POINT('Ctrl Pts',(74.1725719199089,3.71916919894507,331.778857328836));
#32836=CARTESIAN_POINT('Ctrl Pts',(74.1648141083867,3.62655890107261,331.67776376524));
#32837=CARTESIAN_POINT('Ctrl Pts',(74.1570621348637,3.53401829538646,331.576746277757));
#32838=CARTESIAN_POINT('Ctrl Pts',(74.1493101613407,3.43718176796271,331.479519722678));
#32839=CARTESIAN_POINT('Ctrl Pts',(74.1415581878177,3.33639699906906,331.386464594458));
#32840=CARTESIAN_POINT('Ctrl Pts',(74.1338094972601,3.23565491258474,331.293448875141));
#32841=CARTESIAN_POINT('Ctrl Pts',(74.1260608067024,3.13096819687038,331.204601333642));
#32842=CARTESIAN_POINT('Ctrl Pts',(74.1183121161448,3.02272153723828,331.12026578606));
#32843=CARTESIAN_POINT('Ctrl Pts',(74.1105650377669,2.91449739922766,331.035947785193));
#32844=CARTESIAN_POINT('Ctrl Pts',(74.1028179593891,2.8027150987018,330.956140151065));
#32845=CARTESIAN_POINT('Ctrl Pts',(74.0950708810112,2.68779225157625,330.881146291155));
#32846=CARTESIAN_POINT('Ctrl Pts',(74.0873237377054,2.57286844128662,330.806151802724));
#32847=CARTESIAN_POINT('Ctrl Pts',(74.0795765943996,2.45480435924134,330.735971382589));
#32848=CARTESIAN_POINT('Ctrl Pts',(74.0718294510938,2.33404609621532,330.670864764963));
#32849=CARTESIAN_POINT('Ctrl Pts',(74.0640805660657,2.21326068416841,330.605743509986));
#32850=CARTESIAN_POINT('Ctrl Pts',(74.0563316810376,2.08978022983497,330.545698512841));
#32851=CARTESIAN_POINT('Ctrl Pts',(74.0485827960095,1.96407451435586,330.490943073706));
#32852=CARTESIAN_POINT('Ctrl Pts',(74.0408256862348,1.8382353735313,330.436129516583));
#32853=CARTESIAN_POINT('Ctrl Pts',(74.0330685764601,1.71016661233389,330.386616889084));
#32854=CARTESIAN_POINT('Ctrl Pts',(74.0253114666853,1.58035756004787,330.342570124532));
#32855=CARTESIAN_POINT('Ctrl Pts',(74.0175502117591,1.4504791419548,330.298499822797));
#32856=CARTESIAN_POINT('Ctrl Pts',(74.009788956833,1.31885895464051,330.25990131387));
#32857=CARTESIAN_POINT('Ctrl Pts',(74.0020277019068,1.18599953900911,330.226889048433));
#32858=CARTESIAN_POINT('Ctrl Pts',(73.9942540315022,1.0529275916114,330.19382397413));
#32859=CARTESIAN_POINT('Ctrl Pts',(73.9864803610975,0.918612837705174,330.166363078767));
#32860=CARTESIAN_POINT('Ctrl Pts',(73.9787066906928,0.783566895731499,330.14456943388));
#32861=CARTESIAN_POINT('Ctrl Pts',(73.9712948865158,0.654807374847598,330.123790288405));
#32862=CARTESIAN_POINT('Ctrl Pts',(73.9638830823387,0.525383493272115,330.108162680669));
#32863=CARTESIAN_POINT('Ctrl Pts',(73.9564712781616,0.395739427918254,330.097697136275));
#32864=CARTESIAN_POINT('Ctrl Pts',(73.9486961993832,0.259741120730986,330.086718644374));
#32865=CARTESIAN_POINT('Ctrl Pts',(73.9409211206048,0.123070720518009,330.081386332583));
#32866=CARTESIAN_POINT('Ctrl Pts',(73.9331460418263,-0.0137634945639107,
330.081769258288));
#32867=CARTESIAN_POINT('Ctrl Pts',(73.9253805307773,-0.150429326432786,
330.082151712779));
#32868=CARTESIAN_POINT('Ctrl Pts',(73.9176150197283,-0.287258184938828,
330.088235410102));
#32869=CARTESIAN_POINT('Ctrl Pts',(73.9098495086793,-0.423736369538326,
330.100037698958));
#32870=CARTESIAN_POINT('Ctrl Pts',(73.9020916971571,-0.560079235619984,
330.111828285811));
#32871=CARTESIAN_POINT('Ctrl Pts',(73.894333885635,-0.696071732813865,330.129326147118));
#32872=CARTESIAN_POINT('Ctrl Pts',(73.8865760741128,-0.831200213334262,
330.152496594343));
#32873=CARTESIAN_POINT('Ctrl Pts',(73.8788241005898,-0.966227005387988,
330.175649605073));
#32874=CARTESIAN_POINT('Ctrl Pts',(73.8710721270668,-1.10039069125888,330.204466639088));
#32875=CARTESIAN_POINT('Ctrl Pts',(73.8633201535439,-1.23318315529974,330.238861232018));
#32876=CARTESIAN_POINT('Ctrl Pts',(73.8555714629862,-1.36591938165324,330.273241258817));
#32877=CARTESIAN_POINT('Ctrl Pts',(73.8478227724287,-1.49728516357397,330.313194048678));
#32878=CARTESIAN_POINT('Ctrl Pts',(73.8400740818711,-1.62678320347397,330.358582170134));
#32879=CARTESIAN_POINT('Ctrl Pts',(73.8323270034932,-1.75625430022562,330.403960848213));
#32880=CARTESIAN_POINT('Ctrl Pts',(73.8245799251154,-1.88385805926641,330.454772479308));
#32881=CARTESIAN_POINT('Ctrl Pts',(73.8168328467375,-2.00911334284012,330.510830072483));
#32882=CARTESIAN_POINT('Ctrl Pts',(73.8090857034317,-2.13436967617367,330.566888135475));
#32883=CARTESIAN_POINT('Ctrl Pts',(73.8013385601259,-2.25727713800847,330.628192088567));
#32884=CARTESIAN_POINT('Ctrl Pts',(73.7935914168201,-2.37737590699044,330.694507361595));
#32885=CARTESIAN_POINT('Ctrl Pts',(73.785842531792,-2.49750167672545,330.760837543704));
#32886=CARTESIAN_POINT('Ctrl Pts',(73.7780936467639,-2.61481715497616,330.832181098757));
#32887=CARTESIAN_POINT('Ctrl Pts',(73.7703447617358,-2.72888874753884,330.908258406735));
#32888=CARTESIAN_POINT('Ctrl Pts',(73.7625876519611,-2.84308141686853,330.984416463954));
#32889=CARTESIAN_POINT('Ctrl Pts',(73.7548305421864,-2.95402299690558,331.065318093699));
#32890=CARTESIAN_POINT('Ctrl Pts',(73.7470734324116,-3.06130998754793,331.150641063419));
#32891=CARTESIAN_POINT('Ctrl Pts',(73.7393121774855,-3.16865430892728,331.236009627005));
#32892=CARTESIAN_POINT('Ctrl Pts',(73.7315509225593,-3.27233985426807,331.325803982548));
#32893=CARTESIAN_POINT('Ctrl Pts',(73.7237896676332,-3.37199842582913,331.419663468512));
#32894=CARTESIAN_POINT('Ctrl Pts',(73.7160159972285,-3.47181641862617,331.513673099065));
#32895=CARTESIAN_POINT('Ctrl Pts',(73.7082423268239,-3.56759429170676,331.611760574918));
#32896=CARTESIAN_POINT('Ctrl Pts',(73.7004686564192,-3.65900214077594,331.713529796834));
#32897=CARTESIAN_POINT('Ctrl Pts',(73.6930568522421,-3.74615493248003,331.810561636987));
#32898=CARTESIAN_POINT('Ctrl Pts',(73.685645048065,-3.8293352098879,331.910939944884));
#32899=CARTESIAN_POINT('Ctrl Pts',(73.6782332438878,-3.90829375218056,332.014296898691));
#32900=CARTESIAN_POINT('Ctrl Pts',(73.6704427153519,-3.99128687533706,332.12293513019));
#32901=CARTESIAN_POINT('Ctrl Pts',(73.662652186816,-4.069880935998,332.235211862015));
#32902=CARTESIAN_POINT('Ctrl Pts',(73.6548616582801,-4.14374063615689,332.350736592416));
#32903=CARTESIAN_POINT('Ctrl Pts',(73.647080635971,-4.21751021058738,332.466120356222));
#32904=CARTESIAN_POINT('Ctrl Pts',(73.6392996136619,-4.28655670949134,332.584743910954));
#32905=CARTESIAN_POINT('Ctrl Pts',(73.6315185913527,-4.35058515732752,332.706183997932));
#32906=CARTESIAN_POINT('Ctrl Pts',(73.6237454044059,-4.41454912956359,332.827501796728));
#32907=CARTESIAN_POINT('Ctrl Pts',(73.615972217459,-4.47350492478126,332.951630143701));
#32908=CARTESIAN_POINT('Ctrl Pts',(73.6081990305121,-4.52720116778406,333.078117420623));
#32909=CARTESIAN_POINT('Ctrl Pts',(73.6004320138054,-4.58085478750822,333.204504293826));
#32910=CARTESIAN_POINT('Ctrl Pts',(73.5926649970986,-4.62925701260594,333.333246014631));
#32911=CARTESIAN_POINT('Ctrl Pts',(73.5848979803918,-4.67220285223906,333.463867333194));
#32912=CARTESIAN_POINT('Ctrl Pts',(73.5771352940564,-4.71512474813176,333.594415826007));
#32913=CARTESIAN_POINT('Ctrl Pts',(73.5693726077209,-4.75259619253078,333.72684146275));
#32914=CARTESIAN_POINT('Ctrl Pts',(73.5616099213855,-4.78446082557265,333.860650329767));
#32915=CARTESIAN_POINT('Ctrl Pts',(73.5538498962635,-4.81631453474276,333.994413324267));
#32916=CARTESIAN_POINT('Ctrl Pts',(73.5460898711415,-4.84256517022996,334.129558227385));
#32917=CARTESIAN_POINT('Ctrl Pts',(73.5383298460195,-4.863106713813,334.265577674245));
#32918=CARTESIAN_POINT('Ctrl Pts',(73.5305691113377,-4.88365013566995,334.401609558427));
#32919=CARTESIAN_POINT('Ctrl Pts',(73.522808376656,-4.89848335773919,334.538515763089));
#32920=CARTESIAN_POINT('Ctrl Pts',(73.5150476419742,-4.90755181097736,334.675780498623));
#32921=CARTESIAN_POINT('Ctrl Pts',(73.5088771774795,-4.91476202637872,334.784917998065));
#32922=CARTESIAN_POINT('Ctrl Pts',(73.5027067129847,-4.91832896017515,334.89428191533));
#32923=CARTESIAN_POINT('Ctrl Pts',(73.49653624849,-4.91824867386945,335.003611714461));
#32924=CARTESIAN_POINT('',(76.9965362484552,-4.91824952845184,334.997846309397));
#32925=CARTESIAN_POINT('Ctrl Pts',(76.9965362484552,-4.91824952845184,334.997846309397));
#32926=CARTESIAN_POINT('Ctrl Pts',(76.9888439017237,-4.91830869035386,335.132950672227));
#32927=CARTESIAN_POINT('Ctrl Pts',(76.9811515549923,-4.91279667151199,335.268281913705));
#32928=CARTESIAN_POINT('Ctrl Pts',(76.9734592082608,-4.90168365733435,335.403336566556));
#32929=CARTESIAN_POINT('Ctrl Pts',(76.9657758500902,-4.89058362879128,335.538233407103));
#32930=CARTESIAN_POINT('Ctrl Pts',(76.9580924919196,-4.87389565485011,335.672853907188));
#32931=CARTESIAN_POINT('Ctrl Pts',(76.9504091337489,-4.85164191001208,335.806693150779));
#32932=CARTESIAN_POINT('Ctrl Pts',(76.942732822733,-4.82940857624697,335.940409637389));
#32933=CARTESIAN_POINT('Ctrl Pts',(76.9350565117171,-4.80161969232445,336.073345901045));
#32934=CARTESIAN_POINT('Ctrl Pts',(76.9273802007013,-4.7683493178205,336.205001180805));
#32935=CARTESIAN_POINT('Ctrl Pts',(76.9195248432096,-4.73430292690824,336.339727260303));
#32936=CARTESIAN_POINT('Ctrl Pts',(76.9116694857179,-4.69451620765234,336.473111436587));
#32937=CARTESIAN_POINT('Ctrl Pts',(76.9038141282262,-4.64912427591835,336.60462660129));
#32938=CARTESIAN_POINT('Ctrl Pts',(76.8961452572008,-4.60480995025813,336.733019591305));
#32939=CARTESIAN_POINT('Ctrl Pts',(76.8884763861754,-4.55515370478375,336.859630918255));
#32940=CARTESIAN_POINT('Ctrl Pts',(76.88080751515,-4.50033184766666,336.983984960472));
#32941=CARTESIAN_POINT('Ctrl Pts',(76.8731394257967,-4.44551557842832,337.108326327538));
#32942=CARTESIAN_POINT('Ctrl Pts',(76.8654713364435,-4.38553490576362,337.230410501663));
#32943=CARTESIAN_POINT('Ctrl Pts',(76.8578032470902,-4.32061407250618,337.349782351402));
#32944=CARTESIAN_POINT('Ctrl Pts',(76.8501341961009,-4.25568509768783,337.469169171269));
#32945=CARTESIAN_POINT('Ctrl Pts',(76.8424651451115,-4.18581492134049,337.585842639204));
#32946=CARTESIAN_POINT('Ctrl Pts',(76.8347960941222,-4.11127322269474,337.699373177398));
#32947=CARTESIAN_POINT('Ctrl Pts',(76.8268007213537,-4.03355973920203,337.817734494166));
#32948=CARTESIAN_POINT('Ctrl Pts',(76.8188053485854,-3.95076867280854,337.932679113518));
#32949=CARTESIAN_POINT('Ctrl Pts',(76.8108099758169,-3.86325422535034,338.043755879306));
#32950=CARTESIAN_POINT('Ctrl Pts',(76.8031295868382,-3.77918747609316,338.150456691447));
#32951=CARTESIAN_POINT('Ctrl Pts',(76.7954491978594,-3.69076274249829,338.253588344619));
#32952=CARTESIAN_POINT('Ctrl Pts',(76.7877688088806,-3.59833303777858,338.352787260136));
#32953=CARTESIAN_POINT('Ctrl Pts',(76.7800832160429,-3.50584070717496,338.452053388026));
#32954=CARTESIAN_POINT('Ctrl Pts',(76.7723976232051,-3.4093382867939,338.547381194029));
#32955=CARTESIAN_POINT('Ctrl Pts',(76.7647120303674,-3.30921333392912,338.638446120674));
#32956=CARTESIAN_POINT('Ctrl Pts',(76.7570159573274,-3.20895184901355,338.729635224967));
#32957=CARTESIAN_POINT('Ctrl Pts',(76.7493198842875,-3.10505828171344,338.816549598504));
#32958=CARTESIAN_POINT('Ctrl Pts',(76.7416238112475,-2.99795082777614,338.89890675661));
#32959=CARTESIAN_POINT('Ctrl Pts',(76.7406997477987,-2.98509049202248,338.908795337339));
#32960=CARTESIAN_POINT('Ctrl Pts',(76.7397756843499,-2.97218385344695,338.918618271675));
#32961=CARTESIAN_POINT('Ctrl Pts',(76.7388516209011,-2.9592316603781,338.928375114817));
#32962=CARTESIAN_POINT('Ctrl Pts',(76.7310765421227,-2.85025178286683,339.010469287204));
#32963=CARTESIAN_POINT('Ctrl Pts',(76.7233014633442,-2.73768095754818,339.088154814366));
#32964=CARTESIAN_POINT('Ctrl Pts',(76.7155263845658,-2.62191147708508,339.161101208674));
#32965=CARTESIAN_POINT('Ctrl Pts',(76.7077608735168,-2.50628445833817,339.2339578378));
#32966=CARTESIAN_POINT('Ctrl Pts',(76.6999953624678,-2.3874669437934,339.302086731307));
#32967=CARTESIAN_POINT('Ctrl Pts',(76.6922298514188,-2.26588349377321,339.365198169058));
#32968=CARTESIAN_POINT('Ctrl Pts',(76.6844720398966,-2.14442059409745,339.428247031635));
#32969=CARTESIAN_POINT('Ctrl Pts',(76.6767142283744,-2.02019756122928,339.486288159712));
#32970=CARTESIAN_POINT('Ctrl Pts',(76.6689564168522,-1.89366677500193,339.539075809871));
#32971=CARTESIAN_POINT('Ctrl Pts',(76.6612044433292,-1.76723120720391,339.591823735648));
#32972=CARTESIAN_POINT('Ctrl Pts',(76.6534524698062,-1.63849170206592,339.639325902681));
#32973=CARTESIAN_POINT('Ctrl Pts',(76.6457004962832,-1.5079236913063,339.68138325751));
#32974=CARTESIAN_POINT('Ctrl Pts',(76.6379518057255,-1.37741097617676,339.723422801024));
#32975=CARTESIAN_POINT('Ctrl Pts',(76.6302031151679,-1.24507166687453,339.760021998978));
#32976=CARTESIAN_POINT('Ctrl Pts',(76.6224544246103,-1.11139934968372,339.791030635262));
#32977=CARTESIAN_POINT('Ctrl Pts',(76.6147073462325,-0.977754844134961,
339.822032819941));
#32978=CARTESIAN_POINT('Ctrl Pts',(76.6069602678546,-0.842778262877886,
339.847446668292));
#32979=CARTESIAN_POINT('Ctrl Pts',(76.5992131894768,-0.706976081593008,
339.867172473064));
#32980=CARTESIAN_POINT('Ctrl Pts',(76.591466046171,-0.571172762155234,339.886898443158));
#32981=CARTESIAN_POINT('Ctrl Pts',(76.5837189028652,-0.434544215703492,
339.900936218402));
#32982=CARTESIAN_POINT('Ctrl Pts',(76.5759717595594,-0.297604391943369,
339.909237689132));
#32983=CARTESIAN_POINT('Ctrl Pts',(76.5682228745314,-0.160633781203643,
339.917541026209));
#32984=CARTESIAN_POINT('Ctrl Pts',(76.5604739895033,-0.0233521439814797,
339.920105468879));
#32985=CARTESIAN_POINT('Ctrl Pts',(76.5527251044752,0.113724597793962,339.916934998386));
#32986=CARTESIAN_POINT('Ctrl Pts',(76.5449679947005,0.250946834239485,339.913761162724));
#32987=CARTESIAN_POINT('Ctrl Pts',(76.5372108849257,0.387963349418304,339.904840263406));
#32988=CARTESIAN_POINT('Ctrl Pts',(76.529453775151,0.524260820138937,339.890228384745));
#32989=CARTESIAN_POINT('Ctrl Pts',(76.5216925202248,0.660631123870345,339.875608697963));
#32990=CARTESIAN_POINT('Ctrl Pts',(76.5139312652987,0.796281231155387,339.855292030084));
#32991=CARTESIAN_POINT('Ctrl Pts',(76.5061700103725,0.930707056357455,339.829385824072));
#32992=CARTESIAN_POINT('Ctrl Pts',(76.4983963399678,1.0653479190703,339.803438176573));
#32993=CARTESIAN_POINT('Ctrl Pts',(76.4906226695632,1.198760205553,339.771883213311));
#32994=CARTESIAN_POINT('Ctrl Pts',(76.4828489991585,1.3304531955942,339.734878811209));
#32995=CARTESIAN_POINT('Ctrl Pts',(76.4754371949814,1.45601584526583,339.699596972926));
#32996=CARTESIAN_POINT('Ctrl Pts',(76.4680253908043,1.58001538905194,339.659361709951));
#32997=CARTESIAN_POINT('Ctrl Pts',(76.4606135866272,1.70204439015038,339.614350220395));
#32998=CARTESIAN_POINT('Ctrl Pts',(76.4528385078487,1.83005439609802,339.567132583653));
#32999=CARTESIAN_POINT('Ctrl Pts',(76.4450634290703,1.95630034612933,339.514509471391));
#33000=CARTESIAN_POINT('Ctrl Pts',(76.4372883502919,2.08029203407565,339.45663192506));
#33001=CARTESIAN_POINT('Ctrl Pts',(76.4295228392429,2.20413114235634,339.398825600733));
#33002=CARTESIAN_POINT('Ctrl Pts',(76.4217573281938,2.32572115724088,339.335777871404));
#33003=CARTESIAN_POINT('Ctrl Pts',(76.4139918171448,2.4445886929321,339.267688974713));
#33004=CARTESIAN_POINT('Ctrl Pts',(76.4062340056226,2.5633383711152,339.199667588362));
#33005=CARTESIAN_POINT('Ctrl Pts',(76.3984761941004,2.67937060496968,339.126615174643));
#33006=CARTESIAN_POINT('Ctrl Pts',(76.3907183825783,2.79223393492516,339.048779163545));
#33007=CARTESIAN_POINT('Ctrl Pts',(76.3829664090552,2.90501233164598,338.971001726512));
#33008=CARTESIAN_POINT('Ctrl Pts',(76.3752144355323,3.01462625061978,338.88844807836));
#33009=CARTESIAN_POINT('Ctrl Pts',(76.3674624620093,3.12065102016262,338.801410300515));
#33010=CARTESIAN_POINT('Ctrl Pts',(76.3597137714517,3.22663088815254,338.71440938322));
#33011=CARTESIAN_POINT('Ctrl Pts',(76.351965080894,3.32902432841263,338.622928360766));
#33012=CARTESIAN_POINT('Ctrl Pts',(76.3442163903364,3.42743791315231,338.527301009835));
#33013=CARTESIAN_POINT('Ctrl Pts',(76.3364693119586,3.52583102212385,338.431693554974));
#33014=CARTESIAN_POINT('Ctrl Pts',(76.3287222335807,3.62024564245577,338.331941759784));
#33015=CARTESIAN_POINT('Ctrl Pts',(76.3209751552029,3.71032384514119,338.228417573158));
#33016=CARTESIAN_POINT('Ctrl Pts',(76.3132280118971,3.80040280276851,338.1248925189));
#33017=CARTESIAN_POINT('Ctrl Pts',(76.3054808685913,3.88614501368369,338.017595305018));
#33018=CARTESIAN_POINT('Ctrl Pts',(76.2977337252855,3.9672318937667,337.906932087886));
#33019=CARTESIAN_POINT('Ctrl Pts',(76.2899848402574,4.04833700390194,337.796243991313));
#33020=CARTESIAN_POINT('Ctrl Pts',(76.2822359552293,4.12478446957256,337.682188700873));
#33021=CARTESIAN_POINT('Ctrl Pts',(76.2744870702012,4.19629844373307,337.565202220805));
#33022=CARTESIAN_POINT('Ctrl Pts',(76.2667299604265,4.26788832356468,337.448091570078));
#33023=CARTESIAN_POINT('Ctrl Pts',(76.2589728506517,4.3345340473788,337.328043848843));
#33024=CARTESIAN_POINT('Ctrl Pts',(76.251215740877,4.39600498903616,337.205521071962));
#33025=CARTESIAN_POINT('Ctrl Pts',(76.2434544859508,4.45750877879925,337.082932822827));
#33026=CARTESIAN_POINT('Ctrl Pts',(76.2356932310247,4.51383211599612,336.957867238883));
#33027=CARTESIAN_POINT('Ctrl Pts',(76.2279319760985,4.56479256204452,336.830806360051));
#33028=CARTESIAN_POINT('Ctrl Pts',(76.2201583056939,4.61583452819862,336.703542225221));
#33029=CARTESIAN_POINT('Ctrl Pts',(76.2123846352892,4.66149632980786,336.574276786048));
#33030=CARTESIAN_POINT('Ctrl Pts',(76.2046109648846,4.70164517207886,336.443508135885));
#33031=CARTESIAN_POINT('Ctrl Pts',(76.1971991607075,4.73992507608306,336.318826797849));
#33032=CARTESIAN_POINT('Ctrl Pts',(76.1897873565303,4.77319365330056,336.19277932657));
#33033=CARTESIAN_POINT('Ctrl Pts',(76.1823755523532,4.80137942597151,336.065804236414));
#33034=CARTESIAN_POINT('Ctrl Pts',(76.1746004735748,4.83094666732211,335.93260571885));
#33035=CARTESIAN_POINT('Ctrl Pts',(76.1668253947963,4.85501369710965,335.797965420571));
#33036=CARTESIAN_POINT('Ctrl Pts',(76.1590503160179,4.87344225062529,335.662377303597));
#33037=CARTESIAN_POINT('Ctrl Pts',(76.1512848049688,4.89184812663258,335.526956036433));
#33038=CARTESIAN_POINT('Ctrl Pts',(76.1435192939198,4.90462927986278,335.390589654889));
#33039=CARTESIAN_POINT('Ctrl Pts',(76.1357537828708,4.9116979182029,335.25378459926));
#33040=CARTESIAN_POINT('Ctrl Pts',(76.1279959713486,4.91875954796753,335.117115186241));
#33041=CARTESIAN_POINT('Ctrl Pts',(76.1202381598264,4.92011991443344,334.980008352543));
#33042=CARTESIAN_POINT('Ctrl Pts',(76.1124803483042,4.91574277607731,334.842977638714));
#33043=CARTESIAN_POINT('Ctrl Pts',(76.1047283747811,4.91136893165659,334.706050044843));
#33044=CARTESIAN_POINT('Ctrl Pts',(76.0969764012581,4.90126618892265,334.569198845924));
#33045=CARTESIAN_POINT('Ctrl Pts',(76.089224427735,4.88545035116212,334.432939219457));
#33046=CARTESIAN_POINT('Ctrl Pts',(76.0814757371774,4.86964121141834,334.296737299023));
#33047=CARTESIAN_POINT('Ctrl Pts',(76.0737270466198,4.84812383383427,334.16112684021));
#33048=CARTESIAN_POINT('Ctrl Pts',(76.0659783560622,4.82096599198929,334.026619310556));
#33049=CARTESIAN_POINT('Ctrl Pts',(76.0582312776844,4.79381380056013,333.892139766316));
#33050=CARTESIAN_POINT('Ctrl Pts',(76.0504841993065,4.76102355644561,333.758763077698));
#33051=CARTESIAN_POINT('Ctrl Pts',(76.0427371209287,4.72271434347904,333.626991517726));
#33052=CARTESIAN_POINT('Ctrl Pts',(76.0349899776229,4.68440480944441,333.495218853381));
#33053=CARTESIAN_POINT('Ctrl Pts',(76.0272428343171,4.64057632341896,333.365051719848));
#33054=CARTESIAN_POINT('Ctrl Pts',(76.0194956910113,4.59139802681291,333.236977815829));
#33055=CARTESIAN_POINT('Ctrl Pts',(76.0117468059832,4.54220867388169,333.108875118077));
#33056=CARTESIAN_POINT('Ctrl Pts',(76.0039979209551,4.48766725711725,332.982866951112));
#33057=CARTESIAN_POINT('Ctrl Pts',(75.996249035927,4.42799114511993,332.859421227509));
#33058=CARTESIAN_POINT('Ctrl Pts',(75.9884919261522,4.36825169228073,332.735844477339));
#33059=CARTESIAN_POINT('Ctrl Pts',(75.9807348163775,4.30336682767488,332.614835956063));
#33060=CARTESIAN_POINT('Ctrl Pts',(75.9729777066028,4.2336002644193,332.496839624872));
#33061=CARTESIAN_POINT('Ctrl Pts',(75.9652164516766,4.16379642014307,332.378780240215));
#33062=CARTESIAN_POINT('Ctrl Pts',(75.9574551967504,4.08910589203741,332.263736580627));
#33063=CARTESIAN_POINT('Ctrl Pts',(75.9496939418243,4.0098353097686,332.152122922064));
#33064=CARTESIAN_POINT('Ctrl Pts',(75.9419202714196,3.93043792040227,332.040330718022));
#33065=CARTESIAN_POINT('Ctrl Pts',(75.934146601015,3.84644607576806,331.93197978851));
#33066=CARTESIAN_POINT('Ctrl Pts',(75.9263729306103,3.75820677031242,331.8274513504));
#33067=CARTESIAN_POINT('Ctrl Pts',(75.9189611264333,3.67407502575632,331.727788736234));
#33068=CARTESIAN_POINT('Ctrl Pts',(75.9115493222563,3.58608255413759,331.631600960588));
#33069=CARTESIAN_POINT('Ctrl Pts',(75.9041375180794,3.49455943082387,331.539185435921));
#33070=CARTESIAN_POINT('Ctrl Pts',(75.8963624393009,3.39855048660167,331.442240351097));
#33071=CARTESIAN_POINT('Ctrl Pts',(75.8885873605225,3.29835263813812,331.349140281244));
#33072=CARTESIAN_POINT('Ctrl Pts',(75.8808122817441,3.19430644566673,331.260268807298));
#33073=CARTESIAN_POINT('Ctrl Pts',(75.8730467706951,3.09038828865901,331.171506695358));
#33074=CARTESIAN_POINT('Ctrl Pts',(75.865281259646,2.98263150456502,331.086963077178));
#33075=CARTESIAN_POINT('Ctrl Pts',(75.857515748597,2.87141446048222,331.006985842921));
#33076=CARTESIAN_POINT('Ctrl Pts',(75.8497579370748,2.76030768842282,330.927087906325));
#33077=CARTESIAN_POINT('Ctrl Pts',(75.8420001255527,2.64574779927336,330.85174757024));
#33078=CARTESIAN_POINT('Ctrl Pts',(75.8342423140305,2.52814702786863,330.781273217192));
#33079=CARTESIAN_POINT('Ctrl Pts',(75.8264903405075,2.41063475477339,330.71085189833));
#33080=CARTESIAN_POINT('Ctrl Pts',(75.8187383669845,2.29008648822242,330.645289473973));
#33081=CARTESIAN_POINT('Ctrl Pts',(75.8109863934614,2.16694400403005,330.584851446905));
#33082=CARTESIAN_POINT('Ctrl Pts',(75.8032377029038,2.04385367075301,330.524439015377));
#33083=CARTESIAN_POINT('Ctrl Pts',(75.7954890123462,1.91817165513783,330.469146836651));
#33084=CARTESIAN_POINT('Ctrl Pts',(75.7877403217886,1.79036473732038,330.419194702909));
#33085=CARTESIAN_POINT('Ctrl Pts',(75.7799932434108,1.66258441079965,330.369252962125));
#33086=CARTESIAN_POINT('Ctrl Pts',(75.772246165033,1.53268042527964,330.324649198586));
#33087=CARTESIAN_POINT('Ctrl Pts',(75.7644990866551,1.40113959595773,330.285555080909));
#33088=CARTESIAN_POINT('Ctrl Pts',(75.7567519433493,1.26959766419688,330.246460635586));
#33089=CARTESIAN_POINT('Ctrl Pts',(75.7490048000435,1.13641923594893,330.212876039581));
#33090=CARTESIAN_POINT('Ctrl Pts',(75.7412576567377,1.00210595957867,330.184922980026));
#33091=CARTESIAN_POINT('Ctrl Pts',(75.7335087717096,0.867762486732522,330.15696363603));
#33092=CARTESIAN_POINT('Ctrl Pts',(75.7257598866815,0.732284040667951,330.134638427485));
#33093=CARTESIAN_POINT('Ctrl Pts',(75.7180110016534,0.596181729674974,330.118017778842));
#33094=CARTESIAN_POINT('Ctrl Pts',(75.7102538918787,0.45993495828263,330.101379488871));
#33095=CARTESIAN_POINT('Ctrl Pts',(75.7024967821039,0.323063387806579,330.090457901445));
#33096=CARTESIAN_POINT('Ctrl Pts',(75.6947396723292,0.186083064984924,330.085271507456));
#33097=CARTESIAN_POINT('Ctrl Pts',(75.686978417403,0.0490295442586284,330.080082342023));
#33098=CARTESIAN_POINT('Ctrl Pts',(75.6792171624768,-0.0881324539373592,
330.080634475153));
#33099=CARTESIAN_POINT('Ctrl Pts',(75.6714559075507,-0.224888621207158,
330.086894243907));
#33100=CARTESIAN_POINT('Ctrl Pts',(75.663682237146,-0.361863553775857,330.093164026252));
#33101=CARTESIAN_POINT('Ctrl Pts',(75.6559085667414,-0.498430968550139,
330.105159655158));
#33102=CARTESIAN_POINT('Ctrl Pts',(75.6481348963367,-0.634082513525635,
330.122795633917));
#33103=CARTESIAN_POINT('Ctrl Pts',(75.6407230921596,-0.763419446447297,
330.139610653621));
#33104=CARTESIAN_POINT('Ctrl Pts',(75.6333112879824,-0.891923574466551,
330.161552675588));
#33105=CARTESIAN_POINT('Ctrl Pts',(75.6258994838053,-1.01916617438121,330.188505079344));
#33106=CARTESIAN_POINT('Ctrl Pts',(75.6181244050268,-1.15264531315326,330.216778500696));
#33107=CARTESIAN_POINT('Ctrl Pts',(75.6103493262484,-1.28515795325081,330.250655219218));
#33108=CARTESIAN_POINT('Ctrl Pts',(75.6025742474699,-1.4161972365976,330.290056428199));
#33109=CARTESIAN_POINT('Ctrl Pts',(75.5948087364209,-1.54707526776422,330.329409151484));
#33110=CARTESIAN_POINT('Ctrl Pts',(75.5870432253718,-1.67648317890724,330.37427272721));
#33111=CARTESIAN_POINT('Ctrl Pts',(75.5792777143228,-1.80392366561939,330.424517241742));
#33112=CARTESIAN_POINT('Ctrl Pts',(75.5715199028006,-1.93123779471751,330.474711938691));
#33113=CARTESIAN_POINT('Ctrl Pts',(75.5637620912784,-2.05658802011141,330.530276814622));
#33114=CARTESIAN_POINT('Ctrl Pts',(75.5560042797562,-2.17949193243152,330.591032095947));
#33115=CARTESIAN_POINT('Ctrl Pts',(75.5482523062331,-2.30230335566078,330.651741656997));
#33116=CARTESIAN_POINT('Ctrl Pts',(75.5405003327101,-2.42267178110516,330.717633676334));
#33117=CARTESIAN_POINT('Ctrl Pts',(75.532748359187,-2.54013487156683,330.788480334042));
#33118=CARTESIAN_POINT('Ctrl Pts',(75.5249996686294,-2.6575482163394,330.859296988148));
#33119=CARTESIAN_POINT('Ctrl Pts',(75.5172509780717,-2.77205833931942,330.935063905814));
#33120=CARTESIAN_POINT('Ctrl Pts',(75.5095022875141,-2.88322781105554,331.015507503827));
#33121=CARTESIAN_POINT('Ctrl Pts',(75.5017552091363,-2.99437415305456,331.095934364878));
#33122=CARTESIAN_POINT('Ctrl Pts',(75.4940081307584,-3.10218090984829,331.181035741868));
#33123=CARTESIAN_POINT('Ctrl Pts',(75.4862610523806,-3.20624027799651,331.270495161251));
#33124=CARTESIAN_POINT('Ctrl Pts',(75.4785139090748,-3.31030051826226,331.35995533039));
#33125=CARTESIAN_POINT('Ctrl Pts',(75.470766765769,-3.41061301083981,331.453773359959));
#33126=CARTESIAN_POINT('Ctrl Pts',(75.4630196224632,-3.50680395570985,331.551593255035));
#33127=CARTESIAN_POINT('Ctrl Pts',(75.4552707374351,-3.60301652634654,331.649435142101));
#33128=CARTESIAN_POINT('Ctrl Pts',(75.447521852407,-3.69510543141647,331.751280406339));
#33129=CARTESIAN_POINT('Ctrl Pts',(75.4397729673789,-3.78273485947376,331.856737356596));
#33130=CARTESIAN_POINT('Ctrl Pts',(75.4320158576041,-3.87045729831131,331.962306239948));
#33131=CARTESIAN_POINT('Ctrl Pts',(75.4242587478294,-3.95371055465251,332.071494165952));
#33132=CARTESIAN_POINT('Ctrl Pts',(75.4165016380547,-4.03219981661281,332.183877186377));
#33133=CARTESIAN_POINT('Ctrl Pts',(75.4087403831285,-4.11073102072511,332.296320260695));
#33134=CARTESIAN_POINT('Ctrl Pts',(75.4009791282023,-4.18449294777455,332.411961502119));
#33135=CARTESIAN_POINT('Ctrl Pts',(75.3932178732762,-4.25323558385935,332.530350200799));
#33136=CARTESIAN_POINT('Ctrl Pts',(75.3854442028715,-4.32208818575875,332.648928282815));
#33137=CARTESIAN_POINT('Ctrl Pts',(75.3776705324668,-4.38590526986643,332.770262258547));
#33138=CARTESIAN_POINT('Ctrl Pts',(75.3698968620621,-4.44448363375122,332.893878376775));
#33139=CARTESIAN_POINT('Ctrl Pts',(75.3624850578852,-4.50033516070281,333.011740134956));
#33140=CARTESIAN_POINT('Ctrl Pts',(75.3550732537083,-4.55142460355379,333.131676084838));
#33141=CARTESIAN_POINT('Ctrl Pts',(75.3476614495313,-4.59761802422218,333.253262593906));
#33142=CARTESIAN_POINT('Ctrl Pts',(75.3387749079294,-4.65300261678632,333.399041346997));
#33143=CARTESIAN_POINT('Ctrl Pts',(75.3298883663275,-4.7014951093337,333.547575031307));
#33144=CARTESIAN_POINT('Ctrl Pts',(75.3210018247256,-4.74284895472082,333.698244702256));
#33145=CARTESIAN_POINT('Ctrl Pts',(75.3121462132614,-4.78405886558402,333.848389958435));
#33146=CARTESIAN_POINT('Ctrl Pts',(75.3032906017973,-4.81817963094701,334.000656207855));
#33147=CARTESIAN_POINT('Ctrl Pts',(75.2944349903331,-4.84501377317844,334.154408727451));
#33148=CARTESIAN_POINT('Ctrl Pts',(75.2856386784745,-4.87166822662651,334.307131677965));
#33149=CARTESIAN_POINT('Ctrl Pts',(75.2768423666159,-4.89113323208053,334.46132089513));
#33150=CARTESIAN_POINT('Ctrl Pts',(75.2680460547573,-4.90326258944528,334.616334727339));
#33151=CARTESIAN_POINT('Ctrl Pts',(75.2608761193532,-4.91314931358559,334.742687587667));
#33152=CARTESIAN_POINT('Ctrl Pts',(75.2537061839492,-4.91816307902829,334.869587921416));
#33153=CARTESIAN_POINT('Ctrl Pts',(75.2465362485452,-4.91824887921523,334.996679668969));
#33154=CARTESIAN_POINT('',(78.7465362485187,-4.9182479660083,335.004472958214));
#33155=CARTESIAN_POINT('Ctrl Pts',(78.74653624849,-4.91824796600784,335.004472958721));
#33156=CARTESIAN_POINT('Ctrl Pts',(78.7357876945031,-4.91807550825578,335.194099119235));
#33157=CARTESIAN_POINT('Ctrl Pts',(78.7250391405163,-4.90693287809721,335.383246192589));
#33158=CARTESIAN_POINT('Ctrl Pts',(78.7142905865295,-4.88500627415459,335.570873684777));
#33159=CARTESIAN_POINT('Ctrl Pts',(78.7050330112925,-4.86612120496873,335.732474550118));
#33160=CARTESIAN_POINT('Ctrl Pts',(78.6957754360556,-4.83923724108489,335.892949057504));
#33161=CARTESIAN_POINT('Ctrl Pts',(78.6865178608187,-4.80449992880622,336.051647990823));
#33162=CARTESIAN_POINT('Ctrl Pts',(78.6787427820402,-4.77532540603914,336.184933076498));
#33163=CARTESIAN_POINT('Ctrl Pts',(78.6709677032617,-4.7405542433559,336.317213831293));
#33164=CARTESIAN_POINT('Ctrl Pts',(78.6631926244833,-4.70026866985679,336.447983941093));
#33165=CARTESIAN_POINT('Ctrl Pts',(78.6554271134343,-4.66003267032059,336.578593129947));
#33166=CARTESIAN_POINT('Ctrl Pts',(78.6476616023853,-4.61429587580899,336.707695002594));
#33167=CARTESIAN_POINT('Ctrl Pts',(78.6398960913363,-4.56319155663783,336.834793143635));
#33168=CARTESIAN_POINT('Ctrl Pts',(78.632138279814,-4.51213790754781,336.961765266499));
#33169=CARTESIAN_POINT('Ctrl Pts',(78.6243804682918,-4.45572746959211,337.086737251092));
#33170=CARTESIAN_POINT('Ctrl Pts',(78.6166226567696,-4.39414327127363,337.209227913553));
#33171=CARTESIAN_POINT('Ctrl Pts',(78.6088706832466,-4.33260541701741,337.331626397905));
#33172=CARTESIAN_POINT('Ctrl Pts',(78.6011187097236,-4.26590172692788,337.451546929027));
#33173=CARTESIAN_POINT('Ctrl Pts',(78.5933667362005,-4.19426313913914,337.568528719356));
#33174=CARTESIAN_POINT('Ctrl Pts',(78.5856180456429,-4.12265489033486,337.685460967828));
#33175=CARTESIAN_POINT('Ctrl Pts',(78.5778693550853,-4.04611610426616,337.799456618204));
#33176=CARTESIAN_POINT('Ctrl Pts',(78.5701206645277,-3.96492331304977,337.910080099264));
#33177=CARTESIAN_POINT('Ctrl Pts',(78.5623735861498,-3.88374741467179,338.020680564186));
#33178=CARTESIAN_POINT('Ctrl Pts',(78.554626507772,-3.79791966830381,338.127909940428));
#33179=CARTESIAN_POINT('Ctrl Pts',(78.5468794293942,-3.70775929527203,338.231362571861));
#33180=CARTESIAN_POINT('Ctrl Pts',(78.5391322860883,-3.61759816660949,338.334816070327));
#33181=CARTESIAN_POINT('Ctrl Pts',(78.5313851427826,-3.52310459566713,338.434492466179));
#33182=CARTESIAN_POINT('Ctrl Pts',(78.5236379994767,-3.42463709452955,338.530020372926));
#33183=CARTESIAN_POINT('Ctrl Pts',(78.5158891144486,-3.32614745580719,338.625569756375));
#33184=CARTESIAN_POINT('Ctrl Pts',(78.5081402294205,-3.22368238956685,338.716968522696));
#33185=CARTESIAN_POINT('Ctrl Pts',(78.5003913443924,-3.11763584666953,338.80388351426));
#33186=CARTESIAN_POINT('Ctrl Pts',(78.4926342346176,-3.01147674487592,338.890890758294));
#33187=CARTESIAN_POINT('Ctrl Pts',(78.4848771248429,-2.90172887552791,338.973404472609));
#33188=CARTESIAN_POINT('Ctrl Pts',(78.4771200150681,-2.78881816884506,339.05113271612));
#33189=CARTESIAN_POINT('Ctrl Pts',(78.469358760142,-2.67584712629082,339.128902495119));
#33190=CARTESIAN_POINT('Ctrl Pts',(78.4615975052158,-2.55971020947508,339.201881499995));
#33191=CARTESIAN_POINT('Ctrl Pts',(78.4538362502896,-2.44085980698392,339.269822767417));
#33192=CARTESIAN_POINT('Ctrl Pts',(78.446062579885,-2.32181928258195,339.337872718724));
#33193=CARTESIAN_POINT('Ctrl Pts',(78.4382889094803,-2.20005694586107,339.400868649127));
#33194=CARTESIAN_POINT('Ctrl Pts',(78.4305152390756,-2.07604791000877,339.458610561357));
#33195=CARTESIAN_POINT('Ctrl Pts',(78.4231034348987,-1.95781152461267,339.51366457368));
#33196=CARTESIAN_POINT('Ctrl Pts',(78.4156916307217,-1.83753316611684,339.563942597932));
#33197=CARTESIAN_POINT('Ctrl Pts',(78.4082798265448,-1.7156373622172,339.609313561027));
#33198=CARTESIAN_POINT('Ctrl Pts',(78.4005047477663,-1.5877670818572,339.656908290176));
#33199=CARTESIAN_POINT('Ctrl Pts',(78.3927296689879,-1.45771270176755,339.699253184353));
#33200=CARTESIAN_POINT('Ctrl Pts',(78.3849545902095,-1.32594449117312,339.736143396143));
#33201=CARTESIAN_POINT('Ctrl Pts',(78.3771890791605,-1.19433842975042,339.772988212178));
#33202=CARTESIAN_POINT('Ctrl Pts',(78.3694235681114,-1.06102310688679,339.804391597075));
#33203=CARTESIAN_POINT('Ctrl Pts',(78.3616580570624,-0.926488089097307,
339.830196981828));
#33204=CARTESIAN_POINT('Ctrl Pts',(78.3539002455402,-0.792086463169742,
339.855976780467));
#33205=CARTESIAN_POINT('Ctrl Pts',(78.346142434018,-0.656467930357041,339.87616955148));
#33206=CARTESIAN_POINT('Ctrl Pts',(78.3383846224959,-0.520136175659759,
339.890668811244));
#33207=CARTESIAN_POINT('Ctrl Pts',(78.3306326489728,-0.383907014931307,
339.905157159854));
#33208=CARTESIAN_POINT('Ctrl Pts',(78.3228806754498,-0.246966087754619,
339.913960484225));
#33209=CARTESIAN_POINT('Ctrl Pts',(78.3151287019268,-0.109825854096218,
339.917023626572));
#33210=CARTESIAN_POINT('Ctrl Pts',(78.3073800113692,0.0272563005918082,
339.920085471677));
#33211=CARTESIAN_POINT('Ctrl Pts',(78.2996313208116,0.164537203919587,339.917411961076));
#33212=CARTESIAN_POINT('Ctrl Pts',(78.291882630254,0.301500927360121,339.908999923946));
#33213=CARTESIAN_POINT('Ctrl Pts',(78.2841355518761,0.438436154354049,339.90058963701));
#33214=CARTESIAN_POINT('Ctrl Pts',(78.2763884734983,0.575053942829135,339.88644322234));
#33215=CARTESIAN_POINT('Ctrl Pts',(78.2686413951205,0.710840418914877,339.86660959615));
#33216=CARTESIAN_POINT('Ctrl Pts',(78.2608942518146,0.846628033022075,339.846775803735));
#33217=CARTESIAN_POINT('Ctrl Pts',(78.2531471085088,0.98158393407312,339.821254761223));
#33218=CARTESIAN_POINT('Ctrl Pts',(78.245399965203,1.11520180378499,339.790146970536));
#33219=CARTESIAN_POINT('Ctrl Pts',(78.2376510801749,1.24884971363066,339.759032186157));
#33220=CARTESIAN_POINT('Ctrl Pts',(78.2299021951468,1.38115861292424,339.722328242876));
#33221=CARTESIAN_POINT('Ctrl Pts',(78.2221533101188,1.51163515289127,339.680186131667));
#33222=CARTESIAN_POINT('Ctrl Pts',(78.214396200344,1.64225018200598,339.637999290385));
#33223=CARTESIAN_POINT('Ctrl Pts',(78.2066390905693,1.77102859416182,339.590362871134));
#33224=CARTESIAN_POINT('Ctrl Pts',(78.1988819807946,1.89749439459063,339.53747706165));
#33225=CARTESIAN_POINT('Ctrl Pts',(78.1911207258684,2.0240277742996,339.48456299168));
#33226=CARTESIAN_POINT('Ctrl Pts',(78.1833594709422,2.14824572606224,339.42639410773));
#33227=CARTESIAN_POINT('Ctrl Pts',(78.175598216016,2.26969575972321,339.363217186984));
#33228=CARTESIAN_POINT('Ctrl Pts',(78.1678245456114,2.39134007385748,339.299939203755));
#33229=CARTESIAN_POINT('Ctrl Pts',(78.1600508752067,2.51020728281326,339.231637369767));
#33230=CARTESIAN_POINT('Ctrl Pts',(78.1522772048021,2.62587209361402,339.158602987841));
#33231=CARTESIAN_POINT('Ctrl Pts',(78.144865400625,2.73615267964465,339.088968373964));
#33232=CARTESIAN_POINT('Ctrl Pts',(78.1374535964479,2.84352206422753,339.015032060152));
#33233=CARTESIAN_POINT('Ctrl Pts',(78.1300417922708,2.94764028891242,338.937080109635));
#33234=CARTESIAN_POINT('Ctrl Pts',(78.1222667134924,3.05686165794124,338.855307501815));
#33235=CARTESIAN_POINT('Ctrl Pts',(78.114491634714,3.16285027042858,338.768857250998));
#33236=CARTESIAN_POINT('Ctrl Pts',(78.1067165559355,3.2651793761515,338.678013961917));
#33237=CARTESIAN_POINT('Ctrl Pts',(78.0989510448865,3.36738255939524,338.587282461286));
#33238=CARTESIAN_POINT('Ctrl Pts',(78.0911855338376,3.46593490654975,338.492168935626));
#33239=CARTESIAN_POINT('Ctrl Pts',(78.0834200227886,3.56043982286565,338.393000343391));
#33240=CARTESIAN_POINT('Ctrl Pts',(78.0756622112664,3.65485103728194,338.293930077104));
#33241=CARTESIAN_POINT('Ctrl Pts',(78.0679043997442,3.74522253911589,338.190813026624));
#33242=CARTESIAN_POINT('Ctrl Pts',(78.060146588222,3.83119221115989,338.084015127013));
#33243=CARTESIAN_POINT('Ctrl Pts',(78.052394614699,3.91709718829931,337.97729759621));
#33244=CARTESIAN_POINT('Ctrl Pts',(78.044642641176,3.99860668493804,337.866905032992));
#33245=CARTESIAN_POINT('Ctrl Pts',(78.036890667653,4.0753969962245,337.753238526838));
#33246=CARTESIAN_POINT('Ctrl Pts',(78.0291419770954,4.15215478676859,337.639620158516));
#33247=CARTESIAN_POINT('Ctrl Pts',(78.0213932865377,4.22419714863462,337.522730928156));
#33248=CARTESIAN_POINT('Ctrl Pts',(78.0136445959801,4.29124221687945,337.403002975148));
#33249=CARTESIAN_POINT('Ctrl Pts',(78.0058975176023,4.35827333583785,337.283299932541));
#33250=CARTESIAN_POINT('Ctrl Pts',(77.9981504392245,4.42030903841195,337.160759682901));
#33251=CARTESIAN_POINT('Ctrl Pts',(77.9904033608466,4.47711237265312,337.035840825098));
#33252=CARTESIAN_POINT('Ctrl Pts',(77.9826562175408,4.53391618296091,336.910920920355));
#33253=CARTESIAN_POINT('Ctrl Pts',(77.9749090742351,4.58548737567217,336.783622723504));
#33254=CARTESIAN_POINT('Ctrl Pts',(77.9671619309293,4.63163646712052,336.654426395745));
#33255=CARTESIAN_POINT('Ctrl Pts',(77.9594130459012,4.67779593386437,336.52520102191));
#33256=CARTESIAN_POINT('Ctrl Pts',(77.9516641608731,4.71853074220597,336.394077036026));
#33257=CARTESIAN_POINT('Ctrl Pts',(77.943915275845,4.7537008843459,336.261551015484));
#33258=CARTESIAN_POINT('Ctrl Pts',(77.9361581660703,4.78890835643812,336.128884330454));
#33259=CARTESIAN_POINT('Ctrl Pts',(77.9284010562956,4.81853926333295,335.994813016472));
#33260=CARTESIAN_POINT('Ctrl Pts',(77.9206439465208,4.8425043590867,335.859845680763));
#33261=CARTESIAN_POINT('Ctrl Pts',(77.9128826915947,4.86648226102134,335.724806222825));
#33262=CARTESIAN_POINT('Ctrl Pts',(77.9051214366685,4.88478826685253,335.588870176279));
#33263=CARTESIAN_POINT('Ctrl Pts',(77.8973601817424,4.89738502839247,335.452551595044));
#33264=CARTESIAN_POINT('Ctrl Pts',(77.8895865113377,4.9100019406456,335.316014948506));
#33265=CARTESIAN_POINT('Ctrl Pts',(77.8818128409331,4.91689133865514,335.179094935046));
#33266=CARTESIAN_POINT('Ctrl Pts',(77.8740391705284,4.91806803474277,335.04230683327));
#33267=CARTESIAN_POINT('Ctrl Pts',(77.8666273663513,4.91918995534444,334.91188625054));
#33268=CARTESIAN_POINT('Ctrl Pts',(77.8592155621741,4.91511906654999,334.78158586255));
#33269=CARTESIAN_POINT('Ctrl Pts',(77.8518037579969,4.90591195400692,334.651846352838));
#33270=CARTESIAN_POINT('Ctrl Pts',(77.8440286792185,4.89625357345165,334.515747923284));
#33271=CARTESIAN_POINT('Ctrl Pts',(77.83625360044,4.88091223304646,334.379836646643));
#33272=CARTESIAN_POINT('Ctrl Pts',(77.8284785216616,4.8598963239511,334.244625402236));
#33273=CARTESIAN_POINT('Ctrl Pts',(77.8207130106126,4.83890627626982,334.109580543874));
#33274=CARTESIAN_POINT('Ctrl Pts',(77.8129474995636,4.81225561336198,333.975234386281));
#33275=CARTESIAN_POINT('Ctrl Pts',(77.8051819885145,4.78000466139165,333.842097370426));
#33276=CARTESIAN_POINT('Ctrl Pts',(77.7974241769924,4.74778568633409,333.70909236031));
#33277=CARTESIAN_POINT('Ctrl Pts',(77.7896663654701,4.70997756383745,333.577294483556));
#33278=CARTESIAN_POINT('Ctrl Pts',(77.7819085539479,4.66669205410366,333.44720628071));
#33279=CARTESIAN_POINT('Ctrl Pts',(77.7741565804249,4.62343911808864,333.317215973363));
#33280=CARTESIAN_POINT('Ctrl Pts',(77.7664046069019,4.57471712220228,333.188933148429));
#33281=CARTESIAN_POINT('Ctrl Pts',(77.7586526333789,4.52068817587236,333.062847068756));
#33282=CARTESIAN_POINT('Ctrl Pts',(77.7509039428213,4.46668211083326,332.936814386612));
#33283=CARTESIAN_POINT('Ctrl Pts',(77.7431552522636,4.4073737190965,332.812976957912));
#33284=CARTESIAN_POINT('Ctrl Pts',(77.735406561706,4.34297386260081,332.69180566432));
#33285=CARTESIAN_POINT('Ctrl Pts',(77.7276594833282,4.27858740503314,332.570659581427));
#33286=CARTESIAN_POINT('Ctrl Pts',(77.7199124049503,4.20911177309933,332.452178875221));
#33287=CARTESIAN_POINT('Ctrl Pts',(77.7121653265725,4.13480438407849,332.336810977812));
#33288=CARTESIAN_POINT('Ctrl Pts',(77.7044181832667,4.06049637229022,332.221442113508));
#33289=CARTESIAN_POINT('Ctrl Pts',(77.6966710399609,3.98135673430004,332.109186438649));
#33290=CARTESIAN_POINT('Ctrl Pts',(77.6889238966551,3.8976867074221,332.000463136868));
#33291=CARTESIAN_POINT('Ctrl Pts',(77.681175011627,3.81399786974586,331.891715391782));
#33292=CARTESIAN_POINT('Ctrl Pts',(77.6734261265989,3.72577685476512,331.786501909754));
#33293=CARTESIAN_POINT('Ctrl Pts',(77.6656772415708,3.63336547874652,331.685209152849));
#33294=CARTESIAN_POINT('Ctrl Pts',(77.6579201317961,3.5408560163385,331.583808882766));
#33295=CARTESIAN_POINT('Ctrl Pts',(77.6501630220213,3.44414757206624,331.486337940004));
#33296=CARTESIAN_POINT('Ctrl Pts',(77.6424059122466,3.34361954849576,331.393146609936));
#33297=CARTESIAN_POINT('Ctrl Pts',(77.6346446573204,3.24303780596375,331.2999054814));
#33298=CARTESIAN_POINT('Ctrl Pts',(77.6268834023942,3.13863271450823,331.210948775761));
#33299=CARTESIAN_POINT('Ctrl Pts',(77.6191221474681,3.03081634178963,331.126586083977));
#33300=CARTESIAN_POINT('Ctrl Pts',(77.6113484770634,2.92282749801196,331.04208843938));
#33301=CARTESIAN_POINT('Ctrl Pts',(77.6035748066587,2.81141678620896,330.962199721863));
#33302=CARTESIAN_POINT('Ctrl Pts',(77.5958011362541,2.69702553095154,330.887186322249));
#33303=CARTESIAN_POINT('Ctrl Pts',(77.588389332077,2.58795921614838,330.815664814435));
#33304=CARTESIAN_POINT('Ctrl Pts',(77.5809775279,2.47618384853801,330.748575095096));
#33305=CARTESIAN_POINT('Ctrl Pts',(77.573565723723,2.36210063005212,330.686108059303));
#33306=CARTESIAN_POINT('Ctrl Pts',(77.5657906449446,2.24242585319067,330.620579328006));
#33307=CARTESIAN_POINT('Ctrl Pts',(77.5580155661661,2.1198330815448,330.559930798069));
#33308=CARTESIAN_POINT('Ctrl Pts',(77.5502404873877,1.99475814721351,330.504432961614));
#33309=CARTESIAN_POINT('Ctrl Pts',(77.5424749763387,1.86983712555165,330.44900341878));
#33310=CARTESIAN_POINT('Ctrl Pts',(77.5347094652897,1.74244037256878,330.398712115132));
#33311=CARTESIAN_POINT('Ctrl Pts',(77.5269439542407,1.61302977491208,330.353784550008));
#33312=CARTESIAN_POINT('Ctrl Pts',(77.5191861427185,1.48374748823964,330.308901530695));
#33313=CARTESIAN_POINT('Ctrl Pts',(77.5114283311963,1.35245569738056,330.269371793832));
#33314=CARTESIAN_POINT('Ctrl Pts',(77.5036705196741,1.21963747925856,330.235373311403));
#33315=CARTESIAN_POINT('Ctrl Pts',(77.495918546151,1.08691921105769,330.201400413911));
#33316=CARTESIAN_POINT('Ctrl Pts',(77.488166572628,0.952677179135595,330.172950582252));
#33317=CARTESIAN_POINT('Ctrl Pts',(77.480414599105,0.817410541770264,330.150152263349));
#33318=CARTESIAN_POINT('Ctrl Pts',(77.4726659085474,0.682201189906165,330.127363599547));
#33319=CARTESIAN_POINT('Ctrl Pts',(77.4649172179898,0.545968480273064,330.110221752988));
#33320=CARTESIAN_POINT('Ctrl Pts',(77.4571685274321,0.409222496802693,330.098804226456));
#33321=CARTESIAN_POINT('Ctrl Pts',(77.4494214490543,0.272504964476309,330.087389075435));
#33322=CARTESIAN_POINT('Ctrl Pts',(77.4416743706765,0.135274760001691,330.081695907976));
#33323=CARTESIAN_POINT('Ctrl Pts',(77.4339272922987,-0.00195255815189377,
330.081750387585));
#33324=CARTESIAN_POINT('Ctrl Pts',(77.4261801489929,-0.139181026402485,
330.081804867652));
#33325=CARTESIAN_POINT('Ctrl Pts',(77.418433005687,-0.276406217409533,330.087607090712));
#33326=CARTESIAN_POINT('Ctrl Pts',(77.4106858623812,-0.413112613915317,
330.0991305842));
#33327=CARTESIAN_POINT('Ctrl Pts',(77.4029369773531,-0.549849744921395,
330.110656668414));
#33328=CARTESIAN_POINT('Ctrl Pts',(77.3951880923251,-0.686067459916694,
330.127906549751));
#33329=CARTESIAN_POINT('Ctrl Pts',(77.387439207297,-0.821255798311222,330.150801924417));
#33330=CARTESIAN_POINT('Ctrl Pts',(77.3796820975222,-0.956587627004879,
330.17372160047));
#33331=CARTESIAN_POINT('Ctrl Pts',(77.3719249877475,-1.09088751054967,330.202298674433));
#33332=CARTESIAN_POINT('Ctrl Pts',(77.3641678779728,-1.22365557000473,330.236403658107));
#33333=CARTESIAN_POINT('Ctrl Pts',(77.3564066230466,-1.35649457646567,330.270526866394));
#33334=CARTESIAN_POINT('Ctrl Pts',(77.3486453681204,-1.48779975379558,330.310183757427));
#33335=CARTESIAN_POINT('Ctrl Pts',(77.3408841131943,-1.61708776689569,330.355195352153));
#33336=CARTESIAN_POINT('Ctrl Pts',(77.3331104427896,-1.74658259868188,330.400278950762));
#33337=CARTESIAN_POINT('Ctrl Pts',(77.325336772385,-1.87405345449498,330.450734226098));
#33338=CARTESIAN_POINT('Ctrl Pts',(77.3175631019803,-1.99903749455962,330.506334218275));
#33339=CARTESIAN_POINT('Ctrl Pts',(77.3101512978032,-2.11820349749059,330.55934601744));
#33340=CARTESIAN_POINT('Ctrl Pts',(77.302739493626,-2.23510873886439,330.617034211946));
#33341=CARTESIAN_POINT('Ctrl Pts',(77.2953276894489,-2.34937557755609,330.679164726805));
#33342=CARTESIAN_POINT('Ctrl Pts',(77.2875526106704,-2.46924297439482,330.744340443275));
#33343=CARTESIAN_POINT('Ctrl Pts',(77.279777531892,-2.58658560020835,330.814610920793));
#33344=CARTESIAN_POINT('Ctrl Pts',(77.2720024531136,-2.70094013864279,330.889756037658));
#33345=CARTESIAN_POINT('Ctrl Pts',(77.2642369420646,-2.81515395653753,330.964808683673));
#33346=CARTESIAN_POINT('Ctrl Pts',(77.2564714310155,-2.92638667975617,331.044723821029));
#33347=CARTESIAN_POINT('Ctrl Pts',(77.2487059199665,-3.03419872772709,331.129235070021));
#33348=CARTESIAN_POINT('Ctrl Pts',(77.2409481084443,-3.14190387973842,331.213662525863));
#33349=CARTESIAN_POINT('Ctrl Pts',(77.2331902969222,-3.24619480035211,331.302676784951));
#33350=CARTESIAN_POINT('Ctrl Pts',(77.2254324854,-3.34666040848534,331.395967928448));
#33351=CARTESIAN_POINT('Ctrl Pts',(77.2176805118769,-3.44705041306257,331.489188867401));
#33352=CARTESIAN_POINT('Ctrl Pts',(77.2099285383539,-3.54362054973467,331.58668001961));
#33353=CARTESIAN_POINT('Ctrl Pts',(77.2021765648309,-3.63599268155756,331.688091142232));
#33354=CARTESIAN_POINT('Ctrl Pts',(77.1944278742732,-3.72832569372784,331.789459317184));
#33355=CARTESIAN_POINT('Ctrl Pts',(77.1866791837157,-3.8164639744186,331.89474387234));
#33356=CARTESIAN_POINT('Ctrl Pts',(77.178930493158,-3.9000663142004,332.003557808444));
#33357=CARTESIAN_POINT('Ctrl Pts',(77.1711834147802,-3.98365125981715,332.112349104899));
#33358=CARTESIAN_POINT('Ctrl Pts',(77.1634363364023,-4.06270190370081,332.224668011934));
#33359=CARTESIAN_POINT('Ctrl Pts',(77.1556892580245,-4.13691766658959,332.340094873429));
#33360=CARTESIAN_POINT('Ctrl Pts',(77.1479421147187,-4.21113405147789,332.455522702312));
#33361=CARTESIAN_POINT('Ctrl Pts',(77.1401949714129,-4.28051526315522,332.57405820883));
#33362=CARTESIAN_POINT('Ctrl Pts',(77.132447828107,-4.34480458699867,332.6952535577));
#33363=CARTESIAN_POINT('Ctrl Pts',(77.124698943079,-4.40910836444697,332.816476153857));
#33364=CARTESIAN_POINT('Ctrl Pts',(77.1169500580509,-4.46831779297572,332.940359437063));
#33365=CARTESIAN_POINT('Ctrl Pts',(77.1092011730228,-4.52222275097801,333.066432195904));
#33366=CARTESIAN_POINT('Ctrl Pts',(77.101444063248,-4.5761849242597,333.192638769674));
#33367=CARTESIAN_POINT('Ctrl Pts',(77.0936869534733,-4.62483122621104,333.321039101383));
#33368=CARTESIAN_POINT('Ctrl Pts',(77.0859298436986,-4.66800003304214,333.451142758671));
#33369=CARTESIAN_POINT('Ctrl Pts',(77.0781685887724,-4.71119190790331,333.581315939193));
#33370=CARTESIAN_POINT('Ctrl Pts',(77.0704073338462,-4.74890034793319,333.713193883333));
#33371=CARTESIAN_POINT('Ctrl Pts',(77.06264607892,-4.78101430008077,333.846273288459));
#33372=CARTESIAN_POINT('Ctrl Pts',(77.0548724085154,-4.81317962408587,333.979565577263));
#33373=CARTESIAN_POINT('Ctrl Pts',(77.0470987381107,-4.83973250099611,334.114062783995));
#33374=CARTESIAN_POINT('Ctrl Pts',(77.039325067706,-4.86061331706203,334.249252875797));
#33375=CARTESIAN_POINT('Ctrl Pts',(77.031913263529,-4.88052212611612,334.378149836299));
#33376=CARTESIAN_POINT('Ctrl Pts',(77.0245014593521,-4.89527502676103,334.507676340026));
#33377=CARTESIAN_POINT('Ctrl Pts',(77.0170896551751,-4.90486449436498,334.637388149094));
#33378=CARTESIAN_POINT('Ctrl Pts',(77.0102385196134,-4.91372856321389,334.757287861317));
#33379=CARTESIAN_POINT('Ctrl Pts',(77.0033873840517,-4.91819683629662,334.877516539856));
#33380=CARTESIAN_POINT('Ctrl Pts',(76.99653624849,-4.91824952845158,334.997846308785));
#33381=CARTESIAN_POINT('',(80.4965362485215,-4.91824999789874,334.999856232645));
#33382=CARTESIAN_POINT('Ctrl Pts',(80.49653624849,-4.91824999789876,334.999856233204));
#33383=CARTESIAN_POINT('Ctrl Pts',(80.4884388234102,-4.91825420074369,335.143635204458));
#33384=CARTESIAN_POINT('Ctrl Pts',(80.4803413983304,-4.91194928860781,335.287298548783));
#33385=CARTESIAN_POINT('Ctrl Pts',(80.4722439732506,-4.89939146504502,335.430286340411));
#33386=CARTESIAN_POINT('Ctrl Pts',(80.4641365277192,-4.88681810134926,335.573451077453));
#33387=CARTESIAN_POINT('Ctrl Pts',(80.4560290821879,-4.86797641677283,335.715938259107));
#33388=CARTESIAN_POINT('Ctrl Pts',(80.4479216366565,-4.84297405980445,335.857196196073));
#33389=CARTESIAN_POINT('Ctrl Pts',(80.4397956744712,-4.81791459977065,335.99877675307));
#33390=CARTESIAN_POINT('Ctrl Pts',(80.4316697122859,-4.7866663951556,336.139122120127));
#33391=CARTESIAN_POINT('Ctrl Pts',(80.4235437501005,-4.74938795704269,336.277692097494));
#33392=CARTESIAN_POINT('Ctrl Pts',(80.4154080949667,-4.71206505182863,336.416427366259));
#33393=CARTESIAN_POINT('Ctrl Pts',(80.4072724398328,-4.6686976604577,336.553382698982));
#33394=CARTESIAN_POINT('Ctrl Pts',(80.3991367846989,-4.61949320795949,336.688036007944));
#33395=CARTESIAN_POINT('Ctrl Pts',(80.3909826162357,-4.57017678682203,336.822995731204));
#33396=CARTESIAN_POINT('Ctrl Pts',(80.3828284477725,-4.51499687380978,336.955642644701));
#33397=CARTESIAN_POINT('Ctrl Pts',(80.3746742793093,-4.45420855474063,337.085475776262));
#33398=CARTESIAN_POINT('Ctrl Pts',(80.3684315416936,-4.4076697166291,337.184874528913));
#33399=CARTESIAN_POINT('Ctrl Pts',(80.362188804078,-4.35784461194631,337.282624521531));
#33400=CARTESIAN_POINT('Ctrl Pts',(80.3559460664624,-4.30486496663268,337.378512283247));
#33401=CARTESIAN_POINT('Ctrl Pts',(80.3481709876839,-4.23888094786888,337.497936636333));
#33402=CARTESIAN_POINT('Ctrl Pts',(80.3403959089054,-4.16781934094549,337.614801857271));
#33403=CARTESIAN_POINT('Ctrl Pts',(80.332620830127,-4.09190339257262,337.728646127359));
#33404=CARTESIAN_POINT('Ctrl Pts',(80.324855319078,-4.01608086360727,337.842350304825));
#33405=CARTESIAN_POINT('Ctrl Pts',(80.317089808029,-3.9354160936803,337.953040606053));
#33406=CARTESIAN_POINT('Ctrl Pts',(80.30932429698,-3.8501784260975,338.060279260086));
#33407=CARTESIAN_POINT('Ctrl Pts',(80.3015664854578,-3.76502527191038,338.167411586682));
#33408=CARTESIAN_POINT('Ctrl Pts',(80.2938086739356,-3.67530848471277,338.271098772671));
#33409=CARTESIAN_POINT('Ctrl Pts',(80.2860508624134,-3.58134075341484,338.370931840075));
#33410=CARTESIAN_POINT('Ctrl Pts',(80.2782988888904,-3.4874437358146,338.470689779929));
#33411=CARTESIAN_POINT('Ctrl Pts',(80.2705469153674,-3.38930240833154,338.566599090717));
#33412=CARTESIAN_POINT('Ctrl Pts',(80.2627949418444,-3.2872695604019,338.658284010264));
#33413=CARTESIAN_POINT('Ctrl Pts',(80.2550462512868,-3.18527992344387,338.749930101193));
#33414=CARTESIAN_POINT('Ctrl Pts',(80.2472975607291,-3.07940233405125,338.83735509843));
#33415=CARTESIAN_POINT('Ctrl Pts',(80.2395488701715,-2.97002608776162,338.920220414787));
#33416=CARTESIAN_POINT('Ctrl Pts',(80.2318017917937,-2.86067259811348,339.003068490323));
#33417=CARTESIAN_POINT('Ctrl Pts',(80.2240547134158,-2.74782221082323,339.081358536079));
#33418=CARTESIAN_POINT('Ctrl Pts',(80.216307635038,-2.63189660306024,339.154792814726));
#33419=CARTESIAN_POINT('Ctrl Pts',(80.2085604917322,-2.51597002372916,339.228227708824));
#33420=CARTESIAN_POINT('Ctrl Pts',(80.2008133484263,-2.39696850271764,339.296806545474));
#33421=CARTESIAN_POINT('Ctrl Pts',(80.1930662051205,-2.27534159938073,339.360275641359));
#33422=CARTESIAN_POINT('Ctrl Pts',(80.1853173200924,-2.1536873517334,339.423759006444));
#33423=CARTESIAN_POINT('Ctrl Pts',(80.1775684350643,-2.02940689370761,339.482130164028));
#33424=CARTESIAN_POINT('Ctrl Pts',(80.1698195500362,-1.90297284548634,339.535182180667));
#33425=CARTESIAN_POINT('Ctrl Pts',(80.1620624402614,-1.77640459886032,339.588290507265));
#33426=CARTESIAN_POINT('Ctrl Pts',(80.1543053304867,-1.64767855685277,339.636068263444));
#33427=CARTESIAN_POINT('Ctrl Pts',(80.146548220712,-1.51728623251546,339.678357142322));
#33428=CARTESIAN_POINT('Ctrl Pts',(80.1387869657858,-1.38682423068908,339.720668619026));
#33429=CARTESIAN_POINT('Ctrl Pts',(80.1310257108596,-1.2546945486543,339.757485269138));
#33430=CARTESIAN_POINT('Ctrl Pts',(80.1232644559335,-1.12140122780007,339.788699442311));
#33431=CARTESIAN_POINT('Ctrl Pts',(80.1154907855288,-0.987894681072749,
339.819963547988));
#33432=CARTESIAN_POINT('Ctrl Pts',(80.1077171151241,-0.85322115998913,339.845607194568));
#33433=CARTESIAN_POINT('Ctrl Pts',(80.0999434447194,-0.717893088456906,
339.865574228809));
#33434=CARTESIAN_POINT('Ctrl Pts',(80.0925316405424,-0.588864571213662,
339.884611792801));
#33435=CARTESIAN_POINT('Ctrl Pts',(80.0851198363654,-0.459241356943298,
339.89848931303));
#33436=CARTESIAN_POINT('Ctrl Pts',(80.0777080321884,-0.329467724227514,
339.907202266179));
#33437=CARTESIAN_POINT('Ctrl Pts',(80.0699329534099,-0.193333499195371,
339.916342267116));
#33438=CARTESIAN_POINT('Ctrl Pts',(80.0621578746315,-0.0566035286780677,
339.919827522596));
#33439=CARTESIAN_POINT('Ctrl Pts',(80.0543827958531,0.0802130225205787,
339.917595848941));
#33440=CARTESIAN_POINT('Ctrl Pts',(80.0466172848041,0.216861212242528,339.915366921502));
#33441=CARTESIAN_POINT('Ctrl Pts',(80.038851773755,0.353595383569523,339.907435068965));
#33442=CARTESIAN_POINT('Ctrl Pts',(80.031086262706,0.489901648447737,339.893789884879));
#33443=CARTESIAN_POINT('Ctrl Pts',(80.0233284511838,0.626072765267665,339.880158230033));
#33444=CARTESIAN_POINT('Ctrl Pts',(80.0155706396617,0.761816433536126,339.860824555563));
#33445=CARTESIAN_POINT('Ctrl Pts',(80.0078128281395,0.896619521033607,339.835830486793));
#33446=CARTESIAN_POINT('Ctrl Pts',(80.0000608546165,1.0313211649328,339.810855226853));
#33447=CARTESIAN_POINT('Ctrl Pts',(79.9923088810934,1.16508325415929,339.780228122162));
#33448=CARTESIAN_POINT('Ctrl Pts',(79.9845569075704,1.29739888767643,339.744042494409));
#33449=CARTESIAN_POINT('Ctrl Pts',(79.9768082170128,1.42965848544431,339.707872191291));
#33450=CARTESIAN_POINT('Ctrl Pts',(79.9690595264552,1.56047246962644,339.666148150021));
#33451=CARTESIAN_POINT('Ctrl Pts',(79.9613108358975,1.68934544488028,339.619014508568));
#33452=CARTESIAN_POINT('Ctrl Pts',(79.9535637575197,1.81819160703517,339.571890673663));
#33453=CARTESIAN_POINT('Ctrl Pts',(79.9458166791419,1.94509719667202,339.519359611473));
#33454=CARTESIAN_POINT('Ctrl Pts',(79.9380696007641,2.06958364640867,339.461614796575));
#33455=CARTESIAN_POINT('Ctrl Pts',(79.9303224574582,2.19407113946175,339.40386949772));
#33456=CARTESIAN_POINT('Ctrl Pts',(79.9225753141524,2.31613909759164,339.34091052348));
#33457=CARTESIAN_POINT('Ctrl Pts',(79.9148281708466,2.43533091072103,339.272978635307));
#33458=CARTESIAN_POINT('Ctrl Pts',(79.9070792858185,2.55454952070028,339.205031474603));
#33459=CARTESIAN_POINT('Ctrl Pts',(79.8993304007905,2.67089035945508,339.132109368747));
#33460=CARTESIAN_POINT('Ctrl Pts',(79.8915815157624,2.78392365033828,339.054497770574));
#33461=CARTESIAN_POINT('Ctrl Pts',(79.8838244059876,2.89707691592442,338.976803794648));
#33462=CARTESIAN_POINT('Ctrl Pts',(79.8760672962129,3.00691529801813,338.89441060503));
#33463=CARTESIAN_POINT('Ctrl Pts',(79.8683101864382,3.11303968706979,338.807645856593));
#33464=CARTESIAN_POINT('Ctrl Pts',(79.860548931512,3.21922078560176,338.720834743849));
#33465=CARTESIAN_POINT('Ctrl Pts',(79.8527876765858,3.32168364467873,338.629647677277));
#33466=CARTESIAN_POINT('Ctrl Pts',(79.8450264216596,3.42006497310803,338.534450260255));
#33467=CARTESIAN_POINT('Ctrl Pts',(79.837252751255,3.51860367960042,338.439100558391));
#33468=CARTESIAN_POINT('Ctrl Pts',(79.8294790808503,3.61304753891622,338.339727969975));
#33469=CARTESIAN_POINT('Ctrl Pts',(79.8217054104457,3.70307202861645,338.236733015461));
#33470=CARTESIAN_POINT('Ctrl Pts',(79.8142936062686,3.78890585666236,338.13853250086));
#33471=CARTESIAN_POINT('Ctrl Pts',(79.8068818020915,3.87072231850769,338.037039497077));
#33472=CARTESIAN_POINT('Ctrl Pts',(79.7994699979144,3.94827718576553,337.932625159625));
#33473=CARTESIAN_POINT('Ctrl Pts',(79.791694919136,4.02963324809187,337.823093164459));
#33474=CARTESIAN_POINT('Ctrl Pts',(79.7839198403575,4.10655650639041,337.710000086969));
#33475=CARTESIAN_POINT('Ctrl Pts',(79.7761447615791,4.17871913078881,337.593740443545));
#33476=CARTESIAN_POINT('Ctrl Pts',(79.7683792505301,4.25079295448369,337.477623865013));
#33477=CARTESIAN_POINT('Ctrl Pts',(79.7606137394811,4.3181175963772,337.358348802712));
#33478=CARTESIAN_POINT('Ctrl Pts',(79.7528482284321,4.38040621114947,337.236341764539));
#33479=CARTESIAN_POINT('Ctrl Pts',(79.7450904169099,4.44263306657881,337.114455696701));
#33480=CARTESIAN_POINT('Ctrl Pts',(79.7373326053877,4.49983365512129,336.989843389468));
#33481=CARTESIAN_POINT('Ctrl Pts',(79.7295747938655,4.55176529511207,336.862958872523));
#33482=CARTESIAN_POINT('Ctrl Pts',(79.7218228203425,4.60365785489695,336.736169840201));
#33483=CARTESIAN_POINT('Ctrl Pts',(79.7140708468195,4.65028921090893,336.60711236195));
#33484=CARTESIAN_POINT('Ctrl Pts',(79.7063188732965,4.69146352611045,336.476263203387));
#33485=CARTESIAN_POINT('Ctrl Pts',(79.6985701827389,4.73262040396502,336.345469459521));
#33486=CARTESIAN_POINT('Ctrl Pts',(79.6908214921813,4.76832472046394,336.212885916572));
#33487=CARTESIAN_POINT('Ctrl Pts',(79.6830728016237,4.79842959745354,336.079007164379));
#33488=CARTESIAN_POINT('Ctrl Pts',(79.6753257232458,4.82852821087205,335.945156266779));
#33489=CARTESIAN_POINT('Ctrl Pts',(79.667578644868,4.85302961636937,335.810011077058));
#33490=CARTESIAN_POINT('Ctrl Pts',(79.6598315664902,4.87183753057354,335.674078732935));
#33491=CARTESIAN_POINT('Ctrl Pts',(79.6520844231844,4.89064560240612,335.538145249568));
#33492=CARTESIAN_POINT('Ctrl Pts',(79.6443372798786,4.90376003419864,335.401424985824));
#33493=CARTESIAN_POINT('Ctrl Pts',(79.6365901365728,4.91113618947991,335.264432204697));
#33494=CARTESIAN_POINT('Ctrl Pts',(79.6288412515447,4.91851400307749,335.127408624684));
#33495=CARTESIAN_POINT('Ctrl Pts',(79.6210923665166,4.92015095202456,334.990112795603));
#33496=CARTESIAN_POINT('Ctrl Pts',(79.6133434814885,4.91605450289538,334.853060600716));
#33497=CARTESIAN_POINT('Ctrl Pts',(79.6055863717138,4.91195370575279,334.715862937213));
#33498=CARTESIAN_POINT('Ctrl Pts',(79.5978292619391,4.90210736589721,334.578909815789));
#33499=CARTESIAN_POINT('Ctrl Pts',(79.5900721521644,4.88657503422405,334.442714169031));
#33500=CARTESIAN_POINT('Ctrl Pts',(79.5823108972382,4.87103440256944,334.306445743675));
#33501=CARTESIAN_POINT('Ctrl Pts',(79.574549642312,4.84980178526318,334.170935985494));
#33502=CARTESIAN_POINT('Ctrl Pts',(79.5667883873859,4.82298802827421,334.036688242767));
#33503=CARTESIAN_POINT('Ctrl Pts',(79.5590147169812,4.79613137801264,333.902225747403));
#33504=CARTESIAN_POINT('Ctrl Pts',(79.5512410465765,4.7636758398557,333.769029681643));
#33505=CARTESIAN_POINT('Ctrl Pts',(79.5434673761719,4.72578260228544,333.637589687929));
#33506=CARTESIAN_POINT('Ctrl Pts',(79.5360555719948,4.68965330404046,333.512268257545));
#33507=CARTESIAN_POINT('Ctrl Pts',(79.5286437678177,4.64858125403317,333.388543361287));
#33508=CARTESIAN_POINT('Ctrl Pts',(79.5212319636405,4.60274639885732,333.266821229559));
#33509=CARTESIAN_POINT('Ctrl Pts',(79.5134568848621,4.55466504089446,333.139133133565));
#33510=CARTESIAN_POINT('Ctrl Pts',(79.5056818060836,4.50119024821905,333.013245571066));
#33511=CARTESIAN_POINT('Ctrl Pts',(79.4979067273052,4.44247637052532,332.889647716654));
#33512=CARTESIAN_POINT('Ctrl Pts',(79.4901412162561,4.38383474399608,332.76620195727));
#33513=CARTESIAN_POINT('Ctrl Pts',(79.4823757052071,4.31996702630035,332.64504064938));
#33514=CARTESIAN_POINT('Ctrl Pts',(79.4746101941581,4.25107664856845,332.526635815231));
#33515=CARTESIAN_POINT('Ctrl Pts',(79.4668523826359,4.18225457584668,332.40834837982));
#33516=CARTESIAN_POINT('Ctrl Pts',(79.4590945711137,4.10841994883713,332.292812314898));
#33517=CARTESIAN_POINT('Ctrl Pts',(79.4513367595915,4.02982324181151,332.180477398165));
#33518=CARTESIAN_POINT('Ctrl Pts',(79.4435847860686,3.95128568130079,332.068227017021));
#33519=CARTESIAN_POINT('Ctrl Pts',(79.4358328125456,3.86799339696418,331.959173308117));
#33520=CARTESIAN_POINT('Ctrl Pts',(79.4280808390226,3.78024133252202,331.853738960227));
#33521=CARTESIAN_POINT('Ctrl Pts',(79.420332148465,3.69252643113077,331.748349263846));
#33522=CARTESIAN_POINT('Ctrl Pts',(79.4125834579074,3.60035575569038,331.646576179652));
#33523=CARTESIAN_POINT('Ctrl Pts',(79.4048347673498,3.50406573314971,331.54881087156));
#33524=CARTESIAN_POINT('Ctrl Pts',(79.3970876889719,3.40779574455252,331.451065904356));
#33525=CARTESIAN_POINT('Ctrl Pts',(79.3893406105941,3.30740838772562,331.357327332971));
#33526=CARTESIAN_POINT('Ctrl Pts',(79.3815935322163,3.20327802113654,331.267950565466));
#33527=CARTESIAN_POINT('Ctrl Pts',(79.3738463889105,3.09914678183477,331.178573048898));
#33528=CARTESIAN_POINT('Ctrl Pts',(79.3660992456047,2.99127276680282,331.093557663701));
#33529=CARTESIAN_POINT('Ctrl Pts',(79.3583521022989,2.88006427540641,331.013220242849));
#33530=CARTESIAN_POINT('Ctrl Pts',(79.3506032172708,2.7688307819798,330.93286476044));
#33531=CARTESIAN_POINT('Ctrl Pts',(79.3428543322426,2.65426163723137,330.857189563999));
#33532=CARTESIAN_POINT('Ctrl Pts',(79.3351054472145,2.53679469899179,330.786467548758));
#33533=CARTESIAN_POINT('Ctrl Pts',(79.3273483374398,2.41920308013039,330.71567046844));
#33534=CARTESIAN_POINT('Ctrl Pts',(79.319591227665,2.29870785907907,330.649837273316));
#33535=CARTESIAN_POINT('Ctrl Pts',(79.3118341178903,2.17577259820048,330.589195463023));
#33536=CARTESIAN_POINT('Ctrl Pts',(79.3040728629641,2.0527716446491,330.528521247685));
#33537=CARTESIAN_POINT('Ctrl Pts',(79.2963116080379,1.92732841046835,330.473044102855));
#33538=CARTESIAN_POINT('Ctrl Pts',(79.2885503531117,1.79992615707916,330.42294320643));
#33539=CARTESIAN_POINT('Ctrl Pts',(79.280776682707,1.67232010160502,330.372762164899));
#33540=CARTESIAN_POINT('Ctrl Pts',(79.2730030123024,1.54274913429885,330.327974685372));
#33541=CARTESIAN_POINT('Ctrl Pts',(79.2652293418977,1.41171223427289,330.288710194638));
#33542=CARTESIAN_POINT('Ctrl Pts',(79.2578175377207,1.2867751334696,330.251273475395));
#33543=CARTESIAN_POINT('Ctrl Pts',(79.2504057335436,1.16050578567972,330.218857197782));
#33544=CARTESIAN_POINT('Ctrl Pts',(79.2429939293666,1.03334317814458,330.191529875451));
#33545=CARTESIAN_POINT('Ctrl Pts',(79.2352188505882,0.899947952415436,330.162863159649));
#33546=CARTESIAN_POINT('Ctrl Pts',(79.2274437718097,0.765148136717748,330.139706270149));
#33547=CARTESIAN_POINT('Ctrl Pts',(79.2196686930313,0.629438615876122,330.122194131441));
#33548=CARTESIAN_POINT('Ctrl Pts',(79.2119031819823,0.493896094239676,330.104703542535));
#33549=CARTESIAN_POINT('Ctrl Pts',(79.2041376709332,0.357446478798141,330.09284393297));
#33550=CARTESIAN_POINT('Ctrl Pts',(79.1963721598842,0.220596791386352,330.086699671491));
#33551=CARTESIAN_POINT('Ctrl Pts',(79.188614348362,0.0838827908378721,330.080561502064));
#33552=CARTESIAN_POINT('Ctrl Pts',(79.1808565368398,-0.0532301043145716,
330.080127420922));
#33553=CARTESIAN_POINT('Ctrl Pts',(79.1730987253176,-0.190228120404908,
330.085430199427));
#33554=CARTESIAN_POINT('Ctrl Pts',(79.1653467517946,-0.327123041143866,
330.090728987423));
#33555=CARTESIAN_POINT('Ctrl Pts',(79.1575947782716,-0.463902865886357,
330.101756026896));
#33556=CARTESIAN_POINT('Ctrl Pts',(79.1498428047485,-0.600052535652913,
330.118492034529));
#33557=CARTESIAN_POINT('Ctrl Pts',(79.1420941141909,-0.736144545953213,
330.135220954453));
#33558=CARTESIAN_POINT('Ctrl Pts',(79.1343454236333,-0.871606544918365,
330.157653986211));
#33559=CARTESIAN_POINT('Ctrl Pts',(79.1265967330757,-1.00592753454227,330.185719902441));
#33560=CARTESIAN_POINT('Ctrl Pts',(79.1188496546978,-1.14022057756231,330.213779979324));
#33561=CARTESIAN_POINT('Ctrl Pts',(79.11110257632,-1.27337270106844,330.247470529656));
#33562=CARTESIAN_POINT('Ctrl Pts',(79.1033554979422,-1.40488244799375,330.28666907911));
#33563=CARTESIAN_POINT('Ctrl Pts',(79.0956083546363,-1.53639329709758,330.325867957086));
#33564=CARTESIAN_POINT('Ctrl Pts',(79.0878612113306,-1.66626136757738,330.370574814605));
#33565=CARTESIAN_POINT('Ctrl Pts',(79.0801140680247,-1.79400011453196,330.420617219367));
#33566=CARTESIAN_POINT('Ctrl Pts',(79.0723651829967,-1.92176757986786,330.470670874723));
#33567=CARTESIAN_POINT('Ctrl Pts',(79.0646162979686,-2.04740440521303,330.526062321731));
#33568=CARTESIAN_POINT('Ctrl Pts',(79.0568674129405,-2.17044415714877,330.586571035669));
#33569=CARTESIAN_POINT('Ctrl Pts',(79.0491103031658,-2.29361450474921,330.647143974181));
#33570=CARTESIAN_POINT('Ctrl Pts',(79.0413531933911,-2.41418192114389,330.712844856826));
#33571=CARTESIAN_POINT('Ctrl Pts',(79.0335960836164,-2.53170423684092,330.783406977231));
#33572=CARTESIAN_POINT('Ctrl Pts',(79.0258348286902,-2.64928935270599,330.854006803778));
#33573=CARTESIAN_POINT('Ctrl Pts',(79.018073573764,-2.76382579929253,330.929472829269));
#33574=CARTESIAN_POINT('Ctrl Pts',(79.0103123188378,-2.87490138160072,331.009495632308));
#33575=CARTESIAN_POINT('Ctrl Pts',(79.0025386484332,-2.98615464864084,331.089646445752));
#33576=CARTESIAN_POINT('Ctrl Pts',(78.9947649780285,-3.09393568086345,331.174368361358));
#33577=CARTESIAN_POINT('Ctrl Pts',(78.9869913076239,-3.19786561429249,331.263311817207));
#33578=CARTESIAN_POINT('Ctrl Pts',(78.9795795034468,-3.29695758431673,331.348114933788));
#33579=CARTESIAN_POINT('Ctrl Pts',(78.9721676992696,-3.39254871315622,331.436755214322));
#33580=CARTESIAN_POINT('Ctrl Pts',(78.9647558950925,-3.48434382503395,331.52890058174));
#33581=CARTESIAN_POINT('Ctrl Pts',(78.9570876850303,-3.57931452093268,331.62423365001));
#33582=CARTESIAN_POINT('Ctrl Pts',(78.9494194749681,-3.67054001882114,331.723638429202));
#33583=CARTESIAN_POINT('Ctrl Pts',(78.9417512649058,-3.75764359407961,331.826784330939));
#33584=CARTESIAN_POINT('Ctrl Pts',(78.9340926753545,-3.84463788948101,331.92980082617));
#33585=CARTESIAN_POINT('Ctrl Pts',(78.9264340858032,-3.92752028986851,332.036548804794));
#33586=CARTESIAN_POINT('Ctrl Pts',(78.9187754962519,-4.00594956814597,332.146659655777));
#33587=CARTESIAN_POINT('Ctrl Pts',(78.9111257385923,-4.084288401716,332.256643526837));
#33588=CARTESIAN_POINT('Ctrl Pts',(78.9034759809327,-4.15818410357815,332.369982224781));
#33589=CARTESIAN_POINT('Ctrl Pts',(78.8958262232731,-4.2273350211452,332.486273347896));
#33590=CARTESIAN_POINT('Ctrl Pts',(78.8881814101921,-4.29644124159077,332.602489303845));
#33591=CARTESIAN_POINT('Ctrl Pts',(78.8805365971111,-4.3608085705587,332.721653546066));
#33592=CARTESIAN_POINT('Ctrl Pts',(78.8728917840301,-4.42017816297547,332.84333403837));
#33593=CARTESIAN_POINT('Ctrl Pts',(78.8652501499995,-4.47952306689786,332.964963930559));
#33594=CARTESIAN_POINT('Ctrl Pts',(78.8576085159689,-4.53387419159026,333.089107630533));
#33595=CARTESIAN_POINT('Ctrl Pts',(78.8499668819382,-4.58301850033601,333.215308293268));
#33596=CARTESIAN_POINT('Ctrl Pts',(78.8423266643605,-4.63215369969497,333.341485563454));
#33597=CARTESIAN_POINT('Ctrl Pts',(78.8346864467829,-4.67608385838579,333.469718662477));
#33598=CARTESIAN_POINT('Ctrl Pts',(78.8270462292052,-4.71464418982511,333.599531069303));
#33599=CARTESIAN_POINT('Ctrl Pts',(78.8194030799807,-4.75321931734449,333.729393286768));
#33600=CARTESIAN_POINT('Ctrl Pts',(78.8117599307562,-4.78642038397138,333.860835637203));
#33601=CARTESIAN_POINT('Ctrl Pts',(78.8041167815318,-4.81413259656113,333.993366797077));
#33602=CARTESIAN_POINT('Ctrl Pts',(78.7964720323509,-4.84185061020636,334.125925699976));
#33603=CARTESIAN_POINT('Ctrl Pts',(78.78882728317,-4.86407741058527,334.259573469868));
#33604=CARTESIAN_POINT('Ctrl Pts',(78.7811825339891,-4.88074962362938,334.393810117256));
#33605=CARTESIAN_POINT('Ctrl Pts',(78.7735309956044,-4.8974366430522,334.52816597849));
#33606=CARTESIAN_POINT('Ctrl Pts',(78.7658794572198,-4.90855918837742,334.663111360645));
#33607=CARTESIAN_POINT('Ctrl Pts',(78.7582279188351,-4.91410588493564,334.798142589581));
#33608=CARTESIAN_POINT('Ctrl Pts',(78.7543306953963,-4.91693103129809,334.86691919945));
#33609=CARTESIAN_POINT('Ctrl Pts',(78.7504334719575,-4.91831049593728,334.935718080277));
#33610=CARTESIAN_POINT('Ctrl Pts',(78.7465362485187,-4.9182479660083,335.004472958214));
#33611=CARTESIAN_POINT('',(82.2465362484434,-4.91824801864532,334.995585298267));
#33612=CARTESIAN_POINT('Ctrl Pts',(82.2465362484433,-4.91824801864532,334.995585298267));
#33613=CARTESIAN_POINT('Ctrl Pts',(82.2388865763238,-4.9183691106983,335.130489259084));
#33614=CARTESIAN_POINT('Ctrl Pts',(82.2312369042042,-4.91293555636551,335.265570211825));
#33615=CARTESIAN_POINT('Ctrl Pts',(82.2235872320846,-4.90193044563438,335.40032607792));
#33616=CARTESIAN_POINT('Ctrl Pts',(82.215943816417,-4.89093433567417,335.534971730977));
#33617=CARTESIAN_POINT('Ctrl Pts',(82.2083004007494,-4.87437576652904,335.669292426584));
#33618=CARTESIAN_POINT('Ctrl Pts',(82.2006569850817,-4.85228989249124,335.802786311373));
#33619=CARTESIAN_POINT('Ctrl Pts',(82.1930173215805,-4.83021486044863,335.936214663774));
#33620=CARTESIAN_POINT('Ctrl Pts',(82.1853776580793,-4.80261798400293,336.068816615716));
#33621=CARTESIAN_POINT('Ctrl Pts',(82.1777379945781,-4.76958619491484,336.200096076061));
#33622=CARTESIAN_POINT('Ctrl Pts',(82.1701001475853,-4.73656225990584,336.33134432165));
#33623=CARTESIAN_POINT('Ctrl Pts',(82.1624623005925,-4.69810607956381,336.461270310194));
#33624=CARTESIAN_POINT('Ctrl Pts',(82.1548244535996,-4.65435545743641,336.589389297287));
#33625=CARTESIAN_POINT('Ctrl Pts',(82.1471866594079,-4.61060513776078,336.717507398683));
#33626=CARTESIAN_POINT('Ctrl Pts',(82.1395488652162,-4.56156057953586,336.843818142103));
#33627=CARTESIAN_POINT('Ctrl Pts',(82.1319110710244,-4.50740892574639,336.967853612086));
#33628=CARTESIAN_POINT('Ctrl Pts',(82.1242715661789,-4.45324514349038,337.091916862571));
#33629=CARTESIAN_POINT('Ctrl Pts',(82.1166320613334,-4.39397215282391,337.213703457217));
#33630=CARTESIAN_POINT('Ctrl Pts',(82.1089925564879,-4.32982429850132,337.33276758521));
#33631=CARTESIAN_POINT('Ctrl Pts',(82.1013451751211,-4.26561030613049,337.451954471308));
#33632=CARTESIAN_POINT('Ctrl Pts',(82.0936977937542,-4.19651160650226,337.568412931346));
#33633=CARTESIAN_POINT('Ctrl Pts',(82.0860504123874,-4.12280752497341,337.681723545506));
#33634=CARTESIAN_POINT('Ctrl Pts',(82.0783987493311,-4.04906217729369,337.795097601104));
#33635=CARTESIAN_POINT('Ctrl Pts',(82.0707470862748,-3.97070654760736,337.905319974378));
#33636=CARTESIAN_POINT('Ctrl Pts',(82.0630954232185,-3.88806115917067,338.012003234568));
#33637=CARTESIAN_POINT('Ctrl Pts',(82.0554323310357,-3.8052923250742,338.118845845275));
#33638=CARTESIAN_POINT('Ctrl Pts',(82.0477692388529,-3.71822119765673,338.222138480551));
#33639=CARTESIAN_POINT('Ctrl Pts',(82.0401061466702,-3.6272064637596,338.321529215852));
#33640=CARTESIAN_POINT('Ctrl Pts',(82.0351955218154,-3.56888285185939,338.385220295571));
#33641=CARTESIAN_POINT('Ctrl Pts',(82.0302848969607,-3.5089405527216,338.447309850742));
#33642=CARTESIAN_POINT('Ctrl Pts',(82.0253742721059,-3.44748098414941,338.507714059958));
#33643=CARTESIAN_POINT('Ctrl Pts',(82.0175991933275,-3.3501709673038,338.603353107756));
#33644=CARTESIAN_POINT('Ctrl Pts',(82.0098241145491,-3.24872437901894,338.695090894784));
#33645=CARTESIAN_POINT('Ctrl Pts',(82.0020490357706,-3.14348693104863,338.782548476467));
#33646=CARTESIAN_POINT('Ctrl Pts',(81.9942835247216,-3.03837898445794,338.869898436029));
#33647=CARTESIAN_POINT('Ctrl Pts',(81.9865180136726,-2.92948975772514,338.952978422756));
#33648=CARTESIAN_POINT('Ctrl Pts',(81.9787525026236,-2.81720228379485,339.031445690404));
#33649=CARTESIAN_POINT('Ctrl Pts',(81.9709946911015,-2.70502614322196,339.109835157528));
#33650=CARTESIAN_POINT('Ctrl Pts',(81.9632368795792,-2.58945877902461,339.183620784692));
#33651=CARTESIAN_POINT('Ctrl Pts',(81.955479068057,-2.47091655500107,339.252499787269));
#33652=CARTESIAN_POINT('Ctrl Pts',(81.947727094534,-2.35246353776014,339.321326956212));
#33653=CARTESIAN_POINT('Ctrl Pts',(81.939975121011,-2.23104045327232,339.385254654509));
#33654=CARTESIAN_POINT('Ctrl Pts',(81.932223147488,-2.10709262426579,339.444023372493));
#33655=CARTESIAN_POINT('Ctrl Pts',(81.9244744569304,-1.98319728723834,339.50276720189));
#33656=CARTESIAN_POINT('Ctrl Pts',(81.9167257663728,-1.85677968476737,339.55635622934));
#33657=CARTESIAN_POINT('Ctrl Pts',(81.9089770758152,-1.72830952401897,339.604576989441));
#33658=CARTESIAN_POINT('Ctrl Pts',(81.9012299974373,-1.59986609256052,339.652787716809));
#33659=CARTESIAN_POINT('Ctrl Pts',(81.8934829190595,-1.46937131797668,339.695632261179));
#33660=CARTESIAN_POINT('Ctrl Pts',(81.8857358406816,-1.33731429046325,339.732945547016));
#33661=CARTESIAN_POINT('Ctrl Pts',(81.8779886973758,-1.20525615618473,339.770259145575));
#33662=CARTESIAN_POINT('Ctrl Pts',(81.87024155407,-1.07163611900863,339.802041286857));
#33663=CARTESIAN_POINT('Ctrl Pts',(81.8624944107642,-0.936957425638541,
339.828177072668));
#33664=CARTESIAN_POINT('Ctrl Pts',(81.854745525736,-0.802248453638783,339.854318734359));
#33665=CARTESIAN_POINT('Ctrl Pts',(81.8469966407079,-0.666480735475762,
339.874811440123));
#33666=CARTESIAN_POINT('Ctrl Pts',(81.8392477556798,-0.53016628429876,339.889591677583));
#33667=CARTESIAN_POINT('Ctrl Pts',(81.8314906459051,-0.393707147555073,
339.90438760294));
#33668=CARTESIAN_POINT('Ctrl Pts',(81.8237335361304,-0.25670050778807,339.913458905834));
#33669=CARTESIAN_POINT('Ctrl Pts',(81.8159764263556,-0.119662614464011,
339.916794069432));
#33670=CARTESIAN_POINT('Ctrl Pts',(81.8082151714295,0.0174485075283376,
339.920131015234));
#33671=CARTESIAN_POINT('Ctrl Pts',(81.8004539165033,0.154590525739848,339.917725720884));
#33672=CARTESIAN_POINT('Ctrl Pts',(81.7926926615771,0.291249633544186,339.909618795127));
#33673=CARTESIAN_POINT('Ctrl Pts',(81.7849189911725,0.428127351384097,339.90149890093));
#33674=CARTESIAN_POINT('Ctrl Pts',(81.7771453207678,0.56452022605252,339.887659188843));
#33675=CARTESIAN_POINT('Ctrl Pts',(81.7693716503631,0.699921107102996,339.868192016173));
#33676=CARTESIAN_POINT('Ctrl Pts',(81.7619598461861,0.829019044564086,339.849631045075));
#33677=CARTESIAN_POINT('Ctrl Pts',(81.7545480420091,0.957214981620196,339.825954791827));
#33678=CARTESIAN_POINT('Ctrl Pts',(81.747136237832,1.08408180987539,339.797285658786));
#33679=CARTESIAN_POINT('Ctrl Pts',(81.7393611590536,1.21716675930101,339.767211366134));
#33680=CARTESIAN_POINT('Ctrl Pts',(81.7315860802752,1.34920959147742,339.731547346251));
#33681=CARTESIAN_POINT('Ctrl Pts',(81.7238110014968,1.47970455936062,339.690379246874));
#33682=CARTESIAN_POINT('Ctrl Pts',(81.7160454904478,1.61003894487804,339.649261807464));
#33683=CARTESIAN_POINT('Ctrl Pts',(81.7082799793987,1.7388288867988,339.602653881602));
#33684=CARTESIAN_POINT('Ctrl Pts',(81.7005144683497,1.86557888138739,339.550692090201));
#33685=CARTESIAN_POINT('Ctrl Pts',(81.6927566568275,1.9922032029874,339.498781819068));
#33686=CARTESIAN_POINT('Ctrl Pts',(81.6849988453054,2.11679124303774,339.441528393669));
#33687=CARTESIAN_POINT('Ctrl Pts',(81.6772410337832,2.23886306514453,339.379118089071));
#33688=CARTESIAN_POINT('Ctrl Pts',(81.6694890602602,2.3608430243339,339.316754750207));
#33689=CARTESIAN_POINT('Ctrl Pts',(81.6617370867372,2.48031018794034,339.249242433732));
#33690=CARTESIAN_POINT('Ctrl Pts',(81.6539851132142,2.59680533906907,339.176815185459));
#33691=CARTESIAN_POINT('Ctrl Pts',(81.6462364226566,2.71325115443222,339.104418610169));
#33692=CARTESIAN_POINT('Ctrl Pts',(81.6384877320989,2.82672712942346,339.027111448941));
#33693=CARTESIAN_POINT('Ctrl Pts',(81.6307390415413,2.93679957093414,338.945173170174));
#33694=CARTESIAN_POINT('Ctrl Pts',(81.6229919631635,3.04684911095401,338.863251939351));
#33695=CARTESIAN_POINT('Ctrl Pts',(81.6152448847857,3.15349621267817,338.776701740797));
#33696=CARTESIAN_POINT('Ctrl Pts',(81.6074978064078,3.25633738580112,338.685844529051));
#33697=CARTESIAN_POINT('Ctrl Pts',(81.599750663102,3.3591794208323,338.594986555833));
#33698=CARTESIAN_POINT('Ctrl Pts',(81.5920035197962,3.45821517071081,338.49982175622));
#33699=CARTESIAN_POINT('Ctrl Pts',(81.5842563764904,3.55307567942612,338.400711143095));
#33700=CARTESIAN_POINT('Ctrl Pts',(81.5765074914623,3.6479575147976,338.3015782478));
#33701=CARTESIAN_POINT('Ctrl Pts',(81.5687586064342,3.73866197091567,338.19849805608));
#33702=CARTESIAN_POINT('Ctrl Pts',(81.5610097214061,3.82485855917157,338.091866760524));
#33703=CARTESIAN_POINT('Ctrl Pts',(81.5532526116314,3.91114663737677,337.985122285409));
#33704=CARTESIAN_POINT('Ctrl Pts',(81.5454955018567,3.99291704372569,337.874819481628));
#33705=CARTESIAN_POINT('Ctrl Pts',(81.5377383920819,4.06988072125754,337.761386241951));
#33706=CARTESIAN_POINT('Ctrl Pts',(81.5299771371558,4.14688552571796,337.647892387177));
#33707=CARTESIAN_POINT('Ctrl Pts',(81.5222158822296,4.21907827764614,337.531265095478));
#33708=CARTESIAN_POINT('Ctrl Pts',(81.5144546273034,4.28621507555429,337.411958413529));
#33709=CARTESIAN_POINT('Ctrl Pts',(81.5066809568987,4.35345927045917,337.29246087977));
#33710=CARTESIAN_POINT('Ctrl Pts',(81.4989072864941,4.41563117201215,337.170275739314));
#33711=CARTESIAN_POINT('Ctrl Pts',(81.4911336160895,4.47253399723777,337.04587944563));
#33712=CARTESIAN_POINT('Ctrl Pts',(81.4837218119123,4.52678798225952,336.927273829344));
#33713=CARTESIAN_POINT('Ctrl Pts',(81.4763100077352,4.57625229321613,336.806658551757));
#33714=CARTESIAN_POINT('Ctrl Pts',(81.4688982035581,4.62079872799927,336.684459016367));
#33715=CARTESIAN_POINT('Ctrl Pts',(81.4611231247796,4.66752851624786,336.556270117735));
#33716=CARTESIAN_POINT('Ctrl Pts',(81.4533480460012,4.70899383417673,336.425932635588));
#33717=CARTESIAN_POINT('Ctrl Pts',(81.4455729672227,4.74499301604917,336.293918212309));
#33718=CARTESIAN_POINT('Ctrl Pts',(81.4378074561737,4.78094789863643,336.162066241182));
#33719=CARTESIAN_POINT('Ctrl Pts',(81.4300419451247,4.81144992698098,336.028541808362));
#33720=CARTESIAN_POINT('Ctrl Pts',(81.4222764340757,4.83634584302084,335.893835526926));
#33721=CARTESIAN_POINT('Ctrl Pts',(81.4145186225535,4.86121707468753,335.75926280716));
#33722=CARTESIAN_POINT('Ctrl Pts',(81.4067608110313,4.88049318515305,335.623510952628));
#33723=CARTESIAN_POINT('Ctrl Pts',(81.3990029995091,4.89407109597274,335.48708435621));
#33724=CARTESIAN_POINT('Ctrl Pts',(81.3912510259861,4.90763878898393,335.350760425132));
#33725=CARTESIAN_POINT('Ctrl Pts',(81.3834990524631,4.91551677900002,335.213763150234));
#33726=CARTESIAN_POINT('Ctrl Pts',(81.3757470789401,4.91765337152596,335.07660535242));
#33727=CARTESIAN_POINT('Ctrl Pts',(81.3679983883825,4.91978905920369,334.939505641014));
#33728=CARTESIAN_POINT('Ctrl Pts',(81.3602496978249,4.91618817936859,334.802245931916));
#33729=CARTESIAN_POINT('Ctrl Pts',(81.3525010072673,4.90685104673398,334.665342163299));
#33730=CARTESIAN_POINT('Ctrl Pts',(81.3447539288894,4.8975158567678,334.528466878654));
#33731=CARTESIAN_POINT('Ctrl Pts',(81.3370068505116,4.8824468144889,334.391947776912));
#33732=CARTESIAN_POINT('Ctrl Pts',(81.3292597721338,4.86169630657989,334.256298389751));
#33733=CARTESIAN_POINT('Ctrl Pts',(81.321512628828,4.84094562476162,334.120647865717));
#33734=CARTESIAN_POINT('Ctrl Pts',(81.3137654855222,4.81451344144438,333.985867457184));
#33735=CARTESIAN_POINT('Ctrl Pts',(81.3060183422164,4.78250367679576,333.852462791917));
#33736=CARTESIAN_POINT('Ctrl Pts',(81.2982694571882,4.75048671567238,333.719028134449));
#33737=CARTESIAN_POINT('Ctrl Pts',(81.2905205721602,4.71288976916171,333.586970215724));
#33738=CARTESIAN_POINT('Ctrl Pts',(81.282771687132,4.66986715771378,333.456781353208));
#33739=CARTESIAN_POINT('Ctrl Pts',(81.2750145773573,4.62679888162173,333.326454306889));
#33740=CARTESIAN_POINT('Ctrl Pts',(81.2672574675826,4.57829355957558,333.198000651395));
#33741=CARTESIAN_POINT('Ctrl Pts',(81.2595003578078,4.52455459042647,333.071895018224));
#33742=CARTESIAN_POINT('Ctrl Pts',(81.2517391028817,4.47078690489034,332.945721998233));
#33743=CARTESIAN_POINT('Ctrl Pts',(81.2439778479555,4.41178016765363,332.821899853361));
#33744=CARTESIAN_POINT('Ctrl Pts',(81.2362165930293,4.34778420716243,332.70087939628));
#33745=CARTESIAN_POINT('Ctrl Pts',(81.2284429226247,4.28368587399077,332.579665345909));
#33746=CARTESIAN_POINT('Ctrl Pts',(81.22066925222,4.21458256602889,332.461262277031));
#33747=CARTESIAN_POINT('Ctrl Pts',(81.2128955818153,4.1407684526044,332.34609350496));
#33748=CARTESIAN_POINT('Ctrl Pts',(81.2054837776383,4.07039040391877,332.236285866937));
#33749=CARTESIAN_POINT('Ctrl Pts',(81.1980719734612,3.99573042070206,332.129418424974));
#33750=CARTESIAN_POINT('Ctrl Pts',(81.1906601692842,3.9170768563161,332.025829197203));
#33751=CARTESIAN_POINT('Ctrl Pts',(81.1828850905057,3.83456824644225,331.917162752801));
#33752=CARTESIAN_POINT('Ctrl Pts',(81.1751100117273,3.74740393988715,331.811760591978));
#33753=CARTESIAN_POINT('Ctrl Pts',(81.1673349329489,3.65587141789133,331.71004753251));
#33754=CARTESIAN_POINT('Ctrl Pts',(81.1595694218999,3.56445153249132,331.608459637437));
#33755=CARTESIAN_POINT('Ctrl Pts',(81.1518039108509,3.46867438605709,331.510552098841));
#33756=CARTESIAN_POINT('Ctrl Pts',(81.1440383998019,3.3688696088616,331.416719293582));
#33757=CARTESIAN_POINT('Ctrl Pts',(81.1362805882797,3.26916378839321,331.322979523823));
#33758=CARTESIAN_POINT('Ctrl Pts',(81.1285227767575,3.16543856721465,331.233306713367));
#33759=CARTESIAN_POINT('Ctrl Pts',(81.1207649652353,3.05806231839768,331.148060499009));
#33760=CARTESIAN_POINT('Ctrl Pts',(81.1130129917123,2.95076687361304,331.06287843513));
#33761=CARTESIAN_POINT('Ctrl Pts',(81.1052610181893,2.83982617487986,330.982116578907));
#33762=CARTESIAN_POINT('Ctrl Pts',(81.0975090446663,2.7256434893779,330.906095918159));
#33763=CARTESIAN_POINT('Ctrl Pts',(81.0897603541086,2.61150916031104,330.830107452207));
#33764=CARTESIAN_POINT('Ctrl Pts',(81.082011663551,2.49413589992537,330.758856404328));
#33765=CARTESIAN_POINT('Ctrl Pts',(81.0742629729934,2.3739577419484,330.692621713624));
#33766=CARTESIAN_POINT('Ctrl Pts',(81.0665158946156,2.25380458804079,330.626400803601));
#33767=CARTESIAN_POINT('Ctrl Pts',(81.0587688162377,2.13084803943928,330.565194363319));
#33768=CARTESIAN_POINT('Ctrl Pts',(81.0510217378599,2.00554828532923,330.50923624116));
#33769=CARTESIAN_POINT('Ctrl Pts',(81.0432745945541,1.88024748108672,330.453277650017));
#33770=CARTESIAN_POINT('Ctrl Pts',(81.0355274512483,1.75260378906572,330.402567624119));
#33771=CARTESIAN_POINT('Ctrl Pts',(81.0277803079425,1.62309863960799,330.357292398976));
#33772=CARTESIAN_POINT('Ctrl Pts',(81.0200314229144,1.49356437464345,330.312006995002));
#33773=CARTESIAN_POINT('Ctrl Pts',(81.0122825378863,1.36216818838727,330.272158952115));
#33774=CARTESIAN_POINT('Ctrl Pts',(81.0045336528582,1.22940759274902,330.237884920186));
#33775=CARTESIAN_POINT('Ctrl Pts',(80.9967765430835,1.09650608364262,330.203574509445));
#33776=CARTESIAN_POINT('Ctrl Pts',(80.9890194333088,0.962237651305697,330.174850025913));
#33777=CARTESIAN_POINT('Ctrl Pts',(80.9812623235341,0.827111494277802,330.151797277492));
#33778=CARTESIAN_POINT('Ctrl Pts',(80.9735010686079,0.691913130151995,330.12873221042));
#33779=CARTESIAN_POINT('Ctrl Pts',(80.9657398136817,0.555856515574606,330.111344967112));
#33780=CARTESIAN_POINT('Ctrl Pts',(80.9579785587555,0.419455945048126,330.099669422104));
#33781=CARTESIAN_POINT('Ctrl Pts',(80.9502048883509,0.282837178061739,330.087975200029));
#33782=CARTESIAN_POINT('Ctrl Pts',(80.9424312179462,0.145873746338524,330.082010951412));
#33783=CARTESIAN_POINT('Ctrl Pts',(80.9346575475415,0.00908081665911037,
330.081758383195));
#33784=CARTESIAN_POINT('Ctrl Pts',(80.9272457433645,-0.121344369233158,
330.08151757209));
#33785=CARTESIAN_POINT('Ctrl Pts',(80.9198339391874,-0.25161428200463,330.086468639879));
#33786=CARTESIAN_POINT('Ctrl Pts',(80.9124221350103,-0.381288630447359,
330.096552025075));
#33787=CARTESIAN_POINT('Ctrl Pts',(80.9046470562319,-0.517318704987591,
330.107129627017));
#33788=CARTESIAN_POINT('Ctrl Pts',(80.8968719774534,-0.653123238444214,
330.123388794772));
#33789=CARTESIAN_POINT('Ctrl Pts',(80.889096898675,-0.788189419890629,330.145317672507));
#33790=CARTESIAN_POINT('Ctrl Pts',(80.881331387626,-0.923089393801948,330.167219565362));
#33791=CARTESIAN_POINT('Ctrl Pts',(80.8735658765769,-1.05725244140097,330.194777224046));
#33792=CARTESIAN_POINT('Ctrl Pts',(80.8658003655279,-1.19016854091595,330.227926875381));
#33793=CARTESIAN_POINT('Ctrl Pts',(80.8580425540057,-1.32295285373191,330.26104365874));
#33794=CARTESIAN_POINT('Ctrl Pts',(80.8502847424834,-1.45449230206158,330.299741306947));
#33795=CARTESIAN_POINT('Ctrl Pts',(80.8425269309612,-1.58428511184755,330.343904667334));
#33796=CARTESIAN_POINT('Ctrl Pts',(80.8347749574382,-1.71398024842757,330.38803479339));
#33797=CARTESIAN_POINT('Ctrl Pts',(80.8270229839152,-1.84193099416484,330.437622319255));
#33798=CARTESIAN_POINT('Ctrl Pts',(80.8192710103921,-1.96764919254343,330.492501833879));
#33799=CARTESIAN_POINT('Ctrl Pts',(80.8115223198345,-2.0933141491902,330.547358106997));
#33800=CARTESIAN_POINT('Ctrl Pts',(80.8037736292769,-2.21674808149705,330.607501755312));
#33801=CARTESIAN_POINT('Ctrl Pts',(80.7960249387193,-2.33748154306765,330.672718740558));
#33802=CARTESIAN_POINT('Ctrl Pts',(80.7882778603414,-2.45818988503319,330.737922156865));
#33803=CARTESIAN_POINT('Ctrl Pts',(80.7805307819636,-2.57619853014122,330.808196624886));
#33804=CARTESIAN_POINT('Ctrl Pts',(80.7727837035857,-2.69106179552668,330.883281710494));
#33805=CARTESIAN_POINT('Ctrl Pts',(80.7650365602799,-2.80592602357709,330.958367425386));
#33806=CARTESIAN_POINT('Ctrl Pts',(80.7572894169741,-2.91764449215216,331.038263624411));
#33807=CARTESIAN_POINT('Ctrl Pts',(80.7495422736683,-3.02580006225466,331.122666245245));
#33808=CARTESIAN_POINT('Ctrl Pts',(80.7417933886402,-3.13397994802509,331.20708784158));
#33809=CARTESIAN_POINT('Ctrl Pts',(80.7340445036122,-3.23859503330414,331.296017635331));
#33810=CARTESIAN_POINT('Ctrl Pts',(80.7262956185841,-3.33926117405886,331.389111207206));
#33811=CARTESIAN_POINT('Ctrl Pts',(80.7185385088094,-3.44003416289565,331.482303589561));
#33812=CARTESIAN_POINT('Ctrl Pts',(80.7107813990346,-3.53684954696647,331.579668312554));
#33813=CARTESIAN_POINT('Ctrl Pts',(80.7030242892599,-3.62935961202736,331.680823615852));
#33814=CARTESIAN_POINT('Ctrl Pts',(80.6952630343338,-3.72191911150887,331.78203297331));
#33815=CARTESIAN_POINT('Ctrl Pts',(80.6875017794076,-3.81016845642133,331.887036648114));
#33816=CARTESIAN_POINT('Ctrl Pts',(80.6797405244815,-3.89380084667984,331.995420490502));
#33817=CARTESIAN_POINT('Ctrl Pts',(80.6719668540768,-3.97756702150725,332.103977711716));
#33818=CARTESIAN_POINT('Ctrl Pts',(80.6641931836722,-4.05670125727636,332.215925586283));
#33819=CARTESIAN_POINT('Ctrl Pts',(80.6564195132675,-4.13094015070425,332.330821000045));
#33820=CARTESIAN_POINT('Ctrl Pts',(80.6490077090904,-4.20172320578218,332.440368004654));
#33821=CARTESIAN_POINT('Ctrl Pts',(80.6415959049133,-4.26805627193853,332.552594060364));
#33822=CARTESIAN_POINT('Ctrl Pts',(80.6341841007362,-4.3297511688621,332.667096684764));
#33823=CARTESIAN_POINT('Ctrl Pts',(80.6259892272813,-4.39796423291835,332.79369669939));
#33824=CARTESIAN_POINT('Ctrl Pts',(80.6177943538264,-4.46070386279604,332.923444483748));
#33825=CARTESIAN_POINT('Ctrl Pts',(80.6095994803714,-4.51768456457364,333.055852567959));
#33826=CARTESIAN_POINT('Ctrl Pts',(80.60141900125,-4.57456517948293,333.188028076752));
#33827=CARTESIAN_POINT('Ctrl Pts',(80.5932385221284,-4.62570689507404,333.322854273003));
#33828=CARTESIAN_POINT('Ctrl Pts',(80.5850580430069,-4.67086986338482,333.459818912652));
#33829=CARTESIAN_POINT('Ctrl Pts',(80.5768967514728,-4.71592690044302,333.596462297159));
#33830=CARTESIAN_POINT('Ctrl Pts',(80.5687354599387,-4.75503305256771,333.735233811639));
#33831=CARTESIAN_POINT('Ctrl Pts',(80.5605741684045,-4.78799664016023,333.875601833729));
#33832=CARTESIAN_POINT('Ctrl Pts',(80.5524243534081,-4.82091387383258,334.015772468077));
#33833=CARTESIAN_POINT('Ctrl Pts',(80.5442745384117,-4.84770567721586,334.157534818817));
#33834=CARTESIAN_POINT('Ctrl Pts',(80.5361247234153,-4.86822969881815,334.300341038759));
#33835=CARTESIAN_POINT('Ctrl Pts',(80.5279900893834,-4.88871548955942,334.442881248225));
#33836=CARTESIAN_POINT('Ctrl Pts',(80.5198554553515,-4.90295673280841,334.586461125167));
#33837=CARTESIAN_POINT('Ctrl Pts',(80.5117208213197,-4.91086191365771,334.7305221206));
#33838=CARTESIAN_POINT('Ctrl Pts',(80.5066592970536,-4.91578066778231,334.820159616437));
#33839=CARTESIAN_POINT('Ctrl Pts',(80.5015977727876,-4.91824737078159,334.909983125481));
#33840=CARTESIAN_POINT('Ctrl Pts',(80.4965362485215,-4.91824999789874,334.999856232645));
#33841=CARTESIAN_POINT('',(83.9965362485267,-4.91824940115574,335.002427041657));
#33842=CARTESIAN_POINT('Ctrl Pts',(83.99653624849,-4.91824940115542,335.002427042302));
#33843=CARTESIAN_POINT('Ctrl Pts',(83.9887043363345,-4.91818150444409,335.140015480526));
#33844=CARTESIAN_POINT('Ctrl Pts',(83.980872424179,-4.91234057685994,335.277456908605));
#33845=CARTESIAN_POINT('Ctrl Pts',(83.9730405120234,-4.90076020166624,335.414406211662));
#33846=CARTESIAN_POINT('Ctrl Pts',(83.965265433245,-4.88926386110129,335.550361722752));
#33847=CARTESIAN_POINT('Ctrl Pts',(83.9574903544666,-4.87208760806765,335.686053314884));
#33848=CARTESIAN_POINT('Ctrl Pts',(83.9497152756881,-4.84924676253089,335.820968268926));
#33849=CARTESIAN_POINT('Ctrl Pts',(83.9419497646391,-4.82643402410869,335.955717201529));
#33850=CARTESIAN_POINT('Ctrl Pts',(83.9341842535901,-4.79797062738378,336.089691015911));
#33851=CARTESIAN_POINT('Ctrl Pts',(83.9264187425411,-4.76392378964062,336.222380132772));
#33852=CARTESIAN_POINT('Ctrl Pts',(83.9186609310189,-4.72991070943618,336.354937687988));
#33853=CARTESIAN_POINT('Ctrl Pts',(83.9109031194967,-4.69032530168452,336.48621270441));
#33854=CARTESIAN_POINT('Ctrl Pts',(83.9031453079745,-4.64528610626961,336.61570419737));
#33855=CARTESIAN_POINT('Ctrl Pts',(83.8953933344515,-4.60028080427757,336.745098243874));
#33856=CARTESIAN_POINT('Ctrl Pts',(83.8876413609285,-4.54983001161845,336.872711070722));
#33857=CARTESIAN_POINT('Ctrl Pts',(83.8798893874055,-4.49410243340968,336.998055650006));
#33858=CARTESIAN_POINT('Ctrl Pts',(83.8721406968479,-4.43839845586336,337.123347145786));
#33859=CARTESIAN_POINT('Ctrl Pts',(83.8643920062903,-4.37742229593515,337.246371948155));
#33860=CARTESIAN_POINT('Ctrl Pts',(83.8566433157327,-4.31139115845305,337.366662067409));
#33861=CARTESIAN_POINT('Ctrl Pts',(83.8488962373549,-4.24537375930056,337.486927159299));
#33862=CARTESIAN_POINT('Ctrl Pts',(83.841149158977,-4.17430366253076,337.604458357375));
#33863=CARTESIAN_POINT('Ctrl Pts',(83.8334020805992,-4.09844430723293,337.718811748358));
#33864=CARTESIAN_POINT('Ctrl Pts',(83.8256549372934,-4.02258431616073,337.833166097733));
#33865=CARTESIAN_POINT('Ctrl Pts',(83.8179077939876,-3.94193520257662,337.944342261174));
#33866=CARTESIAN_POINT('Ctrl Pts',(83.8101606506818,-3.85680383993657,338.05192516336));
#33867=CARTESIAN_POINT('Ctrl Pts',(83.8024117656537,-3.7716533379588,338.159532252467));
#33868=CARTESIAN_POINT('Ctrl Pts',(83.7946628806256,-3.68201882420734,338.263544166348));
#33869=CARTESIAN_POINT('Ctrl Pts',(83.7869139955975,-3.58824730528171,338.363579096534));
#33870=CARTESIAN_POINT('Ctrl Pts',(83.7791568858228,-3.49437625629705,338.463720204828));
#33871=CARTESIAN_POINT('Ctrl Pts',(83.7713997760481,-3.39635969832406,338.559875611538));
#33872=CARTESIAN_POINT('Ctrl Pts',(83.7636426662733,-3.29458173204331,338.651700189417));
#33873=CARTESIAN_POINT('Ctrl Pts',(83.7558814113472,-3.19274937887168,338.743573835414));
#33874=CARTESIAN_POINT('Ctrl Pts',(83.748120156421,-3.08715191310231,338.831111791885));
#33875=CARTESIAN_POINT('Ctrl Pts',(83.7403589014949,-2.97820554770165,338.914010063623));
#33876=CARTESIAN_POINT('Ctrl Pts',(83.7325852310902,-2.86908490362181,338.997040945579));
#33877=CARTESIAN_POINT('Ctrl Pts',(83.7248115606856,-2.75660497560906,339.0754170879));
#33878=CARTESIAN_POINT('Ctrl Pts',(83.7170378902809,-2.64121064718774,339.148878086867));
#33879=CARTESIAN_POINT('Ctrl Pts',(83.7096260861038,-2.53118795251655,339.218919458658));
#33880=CARTESIAN_POINT('Ctrl Pts',(83.7022142819267,-2.41851633072506,339.284492844179));
#33881=CARTESIAN_POINT('Ctrl Pts',(83.6948024777496,-2.30359952632896,339.345412786468));
#33882=CARTESIAN_POINT('Ctrl Pts',(83.6870273989712,-2.18305030703007,339.4093185966));
#33883=CARTESIAN_POINT('Ctrl Pts',(83.6792523201928,-2.05964929626415,339.468305225468));
#33884=CARTESIAN_POINT('Ctrl Pts',(83.6714772414143,-1.9338359409981,339.522108094219));
#33885=CARTESIAN_POINT('Ctrl Pts',(83.6637117303653,-1.80817740707538,339.575844755115));
#33886=CARTESIAN_POINT('Ctrl Pts',(83.6559462193163,-1.68011279115845,339.624410195947));
#33887=CARTESIAN_POINT('Ctrl Pts',(83.6481807082673,-1.55010698448145,339.667585178565));
#33888=CARTESIAN_POINT('Ctrl Pts',(83.6404228967451,-1.42023007894028,339.710717353062));
#33889=CARTESIAN_POINT('Ctrl Pts',(83.6326650852229,-1.28841618145678,339.748469583111));
#33890=CARTESIAN_POINT('Ctrl Pts',(83.6249072737007,-1.15515072945985,339.780670439879));
#33891=CARTESIAN_POINT('Ctrl Pts',(83.6171553001777,-1.02198556394173,339.81284706448));
#33892=CARTESIAN_POINT('Ctrl Pts',(83.6094033266547,-0.887371396571579,
339.839480539642));
#33893=CARTESIAN_POINT('Ctrl Pts',(83.6016513531317,-0.751809075525826,
339.860449174352));
#33894=CARTESIAN_POINT('Ctrl Pts',(83.5939026625741,-0.616304165203521,
339.881408928832));
#33895=CARTESIAN_POINT('Ctrl Pts',(83.5861539720164,-0.479852285324325,
339.896708554803));
#33896=CARTESIAN_POINT('Ctrl Pts',(83.5784052814588,-0.342964520408958,
339.906277448355));
#33897=CARTESIAN_POINT('Ctrl Pts',(83.570658203081,-0.206105236136298,339.91584435102));
#33898=CARTESIAN_POINT('Ctrl Pts',(83.5629111247032,-0.0688106368933147,
339.91968286565));
#33899=CARTESIAN_POINT('Ctrl Pts',(83.5551640463253,0.0684034191679079,
339.917774296849));
#33900=CARTESIAN_POINT('Ctrl Pts',(83.5474169030195,0.205618625214894,339.915865712052));
#33901=CARTESIAN_POINT('Ctrl Pts',(83.5396697597137,0.342752895897242,339.908209953191));
#33902=CARTESIAN_POINT('Ctrl Pts',(83.5319226164079,0.479291118687179,339.894840455628));
#33903=CARTESIAN_POINT('Ctrl Pts',(83.5241737313798,0.615860038168481,339.881467952317));
#33904=CARTESIAN_POINT('Ctrl Pts',(83.5164248463517,0.751832254166132,339.862379192239));
#33905=CARTESIAN_POINT('Ctrl Pts',(83.5086759613236,0.886698910610572,339.837659362173));
#33906=CARTESIAN_POINT('Ctrl Pts',(83.5009188515489,1.0217087159176,339.812913294225));
#33907=CARTESIAN_POINT('Ctrl Pts',(83.4931617417742,1.15561023251362,339.782524287501));
#33908=CARTESIAN_POINT('Ctrl Pts',(83.4854046319995,1.28790537661639,339.746628572301));
#33909=CARTESIAN_POINT('Ctrl Pts',(83.4776433770733,1.42027121501409,339.710713675579));
#33910=CARTESIAN_POINT('Ctrl Pts',(83.4698821221471,1.55102859806014,339.669286324963));
#33911=CARTESIAN_POINT('Ctrl Pts',(83.462120867221,1.67969665298089,339.622532013568));
#33912=CARTESIAN_POINT('Ctrl Pts',(83.4543471968163,1.80857053485679,339.575702910512));
#33913=CARTESIAN_POINT('Ctrl Pts',(83.4465735264117,1.93534804816124,339.523529967225));
#33914=CARTESIAN_POINT('Ctrl Pts',(83.438799856007,2.05956946184786,339.466246376357));
#33915=CARTESIAN_POINT('Ctrl Pts',(83.4313880518299,2.17800833884226,339.411629350426));
#33916=CARTESIAN_POINT('Ctrl Pts',(83.4239762476527,2.29412347732198,339.352366901423));
#33917=CARTESIAN_POINT('Ctrl Pts',(83.4165644434756,2.40754043324713,339.288698185322));
#33918=CARTESIAN_POINT('Ctrl Pts',(83.4087893646972,2.52651629203309,339.221908875785));
#33919=CARTESIAN_POINT('Ctrl Pts',(83.4010142859187,2.64289877434749,339.15005938272));
#33920=CARTESIAN_POINT('Ctrl Pts',(83.3932392071403,2.7562275802174,339.073376067656));
#33921=CARTESIAN_POINT('Ctrl Pts',(83.3854736960913,2.86941692777683,338.996787116292));
#33922=CARTESIAN_POINT('Ctrl Pts',(83.3777081850423,2.97955975508958,338.915376395347));
#33923=CARTESIAN_POINT('Ctrl Pts',(83.3699426739933,3.08622012079563,338.829416199435));
#33924=CARTESIAN_POINT('Ctrl Pts',(83.3621848624711,3.19277473243855,338.743541233307));
#33925=CARTESIAN_POINT('Ctrl Pts',(83.3544270509489,3.29585345150338,338.653126012689));
#33926=CARTESIAN_POINT('Ctrl Pts',(83.3466692394267,3.39504942177975,338.558485982293));
#33927=CARTESIAN_POINT('Ctrl Pts',(83.3389172659037,3.49417074394273,338.46391717152));
#33928=CARTESIAN_POINT('Ctrl Pts',(83.3311652923807,3.5894148515303,338.36513014795));
#33929=CARTESIAN_POINT('Ctrl Pts',(83.3234133188577,3.68040837428604,338.262480231509));
#33930=CARTESIAN_POINT('Ctrl Pts',(83.3156646283001,3.77136336123088,338.159873787368));
#33931=CARTESIAN_POINT('Ctrl Pts',(83.3079159377425,3.85807108492248,338.053407996009));
#33932=CARTESIAN_POINT('Ctrl Pts',(83.3001672471848,3.94019559586849,337.943474431484));
#33933=CARTESIAN_POINT('Ctrl Pts',(83.292420168807,4.02230302012408,337.833563739555));
#33934=CARTESIAN_POINT('Ctrl Pts',(83.2846730904292,4.09982889457998,337.720187022519));
#33935=CARTESIAN_POINT('Ctrl Pts',(83.2769260120513,4.17247833743341,337.603767959352));
#33936=CARTESIAN_POINT('Ctrl Pts',(83.2691788687455,4.24512838915914,337.487347920481));
#33937=CARTESIAN_POINT('Ctrl Pts',(83.2614317254397,4.31290172083319,337.367885816226));
#33938=CARTESIAN_POINT('Ctrl Pts',(83.2536845821339,4.37554769201968,337.245832909493));
#33939=CARTESIAN_POINT('Ctrl Pts',(83.2459356971058,4.43820774735042,337.123752562676));
#33940=CARTESIAN_POINT('Ctrl Pts',(83.2381868120778,4.49573796991978,336.999080602012));
#33941=CARTESIAN_POINT('Ctrl Pts',(83.2304379270497,4.54793462389251,336.872291034882));
#33942=CARTESIAN_POINT('Ctrl Pts',(83.222680817275,4.60018667993312,336.745366891995));
#33943=CARTESIAN_POINT('Ctrl Pts',(83.2149237075002,4.64709370975516,336.616321014767));
#33944=CARTESIAN_POINT('Ctrl Pts',(83.2071665977255,4.68850073060997,336.485645974507));
#33945=CARTESIAN_POINT('Ctrl Pts',(83.1994053427993,4.72992987805278,336.354901105684));
#33946=CARTESIAN_POINT('Ctrl Pts',(83.1916440878731,4.76585305792996,336.222525716176));
#33947=CARTESIAN_POINT('Ctrl Pts',(83.183882832947,4.79616602750741,336.089024563122));
#33948=CARTESIAN_POINT('Ctrl Pts',(83.1761091625423,4.82652748795718,335.955309851732));
#33949=CARTESIAN_POINT('Ctrl Pts',(83.1683354921377,4.85126073382683,335.820466162819));
#33950=CARTESIAN_POINT('Ctrl Pts',(83.160561821733,4.87031307494354,335.685006287952));
#33951=CARTESIAN_POINT('Ctrl Pts',(83.1531500175559,4.88847852499755,335.55585210285));
#33952=CARTESIAN_POINT('Ctrl Pts',(83.1457382133789,4.90148003143856,335.426138094061));
#33953=CARTESIAN_POINT('Ctrl Pts',(83.1383264092018,4.90931607247105,335.296308560587));
#33954=CARTESIAN_POINT('Ctrl Pts',(83.1305513304233,4.91753618121691,335.160115694936));
#33955=CARTESIAN_POINT('Ctrl Pts',(83.1227762516449,4.92009764886239,335.023365299226));
#33956=CARTESIAN_POINT('Ctrl Pts',(83.1150011728665,4.91694173291969,334.886566946736));
#33957=CARTESIAN_POINT('Ctrl Pts',(83.1072356618175,4.91378970053247,334.749936933329));
#33958=CARTESIAN_POINT('Ctrl Pts',(83.0994701507685,4.90493429232151,334.613259467598));
#33959=CARTESIAN_POINT('Ctrl Pts',(83.0917046397194,4.89036857375248,334.477048496174));
#33960=CARTESIAN_POINT('Ctrl Pts',(83.0839468281972,4.87581729713584,334.340972578324));
#33961=CARTESIAN_POINT('Ctrl Pts',(83.076189016675,4.85556701873552,334.205362620474));
#33962=CARTESIAN_POINT('Ctrl Pts',(83.0684312051528,4.82966282949875,334.070731461924));
#33963=CARTESIAN_POINT('Ctrl Pts',(83.0606792316298,4.80377813398585,333.93620161759));
#33964=CARTESIAN_POINT('Ctrl Pts',(83.0529272581068,4.77224807005836,333.802649488724));
#33965=CARTESIAN_POINT('Ctrl Pts',(83.0451752845838,4.73516938175326,333.67058133434));
#33966=CARTESIAN_POINT('Ctrl Pts',(83.0374265940262,4.69810639629466,333.538569110897));
#33967=CARTESIAN_POINT('Ctrl Pts',(83.0296779034685,4.6554995655707,333.408039987506));
#33968=CARTESIAN_POINT('Ctrl Pts',(83.0219292129109,4.6074963710079,333.279488374451));
#33969=CARTESIAN_POINT('Ctrl Pts',(83.0141821345331,4.55950316391067,333.150963507632));
#33970=CARTESIAN_POINT('Ctrl Pts',(83.0064350561553,4.50611596287135,333.024415698718));
#33971=CARTESIAN_POINT('Ctrl Pts',(82.9986879777774,4.44753147111442,332.900322197111));
#33972=CARTESIAN_POINT('Ctrl Pts',(82.9909408344716,4.38894648836302,332.77622765548));
#33973=CARTESIAN_POINT('Ctrl Pts',(82.9831936911658,4.32516429488406,332.654587815648));
#33974=CARTESIAN_POINT('Ctrl Pts',(82.97544654786,4.25642873136212,332.535857650757));
#33975=CARTESIAN_POINT('Ctrl Pts',(82.9676976628319,4.18767771462625,332.417100792804));
#33976=CARTESIAN_POINT('Ctrl Pts',(82.9599487778038,4.11397130766016,332.301255249701));
#33977=CARTESIAN_POINT('Ctrl Pts',(82.9521998927757,4.03559786023181,332.18874885985));
#33978=CARTESIAN_POINT('Ctrl Pts',(82.944442783001,3.95714122641655,332.076123054555));
#33979=CARTESIAN_POINT('Ctrl Pts',(82.9366856732262,3.87400788054348,331.966843803641));
#33980=CARTESIAN_POINT('Ctrl Pts',(82.9289285634515,3.78652816627843,331.861307994008));
#33981=CARTESIAN_POINT('Ctrl Pts',(82.9211673085253,3.6990017056512,331.755715789412));
#33982=CARTESIAN_POINT('Ctrl Pts',(82.9134060535992,3.60712451041142,331.653871302104));
#33983=CARTESIAN_POINT('Ctrl Pts',(82.905644798673,3.51126462988296,331.556135345076));
#33984=CARTESIAN_POINT('Ctrl Pts',(82.8978711282683,3.41525140478632,331.458243042369));
#33985=CARTESIAN_POINT('Ctrl Pts',(82.8900974578636,3.31524304854875,331.364472670856));
#33986=CARTESIAN_POINT('Ctrl Pts',(82.882323787459,3.2116422648649,331.275146039771));
#33987=CARTESIAN_POINT('Ctrl Pts',(82.8749119832819,3.1128641225863,331.189977584853));
#33988=CARTESIAN_POINT('Ctrl Pts',(82.8675001791048,3.0108207064303,331.108848647568));
#33989=CARTESIAN_POINT('Ctrl Pts',(82.8600883749277,2.90588481337507,331.03200094331));
#33990=CARTESIAN_POINT('Ctrl Pts',(82.8523132961493,2.79580569961331,330.951386704148));
#33991=CARTESIAN_POINT('Ctrl Pts',(82.8445382173708,2.68219553153876,330.875229225503));
#33992=CARTESIAN_POINT('Ctrl Pts',(82.8367631385924,2.56545103126276,330.803853664528));
#33993=CARTESIAN_POINT('Ctrl Pts',(82.8289976275434,2.44885019252674,330.732565935725));
#33994=CARTESIAN_POINT('Ctrl Pts',(82.8212321164944,2.32912302620167,330.666048618153));
#33995=CARTESIAN_POINT('Ctrl Pts',(82.8134666054454,2.20669796829874,330.604585669222));
#33996=CARTESIAN_POINT('Ctrl Pts',(82.8057087939232,2.08439429519707,330.543183660984));
#33997=CARTESIAN_POINT('Ctrl Pts',(82.797950982401,1.95939840092588,330.486826222621));
#33998=CARTESIAN_POINT('Ctrl Pts',(82.7901931708788,1.83216594429326,330.435752962966));
#33999=CARTESIAN_POINT('Ctrl Pts',(82.7824411973558,1.70502923411912,330.384718137559));
#34000=CARTESIAN_POINT('Ctrl Pts',(82.7746892238328,1.57565967295978,330.338959720831));
#34001=CARTESIAN_POINT('Ctrl Pts',(82.7669372503098,1.4445353385708,330.298670324459));
#34002=CARTESIAN_POINT('Ctrl Pts',(82.7591885597521,1.31346653541529,330.258397990671));
#34003=CARTESIAN_POINT('Ctrl Pts',(82.7514398691945,1.18064480995528,330.223590185177));
#34004=CARTESIAN_POINT('Ctrl Pts',(82.7436911786369,1.0465657330079,330.194390441474));
#34005=CARTESIAN_POINT('Ctrl Pts',(82.7359441002591,0.912514552332327,330.165196773022));
#34006=CARTESIAN_POINT('Ctrl Pts',(82.7281970218812,0.777206922197701,330.141608928626));
#34007=CARTESIAN_POINT('Ctrl Pts',(82.7204499435034,0.641150619209999,330.123719763387));
#34008=CARTESIAN_POINT('Ctrl Pts',(82.7127028001976,0.505093175939431,330.105830448218));
#34009=CARTESIAN_POINT('Ctrl Pts',(82.7049556568918,0.368287434839402,330.093639958423));
#34010=CARTESIAN_POINT('Ctrl Pts',(82.697208513586,0.231247948717784,330.087189455239));
#34011=CARTESIAN_POINT('Ctrl Pts',(82.6894596285579,0.0941776532105353,
330.080737501846));
#34012=CARTESIAN_POINT('Ctrl Pts',(82.6817107435298,-0.0431261015229156,
330.080028121332));
#34013=CARTESIAN_POINT('Ctrl Pts',(82.6739618585017,-0.180147494437449,
330.085050362135));
#34014=CARTESIAN_POINT('Ctrl Pts',(82.666204748727,-0.317314323274304,330.090077933597));
#34015=CARTESIAN_POINT('Ctrl Pts',(82.6584476389523,-0.45419780038092,330.100849264602));
#34016=CARTESIAN_POINT('Ctrl Pts',(82.6506905291776,-0.590285407183225,
330.117301340389));
#34017=CARTESIAN_POINT('Ctrl Pts',(82.6429292742514,-0.726445734851458,
330.13376220764));
#34018=CARTESIAN_POINT('Ctrl Pts',(82.6351680193252,-0.861808959241969,
330.155909805313));
#34019=CARTESIAN_POINT('Ctrl Pts',(82.627406764399,-0.995872492405019,330.183629889494));
#34020=CARTESIAN_POINT('Ctrl Pts',(82.6196330939944,-1.13015048352984,330.211394316777));
#34021=CARTESIAN_POINT('Ctrl Pts',(82.6118594235897,-1.2631242494764,330.244748948553));
#34022=CARTESIAN_POINT('Ctrl Pts',(82.6040857531851,-1.39430524791927,330.283529292138));
#34023=CARTESIAN_POINT('Ctrl Pts',(82.596673949008,-1.51937973932368,330.320504401398));
#34024=CARTESIAN_POINT('Ctrl Pts',(82.589262144831,-1.64282434122797,330.362411363902));
#34025=CARTESIAN_POINT('Ctrl Pts',(82.5818503406539,-1.7642340481647,330.409067492786));
#34026=CARTESIAN_POINT('Ctrl Pts',(82.5740752618755,-1.89159440649998,330.458010377528));
#34027=CARTESIAN_POINT('Ctrl Pts',(82.566300183097,-2.01711783593588,330.512334410019));
#34028=CARTESIAN_POINT('Ctrl Pts',(82.5585251043186,-2.1403162157879,330.571881939363));
#34029=CARTESIAN_POINT('Ctrl Pts',(82.5507595932696,-2.26336299219023,330.631356191682));
#34030=CARTESIAN_POINT('Ctrl Pts',(82.5429940822206,-2.38409006326298,330.696040982811));
#34031=CARTESIAN_POINT('Ctrl Pts',(82.5352285711716,-2.5020267918532,330.765729697416));
#34032=CARTESIAN_POINT('Ctrl Pts',(82.5274707596494,-2.61984658583374,330.835349315457));
#34033=CARTESIAN_POINT('Ctrl Pts',(82.5197129481272,-2.73488120873949,330.909962785933));
#34034=CARTESIAN_POINT('Ctrl Pts',(82.511955136605,-2.84668258526416,330.989316601718));
#34035=CARTESIAN_POINT('Ctrl Pts',(82.504203163082,-2.95839982770748,331.068610701241));
#34036=CARTESIAN_POINT('Ctrl Pts',(82.496451189559,-3.06688834931433,331.152637820289));
#34037=CARTESIAN_POINT('Ctrl Pts',(82.4886992160359,-3.17172746351039,331.24110016631));
#34038=CARTESIAN_POINT('Ctrl Pts',(82.4809505254783,-3.27652217827935,331.329525048475));
#34039=CARTESIAN_POINT('Ctrl Pts',(82.4732018349207,-3.37767026146619,331.422381170217));
#34040=CARTESIAN_POINT('Ctrl Pts',(82.4654531443631,-3.47478283088745,331.519329469675));
#34041=CARTESIAN_POINT('Ctrl Pts',(82.4577060659852,-3.57187519522748,331.61625759823));
#34042=CARTESIAN_POINT('Ctrl Pts',(82.4499589876074,-3.66493343942012,331.717275934999));
#34043=CARTESIAN_POINT('Ctrl Pts',(82.4422119092296,-3.75360469257444,331.822007729024));
#34044=CARTESIAN_POINT('Ctrl Pts',(82.4344647659238,-3.84227668887914,331.926740400802));
#34045=CARTESIAN_POINT('Ctrl Pts',(82.426717622618,-3.92656136824199,332.035186293597));
#34046=CARTESIAN_POINT('Ctrl Pts',(82.4189704793122,-4.0061456632488,332.146934983683));
#34047=CARTESIAN_POINT('Ctrl Pts',(82.4112215942841,-4.0857478504948,332.258708797247));
#34048=CARTESIAN_POINT('Ctrl Pts',(82.403472709256,-4.16064732387697,332.373786567349));
#34049=CARTESIAN_POINT('Ctrl Pts',(82.3957238242279,-4.23057415243261,332.491728602549));
#34050=CARTESIAN_POINT('Ctrl Pts',(82.3879667144532,-4.30057520204665,332.609795822644));
#34051=CARTESIAN_POINT('Ctrl Pts',(82.3802096046785,-4.36559286384296,332.73073304409));
#34052=CARTESIAN_POINT('Ctrl Pts',(82.3724524949037,-4.42540277506992,332.85407517818));
#34053=CARTESIAN_POINT('Ctrl Pts',(82.3646912399776,-4.485244646801,332.977483222363));
#34054=CARTESIAN_POINT('Ctrl Pts',(82.3569299850514,-4.53987306727684,333.10329838153));
#34055=CARTESIAN_POINT('Ctrl Pts',(82.3491687301252,-4.58911212746512,333.231036194816));
#34056=CARTESIAN_POINT('Ctrl Pts',(82.3413950597206,-4.63842995410276,333.358978346973));
#34057=CARTESIAN_POINT('Ctrl Pts',(82.3336213893159,-4.68234106743871,333.488848928771));
#34058=CARTESIAN_POINT('Ctrl Pts',(82.3258477189113,-4.72071941459793,333.620148098114));
#34059=CARTESIAN_POINT('Ctrl Pts',(82.3184359147341,-4.75731124046394,333.745335259537));
#34060=CARTESIAN_POINT('Ctrl Pts',(82.3110241105569,-4.78887373898933,333.871820720887));
#34061=CARTESIAN_POINT('Ctrl Pts',(82.3036123063798,-4.81534136375698,333.999165042082));
#34062=CARTESIAN_POINT('Ctrl Pts',(82.2926006445855,-4.85466411507003,334.188359543569));
#34063=CARTESIAN_POINT('Ctrl Pts',(82.2815889827912,-4.88284747263759,334.3799424553));
#34064=CARTESIAN_POINT('Ctrl Pts',(82.2705773209969,-4.89966400728638,334.572828280194));
#34065=CARTESIAN_POINT('Ctrl Pts',(82.2625636301613,-4.91190217007419,334.713200132885));
#34066=CARTESIAN_POINT('Ctrl Pts',(82.2545499393256,-4.91812116425913,334.854261771732));
#34067=CARTESIAN_POINT('Ctrl Pts',(82.2465362484899,-4.91824801864458,334.995585297446));
#34068=CARTESIAN_POINT('',(85.746536248436,-4.91824901287694,335.003116060811));
#34069=CARTESIAN_POINT('Ctrl Pts',(85.7465362484359,-4.91824901287694,335.003116060811));
#34070=CARTESIAN_POINT('Ctrl Pts',(85.7378083397602,-4.91815097020962,335.157862158879));
#34071=CARTESIAN_POINT('Ctrl Pts',(85.7290804310845,-4.91074557489866,335.312332150909));
#34072=CARTESIAN_POINT('Ctrl Pts',(85.7203525224088,-4.89613509597295,335.46588001082));
#34073=CARTESIAN_POINT('Ctrl Pts',(85.7115908771786,-4.88146814221046,335.620021389286));
#34074=CARTESIAN_POINT('Ctrl Pts',(85.7028292319484,-4.8595404069818,335.773233305754));
#34075=CARTESIAN_POINT('Ctrl Pts',(85.6940675867182,-4.83050522521385,335.924879630915));
#34076=CARTESIAN_POINT('Ctrl Pts',(85.6852578442456,-4.80131065418298,336.077358421883));
#34077=CARTESIAN_POINT('Ctrl Pts',(85.676448101773,-4.76493048672398,336.228254199914));
#34078=CARTESIAN_POINT('Ctrl Pts',(85.6676383593005,-4.72156937661856,336.376940697444));
#34079=CARTESIAN_POINT('Ctrl Pts',(85.659248478756,-4.68027480584169,336.518540971997));
#34080=CARTESIAN_POINT('Ctrl Pts',(85.6508585982116,-4.63264928898657,336.658137558858));
#34081=CARTESIAN_POINT('Ctrl Pts',(85.6424687176671,-4.57890908465216,336.795208805958));
#34082=CARTESIAN_POINT('Ctrl Pts',(85.6346936388887,-4.52910690689109,336.922235613887));
#34083=CARTESIAN_POINT('Ctrl Pts',(85.6269185601102,-4.47393611394265,337.04738918135));
#34084=CARTESIAN_POINT('Ctrl Pts',(85.6191434813318,-4.41355765070659,337.170182463847));
#34085=CARTESIAN_POINT('Ctrl Pts',(85.6113779702828,-4.35325348701347,337.292824641393));
#34086=CARTESIAN_POINT('Ctrl Pts',(85.6036124592338,-4.28775457467606,337.413111965645));
#34087=CARTESIAN_POINT('Ctrl Pts',(85.5958469481848,-4.21727070380278,337.530575206025));
#34088=CARTESIAN_POINT('Ctrl Pts',(85.5880891366626,-4.14685671789268,337.64792198126));
#34089=CARTESIAN_POINT('Ctrl Pts',(85.5803313251404,-4.07146780932203,337.762449911949));
#34090=CARTESIAN_POINT('Ctrl Pts',(85.5725735136182,-3.99136050649795,337.873712645633));
#34091=CARTESIAN_POINT('Ctrl Pts',(85.5648215400952,-3.9113134869597,337.984891650581));
#34092=CARTESIAN_POINT('Ctrl Pts',(85.5570695665722,-3.82655536821161,338.092810033455));
#34093=CARTESIAN_POINT('Ctrl Pts',(85.5493175930492,-3.73738677804871,338.197049129082));
#34094=CARTESIAN_POINT('Ctrl Pts',(85.5415689024916,-3.64825595083656,338.301244079391));
#34095=CARTESIAN_POINT('Ctrl Pts',(85.533820211934,-3.55471862076062,338.401762545156));
#34096=CARTESIAN_POINT('Ctrl Pts',(85.5260715213764,-3.45711646912184,338.498217943672));
#34097=CARTESIAN_POINT('Ctrl Pts',(85.5183244429985,-3.35953462442589,338.594653273836));
#34098=CARTESIAN_POINT('Ctrl Pts',(85.5105773646207,-3.25788991820788,338.687026943644));
#34099=CARTESIAN_POINT('Ctrl Pts',(85.5028302862429,-3.15256147672356,338.774988635477));
#34100=CARTESIAN_POINT('Ctrl Pts',(85.4950831429371,-3.04723215248559,338.862951064513));
#34101=CARTESIAN_POINT('Ctrl Pts',(85.4873359996313,-2.93821933141674,338.946501191275));
#34102=CARTESIAN_POINT('Ctrl Pts',(85.4795888563255,-2.82593554286927,339.025328728197));
#34103=CARTESIAN_POINT('Ctrl Pts',(85.4718399712974,-2.71362651054221,339.104173987223));
#34104=CARTESIAN_POINT('Ctrl Pts',(85.4640910862693,-2.59804536725416,339.178294319122));
#34105=CARTESIAN_POINT('Ctrl Pts',(85.4563422012412,-2.47963361798748,339.247422769521));
#34106=CARTESIAN_POINT('Ctrl Pts',(85.4485850914665,-2.36109618526671,339.316624593572));
#34107=CARTESIAN_POINT('Ctrl Pts',(85.4408279816918,-2.23972248302163,339.380823754623));
#34108=CARTESIAN_POINT('Ctrl Pts',(85.4330708719171,-2.11597910507516,339.439799037049));
#34109=CARTESIAN_POINT('Ctrl Pts',(85.4253096169909,-1.99216960262406,339.498805833981));
#34110=CARTESIAN_POINT('Ctrl Pts',(85.4175483620647,-1.86598826069384,339.552583036853));
#34111=CARTESIAN_POINT('Ctrl Pts',(85.4097871071386,-1.73792071748697,339.600958013526));
#34112=CARTESIAN_POINT('Ctrl Pts',(85.4020134367339,-1.60964830794808,339.649410374396));
#34113=CARTESIAN_POINT('Ctrl Pts',(85.3942397663292,-1.47948403897286,339.692443117431));
#34114=CARTESIAN_POINT('Ctrl Pts',(85.3864660959246,-1.34792859282739,339.729933569421));
#34115=CARTESIAN_POINT('Ctrl Pts',(85.3790542917474,-1.22249708434969,339.765678831852));
#34116=CARTESIAN_POINT('Ctrl Pts',(85.3716424875703,-1.09580128225935,339.796386110771));
#34117=CARTESIAN_POINT('Ctrl Pts',(85.3642306833932,-0.968281059423146,
339.821992829989));
#34118=CARTESIAN_POINT('Ctrl Pts',(85.3564556046148,-0.834510690603265,
339.848854610793));
#34119=CARTESIAN_POINT('Ctrl Pts',(85.3486805258364,-0.699410303925138,
339.87018809065));
#34120=CARTESIAN_POINT('Ctrl Pts',(85.3409054470579,-0.563476562020997,
339.885865043833));
#34121=CARTESIAN_POINT('Ctrl Pts',(85.3331399360089,-0.427710095240234,
339.901522705527));
#34122=CARTESIAN_POINT('Ctrl Pts',(85.3253744249599,-0.291112698266287,
339.911537646023));
#34123=CARTESIAN_POINT('Ctrl Pts',(85.3176089139109,-0.15419248656926,339.915832354707));
#34124=CARTESIAN_POINT('Ctrl Pts',(85.3098511023887,-0.0174080316606694,
339.920122805175));
#34125=CARTESIAN_POINT('Ctrl Pts',(85.3020932908665,0.11969821284467,339.918704298513));
#34126=CARTESIAN_POINT('Ctrl Pts',(85.2943354793443,0.256612077399884,339.911551008005));
#34127=CARTESIAN_POINT('Ctrl Pts',(85.2865835058213,0.393422909930045,339.904403100574));
#34128=CARTESIAN_POINT('Ctrl Pts',(85.2788315322983,0.530041261901512,339.891529019612));
#34129=CARTESIAN_POINT('Ctrl Pts',(85.2710795587753,0.665952381888176,339.872955005698));
#34130=CARTESIAN_POINT('Ctrl Pts',(85.2633308682177,0.801805943434835,339.85438885789));
#34131=CARTESIAN_POINT('Ctrl Pts',(85.25558217766,0.936952482238757,339.830127631071));
#34132=CARTESIAN_POINT('Ctrl Pts',(85.2478334871024,1.07088200929846,339.800249450254));
#34133=CARTESIAN_POINT('Ctrl Pts',(85.2400864087246,1.20478367120145,339.770377485842));
#34134=CARTESIAN_POINT('Ctrl Pts',(85.2323393303467,1.33746844375498,339.734890977021));
#34135=CARTESIAN_POINT('Ctrl Pts',(85.2245922519689,1.46843657042959,339.693919162185));
#34136=CARTESIAN_POINT('Ctrl Pts',(85.2168451086631,1.59940579474326,339.652947003965));
#34137=CARTESIAN_POINT('Ctrl Pts',(85.2090979653573,1.72865797143602,339.606489564738));
#34138=CARTESIAN_POINT('Ctrl Pts',(85.2013508220515,1.85570892977093,339.55472583483));
#34139=CARTESIAN_POINT('Ctrl Pts',(85.1936019370234,1.98278845185855,339.502950467337));
#34140=CARTESIAN_POINT('Ctrl Pts',(85.1858530519953,2.10766540891845,339.445866582745));
#34141=CARTESIAN_POINT('Ctrl Pts',(85.1781041669672,2.2298763896427,339.383700987683));
#34142=CARTESIAN_POINT('Ctrl Pts',(85.1703470571925,2.35221708636465,339.321469409416));
#34143=CARTESIAN_POINT('Ctrl Pts',(85.1625899474177,2.47188580522838,339.254145523596));
#34144=CARTESIAN_POINT('Ctrl Pts',(85.154832837643,2.58844402060358,339.182001986454));
#34145=CARTESIAN_POINT('Ctrl Pts',(85.1470715827168,2.70506452096226,339.109819898111));
#34146=CARTESIAN_POINT('Ctrl Pts',(85.1393103277907,2.81857088254616,339.032813245931));
#34147=CARTESIAN_POINT('Ctrl Pts',(85.1315490728645,2.92855512860855,338.95129699228));
#34148=CARTESIAN_POINT('Ctrl Pts',(85.1237754024598,3.03871531362078,338.869650339189));
#34149=CARTESIAN_POINT('Ctrl Pts',(85.1160017320552,3.14534182006872,338.78347991495));
#34150=CARTESIAN_POINT('Ctrl Pts',(85.1082280616505,3.24806054153025,338.693140368447));
#34151=CARTESIAN_POINT('Ctrl Pts',(85.1008162574734,3.34599768179499,338.607006149569));
#34152=CARTESIAN_POINT('Ctrl Pts',(85.0934044532964,3.4403824560634,338.517082417262));
#34153=CARTESIAN_POINT('Ctrl Pts',(85.0859926491193,3.53092420223363,338.423705206437));
#34154=CARTESIAN_POINT('Ctrl Pts',(85.0782175703408,3.62590366909374,338.325751300352));
#34155=CARTESIAN_POINT('Ctrl Pts',(85.0704424915624,3.7169540187255,338.22368727302));
#34156=CARTESIAN_POINT('Ctrl Pts',(85.062667412784,3.80369865073104,338.117861388344));
#34157=CARTESIAN_POINT('Ctrl Pts',(85.054901901735,3.89033653794447,338.012165729157));
#34158=CARTESIAN_POINT('Ctrl Pts',(85.0471363906859,3.9726790045262,337.902717722823));
#34159=CARTESIAN_POINT('Ctrl Pts',(85.0393708796369,4.05038589971157,337.789902709042));
#34160=CARTESIAN_POINT('Ctrl Pts',(85.0316130681147,4.12801574828413,337.677199551675));
#34161=CARTESIAN_POINT('Ctrl Pts',(85.0238552565926,4.2010189518263,337.561136350288));
#34162=CARTESIAN_POINT('Ctrl Pts',(85.0160974450704,4.26909554545549,337.442131504705));
#34163=CARTESIAN_POINT('Ctrl Pts',(85.0083454715473,4.33712090928914,337.323216214042));
#34164=CARTESIAN_POINT('Ctrl Pts',(85.0005934980243,4.40022684936324,337.201364023321));
#34165=CARTESIAN_POINT('Ctrl Pts',(84.9928415245013,4.45815687040664,337.077021998282));
#34166=CARTESIAN_POINT('Ctrl Pts',(84.9850928339437,4.51606235805169,336.952732632164));
#34167=CARTESIAN_POINT('Ctrl Pts',(84.9773441433861,4.56879612168285,336.825955882518));
#34168=CARTESIAN_POINT('Ctrl Pts',(84.9695954528285,4.61614787397732,336.697162887903));
#34169=CARTESIAN_POINT('Ctrl Pts',(84.9618483744506,4.66348977434427,336.568396689745));
#34170=CARTESIAN_POINT('Ctrl Pts',(84.9541012960727,4.70545175588497,336.437615447661));
#34171=CARTESIAN_POINT('Ctrl Pts',(84.9463542176949,4.74187205098695,336.305309355888));
#34172=CARTESIAN_POINT('Ctrl Pts',(84.9386070743891,4.77829265132606,336.173002155262));
#34173=CARTESIAN_POINT('Ctrl Pts',(84.9308599310833,4.80917136885059,336.039170456314));
#34174=CARTESIAN_POINT('Ctrl Pts',(84.9231127877775,4.83439670777787,335.904318270481));
#34175=CARTESIAN_POINT('Ctrl Pts',(84.9153639027494,4.85962771789688,335.769435767015));
#34176=CARTESIAN_POINT('Ctrl Pts',(84.9076150177213,4.87920274841558,335.633532704265));
#34177=CARTESIAN_POINT('Ctrl Pts',(84.8998661326932,4.89306174741782,335.497121512768));
#34178=CARTESIAN_POINT('Ctrl Pts',(84.8921090229185,4.90693545650481,335.360565533023));
#34179=CARTESIAN_POINT('Ctrl Pts',(84.8843519131438,4.91508097499322,335.223500736649));
#34180=CARTESIAN_POINT('Ctrl Pts',(84.876594803369,4.91749027394364,335.086443439136));
#34181=CARTESIAN_POINT('Ctrl Pts',(84.8688335484429,4.91990086034638,334.949312902586));
#34182=CARTESIAN_POINT('Ctrl Pts',(84.8610722935167,4.91656912890944,334.812190263442));
#34183=CARTESIAN_POINT('Ctrl Pts',(84.8533110385905,4.90753915858057,334.675589042265));
#34184=CARTESIAN_POINT('Ctrl Pts',(84.8455373681859,4.89849474324204,334.538769303653));
#34185=CARTESIAN_POINT('Ctrl Pts',(84.8377636977812,4.88373391600003,334.40247303859));
#34186=CARTESIAN_POINT('Ctrl Pts',(84.8299900273765,4.86335245821817,334.26720676201));
#34187=CARTESIAN_POINT('Ctrl Pts',(84.8225782231995,4.8439197621996,334.138237163149));
#34188=CARTESIAN_POINT('Ctrl Pts',(84.8151664190224,4.81937799441778,334.010204101482));
#34189=CARTESIAN_POINT('Ctrl Pts',(84.8077546148453,4.78985243985645,333.883533848744));
#34190=CARTESIAN_POINT('Ctrl Pts',(84.7999795360669,4.75887974991389,333.750655109587));
#34191=CARTESIAN_POINT('Ctrl Pts',(84.7922044572885,4.72232450054317,333.618856226485));
#34192=CARTESIAN_POINT('Ctrl Pts',(84.78442937851,4.68027575420729,333.48864235633));
#34193=CARTESIAN_POINT('Ctrl Pts',(84.776663867461,4.63827875153073,333.358588722632));
#34194=CARTESIAN_POINT('Ctrl Pts',(84.768898356412,4.590801821511,333.230116589432));
#34195=CARTESIAN_POINT('Ctrl Pts',(84.761132845363,4.53798492942499,333.103720526185));
#34196=CARTESIAN_POINT('Ctrl Pts',(84.7533750338408,4.4852204054413,332.977449785003));
#34197=CARTESIAN_POINT('Ctrl Pts',(84.7456172223186,4.4271266056553,332.853251375715));
#34198=CARTESIAN_POINT('Ctrl Pts',(84.7378594107964,4.36389304319397,332.73160396534));
#34199=CARTESIAN_POINT('Ctrl Pts',(84.7301074372734,4.30070706599365,332.610048098499));
#34200=CARTESIAN_POINT('Ctrl Pts',(84.7223554637504,4.2323892044065,332.491039754908));
#34201=CARTESIAN_POINT('Ctrl Pts',(84.7146034902274,4.15917660124078,332.375036559837));
#34202=CARTESIAN_POINT('Ctrl Pts',(84.7068547996698,4.08599500365597,332.259082492188));
#34203=CARTESIAN_POINT('Ctrl Pts',(84.6991061091121,4.00792299557914,332.146131371644));
#34204=CARTESIAN_POINT('Ctrl Pts',(84.6913574185545,3.92524296893848,332.036614993407));
#34205=CARTESIAN_POINT('Ctrl Pts',(84.6836103401767,3.84258014456792,331.927121400968));
#34206=CARTESIAN_POINT('Ctrl Pts',(84.6758632617989,3.75531144399371,331.821061441153));
#34207=CARTESIAN_POINT('Ctrl Pts',(84.668116183421,3.66376154027064,331.718836420028));
#34208=CARTESIAN_POINT('Ctrl Pts',(84.6603690401152,3.57221086927126,331.616610542159));
#34209=CARTESIAN_POINT('Ctrl Pts',(84.6526218968095,3.47637918432452,331.518219958262));
#34210=CARTESIAN_POINT('Ctrl Pts',(84.6448747535037,3.37662998263609,331.424031177029));
#34211=CARTESIAN_POINT('Ctrl Pts',(84.6371258684756,3.27685835520939,331.329821220157));
#34212=CARTESIAN_POINT('Ctrl Pts',(84.6293769834474,3.17316774260688,331.239815214009));
#34213=CARTESIAN_POINT('Ctrl Pts',(84.6216280984194,3.06595656106129,331.154340963088));
#34214=CARTESIAN_POINT('Ctrl Pts',(84.6138709886446,2.95863158445983,331.068775988913));
#34215=CARTESIAN_POINT('Ctrl Pts',(84.6061138788699,2.84777888048379,330.987752622545));
#34216=CARTESIAN_POINT('Ctrl Pts',(84.5983567690952,2.73382828492385,330.911557023627));
#34217=CARTESIAN_POINT('Ctrl Pts',(84.590595514169,2.61981679780916,330.835320708218));
#34218=CARTESIAN_POINT('Ctrl Pts',(84.5828342592429,2.50270445411489,330.763917504127));
#34219=CARTESIAN_POINT('Ctrl Pts',(84.5750730043167,2.38294693788354,330.697588239867));
#34220=CARTESIAN_POINT('Ctrl Pts',(84.567299333912,2.2629978486551,330.631152870401));
#34221=CARTESIAN_POINT('Ctrl Pts',(84.5595256635074,2.14039548101372,330.569807835234));
#34222=CARTESIAN_POINT('Ctrl Pts',(84.5517519931027,2.01561760696511,330.513746694067));
#34223=CARTESIAN_POINT('Ctrl Pts',(84.5443401889256,1.89664817297303,330.46029521251));
#34224=CARTESIAN_POINT('Ctrl Pts',(84.5369283847485,1.77570148119809,330.411646872409));
#34225=CARTESIAN_POINT('Ctrl Pts',(84.5295165805714,1.65320379152928,330.367926999045));
#34226=CARTESIAN_POINT('Ctrl Pts',(84.521741501793,1.52470212518811,330.322064284453));
#34227=CARTESIAN_POINT('Ctrl Pts',(84.5139664230146,1.39408748960774,330.281480435256));
#34228=CARTESIAN_POINT('Ctrl Pts',(84.5061913442361,1.26183287880432,330.24637392631));
#34229=CARTESIAN_POINT('Ctrl Pts',(84.4984258331871,1.12974101571923,330.211310618157));
#34230=CARTESIAN_POINT('Ctrl Pts',(84.4906603221381,0.99601356701873,330.181711338482));
#34231=CARTESIAN_POINT('Ctrl Pts',(84.482894811089,0.861142169952539,330.157726027409));
#34232=CARTESIAN_POINT('Ctrl Pts',(84.4751369995668,0.726404498269299,330.133764497842));
#34233=CARTESIAN_POINT('Ctrl Pts',(84.4673791880446,0.590525517755629,330.115405927689));
#34234=CARTESIAN_POINT('Ctrl Pts',(84.4596213765224,0.454010306148653,330.102749985511));
#34235=CARTESIAN_POINT('Ctrl Pts',(84.4518694029994,0.317597826567557,330.090103567331));
#34236=CARTESIAN_POINT('Ctrl Pts',(84.4441174294764,0.180550456527649,330.083151271223));
#34237=CARTESIAN_POINT('Ctrl Pts',(84.4363654559534,0.0433813544616911,
330.081941326033));
#34238=CARTESIAN_POINT('Ctrl Pts',(84.4286167653958,-0.093729656408104,
330.080731893255));
#34239=CARTESIAN_POINT('Ctrl Pts',(84.4208680748382,-0.23096190672186,330.085259977979));
#34240=CARTESIAN_POINT('Ctrl Pts',(84.4131193842805,-0.367799472204802,
330.09552177997));
#34241=CARTESIAN_POINT('Ctrl Pts',(84.4053723059027,-0.504608567489355,
330.105781446908));
#34242=CARTESIAN_POINT('Ctrl Pts',(84.3976252275249,-0.641022751745491,
330.121772429041));
#34243=CARTESIAN_POINT('Ctrl Pts',(84.389878149147,-0.776528858921388,330.143438871613));
#34244=CARTESIAN_POINT('Ctrl Pts',(84.3821310058412,-0.91203610176898,330.16510549577));
#34245=CARTESIAN_POINT('Ctrl Pts',(84.3743838625354,-1.04663486638488,330.192447613524));
#34246=CARTESIAN_POINT('Ctrl Pts',(84.3666367192296,-1.17982023859552,330.225357891203));
#34247=CARTESIAN_POINT('Ctrl Pts',(84.3588878342015,-1.31303555370516,330.258275567811));
#34248=CARTESIAN_POINT('Ctrl Pts',(84.3511389491734,-1.4448364647144,330.29676380162));
#34249=CARTESIAN_POINT('Ctrl Pts',(84.3433900641453,-1.5747317079378,330.340664949747));
#34250=CARTESIAN_POINT('Ctrl Pts',(84.3356329543706,-1.70476482331461,330.384612695006));
#34251=CARTESIAN_POINT('Ctrl Pts',(84.3278758445958,-1.83288785949952,330.433984706057));
#34252=CARTESIAN_POINT('Ctrl Pts',(84.3201187348211,-1.9586275699325,330.488574382216));
#34253=CARTESIAN_POINT('Ctrl Pts',(84.3123574798949,-2.08443447164635,330.543193229352));
#34254=CARTESIAN_POINT('Ctrl Pts',(84.3045962249688,-2.20785515836516,330.603035126798));
#34255=CARTESIAN_POINT('Ctrl Pts',(84.2968349700426,-2.32844051547162,330.667847206248));
#34256=CARTESIAN_POINT('Ctrl Pts',(84.289061299638,-2.44921876985078,330.732762963903));
#34257=CARTESIAN_POINT('Ctrl Pts',(84.2812876292333,-2.5671522947151,330.802664591954));
#34258=CARTESIAN_POINT('Ctrl Pts',(84.2735139588286,-2.68181977173455,330.877255067988));
#34259=CARTESIAN_POINT('Ctrl Pts',(84.2661021546516,-2.79114945011089,330.948373339417));
#34260=CARTESIAN_POINT('Ctrl Pts',(84.2586903504745,-2.89751007200662,331.023753584545));
#34261=CARTESIAN_POINT('Ctrl Pts',(84.2512785462974,-3.00056557503607,331.103105173037));
#34262=CARTESIAN_POINT('Ctrl Pts',(84.2435911514805,-3.10745295642346,331.185407265149));
#34263=CARTESIAN_POINT('Ctrl Pts',(84.2359037566636,-3.21113912003713,331.272254895859));
#34264=CARTESIAN_POINT('Ctrl Pts',(84.2282163618467,-3.31120629745287,331.363367503004));
#34265=CARTESIAN_POINT('Ctrl Pts',(84.2205384662962,-3.41114982247456,331.454367522862));
#34266=CARTESIAN_POINT('Ctrl Pts',(84.2128605707456,-3.50748296219958,331.549621770662));
#34267=CARTESIAN_POINT('Ctrl Pts',(84.2051826751951,-3.59981823082209,331.648807411153));
#34268=CARTESIAN_POINT('Ctrl Pts',(84.1975123291306,-3.69206270844377,331.747895524842));
#34269=CARTESIAN_POINT('Ctrl Pts',(84.1898419830661,-3.78031686356381,331.850907050325));
#34270=CARTESIAN_POINT('Ctrl Pts',(84.1821716370016,-3.86422790263018,331.957480356837));
#34271=CARTESIAN_POINT('Ctrl Pts',(84.1744368291485,-3.94884413226014,332.0649493082));
#34272=CARTESIAN_POINT('Ctrl Pts',(84.1667020212954,-4.02904359458647,332.176039916274));
#34273=CARTESIAN_POINT('Ctrl Pts',(84.1589672134423,-4.10450368599915,332.290344569116));
#34274=CARTESIAN_POINT('Ctrl Pts',(84.151305538029,-4.17925030389098,332.403568473955));
#34275=CARTESIAN_POINT('Ctrl Pts',(84.1436438626156,-4.2493465680269,332.519945562008));
#34276=CARTESIAN_POINT('Ctrl Pts',(84.1359821872023,-4.31452095120334,332.639048491788));
#34277=CARTESIAN_POINT('Ctrl Pts',(84.1283217735525,-4.37968460113241,332.758131807095));
#34278=CARTESIAN_POINT('Ctrl Pts',(84.1206613599026,-4.43992778997178,332.879939720091));
#34279=CARTESIAN_POINT('Ctrl Pts',(84.1130009462528,-4.4950242715391,333.004019073043));
#34280=CARTESIAN_POINT('Ctrl Pts',(84.1053400457857,-4.55012425447306,333.128106311205));
#34281=CARTESIAN_POINT('Ctrl Pts',(84.0976791453187,-4.60007671776464,333.254464910044));
#34282=CARTESIAN_POINT('Ctrl Pts',(84.0900182448516,-4.64470322883895,333.382620953977));
#34283=CARTESIAN_POINT('Ctrl Pts',(84.0822280784912,-4.69008274353803,333.51293943372));
#34284=CARTESIAN_POINT('Ctrl Pts',(84.0744379121308,-4.7299547920782,333.645116164544));
#34285=CARTESIAN_POINT('Ctrl Pts',(84.0666477457704,-4.76418464552896,333.778636939397));
#34286=CARTESIAN_POINT('Ctrl Pts',(84.0589769385894,-4.79789003685257,333.910111938924));
#34287=CARTESIAN_POINT('Ctrl Pts',(84.0513061314085,-4.8261248771364,334.042889681328));
#34288=CARTESIAN_POINT('Ctrl Pts',(84.0436353242275,-4.84881237358444,334.176470019808));
#34289=CARTESIAN_POINT('Ctrl Pts',(84.0357854782774,-4.87202940249804,334.313168160473));
#34290=CARTESIAN_POINT('Ctrl Pts',(84.0279356323272,-4.88943688677875,334.450706378763));
#34291=CARTESIAN_POINT('Ctrl Pts',(84.0200857863771,-4.9010088882587,334.588545336994));
#34292=CARTESIAN_POINT('Ctrl Pts',(84.012235940427,-4.91258088973864,334.726384295226));
#34293=CARTESIAN_POINT('Ctrl Pts',(84.0043860944769,-4.9183174533213,334.864523548469));
#34294=CARTESIAN_POINT('Ctrl Pts',(83.9965362485268,-4.91824940115574,335.002427041656));
#34295=CARTESIAN_POINT('',(87.4965362485424,-4.91824854721736,334.996219749433));
#34296=CARTESIAN_POINT('Ctrl Pts',(87.4965362484899,-4.91824854721807,334.996219750363));
#34297=CARTESIAN_POINT('Ctrl Pts',(87.4887898181956,-4.9183540119818,335.133433418973));
#34298=CARTESIAN_POINT('Ctrl Pts',(87.4810433879014,-4.9127130140224,335.27071194917));
#34299=CARTESIAN_POINT('Ctrl Pts',(87.4732969576071,-4.90133605169373,335.407538919451));
#34300=CARTESIAN_POINT('Ctrl Pts',(87.4655516439243,-4.88996072930072,335.544346166768));
#34301=CARTESIAN_POINT('Ctrl Pts',(87.4578063302416,-4.8728511191656,335.68070159468));
#34302=CARTESIAN_POINT('Ctrl Pts',(87.4500610165588,-4.85006973752551,335.816092276424));
#34303=CARTESIAN_POINT('Ctrl Pts',(87.4423151479825,-4.82728672377053,335.951492657894));
#34304=CARTESIAN_POINT('Ctrl Pts',(87.4345692794062,-4.79883119428449,336.085927770556));
#34305=CARTESIAN_POINT('Ctrl Pts',(87.4268234108299,-4.76481702747752,336.218893661137));
#34306=CARTESIAN_POINT('Ctrl Pts',(87.4190753158446,-4.73079308391719,336.351897770345));
#34307=CARTESIAN_POINT('Ctrl Pts',(87.4113272208593,-4.69120742003832,336.483431438911));
#34308=CARTESIAN_POINT('Ctrl Pts',(87.403579125874,-4.64622402945685,336.613005062174));
#34309=CARTESIAN_POINT('Ctrl Pts',(87.3958220968729,-4.60118877034202,336.742728091555));
#34310=CARTESIAN_POINT('Ctrl Pts',(87.3880650678718,-4.55074348051424,336.870486191809));
#34311=CARTESIAN_POINT('Ctrl Pts',(87.3803080388706,-4.49510087465192,336.995808404934));
#34312=CARTESIAN_POINT('Ctrl Pts',(87.372546455652,-4.43942560054399,337.121204195792));
#34313=CARTESIAN_POINT('Ctrl Pts',(87.3647848724334,-4.37854710396342,337.244160900628));
#34314=CARTESIAN_POINT('Ctrl Pts',(87.3570232892148,-4.31272402621819,337.364232335491));
#34315=CARTESIAN_POINT('Ctrl Pts',(87.3492487195698,-4.24679081545928,337.484504669938));
#34316=CARTESIAN_POINT('Ctrl Pts',(87.3414741499249,-4.17589669410478,337.601881753829));
#34317=CARTESIAN_POINT('Ctrl Pts',(87.33369958028,-4.10034408335858,337.715945776441));
#34318=CARTESIAN_POINT('Ctrl Pts',(87.3264320279569,-4.02971862409632,337.822571131973));
#34319=CARTESIAN_POINT('Ctrl Pts',(87.3191644756338,-3.95502304272049,337.926301559397));
#34320=CARTESIAN_POINT('Ctrl Pts',(87.3118969233108,-3.87653494268447,338.026823400968));
#34321=CARTESIAN_POINT('Ctrl Pts',(87.3041218445323,-3.79256565924173,338.134365143005));
#34322=CARTESIAN_POINT('Ctrl Pts',(87.2963467657539,-3.70398520819931,338.238579995768));
#34323=CARTESIAN_POINT('Ctrl Pts',(87.2885716869754,-3.6110867843188,338.339047064451));
#34324=CARTESIAN_POINT('Ctrl Pts',(87.2808061759264,-3.51830267786327,338.439390502009));
#34325=CARTESIAN_POINT('Ctrl Pts',(87.2730406648774,-3.42121143382314,338.535995047575));
#34326=CARTESIAN_POINT('Ctrl Pts',(87.2652751538284,-3.32014798085434,338.628470813956));
#34327=CARTESIAN_POINT('Ctrl Pts',(87.2575173423062,-3.21918473259312,338.720854890346));
#34328=CARTESIAN_POINT('Ctrl Pts',(87.249759530784,-3.1142573996672,338.809118072073));
#34329=CARTESIAN_POINT('Ctrl Pts',(87.2420017192618,-3.0057391806178,338.892905732303));
#34330=CARTESIAN_POINT('Ctrl Pts',(87.2342497457388,-2.89730262496962,338.976630339662));
#34331=CARTESIAN_POINT('Ctrl Pts',(87.2264977722158,-2.78528087004586,339.055885891391));
#34332=CARTESIAN_POINT('Ctrl Pts',(87.2187457986928,-2.67008148311988,339.130356877559));
#34333=CARTESIAN_POINT('Ctrl Pts',(87.2109971081352,-2.55493088320274,339.20479632522));
#34334=CARTESIAN_POINT('Ctrl Pts',(87.2032484175775,-2.43660565541755,339.274455025661));
#34335=CARTESIAN_POINT('Ctrl Pts',(87.1954997270199,-2.31554356265198,339.339059929519));
#34336=CARTESIAN_POINT('Ctrl Pts',(87.1877526486421,-2.1945066578662,339.403651391788));
#34337=CARTESIAN_POINT('Ctrl Pts',(87.1800055702643,-2.07073436535895,339.463190965043));
#34338=CARTESIAN_POINT('Ctrl Pts',(87.1722584918865,-1.94468999186234,339.517451039917));
#34339=CARTESIAN_POINT('Ctrl Pts',(87.1645113485807,-1.81864456199213,339.571711569544));
#34340=CARTESIAN_POINT('Ctrl Pts',(87.1567642052748,-1.69032737217248,339.620692357984));
#34341=CARTESIAN_POINT('Ctrl Pts',(87.149017061969,-1.5602223250501,339.664213691386));
#34342=CARTESIAN_POINT('Ctrl Pts',(87.1412681769409,-1.43008802755092,339.707744809308));
#34343=CARTESIAN_POINT('Ctrl Pts',(87.1335192919128,-1.29816544352934,339.745813905828));
#34344=CARTESIAN_POINT('Ctrl Pts',(87.1257704068847,-1.16495388577462,339.778291065488));
#34345=CARTESIAN_POINT('Ctrl Pts',(87.11801329711,-1.03160093589634,339.810802696741));
#34346=CARTESIAN_POINT('Ctrl Pts',(87.1102561873352,-0.896956659667793,
339.837710442007));
#34347=CARTESIAN_POINT('Ctrl Pts',(87.1024990775605,-0.761531368509716,
339.858935381056));
#34348=CARTESIAN_POINT('Ctrl Pts',(87.0947378226343,-0.626033710406198,
339.880171662034));
#34349=CARTESIAN_POINT('Ctrl Pts',(87.0869765677082,-0.489754593925044,
339.895719041593));
#34350=CARTESIAN_POINT('Ctrl Pts',(87.079215312782,-0.353208724307071,339.905550596984));
#34351=CARTESIAN_POINT('Ctrl Pts',(87.0714416423774,-0.216444425797904,
339.91539787966));
#34352=CARTESIAN_POINT('Ctrl Pts',(87.0636679719727,-0.0794129123466384,
339.9195110551));
#34353=CARTESIAN_POINT('Ctrl Pts',(87.055894301568,0.0573709434497541,339.917915375171));
#34354=CARTESIAN_POINT('Ctrl Pts',(87.048482497391,0.187787477849971,339.916393974527));
#34355=CARTESIAN_POINT('Ctrl Pts',(87.0410706932139,0.317978605226491,339.909683266813));
#34356=CARTESIAN_POINT('Ctrl Pts',(87.0336588890369,0.447504879302989,339.897848756903));
#34357=CARTESIAN_POINT('Ctrl Pts',(87.0258838102584,0.583379621911605,339.88543420241));
#34358=CARTESIAN_POINT('Ctrl Pts',(87.01810873148,0.71895207973114,339.867341648025));
#34359=CARTESIAN_POINT('Ctrl Pts',(87.0103336527016,0.853709648829552,339.843589877146));
#34360=CARTESIAN_POINT('Ctrl Pts',(87.0025681416526,0.988301390159919,339.819867334334));
#34361=CARTESIAN_POINT('Ctrl Pts',(86.9948026306035,1.12207985673796,339.790499498643));
#34362=CARTESIAN_POINT('Ctrl Pts',(86.9870371195545,1.25453593499316,339.755557028394));
#34363=CARTESIAN_POINT('Ctrl Pts',(86.9792793080324,1.38686068266104,339.720649203707));
#34364=CARTESIAN_POINT('Ctrl Pts',(86.9715214965101,1.51786527576267,339.680177843096));
#34365=CARTESIAN_POINT('Ctrl Pts',(86.963763684988,1.64704954188327,339.634264868248));
#34366=CARTESIAN_POINT('Ctrl Pts',(86.956011711465,1.77613659274712,339.58838644437));
#34367=CARTESIAN_POINT('Ctrl Pts',(86.9482597379419,1.90340567643511,339.537074687499));
#34368=CARTESIAN_POINT('Ctrl Pts',(86.9405077644189,2.02837091587768,339.480501589122));
#34369=CARTESIAN_POINT('Ctrl Pts',(86.9327590738613,2.15328323246706,339.423952449485));
#34370=CARTESIAN_POINT('Ctrl Pts',(86.9250103833037,2.27589329002514,339.362146560906));
#34371=CARTESIAN_POINT('Ctrl Pts',(86.9172616927461,2.39573457690208,339.29530428486));
#34372=CARTESIAN_POINT('Ctrl Pts',(86.9095146143682,2.51555092979835,339.228475915907));
#34373=CARTESIAN_POINT('Ctrl Pts',(86.9017675359904,2.63259931669743,339.15661343404));
#34374=CARTESIAN_POINT('Ctrl Pts',(86.8940204576126,2.74643761417148,339.079983271285));
#34375=CARTESIAN_POINT('Ctrl Pts',(86.8862733143068,2.86027686572018,339.003352466295));
#34376=CARTESIAN_POINT('Ctrl Pts',(86.8785261710009,2.97090564992886,338.921954118991));
#34377=CARTESIAN_POINT('Ctrl Pts',(86.8707790276951,3.07791097409765,338.836097899954));
#34378=CARTESIAN_POINT('Ctrl Pts',(86.863030142667,3.18494035533518,338.750222378616));
#34379=CARTESIAN_POINT('Ctrl Pts',(86.8552812576389,3.28834435069716,338.659887235798));
#34380=CARTESIAN_POINT('Ctrl Pts',(86.8475323726108,3.38774350470389,338.565442049569));
#34381=CARTESIAN_POINT('Ctrl Pts',(86.8397752628361,3.48724816199954,338.470896618244));
#34382=CARTESIAN_POINT('Ctrl Pts',(86.8320181530613,3.58273920279971,338.372232698784));
#34383=CARTESIAN_POINT('Ctrl Pts',(86.8242610432866,3.67387410260758,338.269836714683));
#34384=CARTESIAN_POINT('Ctrl Pts',(86.8164997883604,3.76505770199198,338.167386013443));
#34385=CARTESIAN_POINT('Ctrl Pts',(86.8087385334343,3.8518802747747,338.061199576194));
#34386=CARTESIAN_POINT('Ctrl Pts',(86.8009772785081,3.93404064450069,337.951695660111));
#34387=CARTESIAN_POINT('Ctrl Pts',(86.7932036081034,4.01633244404224,337.842016573449));
#34388=CARTESIAN_POINT('Ctrl Pts',(86.7854299376988,4.09394691581605,337.729009725593));
#34389=CARTESIAN_POINT('Ctrl Pts',(86.7776562672941,4.16662666754909,337.613121749129));
#34390=CARTESIAN_POINT('Ctrl Pts',(86.7702444631171,4.23592315935297,337.50262838585));
#34391=CARTESIAN_POINT('Ctrl Pts',(86.76283265894,4.3007338714579,337.389516340328));
#34392=CARTESIAN_POINT('Ctrl Pts',(86.7554208547629,4.36087607871603,337.274190600759));
#34393=CARTESIAN_POINT('Ctrl Pts',(86.7476457759845,4.4239660347065,337.153212403156));
#34394=CARTESIAN_POINT('Ctrl Pts',(86.739870697206,4.48211765580835,337.029415711736));
#34395=CARTESIAN_POINT('Ctrl Pts',(86.7320956184276,4.53506933798152,336.903241750856));
#34396=CARTESIAN_POINT('Ctrl Pts',(86.7243301073786,4.58795585973866,336.777223055067));
#34397=CARTESIAN_POINT('Ctrl Pts',(86.7165645963296,4.63565502464282,336.648833267464));
#34398=CARTESIAN_POINT('Ctrl Pts',(86.7087990852806,4.67795074021808,336.518538749783));
#34399=CARTESIAN_POINT('Ctrl Pts',(86.7010412737584,4.72020451946815,336.388373419496));
#34400=CARTESIAN_POINT('Ctrl Pts',(86.6932834622363,4.75706539128104,336.256307486823));
#34401=CARTESIAN_POINT('Ctrl Pts',(86.6855256507141,4.78836521021092,336.122827536241));
#34402=CARTESIAN_POINT('Ctrl Pts',(86.6777736771911,4.8196414750345,335.989448033555));
#34403=CARTESIAN_POINT('Ctrl Pts',(86.670021703668,4.84536492787493,335.854657010004));
#34404=CARTESIAN_POINT('Ctrl Pts',(86.662269730145,4.86541726408165,335.718956124445));
#34405=CARTESIAN_POINT('Ctrl Pts',(86.6545210395874,4.88546110811208,335.583312708291));
#34406=CARTESIAN_POINT('Ctrl Pts',(86.6467723490298,4.89983855534358,335.446760582388));
#34407=CARTESIAN_POINT('Ctrl Pts',(86.6390236584722,4.90848245621954,335.309811296574));
#34408=CARTESIAN_POINT('Ctrl Pts',(86.6312765800944,4.91712455865974,335.172890504203));
#34409=CARTESIAN_POINT('Ctrl Pts',(86.6235295017166,4.92003546292459,335.035573106135));
#34410=CARTESIAN_POINT('Ctrl Pts',(86.6157824233388,4.91719995903452,334.898375075051));
#34411=CARTESIAN_POINT('Ctrl Pts',(86.608035280033,4.9143644313802,334.761175894115));
#34412=CARTESIAN_POINT('Ctrl Pts',(86.6002881367271,4.90578240758793,334.62409647295));
#34413=CARTESIAN_POINT('Ctrl Pts',(86.5925409934213,4.8914908022096,334.487651686449));
#34414=CARTESIAN_POINT('Ctrl Pts',(86.5847921083932,4.87719598377492,334.351176224262));
#34415=CARTESIAN_POINT('Ctrl Pts',(86.5770432233652,4.85718907017415,334.215336069327));
#34416=CARTESIAN_POINT('Ctrl Pts',(86.569294338337,4.83155868393009,334.080639490602));
#34417=CARTESIAN_POINT('Ctrl Pts',(86.5615372285623,4.80590109332929,333.945799943538));
#34418=CARTESIAN_POINT('Ctrl Pts',(86.5537801187876,4.77460818000428,333.812106781963));
#34419=CARTESIAN_POINT('Ctrl Pts',(86.5460230090128,4.73781953605724,333.680057157959));
#34420=CARTESIAN_POINT('Ctrl Pts',(86.5382617540867,4.70101123343516,333.547936970859));
#34421=CARTESIAN_POINT('Ctrl Pts',(86.5305004991605,4.6587014689758,333.417462442956));
#34422=CARTESIAN_POINT('Ctrl Pts',(86.5227392442344,4.61107898019732,333.289113182913));
#34423=CARTESIAN_POINT('Ctrl Pts',(86.5149655738297,4.56338031095693,333.160558605882));
#34424=CARTESIAN_POINT('Ctrl Pts',(86.507191903425,4.51035208589418,333.034136451029));
#34425=CARTESIAN_POINT('Ctrl Pts',(86.4994182330204,4.45223059814982,332.910304863527));
#34426=CARTESIAN_POINT('Ctrl Pts',(86.4920064288432,4.39681467964284,332.792237666214));
#34427=CARTESIAN_POINT('Ctrl Pts',(86.4845946246661,4.33676914258128,332.676525537529));
#34428=CARTESIAN_POINT('Ctrl Pts',(86.477182820489,4.27233566711696,332.563541297296));
#34429=CARTESIAN_POINT('Ctrl Pts',(86.4694077417106,4.2047441150831,332.445019362888));
#34430=CARTESIAN_POINT('Ctrl Pts',(86.4616326629321,4.13211001509869,332.329124930913));
#34431=CARTESIAN_POINT('Ctrl Pts',(86.4538575841537,4.05466283318189,332.216316761606));
#34432=CARTESIAN_POINT('Ctrl Pts',(86.4460920731047,3.97731095495308,332.103647409934));
#34433=CARTESIAN_POINT('Ctrl Pts',(86.4383265620557,3.89515799858936,331.994057083473));
#34434=CARTESIAN_POINT('Ctrl Pts',(86.4305610510067,3.80847919758504,331.887979874091));
#34435=CARTESIAN_POINT('Ctrl Pts',(86.4228032394845,3.72188633886409,331.782007840571));
#34436=CARTESIAN_POINT('Ctrl Pts',(86.4150454279623,3.63077681139094,331.67954229296));
#34437=CARTESIAN_POINT('Ctrl Pts',(86.4072876164401,3.5354688012825,331.580987947132));
#34438=CARTESIAN_POINT('Ctrl Pts',(86.3995356429171,3.44023251347452,331.482507766574));
#34439=CARTESIAN_POINT('Ctrl Pts',(86.3917836693941,3.34080430247368,331.387933209144));
#34440=CARTESIAN_POINT('Ctrl Pts',(86.3840316958711,3.23754200248008,331.297635236139));
#34441=CARTESIAN_POINT('Ctrl Pts',(86.3762830053135,3.13432343413148,331.207375504379));
#34442=CARTESIAN_POINT('Ctrl Pts',(86.3685343147559,3.02727429992282,331.121389011588));
#34443=CARTESIAN_POINT('Ctrl Pts',(86.3607856241982,2.91678843454769,331.040009054229));
#34444=CARTESIAN_POINT('Ctrl Pts',(86.3530385458204,2.80632555667973,330.95864602865));
#34445=CARTESIAN_POINT('Ctrl Pts',(86.3452914674426,2.69242768443144,330.881887863787));
#34446=CARTESIAN_POINT('Ctrl Pts',(86.3375443890648,2.57552047924526,330.81002657246));
#34447=CARTESIAN_POINT('Ctrl Pts',(86.329797245759,2.45861229426402,330.738164678867));
#34448=CARTESIAN_POINT('Ctrl Pts',(86.3220501024532,2.33869505903454,330.671199945355));
#34449=CARTESIAN_POINT('Ctrl Pts',(86.3143029591474,2.21622171942105,330.609379958039));
#34450=CARTESIAN_POINT('Ctrl Pts',(86.3065540741193,2.09372084520096,330.547546072278));
#34451=CARTESIAN_POINT('Ctrl Pts',(86.2988051890912,1.96866307194777,330.490859410412));
#34452=CARTESIAN_POINT('Ctrl Pts',(86.2910563040631,1.84152377260569,330.43952050137));
#34453=CARTESIAN_POINT('Ctrl Pts',(86.2832991942884,1.71424952629734,330.388127100678));
#34454=CARTESIAN_POINT('Ctrl Pts',(86.2755420845137,1.58488970352282,330.342092938058));
#34455=CARTESIAN_POINT('Ctrl Pts',(86.2677849747389,1.45393791137153,330.30156966505));
#34456=CARTESIAN_POINT('Ctrl Pts',(86.2600237198128,1.32291614276945,330.261024737701));
#34457=CARTESIAN_POINT('Ctrl Pts',(86.2522624648866,1.1903010874211,330.225996667599));
#34458=CARTESIAN_POINT('Ctrl Pts',(86.2445012099604,1.05659819518321,330.196586285106));
#34459=CARTESIAN_POINT('Ctrl Pts',(86.2367275395557,0.922681421891414,330.167128855585));
#34460=CARTESIAN_POINT('Ctrl Pts',(86.2289538691511,0.787673719436697,330.143307139255));
#34461=CARTESIAN_POINT('Ctrl Pts',(86.2211801987464,0.652088223646006,330.125170360814));
#34462=CARTESIAN_POINT('Ctrl Pts',(86.2137683945693,0.52281426530389,330.107877853773));
#34463=CARTESIAN_POINT('Ctrl Pts',(86.2063565903922,0.393015382166143,330.095752954512));
#34464=CARTESIAN_POINT('Ctrl Pts',(86.1989447862151,0.263135873376105,330.088794183233));
#34465=CARTESIAN_POINT('Ctrl Pts',(86.1911697074366,0.126890582969666,330.081494341846));
#34466=CARTESIAN_POINT('Ctrl Pts',(86.1833946286582,-0.0098739966229407,
330.07985677894));
#34467=CARTESIAN_POINT('Ctrl Pts',(86.1756195498798,-0.146647906903237,
330.083936793134));
#34468=CARTESIAN_POINT('Ctrl Pts',(86.1678540388307,-0.283253508179759,
330.088011786611));
#34469=CARTESIAN_POINT('Ctrl Pts',(86.1600885277817,-0.419868030332519,
330.097790346334));
#34470=CARTESIAN_POINT('Ctrl Pts',(86.1523230167327,-0.555977491612252,
330.113275934604));
#34471=CARTESIAN_POINT('Ctrl Pts',(86.1445652052104,-0.691951999965223,
330.128746168868));
#34472=CARTESIAN_POINT('Ctrl Pts',(86.1368073936882,-0.827422058137413,
330.149912126973));
#34473=CARTESIAN_POINT('Ctrl Pts',(86.129049582166,-0.961875143152225,330.176725254406));
#34474=CARTESIAN_POINT('Ctrl Pts',(86.121297608643,-1.09622704795599,330.20351820411));
#34475=CARTESIAN_POINT('Ctrl Pts',(86.1135456351199,-1.22956312112094,330.235949788236));
#34476=CARTESIAN_POINT('Ctrl Pts',(86.1057936615969,-1.36137776876012,330.273919844816));
#34477=CARTESIAN_POINT('Ctrl Pts',(86.0980449710393,-1.49313659281804,330.311873821054));
#34478=CARTESIAN_POINT('Ctrl Pts',(86.0902962804817,-1.62337489804639,330.35536149665));
#34479=CARTESIAN_POINT('Ctrl Pts',(86.082547589924,-1.75159928178674,330.404232053449));
#34480=CARTESIAN_POINT('Ctrl Pts',(86.0748005115462,-1.87979698737267,330.453092442321));
#34481=CARTESIAN_POINT('Ctrl Pts',(86.0670534331684,-2.00598123990152,330.507333345609));
#34482=CARTESIAN_POINT('Ctrl Pts',(86.0593063547906,-2.1296761297318,330.566754840419));
#34483=CARTESIAN_POINT('Ctrl Pts',(86.0515592114848,-2.25337205624465,330.626176833238));
#34484=CARTESIAN_POINT('Ctrl Pts',(86.043812068179,-2.37457822611672,330.690779334926));
#34485=CARTESIAN_POINT('Ctrl Pts',(86.0360649248732,-2.49284132390555,330.760315436695));
#34486=CARTESIAN_POINT('Ctrl Pts',(86.0283160398451,-2.61113100974916,330.829867171655));
#34487=CARTESIAN_POINT('Ctrl Pts',(86.020567154817,-2.72647596998999,330.904354515759));
#34488=CARTESIAN_POINT('Ctrl Pts',(86.0128182697889,-2.83845032399687,330.983486235465));
#34489=CARTESIAN_POINT('Ctrl Pts',(86.0050611600142,-2.9505435287403,331.062701946396));
#34490=CARTESIAN_POINT('Ctrl Pts',(85.9973040502395,-3.0592586609519,331.146571654304));
#34491=CARTESIAN_POINT('Ctrl Pts',(85.9895469404648,-3.16420107449538,331.234762341809));
#34492=CARTESIAN_POINT('Ctrl Pts',(85.9817856855386,-3.2691995659094,331.323000155597));
#34493=CARTESIAN_POINT('Ctrl Pts',(85.9740244306124,-3.37042103324849,331.415563286215));
#34494=CARTESIAN_POINT('Ctrl Pts',(85.9662631756862,-3.46750715819042,331.51208125519));
#34495=CARTESIAN_POINT('Ctrl Pts',(85.9584895052816,-3.5647485892919,331.608753621459));
#34496=CARTESIAN_POINT('Ctrl Pts',(85.9507158348769,-3.65784119330613,331.709393181121));
#34497=CARTESIAN_POINT('Ctrl Pts',(85.9429421644722,-3.74646588889447,331.813595065619));
#34498=CARTESIAN_POINT('Ctrl Pts',(85.9355303602952,-3.8309650835803,331.912946327322));
#34499=CARTESIAN_POINT('Ctrl Pts',(85.9281185561182,-3.91140279356588,332.015535498572));
#34500=CARTESIAN_POINT('Ctrl Pts',(85.9207067519412,-3.98753982748235,332.120988157936));
#34501=CARTESIAN_POINT('Ctrl Pts',(85.9128697277735,-4.06804489218859,332.232490704449));
#34502=CARTESIAN_POINT('Ctrl Pts',(85.9050327036058,-4.14399504332485,332.347546226307));
#34503=CARTESIAN_POINT('Ctrl Pts',(85.8971956794381,-4.21506351142011,332.465750079966));
#34504=CARTESIAN_POINT('Ctrl Pts',(85.8893685771602,-4.28604200486538,332.583804284269));
#34505=CARTESIAN_POINT('Ctrl Pts',(85.8815414748823,-4.35215091783572,332.70499856482));
#34506=CARTESIAN_POINT('Ctrl Pts',(85.8737143726044,-4.41310477941014,332.82889676237));
#34507=CARTESIAN_POINT('Ctrl Pts',(85.8658955767316,-4.47399395453352,332.952663474654));
#34508=CARTESIAN_POINT('Ctrl Pts',(85.8580767808588,-4.52973879828343,333.079128052298));
#34509=CARTESIAN_POINT('Ctrl Pts',(85.850257984986,-4.58009824184991,333.207827252327));
#34510=CARTESIAN_POINT('Ctrl Pts',(85.8424458860472,-4.63041455168176,333.336416219264));
#34511=CARTESIAN_POINT('Ctrl Pts',(85.8346337871083,-4.67535450466321,333.467235643882));
#34512=CARTESIAN_POINT('Ctrl Pts',(85.8268216881694,-4.71472404815442,333.599799938489));
#34513=CARTESIAN_POINT('Ctrl Pts',(85.8190150539567,-4.75406605182907,333.732271501608));
#34514=CARTESIAN_POINT('Ctrl Pts',(85.8112084197439,-4.78784529872874,333.866485137799));
#34515=CARTESIAN_POINT('Ctrl Pts',(85.8034017855312,-4.81591686631142,334.001937978241));
#34516=CARTESIAN_POINT('Ctrl Pts',(85.7955983371855,-4.84397697796038,334.137335540732));
#34517=CARTESIAN_POINT('Ctrl Pts',(85.7877948888398,-4.86633397110281,334.273970926373));
#34518=CARTESIAN_POINT('Ctrl Pts',(85.7799914404942,-4.88289356463374,334.41132904016));
#34519=CARTESIAN_POINT('Ctrl Pts',(85.7721889091132,-4.89945121228626,334.548671013323));
#34520=CARTESIAN_POINT('Ctrl Pts',(85.7643863777322,-4.91021276809882,334.686735166231));
#34521=CARTESIAN_POINT('Ctrl Pts',(85.7565838463512,-4.91513558701002,334.824999360551));
#34522=CARTESIAN_POINT('Ctrl Pts',(85.7532346470641,-4.91724868348893,334.884348604845));
#34523=CARTESIAN_POINT('Ctrl Pts',(85.7498854477771,-4.91828663521559,334.943734650103));
#34524=CARTESIAN_POINT('Ctrl Pts',(85.74653624849,-4.91824901287755,335.003116059853));
#34525=CARTESIAN_POINT('',(89.2465362484375,-4.9182497994862,334.998595594818));
#34526=CARTESIAN_POINT('Ctrl Pts',(89.2465362484374,-4.9182497994862,334.998595594818));
#34527=CARTESIAN_POINT('Ctrl Pts',(89.2388185931064,-4.91828848637337,335.134077703145));
#34528=CARTESIAN_POINT('Ctrl Pts',(89.2311009377755,-4.91272478676779,335.269786405984));
#34529=CARTESIAN_POINT('Ctrl Pts',(89.2233832824445,-4.90152866167626,335.405215795924));
#34530=CARTESIAN_POINT('Ctrl Pts',(89.2156749347033,-4.89034603925295,335.540481856309));
#34531=CARTESIAN_POINT('Ctrl Pts',(89.2079665869621,-4.87354453575443,335.675468881894));
#34532=CARTESIAN_POINT('Ctrl Pts',(89.2002582392209,-4.8511460915302,335.809669476472));
#34533=CARTESIAN_POINT('Ctrl Pts',(89.1925572764048,-4.82876910596853,335.943741501172));
#34534=CARTESIAN_POINT('Ctrl Pts',(89.1848563135887,-4.80080591281923,336.077028204597));
#34535=CARTESIAN_POINT('Ctrl Pts',(89.1771553507726,-4.76733033678951,336.209026270362));
#34536=CARTESIAN_POINT('Ctrl Pts',(89.1694598573305,-4.73387853576677,336.340930588528));
#34537=CARTESIAN_POINT('Ctrl Pts',(89.1617643638884,-4.6949222399672,336.471547706784));
#34538=CARTESIAN_POINT('Ctrl Pts',(89.1540688704463,-4.65058645635678,336.600383914706));
#34539=CARTESIAN_POINT('Ctrl Pts',(89.1463761327548,-4.60626654935861,336.729173986475));
#34540=CARTESIAN_POINT('Ctrl Pts',(89.1386833950633,-4.55657111265757,336.856184040658));
#34541=CARTESIAN_POINT('Ctrl Pts',(89.1309906573719,-4.50167509206021,336.980935240745));
#34542=CARTESIAN_POINT('Ctrl Pts',(89.1232990991992,-4.44678748860773,337.105667312871));
#34543=CARTESIAN_POINT('Ctrl Pts',(89.1156075410266,-4.38670104687227,337.228140856245));
#34544=CARTESIAN_POINT('Ctrl Pts',(89.1079159828539,-4.32163877281165,337.347897225142));
#34545=CARTESIAN_POINT('Ctrl Pts',(89.100223878242,-4.25657187646522,337.467662102014));
#34546=CARTESIAN_POINT('Ctrl Pts',(89.0925317736301,-4.18652863431924,337.584709071469));
#34547=CARTESIAN_POINT('Ctrl Pts',(89.0848396690182,-4.11177766731381,337.698604727832));
#34548=CARTESIAN_POINT('Ctrl Pts',(89.0771452919303,-4.03700461665441,337.812534032353));
#34549=CARTESIAN_POINT('Ctrl Pts',(89.0694509148424,-3.95752129254295,337.923309840099));
#34550=CARTESIAN_POINT('Ctrl Pts',(89.0617565377545,-3.8736389428185,338.030528733271));
#34551=CARTESIAN_POINT('Ctrl Pts',(89.0540538399741,-3.78966588279575,338.137863572859));
#34552=CARTESIAN_POINT('Ctrl Pts',(89.0463511421937,-3.70128454467609,338.241633505582));
#34553=CARTESIAN_POINT('Ctrl Pts',(89.0386484444133,-3.60884591006726,338.341468877588));
#34554=CARTESIAN_POINT('Ctrl Pts',(89.0309410313895,-3.51635068870453,338.441365364296));
#34555=CARTESIAN_POINT('Ctrl Pts',(89.0232336183656,-3.41979350602721,338.537322214772));
#34556=CARTESIAN_POINT('Ctrl Pts',(89.0155262053418,-3.31956044271628,338.629008339706));
#34557=CARTESIAN_POINT('Ctrl Pts',(89.0078075361868,-3.21918099611152,338.720828365735));
#34558=CARTESIAN_POINT('Ctrl Pts',(89.0000888670318,-3.11511525407646,338.808364959282));
#34559=CARTESIAN_POINT('Ctrl Pts',(88.9923701978768,-3.00778077722667,338.891328546736));
#34560=CARTESIAN_POINT('Ctrl Pts',(88.988688508236,-2.95658383853328,338.930900936013));
#34561=CARTESIAN_POINT('Ctrl Pts',(88.9850068185952,-2.90464361958345,338.96943354904));
#34562=CARTESIAN_POINT('Ctrl Pts',(88.9813251289544,-2.85200747217322,339.0068986063));
#34563=CARTESIAN_POINT('Ctrl Pts',(88.9735500501759,-2.74084921804736,339.086018195416));
#34564=CARTESIAN_POINT('Ctrl Pts',(88.9657749713975,-2.62622044772756,339.160633722342));
#34565=CARTESIAN_POINT('Ctrl Pts',(88.957999892619,-2.50852224034851,339.230425419763));
#34566=CARTESIAN_POINT('Ctrl Pts',(88.95023438157,-2.39096886810684,339.300131234057));
#34567=CARTESIAN_POINT('Ctrl Pts',(88.942468870521,-2.27035390722286,339.365024832387));
#34568=CARTESIAN_POINT('Ctrl Pts',(88.934703359472,-2.14710959118182,339.424828071909));
#34569=CARTESIAN_POINT('Ctrl Pts',(88.9269455479498,-2.0239874722392,339.484572016345));
#34570=CARTESIAN_POINT('Ctrl Pts',(88.9191877364277,-1.89824153563803,339.53923547646));
#34571=CARTESIAN_POINT('Ctrl Pts',(88.9114299249055,-1.77033063597685,339.588585021749));
#34572=CARTESIAN_POINT('Ctrl Pts',(88.9036779513825,-1.64251599332369,339.637897429941));
#34573=CARTESIAN_POINT('Ctrl Pts',(88.8959259778595,-1.51253999366618,339.681903742773));
#34574=CARTESIAN_POINT('Ctrl Pts',(88.8881740043365,-1.38088327351996,339.720417825512));
#34575=CARTESIAN_POINT('Ctrl Pts',(88.8804253137788,-1.24928231007279,339.758915597515));
#34576=CARTESIAN_POINT('Ctrl Pts',(88.8726766232212,-1.11600241620032,339.791925656085));
#34577=CARTESIAN_POINT('Ctrl Pts',(88.8649279326636,-0.981541056781967,
339.819311176543));
#34578=CARTESIAN_POINT('Ctrl Pts',(88.8571808542858,-0.847107673172575,
339.846690999215));
#34579=CARTESIAN_POINT('Ctrl Pts',(88.8494337759079,-0.711493695729016,
339.868448533491));
#34580=CARTESIAN_POINT('Ctrl Pts',(88.8416866975301,-0.575208109283756,
339.884497793378));
#34581=CARTESIAN_POINT('Ctrl Pts',(88.8339395542243,-0.438921380633828,
339.900547187773));
#34582=CARTESIAN_POINT('Ctrl Pts',(88.8261924109185,-0.301963419947128,
339.910888166642));
#34583=CARTESIAN_POINT('Ctrl Pts',(88.8184452676127,-0.164849289197789,
339.915486524684));
#34584=CARTESIAN_POINT('Ctrl Pts',(88.8106963825846,-0.0277043322809359,
339.920085916535));
#34585=CARTESIAN_POINT('Ctrl Pts',(88.8029474975564,0.109596473985898,339.918940105389));
#34586=CARTESIAN_POINT('Ctrl Pts',(88.7951986125283,0.246537503609198,339.912067011128));
#34587=CARTESIAN_POINT('Ctrl Pts',(88.7874415027536,0.383623883856112,339.905186621694));
#34588=CARTESIAN_POINT('Ctrl Pts',(88.7796843929789,0.520349333637551,339.8925668254));
#34589=CARTESIAN_POINT('Ctrl Pts',(88.7719272832042,0.656202232561501,339.874277555954));
#34590=CARTESIAN_POINT('Ctrl Pts',(88.764166028278,0.792127726930809,339.855978513308));
#34591=CARTESIAN_POINT('Ctrl Pts',(88.7564047733518,0.927179356709075,339.832004029074));
#34592=CARTESIAN_POINT('Ctrl Pts',(88.7486435184257,1.06085612338519,339.802475127263));
#34593=CARTESIAN_POINT('Ctrl Pts',(88.740869848021,1.19474672932282,339.772898988832));
#34594=CARTESIAN_POINT('Ctrl Pts',(88.7330961776164,1.3272576992316,339.737750777714));
#34595=CARTESIAN_POINT('Ctrl Pts',(88.7253225072117,1.45790275785958,339.697201572333));
#34596=CARTESIAN_POINT('Ctrl Pts',(88.7179107030346,1.58246625757705,339.658539942217));
#34597=CARTESIAN_POINT('Ctrl Pts',(88.7104988988575,1.70533338173005,339.61496893066));
#34598=CARTESIAN_POINT('Ctrl Pts',(88.7030870946805,1.82610163012309,339.566676679924));
#34599=CARTESIAN_POINT('Ctrl Pts',(88.695312015902,1.95278909012011,339.516017482124));
#34600=CARTESIAN_POINT('Ctrl Pts',(88.6875369371236,2.07756708358183,339.460002446722));
#34601=CARTESIAN_POINT('Ctrl Pts',(88.6797618583451,2.19994966441851,339.398795805277));
#34602=CARTESIAN_POINT('Ctrl Pts',(88.6719963472961,2.32218164569796,339.337664482502));
#34603=CARTESIAN_POINT('Ctrl Pts',(88.6642308362471,2.44202373319648,339.271354438337));
#34604=CARTESIAN_POINT('Ctrl Pts',(88.6564653251981,2.55900812432425,339.20007862809));
#34605=CARTESIAN_POINT('Ctrl Pts',(88.6487075136759,2.67587652508809,339.128873488017));
#34606=CARTESIAN_POINT('Ctrl Pts',(88.6409497021537,2.78989253648785,339.052712582114));
#34607=CARTESIAN_POINT('Ctrl Pts',(88.6331918906315,2.90061154928129,338.971855448361));
#34608=CARTESIAN_POINT('Ctrl Pts',(88.6254399171085,3.01124724250583,338.891059162166));
#34609=CARTESIAN_POINT('Ctrl Pts',(88.6176879435855,3.11859056123512,338.805573912093));
#34610=CARTESIAN_POINT('Ctrl Pts',(88.6099359700625,3.22222488080447,338.715703147457));
#34611=CARTESIAN_POINT('Ctrl Pts',(88.6021872795049,3.32581531117823,338.625870443144));
#34612=CARTESIAN_POINT('Ctrl Pts',(88.5944385889473,3.42569957184146,338.531656173793));
#34613=CARTESIAN_POINT('Ctrl Pts',(88.5866898983897,3.52149339721162,338.433404624552));
#34614=CARTESIAN_POINT('Ctrl Pts',(88.5789428200118,3.61726729187633,338.335173517366));
#34615=CARTESIAN_POINT('Ctrl Pts',(88.571195741634,3.7089521713491,338.23290708078));
#34616=CARTESIAN_POINT('Ctrl Pts',(88.5634486632562,3.79620028727457,338.126986799044));
#34617=CARTESIAN_POINT('Ctrl Pts',(88.5557015199504,3.88344913442316,338.021065629594));
#34618=CARTESIAN_POINT('Ctrl Pts',(88.5479543766446,3.96626089534252,337.911490855614));
#34619=CARTESIAN_POINT('Ctrl Pts',(88.5402072333388,4.04432807647745,337.798677093256));
#34620=CARTESIAN_POINT('Ctrl Pts',(88.5324583483107,4.12241280877223,337.685837967969));
#34621=CARTESIAN_POINT('Ctrl Pts',(88.5247094632826,4.19575061632469,337.569758726638));
#34622=CARTESIAN_POINT('Ctrl Pts',(88.5169605782545,4.26407753353314,337.450882667636));
#34623=CARTESIAN_POINT('Ctrl Pts',(88.5092034684797,4.33247697363751,337.331880432357));
#34624=CARTESIAN_POINT('Ctrl Pts',(88.501446358705,4.39585470388412,337.210075788828));
#34625=CARTESIAN_POINT('Ctrl Pts',(88.4936892489303,4.45399266586829,337.085936814693));
#34626=CARTESIAN_POINT('Ctrl Pts',(88.4859279940041,4.51216169492042,336.96173150466));
#34627=CARTESIAN_POINT('Ctrl Pts',(88.4781667390779,4.5650852257885,336.835189738904));
#34628=CARTESIAN_POINT('Ctrl Pts',(88.4704054841518,4.61259391110388,336.706798310799));
#34629=CARTESIAN_POINT('Ctrl Pts',(88.4626318137471,4.66017859483271,336.578201498252));
#34630=CARTESIAN_POINT('Ctrl Pts',(88.4548581433424,4.70233100354491,336.447749482818));
#34631=CARTESIAN_POINT('Ctrl Pts',(88.4470844729378,4.73893184929582,336.315943764083));
#34632=CARTESIAN_POINT('Ctrl Pts',(88.4396726687607,4.77382891687134,336.190273633266));
#34633=CARTESIAN_POINT('Ctrl Pts',(88.4322608645836,4.80367957469933,336.063373272853));
#34634=CARTESIAN_POINT('Ctrl Pts',(88.4248490604065,4.82842421967145,335.935682968419));
#34635=CARTESIAN_POINT('Ctrl Pts',(88.4170739816281,4.85438167340417,335.801734181796));
#34636=CARTESIAN_POINT('Ctrl Pts',(88.4092989028497,4.87480196712811,335.666492755274));
#34637=CARTESIAN_POINT('Ctrl Pts',(88.4015238240712,4.88956023335252,335.530456206409));
#34638=CARTESIAN_POINT('Ctrl Pts',(88.3937583130222,4.90430033859078,335.394587059177));
#34639=CARTESIAN_POINT('Ctrl Pts',(88.3859928019732,4.91339223787285,335.257925121314));
#34640=CARTESIAN_POINT('Ctrl Pts',(88.3782272909242,4.91676185503624,335.120979020332));
#34641=CARTESIAN_POINT('Ctrl Pts',(88.370469479402,4.9201281312144,334.984168701809));
#34642=CARTESIAN_POINT('Ctrl Pts',(88.3627116678799,4.91778340662411,334.847075169103));
#34643=CARTESIAN_POINT('Ctrl Pts',(88.3549538563577,4.90970532871861,334.710212754504));
#34644=CARTESIAN_POINT('Ctrl Pts',(88.3472018828347,4.90163332982287,334.573453333212));
#34645=CARTESIAN_POINT('Ctrl Pts',(88.3394499093116,4.88783658841117,334.436925072465));
#34646=CARTESIAN_POINT('Ctrl Pts',(88.3316979357886,4.86834482197517,334.30114253467));
#34647=CARTESIAN_POINT('Ctrl Pts',(88.323949245231,4.84886131031385,334.16541750086));
#34648=CARTESIAN_POINT('Ctrl Pts',(88.3162005546733,4.82368762604653,334.030437947972));
#34649=CARTESIAN_POINT('Ctrl Pts',(88.3084518641157,4.79290533774092,333.896713325579));
#34650=CARTESIAN_POINT('Ctrl Pts',(88.3007047857379,4.76212945394752,333.763016525711));
#34651=CARTESIAN_POINT('Ctrl Pts',(88.2929577073601,4.72574737482395,333.630574517668));
#34652=CARTESIAN_POINT('Ctrl Pts',(88.2852106289822,4.68389171202491,333.499886173477));
#34653=CARTESIAN_POINT('Ctrl Pts',(88.2774634856764,4.64203569843513,333.369196733993));
#34654=CARTESIAN_POINT('Ctrl Pts',(88.2697163423706,4.59470612889139,333.240261359924));
#34655=CARTESIAN_POINT('Ctrl Pts',(88.2619691990648,4.54208526055444,333.113563001753));
#34656=CARTESIAN_POINT('Ctrl Pts',(88.2542203140368,4.48945256192923,332.986836159102));
#34657=CARTESIAN_POINT('Ctrl Pts',(88.2464714290087,4.43152634724096,332.862347694028));
#34658=CARTESIAN_POINT('Ctrl Pts',(88.2387225439806,4.36853654861631,332.740559475024));
#34659=CARTESIAN_POINT('Ctrl Pts',(88.2309654342059,4.30547989196838,332.618641988746));
#34660=CARTESIAN_POINT('Ctrl Pts',(88.2232083244311,4.23734909508655,332.499430821514));
#34661=CARTESIAN_POINT('Ctrl Pts',(88.2154512146564,4.16441977053293,332.383362646966));
#34662=CARTESIAN_POINT('Ctrl Pts',(88.2076899597302,4.09145147488014,332.267232449296));
#34663=CARTESIAN_POINT('Ctrl Pts',(88.199928704804,4.01367976371038,332.154248912699));
#34664=CARTESIAN_POINT('Ctrl Pts',(88.1921674498779,3.93142234837809,332.044817876818));
#34665=CARTESIAN_POINT('Ctrl Pts',(88.1843937794732,3.84903334798889,331.935211786943));
#34666=CARTESIAN_POINT('Ctrl Pts',(88.1766201090686,3.76214455219782,331.829169856289));
#34667=CARTESIAN_POINT('Ctrl Pts',(88.1688464386639,3.67111312915359,331.727063786834));
#34668=CARTESIAN_POINT('Ctrl Pts',(88.1614346344868,3.58431924075284,331.629710779477));
#34669=CARTESIAN_POINT('Ctrl Pts',(88.1540228303097,3.49375992416188,331.535935657913));
#34670=CARTESIAN_POINT('Ctrl Pts',(88.1466110261326,3.39977317025234,331.446026807454));
#34671=CARTESIAN_POINT('Ctrl Pts',(88.1388359473541,3.30117984556167,331.351711256411));
#34672=CARTESIAN_POINT('Ctrl Pts',(88.1310608685757,3.19850303740045,331.261352499728));
#34673=CARTESIAN_POINT('Ctrl Pts',(88.1232857897973,3.0920935459301,331.17532477644));
#34674=CARTESIAN_POINT('Ctrl Pts',(88.1155202787482,2.98581499811352,331.089402915741));
#34675=CARTESIAN_POINT('Ctrl Pts',(88.1077547676992,2.87581320740411,331.00780172743));
#34676=CARTESIAN_POINT('Ctrl Pts',(88.0999892566502,2.76247580266768,330.930858751263));
#34677=CARTESIAN_POINT('Ctrl Pts',(88.092231445128,2.64925077229818,330.853992064281));
#34678=CARTESIAN_POINT('Ctrl Pts',(88.0844736336059,2.53269703086678,330.781774616238));
#34679=CARTESIAN_POINT('Ctrl Pts',(88.0767158220837,2.41323499512445,330.714503538584));
#34680=CARTESIAN_POINT('Ctrl Pts',(88.0689638485607,2.29386285835253,330.647283084549));
#34681=CARTESIAN_POINT('Ctrl Pts',(88.0612118750377,2.17158712275385,330.585001782863));
#34682=CARTESIAN_POINT('Ctrl Pts',(88.0534599015147,2.04685657667291,330.527913102697));
#34683=CARTESIAN_POINT('Ctrl Pts',(88.0457112109571,1.92217885405213,330.47084859962));
#34684=CARTESIAN_POINT('Ctrl Pts',(88.0379625203995,1.7950487433436,330.418972506585));
#34685=CARTESIAN_POINT('Ctrl Pts',(88.0302138298419,1.66593879299465,330.372491923238));
#34686=CARTESIAN_POINT('Ctrl Pts',(88.022466751464,1.53685570504896,330.326021010565));
#34687=CARTESIAN_POINT('Ctrl Pts',(88.0147196730862,1.40579396434206,330.284943507005));
#34688=CARTESIAN_POINT('Ctrl Pts',(88.0069725947084,1.27324484678053,330.249417864867));
#34689=CARTESIAN_POINT('Ctrl Pts',(87.9992254514026,1.14069461832972,330.21389192499));
#34690=CARTESIAN_POINT('Ctrl Pts',(87.9914783080968,1.00665736570963,330.183918040532));
#34691=CARTESIAN_POINT('Ctrl Pts',(87.983731164791,0.87163784209063,330.159604299777));
#34692=CARTESIAN_POINT('Ctrl Pts',(87.9759822797629,0.736587963216725,330.135285092777));
#34693=CARTESIAN_POINT('Ctrl Pts',(87.9682333947348,0.600555758517896,330.116628630912));
#34694=CARTESIAN_POINT('Ctrl Pts',(87.9604845097067,0.464054052530329,330.103691502894));
#34695=CARTESIAN_POINT('Ctrl Pts',(87.952727399932,0.327407462221328,330.090740643275));
#34696=CARTESIAN_POINT('Ctrl Pts',(87.9449702901573,0.190290764900753,330.083521280956));
#34697=CARTESIAN_POINT('Ctrl Pts',(87.9372131803826,0.0532203185172771,
330.082037956613));
#34698=CARTESIAN_POINT('Ctrl Pts',(87.9294519254564,-0.0839233739299897,
330.080553839629));
#34699=CARTESIAN_POINT('Ctrl Pts',(87.9216906705302,-0.221020375705536,
330.084811856092));
#34700=CARTESIAN_POINT('Ctrl Pts',(87.9139294156041,-0.357557475752364,
330.094764458863));
#34701=CARTESIAN_POINT('Ctrl Pts',(87.9061557451994,-0.494312990662116,
330.104732982555));
#34702=CARTESIAN_POINT('Ctrl Pts',(87.8983820747948,-0.630506425535559,
330.120414251265));
#34703=CARTESIAN_POINT('Ctrl Pts',(87.8906084043901,-0.765631924068881,
330.141709063946));
#34704=CARTESIAN_POINT('Ctrl Pts',(87.8831966002129,-0.894467298137263,
330.162012597973));
#34705=CARTESIAN_POINT('Ctrl Pts',(87.8757847960358,-1.02233164096596,330.187418760199));
#34706=CARTESIAN_POINT('Ctrl Pts',(87.8683729918586,-1.14879953693754,330.21779938873));
#34707=CARTESIAN_POINT('Ctrl Pts',(87.8605979130802,-1.2814660012179,330.249669062364));
#34708=CARTESIAN_POINT('Ctrl Pts',(87.8528228343018,-1.41301491992177,330.287113872835));
#34709=CARTESIAN_POINT('Ctrl Pts',(87.8450477555233,-1.54294174936587,330.330041347018));
#34710=CARTESIAN_POINT('Ctrl Pts',(87.8372822444743,-1.6727086955747,330.372915996211));
#34711=CARTESIAN_POINT('Ctrl Pts',(87.8295167334254,-1.80085715656524,330.421259763533));
#34712=CARTESIAN_POINT('Ctrl Pts',(87.8217512223764,-1.92689351973213,330.474929345732));
#34713=CARTESIAN_POINT('Ctrl Pts',(87.8139934108542,-2.052804917478,330.528545714385));
#34714=CARTESIAN_POINT('Ctrl Pts',(87.806235599332,-2.17660802756939,330.587477237147));
#34715=CARTESIAN_POINT('Ctrl Pts',(87.7984777878098,-2.29782547420462,330.651531171482));
#34716=CARTESIAN_POINT('Ctrl Pts',(87.7907258142868,-2.41895170086708,330.715536903199));
#34717=CARTESIAN_POINT('Ctrl Pts',(87.7829738407638,-2.53749579288089,330.78465719186));
#34718=CARTESIAN_POINT('Ctrl Pts',(87.7752218672408,-2.65300173748832,330.858651808483));
#34719=CARTESIAN_POINT('Ctrl Pts',(87.7674731766832,-2.76845876525978,330.932615088342));
#34720=CARTESIAN_POINT('Ctrl Pts',(87.7597244861256,-2.88087987624982,331.011448380047));
#34721=CARTESIAN_POINT('Ctrl Pts',(87.751975795568,-2.98983519286681,331.094866381032));
#34722=CARTESIAN_POINT('Ctrl Pts',(87.7442287171902,-3.09876784042016,331.178267026204));
#34723=CARTESIAN_POINT('Ctrl Pts',(87.7364816388123,-3.20423581773168,331.266250245841));
#34724=CARTESIAN_POINT('Ctrl Pts',(87.7287345604345,-3.30584002129114,331.358488663188));
#34725=CARTESIAN_POINT('Ctrl Pts',(87.7209874171287,-3.40744507639217,331.450727853582));
#34726=CARTESIAN_POINT('Ctrl Pts',(87.7132402738228,-3.50518600374606,331.547222050089));
#34727=CARTESIAN_POINT('Ctrl Pts',(87.705493130517,-3.59869875870711,331.647605287771));
#34728=CARTESIAN_POINT('Ctrl Pts',(87.6977442454889,-3.69223253732062,331.748011093736));
#34729=CARTESIAN_POINT('Ctrl Pts',(87.6899953604608,-3.78153598561045,331.852307394765));
#34730=CARTESIAN_POINT('Ctrl Pts',(87.6822464754326,-3.8662839981385,331.960093569164));
#34731=CARTESIAN_POINT('Ctrl Pts',(87.6744893656579,-3.95112196308247,332.067994148922));
#34732=CARTESIAN_POINT('Ctrl Pts',(87.6667322558832,-4.03139459154995,332.179391693757));
#34733=CARTESIAN_POINT('Ctrl Pts',(87.6589751461085,-4.10681863427376,332.293854444476));
#34734=CARTESIAN_POINT('Ctrl Pts',(87.6512138911824,-4.18228298119431,332.408378360429));
#34735=CARTESIAN_POINT('Ctrl Pts',(87.6434526362562,-4.25289337859473,332.525970411091));
#34736=CARTESIAN_POINT('Ctrl Pts',(87.63569138133,-4.31841208192752,332.646173295852));
#34737=CARTESIAN_POINT('Ctrl Pts',(87.6279177109253,-4.38403559383318,332.766568466054));
#34738=CARTESIAN_POINT('Ctrl Pts',(87.6201440405207,-4.44455096281739,332.889582465288));
#34739=CARTESIAN_POINT('Ctrl Pts',(87.612370370116,-4.49976786128482,333.014736224818));
#34740=CARTESIAN_POINT('Ctrl Pts',(87.6049585659389,-4.55241439984428,333.134064046733));
#34741=CARTESIAN_POINT('Ctrl Pts',(87.5975467617618,-4.60024454877045,333.255336632668));
#34742=CARTESIAN_POINT('Ctrl Pts',(87.5901349575847,-4.64313586533308,333.378126885802));
#34743=CARTESIAN_POINT('Ctrl Pts',(87.5810267921634,-4.69584384264283,333.529020502383));
#34744=CARTESIAN_POINT('Ctrl Pts',(87.5719186267421,-4.74123094441884,333.682596029949));
#34745=CARTESIAN_POINT('Ctrl Pts',(87.5628104613208,-4.77905702408711,333.838192346804));
#34746=CARTESIAN_POINT('Ctrl Pts',(87.5537431289365,-4.81671352474134,333.993091106043));
#34747=CARTESIAN_POINT('Ctrl Pts',(87.5446757965522,-4.84687655935502,334.14999248358));
#34748=CARTESIAN_POINT('Ctrl Pts',(87.5356084641679,-4.86935592408862,334.308222617424));
#34749=CARTESIAN_POINT('Ctrl Pts',(87.5266169340333,-4.8916473629422,334.465129958676));
#34750=CARTESIAN_POINT('Ctrl Pts',(87.5176254038986,-4.90638298903107,334.623343823302));
#34751=CARTESIAN_POINT('Ctrl Pts',(87.508633873764,-4.91342453997809,334.782187345544));
#34752=CARTESIAN_POINT('Ctrl Pts',(87.5046013320235,-4.91658255064887,334.853425847118));
#34753=CARTESIAN_POINT('Ctrl Pts',(87.5005687902829,-4.91819364564975,334.924790739551));
#34754=CARTESIAN_POINT('Ctrl Pts',(87.4965362485424,-4.91824854721736,334.996219749433));
#34755=CARTESIAN_POINT('',(90.9965362484616,-4.91824791233306,335.004531592596));
#34756=CARTESIAN_POINT('Ctrl Pts',(90.9965362484616,-4.91824791233306,335.004531592596));
#34757=CARTESIAN_POINT('Ctrl Pts',(90.9864706741919,-4.91808413604804,335.182281987159));
#34758=CARTESIAN_POINT('Ctrl Pts',(90.9764050999222,-4.90828083222216,335.359603187475));
#34759=CARTESIAN_POINT('Ctrl Pts',(90.9663395256525,-4.88899777647855,335.53561535087));
#34760=CARTESIAN_POINT('Ctrl Pts',(90.956026782763,-4.86924120912543,335.715949640586));
#34761=CARTESIAN_POINT('Ctrl Pts',(90.9457140398736,-4.83953357743045,335.894910145243));
#34762=CARTESIAN_POINT('Ctrl Pts',(90.9354012969841,-4.80009451970844,336.07157625224));
#34763=CARTESIAN_POINT('Ctrl Pts',(90.9332646542801,-4.7919233497454,336.108178769399));
#34764=CARTESIAN_POINT('Ctrl Pts',(90.9311280115761,-4.78333461513977,336.144682874129));
#34765=CARTESIAN_POINT('Ctrl Pts',(90.9289913688721,-4.77433052225825,336.181080491217));
#34766=CARTESIAN_POINT('Ctrl Pts',(90.9212162900936,-4.7415653194704,336.313528625702));
#34767=CARTESIAN_POINT('Ctrl Pts',(90.9134412113152,-4.70323265688646,336.444821576094));
#34768=CARTESIAN_POINT('Ctrl Pts',(90.9056661325368,-4.65942841407308,336.574455434945));
#34769=CARTESIAN_POINT('Ctrl Pts',(90.8979006214878,-4.61567807516919,336.70392977108));
#34770=CARTESIAN_POINT('Ctrl Pts',(90.8901351104388,-4.56646967696209,336.831748711144));
#34771=CARTESIAN_POINT('Ctrl Pts',(90.8823695993897,-4.51194985413787,336.957419621912));
#34772=CARTESIAN_POINT('Ctrl Pts',(90.8746117878675,-4.45748408787668,337.082965929605));
#34773=CARTESIAN_POINT('Ctrl Pts',(90.8668539763453,-4.39771753178151,337.206368090105));
#34774=CARTESIAN_POINT('Ctrl Pts',(90.8590961648231,-4.33284614900619,337.327150040617));
#34775=CARTESIAN_POINT('Ctrl Pts',(90.8513441913001,-4.26802358400369,337.44784109888));
#34776=CARTESIAN_POINT('Ctrl Pts',(90.8435922177771,-4.19810402293034,337.565915528946));
#34777=CARTESIAN_POINT('Ctrl Pts',(90.8358402442541,-4.12333076997611,337.68091895138));
#34778=CARTESIAN_POINT('Ctrl Pts',(90.8280915536965,-4.04858918353885,337.795873669797));
#34779=CARTESIAN_POINT('Ctrl Pts',(90.8203428631388,-3.96899820616832,337.907759640314));
#34780=CARTESIAN_POINT('Ctrl Pts',(90.8125941725812,-3.88484603805112,338.016148922573));
#34781=CARTESIAN_POINT('Ctrl Pts',(90.8048470942034,-3.80071137849535,338.124515653536));
#34782=CARTESIAN_POINT('Ctrl Pts',(90.7971000158255,-3.71201765536447,338.229386834769));
#34783=CARTESIAN_POINT('Ctrl Pts',(90.7893529374477,-3.61909493417,338.330365583531));
#34784=CARTESIAN_POINT('Ctrl Pts',(90.7816057941419,-3.5261714341937,338.431345178591));
#34785=CARTESIAN_POINT('Ctrl Pts',(90.7738586508361,-3.42901913013828,338.528431988489));
#34786=CARTESIAN_POINT('Ctrl Pts',(90.7661115075303,-3.32800643797098,338.621264449239));
#34787=CARTESIAN_POINT('Ctrl Pts',(90.7583626225022,-3.22697103600585,338.714117780697));
#34788=CARTESIAN_POINT('Ctrl Pts',(90.750613737474,-3.12207380665144,338.802714595304));
#34789=CARTESIAN_POINT('Ctrl Pts',(90.7428648524459,-3.01371755877787,338.886732501525));
#34790=CARTESIAN_POINT('Ctrl Pts',(90.7351077426712,-2.90524630046335,338.97083958522));
#34791=CARTESIAN_POINT('Ctrl Pts',(90.7273506328964,-2.79330899897093,339.050357812131));
#34792=CARTESIAN_POINT('Ctrl Pts',(90.7195935231217,-2.67833931719225,339.125006856295));
#34793=CARTESIAN_POINT('Ctrl Pts',(90.7118322681955,-2.56330819929157,339.199695790522));
#34794=CARTESIAN_POINT('Ctrl Pts',(90.7040710132694,-2.4452418085812,339.269510158561));
#34795=CARTESIAN_POINT('Ctrl Pts',(90.6963097583432,-2.32459904137099,339.334215310683));
#34796=CARTESIAN_POINT('Ctrl Pts',(90.6885360879385,-2.20376328505072,339.39902396996));
#34797=CARTESIAN_POINT('Ctrl Pts',(90.6807624175338,-2.08034326860222,339.45870691083));
#34798=CARTESIAN_POINT('Ctrl Pts',(90.6729887471292,-1.95481933562801,339.51307704649));
#34799=CARTESIAN_POINT('Ctrl Pts',(90.6655769429521,-1.83513857193331,339.564916239254));
#34800=CARTESIAN_POINT('Ctrl Pts',(90.658165138775,-1.7135456267381,339.61192601403));
#34801=CARTESIAN_POINT('Ctrl Pts',(90.6507533345979,-1.590468414307,339.653986816225));
#34802=CARTESIAN_POINT('Ctrl Pts',(90.6429782558195,-1.46135882106628,339.698109143627));
#34803=CARTESIAN_POINT('Ctrl Pts',(90.6352031770411,-1.33020777481749,339.736924538914));
#34804=CARTESIAN_POINT('Ctrl Pts',(90.6274280982626,-1.19749090801891,339.770240936023));
#34805=CARTESIAN_POINT('Ctrl Pts',(90.6196625872136,-1.06493735777411,339.803516335185));
#34806=CARTESIAN_POINT('Ctrl Pts',(90.6118970761646,-0.93082219632958,339.831306106035));
#34807=CARTESIAN_POINT('Ctrl Pts',(90.6041315651156,-0.795639041917121,
339.853466964704));
#34808=CARTESIAN_POINT('Ctrl Pts',(90.5963737535934,-0.660589921995745,
339.875605850818));
#34809=CARTESIAN_POINT('Ctrl Pts',(90.5886159420712,-0.524475299654361,
339.892126868595));
#34810=CARTESIAN_POINT('Ctrl Pts',(90.580858130549,-0.387801553160386,339.902937182737));
#34811=CARTESIAN_POINT('Ctrl Pts',(90.573106157026,-0.2512306579951,339.913739361775));
#34812=CARTESIAN_POINT('Ctrl Pts',(90.565354183503,-0.114101864265123,339.918839360418));
#34813=CARTESIAN_POINT('Ctrl Pts',(90.55760220998,0.0230710648120109,339.918195887566));
#34814=CARTESIAN_POINT('Ctrl Pts',(90.5498535194224,0.160185901072334,339.917552687224));
#34815=CARTESIAN_POINT('Ctrl Pts',(90.5421048288647,0.297344445447526,339.911170855017));
#34816=CARTESIAN_POINT('Ctrl Pts',(90.5343561383071,0.434030872101439,339.899061161545));
#34817=CARTESIAN_POINT('Ctrl Pts',(90.5266090599293,0.570688860002659,339.886953987597));
#34818=CARTESIAN_POINT('Ctrl Pts',(90.5188619815514,0.706874536460283,339.86912135729));
#34819=CARTESIAN_POINT('Ctrl Pts',(90.5111149031736,0.842075536924039,339.845626053733));
#34820=CARTESIAN_POINT('Ctrl Pts',(90.5033677598678,0.977277670502308,339.822130553262));
#34821=CARTESIAN_POINT('Ctrl Pts',(90.495620616562,1.11149472652386,339.792972351804));
#34822=CARTESIAN_POINT('Ctrl Pts',(90.4878734732562,1.24422328710095,339.758265595187));
#34823=CARTESIAN_POINT('Ctrl Pts',(90.4801245882281,1.37698168787638,339.723551035753));
#34824=CARTESIAN_POINT('Ctrl Pts',(90.4723757032,1.50825054921469,339.683285537773));
#34825=CARTESIAN_POINT('Ctrl Pts',(90.4646268181719,1.63754078220388,339.63763336726));
#34826=CARTESIAN_POINT('Ctrl Pts',(90.4568697083972,1.76696824518228,339.591932741061));
#34827=CARTESIAN_POINT('Ctrl Pts',(90.4491125986225,1.89441251543709,339.540834151494));
#34828=CARTESIAN_POINT('Ctrl Pts',(90.4413554888477,2.01940318101161,339.484550574475));
#34829=CARTESIAN_POINT('Ctrl Pts',(90.4335942339216,2.1444606376013,339.428236921311));
#34830=CARTESIAN_POINT('Ctrl Pts',(90.4258329789954,2.26706152777124,339.36673293502));
#34831=CARTESIAN_POINT('Ctrl Pts',(90.4180717240692,2.38676019443191,339.300297528867));
#34832=CARTESIAN_POINT('Ctrl Pts',(90.4102980536645,2.50665033994954,339.233755847714));
#34833=CARTESIAN_POINT('Ctrl Pts',(90.4025243832599,2.62362865094576,339.162267186743));
#34834=CARTESIAN_POINT('Ctrl Pts',(90.3947507128552,2.73727786065232,339.086134233733));
#34835=CARTESIAN_POINT('Ctrl Pts',(90.3873389086782,2.84563667230385,339.013545288002));
#34836=CARTESIAN_POINT('Ctrl Pts',(90.3799271045011,2.95096911446867,338.936734872868));
#34837=CARTESIAN_POINT('Ctrl Pts',(90.3725153003241,3.05294308217669,338.855998132713));
#34838=CARTESIAN_POINT('Ctrl Pts',(90.3647402215457,3.15991509780755,338.771304244421));
#34839=CARTESIAN_POINT('Ctrl Pts',(90.3569651427673,3.26352914836477,338.682021769262));
#34840=CARTESIAN_POINT('Ctrl Pts',(90.3491900639888,3.36336632938506,338.588446738752));
#34841=CARTESIAN_POINT('Ctrl Pts',(90.3414245529398,3.46308065439822,338.494986858274));
#34842=CARTESIAN_POINT('Ctrl Pts',(90.3336590418908,3.55902707495898,338.397245197377));
#34843=CARTESIAN_POINT('Ctrl Pts',(90.3258935308418,3.65081797545538,338.295559311041));
#34844=CARTESIAN_POINT('Ctrl Pts',(90.3181357193196,3.74251786500662,338.193974246558));
#34845=CARTESIAN_POINT('Ctrl Pts',(90.3103779077974,3.83007017371988,338.088453027448));
#34846=CARTESIAN_POINT('Ctrl Pts',(90.3026200962752,3.91312280407602,337.979371239493));
#34847=CARTESIAN_POINT('Ctrl Pts',(90.2948681227522,3.996112934694,337.870371539043));
#34848=CARTESIAN_POINT('Ctrl Pts',(90.2871161492292,4.07460989109229,337.757816912785));
#34849=CARTESIAN_POINT('Ctrl Pts',(90.2793641757062,4.14830092394737,337.642117050185));
#34850=CARTESIAN_POINT('Ctrl Pts',(90.2716154851486,4.22196074860629,337.526466186545));
#34851=CARTESIAN_POINT('Ctrl Pts',(90.2638667945909,4.29081848826982,337.407673064834));
#34852=CARTESIAN_POINT('Ctrl Pts',(90.2561181040333,4.35460405720851,337.286177282593));
#34853=CARTESIAN_POINT('Ctrl Pts',(90.2483710256555,4.41837635502684,337.164706778563));
#34854=CARTESIAN_POINT('Ctrl Pts',(90.2406239472776,4.47707839962336,337.040535078341));
#34855=CARTESIAN_POINT('Ctrl Pts',(90.2328768688998,4.53048571679436,336.91412701575));
#34856=CARTESIAN_POINT('Ctrl Pts',(90.225129725594,4.58389348157008,336.787717893737));
#34857=CARTESIAN_POINT('Ctrl Pts',(90.2173825822882,4.63200627828735,336.659072732027));
#34858=CARTESIAN_POINT('Ctrl Pts',(90.2096354389824,4.67464766630308,336.528676636319));
#34859=CARTESIAN_POINT('Ctrl Pts',(90.2018865539544,4.71729864100816,336.3982512248));
#34860=CARTESIAN_POINT('Ctrl Pts',(90.1941376689262,4.75447563780562,336.266074467412));
#34861=CARTESIAN_POINT('Ctrl Pts',(90.1863887838982,4.78605211741718,336.132646543219));
#34862=CARTESIAN_POINT('Ctrl Pts',(90.1786316741234,4.81766211263045,335.99907699725));
#34863=CARTESIAN_POINT('Ctrl Pts',(90.1708745643487,4.84365962590922,335.864254012637));
#34864=CARTESIAN_POINT('Ctrl Pts',(90.1631174545739,4.86396918634112,335.728688422321));
#34865=CARTESIAN_POINT('Ctrl Pts',(90.1553561996478,4.88428959955274,335.593050390087));
#34866=CARTESIAN_POINT('Ctrl Pts',(90.1475949447216,4.89891596185973,335.456669349888));
#34867=CARTESIAN_POINT('Ctrl Pts',(90.1398336897955,4.90782482832607,335.320060177101));
#34868=CARTESIAN_POINT('Ctrl Pts',(90.1320600193908,4.91674794607535,335.183232474159));
#34869=CARTESIAN_POINT('Ctrl Pts',(90.1242863489861,4.9199352822153,335.04617630035));
#34870=CARTESIAN_POINT('Ctrl Pts',(90.1165126785815,4.9174155663663,334.909406345927));
#34871=CARTESIAN_POINT('Ctrl Pts',(90.1091008744043,4.91501314389626,334.779003065785));
#34872=CARTESIAN_POINT('Ctrl Pts',(90.1016890702272,4.90742305556099,334.648860244988));
#34873=CARTESIAN_POINT('Ctrl Pts',(90.0942772660501,4.89471377351411,334.519416877251));
#34874=CARTESIAN_POINT('Ctrl Pts',(90.0865021872716,4.88138157169519,334.38362910447));
#34875=CARTESIAN_POINT('Ctrl Pts',(90.0787271084932,4.8623735417055,334.248181968511));
#34876=CARTESIAN_POINT('Ctrl Pts',(90.0709520297147,4.83771192951968,334.113587934715));
#34877=CARTESIAN_POINT('Ctrl Pts',(90.0631865186657,4.81308066501769,333.979159527446));
#34878=CARTESIAN_POINT('Ctrl Pts',(90.0554210076167,4.78280973071296,333.845582514343));
#34879=CARTESIAN_POINT('Ctrl Pts',(90.0476554965677,4.74697322273925,333.713365520011));
#34880=CARTESIAN_POINT('Ctrl Pts',(90.0398976850455,4.71117224676752,333.581279619214));
#34881=CARTESIAN_POINT('Ctrl Pts',(90.0321398735233,4.66981678041663,333.450551428504));
#34882=CARTESIAN_POINT('Ctrl Pts',(90.0243820620011,4.62303212161206,333.321680285213));
#34883=CARTESIAN_POINT('Ctrl Pts',(90.0166300884781,4.57628266974691,333.192906121544));
#34884=CARTESIAN_POINT('Ctrl Pts',(90.0088781149551,4.52411229053993,333.065986589598));
#34885=CARTESIAN_POINT('Ctrl Pts',(90.0011261414321,4.46669625399965,332.941406393431));
#34886=CARTESIAN_POINT('Ctrl Pts',(89.9933774508745,4.40930453318493,332.816878957052));
#34887=CARTESIAN_POINT('Ctrl Pts',(89.9856287603168,4.34667173678616,332.694689240247));
#34888=CARTESIAN_POINT('Ctrl Pts',(89.9778800697592,4.27902137286804,332.575302255324));
#34889=CARTESIAN_POINT('Ctrl Pts',(89.9701329913814,4.21138508417316,332.455940109859));
#34890=CARTESIAN_POINT('Ctrl Pts',(89.9623859130035,4.13873349702308,332.339379876244));
#34891=CARTESIAN_POINT('Ctrl Pts',(89.9546388346257,4.06133602422417,332.226061867878));
#34892=CARTESIAN_POINT('Ctrl Pts',(89.9468916913199,3.98393790275988,332.112742909798));
#34893=CARTESIAN_POINT('Ctrl Pts',(89.9391445480141,3.90179403676904,332.002666553938));
#34894=CARTESIAN_POINT('Ctrl Pts',(89.9313974047083,3.81521687982707,331.896243691528));
#34895=CARTESIAN_POINT('Ctrl Pts',(89.9236485196802,3.72862025850221,331.789796902998));
#34896=CARTESIAN_POINT('Ctrl Pts',(89.9158996346521,3.63758860952924,331.687005545531));
#34897=CARTESIAN_POINT('Ctrl Pts',(89.908150749624,3.54247406649159,331.588246704298));
#34898=CARTESIAN_POINT('Ctrl Pts',(89.9003936398493,3.44725856789517,331.48938303941));
#34899=CARTESIAN_POINT('Ctrl Pts',(89.8926365300745,3.34795178998452,331.394560722746));
#34900=CARTESIAN_POINT('Ctrl Pts',(89.8848794202998,3.24494246143393,331.304119660421));
#34901=CARTESIAN_POINT('Ctrl Pts',(89.8771181653736,3.14187808799183,331.213630269285));
#34902=CARTESIAN_POINT('Ctrl Pts',(89.8693569104475,3.03510752563133,331.127527042787));
#34903=CARTESIAN_POINT('Ctrl Pts',(89.8615956555213,2.92505105664167,331.046108324886));
#34904=CARTESIAN_POINT('Ctrl Pts',(89.8538219851167,2.81481853316894,330.96455936357));
#34905=CARTESIAN_POINT('Ctrl Pts',(89.846048314712,2.70128992312181,330.887710104681));
#34906=CARTESIAN_POINT('Ctrl Pts',(89.8382746443073,2.58491358776074,330.815814917298));
#34907=CARTESIAN_POINT('Ctrl Pts',(89.8308628401303,2.47395459881013,330.747266468184));
#34908=CARTESIAN_POINT('Ctrl Pts',(89.8234510359533,2.36040729201062,330.683221387467));
#34909=CARTESIAN_POINT('Ctrl Pts',(89.8160392317762,2.2446778807548,330.62385966014));
#34910=CARTESIAN_POINT('Ctrl Pts',(89.8082641529978,2.12327622631235,330.561588437727));
#34911=CARTESIAN_POINT('Ctrl Pts',(89.8004890742194,1.99908950433923,330.504274478442));
#34912=CARTESIAN_POINT('Ctrl Pts',(89.7927139954409,1.87256069644547,330.45217639957));
#34913=CARTESIAN_POINT('Ctrl Pts',(89.7849484843919,1.74618759030504,330.400142430701));
#34914=CARTESIAN_POINT('Ctrl Pts',(89.7771829733429,1.61747849074813,330.353311718723));
#34915=CARTESIAN_POINT('Ctrl Pts',(89.7694174622939,1.48690120872592,330.311897200574));
#34916=CARTESIAN_POINT('Ctrl Pts',(89.7616596507717,1.35645339445901,330.27052374504));
#34917=CARTESIAN_POINT('Ctrl Pts',(89.7539018392496,1.22414145410857,330.234555913799));
#34918=CARTESIAN_POINT('Ctrl Pts',(89.7461440277274,1.09045309698793,330.204158561236));
#34919=CARTESIAN_POINT('Ctrl Pts',(89.7383920542043,0.956865344595516,330.173784083644));
#34920=CARTESIAN_POINT('Ctrl Pts',(89.7306400806814,0.821903616748002,330.148971827148));
#34921=CARTESIAN_POINT('Ctrl Pts',(89.7228881071583,0.686070360086097,330.129836704636));
#34922=CARTESIAN_POINT('Ctrl Pts',(89.7151394166007,0.550294628889126,330.11070968586));
#34923=CARTESIAN_POINT('Ctrl Pts',(89.7073907260431,0.41364848922479,330.097255073556));
#34924=CARTESIAN_POINT('Ctrl Pts',(89.6996420354855,0.276643932899942,330.089536559866));
#34925=CARTESIAN_POINT('Ctrl Pts',(89.6918949571076,0.139667881517228,330.081819652078));
#34926=CARTESIAN_POINT('Ctrl Pts',(89.6841478787298,0.00233395181259097,
330.079836491032));
#34927=CARTESIAN_POINT('Ctrl Pts',(89.676400800352,-0.134841792553407,330.083598800598));
#34928=CARTESIAN_POINT('Ctrl Pts',(89.6686536570462,-0.272018686584173,
330.087361141696));
#34929=CARTESIAN_POINT('Ctrl Pts',(89.6609065137404,-0.409037001904642,
330.096869038734));
#34930=CARTESIAN_POINT('Ctrl Pts',(89.6531593704346,-0.545382124755205,
330.112082099657));
#34931=CARTESIAN_POINT('Ctrl Pts',(89.6454104854065,-0.681757900883981,
330.127298580798));
#34932=CARTESIAN_POINT('Ctrl Pts',(89.6376616003784,-0.817459794989565,
330.148222734802));
#34933=CARTESIAN_POINT('Ctrl Pts',(89.6299127153503,-0.951980148418879,
330.174762507449));
#34934=CARTESIAN_POINT('Ctrl Pts',(89.6221556055756,-1.08664328314127,330.201330449686));
#34935=CARTESIAN_POINT('Ctrl Pts',(89.6143984958009,-1.22012198791813,330.233525841398));
#34936=CARTESIAN_POINT('Ctrl Pts',(89.6066413860261,-1.35192006505528,330.271205735052));
#34937=CARTESIAN_POINT('Ctrl Pts',(89.5988801311,-1.48378857087077,330.308905763637));
#34938=CARTESIAN_POINT('Ctrl Pts',(89.5911188761738,-1.61397428875126,330.352096010916));
#34939=CARTESIAN_POINT('Ctrl Pts',(89.5833576212476,-1.74199889603575,330.40058450358));
#34940=CARTESIAN_POINT('Ctrl Pts',(89.575583950843,-1.87022830096878,330.449150562029));
#34941=CARTESIAN_POINT('Ctrl Pts',(89.5678102804383,-1.99628932744208,330.50303164865));
#34942=CARTESIAN_POINT('Ctrl Pts',(89.5600366100336,-2.11972543706607,330.561988380597));
#34943=CARTESIAN_POINT('Ctrl Pts',(89.5526248058565,-2.23741556609071,330.618200662488));
#34944=CARTESIAN_POINT('Ctrl Pts',(89.5452130016794,-2.35271940386158,330.67902654712));
#34945=CARTESIAN_POINT('Ctrl Pts',(89.5378011975023,-2.46526577178178,330.744221841193));
#34946=CARTESIAN_POINT('Ctrl Pts',(89.5300261187238,-2.5833283724514,330.812612550834));
#34947=CARTESIAN_POINT('Ctrl Pts',(89.5222510399454,-2.69872946464623,330.886027942706));
#34948=CARTESIAN_POINT('Ctrl Pts',(89.514475961167,-2.811011848806,330.964235456772));
#34949=CARTESIAN_POINT('Ctrl Pts',(89.506710450118,-2.92315606234381,331.042346731514));
#34950=CARTESIAN_POINT('Ctrl Pts',(89.498944939069,-3.03218888623276,331.125238173823));
#34951=CARTESIAN_POINT('Ctrl Pts',(89.49117942802,-3.13767809790927,331.212631623884));
#34952=CARTESIAN_POINT('Ctrl Pts',(89.4834216164978,-3.24306271672512,331.299938423086));
#34953=CARTESIAN_POINT('Ctrl Pts',(89.4756638049756,-3.34491041633648,331.39173809916));
#34954=CARTESIAN_POINT('Ctrl Pts',(89.4679059934534,-3.44281863968047,331.487709739106));
#34955=CARTESIAN_POINT('Ctrl Pts',(89.4601540199304,-3.54065318398155,331.583609157351));
#34956=CARTESIAN_POINT('Ctrl Pts',(89.4524020464075,-3.63455387485573,331.683674017863));
#34957=CARTESIAN_POINT('Ctrl Pts',(89.4446500728845,-3.72415217689618,331.7875439885));
#34958=CARTESIAN_POINT('Ctrl Pts',(89.4369013823268,-3.81371253400264,331.891369970144));
#34959=CARTESIAN_POINT('Ctrl Pts',(89.4291526917692,-3.8989738714565,331.998997561463));
#34960=CARTESIAN_POINT('Ctrl Pts',(89.4214040012116,-3.97960556103291,332.110030685094));
#34961=CARTESIAN_POINT('Ctrl Pts',(89.4136569228338,-4.06022047451285,332.221040707357));
#34962=CARTESIAN_POINT('Ctrl Pts',(89.4059098444559,-4.13620742652772,332.335454536501));
#34963=CARTESIAN_POINT('Ctrl Pts',(89.3981627660781,-4.20727728656692,332.452844548042));
#34964=CARTESIAN_POINT('Ctrl Pts',(89.3904156227723,-4.2783477422399,332.570235543425));
#34965=CARTESIAN_POINT('Ctrl Pts',(89.3826684794665,-4.34450082130757,332.690602436585));
#34966=CARTESIAN_POINT('Ctrl Pts',(89.3749213361608,-4.40549200327767,332.813490619376));
#34967=CARTESIAN_POINT('Ctrl Pts',(89.3671724511327,-4.46649689736039,332.936406430039));
#34968=CARTESIAN_POINT('Ctrl Pts',(89.3594235661046,-4.52233741133484,333.061844308225));
#34969=CARTESIAN_POINT('Ctrl Pts',(89.3516746810765,-4.57281623233117,333.189327537121));
#34970=CARTESIAN_POINT('Ctrl Pts',(89.3439175713018,-4.62334863206966,333.316946078033));
#34971=CARTESIAN_POINT('Ctrl Pts',(89.3361604615271,-4.66850782648172,333.44661394235));
#34972=CARTESIAN_POINT('Ctrl Pts',(89.3284033517524,-4.70814550215337,333.577836509731));
#34973=CARTESIAN_POINT('Ctrl Pts',(89.3206420968262,-4.74780435893156,333.709129198257));
#34974=CARTESIAN_POINT('Ctrl Pts',(89.3128808419,-4.78193572057139,333.841977866872));
#34975=CARTESIAN_POINT('Ctrl Pts',(89.3051195869739,-4.81044217368608,333.975876396072));
#34976=CARTESIAN_POINT('Ctrl Pts',(89.2973459165692,-4.83899422783549,334.109989119281));
#34977=CARTESIAN_POINT('Ctrl Pts',(89.2895722461646,-4.86190332739835,334.245154673503));
#34978=CARTESIAN_POINT('Ctrl Pts',(89.2817985757599,-4.87912371539755,334.380859602073));
#34979=CARTESIAN_POINT('Ctrl Pts',(89.2743867715828,-4.89554249019254,334.51024743357));
#34980=CARTESIAN_POINT('Ctrl Pts',(89.2669749674057,-4.90679022889298,334.640125267014));
#34981=CARTESIAN_POINT('Ctrl Pts',(89.2595631632285,-4.91287141281748,334.770048823398));
#34982=CARTESIAN_POINT('Ctrl Pts',(89.2552208583156,-4.91643415600394,334.846166281941));
#34983=CARTESIAN_POINT('Ctrl Pts',(89.2508785534028,-4.91822803246434,334.922367180039));
#34984=CARTESIAN_POINT('Ctrl Pts',(89.2465362484899,-4.91824979948594,334.998595593897));
#34985=CARTESIAN_POINT('',(92.7465362485305,-4.91824992232871,334.999125921265));
#34986=CARTESIAN_POINT('Ctrl Pts',(92.74653624849,-4.91824992232884,334.999125921985));
#34987=CARTESIAN_POINT('Ctrl Pts',(92.7385216442954,-4.9182752111004,335.141420427261));
#34988=CARTESIAN_POINT('Ctrl Pts',(92.7305070401008,-4.91212087654961,335.283631968748));
#34989=CARTESIAN_POINT('Ctrl Pts',(92.7224924359062,-4.899834566952,335.425210864163));
#34990=CARTESIAN_POINT('Ctrl Pts',(92.7144706815551,-4.8875372962347,335.566916067906));
#34991=CARTESIAN_POINT('Ctrl Pts',(92.706448927204,-4.86909717163168,335.70798715086));
#34992=CARTESIAN_POINT('Ctrl Pts',(92.698427172853,-4.84461342652192,335.847881955265));
#34993=CARTESIAN_POINT('Ctrl Pts',(92.6900932063248,-4.81917675727255,335.993221561334));
#34994=CARTESIAN_POINT('Ctrl Pts',(92.6817592397967,-4.78721663899655,336.137291062448));
#34995=CARTESIAN_POINT('Ctrl Pts',(92.6734252732686,-4.74890158037103,336.279498668405));
#34996=CARTESIAN_POINT('Ctrl Pts',(92.6653798140736,-4.71191292200677,336.41678329597));
#34997=CARTESIAN_POINT('Ctrl Pts',(92.6573343548786,-4.66900215389861,336.552332486576));
#34998=CARTESIAN_POINT('Ctrl Pts',(92.6492888956835,-4.62037042257736,336.68563347756));
#34999=CARTESIAN_POINT('Ctrl Pts',(92.6412347778026,-4.57168635280338,336.819077929767));
#35000=CARTESIAN_POINT('Ctrl Pts',(92.6331806599216,-4.51726917308143,336.950269033648));
#35001=CARTESIAN_POINT('Ctrl Pts',(92.6251265420407,-4.45736701682273,337.07871651262));
#35002=CARTESIAN_POINT('Ctrl Pts',(92.617057771837,-4.39735588454188,337.207397667577));
#35003=CARTESIAN_POINT('Ctrl Pts',(92.6089890016333,-4.33184000147973,337.333324915718));
#35004=CARTESIAN_POINT('Ctrl Pts',(92.6009202314296,-4.26111252886422,337.45603401419));
#35005=CARTESIAN_POINT('Ctrl Pts',(92.600086679125,-4.25380595719205,337.468710599251));
#35006=CARTESIAN_POINT('Ctrl Pts',(92.5992531268204,-4.24644380349574,337.481352867268));
#35007=CARTESIAN_POINT('Ctrl Pts',(92.5984195745157,-4.2390264160805,337.493960325721));
#35008=CARTESIAN_POINT('Ctrl Pts',(92.5906444957373,-4.16983967019412,337.611558204256));
#35009=CARTESIAN_POINT('Ctrl Pts',(92.5828694169588,-4.09564633712657,337.726460689746));
#35010=CARTESIAN_POINT('Ctrl Pts',(92.5750943381804,-4.01668206031312,337.838212164173));
#35011=CARTESIAN_POINT('Ctrl Pts',(92.5673288271314,-3.93781495406951,337.949826121296));
#35012=CARTESIAN_POINT('Ctrl Pts',(92.5595633160824,-3.85418880899566,338.058296466337));
#35013=CARTESIAN_POINT('Ctrl Pts',(92.5517978050334,-3.76608469852817,338.163192865763));
#35014=CARTESIAN_POINT('Ctrl Pts',(92.5440399935111,-3.67806794354261,338.267985260104));
#35015=CARTESIAN_POINT('Ctrl Pts',(92.5362821819889,-3.58558230861974,338.369210463371));
#35016=CARTESIAN_POINT('Ctrl Pts',(92.5285243704667,-3.48895141899565,338.466468095683));
#35017=CARTESIAN_POINT('Ctrl Pts',(92.5207723969437,-3.3923932471804,338.563652538543));
#35018=CARTESIAN_POINT('Ctrl Pts',(92.5130204234207,-3.29169630413375,338.656875077218));
#35019=CARTESIAN_POINT('Ctrl Pts',(92.5052684498977,-3.18722340349391,338.745769619013));
#35020=CARTESIAN_POINT('Ctrl Pts',(92.4975197593401,-3.08279474718951,338.834626513916));
#35021=CARTESIAN_POINT('Ctrl Pts',(92.4897710687824,-2.97459361090222,338.919158804691));
#35022=CARTESIAN_POINT('Ctrl Pts',(92.4820223782248,-2.86301829658375,338.999038546442));
#35023=CARTESIAN_POINT('Ctrl Pts',(92.474275299847,-2.75146619644132,339.078901668545));
#35024=CARTESIAN_POINT('Ctrl Pts',(92.4665282214691,-2.63654163226802,339.154113939655));
#35025=CARTESIAN_POINT('Ctrl Pts',(92.4587811430913,-2.5186741720712,339.224389124766));
#35026=CARTESIAN_POINT('Ctrl Pts',(92.4510339997855,-2.40080572403161,339.294664898851));
#35027=CARTESIAN_POINT('Ctrl Pts',(92.4432868564797,-2.27999466650391,339.360003304237));
#35028=CARTESIAN_POINT('Ctrl Pts',(92.4355397131739,-2.15669724917237,339.420162897215));
#35029=CARTESIAN_POINT('Ctrl Pts',(92.4277908281458,-2.0333721119639,339.480336015345));
#35030=CARTESIAN_POINT('Ctrl Pts',(92.4200419431176,-1.90755985385148,339.535327832858));
#35031=CARTESIAN_POINT('Ctrl Pts',(92.4122930580895,-1.7797385137572,339.584944261946));
#35032=CARTESIAN_POINT('Ctrl Pts',(92.4045359483148,-1.65178150277155,339.634613354424));
#35033=CARTESIAN_POINT('Ctrl Pts',(92.3967788385401,-1.52181151497495,339.678895519555));
#35034=CARTESIAN_POINT('Ctrl Pts',(92.3890217287654,-1.39032416138223,339.717645788821));
#35035=CARTESIAN_POINT('Ctrl Pts',(92.3812604738392,-1.25876654515208,339.756416764991));
#35036=CARTESIAN_POINT('Ctrl Pts',(92.373499218913,-1.12569032650598,339.789649860408));
#35037=CARTESIAN_POINT('Ctrl Pts',(92.3657379639868,-0.991602271494193,
339.817251083104));
#35038=CARTESIAN_POINT('Ctrl Pts',(92.3579642935822,-0.857299719293586,
339.844896458762));
#35039=CARTESIAN_POINT('Ctrl Pts',(92.3501906231775,-0.72198248228191,339.866891895982));
#35040=CARTESIAN_POINT('Ctrl Pts',(92.3424169527729,-0.586164314528041,
339.883195107599));
#35041=CARTESIAN_POINT('Ctrl Pts',(92.3350051485958,-0.456668515159256,
339.898739400792));
#35042=CARTESIAN_POINT('Ctrl Pts',(92.3275933444187,-0.326717659055883,
339.909109465582));
#35043=CARTESIAN_POINT('Ctrl Pts',(92.3201815402416,-0.196755984812248,
339.914312784606));
#35044=CARTESIAN_POINT('Ctrl Pts',(92.3124064614632,-0.0604245017779839,
339.919771133795));
#35045=CARTESIAN_POINT('Ctrl Pts',(92.3046313826847,0.0763497193427593,
339.919560705175));
#35046=CARTESIAN_POINT('Ctrl Pts',(92.2968563039063,0.213056019454141,339.913633095284));
#35047=CARTESIAN_POINT('Ctrl Pts',(92.2890907928573,0.3495940937599,339.907712779695));
#35048=CARTESIAN_POINT('Ctrl Pts',(92.2813252818083,0.486064026584502,339.896089297945));
#35049=CARTESIAN_POINT('Ctrl Pts',(92.2735597707593,0.621951836315044,339.878766132518));
#35050=CARTESIAN_POINT('Ctrl Pts',(92.2658019592371,0.757704912887165,339.86146014306));
#35051=CARTESIAN_POINT('Ctrl Pts',(92.2580441477149,0.892876629740933,339.838465765347));
#35052=CARTESIAN_POINT('Ctrl Pts',(92.2502863361926,1.0269551667081,339.809838474218));
#35053=CARTESIAN_POINT('Ctrl Pts',(92.2425343626696,1.16093280532377,339.781232726034));
#35054=CARTESIAN_POINT('Ctrl Pts',(92.2347823891467,1.29381852078329,339.747002583137));
#35055=CARTESIAN_POINT('Ctrl Pts',(92.2270304156237,1.42510811864993,339.70725502949));
#35056=CARTESIAN_POINT('Ctrl Pts',(92.219281725066,1.55634211529402,339.667524308956));
#35057=CARTESIAN_POINT('Ctrl Pts',(92.2115330345084,1.68598096544852,339.622280938082));
#35058=CARTESIAN_POINT('Ctrl Pts',(92.2037843439508,1.81353334921395,339.571682387676));
#35059=CARTESIAN_POINT('Ctrl Pts',(92.196037265573,1.9410591946406,339.521094364722));
#35060=CARTESIAN_POINT('Ctrl Pts',(92.1882901871952,2.06649907404425,339.465153522477));
#35061=CARTESIAN_POINT('Ctrl Pts',(92.1805431088173,2.18937982240547,339.404066195659));
#35062=CARTESIAN_POINT('Ctrl Pts',(92.1727959655115,2.31226160062556,339.34297835687));
#35063=CARTESIAN_POINT('Ctrl Pts',(92.1650488222057,2.4325838550137,339.276744121475));
#35064=CARTESIAN_POINT('Ctrl Pts',(92.1573016788999,2.54989664751896,339.205616500523));
#35065=CARTESIAN_POINT('Ctrl Pts',(92.1495527938718,2.66723581443075,339.134472888571));
#35066=CARTESIAN_POINT('Ctrl Pts',(92.1418039088437,2.78156383894635,339.058433904523));
#35067=CARTESIAN_POINT('Ctrl Pts',(92.1340550238156,2.89245881419868,338.977796509459));
#35068=CARTESIAN_POINT('Ctrl Pts',(92.1262979140409,3.0034714945235,338.89707352503));
#35069=CARTESIAN_POINT('Ctrl Pts',(92.1185408042661,3.11104352997321,338.811742609967));
#35070=CARTESIAN_POINT('Ctrl Pts',(92.1107836944914,3.21478480987089,338.72214208336));
#35071=CARTESIAN_POINT('Ctrl Pts',(92.1030224395653,3.31858152579155,338.632493677098));
#35072=CARTESIAN_POINT('Ctrl Pts',(92.0952611846391,3.4185431225455,338.538571380626));
#35073=CARTESIAN_POINT('Ctrl Pts',(92.0874999297129,3.51431632009507,338.440750479883));
#35074=CARTESIAN_POINT('Ctrl Pts',(92.0797262593083,3.61024272354825,338.342773097578));
#35075=CARTESIAN_POINT('Ctrl Pts',(92.0719525889036,3.70196707740749,338.240884939286));
#35076=CARTESIAN_POINT('Ctrl Pts',(92.0641789184989,3.78917579968558,338.135495147752));
#35077=CARTESIAN_POINT('Ctrl Pts',(92.0567671143219,3.87232493496041,338.035011276369));
#35078=CARTESIAN_POINT('Ctrl Pts',(92.0493553101448,3.95136920849405,337.931344666184));
#35079=CARTESIAN_POINT('Ctrl Pts',(92.0419435059677,4.02607450960209,337.824872936192));
#35080=CARTESIAN_POINT('Ctrl Pts',(92.0341684271893,4.10444134005321,337.713182709551));
#35081=CARTESIAN_POINT('Ctrl Pts',(92.0263933484108,4.17828076528896,337.598052474059));
#35082=CARTESIAN_POINT('Ctrl Pts',(92.0186182696323,4.24727573486787,337.479885459956));
#35083=CARTESIAN_POINT('Ctrl Pts',(92.0108527585833,4.31618580174423,337.361863857887));
#35084=CARTESIAN_POINT('Ctrl Pts',(92.0030872475343,4.38026307925953,337.240813246986));
#35085=CARTESIAN_POINT('Ctrl Pts',(91.9953217364853,4.43923235096435,337.117167729929));
#35086=CARTESIAN_POINT('Ctrl Pts',(91.9875639249631,4.49814315446468,336.993644807761));
#35087=CARTESIAN_POINT('Ctrl Pts',(91.9798061134409,4.55195586382368,336.867532450099));
#35088=CARTESIAN_POINT('Ctrl Pts',(91.9720483019187,4.60044015375487,336.73929107806));
#35089=CARTESIAN_POINT('Ctrl Pts',(91.9642963283957,4.64888795772016,336.611146211721));
#35090=CARTESIAN_POINT('Ctrl Pts',(91.9565443548727,4.6920151859054,336.480875884152));
#35091=CARTESIAN_POINT('Ctrl Pts',(91.9487923813497,4.72963895486805,336.348961978373));
#35092=CARTESIAN_POINT('Ctrl Pts',(91.9410436907921,4.76724679014225,336.217103938211));
#35093=CARTESIAN_POINT('Ctrl Pts',(91.9332950002345,4.79935569484358,336.083604079348));
#35094=CARTESIAN_POINT('Ctrl Pts',(91.9255463096768,4.82583220814465,335.94896077966));
#35095=CARTESIAN_POINT('Ctrl Pts',(91.917799231299,4.85230321278598,335.814345493636));
#35096=CARTESIAN_POINT('Ctrl Pts',(91.9100521529212,4.87314408158095,335.678587623279));
#35097=CARTESIAN_POINT('Ctrl Pts',(91.9023050745433,4.88827226905249,335.542196722705));
#35098=CARTESIAN_POINT('Ctrl Pts',(91.8945579312375,4.90340058331285,335.405804679044));
#35099=CARTESIAN_POINT('Ctrl Pts',(91.8868107879317,4.91281607766325,335.268779983074));
#35100=CARTESIAN_POINT('Ctrl Pts',(91.8790636446259,4.91648802719435,335.131637916098));
#35101=CARTESIAN_POINT('Ctrl Pts',(91.8713147595978,4.92016080225764,334.994465016674));
#35102=CARTESIAN_POINT('Ctrl Pts',(91.8635658745697,4.91808745255723,334.857175084394));
#35103=CARTESIAN_POINT('Ctrl Pts',(91.8558169895417,4.91028938098563,334.720283612422));
#35104=CARTESIAN_POINT('Ctrl Pts',(91.8480598797669,4.90248303246025,334.583246842427));
#35105=CARTESIAN_POINT('Ctrl Pts',(91.8403027699922,4.88893984639177,334.44660976844));
#35106=CARTESIAN_POINT('Ctrl Pts',(91.8325456602174,4.86973321125132,334.310883526727));
#35107=CARTESIAN_POINT('Ctrl Pts',(91.8247844052913,4.85051631269918,334.17508475725));
#35108=CARTESIAN_POINT('Ctrl Pts',(91.8170231503651,4.82563000565068,334.040198174072));
#35109=CARTESIAN_POINT('Ctrl Pts',(91.8092618954389,4.79519869595694,333.906723946666));
#35110=CARTESIAN_POINT('Ctrl Pts',(91.8014882250343,4.76471870608524,333.773036203996));
#35111=CARTESIAN_POINT('Ctrl Pts',(91.7937145546296,4.72867609110482,333.64076570919));
#35112=CARTESIAN_POINT('Ctrl Pts',(91.785940884225,4.68724521067128,333.510397570645));
#35113=CARTESIAN_POINT('Ctrl Pts',(91.7785290800479,4.64774294768982,333.386098100316));
#35114=CARTESIAN_POINT('Ctrl Pts',(91.7711172758708,4.60334287552367,333.263528133206));
#35115=CARTESIAN_POINT('Ctrl Pts',(91.7637054716938,4.55423585131794,333.143088889292));
#35116=CARTESIAN_POINT('Ctrl Pts',(91.7559303929154,4.50272194557331,333.016746559263));
#35117=CARTESIAN_POINT('Ctrl Pts',(91.7481553141369,4.44586522425323,332.892349834692));
#35118=CARTESIAN_POINT('Ctrl Pts',(91.7403802353585,4.38383319808107,332.770383541077));
#35119=CARTESIAN_POINT('Ctrl Pts',(91.7326147243095,4.32187750626643,332.648567334751));
#35120=CARTESIAN_POINT('Ctrl Pts',(91.7248492132605,4.25475935667564,332.529175953619));
#35121=CARTESIAN_POINT('Ctrl Pts',(91.7170837022115,4.18269486009623,332.41267575093));
#35122=CARTESIAN_POINT('Ctrl Pts',(91.7093258906893,4.11070181567483,332.296291058531));
#35123=CARTESIAN_POINT('Ctrl Pts',(91.7015680791671,4.0337723884349,332.182792170131));
#35124=CARTESIAN_POINT('Ctrl Pts',(91.6938102676449,3.95216911408752,332.072621931463));
#35125=CARTESIAN_POINT('Ctrl Pts',(91.6860582941219,3.87062724879194,331.962534599392));
#35126=CARTESIAN_POINT('Ctrl Pts',(91.6783063205989,3.78441876895418,331.855771243975));
#35127=CARTESIAN_POINT('Ctrl Pts',(91.6705543470759,3.69384993156173,331.75274643035));
#35128=CARTESIAN_POINT('Ctrl Pts',(91.6628056565183,3.6033194501257,331.649765247796));
#35129=CARTESIAN_POINT('Ctrl Pts',(91.6550569659607,3.50843254145613,331.550519750968));
#35130=CARTESIAN_POINT('Ctrl Pts',(91.647308275403,3.40953607882918,331.45539187079));
#35131=CARTESIAN_POINT('Ctrl Pts',(91.6395611970252,3.31066019243734,331.360283782761));
#35132=CARTESIAN_POINT('Ctrl Pts',(91.6318141186474,3.20777669294131,331.269291878137));
#35133=CARTESIAN_POINT('Ctrl Pts',(91.6240670402696,3.10126940517231,331.182761320137));
#35134=CARTESIAN_POINT('Ctrl Pts',(91.6163198969638,2.9947612247698,331.096230036928));
#35135=CARTESIAN_POINT('Ctrl Pts',(91.608572753658,2.88462949888965,331.014160421394));
#35136=CARTESIAN_POINT('Ctrl Pts',(91.6008256103522,2.7712909115599,330.936857159045));
#35137=CARTESIAN_POINT('Ctrl Pts',(91.5930767253241,2.65792684330955,330.859536517281));
#35138=CARTESIAN_POINT('Ctrl Pts',(91.585327840296,2.54135480181096,330.786984581226));
#35139=CARTESIAN_POINT('Ctrl Pts',(91.5775789552679,2.42201985859766,330.71946231566));
#35140=CARTESIAN_POINT('Ctrl Pts',(91.5698218454932,2.30255825204242,330.651868381263));
#35141=CARTESIAN_POINT('Ctrl Pts',(91.5620647357185,2.18032822641381,330.589314974392));
#35142=CARTESIAN_POINT('Ctrl Pts',(91.5543076259438,2.0557993218143,330.532016986276));
#35143=CARTESIAN_POINT('Ctrl Pts',(91.5465463710176,1.93120387294966,330.474688379947));
#35144=CARTESIAN_POINT('Ctrl Pts',(91.5387851160914,1.80430745875579,330.422620936522));
#35145=CARTESIAN_POINT('Ctrl Pts',(91.5310238611652,1.67559800555924,330.375980710868));
#35146=CARTESIAN_POINT('Ctrl Pts',(91.5232501907605,1.54668265918398,330.329265876053));
#35147=CARTESIAN_POINT('Ctrl Pts',(91.5154765203559,1.41594885114326,330.287995725506));
#35148=CARTESIAN_POINT('Ctrl Pts',(91.5077028499513,1.28389887545314,330.252286156463));
#35149=CARTESIAN_POINT('Ctrl Pts',(91.5002910457741,1.15799585790016,330.21823887645));
#35150=CARTESIAN_POINT('Ctrl Pts',(91.492879241597,1.03089673091616,330.189246202102));
#35151=CARTESIAN_POINT('Ctrl Pts',(91.4854674374199,0.903042172690774,330.165364760725));
#35152=CARTESIAN_POINT('Ctrl Pts',(91.4776923586414,0.768921081708359,330.140312818766));
#35153=CARTESIAN_POINT('Ctrl Pts',(91.469917279863,0.63354478778416,330.120806643161));
#35154=CARTESIAN_POINT('Ctrl Pts',(91.4621422010846,0.497411640688017,330.106967737465));
#35155=CARTESIAN_POINT('Ctrl Pts',(91.4543766900356,0.361446014095945,330.093145861423));
#35156=CARTESIAN_POINT('Ctrl Pts',(91.4466111789865,0.224725772616025,330.084977418311));
#35157=CARTESIAN_POINT('Ctrl Pts',(91.4388456679375,0.0877600325927998,
330.082533046458));
#35158=CARTESIAN_POINT('Ctrl Pts',(91.4310878564153,-0.0490699054997757,
330.080091098207));
#35159=CARTESIAN_POINT('Ctrl Pts',(91.4233300448932,-0.186144469436422,
330.083361933712));
#35160=CARTESIAN_POINT('Ctrl Pts',(91.415572233371,-0.322949187655547,330.09236443033));
#35161=CARTESIAN_POINT('Ctrl Pts',(91.407820259848,-0.459650955985886,330.101360152283));
#35162=CARTESIAN_POINT('Ctrl Pts',(91.4000682863251,-0.596082894334293,
330.116078924459));
#35163=CARTESIAN_POINT('Ctrl Pts',(91.3923163128021,-0.731730652800285,
330.136487553809));
#35164=CARTESIAN_POINT('Ctrl Pts',(91.3845676222444,-0.867320964360587,
330.156887540093));
#35165=CARTESIAN_POINT('Ctrl Pts',(91.3768189316868,-1.00212737084362,330.182972532877));
#35166=CARTESIAN_POINT('Ctrl Pts',(91.3690702411292,-1.1356409853554,330.214657523763));
#35167=CARTESIAN_POINT('Ctrl Pts',(91.3613231627513,-1.26912682124464,330.246335922321));
#35168=CARTESIAN_POINT('Ctrl Pts',(91.3535760843735,-1.40132002010244,330.283611911263));
#35169=CARTESIAN_POINT('Ctrl Pts',(91.3458290059957,-1.53172261717168,330.326349511726));
#35170=CARTESIAN_POINT('Ctrl Pts',(91.3380818626899,-1.66212630714002,330.36908747037));
#35171=CARTESIAN_POINT('Ctrl Pts',(91.3303347193841,-1.79073899395236,330.417287010101));
#35172=CARTESIAN_POINT('Ctrl Pts',(91.3225875760783,-1.9170789694255,330.470762615242));
#35173=CARTESIAN_POINT('Ctrl Pts',(91.3148386910501,-2.04344734880809,330.524250242835));
#35174=CARTESIAN_POINT('Ctrl Pts',(91.307089806022,-2.1675416402231,330.583016143858));
#35175=CARTESIAN_POINT('Ctrl Pts',(91.2993409209939,-2.28890153907308,330.646827271182));
#35176=CARTESIAN_POINT('Ctrl Pts',(91.2915838112191,-2.41039025057309,330.710706128294));
#35177=CARTESIAN_POINT('Ctrl Pts',(91.2838267014444,-2.5291384253549,330.779640726737));
#35178=CARTESIAN_POINT('Ctrl Pts',(91.2760695916697,-2.64471126170638,330.853352510195));
#35179=CARTESIAN_POINT('Ctrl Pts',(91.2683083367435,-2.7603458564859,330.927103682874));
#35180=CARTESIAN_POINT('Ctrl Pts',(91.2605470818174,-2.87280141150711,331.005636903518));
#35181=CARTESIAN_POINT('Ctrl Pts',(91.2527858268912,-2.9816742427561,331.08863172629));
#35182=CARTESIAN_POINT('Ctrl Pts',(91.2450121564865,-3.09072123505374,331.17175931373));
#35183=CARTESIAN_POINT('Ctrl Pts',(91.2372384860819,-3.19617375014363,331.259362515454));
#35184=CARTESIAN_POINT('Ctrl Pts',(91.2294648156772,-3.29766250745396,331.35108166035));
#35185=CARTESIAN_POINT('Ctrl Pts',(91.2220530115001,-3.39442693869492,331.438531256986));
#35186=CARTESIAN_POINT('Ctrl Pts',(91.214641207323,-3.48758812764284,331.529722024718));
#35187=CARTESIAN_POINT('Ctrl Pts',(91.2072294031459,-3.57685997893381,331.624314032141));
#35188=CARTESIAN_POINT('Ctrl Pts',(91.1995477071593,-3.66938255581156,331.722350492147));
#35189=CARTESIAN_POINT('Ctrl Pts',(91.1918660111727,-3.75803546327572,331.824367545194));
#35190=CARTESIAN_POINT('Ctrl Pts',(91.1841843151861,-3.84245036478083,331.930023085315));
#35191=CARTESIAN_POINT('Ctrl Pts',(91.1763656457404,-3.92837048089958,332.037562585024));
#35192=CARTESIAN_POINT('Ctrl Pts',(91.1685469762948,-4.00989966813559,332.148871329607));
#35193=CARTESIAN_POINT('Ctrl Pts',(91.1607283068491,-4.08668713848287,332.263547680909));
#35194=CARTESIAN_POINT('Ctrl Pts',(91.1530654938859,-4.16194393598232,332.375938086647));
#35195=CARTESIAN_POINT('Ctrl Pts',(91.1454026809227,-4.2326460286149,332.491562759607));
#35196=CARTESIAN_POINT('Ctrl Pts',(91.1377398679595,-4.29850296491242,332.610009346642));
#35197=CARTESIAN_POINT('Ctrl Pts',(91.1300820975968,-4.36431656331045,332.728377988564));
#35198=CARTESIAN_POINT('Ctrl Pts',(91.122424327234,-4.42529115152225,332.849564502683));
#35199=CARTESIAN_POINT('Ctrl Pts',(91.1147665568713,-4.48117994661044,332.973128186442));
#35200=CARTESIAN_POINT('Ctrl Pts',(91.1071120720526,-4.53704476277447,333.096638855563));
#35201=CARTESIAN_POINT('Ctrl Pts',(91.0994575872338,-4.58782796147704,333.222524300614));
#35202=CARTESIAN_POINT('Ctrl Pts',(91.0918031024151,-4.63332927429757,333.350320364908));
#35203=CARTESIAN_POINT('Ctrl Pts',(91.0838641979213,-4.68052129118407,333.482864980664));
#35204=CARTESIAN_POINT('Ctrl Pts',(91.0759252934276,-4.72203111363083,333.617464540475));
#35205=CARTESIAN_POINT('Ctrl Pts',(91.0679863889338,-4.75769068907947,333.753580179255));
#35206=CARTESIAN_POINT('Ctrl Pts',(91.0603311154467,-4.79207626491121,333.884832852913));
#35207=CARTESIAN_POINT('Ctrl Pts',(91.0526758419597,-4.82102236314032,334.017494719986));
#35208=CARTESIAN_POINT('Ctrl Pts',(91.0450205684727,-4.84442983550854,334.151069713501));
#35209=CARTESIAN_POINT('Ctrl Pts',(91.0373637237924,-4.86784211210249,334.284672122383));
#35210=CARTESIAN_POINT('Ctrl Pts',(91.0297068791121,-4.88571344104874,334.419187634097));
#35211=CARTESIAN_POINT('Ctrl Pts',(91.0220500344319,-4.89799632491054,334.554113171687));
#35212=CARTESIAN_POINT('Ctrl Pts',(91.0143877267148,-4.91028797241442,334.6891349765));
#35213=CARTESIAN_POINT('Ctrl Pts',(91.0067254189978,-4.91698319519118,334.824566991026));
#35214=CARTESIAN_POINT('Ctrl Pts',(90.9990631112807,-4.91808655900643,334.959904356592));
#35215=CARTESIAN_POINT('Ctrl Pts',(90.9982208236838,-4.91820784748646,334.974781465242));
#35216=CARTESIAN_POINT('Ctrl Pts',(90.9973785360868,-4.91826161713711,334.989657433038));
#35217=CARTESIAN_POINT('Ctrl Pts',(90.9965362484899,-4.91824791233352,335.004531592096));
#35218=CARTESIAN_POINT('',(94.4965362484452,-4.91824822735333,334.995824280208));
#35219=CARTESIAN_POINT('Ctrl Pts',(94.4965362484452,-4.91824822735333,334.995824280208));
#35220=CARTESIAN_POINT('Ctrl Pts',(94.4888886712765,-4.91836262203263,335.130560674578));
#35221=CARTESIAN_POINT('Ctrl Pts',(94.4812410941079,-4.91293616218613,335.26549038709));
#35222=CARTESIAN_POINT('Ctrl Pts',(94.4735935169392,-4.90194789488013,335.400112357195));
#35223=CARTESIAN_POINT('Ctrl Pts',(94.4659528995935,-4.89096962765567,335.534611812017));
#35224=CARTESIAN_POINT('Ctrl Pts',(94.4583122822477,-4.87443965323708,335.668803681708));
#35225=CARTESIAN_POINT('Ctrl Pts',(94.450671664902,-4.85238907099769,335.802186615547));
#35226=CARTESIAN_POINT('Ctrl Pts',(94.4430357359871,-4.83035201942287,335.935487703032));
#35227=CARTESIAN_POINT('Ctrl Pts',(94.4353998070723,-4.8028011628594,336.067980445035));
#35228=CARTESIAN_POINT('Ctrl Pts',(94.4277638781574,-4.76981941654863,336.199168793797));
#35229=CARTESIAN_POINT('Ctrl Pts',(94.4201303938493,-4.73684822918865,336.330315143226));
#35230=CARTESIAN_POINT('Ctrl Pts',(94.4124969095411,-4.69844970651333,336.460157538624));
#35231=CARTESIAN_POINT('Ctrl Pts',(94.4048634252329,-4.6547577374,336.588210775878));
#35232=CARTESIAN_POINT('Ctrl Pts',(94.39723061841,-4.61106964602646,336.71625264818));
#35233=CARTESIAN_POINT('Ctrl Pts',(94.3895978115871,-4.56208917268773,336.842505296178));
#35234=CARTESIAN_POINT('Ctrl Pts',(94.3819650047642,-4.5079997054631,336.966499864746));
#35235=CARTESIAN_POINT('Ctrl Pts',(94.3743311090654,-4.45390252197905,337.090512122048));
#35236=CARTESIAN_POINT('Ctrl Pts',(94.3666972133666,-4.39469505718639,337.212265289701));
#35237=CARTESIAN_POINT('Ctrl Pts',(94.3590633176678,-4.33060811467945,337.331312166908));
#35238=CARTESIAN_POINT('Ctrl Pts',(94.3514218949351,-4.26645798233973,337.450476424536));
#35239=CARTESIAN_POINT('Ctrl Pts',(94.3437804722023,-4.19741895439889,337.566928706103));
#35240=CARTESIAN_POINT('Ctrl Pts',(94.3361390494696,-4.12376710295986,337.680247739118));
#35241=CARTESIAN_POINT('Ctrl Pts',(94.3284938982079,-4.05007931409524,337.793622064623));
#35242=CARTESIAN_POINT('Ctrl Pts',(94.3208487469462,-3.97177445363895,337.90385976865));
#35243=CARTESIAN_POINT('Ctrl Pts',(94.3132035956845,-3.88917011445415,338.010571188884));
#35244=CARTESIAN_POINT('Ctrl Pts',(94.3055463263312,-3.8064348416994,338.117451754073));
#35245=CARTESIAN_POINT('Ctrl Pts',(94.2978890569779,-3.71938673538526,338.220794560457));
#35246=CARTESIAN_POINT('Ctrl Pts',(94.2902317876246,-3.62838208559448,338.320244946301));
#35247=CARTESIAN_POINT('Ctrl Pts',(94.2827704518028,-3.53970605474,338.417150604461));
#35248=CARTESIAN_POINT('Ctrl Pts',(94.275309115981,-3.44727379825481,338.510360436865));
#35249=CARTESIAN_POINT('Ctrl Pts',(94.2678477801592,-3.35144469859913,338.599583516844));
#35250=CARTESIAN_POINT('Ctrl Pts',(94.2600727013807,-3.2515860651206,338.69255835302));
#35251=CARTESIAN_POINT('Ctrl Pts',(94.2522976226023,-3.14769778161514,338.781521583591));
#35252=CARTESIAN_POINT('Ctrl Pts',(94.2445225438239,-3.04013567261027,338.866103743386));
#35253=CARTESIAN_POINT('Ctrl Pts',(94.2367570327749,-2.93270592562819,338.950581819449));
#35254=CARTESIAN_POINT('Ctrl Pts',(94.2289915217258,-2.82161165271248,339.030689312347));
#35255=CARTESIAN_POINT('Ctrl Pts',(94.2212260106768,-2.70724500788517,339.106093950433));
#35256=CARTESIAN_POINT('Ctrl Pts',(94.2134681991546,-2.59299175791934,339.1814238246));
#35257=CARTESIAN_POINT('Ctrl Pts',(94.2057103876325,-2.47547291713893,339.252059909607));
#35258=CARTESIAN_POINT('Ctrl Pts',(94.1979525761103,-2.3551128784969,339.317710781425));
#35259=CARTESIAN_POINT('Ctrl Pts',(94.1902006025873,-2.23484341460095,339.383312248881));
#35260=CARTESIAN_POINT('Ctrl Pts',(94.1824486290643,-2.11173735037519,339.443935783971));
#35261=CARTESIAN_POINT('Ctrl Pts',(94.1746966555413,-1.98624685785034,339.499334004292));
#35262=CARTESIAN_POINT('Ctrl Pts',(94.1669479649836,-1.86080951062341,339.554708763434));
#35263=CARTESIAN_POINT('Ctrl Pts',(94.159199274426,-1.73299010036903,339.60486245163));
#35264=CARTESIAN_POINT('Ctrl Pts',(94.1514505838684,-1.60326393054789,339.649594372793));
#35265=CARTESIAN_POINT('Ctrl Pts',(94.1437035054906,-1.47356475133979,339.694316987105));
#35266=CARTESIAN_POINT('Ctrl Pts',(94.1359564271127,-1.3419599709547,339.733619950806));
#35267=CARTESIAN_POINT('Ctrl Pts',(94.1282093487349,-1.20894296132336,339.767351463734));
#35268=CARTESIAN_POINT('Ctrl Pts',(94.1204622054291,-1.07592483688136,339.801083259364));
#35269=CARTESIAN_POINT('Ctrl Pts',(94.1127150621233,-0.941494838467383,
339.829243415007));
#35270=CARTESIAN_POINT('Ctrl Pts',(94.1049679188175,-0.80615913357158,339.851730672024));
#35271=CARTESIAN_POINT('Ctrl Pts',(94.0972190337894,-0.670793002336426,
339.874222984654));
#35272=CARTESIAN_POINT('Ctrl Pts',(94.0894701487613,-0.534521144946693,
339.891039796723));
#35273=CARTESIAN_POINT('Ctrl Pts',(94.0817212637332,-0.397857103704945,
339.902131453514));
#35274=CARTESIAN_POINT('Ctrl Pts',(94.0739641539585,-0.26104800583754,339.913234883105));
#35275=CARTESIAN_POINT('Ctrl Pts',(94.0662070441838,-0.123846282792389,
339.918600986893));
#35276=CARTESIAN_POINT('Ctrl Pts',(94.058449934409,0.0132316932650192,339.918232201187));
#35277=CARTESIAN_POINT('Ctrl Pts',(94.0506886794829,0.150382919409742,339.917863218414));
#35278=CARTESIAN_POINT('Ctrl Pts',(94.0429274245567,0.287409876515621,339.911753257175));
#35279=CARTESIAN_POINT('Ctrl Pts',(94.0351661696306,0.423800042786107,339.899956794323));
#35280=CARTESIAN_POINT('Ctrl Pts',(94.0273924992259,0.560408388873267,339.888141460975));
#35281=CARTESIAN_POINT('Ctrl Pts',(94.0196188288213,0.696377520671859,339.870621498393));
#35282=CARTESIAN_POINT('Ctrl Pts',(94.0118451584166,0.831202968369057,339.847502933251));
#35283=CARTESIAN_POINT('Ctrl Pts',(94.0044333542395,0.959752259039186,339.825460542878));
#35284=CARTESIAN_POINT('Ctrl Pts',(93.9970215500624,1.08726166490504,339.798329109787));
#35285=CARTESIAN_POINT('Ctrl Pts',(93.9896097458853,1.21330754079101,339.766242532012));
#35286=CARTESIAN_POINT('Ctrl Pts',(93.9818346671069,1.34553130052533,339.732583295479));
#35287=CARTESIAN_POINT('Ctrl Pts',(93.9740595883284,1.47656229037344,339.693364530291));
#35288=CARTESIAN_POINT('Ctrl Pts',(93.96628450955,1.60589726212151,339.64868551808));
#35289=CARTESIAN_POINT('Ctrl Pts',(93.9585189985009,1.73507307895307,339.604061486238));
#35290=CARTESIAN_POINT('Ctrl Pts',(93.9507534874519,1.86255666441301,339.553990703026));
#35291=CARTESIAN_POINT('Ctrl Pts',(93.9429879764029,1.98785638713942,339.49862312787));
#35292=CARTESIAN_POINT('Ctrl Pts',(93.9352301648807,2.11303187482587,339.443310449827));
#35293=CARTESIAN_POINT('Ctrl Pts',(93.9274723533585,2.23602745363899,339.382711588155));
#35294=CARTESIAN_POINT('Ctrl Pts',(93.9197145418363,2.35636839551839,339.317025717679));
#35295=CARTESIAN_POINT('Ctrl Pts',(93.9119625683133,2.47661877702239,339.251389277904));
#35296=CARTESIAN_POINT('Ctrl Pts',(93.9042105947903,2.59421815620286,339.180673635559));
#35297=CARTESIAN_POINT('Ctrl Pts',(93.8964586212673,2.70871380768813,339.105125158937));
#35298=CARTESIAN_POINT('Ctrl Pts',(93.8887099307097,2.82316097019724,339.02960867714));
#35299=CARTESIAN_POINT('Ctrl Pts',(93.880961240152,2.93450669374803,338.949263646651));
#35300=CARTESIAN_POINT('Ctrl Pts',(93.8732125495944,3.04232499474377,338.86438115212));
#35301=CARTESIAN_POINT('Ctrl Pts',(93.8654654712166,3.15012086324154,338.779516318101));
#35302=CARTESIAN_POINT('Ctrl Pts',(93.8577183928387,3.25439046205659,338.690116139472));
#35303=CARTESIAN_POINT('Ctrl Pts',(93.8499713144609,3.35473914733377,338.596513355438));
#35304=CARTESIAN_POINT('Ctrl Pts',(93.8422241711551,3.45508867362944,338.502909786923));
#35305=CARTESIAN_POINT('Ctrl Pts',(93.8344770278493,3.55151693501322,338.405103809366));
#35306=CARTESIAN_POINT('Ctrl Pts',(93.8267298845435,3.64366486466372,338.30346627295));
#35307=CARTESIAN_POINT('Ctrl Pts',(93.8189809995154,3.73583351112517,338.201805886257));
#35308=CARTESIAN_POINT('Ctrl Pts',(93.8112321144873,3.8237196484758,338.096312516103));
#35309=CARTESIAN_POINT('Ctrl Pts',(93.8034832294592,3.90700361379893,337.987391140153));
#35310=CARTESIAN_POINT('Ctrl Pts',(93.7957261196845,3.9903759775834,337.878354153928));
#35311=CARTESIAN_POINT('Ctrl Pts',(93.7879690099097,4.06913617371249,337.765882204615));
#35312=CARTESIAN_POINT('Ctrl Pts',(93.780211900135,4.14300681232222,337.650410839012));
#35313=CARTESIAN_POINT('Ctrl Pts',(93.7724506452088,4.21691692503935,337.534877769203));
#35314=CARTESIAN_POINT('Ctrl Pts',(93.7646893902826,4.28593207737853,337.416342427014));
#35315=CARTESIAN_POINT('Ctrl Pts',(93.7569281353565,4.34982072513485,337.29526528351));
#35316=CARTESIAN_POINT('Ctrl Pts',(93.7491544649518,4.41381157390618,337.173994456036));
#35317=CARTESIAN_POINT('Ctrl Pts',(93.7413807945471,4.47265936272183,337.050174055283));
#35318=CARTESIAN_POINT('Ctrl Pts',(93.7336071241425,4.52618025411252,336.924285677799));
#35319=CARTESIAN_POINT('Ctrl Pts',(93.7261953199655,4.57720973513215,336.804257434574));
#35320=CARTESIAN_POINT('Ctrl Pts',(93.7187835157884,4.62339699022363,336.682349679642));
#35321=CARTESIAN_POINT('Ctrl Pts',(93.7113717116114,4.66462535838777,336.558991125179));
#35322=CARTESIAN_POINT('Ctrl Pts',(93.703596632833,4.707874451689,336.429586400494));
#35323=CARTESIAN_POINT('Ctrl Pts',(93.6958215540545,4.74580294251021,336.298176121491));
#35324=CARTESIAN_POINT('Ctrl Pts',(93.6880464752761,4.77822198240916,336.16523720732));
#35325=CARTESIAN_POINT('Ctrl Pts',(93.6802809642271,4.81060112861556,336.032461882945));
#35326=CARTESIAN_POINT('Ctrl Pts',(93.6725154531781,4.83748422189758,335.898162042332));
#35327=CARTESIAN_POINT('Ctrl Pts',(93.6647499421291,4.85873131639776,335.762832260432));
#35328=CARTESIAN_POINT('Ctrl Pts',(93.6569921306069,4.87995734434189,335.627636658405));
#35329=CARTESIAN_POINT('Ctrl Pts',(93.6492343190848,4.89555843392246,335.491413530973));
#35330=CARTESIAN_POINT('Ctrl Pts',(93.6414765075626,4.9054451729057,335.354669872016));
#35331=CARTESIAN_POINT('Ctrl Pts',(93.6337245340396,4.91532447180431,335.218029117));
#35332=CARTESIAN_POINT('Ctrl Pts',(93.6259725605165,4.91949795142964,335.080868998439));
#35333=CARTESIAN_POINT('Ctrl Pts',(93.6182205869935,4.9179277924604,334.943703546777));
#35334=CARTESIAN_POINT('Ctrl Pts',(93.6104718964359,4.91635829845442,334.806596184764));
#35335=CARTESIAN_POINT('Ctrl Pts',(93.6027232058783,4.90905000825922,334.669483884179));
#35336=CARTESIAN_POINT('Ctrl Pts',(93.5949745153207,4.89601717700128,334.532882386322));
#35337=CARTESIAN_POINT('Ctrl Pts',(93.5872274369429,4.88298705733276,334.396309309548));
#35338=CARTESIAN_POINT('Ctrl Pts',(93.579480358565,4.864234802762,334.260247212973));
#35339=CARTESIAN_POINT('Ctrl Pts',(93.5717332801872,4.83982665635039,334.125208025311));
#35340=CARTESIAN_POINT('Ctrl Pts',(93.5639861368814,4.81541830537501,333.990167705891));
#35341=CARTESIAN_POINT('Ctrl Pts',(93.5562389935757,4.78535403753573,333.856150697125));
#35342=CARTESIAN_POINT('Ctrl Pts',(93.5484918502699,4.74975139700213,333.723659634276));
#35343=CARTESIAN_POINT('Ctrl Pts',(93.5407429652418,4.71414075223912,333.591138784624));
#35344=CARTESIAN_POINT('Ctrl Pts',(93.5329940802137,4.6729893585012,333.460144940959));
#35345=CARTESIAN_POINT('Ctrl Pts',(93.5252451951856,4.62646478219798,333.3311660713));
#35346=CARTESIAN_POINT('Ctrl Pts',(93.5174880854109,4.57989082422868,333.202050302135));
#35347=CARTESIAN_POINT('Ctrl Pts',(93.5097309756361,4.52793242395274,333.074954147523));
#35348=CARTESIAN_POINT('Ctrl Pts',(93.5019738658614,4.47080573039162,332.950346569881));
#35349=CARTESIAN_POINT('Ctrl Pts',(93.4942126109352,4.41364851015185,332.825672405934));
#35350=CARTESIAN_POINT('Ctrl Pts',(93.4864513560091,4.35131767108438,332.703489816744));
#35351=CARTESIAN_POINT('Ctrl Pts',(93.4786901010829,4.28407513127517,332.584242700086));
#35352=CARTESIAN_POINT('Ctrl Pts',(93.4709164306782,4.21672502531679,332.464804826904));
#35353=CARTESIAN_POINT('Ctrl Pts',(93.4631427602736,4.14444772394551,332.348312142166));
#35354=CARTESIAN_POINT('Ctrl Pts',(93.4553690898689,4.06754872696771,332.235179858247));
#35355=CARTESIAN_POINT('Ctrl Pts',(93.4479572856918,3.99422939679938,332.127313909361));
#35356=CARTESIAN_POINT('Ctrl Pts',(93.4405454815146,3.91670913884197,332.022502779932));
#35357=CARTESIAN_POINT('Ctrl Pts',(93.4331336773375,3.83528533434979,331.92107657344));
#35358=CARTESIAN_POINT('Ctrl Pts',(93.425358598559,3.74987070665105,331.814679166435));
#35359=CARTESIAN_POINT('Ctrl Pts',(93.4175835197806,3.65989028224242,331.711670647046));
#35360=CARTESIAN_POINT('Ctrl Pts',(93.4098084410021,3.56564291588129,331.612467910274));
#35361=CARTESIAN_POINT('Ctrl Pts',(93.4020429299531,3.47151152690454,331.513387248784));
#35362=CARTESIAN_POINT('Ctrl Pts',(93.3942774189041,3.3731239100977,331.418103332239));
#35363=CARTESIAN_POINT('Ctrl Pts',(93.3865119078551,3.27082023135558,331.327001486979));
#35364=CARTESIAN_POINT('Ctrl Pts',(93.3787540963329,3.16861798700885,331.235989969464));
#35365=CARTESIAN_POINT('Ctrl Pts',(93.3709962848106,3.06250769772058,331.149152529666));
#35366=CARTESIAN_POINT('Ctrl Pts',(93.3632384732884,2.95286731937084,331.06683871972));
#35367=CARTESIAN_POINT('Ctrl Pts',(93.3554864997654,2.84330944888308,330.984586853527));
#35368=CARTESIAN_POINT('Ctrl Pts',(93.3477345262425,2.73022708830162,330.906852075073));
#35369=CARTESIAN_POINT('Ctrl Pts',(93.3399825527195,2.61403203058852,330.833944358802));
#35370=CARTESIAN_POINT('Ctrl Pts',(93.3322338621619,2.49788618155103,330.761067518992));
#35371=CARTESIAN_POINT('Ctrl Pts',(93.3244851716042,2.37863058765178,330.693013882784));
#35372=CARTESIAN_POINT('Ctrl Pts',(93.3167364810466,2.25670666102128,330.630050559949));
#35373=CARTESIAN_POINT('Ctrl Pts',(93.3089894026688,2.13480810168196,330.56710033716));
#35374=CARTESIAN_POINT('Ctrl Pts',(93.3012423242909,2.01024266096208,330.509238500392));
#35375=CARTESIAN_POINT('Ctrl Pts',(93.2934952459131,1.88347667855987,330.456686378443));
#35376=CARTESIAN_POINT('Ctrl Pts',(93.2857481026073,1.7567096337368,330.404133816058));
#35377=CARTESIAN_POINT('Ctrl Pts',(93.2780009593015,1.62774237152265,330.356891206939));
#35378=CARTESIAN_POINT('Ctrl Pts',(93.2702538159957,1.49706117852844,330.31513171047));
#35379=CARTESIAN_POINT('Ctrl Pts',(93.2625049309676,1.36635060562787,330.27336282558));
#35380=CARTESIAN_POINT('Ctrl Pts',(93.2547560459395,1.23392570744121,330.237079625268));
#35381=CARTESIAN_POINT('Ctrl Pts',(93.2470071609114,1.10028750648357,330.206405266861));
#35382=CARTESIAN_POINT('Ctrl Pts',(93.2392500511367,0.966507460558331,330.175698350373));
#35383=CARTESIAN_POINT('Ctrl Pts',(93.2314929413619,0.831511920905739,330.150612255613));
#35384=CARTESIAN_POINT('Ctrl Pts',(93.2237358315872,0.695812218666052,330.13121900073));
#35385=CARTESIAN_POINT('Ctrl Pts',(93.215974576661,0.560040002844047,330.111815382711));
#35386=CARTESIAN_POINT('Ctrl Pts',(93.2082133217349,0.423563263380268,330.098110705207));
#35387=CARTESIAN_POINT('Ctrl Pts',(93.2004520668087,0.286897022290014,330.090124934268));
#35388=CARTESIAN_POINT('Ctrl Pts',(93.192678396404,0.150012159753719,330.082126388697));
#35389=CARTESIAN_POINT('Ctrl Pts',(93.1849047259994,0.0129375808524576,
330.079865037328));
#35390=CARTESIAN_POINT('Ctrl Pts',(93.1771310555947,-0.123812229994912,
330.083308674098));
#35391=CARTESIAN_POINT('Ctrl Pts',(93.1697192514176,-0.254196304247234,
330.086592008747));
#35392=CARTESIAN_POINT('Ctrl Pts',(93.1623074472405,-0.384284878722951,
330.09506113129));
#35393=CARTESIAN_POINT('Ctrl Pts',(93.1548956430634,-0.513639432302017,
330.10864460542));
#35394=CARTESIAN_POINT('Ctrl Pts',(93.147120564285,-0.649334037879509,330.122893846081));
#35395=CARTESIAN_POINT('Ctrl Pts',(93.1393454855065,-0.784649670147129,
330.142816484146));
#35396=CARTESIAN_POINT('Ctrl Pts',(93.1315704067281,-0.919074025747627,
330.168386812079));
#35397=CARTESIAN_POINT('Ctrl Pts',(93.1238048956791,-1.05333296362087,330.193925674095));
#35398=CARTESIAN_POINT('Ctrl Pts',(93.1160393846301,-1.18670242677202,330.225098325443));
#35399=CARTESIAN_POINT('Ctrl Pts',(93.108273873581,-1.31867430277485,330.261827235558));
#35400=CARTESIAN_POINT('Ctrl Pts',(93.1005160620588,-1.45051532827795,330.298519728851));
#35401=CARTESIAN_POINT('Ctrl Pts',(93.0927582505366,-1.58096115014035,330.340757413472));
#35402=CARTESIAN_POINT('Ctrl Pts',(93.0850004390145,-1.70951328890067,330.388411620973));
#35403=CARTESIAN_POINT('Ctrl Pts',(93.0772484654914,-1.83796868810056,330.436029967173));
#35404=CARTESIAN_POINT('Ctrl Pts',(93.0694964919684,-1.96453287567694,330.489056587651));
#35405=CARTESIAN_POINT('Ctrl Pts',(93.0617445184454,-2.08872234270765,330.547312941877));
#35406=CARTESIAN_POINT('Ctrl Pts',(93.0539958278878,-2.21285921542484,330.605544624502));
#35407=CARTESIAN_POINT('Ctrl Pts',(93.0462471373301,-2.33462301471646,330.66900147015));
#35408=CARTESIAN_POINT('Ctrl Pts',(93.0384984467725,-2.45355024884488,330.737456834366));
#35409=CARTESIAN_POINT('Ctrl Pts',(93.0307513683947,-2.57245273916926,330.805897955872));
#35410=CARTESIAN_POINT('Ctrl Pts',(93.0230042900168,-2.68851949967266,330.879335332474));
#35411=CARTESIAN_POINT('Ctrl Pts',(93.015257211639,-2.8013120470779,330.957496582884));
#35412=CARTESIAN_POINT('Ctrl Pts',(93.0075100683331,-2.91410553979324,331.03565848836));
#35413=CARTESIAN_POINT('Ctrl Pts',(92.9997629250273,-3.02362444340221,331.118544123978));
#35414=CARTESIAN_POINT('Ctrl Pts',(92.9920157817215,-3.12945998689764,331.205838267429));
#35415=CARTESIAN_POINT('Ctrl Pts',(92.9842668966934,-3.23531932446999,331.293152036457));
#35416=CARTESIAN_POINT('Ctrl Pts',(92.9765180116653,-3.33749335262792,331.384876036886));
#35417=CARTESIAN_POINT('Ctrl Pts',(92.9687691266372,-3.43560737371789,331.480655595689));
#35418=CARTESIAN_POINT('Ctrl Pts',(92.9610120168625,-3.53382553404348,331.576536815906));
#35419=CARTESIAN_POINT('Ctrl Pts',(92.9532549070878,-3.62797479886419,331.676481919888));
#35420=CARTESIAN_POINT('Ctrl Pts',(92.9454977973131,-3.71771789596114,331.780099891526));
#35421=CARTESIAN_POINT('Ctrl Pts',(92.9377365423869,-3.80750894889958,331.883773233295));
#35422=CARTESIAN_POINT('Ctrl Pts',(92.9299752874608,-3.89288889934658,331.991123047741));
#35423=CARTESIAN_POINT('Ctrl Pts',(92.9222140325346,-3.97356224945927,332.101727046641));
#35424=CARTESIAN_POINT('Ctrl Pts',(92.91444036213,-4.05436465064087,332.212507975894));
#35425=CARTESIAN_POINT('Ctrl Pts',(92.9066666917253,-4.13044518923159,332.326553166668));
#35426=CARTESIAN_POINT('Ctrl Pts',(92.8988930213207,-4.20155253095749,332.44341254949));
#35427=CARTESIAN_POINT('Ctrl Pts',(92.8914812171437,-4.26934980881759,332.554832099926));
#35428=CARTESIAN_POINT('Ctrl Pts',(92.8840694129667,-4.33262633511903,332.668809485685));
#35429=CARTESIAN_POINT('Ctrl Pts',(92.8766576087897,-4.39120487323533,332.784937286718));
#35430=CARTESIAN_POINT('Ctrl Pts',(92.8683539196665,-4.45683234506283,332.915039099356));
#35431=CARTESIAN_POINT('Ctrl Pts',(92.8600502305431,-4.51674859593692,333.048207284752));
#35432=CARTESIAN_POINT('Ctrl Pts',(92.8517465414198,-4.57067641724909,333.183932778969));
#35433=CARTESIAN_POINT('Ctrl Pts',(92.8434591402355,-4.6244984574984,333.319392043498));
#35434=CARTESIAN_POINT('Ctrl Pts',(92.8351717390511,-4.67235536885029,333.457398331321));
#35435=CARTESIAN_POINT('Ctrl Pts',(92.8268843378668,-4.71401640749578,333.597419388284));
#35436=CARTESIAN_POINT('Ctrl Pts',(92.8186195205387,-4.75556391635215,333.737058876242));
#35437=CARTESIAN_POINT('Ctrl Pts',(92.8103547032106,-4.79094913653858,333.878701887954));
#35438=CARTESIAN_POINT('Ctrl Pts',(92.8020898858825,-4.81999013535232,334.021798508687));
#35439=CARTESIAN_POINT('Ctrl Pts',(92.793839113524,-4.84898178280976,334.164651955542));
#35440=CARTESIAN_POINT('Ctrl Pts',(92.7855883411655,-4.87165063190238,334.308953787067));
#35441=CARTESIAN_POINT('Ctrl Pts',(92.777337568807,-4.88786446438492,334.454139174969));
#35442=CARTESIAN_POINT('Ctrl Pts',(92.7691055753873,-4.90404139382923,334.598994117746));
#35443=CARTESIAN_POINT('Ctrl Pts',(92.7608735819676,-4.91379256717959,334.744728300258));
#35444=CARTESIAN_POINT('Ctrl Pts',(92.7526415885479,-4.91703684368418,334.890767494067));
#35445=CARTESIAN_POINT('Ctrl Pts',(92.7506064752088,-4.91783889369244,334.926871302246));
#35446=CARTESIAN_POINT('Ctrl Pts',(92.7485713618697,-4.91824350085643,334.962993700791));
#35447=CARTESIAN_POINT('Ctrl Pts',(92.7465362485306,-4.91824992232871,334.999125921265));
#35448=CARTESIAN_POINT('',(96.2465362485274,-4.91824904506439,335.003064836579));
#35449=CARTESIAN_POINT('Ctrl Pts',(96.2465362484899,-4.91824904506398,335.003064837238));
#35450=CARTESIAN_POINT('Ctrl Pts',(96.2361955056856,-4.91813576058702,335.184856308468));
#35451=CARTESIAN_POINT('Ctrl Pts',(96.2258547628812,-4.90794384176267,335.366332575828));
#35452=CARTESIAN_POINT('Ctrl Pts',(96.2155140200769,-4.88777377337727,335.546672299267));
#35453=CARTESIAN_POINT('Ctrl Pts',(96.2077389412984,-4.87260814421216,335.682267544516));
#35454=CARTESIAN_POINT('Ctrl Pts',(96.19996386252,-4.85177180734536,335.817445497264));
#35455=CARTESIAN_POINT('Ctrl Pts',(96.1921887837416,-4.82529393069937,335.951694039519));
#35456=CARTESIAN_POINT('Ctrl Pts',(96.1844232726926,-4.7988486367663,336.085777380395));
#35457=CARTESIAN_POINT('Ctrl Pts',(96.1766577616436,-4.76677569110059,336.218933206589));
#35458=CARTESIAN_POINT('Ctrl Pts',(96.1688922505946,-4.72915605515843,336.350653941044));
#35459=CARTESIAN_POINT('Ctrl Pts',(96.1611344390724,-4.69157371919482,336.482244074007));
#35460=CARTESIAN_POINT('Ctrl Pts',(96.1533766275502,-4.64845574403999,336.612401573453));
#35461=CARTESIAN_POINT('Ctrl Pts',(96.145618816028,-4.59993416278677,336.740628840542));
#35462=CARTESIAN_POINT('Ctrl Pts',(96.137866842505,-4.55144909556219,336.868759612546));
#35463=CARTESIAN_POINT('Ctrl Pts',(96.130114868982,-4.49756865395786,336.994962679341));
#35464=CARTESIAN_POINT('Ctrl Pts',(96.122362895459,-4.43847464087635,337.118755749207));
#35465=CARTESIAN_POINT('Ctrl Pts',(96.1146142049014,-4.37940565414439,337.242496392634));
#35466=CARTESIAN_POINT('Ctrl Pts',(96.1068655143438,-4.31512765542954,337.363828717093));
#35467=CARTESIAN_POINT('Ctrl Pts',(96.0991168237861,-4.24587041522989,337.482290772568));
#35468=CARTESIAN_POINT('Ctrl Pts',(96.0913697454083,-4.17662758457751,337.600728181022));
#35469=CARTESIAN_POINT('Ctrl Pts',(96.0836226670305,-4.10240777021781,337.716296171107));
#35470=CARTESIAN_POINT('Ctrl Pts',(96.0758755886527,-4.02348630949061,337.828558109681));
#35471=CARTESIAN_POINT('Ctrl Pts',(96.0681284453469,-3.94456418732567,337.940820989118));
#35472=CARTESIAN_POINT('Ctrl Pts',(96.0603813020411,-3.86094056499591,338.049777442014));
#35473=CARTESIAN_POINT('Ctrl Pts',(96.0526341587353,-3.77293341915518,338.155020836242));
#35474=CARTESIAN_POINT('Ctrl Pts',(96.0448852737072,-3.68490648743968,338.26028789142));
#35475=CARTESIAN_POINT('Ctrl Pts',(96.0371363886791,-3.59249432185405,338.361839927029));
#35476=CARTESIAN_POINT('Ctrl Pts',(96.0293875036511,-3.49605411868056,338.459304650035));
#35477=CARTESIAN_POINT('Ctrl Pts',(96.0216303938763,-3.39951155287887,338.556872823106));
#35478=CARTESIAN_POINT('Ctrl Pts',(96.0138732841016,-3.2989326843352,338.650344739096));
#35479=CARTESIAN_POINT('Ctrl Pts',(96.0061161743269,-3.19471079875179,338.739385775076));
#35480=CARTESIAN_POINT('Ctrl Pts',(95.9983549194007,-3.09043322032509,338.828474391738));
#35481=CARTESIAN_POINT('Ctrl Pts',(95.9905936644746,-2.98250905325593,338.91312716938));
#35482=CARTESIAN_POINT('Ctrl Pts',(95.9828324095484,-2.87136257243016,338.993051469759));
#35483=CARTESIAN_POINT('Ctrl Pts',(95.9750587391437,-2.76003829345763,339.073103622972));
#35484=CARTESIAN_POINT('Ctrl Pts',(95.9672850687391,-2.64548172699808,339.148411968937));
#35485=CARTESIAN_POINT('Ctrl Pts',(95.9595113983344,-2.5281446301959,339.218728219655));
#35486=CARTESIAN_POINT('Ctrl Pts',(95.9520995941572,-2.41626960347716,339.285771231986));
#35487=CARTESIAN_POINT('Ctrl Pts',(95.94468778998,-2.30186734070033,339.348276315923));
#35488=CARTESIAN_POINT('Ctrl Pts',(95.9372759858027,-2.18534644997726,339.406068991297));
#35489=CARTESIAN_POINT('Ctrl Pts',(95.9295009070243,-2.06311452330447,339.466694257846));
#35490=CARTESIAN_POINT('Ctrl Pts',(95.9217258282459,-1.93816476147536,339.522325084392));
#35491=CARTESIAN_POINT('Ctrl Pts',(95.9139507494674,-1.81094359987295,339.572708862434));
#35492=CARTESIAN_POINT('Ctrl Pts',(95.9061852384184,-1.68387899200919,339.623030640028));
#35493=CARTESIAN_POINT('Ctrl Pts',(95.8984197273694,-1.55454890576231,339.668118073805));
#35494=CARTESIAN_POINT('Ctrl Pts',(95.8906542163204,-1.42342398639763,339.707764566909));
#35495=CARTESIAN_POINT('Ctrl Pts',(95.8828964047982,-1.29242907777226,339.7473717504));
#35496=CARTESIAN_POINT('Ctrl Pts',(95.875138593276,-1.15964324923439,339.781548616597));
#35497=CARTESIAN_POINT('Ctrl Pts',(95.8673807817538,-1.02555639294622,339.810136915659));
#35498=CARTESIAN_POINT('Ctrl Pts',(95.8596288082308,-0.891570441269536,
339.83870370112));
#35499=CARTESIAN_POINT('Ctrl Pts',(95.8518768347078,-0.756285791365676,
339.861690209259));
#35500=CARTESIAN_POINT('Ctrl Pts',(95.8441248611848,-0.620206396613705,
339.878988326293));
#35501=CARTESIAN_POINT('Ctrl Pts',(95.8363761706271,-0.484184631566295,
339.896279117563));
#35502=CARTESIAN_POINT('Ctrl Pts',(95.8286274800695,-0.347369178041581,
339.907886259945));
#35503=CARTESIAN_POINT('Ctrl Pts',(95.8208787895119,-0.210272841664043,
339.913752984691));
#35504=CARTESIAN_POINT('Ctrl Pts',(95.8131317111341,-0.0732050293243404,
339.919618488816));
#35505=CARTESIAN_POINT('Ctrl Pts',(95.8053846327563,0.0641431593551316,
339.919745934235));
#35506=CARTESIAN_POINT('Ctrl Pts',(95.7976375543785,0.201255549417171,339.914130570745));
#35507=CARTESIAN_POINT('Ctrl Pts',(95.7898904110726,0.338369088613009,339.908515160192));
#35508=CARTESIAN_POINT('Ctrl Pts',(95.7821432677668,0.475246434702793,339.897156860725));
#35509=CARTESIAN_POINT('Ctrl Pts',(95.774396124461,0.611373566642237,339.880103013719));
#35510=CARTESIAN_POINT('Ctrl Pts',(95.7666472394329,0.74753130285091,339.863045332646));
#35511=CARTESIAN_POINT('Ctrl Pts',(95.7588983544049,0.882938101519794,339.840289604601));
#35512=CARTESIAN_POINT('Ctrl Pts',(95.7511494693768,1.01708759408973,339.811934734434));
#35513=CARTESIAN_POINT('Ctrl Pts',(95.743392359602,1.15137947431728,339.783549768115));
#35514=CARTESIAN_POINT('Ctrl Pts',(95.7356352498273,1.28441099959263,339.74955386896));
#35515=CARTESIAN_POINT('Ctrl Pts',(95.7278781400526,1.41568794889479,339.710096675638));
#35516=CARTESIAN_POINT('Ctrl Pts',(95.7201168851264,1.54703504840114,339.670618397654));
#35517=CARTESIAN_POINT('Ctrl Pts',(95.7123556302003,1.67662533459653,339.625673138461));
#35518=CARTESIAN_POINT('Ctrl Pts',(95.7045943752741,1.8039831222545,339.575459316519));
#35519=CARTESIAN_POINT('Ctrl Pts',(95.6968207048694,1.93154464086691,339.525165168827));
#35520=CARTESIAN_POINT('Ctrl Pts',(95.6890470344647,2.0568661669874,339.469585775327));
#35521=CARTESIAN_POINT('Ctrl Pts',(95.6812733640601,2.17949443822818,339.408966665357));
#35522=CARTESIAN_POINT('Ctrl Pts',(95.673861559883,2.29641433393921,339.351169389542));
#35523=CARTESIAN_POINT('Ctrl Pts',(95.666449755706,2.41088582129536,339.288791173568));
#35524=CARTESIAN_POINT('Ctrl Pts',(95.659037951529,2.52254105490457,339.222081203485));
#35525=CARTESIAN_POINT('Ctrl Pts',(95.6512628727505,2.63966884411758,339.152101579049));
#35526=CARTESIAN_POINT('Ctrl Pts',(95.6434877939721,2.75406747873376,339.077133690981));
#35527=CARTESIAN_POINT('Ctrl Pts',(95.6357127151937,2.86528294307118,338.997416255364));
#35528=CARTESIAN_POINT('Ctrl Pts',(95.6279472041447,2.97636154969935,338.917796917126));
#35529=CARTESIAN_POINT('Ctrl Pts',(95.6201816930957,3.08426446528733,338.833439885998));
#35530=CARTESIAN_POINT('Ctrl Pts',(95.6124161820467,3.18856326497391,338.744629136211));
#35531=CARTESIAN_POINT('Ctrl Pts',(95.6046583705245,3.29275865209695,338.655906442541));
#35532=CARTESIAN_POINT('Ctrl Pts',(95.5969005590022,3.39335673908397,338.562739069829));
#35533=CARTESIAN_POINT('Ctrl Pts',(95.58914274748,3.48995934150991,338.465453340778));
#35534=CARTESIAN_POINT('Ctrl Pts',(95.581390773957,3.58648924741407,338.368240822323));
#35535=CARTESIAN_POINT('Ctrl Pts',(95.573638800434,3.6790293791985,338.266916392567));
#35536=CARTESIAN_POINT('Ctrl Pts',(95.565886826911,3.76721610358526,338.161845330086));
#35537=CARTESIAN_POINT('Ctrl Pts',(95.5581381363534,3.85536548084189,338.056818765263));
#35538=CARTESIAN_POINT('Ctrl Pts',(95.5503894457958,3.93916486686945,337.948049022325));
#35539=CARTESIAN_POINT('Ctrl Pts',(95.5426407552382,4.01828901506963,337.835936609635));
#35540=CARTESIAN_POINT('Ctrl Pts',(95.5348936768603,4.09739670082993,337.72384752287));
#35541=CARTESIAN_POINT('Ctrl Pts',(95.5271465984825,4.1718308583338,337.608417468844));
#35542=CARTESIAN_POINT('Ctrl Pts',(95.5193995201046,4.24130816114614,337.490077939482));
#35543=CARTESIAN_POINT('Ctrl Pts',(95.5116523767988,4.31078604624514,337.371737418321));
#35544=CARTESIAN_POINT('Ctrl Pts',(95.503905233493,4.37530679589446,337.250487710264));
#35545=CARTESIAN_POINT('Ctrl Pts',(95.4961580901872,4.43463205418474,337.126786685706));
#35546=CARTESIAN_POINT('Ctrl Pts',(95.4884092051591,4.4939706500526,337.003057850532));
#35547=CARTESIAN_POINT('Ctrl Pts',(95.480660320131,4.54811126126718,336.876876954585));
#35548=CARTESIAN_POINT('Ctrl Pts',(95.4729114351029,4.5968630339452,336.74872333708));
#35549=CARTESIAN_POINT('Ctrl Pts',(95.4651543253282,4.64566655225844,336.620433696001));
#35550=CARTESIAN_POINT('Ctrl Pts',(95.4573972155535,4.68906966706212,336.490167516577));
#35551=CARTESIAN_POINT('Ctrl Pts',(95.4496401057787,4.72693076135279,336.358421377878));
#35552=CARTESIAN_POINT('Ctrl Pts',(95.4418788508526,4.76481208740169,336.226604838256));
#35553=CARTESIAN_POINT('Ctrl Pts',(95.4341175959264,4.79714539983116,336.093307143199));
#35554=CARTESIAN_POINT('Ctrl Pts',(95.4263563410002,4.82384013238535,335.959035682177));
#35555=CARTESIAN_POINT('Ctrl Pts',(95.4185826705956,4.85057756781183,335.824549430576));
#35556=CARTESIAN_POINT('Ctrl Pts',(95.4108090001909,4.87165833881507,335.689086686676));
#35557=CARTESIAN_POINT('Ctrl Pts',(95.4030353297863,4.88704362996701,335.553161478502));
#35558=CARTESIAN_POINT('Ctrl Pts',(95.3956235256092,4.90171273211439,335.42356362147));
#35559=CARTESIAN_POINT('Ctrl Pts',(95.388211721432,4.91120464970279,335.293545673685));
#35560=CARTESIAN_POINT('Ctrl Pts',(95.3807999172549,4.91552986634681,335.163551813052));
#35561=CARTESIAN_POINT('Ctrl Pts',(95.3730248384765,4.92006707474269,335.027186566078));
#35562=CARTESIAN_POINT('Ctrl Pts',(95.3652497596981,4.91893264367984,334.890416887752));
#35563=CARTESIAN_POINT('Ctrl Pts',(95.3574746809196,4.91208162066749,334.753753752515));
#35564=CARTESIAN_POINT('Ctrl Pts',(95.3497091698706,4.9052390282751,334.617258789966));
#35565=CARTESIAN_POINT('Ctrl Pts',(95.3419436588216,4.89269386021368,334.480870496291));
#35566=CARTESIAN_POINT('Ctrl Pts',(95.3341781477726,4.8744530711977,334.345102817847));
#35567=CARTESIAN_POINT('Ctrl Pts',(95.3264203362504,4.85623036797715,334.209469753453));
#35568=CARTESIAN_POINT('Ctrl Pts',(95.3186625247282,4.83232333381084,334.074456464622));
#35569=CARTESIAN_POINT('Ctrl Pts',(95.310904713206,4.80279089998048,333.940574385072));
#35570=CARTESIAN_POINT('Ctrl Pts',(95.303152739683,4.7732806902431,333.806793056033));
#35571=CARTESIAN_POINT('Ctrl Pts',(95.29540076616,4.73815359085979,333.674141622023));
#35572=CARTESIAN_POINT('Ctrl Pts',(95.287648792637,4.69751998954568,333.54312354322));
#35573=CARTESIAN_POINT('Ctrl Pts',(95.2799001020794,4.65690359658586,333.412160950652));
#35574=CARTESIAN_POINT('Ctrl Pts',(95.2721514115218,4.61078545543573,333.282830710049));
#35575=CARTESIAN_POINT('Ctrl Pts',(95.2644027209641,4.55932635252582,333.155623066273));
#35576=CARTESIAN_POINT('Ctrl Pts',(95.2566556425863,4.50787795611206,333.02844188911));
#35577=CARTESIAN_POINT('Ctrl Pts',(95.2489085642085,4.45109095474543,332.903382792473));
#35578=CARTESIAN_POINT('Ctrl Pts',(95.2411614858307,4.38917487500052,332.780917536646));
#35579=CARTESIAN_POINT('Ctrl Pts',(95.2334143425249,4.32725827633928,332.658451254443));
#35580=CARTESIAN_POINT('Ctrl Pts',(95.2256671992191,4.26021268991968,332.538579205236));
#35581=CARTESIAN_POINT('Ctrl Pts',(95.2179200559133,4.18829416066721,332.42174960754));
#35582=CARTESIAN_POINT('Ctrl Pts',(95.2101711708852,4.11635946260249,332.304893744069));
#35583=CARTESIAN_POINT('Ctrl Pts',(95.2024222858571,4.0395498465652,332.191082026005));
#35584=CARTESIAN_POINT('Ctrl Pts',(95.194673400829,3.95816511713959,332.080734344401));
#35585=CARTESIAN_POINT('Ctrl Pts',(95.1869162910543,3.87669400512125,331.970269538628));
#35586=CARTESIAN_POINT('Ctrl Pts',(95.1791591812796,3.7906383116269,331.863276429067));
#35587=CARTESIAN_POINT('Ctrl Pts',(95.1714020715048,3.7003389835044,331.760142831905));
#35588=CARTESIAN_POINT('Ctrl Pts',(95.1636408165787,3.60999140230822,331.656954123446));
#35589=CARTESIAN_POINT('Ctrl Pts',(95.1558795616525,3.51539593739415,331.557629319808));
#35590=CARTESIAN_POINT('Ctrl Pts',(95.1481183067264,3.41693025279318,331.462519157642));
#35591=CARTESIAN_POINT('Ctrl Pts',(95.1403446363217,3.31830705518674,331.367256850213));
#35592=CARTESIAN_POINT('Ctrl Pts',(95.1325709659171,3.21580155867471,331.276222916564));
#35593=CARTESIAN_POINT('Ctrl Pts',(95.1247972955124,3.10982501513417,331.189728167473));
#35594=CARTESIAN_POINT('Ctrl Pts',(95.1173854913353,3.00878170519172,331.107259769763));
#35595=CARTESIAN_POINT('Ctrl Pts',(95.1099736871582,2.90458346034091,331.028917641786));
#35596=CARTESIAN_POINT('Ctrl Pts',(95.1025618829811,2.79760947254461,330.954933337802));
#35597=CARTESIAN_POINT('Ctrl Pts',(95.0947868042026,2.68539237094752,330.877322842691));
#35598=CARTESIAN_POINT('Ctrl Pts',(95.0870117254242,2.56976592484781,330.804262889189));
#35599=CARTESIAN_POINT('Ctrl Pts',(95.0792366466458,2.45113549718315,330.736067796394));
#35600=CARTESIAN_POINT('Ctrl Pts',(95.0714711355968,2.33265105181212,330.667956622003));
#35601=CARTESIAN_POINT('Ctrl Pts',(95.0637056245478,2.21117031566477,330.604698589799));
#35602=CARTESIAN_POINT('Ctrl Pts',(95.0559401134988,2.08712924079251,330.546565977279));
#35603=CARTESIAN_POINT('Ctrl Pts',(95.0481823019766,1.96321115300712,330.488491003414));
#35604=CARTESIAN_POINT('Ctrl Pts',(95.0404244904544,1.83673813007454,330.435531500831));
#35605=CARTESIAN_POINT('Ctrl Pts',(95.0326666789322,1.70817213861591,330.38791467909));
#35606=CARTESIAN_POINT('Ctrl Pts',(95.0249147054091,1.579702897143,330.340333690516));
#35607=CARTESIAN_POINT('Ctrl Pts',(95.0171627318861,1.44914418722087,330.298087515311));
#35608=CARTESIAN_POINT('Ctrl Pts',(95.0094107583631,1.31697911638087,330.26135577728));
#35609=CARTESIAN_POINT('Ctrl Pts',(95.0016620678055,1.18487001752685,330.224639595162));
#35610=CARTESIAN_POINT('Ctrl Pts',(94.9939133772479,1.05115628662986,330.193433309785));
#35611=CARTESIAN_POINT('Ctrl Pts',(94.9861646866903,0.916337191815168,330.167867012033));
#35612=CARTESIAN_POINT('Ctrl Pts',(94.9784176083124,0.78154614723918,330.142306033563));
#35613=CARTESIAN_POINT('Ctrl Pts',(94.9706705299346,0.645650579981453,330.122382781431));
#35614=CARTESIAN_POINT('Ctrl Pts',(94.9629234515567,0.509160590181383,330.108176356827));
#35615=CARTESIAN_POINT('Ctrl Pts',(94.9551763082509,0.372669456463735,330.09396981316));
#35616=CARTESIAN_POINT('Ctrl Pts',(94.9474291649451,0.235584279041177,330.085480233053));
#35617=CARTESIAN_POINT('Ctrl Pts',(94.9396820216393,0.0984205350251209,
330.082734859621));
#35618=CARTESIAN_POINT('Ctrl Pts',(94.9319331366112,-0.0387740463125655,
330.079988868971));
#35619=CARTESIAN_POINT('Ctrl Pts',(94.9241842515831,-0.176046838672367,
330.082989662599));
#35620=CARTESIAN_POINT('Ctrl Pts',(94.916435366555,-0.312882505244331,330.091712355575));
#35621=CARTESIAN_POINT('Ctrl Pts',(94.9086782567803,-0.449863410606665,
330.100444306909));
#35622=CARTESIAN_POINT('Ctrl Pts',(94.9009211470056,-0.586405872659239,
330.114910264639));
#35623=CARTESIAN_POINT('Ctrl Pts',(94.8931640372308,-0.721999262592784,
330.13503338888));
#35624=CARTESIAN_POINT('Ctrl Pts',(94.8854027823047,-0.857665109298382,
330.155167266275));
#35625=CARTESIAN_POINT('Ctrl Pts',(94.8776415273785,-0.99238048963109,330.180964260322));
#35626=CARTESIAN_POINT('Ctrl Pts',(94.8698802724523,-1.12564608597999,330.212296589009));
#35627=CARTESIAN_POINT('Ctrl Pts',(94.8621066020477,-1.25912486385199,330.24367903921));
#35628=CARTESIAN_POINT('Ctrl Pts',(94.854332931643,-1.39114884670889,330.280614413062));
#35629=CARTESIAN_POINT('Ctrl Pts',(94.8465592612384,-1.52123411514601,330.322925077635));
#35630=CARTESIAN_POINT('Ctrl Pts',(94.8391474570613,-1.64526388304059,330.363266170593));
#35631=CARTESIAN_POINT('Ctrl Pts',(94.8317356528842,-1.76753109899429,330.408493276942));
#35632=CARTESIAN_POINT('Ctrl Pts',(94.8243238487071,-1.88763584156343,330.458412833365));
#35633=CARTESIAN_POINT('Ctrl Pts',(94.8165487699287,-2.01362727533945,330.510779095951));
#35634=CARTESIAN_POINT('Ctrl Pts',(94.8087736911502,-2.13763705353376,330.568474908239));
#35635=CARTESIAN_POINT('Ctrl Pts',(94.8009986123718,-2.25918149336502,330.631329487986));
#35636=CARTESIAN_POINT('Ctrl Pts',(94.7932331013228,-2.38057636502517,330.694106721172));
#35637=CARTESIAN_POINT('Ctrl Pts',(94.7854675902738,-2.49951159074864,330.762029912906));
#35638=CARTESIAN_POINT('Ctrl Pts',(94.7777020792248,-2.6155222879101,330.834879806783));
#35639=CARTESIAN_POINT('Ctrl Pts',(94.7699442677026,-2.73141796012757,330.907657469778));
#35640=CARTESIAN_POINT('Ctrl Pts',(94.7621864561804,-2.84439454541985,330.985351907283));
#35641=CARTESIAN_POINT('Ctrl Pts',(94.7544286446582,-2.954010981776,331.067697597838));
#35642=CARTESIAN_POINT('Ctrl Pts',(94.7466766711352,-3.0635449282875,331.14998132065));
#35643=CARTESIAN_POINT('Ctrl Pts',(94.7389246976122,-3.16972344769618,331.236909095683));
#35644=CARTESIAN_POINT('Ctrl Pts',(94.7311727240892,-3.27213405330532,331.328171872255));
#35645=CARTESIAN_POINT('Ctrl Pts',(94.7234240335316,-3.37450128796226,331.419395998987));
#35646=CARTESIAN_POINT('Ctrl Pts',(94.715675342974,-3.47310349137332,331.514951216322));
#35647=CARTESIAN_POINT('Ctrl Pts',(94.7079266524164,-3.56756108470789,331.614488078683));
#35648=CARTESIAN_POINT('Ctrl Pts',(94.7001795740386,-3.66199902535125,331.714004231569));
#35649=CARTESIAN_POINT('Ctrl Pts',(94.6924324956608,-3.75229380224291,331.817500098356));
#35650=CARTESIAN_POINT('Ctrl Pts',(94.684685417283,-3.83810285304755,331.924589531147));
#35651=CARTESIAN_POINT('Ctrl Pts',(94.6769382739772,-3.92391262301458,332.031679861451));
#35652=CARTESIAN_POINT('Ctrl Pts',(94.6691911306714,-4.00523634749315,332.142363512802));
#35653=CARTESIAN_POINT('Ctrl Pts',(94.6614439873656,-4.08177216292266,332.256221752311));
#35654=CARTESIAN_POINT('Ctrl Pts',(94.6536951023375,-4.15832518522842,332.370105589571));
#35655=CARTESIAN_POINT('Ctrl Pts',(94.6459462173094,-4.23008793850525,332.48716511087));
#35656=CARTESIAN_POINT('Ctrl Pts',(94.6381973322813,-4.29680247070164,332.606953491828));
#35657=CARTESIAN_POINT('Ctrl Pts',(94.6304402225066,-4.36358781439183,332.726869017413));
#35658=CARTESIAN_POINT('Ctrl Pts',(94.6226831127319,-4.42531404294046,332.849518846542));
#35659=CARTESIAN_POINT('Ctrl Pts',(94.6149260029572,-4.48176944209824,332.974431998087));
#35660=CARTESIAN_POINT('Ctrl Pts',(94.607164748031,-4.53825500921624,333.099411899226));
#35661=CARTESIAN_POINT('Ctrl Pts',(94.5994034931048,-4.5894639888321,333.226657170284));
#35662=CARTESIAN_POINT('Ctrl Pts',(94.5916422381787,-4.63523362615662,333.355678774252));
#35663=CARTESIAN_POINT('Ctrl Pts',(94.583868567774,-4.68107647998455,333.484906770737));
#35664=CARTESIAN_POINT('Ctrl Pts',(94.5760948973694,-4.72146248878933,333.615916404672));
#35665=CARTESIAN_POINT('Ctrl Pts',(94.5683212269647,-4.7562791513337,333.748204610534));
#35666=CARTESIAN_POINT('Ctrl Pts',(94.5609094227876,-4.78947508986059,333.874334768588));
#35667=CARTESIAN_POINT('Ctrl Pts',(94.5534976186104,-4.8176084574982,334.001626861317));
#35668=CARTESIAN_POINT('Ctrl Pts',(94.5460858144332,-4.84062560532807,334.129639838031));
#35669=CARTESIAN_POINT('Ctrl Pts',(94.5342147471232,-4.87749086844671,334.334670978468));
#35670=CARTESIAN_POINT('Ctrl Pts',(94.5223436798131,-4.90133740109321,334.54210843251));
#35671=CARTESIAN_POINT('Ctrl Pts',(94.510472612503,-4.91192361891552,334.750621924701));
#35672=CARTESIAN_POINT('Ctrl Pts',(94.505827157832,-4.91606627885895,334.832218629611));
#35673=CARTESIAN_POINT('Ctrl Pts',(94.5011817031609,-4.91817873928009,334.913979820873));
#35674=CARTESIAN_POINT('Ctrl Pts',(94.4965362484899,-4.91824822735267,334.995824279422));
#35675=CARTESIAN_POINT('',(97.9965362484409,-4.91824934462186,335.002539020807));
#35676=CARTESIAN_POINT('Ctrl Pts',(97.9965362484409,-4.91824934462186,335.002539020807));
#35677=CARTESIAN_POINT('Ctrl Pts',(97.9879926354055,-4.91817110136582,335.154101324522));
#35678=CARTESIAN_POINT('Ctrl Pts',(97.9794490223701,-4.9110828885401,335.305421301889));
#35679=CARTESIAN_POINT('Ctrl Pts',(97.9709054093347,-4.89707624575504,335.455880802142));
#35680=CARTESIAN_POINT('Ctrl Pts',(97.9623163776358,-4.882995142318,335.607140159482));
#35681=CARTESIAN_POINT('Ctrl Pts',(97.9537273459368,-4.86192194224941,335.757529630768));
#35682=CARTESIAN_POINT('Ctrl Pts',(97.9451383142378,-4.83399989550252,335.906437020858));
#35683=CARTESIAN_POINT('Ctrl Pts',(97.9365257974073,-4.80600150104108,336.055751570889));
#35684=CARTESIAN_POINT('Ctrl Pts',(97.9279132805768,-4.77111687327354,336.203575703206));
#35685=CARTESIAN_POINT('Ctrl Pts',(97.9193007637463,-4.72953924477512,336.349311526161));
#35686=CARTESIAN_POINT('Ctrl Pts',(97.9106573473402,-4.68781244605122,336.495570213127));
#35687=CARTESIAN_POINT('Ctrl Pts',(97.902013930934,-4.63934465573974,336.639725363794));
#35688=CARTESIAN_POINT('Ctrl Pts',(97.8933705145278,-4.58437848914165,336.781195365701));
#35689=CARTESIAN_POINT('Ctrl Pts',(97.8905610849254,-4.5665124546577,336.827178341938));
#35690=CARTESIAN_POINT('Ctrl Pts',(97.887751655323,-4.54796023666128,336.872877826948));
#35691=CARTESIAN_POINT('Ctrl Pts',(97.8849422257206,-4.52873120316474,336.918274420406));
#35692=CARTESIAN_POINT('Ctrl Pts',(97.8771671469422,-4.47551497374203,337.043909207659));
#35693=CARTESIAN_POINT('Ctrl Pts',(97.8693920681638,-4.41698270373259,337.167526379649));
#35694=CARTESIAN_POINT('Ctrl Pts',(97.8616169893853,-4.35330843910294,337.288643418389));
#35695=CARTESIAN_POINT('Ctrl Pts',(97.8538514783363,-4.28971252970961,337.409611414902));
#35696=CARTESIAN_POINT('Ctrl Pts',(97.8460859672873,-4.22098739585917,337.528085056993));
#35697=CARTESIAN_POINT('Ctrl Pts',(97.8383204562383,-4.1473554295654,337.64360095388));
#35698=CARTESIAN_POINT('Ctrl Pts',(97.8305626447161,-4.07379646958064,337.759002316418));
#35699=CARTESIAN_POINT('Ctrl Pts',(97.8228048331939,-3.99534056779839,337.871451442333));
#35700=CARTESIAN_POINT('Ctrl Pts',(97.8150470216717,-3.91225621930559,337.980509073465));
#35701=CARTESIAN_POINT('Ctrl Pts',(97.8072950481487,-3.8292343944195,338.089484635271));
#35702=CARTESIAN_POINT('Ctrl Pts',(97.7995430746256,-3.74159129158938,338.195073472666));
#35703=CARTESIAN_POINT('Ctrl Pts',(97.7917911011026,-3.64963874108538,338.296865196223));
#35704=CARTESIAN_POINT('Ctrl Pts',(97.784042410545,-3.55772513254136,338.398613810925));
#35705=CARTESIAN_POINT('Ctrl Pts',(97.7762937199874,-3.46150596769722,338.496568220699));
#35706=CARTESIAN_POINT('Ctrl Pts',(97.7685450294297,-3.36133324847963,338.59035121613));
#35707=CARTESIAN_POINT('Ctrl Pts',(97.7607979510519,-3.26118137103292,338.684114699225));
#35708=CARTESIAN_POINT('Ctrl Pts',(97.7530508726741,-3.15707786052404,338.773708227315));
#35709=CARTESIAN_POINT('Ctrl Pts',(97.7453037942962,-3.04941117028915,338.858791854586));
#35710=CARTESIAN_POINT('Ctrl Pts',(97.7375566509904,-2.94174357770384,338.943876194939));
#35711=CARTESIAN_POINT('Ctrl Pts',(97.7298095076846,-2.83051305250342,339.024450316733));
#35712=CARTESIAN_POINT('Ctrl Pts',(97.7220623643788,-2.71614035732249,339.100215192136));
#35713=CARTESIAN_POINT('Ctrl Pts',(97.7143134793507,-2.60174194873155,339.175997101091));
#35714=CARTESIAN_POINT('Ctrl Pts',(97.7065645943227,-2.48420029024814,339.246967396325));
#35715=CARTESIAN_POINT('Ctrl Pts',(97.6988157092946,-2.36396393870532,339.31287115029));
#35716=CARTESIAN_POINT('Ctrl Pts',(97.6910585995198,-2.24359996705653,339.378844855179));
#35717=CARTESIAN_POINT('Ctrl Pts',(97.6833014897451,-2.12053593218395,339.43974108821));
#35718=CARTESIAN_POINT('Ctrl Pts',(97.6755443799704,-1.99524423475104,339.495351321776));
#35719=CARTESIAN_POINT('Ctrl Pts',(97.6677831250442,-1.86988558544098,339.550991271673));
#35720=CARTESIAN_POINT('Ctrl Pts',(97.660021870118,-1.74229726501254,339.601339450293));
#35721=CARTESIAN_POINT('Ctrl Pts',(97.6522606151919,-1.61296939884124,339.646236410354));
#35722=CARTESIAN_POINT('Ctrl Pts',(97.6444869447872,-1.483434650232,339.69120519092));
#35723=CARTESIAN_POINT('Ctrl Pts',(97.6367132743825,-1.35215516970395,339.730705214759));
#35724=CARTESIAN_POINT('Ctrl Pts',(97.6289396039779,-1.21963477132505,339.764627381766));
#35725=CARTESIAN_POINT('Ctrl Pts',(97.6215277998007,-1.09328322937226,339.796970463738));
#35726=CARTESIAN_POINT('Ctrl Pts',(97.6141159956236,-0.965803980530105,
339.824243240654));
#35727=CARTESIAN_POINT('Ctrl Pts',(97.6067041914464,-0.837638427861508,
339.846395044429));
#35728=CARTESIAN_POINT('Ctrl Pts',(97.598929112668,-0.703191099672106,339.869632574095));
#35729=CARTESIAN_POINT('Ctrl Pts',(97.5911540338895,-0.567563612605447,
339.887307884428));
#35730=CARTESIAN_POINT('Ctrl Pts',(97.5833789551111,-0.43125591259095,339.899306216226));
#35731=CARTESIAN_POINT('Ctrl Pts',(97.5756134440621,-0.295115947879001,
339.911289783313));
#35732=CARTESIAN_POINT('Ctrl Pts',(97.567847933013,-0.158297821345965,339.917610237824));
#35733=CARTESIAN_POINT('Ctrl Pts',(97.560082421964,-0.0213115572672648,
339.918203826604));
#35734=CARTESIAN_POINT('Ctrl Pts',(97.5523246104418,0.115538884531684,339.91879682684));
#35735=CARTESIAN_POINT('Ctrl Pts',(97.5445667989196,0.252556743763496,339.91367425961));
#35736=CARTESIAN_POINT('Ctrl Pts',(97.5368089873974,0.389227340773018,339.902824200366));
#35737=CARTESIAN_POINT('Ctrl Pts',(97.5290570138744,0.525795088824123,339.891982306136));
#35738=CARTESIAN_POINT('Ctrl Pts',(97.5213050403514,0.662015706729819,339.875421529783));
#35739=CARTESIAN_POINT('Ctrl Pts',(97.5135530668284,0.797375340014243,339.853182010768));
#35740=CARTESIAN_POINT('Ctrl Pts',(97.5058043762707,0.932677648413699,339.830951910201));
#35741=CARTESIAN_POINT('Ctrl Pts',(97.4980556857131,1.06711931250994,339.803047913489));
#35742=CARTESIAN_POINT('Ctrl Pts',(97.4903069951555,1.20019264041815,339.769561896903));
#35743=CARTESIAN_POINT('Ctrl Pts',(97.4825599167777,1.33323828130903,339.736082847361));
#35744=CARTESIAN_POINT('Ctrl Pts',(97.4748128383998,1.46491577346851,339.697024183348));
#35745=CARTESIAN_POINT('Ctrl Pts',(97.467065760022,1.59472903481945,339.652528599375));
#35746=CARTESIAN_POINT('Ctrl Pts',(97.4593186167162,1.72454338413047,339.608032642486));
#35747=CARTESIAN_POINT('Ctrl Pts',(97.4515714734104,1.85249310171334,339.558099801491));
#35748=CARTESIAN_POINT('Ctrl Pts',(97.4438243301046,1.97809902987863,339.502922083547));
#35749=CARTESIAN_POINT('Ctrl Pts',(97.4360754450765,2.10373319692309,339.44773196048));
#35750=CARTESIAN_POINT('Ctrl Pts',(97.4283265600483,2.22702216821446,339.387294771246));
#35751=CARTESIAN_POINT('Ctrl Pts',(97.4205776750202,2.34750882989827,339.32184976093));
#35752=CARTESIAN_POINT('Ctrl Pts',(97.4128205652455,2.46812337736981,339.256335286604));
#35753=CARTESIAN_POINT('Ctrl Pts',(97.4050634554708,2.58592932957166,339.185802560141));
#35754=CARTESIAN_POINT('Ctrl Pts',(97.3973063456961,2.70049568808664,339.110535987086));
#35755=CARTESIAN_POINT('Ctrl Pts',(97.3895450907699,2.81512326720042,339.03522919398));
#35756=CARTESIAN_POINT('Ctrl Pts',(97.3817838358437,2.92650748593328,338.955183741783));
#35757=CARTESIAN_POINT('Ctrl Pts',(97.3740225809175,3.03424902670012,338.870725501307));
#35758=CARTESIAN_POINT('Ctrl Pts',(97.3662489105129,3.14216291881931,338.786132155171));
#35759=CARTESIAN_POINT('Ctrl Pts',(97.3584752401082,3.24642219128993,338.69711216868));
#35760=CARTESIAN_POINT('Ctrl Pts',(97.3507015697036,3.34666245680582,338.604030169506));
#35761=CARTESIAN_POINT('Ctrl Pts',(97.3432897655266,3.44223651384464,338.515281159788));
#35762=CARTESIAN_POINT('Ctrl Pts',(97.3358779613495,3.53415711009659,338.422840004288));
#35763=CARTESIAN_POINT('Ctrl Pts',(97.3284661571725,3.6221427691649,338.327050468852));
#35764=CARTESIAN_POINT('Ctrl Pts',(97.3206910783941,3.71444086748068,338.226566002941));
#35765=CARTESIAN_POINT('Ctrl Pts',(97.3129159996156,3.80270022858172,338.122079080211));
#35766=CARTESIAN_POINT('Ctrl Pts',(97.3051409208372,3.88655379957592,338.013948013072));
#35767=CARTESIAN_POINT('Ctrl Pts',(97.2973754097882,3.97030418341263,337.905950008095));
#35768=CARTESIAN_POINT('Ctrl Pts',(97.2896098987392,4.04965932734085,337.79431708721));
#35769=CARTESIAN_POINT('Ctrl Pts',(97.2818443876902,4.12428961657313,337.679443640222));
#35770=CARTESIAN_POINT('Ctrl Pts',(97.274086576168,4.19884590965631,337.564684090591));
#35771=CARTESIAN_POINT('Ctrl Pts',(97.2663287646458,4.26868645930068,337.446690734555));
#35772=CARTESIAN_POINT('Ctrl Pts',(97.2585709531237,4.33352271520574,337.325889924157));
#35773=CARTESIAN_POINT('Ctrl Pts',(97.2508189796007,4.39831017977215,337.2051800202));
#35774=CARTESIAN_POINT('Ctrl Pts',(97.2430670060776,4.45810066231457,337.081667210123));
#35775=CARTESIAN_POINT('Ctrl Pts',(97.2353150325546,4.51264984081943,336.95580532688));
#35776=CARTESIAN_POINT('Ctrl Pts',(97.227566341997,4.56717591771481,336.82999674622));
#35777=CARTESIAN_POINT('Ctrl Pts',(97.2198176514394,4.61646495027763,336.701841428943));
#35778=CARTESIAN_POINT('Ctrl Pts',(97.2120689608818,4.66031945801409,336.571816023508));
#35779=CARTESIAN_POINT('Ctrl Pts',(97.204321882504,4.70416484145393,336.441817670944));
#35780=CARTESIAN_POINT('Ctrl Pts',(97.1965748041262,4.74257782426578,336.309950374288));
#35781=CARTESIAN_POINT('Ctrl Pts',(97.1888277257484,4.77540994283155,336.17670851973));
#35782=CARTESIAN_POINT('Ctrl Pts',(97.1810805824425,4.80824233656211,336.043465548477));
#35783=CARTESIAN_POINT('Ctrl Pts',(97.1733334391367,4.83549367923626,335.908848375866));
#35784=CARTESIAN_POINT('Ctrl Pts',(97.1655862958309,4.85706613404898,335.77336384191));
#35785=CARTESIAN_POINT('Ctrl Pts',(97.1578374108028,4.87864343880753,335.637848848155));
#35786=CARTESIAN_POINT('Ctrl Pts',(97.1500885257747,4.89453925369501,335.501466490962));
#35787=CARTESIAN_POINT('Ctrl Pts',(97.1423396407467,4.90470739447279,335.364730636366));
#35788=CARTESIAN_POINT('Ctrl Pts',(97.1345825309719,4.91488632782025,335.227849648921));
#35789=CARTESIAN_POINT('Ctrl Pts',(97.1268254211972,4.91932541382876,335.090614804979));
#35790=CARTESIAN_POINT('Ctrl Pts',(97.1190683114225,4.91803057721332,334.953542448463));
#35791=CARTESIAN_POINT('Ctrl Pts',(97.1113070564963,4.91673504867859,334.816396844861));
#35792=CARTESIAN_POINT('Ctrl Pts',(97.1035458015702,4.90969951221332,334.67941429186));
#35793=CARTESIAN_POINT('Ctrl Pts',(97.095784546644,4.89698190587674,334.54310693153));
#35794=CARTESIAN_POINT('Ctrl Pts',(97.0880108762394,4.88424395551469,334.406581523846));
#35795=CARTESIAN_POINT('Ctrl Pts',(97.0802372058347,4.86580582444609,334.270733854695));
#35796=CARTESIAN_POINT('Ctrl Pts',(97.0724635354301,4.84177694497911,334.136067666094));
#35797=CARTESIAN_POINT('Ctrl Pts',(97.0650517312529,4.8188666156321,334.007670220969));
#35798=CARTESIAN_POINT('Ctrl Pts',(97.0576399270758,4.79087438486096,333.880347017025));
#35799=CARTESIAN_POINT('Ctrl Pts',(97.0502281228986,4.75793700966978,333.754520785194));
#35800=CARTESIAN_POINT('Ctrl Pts',(97.0424530441202,4.72338527560537,333.622527434924));
#35801=CARTESIAN_POINT('Ctrl Pts',(97.0346779653417,4.68328219776451,333.491764385896));
#35802=CARTESIAN_POINT('Ctrl Pts',(97.0269028865633,4.6377304553138,333.362734204121));
#35803=CARTESIAN_POINT('Ctrl Pts',(97.0191373755143,4.59223476718217,333.233862802199));
#35804=CARTESIAN_POINT('Ctrl Pts',(97.0113718644653,4.54130388420285,333.106720389716));
#35805=CARTESIAN_POINT('Ctrl Pts',(97.0036063534162,4.48509108370171,332.981797573731));
#35806=CARTESIAN_POINT('Ctrl Pts',(96.995848541894,4.42893401835588,332.856998619081));
#35807=CARTESIAN_POINT('Ctrl Pts',(96.9880907303718,4.36750561684908,332.734415235493));
#35808=CARTESIAN_POINT('Ctrl Pts',(96.9803329188496,4.30100825658723,332.614520794627));
#35809=CARTESIAN_POINT('Ctrl Pts',(96.9725809453266,4.23456093769777,332.494716578129));
#35810=CARTESIAN_POINT('Ctrl Pts',(96.9648289718036,4.16305244155381,332.377597617088));
#35811=CARTESIAN_POINT('Ctrl Pts',(96.9570769982806,4.08673218930972,332.263614962152));
#35812=CARTESIAN_POINT('Ctrl Pts',(96.949328307723,4.01044425873778,332.149680578937));
#35813=CARTESIAN_POINT('Ctrl Pts',(96.9415796171654,3.92934884208925,332.038880184191));
#35814=CARTESIAN_POINT('Ctrl Pts',(96.9338309266078,3.84373989519572,331.931637785303));
#35815=CARTESIAN_POINT('Ctrl Pts',(96.9260838482299,3.75814875995866,331.824417699092));
#35816=CARTESIAN_POINT('Ctrl Pts',(96.9183367698521,3.66804620607121,331.720754441576));
#35817=CARTESIAN_POINT('Ctrl Pts',(96.9105896914743,3.57376763124534,331.621040399714));
#35818=CARTESIAN_POINT('Ctrl Pts',(96.9028425481685,3.47948826627414,331.521325522153));
#35819=CARTESIAN_POINT('Ctrl Pts',(96.8950954048626,3.38103307909655,331.425560210284));
#35820=CARTESIAN_POINT('Ctrl Pts',(96.8873482615568,3.27877533718385,331.33410101738));
#35821=CARTESIAN_POINT('Ctrl Pts',(96.8795993765287,3.17649460555992,331.242621262507));
#35822=CARTESIAN_POINT('Ctrl Pts',(96.8718504915006,3.07040990934296,331.155449813551));
#35823=CARTESIAN_POINT('Ctrl Pts',(96.8641016064725,2.96092837650429,331.072903590219));
#35824=CARTESIAN_POINT('Ctrl Pts',(96.8563444966978,2.85133063883543,330.990269751474));
#35825=CARTESIAN_POINT('Ctrl Pts',(96.8485873869231,2.73832917494129,330.912271180755));
#35826=CARTESIAN_POINT('Ctrl Pts',(96.8408302771484,2.62236139564555,330.839182319168));
#35827=CARTESIAN_POINT('Ctrl Pts',(96.8330690222222,2.50633164687649,330.76605440123));
#35828=CARTESIAN_POINT('Ctrl Pts',(96.825307767296,2.38733276318271,330.697841614454));
#35829=CARTESIAN_POINT('Ctrl Pts',(96.8175465123698,2.26582676936601,330.634772386951));
#35830=CARTESIAN_POINT('Ctrl Pts',(96.8097728419652,2.14412640555791,330.571602269239));
#35831=CARTESIAN_POINT('Ctrl Pts',(96.8019991715605,2.01991127168514,330.5135923183));
#35832=CARTESIAN_POINT('Ctrl Pts',(96.7942255011559,1.8936641952562,330.46092311388));
#35833=CARTESIAN_POINT('Ctrl Pts',(96.7868136969788,1.77329395060893,330.410705673599));
#35834=CARTESIAN_POINT('Ctrl Pts',(96.7794018928018,1.65107694982862,330.365343046185));
#35835=CARTESIAN_POINT('Ctrl Pts',(96.7719900886247,1.52744268343612,330.32494899372));
#35836=CARTESIAN_POINT('Ctrl Pts',(96.7642150098463,1.3977487333596,330.282575108416));
#35837=CARTESIAN_POINT('Ctrl Pts',(96.7564399310679,1.26608521919088,330.245535253123));
#35838=CARTESIAN_POINT('Ctrl Pts',(96.7486648522894,1.13293032499963,330.214015050045));
#35839=CARTESIAN_POINT('Ctrl Pts',(96.7408993412404,0.999939286382824,330.182533634583));
#35840=CARTESIAN_POINT('Ctrl Pts',(96.7331338301914,0.865460896067515,330.156558445819));
#35841=CARTESIAN_POINT('Ctrl Pts',(96.7253683191424,0.729990663153302,330.136226085208));
#35842=CARTESIAN_POINT('Ctrl Pts',(96.7176105076202,0.594654749369434,330.115913884193));
#35843=CARTESIAN_POINT('Ctrl Pts',(96.709852696098,0.458329334092584,330.101233434845));
#35844=CARTESIAN_POINT('Ctrl Pts',(96.7020948845758,0.321522003676771,330.092270722253));
#35845=CARTESIAN_POINT('Ctrl Pts',(96.6943429110528,0.184817625115412,330.083314754387));
#35846=CARTESIAN_POINT('Ctrl Pts',(96.6865909375298,0.0476324417326503,
330.080067984258));
#35847=CARTESIAN_POINT('Ctrl Pts',(96.6788389640067,-0.0895192722610985,
330.082564757682));
#35848=CARTESIAN_POINT('Ctrl Pts',(96.6710902734491,-0.22661290242245,330.08506047372));
#35849=CARTESIAN_POINT('Ctrl Pts',(96.6633415828915,-0.36367270139029,330.093294888352));
#35850=CARTESIAN_POINT('Ctrl Pts',(96.6555928923339,-0.500183035935528,
330.107250262576));
#35851=CARTESIAN_POINT('Ctrl Pts',(96.6478458139561,-0.636664968365415,
330.121202733268));
#35852=CARTESIAN_POINT('Ctrl Pts',(96.6400987355782,-0.77259727516104,330.140873756247));
#35853=CARTESIAN_POINT('Ctrl Pts',(96.6323516572004,-0.907468486810217,
330.166193631521));
#35854=CARTESIAN_POINT('Ctrl Pts',(96.6246045138946,-1.04234082880996,330.191513719));
#35855=CARTESIAN_POINT('Ctrl Pts',(96.6168573705888,-1.17615167376231,330.222482681083));
#35856=CARTESIAN_POINT('Ctrl Pts',(96.609110227283,-1.30839919196864,330.258979580622));
#35857=CARTESIAN_POINT('Ctrl Pts',(96.6013613422549,-1.44067644222476,330.29548468544));
#35858=CARTESIAN_POINT('Ctrl Pts',(96.5936124572268,-1.57138928963526,330.337520096779));
#35859=CARTESIAN_POINT('Ctrl Pts',(96.5858635721987,-1.70005090934896,330.384914955483));
#35860=CARTESIAN_POINT('Ctrl Pts',(96.578106462424,-1.82884909183523,330.43236011958));
#35861=CARTESIAN_POINT('Ctrl Pts',(96.5703493526493,-1.95559133011509,330.485175959176));
#35862=CARTESIAN_POINT('Ctrl Pts',(96.5625922428746,-2.07981013271289,330.543143162007));
#35863=CARTESIAN_POINT('Ctrl Pts',(96.5548309879484,-2.20409531386705,330.601141340658));
#35864=CARTESIAN_POINT('Ctrl Pts',(96.5470697330223,-2.32585402564403,330.664296187712));
#35865=CARTESIAN_POINT('Ctrl Pts',(96.5393084780961,-2.44464414984062,330.732342792216));
#35866=CARTESIAN_POINT('Ctrl Pts',(96.5315348076914,-2.56362429952231,330.800498249111));
#35867=CARTESIAN_POINT('Ctrl Pts',(96.5237611372868,-2.67962604125641,330.873560892135));
#35868=CARTESIAN_POINT('Ctrl Pts',(96.5159874668821,-2.79223623601205,330.951222423397));
#35869=CARTESIAN_POINT('Ctrl Pts',(96.508575662705,-2.89960439910991,331.025268791696));
#35870=CARTESIAN_POINT('Ctrl Pts',(96.5011638585279,-3.00388943220456,331.103495354437));
#35871=CARTESIAN_POINT('Ctrl Pts',(96.4937520543508,-3.10476324837013,331.18560250707));
#35872=CARTESIAN_POINT('Ctrl Pts',(96.4860800008919,-3.20917902781154,331.270592672663));
#35873=CARTESIAN_POINT('Ctrl Pts',(96.478407947433,-3.31028861217652,331.360025256184));
#35874=CARTESIAN_POINT('Ctrl Pts',(96.4707358939742,-3.40768282566073,331.453610170582));
#35875=CARTESIAN_POINT('Ctrl Pts',(96.4630733301437,-3.50495657141171,331.547079329002));
#35876=CARTESIAN_POINT('Ctrl Pts',(96.4554107663131,-3.59852379853239,331.644690328441));
#35877=CARTESIAN_POINT('Ctrl Pts',(96.4477482024826,-3.68800667994101,331.746111589005));
#35878=CARTESIAN_POINT('Ctrl Pts',(96.4400931667297,-3.77740164898974,331.84743320836));
#35879=CARTESIAN_POINT('Ctrl Pts',(96.4324381309767,-3.8627199896584,331.952557343243));
#35880=CARTESIAN_POINT('Ctrl Pts',(96.4247830952237,-3.94361955953311,332.06111452551));
#35881=CARTESIAN_POINT('Ctrl Pts',(96.4171337060828,-4.02445945516137,332.169591632344));
#35882=CARTESIAN_POINT('Ctrl Pts',(96.409484316942,-4.10088682606692,332.281496426618));
#35883=CARTESIAN_POINT('Ctrl Pts',(96.4018349278011,-4.17259913516054,332.396425626229));
#35884=CARTESIAN_POINT('Ctrl Pts',(96.394188539377,-4.24428331281478,332.511309741197));
#35885=CARTESIAN_POINT('Ctrl Pts',(96.3865421509528,-4.3112558936099,332.629215562045));
#35886=CARTESIAN_POINT('Ctrl Pts',(96.3788957625287,-4.37325731383819,332.749710345431));
#35887=CARTESIAN_POINT('Ctrl Pts',(96.3712506150443,-4.43524867179663,332.870185573603));
#35888=CARTESIAN_POINT('Ctrl Pts',(96.3636054675598,-4.49227028999564,332.993248571103));
#35889=CARTESIAN_POINT('Ctrl Pts',(96.3559603200754,-4.5441085445541,333.118441975965));
#35890=CARTESIAN_POINT('Ctrl Pts',(96.3483146550027,-4.59595030864192,333.243643856612));
#35891=CARTESIAN_POINT('Ctrl Pts',(96.3406689899301,-4.64260785844706,333.370976059466));
#35892=CARTESIAN_POINT('Ctrl Pts',(96.3330233248575,-4.68391591590268,333.499961748737));
#35893=CARTESIAN_POINT('Ctrl Pts',(96.3253714154608,-4.72525771023993,333.629052782465));
#35894=CARTESIAN_POINT('Ctrl Pts',(96.317719506064,-4.76124116337068,333.759799616223));
#35895=CARTESIAN_POINT('Ctrl Pts',(96.3100675966673,-4.79175099174716,333.891710554237));
#35896=CARTESIAN_POINT('Ctrl Pts',(96.3024124480701,-4.82227373552095,334.023677332688));
#35897=CARTESIAN_POINT('Ctrl Pts',(96.294757299473,-4.84731816497479,334.15680880187));
#35898=CARTESIAN_POINT('Ctrl Pts',(96.2871021508758,-4.86682048194327,334.29060486396));
#35899=CARTESIAN_POINT('Ctrl Pts',(96.279436680303,-4.88634909525836,334.424581332697));
#35900=CARTESIAN_POINT('Ctrl Pts',(96.2717712097301,-4.9003206283876,334.559223784412));
#35901=CARTESIAN_POINT('Ctrl Pts',(96.2641057391573,-4.90872329639167,334.694028331439));
#35902=CARTESIAN_POINT('Ctrl Pts',(96.2582492422806,-4.91514301954547,334.797020365799));
#35903=CARTESIAN_POINT('Ctrl Pts',(96.252392745404,-4.91831320390242,334.900106934656));
#35904=CARTESIAN_POINT('Ctrl Pts',(96.2465362485274,-4.91824904506439,335.003064836579));
#35905=CARTESIAN_POINT('',(99.7465362485345,-4.91824825774415,334.995860229884));
#35906=CARTESIAN_POINT('Ctrl Pts',(99.7465362484899,-4.91824825774482,334.995860230674));
#35907=CARTESIAN_POINT('Ctrl Pts',(99.738529339443,-4.91836754104053,335.137574614991));
#35908=CARTESIAN_POINT('Ctrl Pts',(99.7305224303961,-4.91235682468743,335.279387806484));
#35909=CARTESIAN_POINT('Ctrl Pts',(99.7225155213492,-4.90022160490974,335.420727091207));
#35910=CARTESIAN_POINT('Ctrl Pts',(99.7148038386915,-4.88853382834601,335.556854990807));
#35911=CARTESIAN_POINT('Ctrl Pts',(99.7070921560339,-4.87116521328685,335.692542885174));
#35912=CARTESIAN_POINT('Ctrl Pts',(99.6993804733762,-4.84817370561067,335.82728156194));
#35913=CARTESIAN_POINT('Ctrl Pts',(99.6916692052917,-4.82518343393723,335.962012995275));
#35914=CARTESIAN_POINT('Ctrl Pts',(99.6839579372071,-4.79657093696615,336.095794923497));
#35915=CARTESIAN_POINT('Ctrl Pts',(99.6762466691226,-4.76244560785376,336.22812657928));
#35916=CARTESIAN_POINT('Ctrl Pts',(99.6685341094029,-4.72831456275896,336.360480400576));
#35917=CARTESIAN_POINT('Ctrl Pts',(99.6608215496833,-4.68866894691457,336.49138308404));
#35918=CARTESIAN_POINT('Ctrl Pts',(99.6531089899637,-4.64366840174913,336.620347751903));
#35919=CARTESIAN_POINT('Ctrl Pts',(99.6453934318526,-4.59865036184059,336.749362557019));
#35920=CARTESIAN_POINT('Ctrl Pts',(99.6376778737415,-4.54827338055376,336.876437475271));
#35921=CARTESIAN_POINT('Ctrl Pts',(99.6299623156304,-4.49274555821127,337.001104797774));
#35922=CARTESIAN_POINT('Ctrl Pts',(99.6222378048506,-4.43715330473034,337.125916776724));
#35923=CARTESIAN_POINT('Ctrl Pts',(99.6145132940709,-4.37639844029515,337.248315222935));
#35924=CARTESIAN_POINT('Ctrl Pts',(99.6067887832912,-4.31073559827855,337.367855921342));
#35925=CARTESIAN_POINT('Ctrl Pts',(99.5990589508225,-4.24502751880551,337.487478975568));
#35926=CARTESIAN_POINT('Ctrl Pts',(99.5913291183538,-4.17440493187114,337.604240024921));
#35927=CARTESIAN_POINT('Ctrl Pts',(99.5835992858851,-4.09916563858818,337.717724071704));
#35928=CARTESIAN_POINT('Ctrl Pts',(99.5758583020993,-4.0238178025622,337.831371834402));
#35929=CARTESIAN_POINT('Ctrl Pts',(99.5681173183136,-3.9438401978577,337.94173284126));
#35930=CARTESIAN_POINT('Ctrl Pts',(99.5603763345278,-3.85957089418946,338.048425097526));
#35931=CARTESIAN_POINT('Ctrl Pts',(99.5583743668066,-3.83777722680782,338.076017772961));
#35932=CARTESIAN_POINT('Ctrl Pts',(99.5563723990853,-3.81569670409654,338.10336526122));
#35933=CARTESIAN_POINT('Ctrl Pts',(99.5543704313641,-3.79333556177948,338.130461368271));
#35934=CARTESIAN_POINT('Ctrl Pts',(99.5465953525857,-3.70649118299784,338.235695016484));
#35935=CARTESIAN_POINT('Ctrl Pts',(99.5388202738073,-3.61512721192145,338.337478397409));
#35936=CARTESIAN_POINT('Ctrl Pts',(99.5310451950288,-3.51954810874501,338.435398691961));
#35937=CARTESIAN_POINT('Ctrl Pts',(99.5232796839798,-3.42408662173995,338.533198489357));
#35938=CARTESIAN_POINT('Ctrl Pts',(99.5155141729308,-3.32442059367024,338.627144381986));
#35939=CARTESIAN_POINT('Ctrl Pts',(99.5077486618818,-3.22089536556936,338.716855674701));
#35940=CARTESIAN_POINT('Ctrl Pts',(99.4999908503596,-3.11747278303341,338.806478018407));
#35941=CARTESIAN_POINT('Ctrl Pts',(99.4922330388374,-3.01019890872618,338.891873863356));
#35942=CARTESIAN_POINT('Ctrl Pts',(99.4844752273152,-2.89945638686753,338.972698795926));
#35943=CARTESIAN_POINT('Ctrl Pts',(99.4767232537922,-2.78879720226804,339.053462905171));
#35944=CARTESIAN_POINT('Ctrl Pts',(99.4689712802691,-2.67467488018255,339.1296627192));
#35945=CARTESIAN_POINT('Ctrl Pts',(99.4612193067461,-2.55750536408549,339.200993855646));
#35946=CARTESIAN_POINT('Ctrl Pts',(99.4534706161884,-2.44038546934846,339.272294783313));
#35947=CARTESIAN_POINT('Ctrl Pts',(99.4457219256308,-2.32022128046657,339.338730931514));
#35948=CARTESIAN_POINT('Ctrl Pts',(99.4379732350732,-2.19745777822956,339.40004117883));
#35949=CARTESIAN_POINT('Ctrl Pts',(99.4302261566953,-2.07471981796444,339.461338670037));
#35950=CARTESIAN_POINT('Ctrl Pts',(99.4224790783175,-1.94938396952175,339.517512207143));
#35951=CARTESIAN_POINT('Ctrl Pts',(99.4147319999397,-1.82191952043152,339.568346782324));
#35952=CARTESIAN_POINT('Ctrl Pts',(99.4069848566339,-1.69445400306669,339.619181783548));
#35953=CARTESIAN_POINT('Ctrl Pts',(99.399237713328,-1.56486021253767,339.664677588801));
#35954=CARTESIAN_POINT('Ctrl Pts',(99.3914905700222,-1.43362673064403,339.704667624783));
#35955=CARTESIAN_POINT('Ctrl Pts',(99.3837416849941,-1.30236374467723,339.744666651374));
#35956=CARTESIAN_POINT('Ctrl Pts',(99.375992799966,-1.16946070762542,339.779157331668));
#35957=CARTESIAN_POINT('Ctrl Pts',(99.3682439149379,-1.03542026026359,339.808023288955));
#35958=CARTESIAN_POINT('Ctrl Pts',(99.3604868051631,-0.901237540986117,
339.836919884867));
#35959=CARTESIAN_POINT('Ctrl Pts',(99.3527296953884,-0.76591538250305,339.86017974944));
#35960=CARTESIAN_POINT('Ctrl Pts',(99.3449725856137,-0.629966042326224,
339.877737779752));
#35961=CARTESIAN_POINT('Ctrl Pts',(99.3372113306875,-0.49394405516901,339.895305192513));
#35962=CARTESIAN_POINT('Ctrl Pts',(99.3294500757614,-0.357294607722734,
339.907164666055));
#35963=CARTESIAN_POINT('Ctrl Pts',(99.3216888208352,-0.220532944755472,
339.913303194672));
#35964=CARTESIAN_POINT('Ctrl Pts',(99.3139151504305,-0.0835525076979857,
339.919451542934));
#35965=CARTESIAN_POINT('Ctrl Pts',(99.3061414800259,0.05354011251302,339.919860657402));
#35966=CARTESIAN_POINT('Ctrl Pts',(99.2983678096212,0.190230913560278,339.914569692458));
#35967=CARTESIAN_POINT('Ctrl Pts',(99.2909560054441,0.320558724932695,339.909525023205));
#35968=CARTESIAN_POINT('Ctrl Pts',(99.2835442012671,0.450520997721607,339.899299031945));
#35969=CARTESIAN_POINT('Ctrl Pts',(99.27613239709,0.579680216019076,339.883969073372));
#35970=CARTESIAN_POINT('Ctrl Pts',(99.2683573183115,0.715169912351052,339.867887747865));
#35971=CARTESIAN_POINT('Ctrl Pts',(99.2605822395331,0.850204016037191,339.846138663169));
#35972=CARTESIAN_POINT('Ctrl Pts',(99.2528071607547,0.984270617820415,339.818754446265));
#35973=CARTESIAN_POINT('Ctrl Pts',(99.2450416497056,1.11817224211523,339.791403927382));
#35974=CARTESIAN_POINT('Ctrl Pts',(99.2372761386566,1.25110835409944,339.758432151213));
#35975=CARTESIAN_POINT('Ctrl Pts',(99.2295106276076,1.38257193525139,339.719923506409));
#35976=CARTESIAN_POINT('Ctrl Pts',(99.2217528160854,1.51390516987935,339.681453043039));
#35977=CARTESIAN_POINT('Ctrl Pts',(99.2139950045632,1.64376840649856,339.637456745261));
#35978=CARTESIAN_POINT('Ctrl Pts',(99.206237193041,1.77166494960274,339.588070004789));
#35979=CARTESIAN_POINT('Ctrl Pts',(99.198485219518,1.89946524650248,339.538720429406));
#35980=CARTESIAN_POINT('Ctrl Pts',(99.1907332459951,2.02530143258804,339.483988625787));
#35981=CARTESIAN_POINT('Ctrl Pts',(99.1829812724721,2.14869245535333,339.42405965091));
#35982=CARTESIAN_POINT('Ctrl Pts',(99.1752325819145,2.27203122194747,339.364156055989));
#35983=CARTESIAN_POINT('Ctrl Pts',(99.1674838913568,2.39292653394667,339.299059837865));
#35984=CARTESIAN_POINT('Ctrl Pts',(99.1597352007992,2.51091800413993,339.229003882593));
#35985=CARTESIAN_POINT('Ctrl Pts',(99.1519881224214,2.62888492522242,339.158962503048));
#35986=CARTESIAN_POINT('Ctrl Pts',(99.1442410440435,2.74394887034699,339.083963638334));
#35987=CARTESIAN_POINT('Ctrl Pts',(99.1364939656657,2.85567507643598,339.004285569277));
#35988=CARTESIAN_POINT('Ctrl Pts',(99.1287468223599,2.96740221889789,338.924606832441));
#35989=CARTESIAN_POINT('Ctrl Pts',(99.1209996790541,3.07579124829143,338.840249039995));
#35990=CARTESIAN_POINT('Ctrl Pts',(99.1132525357483,3.18043768992683,338.751532908425));
#35991=CARTESIAN_POINT('Ctrl Pts',(99.1055036507201,3.28510765830452,338.662796831584));
#35992=CARTESIAN_POINT('Ctrl Pts',(99.097754765692,3.38603306651375,338.569700718547));
#35993=CARTESIAN_POINT('Ctrl Pts',(99.0900058806639,3.48284404313138,338.472604272549));
#35994=CARTESIAN_POINT('Ctrl Pts',(99.0822487708892,3.57975777591951,338.37540476738));
#35995=CARTESIAN_POINT('Ctrl Pts',(99.0744916611144,3.67254807700514,338.274196724711));
#35996=CARTESIAN_POINT('Ctrl Pts',(99.0667345513397,3.76088298801926,338.169375681886));
#35997=CARTESIAN_POINT('Ctrl Pts',(99.0589732964135,3.84926510238537,338.064498626046));
#35998=CARTESIAN_POINT('Ctrl Pts',(99.0512120414874,3.93318684365483,337.956005032031));
#35999=CARTESIAN_POINT('Ctrl Pts',(99.0434507865612,4.01235844654264,337.844321142023));
#36000=CARTESIAN_POINT('Ctrl Pts',(99.0356771161565,4.09165669819311,337.732458594188));
#36001=CARTESIAN_POINT('Ctrl Pts',(99.0279034457519,4.16618941444608,337.617395880424));
#36002=CARTESIAN_POINT('Ctrl Pts',(99.0201297753472,4.23571136490989,337.499586424926));
#36003=CARTESIAN_POINT('Ctrl Pts',(99.0127179711702,4.30199705185293,337.387261027926));
#36004=CARTESIAN_POINT('Ctrl Pts',(99.0053061669932,4.36372784067942,337.272439109477));
#36005=CARTESIAN_POINT('Ctrl Pts',(98.9978943628162,4.4207320156403,337.155530447104));
#36006=CARTESIAN_POINT('Ctrl Pts',(98.9901192840378,4.48053013502324,337.032891742934));
#36007=CARTESIAN_POINT('Ctrl Pts',(98.9823442052593,4.53531556746633,336.907569006628));
#36008=CARTESIAN_POINT('Ctrl Pts',(98.9745691264809,4.58483872621954,336.78001036993));
#36009=CARTESIAN_POINT('Ctrl Pts',(98.9668036154319,4.63430094357308,336.652608702255));
#36010=CARTESIAN_POINT('Ctrl Pts',(98.9590381043829,4.67851363163728,336.522976969615));
#36011=CARTESIAN_POINT('Ctrl Pts',(98.9512725933339,4.71727337781604,336.391587202244));
#36012=CARTESIAN_POINT('Ctrl Pts',(98.9435147818117,4.75599469359367,336.260327708209));
#36013=CARTESIAN_POINT('Ctrl Pts',(98.9357569702895,4.78927371705804,336.12731402079));
#36014=CARTESIAN_POINT('Ctrl Pts',(98.9279991587673,4.81695551155129,335.99303709006));
#36015=CARTESIAN_POINT('Ctrl Pts',(98.9202471852443,4.84461647461643,335.858861206979));
#36016=CARTESIAN_POINT('Ctrl Pts',(98.9124952117212,4.86668851407112,335.723424354053));
#36017=CARTESIAN_POINT('Ctrl Pts',(98.9047432381982,4.88306692316215,335.587231203547));
#36018=CARTESIAN_POINT('Ctrl Pts',(98.8969945476405,4.89943839598715,335.451095730922));
#36019=CARTESIAN_POINT('Ctrl Pts',(98.889245857083,4.91012098769387,335.314204985027));
#36020=CARTESIAN_POINT('Ctrl Pts',(98.8814971665253,4.91506139519829,335.177072143296));
#36021=CARTESIAN_POINT('Ctrl Pts',(98.8737500881475,4.92000077480966,335.039967833199));
#36022=CARTESIAN_POINT('Ctrl Pts',(98.8660030097696,4.91920033251634,334.902621917832));
#36023=CARTESIAN_POINT('Ctrl Pts',(98.8582559313918,4.91265880535237,334.765550592464));
#36024=CARTESIAN_POINT('Ctrl Pts',(98.850508788086,4.9061172233641,334.628478118307));
#36025=CARTESIAN_POINT('Ctrl Pts',(98.8427616447802,4.89383447916726,334.49168062917));
#36026=CARTESIAN_POINT('Ctrl Pts',(98.8350145014744,4.87586138563468,334.355671814541));
#36027=CARTESIAN_POINT('Ctrl Pts',(98.8272656164463,4.85788425136914,334.219632422244));
#36028=CARTESIAN_POINT('Ctrl Pts',(98.8195167314183,4.83421427327873,334.084382444714));
#36029=CARTESIAN_POINT('Ctrl Pts',(98.8117678463902,4.80495377483786,333.950427570784));
#36030=CARTESIAN_POINT('Ctrl Pts',(98.8040107366155,4.77566221900155,333.816330515765));
#36031=CARTESIAN_POINT('Ctrl Pts',(98.7962536268407,4.74076837296629,333.683531692784));
#36032=CARTESIAN_POINT('Ctrl Pts',(98.788496517066,4.70042521080144,333.552524300666));
#36033=CARTESIAN_POINT('Ctrl Pts',(98.7807352621398,4.66006049054065,333.421446902387));
#36034=CARTESIAN_POINT('Ctrl Pts',(98.7729740072136,4.61424078235331,333.292163210679));
#36035=CARTESIAN_POINT('Ctrl Pts',(98.7652127522875,4.56316771376261,333.165147559455));
#36036=CARTESIAN_POINT('Ctrl Pts',(98.7574390818828,4.51201294490686,333.037928724583));
#36037=CARTESIAN_POINT('Ctrl Pts',(98.7496654114782,4.4555881835977,332.912985536685));
#36038=CARTESIAN_POINT('Ctrl Pts',(98.7418917410735,4.39414201567991,332.790769589079));
#36039=CARTESIAN_POINT('Ctrl Pts',(98.7344799368964,4.3355561816615,332.674242823238));
#36040=CARTESIAN_POINT('Ctrl Pts',(98.7270681327193,4.27240605276472,332.56019535739));
#36041=CARTESIAN_POINT('Ctrl Pts',(98.7196563285422,4.2049432944078,332.448993345106));
#36042=CARTESIAN_POINT('Ctrl Pts',(98.7118812497637,4.13417398530278,332.332340990946));
#36043=CARTESIAN_POINT('Ctrl Pts',(98.7041061709853,4.05843496378142,332.218451428376));
#36044=CARTESIAN_POINT('Ctrl Pts',(98.6963310922068,3.97796800767736,332.107777050019));
#36045=CARTESIAN_POINT('Ctrl Pts',(98.6885655811578,3.89760007128557,331.997238863531));
#36046=CARTESIAN_POINT('Ctrl Pts',(98.6808000701088,3.81251600417157,331.889908302103));
#36047=CARTESIAN_POINT('Ctrl Pts',(98.6730345590598,3.72300266840189,331.78621186237));
#36048=CARTESIAN_POINT('Ctrl Pts',(98.6652767475376,3.6335780853656,331.682618237959));
#36049=CARTESIAN_POINT('Ctrl Pts',(98.6575189360155,3.53973322703933,331.582651858565));
#36050=CARTESIAN_POINT('Ctrl Pts',(98.6497611244933,3.44179709869773,331.486708694985));
#36051=CARTESIAN_POINT('Ctrl Pts',(98.6420091509703,3.34393467039838,331.390837731677));
#36052=CARTESIAN_POINT('Ctrl Pts',(98.6342571774473,3.2419873783973,331.298984230331));
#36053=CARTESIAN_POINT('Ctrl Pts',(98.6265052039243,3.13632294953612,331.211509348208));
#36054=CARTESIAN_POINT('Ctrl Pts',(98.6187565133667,3.03070326962321,331.12407151175));
#36055=CARTESIAN_POINT('Ctrl Pts',(98.6110078228091,2.92136988430319,331.041008855088));
#36056=CARTESIAN_POINT('Ctrl Pts',(98.6032591322515,2.80872549007244,330.962643911677));
#36057=CARTESIAN_POINT('Ctrl Pts',(98.5955120538736,2.69610453244866,330.884295272748));
#36058=CARTESIAN_POINT('Ctrl Pts',(98.5877649754958,2.58017425681572,330.810642626037));
#36059=CARTESIAN_POINT('Ctrl Pts',(98.580017897118,2.46136805932454,330.741966376479));
#36060=CARTESIAN_POINT('Ctrl Pts',(98.5722707538122,2.34256086612308,330.673289551348));
#36061=CARTESIAN_POINT('Ctrl Pts',(98.5645236105064,2.22087804139224,330.609589402173));
#36062=CARTESIAN_POINT('Ctrl Pts',(98.5567764672006,2.09677905534404,330.551101186184));
#36063=CARTESIAN_POINT('Ctrl Pts',(98.5490275821725,1.97265216920925,330.492599820803));
#36064=CARTESIAN_POINT('Ctrl Pts',(98.5412786971444,1.84610839434497,330.439312886872));
#36065=CARTESIAN_POINT('Ctrl Pts',(98.5335298121163,1.71762834838097,330.391427995644));
#36066=CARTESIAN_POINT('Ctrl Pts',(98.5257727023416,1.58901193236857,330.343492278896));
#36067=CARTESIAN_POINT('Ctrl Pts',(98.5180155925669,1.45845550668665,330.300970195345));
#36068=CARTESIAN_POINT('Ctrl Pts',(98.5102584827922,1.32645659579741,330.264000004015));
#36069=CARTESIAN_POINT('Ctrl Pts',(98.502497227866,1.19438714891078,330.227010056998));
#36070=CARTESIAN_POINT('Ctrl Pts',(98.4947359729398,1.06087406117239,330.195578003253));
#36071=CARTESIAN_POINT('Ctrl Pts',(98.4869747180137,0.926425322311606,330.169790979194));
#36072=CARTESIAN_POINT('Ctrl Pts',(98.479201047609,0.791761509285206,330.143962704299));
#36073=CARTESIAN_POINT('Ctrl Pts',(98.4714273772044,0.656159441039006,330.123797561643));
#36074=CARTESIAN_POINT('Ctrl Pts',(98.4636537067997,0.520133396093588,330.109330893143));
#36075=CARTESIAN_POINT('Ctrl Pts',(98.4562419026226,0.390439396265707,330.095537651541));
#36076=CARTESIAN_POINT('Ctrl Pts',(98.4488300984455,0.260360290838765,330.086924314367));
#36077=CARTESIAN_POINT('Ctrl Pts',(98.4414182942683,0.130340176758547,330.083477397507));
#36078=CARTESIAN_POINT('Ctrl Pts',(98.4336432154899,-0.00605261042199617,
330.079861536984));
#36079=CARTESIAN_POINT('Ctrl Pts',(98.4258681367115,-0.142811503763694,
330.081919918714));
#36080=CARTESIAN_POINT('Ctrl Pts',(98.4180930579331,-0.279425236798542,
330.089694042166));
#36081=CARTESIAN_POINT('Ctrl Pts',(98.410327546884,-0.415870857937821,330.097458599064));
#36082=CARTESIAN_POINT('Ctrl Pts',(98.402562035835,-0.552171287678357,330.110924880874));
#36083=CARTESIAN_POINT('Ctrl Pts',(98.394796524786,-0.68781263837535,330.130082460966));
#36084=CARTESIAN_POINT('Ctrl Pts',(98.3870387132638,-0.823319500277665,
330.149221046262));
#36085=CARTESIAN_POINT('Ctrl Pts',(98.3792809017416,-0.958168199056252,
330.174039645761));
#36086=CARTESIAN_POINT('Ctrl Pts',(98.3715230902194,-1.09184771078839,330.204475874428));
#36087=CARTESIAN_POINT('Ctrl Pts',(98.3637711166964,-1.22542662444972,330.234889198868));
#36088=CARTESIAN_POINT('Ctrl Pts',(98.3560191431733,-1.3578377227775,330.27091165153));
#36089=CARTESIAN_POINT('Ctrl Pts',(98.3482671696503,-1.4885783028302,330.312429445988));
#36090=CARTESIAN_POINT('Ctrl Pts',(98.3405184790927,-1.6192635141691,330.353929657634));
#36091=CARTESIAN_POINT('Ctrl Pts',(98.332769788535,-1.74827924256604,330.400920464221));
#36092=CARTESIAN_POINT('Ctrl Pts',(98.3250210979774,-1.87513634057516,330.453237771034));
#36093=CARTESIAN_POINT('Ctrl Pts',(98.3172740195996,-2.00196704490534,330.505544192794));
#36094=CARTESIAN_POINT('Ctrl Pts',(98.3095269412218,-2.12663965105759,330.563174761514));
#36095=CARTESIAN_POINT('Ctrl Pts',(98.3017798628439,-2.24868382501489,330.625916768325));
#36096=CARTESIAN_POINT('Ctrl Pts',(98.2940327195381,-2.37072902181983,330.688659300975));
#36097=CARTESIAN_POINT('Ctrl Pts',(98.2862855762323,-2.4901453948647,330.756513178448));
#36098=CARTESIAN_POINT('Ctrl Pts',(98.2785384329265,-2.60648646563008,330.829219333627));
#36099=CARTESIAN_POINT('Ctrl Pts',(98.2707895478984,-2.722853692338,330.901941834694));
#36100=CARTESIAN_POINT('Ctrl Pts',(98.2630406628703,-2.8361439095662,330.979518577117));
#36101=CARTESIAN_POINT('Ctrl Pts',(98.2552917778422,-2.94593926123445,331.061646926491));
#36102=CARTESIAN_POINT('Ctrl Pts',(98.2475346680675,-3.05585115082365,331.143862447744));
#36103=CARTESIAN_POINT('Ctrl Pts',(98.2397775582927,-3.16226045131371,331.230638992073));
#36104=CARTESIAN_POINT('Ctrl Pts',(98.232020448518,-3.2647816587051,331.321633000436));
#36105=CARTESIAN_POINT('Ctrl Pts',(98.2242591935918,-3.36735765015165,331.412675633087));
#36106=CARTESIAN_POINT('Ctrl Pts',(98.2164979386657,-3.46604112747362,331.507939949091));
#36107=CARTESIAN_POINT('Ctrl Pts',(98.2087366837395,-3.56048391341217,331.60704592356));
#36108=CARTESIAN_POINT('Ctrl Pts',(98.2009630133348,-3.65507777702939,331.706310435289));
#36109=CARTESIAN_POINT('Ctrl Pts',(98.1931893429302,-3.7454171356662,331.809428591653));
#36110=CARTESIAN_POINT('Ctrl Pts',(98.1854156725255,-3.83119396393381,331.915987050413));
#36111=CARTESIAN_POINT('Ctrl Pts',(98.1780038683485,-3.91297786020839,332.017585187281));
#36112=CARTESIAN_POINT('Ctrl Pts',(98.1705920641714,-3.99061426707868,332.122310311172));
#36113=CARTESIAN_POINT('Ctrl Pts',(98.1631802599944,-4.06387419728365,332.229781674461));
#36114=CARTESIAN_POINT('Ctrl Pts',(98.1552885578527,-4.14187754630421,332.344211571363));
#36115=CARTESIAN_POINT('Ctrl Pts',(98.1473968557111,-4.21516087342881,332.462109660984));
#36116=CARTESIAN_POINT('Ctrl Pts',(98.1395051535695,-4.28340595589162,332.583056376427));
#36117=CARTESIAN_POINT('Ctrl Pts',(98.1316239051704,-4.35156063751223,332.703842879814));
#36118=CARTESIAN_POINT('Ctrl Pts',(98.1237426567713,-4.41469017547625,332.827669647362));
#36119=CARTESIAN_POINT('Ctrl Pts',(98.1158614083722,-4.47251859532413,332.954086884303));
#36120=CARTESIAN_POINT('Ctrl Pts',(98.1079890773332,-4.53028158431405,333.080361084511));
#36121=CARTESIAN_POINT('Ctrl Pts',(98.1001167462942,-4.58275524058733,333.209219580141));
#36122=CARTESIAN_POINT('Ctrl Pts',(98.0922444152552,-4.62970875904289,333.340186796973));
#36123=CARTESIAN_POINT('Ctrl Pts',(98.0842687346914,-4.67727869261043,333.472873377429));
#36124=CARTESIAN_POINT('Ctrl Pts',(98.0762930541276,-4.71918230838665,333.607724111206));
#36125=CARTESIAN_POINT('Ctrl Pts',(98.0683173735638,-4.75522891826669,333.744220959969));
#36126=CARTESIAN_POINT('Ctrl Pts',(98.0604592572084,-4.79074418901906,333.87870579937));
#36127=CARTESIAN_POINT('Ctrl Pts',(98.052601140853,-4.8205738361938,334.014788181689));
#36128=CARTESIAN_POINT('Ctrl Pts',(98.0447430244975,-4.84458495519773,334.151955381851));
#36129=CARTESIAN_POINT('Ctrl Pts',(98.0367085618296,-4.86913491482242,334.292200791707));
#36130=CARTESIAN_POINT('Ctrl Pts',(98.0286740991616,-4.88760196514298,334.433579907344));
#36131=CARTESIAN_POINT('Ctrl Pts',(98.0206396364937,-4.89989898113148,334.57553205397));
#36132=CARTESIAN_POINT('Ctrl Pts',(98.0126051738258,-4.91219599711999,334.717484200597));
#36133=CARTESIAN_POINT('Ctrl Pts',(98.0045707111579,-4.91832292500355,334.860008960813));
#36134=CARTESIAN_POINT('Ctrl Pts',(97.9965362484899,-4.91824934462231,335.002539019938));
#36135=CARTESIAN_POINT('',(101.496536248439,-4.91824996307027,334.999397290091));
#36136=CARTESIAN_POINT('Ctrl Pts',(101.496536248439,-4.91824996307028,334.999397290091));
#36137=CARTESIAN_POINT('Ctrl Pts',(101.488787543807,-4.91826662769589,335.135384425997));
#36138=CARTESIAN_POINT('Ctrl Pts',(101.481038839174,-4.91263905510794,335.271593521368));
#36139=CARTESIAN_POINT('Ctrl Pts',(101.473290134542,-4.90133800926562,335.407515375695));
#36140=CARTESIAN_POINT('Ctrl Pts',(101.465550940153,-4.89005083357312,335.543270408605));
#36141=CARTESIAN_POINT('Ctrl Pts',(101.457811745764,-4.87310406998696,335.678738513187));
#36142=CARTESIAN_POINT('Ctrl Pts',(101.450072551375,-4.85052045818359,335.813409089722));
#36143=CARTESIAN_POINT('Ctrl Pts',(101.442340971951,-4.82795906748272,335.947947157396));
#36144=CARTESIAN_POINT('Ctrl Pts',(101.434609392528,-4.79977192949126,336.081688872592));
#36145=CARTESIAN_POINT('Ctrl Pts',(101.426877813105,-4.76603365967239,336.214127759904));
#36146=CARTESIAN_POINT('Ctrl Pts',(101.419151960248,-4.73232037885692,336.346468553395));
#36147=CARTESIAN_POINT('Ctrl Pts',(101.411426107392,-4.6930642460017,336.47750805938));
#36148=CARTESIAN_POINT('Ctrl Pts',(101.403700254536,-4.64839105527419,336.606749407887));
#36149=CARTESIAN_POINT('Ctrl Pts',(101.395977514058,-4.6037358612468,336.735938691213));
#36150=CARTESIAN_POINT('Ctrl Pts',(101.388254773579,-4.5536680771719,336.863330886013));
#36151=CARTESIAN_POINT('Ctrl Pts',(101.380532033101,-4.49836344221849,336.98844396557));
#36152=CARTESIAN_POINT('Ctrl Pts',(101.37281075426,-4.44306927444177,337.113533365725));
#36153=CARTESIAN_POINT('Ctrl Pts',(101.365089475418,-4.38254038615454,337.236344148507));
#36154=CARTESIAN_POINT('Ctrl Pts',(101.357368196577,-4.31700061305907,337.356414388292));
#36155=CARTESIAN_POINT('Ctrl Pts',(101.349646678094,-4.25145880583766,337.476488354637));
#36156=CARTESIAN_POINT('Ctrl Pts',(101.341925159611,-4.18090599301653,337.593821263021));
#36157=CARTESIAN_POINT('Ctrl Pts',(101.334203641128,-4.10561169630126,337.707976303754));
#36158=CARTESIAN_POINT('Ctrl Pts',(101.326480181903,-4.03029847497236,337.822160036435));
#36159=CARTESIAN_POINT('Ctrl Pts',(101.318756722679,-3.95024161557251,337.933163983724));
#36160=CARTESIAN_POINT('Ctrl Pts',(101.311033263455,-3.86575338025264,338.040581172336));
#36161=CARTESIAN_POINT('Ctrl Pts',(101.303301555462,-3.78117491025085,338.148113084091));
#36162=CARTESIAN_POINT('Ctrl Pts',(101.295569847469,-3.69215585612748,338.252050276794));
#36163=CARTESIAN_POINT('Ctrl Pts',(101.287838139476,-3.59904841592456,338.352019326068));
#36164=CARTESIAN_POINT('Ctrl Pts',(101.280102061374,-3.50588834960681,338.452044879769));
#36165=CARTESIAN_POINT('Ctrl Pts',(101.272365983271,-3.4086355738239,338.54809754579));
#36166=CARTESIAN_POINT('Ctrl Pts',(101.264629905168,-3.30767761363785,338.639842285971));
#36167=CARTESIAN_POINT('Ctrl Pts',(101.256881904041,-3.2065640546801,338.731728425293));
#36168=CARTESIAN_POINT('Ctrl Pts',(101.249133902913,-3.1017342061043,338.819293123715));
#36169=CARTESIAN_POINT('Ctrl Pts',(101.241385901786,-2.99360752957126,338.902242563116));
#36170=CARTESIAN_POINT('Ctrl Pts',(101.235523480193,-2.91179492360666,338.965005148801));
#36171=CARTESIAN_POINT('Ctrl Pts',(101.229661058601,-2.82809554193822,339.025126363737));
#36172=CARTESIAN_POINT('Ctrl Pts',(101.223798637008,-2.74270074531183,339.082496256479));
#36173=CARTESIAN_POINT('Ctrl Pts',(101.21602355823,-2.62944528243802,339.158583489123));
#36174=CARTESIAN_POINT('Ctrl Pts',(101.208248479451,-2.51284226915805,339.230074531481));
#36175=CARTESIAN_POINT('Ctrl Pts',(101.200473400673,-2.39330127820999,339.29666057005));
#36176=CARTESIAN_POINT('Ctrl Pts',(101.192707889624,-2.27390739006172,339.363164670259));
#36177=CARTESIAN_POINT('Ctrl Pts',(101.184942378575,-2.15158305600174,339.424775588041));
#36178=CARTESIAN_POINT('Ctrl Pts',(101.177176867526,-2.02676786706079,339.481226960951));
#36179=CARTESIAN_POINT('Ctrl Pts',(101.169419056004,-1.90207643274323,339.53762236216));
#36180=CARTESIAN_POINT('Ctrl Pts',(101.161661244481,-1.77489941221519,339.588868238999));
#36181=CARTESIAN_POINT('Ctrl Pts',(101.153903432959,-1.64570179978444,339.634743644333));
#36182=CARTESIAN_POINT('Ctrl Pts',(101.146151459436,-1.51660141265351,339.680584526971));
#36183=CARTESIAN_POINT('Ctrl Pts',(101.138399485913,-1.38548382707886,339.721062852148));
#36184=CARTESIAN_POINT('Ctrl Pts',(101.13064751239,-1.25283453341215,339.756005539777));
#36185=CARTESIAN_POINT('Ctrl Pts',(101.122898821833,-1.12024141680033,339.790933429157));
#36186=CARTESIAN_POINT('Ctrl Pts',(101.115150131275,-0.98611825946724,339.820330244366));
#36187=CARTESIAN_POINT('Ctrl Pts',(101.107401440717,-0.850966041638258,
339.844072652064));
#36188=CARTESIAN_POINT('Ctrl Pts',(101.099654362339,-0.715841943357102,
339.867810119956));
#36189=CARTESIAN_POINT('Ctrl Pts',(101.091907283962,-0.579689595186712,
339.885895452785));
#36190=CARTESIAN_POINT('Ctrl Pts',(101.084160205584,-0.443020119450266,
339.898256448601));
#36191=CARTESIAN_POINT('Ctrl Pts',(101.076413062278,-0.306349498291885,
339.910617548014));
#36192=CARTESIAN_POINT('Ctrl Pts',(101.068665918972,-0.169162130208226,
339.917254179514));
#36193=CARTESIAN_POINT('Ctrl Pts',(101.060918775666,-0.031973813343201,
339.918146067144));
#36194=CARTESIAN_POINT('Ctrl Pts',(101.053169890638,0.105245346367392,339.919038155288));
#36195=CARTESIAN_POINT('Ctrl Pts',(101.04542100561,0.242465064494158,339.914182927));
#36196=CARTESIAN_POINT('Ctrl Pts',(101.037672120582,0.37917038748985,339.90361222771));
#36197=CARTESIAN_POINT('Ctrl Pts',(101.029915010807,0.516020810928358,339.893030308571));
#36198=CARTESIAN_POINT('Ctrl Pts',(101.022157901033,0.652355358254423,339.87672083029));
#36199=CARTESIAN_POINT('Ctrl Pts',(101.014400791258,0.787664485461182,339.854767524902));
#36200=CARTESIAN_POINT('Ctrl Pts',(101.006639536332,0.923045917539265,339.83280248837));
#36201=CARTESIAN_POINT('Ctrl Pts',(100.998878281406,1.0574004549784,339.805187693972));
#36202=CARTESIAN_POINT('Ctrl Pts',(100.99111702648,1.1902305522226,339.772057658396));
#36203=CARTESIAN_POINT('Ctrl Pts',(100.983343356075,1.32327313433306,339.73887462556));
#36204=CARTESIAN_POINT('Ctrl Pts',(100.97556968567,1.45478602802753,339.700158831844));
#36205=CARTESIAN_POINT('Ctrl Pts',(100.967796015265,1.58428775809218,339.656094432253));
#36206=CARTESIAN_POINT('Ctrl Pts',(100.960384211088,1.70776115146784,339.614081241064));
#36207=CARTESIAN_POINT('Ctrl Pts',(100.952972406911,1.82940613829515,339.56720629652));
#36208=CARTESIAN_POINT('Ctrl Pts',(100.945560602734,1.94882544889128,339.515668547652));
#36209=CARTESIAN_POINT('Ctrl Pts',(100.937785523955,2.07409785562988,339.46160478019));
#36210=CARTESIAN_POINT('Ctrl Pts',(100.930010445177,2.19731677950854,339.402238723881));
#36211=CARTESIAN_POINT('Ctrl Pts',(100.922235366399,2.31800088935477,339.337747680473));
#36212=CARTESIAN_POINT('Ctrl Pts',(100.91446985535,2.43853648972047,339.2733359974));
#36213=CARTESIAN_POINT('Ctrl Pts',(100.906704344301,2.55654314102322,339.203812058059));
#36214=CARTESIAN_POINT('Ctrl Pts',(100.898938833252,2.67155896547046,339.129401379924));
#36215=CARTESIAN_POINT('Ctrl Pts',(100.891181021729,2.78646075139305,339.055064480192));
#36216=CARTESIAN_POINT('Ctrl Pts',(100.883423210207,2.89837728573366,338.975850694872));
#36217=CARTESIAN_POINT('Ctrl Pts',(100.875665398685,3.0068711342323,338.892031480425));
#36218=CARTESIAN_POINT('Ctrl Pts',(100.867913425162,3.11528333766948,338.808275342595));
#36219=CARTESIAN_POINT('Ctrl Pts',(100.860161451639,3.22027767395822,338.719920912013));
#36220=CARTESIAN_POINT('Ctrl Pts',(100.852409478116,3.3214458696728,338.627282784308));
#36221=CARTESIAN_POINT('Ctrl Pts',(100.844660787558,3.42257122059623,338.534683888904));
#36222=CARTESIAN_POINT('Ctrl Pts',(100.836912097001,3.51987336607719,338.437805168009));
#36223=CARTESIAN_POINT('Ctrl Pts',(100.829163406443,3.61297748333231,338.337001163835));
#36224=CARTESIAN_POINT('Ctrl Pts',(100.821416328065,3.70606222949821,338.236218132776));
#36225=CARTESIAN_POINT('Ctrl Pts',(100.813669249687,3.79495041972273,338.131511729846));
#36226=CARTESIAN_POINT('Ctrl Pts',(100.805922171309,3.87930474022827,338.023272696093));
#36227=CARTESIAN_POINT('Ctrl Pts',(100.798175028004,3.96365976770414,337.915032755193));
#36228=CARTESIAN_POINT('Ctrl Pts',(100.790427884698,4.04348060939842,337.803260432722));
#36229=CARTESIAN_POINT('Ctrl Pts',(100.782680741392,4.11847108685283,337.688378501859));
#36230=CARTESIAN_POINT('Ctrl Pts',(100.774931856364,4.19347842375881,337.573470743098));
#36231=CARTESIAN_POINT('Ctrl Pts',(100.767182971336,4.2636530218539,337.455452312051));
#36232=CARTESIAN_POINT('Ctrl Pts',(100.759434086308,4.32874298972811,337.33477347753));
#36233=CARTESIAN_POINT('Ctrl Pts',(100.751676976533,4.39390204476664,337.213966553249));
#36234=CARTESIAN_POINT('Ctrl Pts',(100.743919866758,4.45396550296464,337.090493929296));
#36235=CARTESIAN_POINT('Ctrl Pts',(100.736162756984,4.50872803287847,336.964829404309));
#36236=CARTESIAN_POINT('Ctrl Pts',(100.728401502057,4.56351982613743,336.839097728217));
#36237=CARTESIAN_POINT('Ctrl Pts',(100.720640247131,4.61300490586243,336.71117218157));
#36238=CARTESIAN_POINT('Ctrl Pts',(100.712878992205,4.65702713955602,336.58154395574));
#36239=CARTESIAN_POINT('Ctrl Pts',(100.7051053218,4.70111979447662,336.451708366995));
#36240=CARTESIAN_POINT('Ctrl Pts',(100.697331651396,4.73973203056139,336.320165031491));
#36241=CARTESIAN_POINT('Ctrl Pts',(100.689557980991,4.77275815381855,336.187418488848));
#36242=CARTESIAN_POINT('Ctrl Pts',(100.682146176814,4.80424690309206,336.060851329704));
#36243=CARTESIAN_POINT('Ctrl Pts',(100.674734372637,4.83065784455062,335.933190742926));
#36244=CARTESIAN_POINT('Ctrl Pts',(100.66732256846,4.85194329325969,335.804878463802));
#36245=CARTESIAN_POINT('Ctrl Pts',(100.659547489682,4.87427200521635,335.670277217654));
#36246=CARTESIAN_POINT('Ctrl Pts',(100.651772410903,4.89103065195819,335.534533416312));
#36247=CARTESIAN_POINT('Ctrl Pts',(100.643997332125,4.90210785439088,335.398147769577));
#36248=CARTESIAN_POINT('Ctrl Pts',(100.636231821076,4.91317142562076,335.261929954063));
#36249=CARTESIAN_POINT('Ctrl Pts',(100.628466310027,4.91856743204089,335.125072250561));
#36250=CARTESIAN_POINT('Ctrl Pts',(100.620700798978,4.91823556752981,334.988085102406));
#36251=CARTESIAN_POINT('Ctrl Pts',(100.612942987456,4.91790403206337,334.851233777407));
#36252=CARTESIAN_POINT('Ctrl Pts',(100.605185175933,4.9118559285371,334.714253651524));
#36253=CARTESIAN_POINT('Ctrl Pts',(100.597427364411,4.90008280970267,334.577659473225));
#36254=CARTESIAN_POINT('Ctrl Pts',(100.589675390888,4.8883185505134,334.441168086376));
#36255=CARTESIAN_POINT('Ctrl Pts',(100.581923417365,4.87083788481801,334.305062456871));
#36256=CARTESIAN_POINT('Ctrl Pts',(100.574171443842,4.8476844226134,334.169856156289));
#36257=CARTESIAN_POINT('Ctrl Pts',(100.566422753285,4.82454076591387,334.034707115656));
#36258=CARTESIAN_POINT('Ctrl Pts',(100.558674062727,4.79572915681226,333.900457030895));
#36259=CARTESIAN_POINT('Ctrl Pts',(100.550925372169,4.76134489930317,333.767612961615));
#36260=CARTESIAN_POINT('Ctrl Pts',(100.543178293791,4.72696779572603,333.634796531653));
#36261=CARTESIAN_POINT('Ctrl Pts',(100.535431215414,4.68702044782326,333.503385913469));
#36262=CARTESIAN_POINT('Ctrl Pts',(100.527684137036,4.64164889823777,333.373876213818));
#36263=CARTESIAN_POINT('Ctrl Pts',(100.51993699373,4.596276968395,333.24436542875));
#36264=CARTESIAN_POINT('Ctrl Pts',(100.512189850424,4.54548087543105,333.116755962883));
#36265=CARTESIAN_POINT('Ctrl Pts',(100.504442707118,4.48945585917286,332.991525665825));
#36266=CARTESIAN_POINT('Ctrl Pts',(100.49669382209,4.43341824730153,332.866267214338));
#36267=CARTESIAN_POINT('Ctrl Pts',(100.488944937062,4.3721495324679,332.743389352755));
#36268=CARTESIAN_POINT('Ctrl Pts',(100.481196052034,4.30589204242829,332.623347568227));
#36269=CARTESIAN_POINT('Ctrl Pts',(100.473438942259,4.23956422600428,332.503178370109));
#36270=CARTESIAN_POINT('Ctrl Pts',(100.465681832485,4.16823724602133,332.385851605034));
#36271=CARTESIAN_POINT('Ctrl Pts',(100.45792472271,4.09219841323417,332.271796340222));
#36272=CARTESIAN_POINT('Ctrl Pts',(100.450163467784,4.01611894772591,332.157680127924));
#36273=CARTESIAN_POINT('Ctrl Pts',(100.442402212858,3.93532284247185,332.046839215009));
#36274=CARTESIAN_POINT('Ctrl Pts',(100.434640957931,3.85013865852148,331.93967070846));
#36275=CARTESIAN_POINT('Ctrl Pts',(100.426867287527,3.76481820763837,331.832330767227));
#36276=CARTESIAN_POINT('Ctrl Pts',(100.419093617122,3.67509590697439,331.728675267351));
#36277=CARTESIAN_POINT('Ctrl Pts',(100.411319946717,3.58133883757604,331.629066124504));
#36278=CARTESIAN_POINT('Ctrl Pts',(100.40390814254,3.49194618231444,331.53409381122));
#36279=CARTESIAN_POINT('Ctrl Pts',(100.396496338363,3.39888614725456,331.442799818424));
#36280=CARTESIAN_POINT('Ctrl Pts',(100.389084534186,3.3025043919707,331.355463293707));
#36281=CARTESIAN_POINT('Ctrl Pts',(100.381309455408,3.20139867975431,331.263846145752));
#36282=CARTESIAN_POINT('Ctrl Pts',(100.373534376629,3.0963178866018,331.176294682293));
#36283=CARTESIAN_POINT('Ctrl Pts',(100.365759297851,2.98762279644792,331.093173527191));
#36284=CARTESIAN_POINT('Ctrl Pts',(100.357993786802,2.87906146252249,331.010154657961));
#36285=CARTESIAN_POINT('Ctrl Pts',(100.350228275753,2.76689498861329,330.931555484785));
#36286=CARTESIAN_POINT('Ctrl Pts',(100.342462764704,2.65151998230749,330.857702950545));
#36287=CARTESIAN_POINT('Ctrl Pts',(100.334704953181,2.53625937065612,330.783923641307));
#36288=CARTESIAN_POINT('Ctrl Pts',(100.326947141659,2.41779688459907,330.714881814559));
#36289=CARTESIAN_POINT('Ctrl Pts',(100.319189330137,2.29656081581479,330.650863133705));
#36290=CARTESIAN_POINT('Ctrl Pts',(100.311437356614,2.17541598101747,330.586892628939));
#36291=CARTESIAN_POINT('Ctrl Pts',(100.303685383091,2.05150206223303,330.527937927792));
#36292=CARTESIAN_POINT('Ctrl Pts',(100.295933409568,1.92527453263051,330.474240280737));
#36293=CARTESIAN_POINT('Ctrl Pts',(100.288184719011,1.79910046046129,330.420565374667));
#36294=CARTESIAN_POINT('Ctrl Pts',(100.280436028453,1.67061508519094,330.372143247297));
#36295=CARTESIAN_POINT('Ctrl Pts',(100.272687337895,1.54029637852283,330.329168154514));
#36296=CARTESIAN_POINT('Ctrl Pts',(100.264940259517,1.41000478575017,330.286202003057));
#36297=CARTESIAN_POINT('Ctrl Pts',(100.25719318114,1.27788099126858,330.248680754309));
#36298=CARTESIAN_POINT('Ctrl Pts',(100.249446102762,1.14442037296369,330.216749528569));
#36299=CARTESIAN_POINT('Ctrl Pts',(100.241698959456,1.01095863613017,330.184818035214));
#36300=CARTESIAN_POINT('Ctrl Pts',(100.23395181615,0.876160433271687,330.158476749264));
#36301=CARTESIAN_POINT('Ctrl Pts',(100.226204672844,0.740533253792945,330.137820081226));
#36302=CARTESIAN_POINT('Ctrl Pts',(100.218455787816,0.604875582445456,330.117158769131));
#36303=CARTESIAN_POINT('Ctrl Pts',(100.210706902788,0.468388949961799,330.102184676912));
#36304=CARTESIAN_POINT('Ctrl Pts',(100.20295801776,0.331587522659386,330.092940516224));
#36305=CARTESIAN_POINT('Ctrl Pts',(100.195200907985,0.194640892907958,330.083686543688));
#36306=CARTESIAN_POINT('Ctrl Pts',(100.187443798211,0.0573791914896888,
330.08017467806));
#36307=CARTESIAN_POINT('Ctrl Pts',(100.179686688436,-0.0796812894812625,
330.082395506488));
#36308=CARTESIAN_POINT('Ctrl Pts',(100.17192543351,-0.216815011190714,330.084617521657));
#36309=CARTESIAN_POINT('Ctrl Pts',(100.164164178584,-0.353746908180597,
330.092578312245));
#36310=CARTESIAN_POINT('Ctrl Pts',(100.156402923657,-0.489965241480037,
330.106216481633));
#36311=CARTESIAN_POINT('Ctrl Pts',(100.148629253253,-0.62640147971949,330.119876467647));
#36312=CARTESIAN_POINT('Ctrl Pts',(100.140855582848,-0.762121486112149,
330.139231925682));
#36313=CARTESIAN_POINT('Ctrl Pts',(100.133081912443,-0.896622269431508,
330.164170022792));
#36314=CARTESIAN_POINT('Ctrl Pts',(100.125670108266,-1.02486200892952,330.187947245483));
#36315=CARTESIAN_POINT('Ctrl Pts',(100.118258304089,-1.15199319989853,330.216798996364));
#36316=CARTESIAN_POINT('Ctrl Pts',(100.110846499912,-1.2775940449448,330.250585665703));
#36317=CARTESIAN_POINT('Ctrl Pts',(100.103071421134,-1.40935096155144,330.286028320353));
#36318=CARTESIAN_POINT('Ctrl Pts',(100.095296342355,-1.53984010171249,330.327013880536));
#36319=CARTESIAN_POINT('Ctrl Pts',(100.087521263577,-1.66855960455591,330.373436274237));
#36320=CARTESIAN_POINT('Ctrl Pts',(100.079755752528,-1.79712070985586,330.419801542228));
#36321=CARTESIAN_POINT('Ctrl Pts',(100.071990241479,-1.92391614656229,330.47159020048));
#36322=CARTESIAN_POINT('Ctrl Pts',(100.06422473043,-2.0484563543082,330.528645660765));
#36323=CARTESIAN_POINT('Ctrl Pts',(100.056466918907,-2.17287308007527,330.585644550395));
#36324=CARTESIAN_POINT('Ctrl Pts',(100.048709107385,-2.29503867371132,330.647899688134));
#36325=CARTESIAN_POINT('Ctrl Pts',(100.040951295863,-2.41448114156284,330.715205503232));
#36326=CARTESIAN_POINT('Ctrl Pts',(100.03319932234,-2.53383372516972,330.782460668569));
#36327=CARTESIAN_POINT('Ctrl Pts',(100.025447348817,-2.65046692274143,330.854758754851));
#36328=CARTESIAN_POINT('Ctrl Pts',(100.017695375294,-2.76393137894123,330.931847299449));
#36329=CARTESIAN_POINT('Ctrl Pts',(100.009946684736,-2.87734778287708,331.008903197002));
#36330=CARTESIAN_POINT('Ctrl Pts',(100.002197994179,-2.98759779187196,331.090745298601));
#36331=CARTESIAN_POINT('Ctrl Pts',(99.9944493036212,-3.09425939409105,331.177076790651));
#36332=CARTESIAN_POINT('Ctrl Pts',(99.9867022252433,-3.20089880447274,331.263390320713));
#36333=CARTESIAN_POINT('Ctrl Pts',(99.9789551468655,-3.30395098948162,331.354191137564));
#36334=CARTESIAN_POINT('Ctrl Pts',(99.9712080684876,-3.40302583696322,331.449141200292));
#36335=CARTESIAN_POINT('Ctrl Pts',(99.9634609251818,-3.50210151478734,331.544092058794));
#36336=CARTESIAN_POINT('Ctrl Pts',(99.955713781876,-3.59719950639529,331.643191962081));
#36337=CARTESIAN_POINT('Ctrl Pts',(99.9479666385702,-3.68796578834079,331.746065242429));
#36338=CARTESIAN_POINT('Ctrl Pts',(99.9402177535422,-3.77875247647306,331.848961650874));
#36339=CARTESIAN_POINT('Ctrl Pts',(99.9324688685141,-3.8652052585162,331.955632831432));
#36340=CARTESIAN_POINT('Ctrl Pts',(99.924719983486,-3.94700997243212,332.065669524402));
#36341=CARTESIAN_POINT('Ctrl Pts',(99.9169628737113,-4.02890151471693,332.175823011456));
#36342=CARTESIAN_POINT('Ctrl Pts',(99.9092057639366,-4.10613490015827,332.289348832527));
#36343=CARTESIAN_POINT('Ctrl Pts',(99.9014486541619,-4.17843864893525,332.405807732726));
#36344=CARTESIAN_POINT('Ctrl Pts',(99.8936873992357,-4.2507810345239,332.522328864838));
#36345=CARTESIAN_POINT('Ctrl Pts',(99.8859261443095,-4.31818834249381,332.641785858909));
#36346=CARTESIAN_POINT('Ctrl Pts',(99.8781648893833,-4.38043527125306,332.763715157485));
#36347=CARTESIAN_POINT('Ctrl Pts',(99.8703912189787,-4.44278177481197,332.885839503202));
#36348=CARTESIAN_POINT('Ctrl Pts',(99.862617548574,-4.49995124029065,333.010443700996));
#36349=CARTESIAN_POINT('Ctrl Pts',(99.8548438781693,-4.55176635390703,333.137043714431));
#36350=CARTESIAN_POINT('Ctrl Pts',(99.8474320739922,-4.60116946151882,333.257750466784));
#36351=CARTESIAN_POINT('Ctrl Pts',(99.8400202698151,-4.64570539089723,333.380271135409));
#36352=CARTESIAN_POINT('Ctrl Pts',(99.832608465638,-4.68526328407162,333.504175471043));
#36353=CARTESIAN_POINT('Ctrl Pts',(99.8232353781635,-4.73528883576806,333.660866898474));
#36354=CARTESIAN_POINT('Ctrl Pts',(99.8138622906892,-4.7774827072035,333.820172031332));
#36355=CARTESIAN_POINT('Ctrl Pts',(99.8044892032148,-4.81161011964247,333.981377833024));
#36356=CARTESIAN_POINT('Ctrl Pts',(99.7948303774347,-4.84677790528113,334.147497989006));
#36357=CARTESIAN_POINT('Ctrl Pts',(99.7851715516546,-4.87337953316264,334.315636592827));
#36358=CARTESIAN_POINT('Ctrl Pts',(99.7755127258746,-4.89121119682611,334.484989232595));
#36359=CARTESIAN_POINT('Ctrl Pts',(99.7658539000946,-4.90904286048958,334.654341872363));
#36360=CARTESIAN_POINT('Ctrl Pts',(99.7561950743145,-4.91810436491552,334.824908550451));
#36361=CARTESIAN_POINT('Ctrl Pts',(99.7465362485345,-4.91824825774415,334.995860229885));
#36362=CARTESIAN_POINT('',(103.246536248441,-4.9182479760333,335.004461921597));
#36363=CARTESIAN_POINT('Ctrl Pts',(103.246536248441,-4.9182479760333,335.004461921597));
#36364=CARTESIAN_POINT('Ctrl Pts',(103.236856380282,-4.91809274950663,335.175563661959));
#36365=CARTESIAN_POINT('Ctrl Pts',(103.227176512124,-4.90900520981435,335.346267587011));
#36366=CARTESIAN_POINT('Ctrl Pts',(103.217496643965,-4.89113126270125,335.515769360787));
#36367=CARTESIAN_POINT('Ctrl Pts',(103.207644322872,-4.87293887998704,335.68829091519));
#36368=CARTESIAN_POINT('Ctrl Pts',(103.197792001779,-4.84564425788045,335.859567237283));
#36369=CARTESIAN_POINT('Ctrl Pts',(103.187939680686,-4.80944972616464,336.028774219153));
#36370=CARTESIAN_POINT('Ctrl Pts',(103.182448079432,-4.78927519735431,336.123088773558));
#36371=CARTESIAN_POINT('Ctrl Pts',(103.176956478179,-4.76633645145549,336.21676082811));
#36372=CARTESIAN_POINT('Ctrl Pts',(103.171464876925,-4.74067489486865,336.30965056548));
#36373=CARTESIAN_POINT('Ctrl Pts',(103.163689798147,-4.70434293724311,336.441165035016));
#36374=CARTESIAN_POINT('Ctrl Pts',(103.155914719368,-4.66247676530616,336.571374310764));
#36375=CARTESIAN_POINT('Ctrl Pts',(103.14813964059,-4.61518583907942,336.699777259896));
#36376=CARTESIAN_POINT('Ctrl Pts',(103.140374129541,-4.5679531073481,336.828022201025));
#36377=CARTESIAN_POINT('Ctrl Pts',(103.132608618492,-4.51530903746602,336.95446487499));
#36378=CARTESIAN_POINT('Ctrl Pts',(103.124843107443,-4.45741352141672,337.078616790462));
#36379=CARTESIAN_POINT('Ctrl Pts',(103.11708529592,-4.39957540894019,337.202645608948));
#36380=CARTESIAN_POINT('Ctrl Pts',(103.109327484398,-4.33649637630331,337.324387836976));
#36381=CARTESIAN_POINT('Ctrl Pts',(103.101569672876,-4.26838517821838,337.443372880439));
#36382=CARTESIAN_POINT('Ctrl Pts',(103.093817699353,-4.20032523596984,337.562268383884));
#36383=CARTESIAN_POINT('Ctrl Pts',(103.08606572583,-4.12724085924443,337.678410494829));
#36384=CARTESIAN_POINT('Ctrl Pts',(103.078313752307,-4.04938754062701,337.791351573757));
#36385=CARTESIAN_POINT('Ctrl Pts',(103.070565061749,-3.97156719293634,337.90424482207));
#36386=CARTESIAN_POINT('Ctrl Pts',(103.062816371192,-3.8889821416736,338.013939413484));
#36387=CARTESIAN_POINT('Ctrl Pts',(103.055067680634,-3.80193204465115,338.120015350981));
#36388=CARTESIAN_POINT('Ctrl Pts',(103.047320602256,-3.71490005912839,338.226069218493));
#36389=CARTESIAN_POINT('Ctrl Pts',(103.039573523878,-3.62340512347811,338.328505627676));
#36390=CARTESIAN_POINT('Ctrl Pts',(103.0318264455,-3.52778790638298,338.426936758984));
#36391=CARTESIAN_POINT('Ctrl Pts',(103.024079302195,-3.43216988792355,338.525368715241));
#36392=CARTESIAN_POINT('Ctrl Pts',(103.016332158889,-3.3324297914626,338.6197950463));
#36393=CARTESIAN_POINT('Ctrl Pts',(103.008585015583,-3.2289456678323,338.709864274699));
#36394=CARTESIAN_POINT('Ctrl Pts',(103.000836130555,-3.12543827877412,338.799953752572));
#36395=CARTESIAN_POINT('Ctrl Pts',(102.993087245527,-3.01818548236551,338.885683921983));
#36396=CARTESIAN_POINT('Ctrl Pts',(102.985338360499,-2.90759865135431,338.966743392903));
#36397=CARTESIAN_POINT('Ctrl Pts',(102.977581250724,-2.79689444233794,339.047888901184));
#36398=CARTESIAN_POINT('Ctrl Pts',(102.969824140949,-2.68284944542831,339.124353576403));
#36399=CARTESIAN_POINT('Ctrl Pts',(102.962067031174,-2.56590473952805,339.195868912415));
#36400=CARTESIAN_POINT('Ctrl Pts',(102.954305776248,-2.44889754211613,339.267422463935));
#36401=CARTESIAN_POINT('Ctrl Pts',(102.946544521322,-2.32898788970553,339.334021216618));
#36402=CARTESIAN_POINT('Ctrl Pts',(102.938783266396,-2.20664085124335,339.395443005673));
#36403=CARTESIAN_POINT('Ctrl Pts',(102.931009595991,-2.08409809739251,339.456963049574));
#36404=CARTESIAN_POINT('Ctrl Pts',(102.923235925587,-1.95911052263342,339.513289420368));
#36405=CARTESIAN_POINT('Ctrl Pts',(102.915462255182,-1.83216335023625,339.564248078331));
#36406=CARTESIAN_POINT('Ctrl Pts',(102.908050451005,-1.71112559925907,339.612834598505));
#36407=CARTESIAN_POINT('Ctrl Pts',(102.900638646828,-1.58830685465758,339.656541797219));
#36408=CARTESIAN_POINT('Ctrl Pts',(102.893226842651,-1.46413810480163,339.695261725673));
#36409=CARTESIAN_POINT('Ctrl Pts',(102.885451763873,-1.33388347463229,339.735879433162));
#36410=CARTESIAN_POINT('Ctrl Pts',(102.877676685094,-1.20173152884744,339.771136986518));
#36411=CARTESIAN_POINT('Ctrl Pts',(102.869901606316,-1.06816291583152,339.800855241282));
#36412=CARTESIAN_POINT('Ctrl Pts',(102.862136095267,-0.934758667497211,
339.830536925841));
#36413=CARTESIAN_POINT('Ctrl Pts',(102.854370584218,-0.799941598494425,
339.854692790527));
#36414=CARTESIAN_POINT('Ctrl Pts',(102.846605073169,-0.664209018331135,
339.873192941231));
#36415=CARTESIAN_POINT('Ctrl Pts',(102.838847261647,-0.528611017416344,
339.891674748983));
#36416=CARTESIAN_POINT('Ctrl Pts',(102.831089450124,-0.392099696577586,
339.90451194986));
#36417=CARTESIAN_POINT('Ctrl Pts',(102.823331638602,-0.25518375759123,339.91162542468));
#36418=CARTESIAN_POINT('Ctrl Pts',(102.815579665079,-0.118370852191,339.918733546385));
#36419=CARTESIAN_POINT('Ctrl Pts',(102.807827691556,0.0188456765122954,
339.920126495275));
#36420=CARTESIAN_POINT('Ctrl Pts',(102.800075718033,0.155951137200529,339.915776877087));
#36421=CARTESIAN_POINT('Ctrl Pts',(102.792327027475,0.292998533644854,339.911429100966));
#36422=CARTESIAN_POINT('Ctrl Pts',(102.784578336918,0.429934565763458,339.901343607172));
#36423=CARTESIAN_POINT('Ctrl Pts',(102.77682964636,0.566243887067581,339.885545099869));
#36424=CARTESIAN_POINT('Ctrl Pts',(102.769082567982,0.70252484807893,339.869749879578));
#36425=CARTESIAN_POINT('Ctrl Pts',(102.761335489605,0.838178969604223,339.84824405504));
#36426=CARTESIAN_POINT('Ctrl Pts',(102.753588411227,0.9726957705425,339.821104230409));
#36427=CARTESIAN_POINT('Ctrl Pts',(102.745841267921,1.10721369886104,339.793964178321));
#36428=CARTESIAN_POINT('Ctrl Pts',(102.738094124615,1.24059390442689,339.761190109263));
#36429=CARTESIAN_POINT('Ctrl Pts',(102.730346981309,1.37233623734387,339.722909729624));
#36430=CARTESIAN_POINT('Ctrl Pts',(102.722598096281,1.50410818873425,339.684620743742));
#36431=CARTESIAN_POINT('Ctrl Pts',(102.714849211253,1.63424115946567,339.640823092968));
#36432=CARTESIAN_POINT('Ctrl Pts',(102.707100326225,1.76225067762179,339.591694198411));
#36433=CARTESIAN_POINT('Ctrl Pts',(102.69934321645,1.89039606640315,339.542513157937));
#36434=CARTESIAN_POINT('Ctrl Pts',(102.691586106676,2.01641313482551,339.487989710296));
#36435=CARTESIAN_POINT('Ctrl Pts',(102.683828996901,2.13983739723886,339.428349464064));
#36436=CARTESIAN_POINT('Ctrl Pts',(102.676067741975,2.2633276136317,339.368677347991));
#36437=CARTESIAN_POINT('Ctrl Pts',(102.668306487049,2.38422191891857,339.303883169632));
#36438=CARTESIAN_POINT('Ctrl Pts',(102.660545232122,2.50208181449505,339.234237789269));
#36439=CARTESIAN_POINT('Ctrl Pts',(102.652771561718,2.62013024749392,339.164480998995));
#36440=CARTESIAN_POINT('Ctrl Pts',(102.644997891313,2.73513424285291,339.089857712131));
#36441=CARTESIAN_POINT('Ctrl Pts',(102.637224220908,2.84668486470064,339.010681780394));
#36442=CARTESIAN_POINT('Ctrl Pts',(102.629812416731,2.95304277826437,338.935191507328));
#36443=CARTESIAN_POINT('Ctrl Pts',(102.622400612554,3.0562613641603,338.85556307791));
#36444=CARTESIAN_POINT('Ctrl Pts',(102.614988808377,3.15601661340184,338.772100502165));
#36445=CARTESIAN_POINT('Ctrl Pts',(102.607213729599,3.26066116456381,338.684547176961));
#36446=CARTESIAN_POINT('Ctrl Pts',(102.59943865082,3.36182499410937,338.592497671611));
#36447=CARTESIAN_POINT('Ctrl Pts',(102.591663572042,3.45909734921933,338.49625922825));
#36448=CARTESIAN_POINT('Ctrl Pts',(102.583898060993,3.55625000450366,338.400139212421));
#36449=CARTESIAN_POINT('Ctrl Pts',(102.576132549944,3.64952043829995,338.299840787345));
#36450=CARTESIAN_POINT('Ctrl Pts',(102.568367038895,3.73853029717096,338.195711858043));
#36451=CARTESIAN_POINT('Ctrl Pts',(102.560609227373,3.82745190250776,338.091686172877));
#36452=CARTESIAN_POINT('Ctrl Pts',(102.55285141585,3.91212108731851,337.983837836835));
#36453=CARTESIAN_POINT('Ctrl Pts',(102.545093604328,3.99219603087451,337.872551812165));
#36454=CARTESIAN_POINT('Ctrl Pts',(102.537341630805,4.07221071549611,337.761349533756));
#36455=CARTESIAN_POINT('Ctrl Pts',(102.529589657282,4.14763781309923,337.646715031955));
#36456=CARTESIAN_POINT('Ctrl Pts',(102.521837683759,4.2181757582583,337.529066297063));
#36457=CARTESIAN_POINT('Ctrl Pts',(102.514088993202,4.28868383055571,337.411467386481));
#36458=CARTESIAN_POINT('Ctrl Pts',(102.506340302644,4.35430666802759,337.290857116273));
#36459=CARTESIAN_POINT('Ctrl Pts',(102.498591612086,4.41478616137502,337.167682221137));
#36460=CARTESIAN_POINT('Ctrl Pts',(102.490844533709,4.47525307145877,337.044532953566));
#36461=CARTESIAN_POINT('Ctrl Pts',(102.483097455331,4.5305785937871,336.91882047306));
#36462=CARTESIAN_POINT('Ctrl Pts',(102.475350376953,4.58055089581245,336.79101550897));
#36463=CARTESIAN_POINT('Ctrl Pts',(102.467603233647,4.63052361665375,336.663209473752));
#36464=CARTESIAN_POINT('Ctrl Pts',(102.459856090341,4.67514288536555,336.533311284007));
#36465=CARTESIAN_POINT('Ctrl Pts',(102.452108947036,4.71424543316517,336.401810635707));
#36466=CARTESIAN_POINT('Ctrl Pts',(102.444360062008,4.7533567720477,336.270280423269));
#36467=CARTESIAN_POINT('Ctrl Pts',(102.436611176979,4.7869488106213,336.137147409974));
#36468=CARTESIAN_POINT('Ctrl Pts',(102.428862291951,4.81490857052794,336.002915011333));
#36469=CARTESIAN_POINT('Ctrl Pts',(102.421105182177,4.84289800721261,335.868540137037));
#36470=CARTESIAN_POINT('Ctrl Pts',(102.413348072402,4.86524314346552,335.733063929671));
#36471=CARTESIAN_POINT('Ctrl Pts',(102.405590962627,4.88188233851452,335.596999074874));
#36472=CARTESIAN_POINT('Ctrl Pts',(102.397829707701,4.89853042501733,335.460861511368));
#36473=CARTESIAN_POINT('Ctrl Pts',(102.390068452775,4.9094664636159,335.324135063086));
#36474=CARTESIAN_POINT('Ctrl Pts',(102.382307197849,4.91468092974551,335.1873350509));
#36475=CARTESIAN_POINT('Ctrl Pts',(102.374533527444,4.91990373732155,335.050316203277));
#36476=CARTESIAN_POINT('Ctrl Pts',(102.366759857039,4.91938668419584,334.913223947672));
#36477=CARTESIAN_POINT('Ctrl Pts',(102.358986186635,4.91317239630912,334.776572010155));
#36478=CARTESIAN_POINT('Ctrl Pts',(102.351574382458,4.90724738501865,334.646281253207));
#36479=CARTESIAN_POINT('Ctrl Pts',(102.344162578281,4.89614363943262,334.516391030021));
#36480=CARTESIAN_POINT('Ctrl Pts',(102.336750774104,4.87994146821236,334.387338323933));
#36481=CARTESIAN_POINT('Ctrl Pts',(102.328975695325,4.8629451803167,334.251960360291));
#36482=CARTESIAN_POINT('Ctrl Pts',(102.321200616547,4.84028434042474,334.117076268646));
#36483=CARTESIAN_POINT('Ctrl Pts',(102.313425537768,4.81199503308198,333.983197726156));
#36484=CARTESIAN_POINT('Ctrl Pts',(102.305660026719,4.78374053753292,333.849483929736));
#36485=CARTESIAN_POINT('Ctrl Pts',(102.29789451567,4.74987143569738,333.716773599188));
#36486=CARTESIAN_POINT('Ctrl Pts',(102.290129004621,4.71047553957375,333.58557317136));
#36487=CARTESIAN_POINT('Ctrl Pts',(102.282371193099,4.67111870459582,333.454502829137));
#36488=CARTESIAN_POINT('Ctrl Pts',(102.274613381577,4.62624609219297,333.324939782324));
#36489=CARTESIAN_POINT('Ctrl Pts',(102.266855570055,4.57599644652163,333.197379800423));
#36490=CARTESIAN_POINT('Ctrl Pts',(102.259103596532,4.52578461530216,333.069915811455));
#36491=CARTESIAN_POINT('Ctrl Pts',(102.251351623009,4.47020394763686,332.944452249263));
#36492=CARTESIAN_POINT('Ctrl Pts',(102.243599649486,4.40944274613266,332.821468905184));
#36493=CARTESIAN_POINT('Ctrl Pts',(102.235850958928,4.34870727703337,332.698537644625));
#36494=CARTESIAN_POINT('Ctrl Pts',(102.22810226837,4.28279581050217,332.578084862768));
#36495=CARTESIAN_POINT('Ctrl Pts',(102.220353577813,4.21194433752394,332.460569363007));
#36496=CARTESIAN_POINT('Ctrl Pts',(102.212606499435,4.14110760578643,332.343078313326));
#36497=CARTESIAN_POINT('Ctrl Pts',(102.204859421057,4.06533311368053,332.2285236647));
#36498=CARTESIAN_POINT('Ctrl Pts',(102.197112342679,3.98490207281434,332.117338290298));
#36499=CARTESIAN_POINT('Ctrl Pts',(102.189365199373,3.90447035785861,332.006151984056));
#36500=CARTESIAN_POINT('Ctrl Pts',(102.181618056068,3.81938224539899,331.898335325059));
#36501=CARTESIAN_POINT('Ctrl Pts',(102.173870912762,3.72996117711833,331.794290612097));
#36502=CARTESIAN_POINT('Ctrl Pts',(102.166122027734,3.64052000508312,331.690222507675));
#36503=CARTESIAN_POINT('Ctrl Pts',(102.158373142706,3.54674419351778,331.589928333119));
#36504=CARTESIAN_POINT('Ctrl Pts',(102.150624257677,3.4489959361942,331.49377552136));
#36505=CARTESIAN_POINT('Ctrl Pts',(102.142867147903,3.35114392786029,331.397520652013));
#36506=CARTESIAN_POINT('Ctrl Pts',(102.135110038128,3.24931133021835,331.305416200796));
#36507=CARTESIAN_POINT('Ctrl Pts',(102.127352928353,3.14389591420087,331.217791446367));
#36508=CARTESIAN_POINT('Ctrl Pts',(102.119591673427,3.03842416755553,331.130119868071));
#36509=CARTESIAN_POINT('Ctrl Pts',(102.111830418501,2.92936609825969,331.046932993376));
#36510=CARTESIAN_POINT('Ctrl Pts',(102.104069163575,2.81714989634082,330.968517701385));
#36511=CARTESIAN_POINT('Ctrl Pts',(102.09629549317,2.70475418507014,330.889976970482));
#36512=CARTESIAN_POINT('Ctrl Pts',(102.088521822765,2.58919057548164,330.816223285626));
#36513=CARTESIAN_POINT('Ctrl Pts',(102.080748152361,2.47091413813151,330.747498808409));
#36514=CARTESIAN_POINT('Ctrl Pts',(102.073336348184,2.35814349739529,330.681973472141));
#36515=CARTESIAN_POINT('Ctrl Pts',(102.065924544006,2.24290716376067,330.621019795825));
#36516=CARTESIAN_POINT('Ctrl Pts',(102.058512739829,2.12561606546375,330.564806722955));
#36517=CARTESIAN_POINT('Ctrl Pts',(102.050737661051,2.00257618104758,330.505838479934));
#36518=CARTESIAN_POINT('Ctrl Pts',(102.042962582272,1.87688619001357,330.45190094201));
#36519=CARTESIAN_POINT('Ctrl Pts',(102.035187503494,1.74899590001713,330.40324066279));
#36520=CARTESIAN_POINT('Ctrl Pts',(102.027421992445,1.62126298716442,330.354640263142));
#36521=CARTESIAN_POINT('Ctrl Pts',(102.019656481396,1.49133552454444,330.311304338665));
#36522=CARTESIAN_POINT('Ctrl Pts',(102.011890970347,1.35968690581637,330.273433108412));
#36523=CARTESIAN_POINT('Ctrl Pts',(102.004133158825,1.22816881707706,330.235599427595));
#36524=CARTESIAN_POINT('Ctrl Pts',(101.996375347303,1.09493334154405,330.203219765723));
#36525=CARTESIAN_POINT('Ctrl Pts',(101.98861753578,0.960472464794403,330.176445739201));
#36526=CARTESIAN_POINT('Ctrl Pts',(101.980865562257,0.826112774118606,330.149691860983));
#36527=CARTESIAN_POINT('Ctrl Pts',(101.973113588735,0.690529899532061,330.128535297584));
#36528=CARTESIAN_POINT('Ctrl Pts',(101.965361615212,0.554229209151167,330.113077343949));
#36529=CARTESIAN_POINT('Ctrl Pts',(101.957612924654,0.417986242193478,330.097625936766));
#36530=CARTESIAN_POINT('Ctrl Pts',(101.949864234096,0.281026451643177,330.08786838329));
#36531=CARTESIAN_POINT('Ctrl Pts',(101.942115543539,0.143863363325315,330.083854518508));
#36532=CARTESIAN_POINT('Ctrl Pts',(101.934368465161,0.00672881293358724,
330.079841488845));
#36533=CARTESIAN_POINT('Ctrl Pts',(101.926621386783,-0.130608560630653,
330.081569782318));
#36534=CARTESIAN_POINT('Ctrl Pts',(101.918874308405,-0.267632565345737,
330.089037174599));
#36535=CARTESIAN_POINT('Ctrl Pts',(101.911127165099,-0.404657718453866,
330.096504629465));
#36536=CARTESIAN_POINT('Ctrl Pts',(101.903380021794,-0.541369107179274,
330.109711257805));
#36537=CARTESIAN_POINT('Ctrl Pts',(101.895632878488,-0.677253397031937,
330.128602777569));
#36538=CARTESIAN_POINT('Ctrl Pts',(101.88788399346,-0.813168236557865,330.147498544548));
#36539=CARTESIAN_POINT('Ctrl Pts',(101.880135108432,-0.948255220117501,
330.172081692381));
#36540=CARTESIAN_POINT('Ctrl Pts',(101.872386223404,-1.08200936168753,330.202246483643));
#36541=CARTESIAN_POINT('Ctrl Pts',(101.864629113629,-1.21590547128545,330.232443292125));
#36542=CARTESIAN_POINT('Ctrl Pts',(101.856872003854,-1.34846553101308,330.26823349248));
#36543=CARTESIAN_POINT('Ctrl Pts',(101.849114894079,-1.47919738674698,330.309460782219));
#36544=CARTESIAN_POINT('Ctrl Pts',(101.841353639153,-1.60999910140449,330.350710102504));
#36545=CARTESIAN_POINT('Ctrl Pts',(101.833592384227,-1.73897029809642,330.397402168467));
#36546=CARTESIAN_POINT('Ctrl Pts',(101.825831129301,-1.86563801587126,330.449332152724));
#36547=CARTESIAN_POINT('Ctrl Pts',(101.818057458896,-1.99250836071363,330.501345208031));
#36548=CARTESIAN_POINT('Ctrl Pts',(101.810283788492,-2.11706750796173,330.558612761914));
#36549=CARTESIAN_POINT('Ctrl Pts',(101.802510118087,-2.23886555397652,330.620883183367));
#36550=CARTESIAN_POINT('Ctrl Pts',(101.79509831391,-2.35499387164689,330.68025490172));
#36551=CARTESIAN_POINT('Ctrl Pts',(101.787686509733,-2.46861211083911,330.744174061358));
#36552=CARTESIAN_POINT('Ctrl Pts',(101.780274705556,-2.57935582651927,330.812386528976));
#36553=CARTESIAN_POINT('Ctrl Pts',(101.772499626777,-2.69552742159293,330.883942292826));
#36554=CARTESIAN_POINT('Ctrl Pts',(101.764724547999,-2.8089027141783,330.96044899106));
#36555=CARTESIAN_POINT('Ctrl Pts',(101.75694946922,-2.91903095535628,331.041661795125));
#36556=CARTESIAN_POINT('Ctrl Pts',(101.749183958171,-3.02902367672238,331.122774661665));
#36557=CARTESIAN_POINT('Ctrl Pts',(101.741418447122,-3.13577698540662,331.208581881513));
#36558=CARTESIAN_POINT('Ctrl Pts',(101.733652936073,-3.23886633246278,331.298793717862));
#36559=CARTESIAN_POINT('Ctrl Pts',(101.725895124551,-3.34185346613127,331.388916108912));
#36560=CARTESIAN_POINT('Ctrl Pts',(101.718137313029,-3.44118357545025,331.483434169758));
#36561=CARTESIAN_POINT('Ctrl Pts',(101.710379501507,-3.53646292132437,331.58201622757));
#36562=CARTESIAN_POINT('Ctrl Pts',(101.702627527984,-3.63167056646917,331.680524099256));
#36563=CARTESIAN_POINT('Ctrl Pts',(101.694875554461,-3.72283324516891,331.783089600612));
#36564=CARTESIAN_POINT('Ctrl Pts',(101.687123580938,-3.80959229265892,331.889342573311));
#36565=CARTESIAN_POINT('Ctrl Pts',(101.67937489038,-3.89631459764081,331.995550547814));
#36566=CARTESIAN_POINT('Ctrl Pts',(101.671626199822,-3.97863673394537,332.105442585522));
#36567=CARTESIAN_POINT('Ctrl Pts',(101.663877509265,-4.05623889597741,332.218613820186));
#36568=CARTESIAN_POINT('Ctrl Pts',(101.656130430887,-4.13382491223149,332.331761508629));
#36569=CARTESIAN_POINT('Ctrl Pts',(101.648383352509,-4.20669268663047,332.448186714792));
#36570=CARTESIAN_POINT('Ctrl Pts',(101.640636274131,-4.2745647485384,332.567454158078));
#36571=CARTESIAN_POINT('Ctrl Pts',(101.632889130825,-4.34243737927953,332.68672260094));
#36572=CARTESIAN_POINT('Ctrl Pts',(101.62514198752,-4.4053140206942,332.80883298872));
#36573=CARTESIAN_POINT('Ctrl Pts',(101.617394844214,-4.4629625249699,332.93332427236));
#36574=CARTESIAN_POINT('Ctrl Pts',(101.609645959186,-4.52062398985323,333.057843544285));
#36575=CARTESIAN_POINT('Ctrl Pts',(101.601897074158,-4.573054814475,333.184744422588));
#36576=CARTESIAN_POINT('Ctrl Pts',(101.59414818913,-4.62007063878045,333.31354503316));
#36577=CARTESIAN_POINT('Ctrl Pts',(101.586391079355,-4.66713636616762,333.442482354031));
#36578=CARTESIAN_POINT('Ctrl Pts',(101.57863396958,-4.7087754777521,333.573323067354));
#36579=CARTESIAN_POINT('Ctrl Pts',(101.570876859805,-4.74485307879436,333.705568725982));
#36580=CARTESIAN_POINT('Ctrl Pts',(101.563115604879,-4.78094995855313,333.837885052462));
#36581=CARTESIAN_POINT('Ctrl Pts',(101.555354349953,-4.81147931904884,333.971607439323));
#36582=CARTESIAN_POINT('Ctrl Pts',(101.547593095027,-4.83635745769027,334.10622731976));
#36583=CARTESIAN_POINT('Ctrl Pts',(101.539819424622,-4.86127539324571,334.241062548133));
#36584=CARTESIAN_POINT('Ctrl Pts',(101.532045754218,-4.88052398721385,334.376797751824));
#36585=CARTESIAN_POINT('Ctrl Pts',(101.524272083813,-4.89407137280176,334.51291842529));
#36586=CARTESIAN_POINT('Ctrl Pts',(101.516860279636,-4.9069881243313,334.642702648657));
#36587=CARTESIAN_POINT('Ctrl Pts',(101.509448475459,-4.91472248797685,334.772836974893));
#36588=CARTESIAN_POINT('Ctrl Pts',(101.502036671282,-4.91729094773511,334.902877408281));
#36589=CARTESIAN_POINT('Ctrl Pts',(101.500203197018,-4.91792631326182,334.935045795652));
#36590=CARTESIAN_POINT('Ctrl Pts',(101.498369722754,-4.91824601993271,334.967220438261));
#36591=CARTESIAN_POINT('Ctrl Pts',(101.49653624849,-4.91824996307017,334.999397289198));
#36592=CARTESIAN_POINT('',(104.996536248525,-4.91824974554793,334.998417938773));
#36593=CARTESIAN_POINT('Ctrl Pts',(104.99653624849,-4.91824974554813,334.99841793939));
#36594=CARTESIAN_POINT('Ctrl Pts',(104.988593885279,-4.91829509434603,335.139396554485));
#36595=CARTESIAN_POINT('Ctrl Pts',(104.980651522069,-4.91227449297855,335.280324386072));
#36596=CARTESIAN_POINT('Ctrl Pts',(104.972709158858,-4.90022731154389,335.420660620571));
#36597=CARTESIAN_POINT('Ctrl Pts',(104.964761972148,-4.88817281370081,335.561082083073));
#36598=CARTESIAN_POINT('Ctrl Pts',(104.956814785438,-4.87008447169581,335.700910871338));
#36599=CARTESIAN_POINT('Ctrl Pts',(104.948867598728,-4.84605336641541,335.839612906257));
#36600=CARTESIAN_POINT('Ctrl Pts',(104.940914261939,-4.82200366421589,335.978422278334));
#36601=CARTESIAN_POINT('Ctrl Pts',(104.932960925151,-4.79200209388668,336.116102802447));
#36602=CARTESIAN_POINT('Ctrl Pts',(104.925007588362,-4.75619049114916,336.252132211231));
#36603=CARTESIAN_POINT('Ctrl Pts',(104.917041026786,-4.72031934097304,336.388387809357));
#36604=CARTESIAN_POINT('Ctrl Pts',(104.90907446521,-4.67861894877477,336.522986456037));
#36605=CARTESIAN_POINT('Ctrl Pts',(104.901107903634,-4.6312808721615,336.65542156131));
#36606=CARTESIAN_POINT('Ctrl Pts',(104.893134004349,-4.58389919417668,336.787978647717));
#36607=CARTESIAN_POINT('Ctrl Pts',(104.885160105064,-4.53086961314969,336.918367884027));
#36608=CARTESIAN_POINT('Ctrl Pts',(104.877186205779,-4.47243101695501,337.046104557709));
#36609=CARTESIAN_POINT('Ctrl Pts',(104.86919775366,-4.41388576689024,337.174074358323));
#36610=CARTESIAN_POINT('Ctrl Pts',(104.861209301541,-4.34991194027478,337.299381600503));
#36611=CARTESIAN_POINT('Ctrl Pts',(104.853220849422,-4.28079390098626,337.421566980238));
#36612=CARTESIAN_POINT('Ctrl Pts',(104.849111593804,-4.2452396175053,337.484419076059));
#36613=CARTESIAN_POINT('Ctrl Pts',(104.845002338186,-4.20832483760696,337.546445589308));
#36614=CARTESIAN_POINT('Ctrl Pts',(104.840893082569,-4.17009252427013,337.607587275917));
#36615=CARTESIAN_POINT('Ctrl Pts',(104.83311800379,-4.09775357149106,337.723272809814));
#36616=CARTESIAN_POINT('Ctrl Pts',(104.825342925012,-4.02048268832412,337.836128657948));
#36617=CARTESIAN_POINT('Ctrl Pts',(104.817567846234,-3.93852774286272,337.945705735677));
#36618=CARTESIAN_POINT('Ctrl Pts',(104.809802335185,-3.85667364817927,338.055147971836));
#36619=CARTESIAN_POINT('Ctrl Pts',(104.802036824136,-3.77014719185178,338.161319155537));
#36620=CARTESIAN_POINT('Ctrl Pts',(104.794271313087,-3.6792409722076,338.263796704902));
#36621=CARTESIAN_POINT('Ctrl Pts',(104.786513501564,-3.58842488634493,338.366172647478));
#36622=CARTESIAN_POINT('Ctrl Pts',(104.778755690042,-3.49323793679871,338.464861953279));
#36623=CARTESIAN_POINT('Ctrl Pts',(104.77099787852,-3.39401444881945,338.559473132881));
#36624=CARTESIAN_POINT('Ctrl Pts',(104.763245904997,-3.29486562966159,338.65401311457));
#36625=CARTESIAN_POINT('Ctrl Pts',(104.755493931474,-3.19168660005859,338.744480809944));
#36626=CARTESIAN_POINT('Ctrl Pts',(104.747741957951,-3.08484993292376,338.830520063104));
#36627=CARTESIAN_POINT('Ctrl Pts',(104.739993267393,-2.97805851118067,338.916522878589));
#36628=CARTESIAN_POINT('Ctrl Pts',(104.732244576836,-2.86761283657499,338.99810073734));
#36629=CARTESIAN_POINT('Ctrl Pts',(104.724495886278,-2.7539199266321,339.074936576218));
#36630=CARTESIAN_POINT('Ctrl Pts',(104.7167488079,-2.6402506714487,339.151756428758));
#36631=CARTESIAN_POINT('Ctrl Pts',(104.709001729522,-2.52333584842224,339.223836005148));
#36632=CARTESIAN_POINT('Ctrl Pts',(104.701254651145,-2.40361260272703,339.290900781714));
#36633=CARTESIAN_POINT('Ctrl Pts',(104.693507507839,-2.28388835363571,339.357966120347));
#36634=CARTESIAN_POINT('Ctrl Pts',(104.685760364533,-2.16135597594495,339.420016384302));
#36635=CARTESIAN_POINT('Ctrl Pts',(104.678013221227,-2.03647807651427,339.476822545777));
#36636=CARTESIAN_POINT('Ctrl Pts',(104.670264336199,-1.91157210188065,339.533641478483));
#36637=CARTESIAN_POINT('Ctrl Pts',(104.662515451171,-1.78431991191573,339.585213800845));
#36638=CARTESIAN_POINT('Ctrl Pts',(104.654766566143,-1.65520461521616,339.631358412417));
#36639=CARTESIAN_POINT('Ctrl Pts',(104.647009456368,-1.52595227420649,339.677552002357));
#36640=CARTESIAN_POINT('Ctrl Pts',(104.639252346594,-1.39483324483411,339.718306241558));
#36641=CARTESIAN_POINT('Ctrl Pts',(104.631495236819,-1.26234687418126,339.753489605726));
#36642=CARTESIAN_POINT('Ctrl Pts',(104.623733981893,-1.12978970704803,339.788691770758));
#36643=CARTESIAN_POINT('Ctrl Pts',(104.615972726966,-0.995864124176255,
339.81831704464));
#36644=CARTESIAN_POINT('Ctrl Pts',(104.60821147204,-0.861079246236491,339.842285162421));
#36645=CARTESIAN_POINT('Ctrl Pts',(104.600437801636,-0.726078756418496,
339.866291621379));
#36646=CARTESIAN_POINT('Ctrl Pts',(104.592664131231,-0.590216612258507,
339.88462278815));
#36647=CARTESIAN_POINT('Ctrl Pts',(104.584890460826,-0.454007522842867,
339.897250272521));
#36648=CARTESIAN_POINT('Ctrl Pts',(104.577478656649,-0.324138999309171,
339.909289944456));
#36649=CARTESIAN_POINT('Ctrl Pts',(104.570066852472,-0.193955391616291,
339.916144981575));
#36650=CARTESIAN_POINT('Ctrl Pts',(104.562655048295,-0.0639005739877349,
339.917834867006));
#36651=CARTESIAN_POINT('Ctrl Pts',(104.554879969517,0.0725286176657191,
339.919607578757));
#36652=CARTESIAN_POINT('Ctrl Pts',(104.547104890738,0.20924721671919,339.915701619692));
#36653=CARTESIAN_POINT('Ctrl Pts',(104.53932981196,0.345743442668588,339.906082401912));
#36654=CARTESIAN_POINT('Ctrl Pts',(104.531564300911,0.482071701322272,339.896475021192));
#36655=CARTESIAN_POINT('Ctrl Pts',(104.523798789862,0.618177745165577,339.881168397707));
#36656=CARTESIAN_POINT('Ctrl Pts',(104.516033278813,0.753547874336392,339.860179900331));
#36657=CARTESIAN_POINT('Ctrl Pts',(104.508275467291,0.888783783630108,339.839212213111));
#36658=CARTESIAN_POINT('Ctrl Pts',(104.500517655768,1.02328484654803,339.812573922674));
#36659=CARTESIAN_POINT('Ctrl Pts',(104.492759844246,1.15654092870476,339.780334312863));
#36660=CARTESIAN_POINT('Ctrl Pts',(104.485007870723,1.28969673143379,339.74811896438));
#36661=CARTESIAN_POINT('Ctrl Pts',(104.4772558972,1.42160903984659,339.710310778161));
#36662=CARTESIAN_POINT('Ctrl Pts',(104.469503923677,1.55177673426961,339.667030322323));
#36663=CARTESIAN_POINT('Ctrl Pts',(104.46175523312,1.68188930259684,339.623768195784));
#36664=CARTESIAN_POINT('Ctrl Pts',(104.454006542562,1.81025835630819,339.575038532059));
#36665=CARTESIAN_POINT('Ctrl Pts',(104.446257852004,1.93639700970948,339.521012019812));
#36666=CARTESIAN_POINT('Ctrl Pts',(104.438510773626,2.06250941891041,339.466996748233));
#36667=CARTESIAN_POINT('Ctrl Pts',(104.430763695249,2.18639199175782,339.407686973991));
#36668=CARTESIAN_POINT('Ctrl Pts',(104.423016616871,2.30757731110058,339.343301741279));
#36669=CARTESIAN_POINT('Ctrl Pts',(104.415269473565,2.42876364609295,339.278915968956));
#36670=CARTESIAN_POINT('Ctrl Pts',(104.407522330259,2.54725233731143,339.209454836711));
#36671=CARTESIAN_POINT('Ctrl Pts',(104.399775186953,2.66260044727664,339.135183420438));
#36672=CARTESIAN_POINT('Ctrl Pts',(104.392026301925,2.77797448994597,339.060895306373));
#36673=CARTESIAN_POINT('Ctrl Pts',(104.384277416897,2.89020621778648,338.981794967874));
#36674=CARTESIAN_POINT('Ctrl Pts',(104.376528531869,2.99888190178801,338.898190657424));
#36675=CARTESIAN_POINT('Ctrl Pts',(104.368771422094,3.10767293528331,338.814497608495));
#36676=CARTESIAN_POINT('Ctrl Pts',(104.36101431232,3.2129000748831,338.726291276704));
#36677=CARTESIAN_POINT('Ctrl Pts',(104.353257202545,3.31418249364234,338.633920398321));
#36678=CARTESIAN_POINT('Ctrl Pts',(104.345495947619,3.41551903448778,338.541500159894));
#36679=CARTESIAN_POINT('Ctrl Pts',(104.337734692692,3.51290637686259,338.444911215676));
#36680=CARTESIAN_POINT('Ctrl Pts',(104.329973437766,3.60600150984952,338.344538260128));
#36681=CARTESIAN_POINT('Ctrl Pts',(104.322199767362,3.6992455647096,338.244004740564));
#36682=CARTESIAN_POINT('Ctrl Pts',(104.314426096957,3.78818343589915,338.13967541123));
#36683=CARTESIAN_POINT('Ctrl Pts',(104.306652426552,3.87251271086054,338.031967738404));
#36684=CARTESIAN_POINT('Ctrl Pts',(104.299240622375,3.95291643778421,337.929273883661));
#36685=CARTESIAN_POINT('Ctrl Pts',(104.291828818198,4.02913080480014,337.823509364534));
#36686=CARTESIAN_POINT('Ctrl Pts',(104.284417014021,4.10093198987428,337.715057987765));
#36687=CARTESIAN_POINT('Ctrl Pts',(104.276641935242,4.17625236491337,337.60129108596));
#36688=CARTESIAN_POINT('Ctrl Pts',(104.268866856464,4.24695403946529,337.484207760679));
#36689=CARTESIAN_POINT('Ctrl Pts',(104.261091777686,4.31273097402997,337.364219661568));
#36690=CARTESIAN_POINT('Ctrl Pts',(104.253326266637,4.37842696588925,337.24437921545));
#36691=CARTESIAN_POINT('Ctrl Pts',(104.245560755588,4.4392100897353,337.121641447226));
#36692=CARTESIAN_POINT('Ctrl Pts',(104.237795244539,4.49481695895252,336.996447737361));
#36693=CARTESIAN_POINT('Ctrl Pts',(104.230037433016,4.55036869379697,336.871378157424));
#36694=CARTESIAN_POINT('Ctrl Pts',(104.222279621494,4.60075422987901,336.743857836701));
#36695=CARTESIAN_POINT('Ctrl Pts',(104.214521809972,4.64575576647428,336.614353251544));
#36696=CARTESIAN_POINT('Ctrl Pts',(104.206769836449,4.69072343798624,336.484946122694));
#36697=CARTESIAN_POINT('Ctrl Pts',(104.199017862926,4.73031504680062,336.353558069327));
#36698=CARTESIAN_POINT('Ctrl Pts',(104.191265889403,4.76436079661151,336.220675739995));
#36699=CARTESIAN_POINT('Ctrl Pts',(104.183517198845,4.79839212802707,336.087849686408));
#36700=CARTESIAN_POINT('Ctrl Pts',(104.175768508288,4.82688217497702,335.953530993359));
#36701=CARTESIAN_POINT('Ctrl Pts',(104.16801981773,4.84971099141352,335.818221462847));
#36702=CARTESIAN_POINT('Ctrl Pts',(104.160272739352,4.87253505812408,335.682940084612));
#36703=CARTESIAN_POINT('Ctrl Pts',(104.152525660974,4.88970017219383,335.54666866415));
#36704=CARTESIAN_POINT('Ctrl Pts',(104.144778582596,4.90113758631536,335.409918799894));
#36705=CARTESIAN_POINT('Ctrl Pts',(104.137031439291,4.91257509629344,335.273167789543));
#36706=CARTESIAN_POINT('Ctrl Pts',(104.129284295985,4.91828477799844,335.135938716916));
#36707=CARTESIAN_POINT('Ctrl Pts',(104.121537152679,4.91824984051819,334.998747505363));
#36708=CARTESIAN_POINT('Ctrl Pts',(104.113788267651,4.91821489518325,334.861525450314));
#36709=CARTESIAN_POINT('Ctrl Pts',(104.106039382623,4.91243276079728,334.724341664076));
#36710=CARTESIAN_POINT('Ctrl Pts',(104.098290497595,4.90093876094261,334.587710873306));
#36711=CARTESIAN_POINT('Ctrl Pts',(104.09053338782,4.88943256123775,334.450935061203));
#36712=CARTESIAN_POINT('Ctrl Pts',(104.082776278045,4.8722024182041,334.314713807181));
#36713=CARTESIAN_POINT('Ctrl Pts',(104.07501916827,4.84933550430027,334.179556077947));
#36714=CARTESIAN_POINT('Ctrl Pts',(104.067257913344,4.82645637104883,334.044326124746));
#36715=CARTESIAN_POINT('Ctrl Pts',(104.059496658418,4.79793454626403,333.910161210886));
#36716=CARTESIAN_POINT('Ctrl Pts',(104.051735403492,4.76390790483787,333.777557961814));
#36717=CARTESIAN_POINT('Ctrl Pts',(104.043961733087,4.72982683187461,333.644742590759));
#36718=CARTESIAN_POINT('Ctrl Pts',(104.036188062683,4.69022345842358,333.513494250952));
#36719=CARTESIAN_POINT('Ctrl Pts',(104.028414392278,4.64528518799639,333.384293162519));
#36720=CARTESIAN_POINT('Ctrl Pts',(104.021002588101,4.60243880486978,333.26110641584));
#36721=CARTESIAN_POINT('Ctrl Pts',(104.013590783924,4.55474313152118,333.139780878589));
#36722=CARTESIAN_POINT('Ctrl Pts',(104.006178979747,4.50239979628299,333.020712467343));
#36723=CARTESIAN_POINT('Ctrl Pts',(103.998403900969,4.44749095826124,332.895808158573));
#36724=CARTESIAN_POINT('Ctrl Pts',(103.99062882219,4.38729382513031,332.772993106539));
#36725=CARTESIAN_POINT('Ctrl Pts',(103.982853743412,4.32198894632623,332.652747433629));
#36726=CARTESIAN_POINT('Ctrl Pts',(103.975088232363,4.25676442933307,332.532649730675));
#36727=CARTESIAN_POINT('Ctrl Pts',(103.967322721314,4.1864448575858,332.415115456004));
#36728=CARTESIAN_POINT('Ctrl Pts',(103.959557210265,4.11125886372488,332.300604953338));
#36729=CARTESIAN_POINT('Ctrl Pts',(103.951799398742,4.03614741699566,332.186207988168));
#36730=CARTESIAN_POINT('Ctrl Pts',(103.94404158722,3.95617936346873,332.074829153291));
#36731=CARTESIAN_POINT('Ctrl Pts',(103.936283775698,3.87162910859075,331.966904039102));
#36732=CARTESIAN_POINT('Ctrl Pts',(103.928531802175,3.7871424804607,331.859060141985));
#36733=CARTESIAN_POINT('Ctrl Pts',(103.920779828652,3.69808075463874,331.754665098761));
#36734=CARTESIAN_POINT('Ctrl Pts',(103.913027855129,3.60476127775036,331.654125048223));
#36735=CARTESIAN_POINT('Ctrl Pts',(103.905279164571,3.51148132171605,331.553627576455));
#36736=CARTESIAN_POINT('Ctrl Pts',(103.897530474014,3.41394746633127,331.456982136153));
#36737=CARTESIAN_POINT('Ctrl Pts',(103.889781783456,3.31251677791223,331.364561146361));
#36738=CARTESIAN_POINT('Ctrl Pts',(103.882034705078,3.21110719299501,331.272159385527));
#36739=CARTESIAN_POINT('Ctrl Pts',(103.874287626701,3.10580267646215,331.183980590039));
#36740=CARTESIAN_POINT('Ctrl Pts',(103.866540548323,2.99699623923926,331.100359426244));
#36741=CARTESIAN_POINT('Ctrl Pts',(103.858793405017,2.88818889011371,331.016737561622));
#36742=CARTESIAN_POINT('Ctrl Pts',(103.851046261711,2.77587987167948,330.937673643065));
#36743=CARTESIAN_POINT('Ctrl Pts',(103.843299118405,2.6604939483639,330.863460986136));
#36744=CARTESIAN_POINT('Ctrl Pts',(103.835550233377,2.54508208384367,330.789231644627));
#36745=CARTESIAN_POINT('Ctrl Pts',(103.827801348349,2.42659226661401,330.719855946451));
#36746=CARTESIAN_POINT('Ctrl Pts',(103.820052463321,2.30547645691958,330.655582735384));
#36747=CARTESIAN_POINT('Ctrl Pts',(103.812295353546,2.18423209365288,330.591241304067));
#36748=CARTESIAN_POINT('Ctrl Pts',(103.804538243772,2.06035651593169,330.532013362007));
#36749=CARTESIAN_POINT('Ctrl Pts',(103.796781133997,1.93432489873964,330.478101035116));
#36750=CARTESIAN_POINT('Ctrl Pts',(103.789019879071,1.80822593428116,330.424159899202));
#36751=CARTESIAN_POINT('Ctrl Pts',(103.781258624145,1.67996899996075,330.375540176879));
#36752=CARTESIAN_POINT('Ctrl Pts',(103.773497369218,1.55004633072628,330.332394678735));
#36753=CARTESIAN_POINT('Ctrl Pts',(103.765723698814,1.41991582756264,330.289180161855));
#36754=CARTESIAN_POINT('Ctrl Pts',(103.757950028409,1.2881146407426,330.251457475793));
#36755=CARTESIAN_POINT('Ctrl Pts',(103.750176358004,1.15514801241047,330.219328903603));
#36756=CARTESIAN_POINT('Ctrl Pts',(103.742764553827,1.02837101261596,330.188695924179));
#36757=CARTESIAN_POINT('Ctrl Pts',(103.73535274965,0.900534914346303,330.163148023575));
#36758=CARTESIAN_POINT('Ctrl Pts',(103.727940945473,0.772081764955789,330.142729901403));
#36759=CARTESIAN_POINT('Ctrl Pts',(103.720165866695,0.637332744072424,330.121311026241));
#36760=CARTESIAN_POINT('Ctrl Pts',(103.712390787916,0.501478823824455,330.105469807959));
#36761=CARTESIAN_POINT('Ctrl Pts',(103.704615709138,0.365021455031457,330.095314240457));
#36762=CARTESIAN_POINT('Ctrl Pts',(103.696850198089,0.228732005718524,330.085171170027));
#36763=CARTESIAN_POINT('Ctrl Pts',(103.68908468704,0.0918409714555158,330.080699857972));
#36764=CARTESIAN_POINT('Ctrl Pts',(103.681319175991,-0.045140808660564,
330.081957160628));
#36765=CARTESIAN_POINT('Ctrl Pts',(103.673561364469,-0.181986770943126,
330.083213216666));
#36766=CARTESIAN_POINT('Ctrl Pts',(103.665803552946,-0.318922911683839,
330.090186580452));
#36767=CARTESIAN_POINT('Ctrl Pts',(103.658045741424,-0.455434437093222,
330.10288222155));
#36768=CARTESIAN_POINT('Ctrl Pts',(103.650293767901,-0.591843233250147,
330.115568308776));
#36769=CARTESIAN_POINT('Ctrl Pts',(103.642541794378,-0.727827662469809,
330.133968065993));
#36770=CARTESIAN_POINT('Ctrl Pts',(103.634789820855,-0.862874459509467,
330.158034414659));
#36771=CARTESIAN_POINT('Ctrl Pts',(103.627041130298,-0.997864064151229,
330.182090571212));
#36772=CARTESIAN_POINT('Ctrl Pts',(103.61929243974,-1.13191644238182,330.211808477737));
#36773=CARTESIAN_POINT('Ctrl Pts',(103.611543749183,-1.26452519000914,330.247089406865));
#36774=CARTESIAN_POINT('Ctrl Pts',(103.603796670805,-1.39710634727831,330.282362995502));
#36775=CARTESIAN_POINT('Ctrl Pts',(103.596049592427,-1.5282440938834,330.323197204091));
#36776=CARTESIAN_POINT('Ctrl Pts',(103.588302514049,-1.65744432099134,330.369442648523));
#36777=CARTESIAN_POINT('Ctrl Pts',(103.580555370743,-1.78664563092163,330.415688480538));
#36778=CARTESIAN_POINT('Ctrl Pts',(103.572808227438,-1.9139090209562,330.467345507128));
#36779=CARTESIAN_POINT('Ctrl Pts',(103.565061084132,-2.03875797137367,330.524215264709));
#36780=CARTESIAN_POINT('Ctrl Pts',(103.557312199104,-2.16363499048649,330.58109780782));
#36781=CARTESIAN_POINT('Ctrl Pts',(103.549563314076,-2.28609613419626,330.643195251938));
#36782=CARTESIAN_POINT('Ctrl Pts',(103.541814429047,-2.40568756284156,330.710262197699));
#36783=CARTESIAN_POINT('Ctrl Pts',(103.534057319273,-2.52540592706458,330.777400329009));
#36784=CARTESIAN_POINT('Ctrl Pts',(103.526300209498,-2.6422481501996,330.849518307137));
#36785=CARTESIAN_POINT('Ctrl Pts',(103.518543099723,-2.75578711580683,330.926325929231));
#36786=CARTESIAN_POINT('Ctrl Pts',(103.510781844797,-2.86938675300669,331.003174594863));
#36787=CARTESIAN_POINT('Ctrl Pts',(103.503020589871,-2.97967930130635,331.084717665626));
#36788=CARTESIAN_POINT('Ctrl Pts',(103.495259334945,-3.08626988244834,331.17062390523));
#36789=CARTESIAN_POINT('Ctrl Pts',(103.48748566454,-3.19303097378257,331.256667566821));
#36790=CARTESIAN_POINT('Ctrl Pts',(103.479711994135,-3.29607797020962,331.347088086718));
#36791=CARTESIAN_POINT('Ctrl Pts',(103.471938323731,-3.39505144421095,331.441515947252));
#36792=CARTESIAN_POINT('Ctrl Pts',(103.464526519554,-3.48941767918654,331.531548168161));
#36793=CARTESIAN_POINT('Ctrl Pts',(103.457114715376,-3.58008090185183,331.625222835505));
#36794=CARTESIAN_POINT('Ctrl Pts',(103.449702911199,-3.66676430616309,331.722192411756));
#36795=CARTESIAN_POINT('Ctrl Pts',(103.442001504964,-3.75683469853705,331.822950888545));
#36796=CARTESIAN_POINT('Ctrl Pts',(103.434300098729,-3.8429057633272,331.927600371559));
#36797=CARTESIAN_POINT('Ctrl Pts',(103.426598692494,-3.92461757230766,332.035786786745));
#36798=CARTESIAN_POINT('Ctrl Pts',(103.418909461983,-4.00620019703642,332.143802162014));
#36799=CARTESIAN_POINT('Ctrl Pts',(103.411220231472,-4.0834370496851,332.255343020752));
#36800=CARTESIAN_POINT('Ctrl Pts',(103.40353100096,-4.15600610259396,332.370019707735));
#36801=CARTESIAN_POINT('Ctrl Pts',(103.395848776324,-4.22850903578516,332.484591909544));
#36802=CARTESIAN_POINT('Ctrl Pts',(103.388166551688,-4.29635241396984,332.602293923805));
#36803=CARTESIAN_POINT('Ctrl Pts',(103.380484327052,-4.35925535044355,332.722704267749));
#36804=CARTESIAN_POINT('Ctrl Pts',(103.372807360204,-4.42211523555385,332.843032201717));
#36805=CARTESIAN_POINT('Ctrl Pts',(103.365130393355,-4.48004121993017,332.966064426588));
#36806=CARTESIAN_POINT('Ctrl Pts',(103.357453426506,-4.53279679509627,333.091352238661));
#36807=CARTESIAN_POINT('Ctrl Pts',(103.349779973757,-4.58552822161464,333.216582700753));
#36808=CARTESIAN_POINT('Ctrl Pts',(103.342106521008,-4.63309379327532,333.344066328791));
#36809=CARTESIAN_POINT('Ctrl Pts',(103.334433068259,-4.67530408647686,333.473332137801));
#36810=CARTESIAN_POINT('Ctrl Pts',(103.326759581296,-4.71751456788961,333.602598523193));
#36811=CARTESIAN_POINT('Ctrl Pts',(103.319086094332,-4.75436958686064,333.733646730297));
#36812=CARTESIAN_POINT('Ctrl Pts',(103.311412607368,-4.78572885309172,333.86598835668));
#36813=CARTESIAN_POINT('Ctrl Pts',(103.303739372935,-4.81708708730259,333.998325627756));
#36814=CARTESIAN_POINT('Ctrl Pts',(103.296066138502,-4.84294984225035,334.131955843638));
#36815=CARTESIAN_POINT('Ctrl Pts',(103.28839290407,-4.86322765882695,334.266378980045));
#36816=CARTESIAN_POINT('Ctrl Pts',(103.280714799051,-4.88351834674777,334.400887441538));
#36817=CARTESIAN_POINT('Ctrl Pts',(103.273036694033,-4.89821695898867,334.536189433322));
#36818=CARTESIAN_POINT('Ctrl Pts',(103.265358589015,-4.90728575814236,334.671778199333));
#36819=CARTESIAN_POINT('Ctrl Pts',(103.259084475506,-4.9146962683057,334.782573676389));
#36820=CARTESIAN_POINT('Ctrl Pts',(103.252810361998,-4.9183485878029,334.893560437054));
#36821=CARTESIAN_POINT('Ctrl Pts',(103.24653624849,-4.91824797603409,335.004461920724));
#36822=CARTESIAN_POINT('',(106.746536248459,-4.91824852393639,334.996189580397));
#36823=CARTESIAN_POINT('Ctrl Pts',(106.746536248459,-4.91824852393639,334.996189580397));
#36824=CARTESIAN_POINT('Ctrl Pts',(106.738885073854,-4.9183528630231,335.130863871606));
#36825=CARTESIAN_POINT('Ctrl Pts',(106.731233899249,-4.91292145302669,335.265744929164));
#36826=CARTESIAN_POINT('Ctrl Pts',(106.723582724644,-4.90192995717744,335.400332058954));
#36827=CARTESIAN_POINT('Ctrl Pts',(106.715939142596,-4.89094936861568,335.534785632717));
#36828=CARTESIAN_POINT('Ctrl Pts',(106.708295560548,-4.87441970043182,335.668945459565));
#36829=CARTESIAN_POINT('Ctrl Pts',(106.7006519785,-4.852368651929,335.802310119765));
#36830=CARTESIAN_POINT('Ctrl Pts',(106.692721533071,-4.82949002830698,335.94067995124));
#36831=CARTESIAN_POINT('Ctrl Pts',(106.684791087643,-4.80066747843367,336.078193324683));
#36832=CARTESIAN_POINT('Ctrl Pts',(106.676860642214,-4.76599113994609,336.214294658003));
#36833=CARTESIAN_POINT('Ctrl Pts',(106.66922570775,-4.73260694051098,336.345324468332));
#36834=CARTESIAN_POINT('Ctrl Pts',(106.661590773286,-4.69379749282756,336.47504515645));
#36835=CARTESIAN_POINT('Ctrl Pts',(106.653955838822,-4.64969532675885,336.602971126008));
#36836=CARTESIAN_POINT('Ctrl Pts',(106.646322084699,-4.60559997876458,336.730877318562));
#36837=CARTESIAN_POINT('Ctrl Pts',(106.638688330575,-4.5562136706169,336.856988962874));
#36838=CARTESIAN_POINT('Ctrl Pts',(106.631054576451,-4.50171850167197,336.980836589475));
#36839=CARTESIAN_POINT('Ctrl Pts',(106.623420236805,-4.447219152853,337.104693715404));
#36840=CARTESIAN_POINT('Ctrl Pts',(106.615785897159,-4.38761032693191,337.226286109175));
#36841=CARTESIAN_POINT('Ctrl Pts',(106.608151557513,-4.3231216381909,337.345165743376));
#36842=CARTESIAN_POINT('Ctrl Pts',(106.600514866197,-4.25861308445501,337.464081997075));
#36843=CARTESIAN_POINT('Ctrl Pts',(106.59287817488,-4.18922187160373,337.580283475428));
#36844=CARTESIAN_POINT('Ctrl Pts',(106.585241483564,-4.11522249065059,337.693348643407));
#36845=CARTESIAN_POINT('Ctrl Pts',(106.577596621492,-4.04114393523625,337.806534783665));
#36846=CARTESIAN_POINT('Ctrl Pts',(106.569951759419,-3.96244759290779,337.916577578988));
#36847=CARTESIAN_POINT('Ctrl Pts',(106.562306897347,-3.87945015744457,338.023086095103));
#36848=CARTESIAN_POINT('Ctrl Pts',(106.554657172124,-3.79639992455868,338.129662364818));
#36849=CARTESIAN_POINT('Ctrl Pts',(106.547007446901,-3.70904341289482,338.232699573942));
#36850=CARTESIAN_POINT('Ctrl Pts',(106.539357721678,-3.61773524267658,338.331842549761));
#36851=CARTESIAN_POINT('Ctrl Pts',(106.5316973497,-3.52629999133566,338.431123511048));
#36852=CARTESIAN_POINT('Ctrl Pts',(106.524036977723,-3.43090239176658,338.526499141421));
#36853=CARTESIAN_POINT('Ctrl Pts',(106.516376605745,-3.33193141217521,338.617653400626));
#36854=CARTESIAN_POINT('Ctrl Pts',(106.514358166568,-3.30585344843455,338.641671728788));
#36855=CARTESIAN_POINT('Ctrl Pts',(106.51233972739,-3.27952755584444,338.665397207074));
#36856=CARTESIAN_POINT('Ctrl Pts',(106.510321288212,-3.25296118483706,338.688824554305));
#36857=CARTESIAN_POINT('Ctrl Pts',(106.502546209434,-3.15062685159784,338.779067288543));
#36858=CARTESIAN_POINT('Ctrl Pts',(106.494771130655,-3.04437273219843,338.865191001619));
#36859=CARTESIAN_POINT('Ctrl Pts',(106.486996051877,-2.93456450411663,338.946835977549));
#36860=CARTESIAN_POINT('Ctrl Pts',(106.479230540828,-2.82489140205007,339.028380484139));
#36861=CARTESIAN_POINT('Ctrl Pts',(106.471465029779,-2.7116732040988,339.105456988639));
#36862=CARTESIAN_POINT('Ctrl Pts',(106.46369951873,-2.59531089901102,339.177743936621));
#36863=CARTESIAN_POINT('Ctrl Pts',(106.455941707208,-2.47906396748767,339.249959211884));
#36864=CARTESIAN_POINT('Ctrl Pts',(106.448183895685,-2.35967946249722,339.317394176195));
#36865=CARTESIAN_POINT('Ctrl Pts',(106.440426084163,-2.23758949625525,339.379768978924));
#36866=CARTESIAN_POINT('Ctrl Pts',(106.43267411064,-2.11559140658456,339.442096842637));
#36867=CARTESIAN_POINT('Ctrl Pts',(106.424922137117,-1.99089225478948,339.499371947155));
#36868=CARTESIAN_POINT('Ctrl Pts',(106.417170163594,-1.86395073202679,339.551359217978));
#36869=CARTESIAN_POINT('Ctrl Pts',(106.409421473037,-1.73706296907437,339.603324472161));
#36870=CARTESIAN_POINT('Ctrl Pts',(106.401672782479,-1.60793508489533,339.650006198831));
#36871=CARTESIAN_POINT('Ctrl Pts',(106.393924091921,-1.47704763217791,339.691216617763));
#36872=CARTESIAN_POINT('Ctrl Pts',(106.386177013543,-1.34618741168822,339.732418462523));
#36873=CARTESIAN_POINT('Ctrl Pts',(106.378429935166,-1.21356872344179,339.768151146493));
#36874=CARTESIAN_POINT('Ctrl Pts',(106.370682856788,-1.07968886084365,339.798276255727));
#36875=CARTESIAN_POINT('Ctrl Pts',(106.362935713482,-0.945807876203221,
339.828401617438));
#36876=CARTESIAN_POINT('Ctrl Pts',(106.355188570176,-0.810666077468183,
339.852919224868));
#36877=CARTESIAN_POINT('Ctrl Pts',(106.34744142687,-0.674772183311245,339.871741532874));
#36878=CARTESIAN_POINT('Ctrl Pts',(106.339692541842,-0.538847737321976,
339.890568072535));
#36879=CARTESIAN_POINT('Ctrl Pts',(106.331943656814,-0.402171246548947,
339.903696711254));
#36880=CARTESIAN_POINT('Ctrl Pts',(106.324194771786,-0.265257407458893,
339.911091688239));
#36881=CARTESIAN_POINT('Ctrl Pts',(106.316437662011,-0.12819824660535,339.918494514328));
#36882=CARTESIAN_POINT('Ctrl Pts',(106.308680552237,0.00909837488508905,
339.920151500675));
#36883=CARTESIAN_POINT('Ctrl Pts',(106.300923442462,0.146116339203136,339.916079034954));
#36884=CARTESIAN_POINT('Ctrl Pts',(106.293162187536,0.283207521540329,339.912004393038));
#36885=CARTESIAN_POINT('Ctrl Pts',(106.285400932609,0.420019360322044,339.90219422641));
#36886=CARTESIAN_POINT('Ctrl Pts',(106.277639677683,0.556040992825429,339.886716840251));
#36887=CARTESIAN_POINT('Ctrl Pts',(106.269866007279,0.69228021561138,339.871214695319));
#36888=CARTESIAN_POINT('Ctrl Pts',(106.262092336874,0.827726319746574,339.850027275336));
#36889=CARTESIAN_POINT('Ctrl Pts',(106.254318666469,0.961877884416177,339.82327419892));
#36890=CARTESIAN_POINT('Ctrl Pts',(106.246906862292,1.08978466147432,339.797766484649));
#36891=CARTESIAN_POINT('Ctrl Pts',(106.239495058115,1.21651442865383,339.767199683114));
#36892=CARTESIAN_POINT('Ctrl Pts',(106.232083253938,1.34164731334559,339.731719090256));
#36893=CARTESIAN_POINT('Ctrl Pts',(106.22430817516,1.47291333346866,339.694499487851));
#36894=CARTESIAN_POINT('Ctrl Pts',(106.216533096381,1.60283680203027,339.651754614939));
#36895=CARTESIAN_POINT('Ctrl Pts',(106.208758017603,1.73091733711911,339.603597314553));
#36896=CARTESIAN_POINT('Ctrl Pts',(106.200992506554,1.8588402609556,339.555499274791));
#36897=CARTESIAN_POINT('Ctrl Pts',(106.193226995505,1.98492440131458,339.502002195963));
#36898=CARTESIAN_POINT('Ctrl Pts',(106.185461484456,2.10868235819741,339.443269266512));
#36899=CARTESIAN_POINT('Ctrl Pts',(106.177703672934,2.23231760870585,339.38459457093));
#36900=CARTESIAN_POINT('Ctrl Pts',(106.169945861412,2.35363091478896,339.320694522333));
#36901=CARTESIAN_POINT('Ctrl Pts',(106.16218804989,2.47215310336668,339.251781049868));
#36902=CARTESIAN_POINT('Ctrl Pts',(106.154436076367,2.59058610023871,339.182919436976));
#36903=CARTESIAN_POINT('Ctrl Pts',(106.146684102844,2.70623182381113,339.109052105391));
#36904=CARTESIAN_POINT('Ctrl Pts',(106.138932129321,2.81864437081585,339.030437565993));
#36905=CARTESIAN_POINT('Ctrl Pts',(106.131183438763,2.93100931104025,338.951856319899));
#36906=CARTESIAN_POINT('Ctrl Pts',(106.123434748205,3.04014347839367,338.868532088168));
#36907=CARTESIAN_POINT('Ctrl Pts',(106.115686057648,3.14562890984503,338.780767359154));
#36908=CARTESIAN_POINT('Ctrl Pts',(106.10793897927,3.25109239417135,338.693020890325));
#36909=CARTESIAN_POINT('Ctrl Pts',(106.100191900892,3.35290835231354,338.60083601172));
#36910=CARTESIAN_POINT('Ctrl Pts',(106.092444822514,3.45069127503616,338.504556004245));
#36911=CARTESIAN_POINT('Ctrl Pts',(106.084697679209,3.54847501727372,338.408275189851));
#36912=CARTESIAN_POINT('Ctrl Pts',(106.076950535903,3.64222537815163,338.307899452371));
#36913=CARTESIAN_POINT('Ctrl Pts',(106.069203392597,3.73159344222866,338.203809208492));
#36914=CARTESIAN_POINT('Ctrl Pts',(106.061454507569,3.82098159814384,338.099695562916));
#36915=CARTESIAN_POINT('Ctrl Pts',(106.053705622541,3.9059852421832,337.991866045692));
#36916=CARTESIAN_POINT('Ctrl Pts',(106.045956737513,3.98629577054028,337.880734123843));
#36917=CARTESIAN_POINT('Ctrl Pts',(106.038199627738,4.06669154132203,337.769484245423));
#36918=CARTESIAN_POINT('Ctrl Pts',(106.030442517963,4.14238401645871,337.654925277707));
#36919=CARTESIAN_POINT('Ctrl Pts',(106.022685408189,4.21310767573346,337.537500103483));
#36920=CARTESIAN_POINT('Ctrl Pts',(106.014924153263,4.28386912747032,337.420012181));
#36921=CARTESIAN_POINT('Ctrl Pts',(106.007162898336,4.34965628528845,337.299655342946));
#36922=CARTESIAN_POINT('Ctrl Pts',(105.99940164341,4.41025013133962,337.176896148538));
#36923=CARTESIAN_POINT('Ctrl Pts',(105.991627973006,4.47094090779707,337.053940579425));
#36924=CARTESIAN_POINT('Ctrl Pts',(105.983854302601,4.52642161316247,336.928575332155));
#36925=CARTESIAN_POINT('Ctrl Pts',(105.976080632196,4.57652148971107,336.801286794687));
#36926=CARTESIAN_POINT('Ctrl Pts',(105.968668828019,4.62428920495381,336.679923569259));
#36927=CARTESIAN_POINT('Ctrl Pts',(105.961257023842,4.66716567820311,336.556812354141));
#36928=CARTESIAN_POINT('Ctrl Pts',(105.953845219665,4.70504587475491,336.432384857136));
#36929=CARTESIAN_POINT('Ctrl Pts',(105.946070140886,4.74478269257842,336.301858797854));
#36930=CARTESIAN_POINT('Ctrl Pts',(105.938295062108,4.77914666087071,336.169471677912));
#36931=CARTESIAN_POINT('Ctrl Pts',(105.930519983329,4.80796188638133,336.035705344972));
#36932=CARTESIAN_POINT('Ctrl Pts',(105.92275447228,4.83674165292247,335.902103620022));
#36933=CARTESIAN_POINT('Ctrl Pts',(105.914988961231,4.85998618108075,335.767126437491));
#36934=CARTESIAN_POINT('Ctrl Pts',(105.907223450182,4.87756893939187,335.631271973067));
#36935=CARTESIAN_POINT('Ctrl Pts',(105.89946563866,4.89513426434692,335.49555220874));
#36936=CARTESIAN_POINT('Ctrl Pts',(105.891707827138,4.90704894111149,335.358957278669));
#36937=CARTESIAN_POINT('Ctrl Pts',(105.883950015616,4.91323728895161,335.221996407528));
#36938=CARTESIAN_POINT('Ctrl Pts',(105.876198042093,4.91942097986372,335.085138603787));
#36939=CARTESIAN_POINT('Ctrl Pts',(105.86844606857,4.91988690161919,334.947915796015));
#36940=CARTESIAN_POINT('Ctrl Pts',(105.860694095047,4.91461113768627,334.810842848853));
#36941=CARTESIAN_POINT('Ctrl Pts',(105.852945404489,4.90933760804249,334.673827952165));
#36942=CARTESIAN_POINT('Ctrl Pts',(105.845196713932,4.89832724400769,334.536963179629));
#36943=CARTESIAN_POINT('Ctrl Pts',(105.837448023374,4.88160823071242,334.40076369908));
#36944=CARTESIAN_POINT('Ctrl Pts',(105.829700944996,4.8648926959475,334.26459255597));
#36945=CARTESIAN_POINT('Ctrl Pts',(105.821953866618,4.84247092199935,334.129086817239));
#36946=CARTESIAN_POINT('Ctrl Pts',(105.81420678824,4.81442295993736,333.994756434824));
#36947=CARTESIAN_POINT('Ctrl Pts',(105.806459644935,4.78637476280644,333.860424926591));
#36948=CARTESIAN_POINT('Ctrl Pts',(105.798712501629,4.75270036340273,333.727269176943));
#36949=CARTESIAN_POINT('Ctrl Pts',(105.790965358323,4.7135308440669,333.595788461616));
#36950=CARTESIAN_POINT('Ctrl Pts',(105.783216473295,4.67435251859141,333.464278186633));
#36951=CARTESIAN_POINT('Ctrl Pts',(105.775467588267,4.6296767264136,333.33444406986));
#36952=CARTESIAN_POINT('Ctrl Pts',(105.767718703239,4.57968415754549,333.206769373553));
#36953=CARTESIAN_POINT('Ctrl Pts',(105.759961593464,4.52963852604845,333.078959162005));
#36954=CARTESIAN_POINT('Ctrl Pts',(105.752204483689,4.47426498761729,332.953313314011));
#36955=CARTESIAN_POINT('Ctrl Pts',(105.744447373914,4.41379228361154,332.830294780476));
#36956=CARTESIAN_POINT('Ctrl Pts',(105.736686118988,4.35328726492628,332.707210509769));
#36957=CARTESIAN_POINT('Ctrl Pts',(105.728924864062,4.28767783806774,332.586756694108));
#36958=CARTESIAN_POINT('Ctrl Pts',(105.721163609136,4.21723781950897,332.469369992234));
#36959=CARTESIAN_POINT('Ctrl Pts',(105.713389938731,4.14668511987695,332.351795509895));
#36960=CARTESIAN_POINT('Ctrl Pts',(105.705616268327,4.07128660205224,332.23729827237));
#36961=CARTESIAN_POINT('Ctrl Pts',(105.697842597922,3.99135887324377,332.126285085907));
#36962=CARTESIAN_POINT('Ctrl Pts',(105.690430793745,3.91515179944236,332.020439589985));
#36963=CARTESIAN_POINT('Ctrl Pts',(105.683018989568,3.83482787211581,331.917761306283));
#36964=CARTESIAN_POINT('Ctrl Pts',(105.675607185391,3.75069328326275,331.81857218259));
#36965=CARTESIAN_POINT('Ctrl Pts',(105.667832106613,3.66243500758424,331.714521504474));
#36966=CARTESIAN_POINT('Ctrl Pts',(105.660057027834,3.56970416911645,331.613981843442));
#36967=CARTESIAN_POINT('Ctrl Pts',(105.652281949056,3.47281077790956,331.5173618673));
#36968=CARTESIAN_POINT('Ctrl Pts',(105.644516438007,3.37603662018921,331.42086078819));
#36969=CARTESIAN_POINT('Ctrl Pts',(105.636750926958,3.27511037574467,331.328270070105));
#36970=CARTESIAN_POINT('Ctrl Pts',(105.628985415909,3.17038249770311,331.239965707502));
#36971=CARTESIAN_POINT('Ctrl Pts',(105.621227604386,3.06575845765769,331.151748898932));
#36972=CARTESIAN_POINT('Ctrl Pts',(105.613469792864,2.95734058209763,331.067810238576));
#36973=CARTESIAN_POINT('Ctrl Pts',(105.605711981342,2.84551613372756,330.988488938667));
#36974=CARTESIAN_POINT('Ctrl Pts',(105.597960007819,2.73377583680112,330.909227330552));
#36975=CARTESIAN_POINT('Ctrl Pts',(105.590208034296,2.61863438722192,330.83457639188));
#36976=CARTESIAN_POINT('Ctrl Pts',(105.582456060773,2.5005118030427,330.76483485737));
#36977=CARTESIAN_POINT('Ctrl Pts',(105.574707370216,2.38243924384793,330.695122858443));
#36978=CARTESIAN_POINT('Ctrl Pts',(105.566958679658,2.26138839698723,330.630316326737));
#36979=CARTESIAN_POINT('Ctrl Pts',(105.5592099891,2.1378077306745,330.570670347652));
#36980=CARTESIAN_POINT('Ctrl Pts',(105.551462910722,2.01425277635156,330.511036778411));
#36981=CARTESIAN_POINT('Ctrl Pts',(105.543715832345,1.88816940132079,330.456561795927));
#36982=CARTESIAN_POINT('Ctrl Pts',(105.535968753967,1.76002975527161,330.407454047801));
#36983=CARTESIAN_POINT('Ctrl Pts',(105.528221610661,1.63188903528895,330.358345888105));
#36984=CARTESIAN_POINT('Ctrl Pts',(105.520474467355,1.50169237490352,330.314605192366));
#36985=CARTESIAN_POINT('Ctrl Pts',(105.512727324049,1.36993056190864,330.276391917395));
#36986=CARTESIAN_POINT('Ctrl Pts',(105.504978439021,1.23813912606116,330.238170051269));
#36987=CARTESIAN_POINT('Ctrl Pts',(105.497229553993,1.10478221273518,330.205478187562));
#36988=CARTESIAN_POINT('Ctrl Pts',(105.489480668965,0.970363989204162,330.178425901124));
#36989=CARTESIAN_POINT('Ctrl Pts',(105.481723559191,0.835803092781339,330.151344901109));
#36990=CARTESIAN_POINT('Ctrl Pts',(105.473966449416,0.700179019689055,330.129915513011));
#36991=CARTESIAN_POINT('Ctrl Pts',(105.466209339641,0.564004860293756,330.11419591264));
#36992=CARTESIAN_POINT('Ctrl Pts',(105.458448084715,0.427757933781589,330.098467912217));
#36993=CARTESIAN_POINT('Ctrl Pts',(105.450686829789,0.290960724881314,330.088455807685));
#36994=CARTESIAN_POINT('Ctrl Pts',(105.442925574863,0.154128607051445,330.084165642031));
#36995=CARTESIAN_POINT('Ctrl Pts',(105.435151904458,0.017077602426625,330.079868613511));
#36996=CARTESIAN_POINT('Ctrl Pts',(105.427378234053,-0.120008031660257,
330.081311810631));
#36997=CARTESIAN_POINT('Ctrl Pts',(105.419604563649,-0.256614868829094,
330.088449137839));
#36998=CARTESIAN_POINT('Ctrl Pts',(105.412192759471,-0.38686262486442,330.095254220748));
#36999=CARTESIAN_POINT('Ctrl Pts',(105.404780955294,-0.516674870241541,
330.107235213883));
#37000=CARTESIAN_POINT('Ctrl Pts',(105.397369151117,-0.645615174136864,
330.124308858282));
#37001=CARTESIAN_POINT('Ctrl Pts',(105.389594072339,-0.780875226417314,
330.142219332853));
#37002=CARTESIAN_POINT('Ctrl Pts',(105.38181899356,-0.915603149888324,330.165790893697));
#37003=CARTESIAN_POINT('Ctrl Pts',(105.374043914782,-1.04928752284639,330.194984000349));
#37004=CARTESIAN_POINT('Ctrl Pts',(105.366278403733,-1.18280738867303,330.224141183026));
#37005=CARTESIAN_POINT('Ctrl Pts',(105.358512892684,-1.31528588086312,330.258906064736));
#37006=CARTESIAN_POINT('Ctrl Pts',(105.350747381635,-1.44621716736012,330.299187414145));
#37007=CARTESIAN_POINT('Ctrl Pts',(105.342989570112,-1.57701863510466,330.339428824478));
#37008=CARTESIAN_POINT('Ctrl Pts',(105.33523175859,-1.70627557883314,330.385175703513));
#37009=CARTESIAN_POINT('Ctrl Pts',(105.327473947068,-1.8334931776704,330.436285960981));
#37010=CARTESIAN_POINT('Ctrl Pts',(105.319721973545,-1.96061504122989,330.48735775636));
#37011=CARTESIAN_POINT('Ctrl Pts',(105.311970000022,-2.08570025334977,330.543784751361));
#37012=CARTESIAN_POINT('Ctrl Pts',(105.304218026499,-2.20827030576032,330.60537540634));
#37013=CARTESIAN_POINT('Ctrl Pts',(105.296469335941,-2.33078844968148,330.666939977642));
#37014=CARTESIAN_POINT('Ctrl Pts',(105.288720645384,-2.45079320391194,330.73366368437));
#37015=CARTESIAN_POINT('Ctrl Pts',(105.280971954826,-2.56782736981495,330.805307441382));
#37016=CARTESIAN_POINT('Ctrl Pts',(105.273224876448,-2.68483718578234,330.876936292311));
#37017=CARTESIAN_POINT('Ctrl Pts',(105.265477798071,-2.798877309618,330.95348295345));
#37018=CARTESIAN_POINT('Ctrl Pts',(105.257730719693,-2.90951677781358,331.034663295239));
#37019=CARTESIAN_POINT('Ctrl Pts',(105.249983576387,-3.02015717327394,331.115844317398));
#37020=CARTESIAN_POINT('Ctrl Pts',(105.242236433081,-3.12739654110512,331.201658866435));
#37021=CARTESIAN_POINT('Ctrl Pts',(105.234489289775,-3.23083477677504,331.291780790234));
#37022=CARTESIAN_POINT('Ctrl Pts',(105.226740404747,-3.33429626755688,331.381922975354));
#37023=CARTESIAN_POINT('Ctrl Pts',(105.218991519719,-3.43395463101785,331.476374205505));
#37024=CARTESIAN_POINT('Ctrl Pts',(105.211242634691,-3.5294448894884,331.574769812908));
#37025=CARTESIAN_POINT('Ctrl Pts',(105.203485524916,-3.62503650230577,331.673269858426));
#37026=CARTESIAN_POINT('Ctrl Pts',(105.195728415141,-3.71645089999087,331.775722363384));
#37027=CARTESIAN_POINT('Ctrl Pts',(105.187971305367,-3.80336149862639,331.881727341417));
#37028=CARTESIAN_POINT('Ctrl Pts',(105.18021005044,-3.8903185395069,331.98778896512));
#37029=CARTESIAN_POINT('Ctrl Pts',(105.172448795514,-3.97276675096495,332.097406532268));
#37030=CARTESIAN_POINT('Ctrl Pts',(105.164687540588,-4.05042215317255,332.210149924532));
#37031=CARTESIAN_POINT('Ctrl Pts',(105.156913870183,-4.12820177871589,332.32307366948));
#37032=CARTESIAN_POINT('Ctrl Pts',(105.149140199779,-4.20117306604447,332.43913290055));
#37033=CARTESIAN_POINT('Ctrl Pts',(105.141366529374,-4.26909693341785,332.557870921597));
#37034=CARTESIAN_POINT('Ctrl Pts',(105.133954725197,-4.33385892842347,332.671081659197));
#37035=CARTESIAN_POINT('Ctrl Pts',(105.12654292102,-4.39403271029031,332.78672714861));
#37036=CARTESIAN_POINT('Ctrl Pts',(105.119131116843,-4.44945211549495,332.904395329644));
#37037=CARTESIAN_POINT('Ctrl Pts',(105.110702461519,-4.51247470130265,333.03820681695));
#37038=CARTESIAN_POINT('Ctrl Pts',(105.102273806194,-4.56952356562858,333.175004286875));
#37039=CARTESIAN_POINT('Ctrl Pts',(105.09384515087,-4.62032959520875,333.314254617643));
#37040=CARTESIAN_POINT('Ctrl Pts',(105.085444938978,-4.67096417420701,333.453035032725));
#37041=CARTESIAN_POINT('Ctrl Pts',(105.077044727086,-4.7153978376093,333.594251532157));
#37042=CARTESIAN_POINT('Ctrl Pts',(105.068644515194,-4.753409471131,333.737351409828));
#37043=CARTESIAN_POINT('Ctrl Pts',(105.060261676269,-4.79134249058272,333.88015533432));
#37044=CARTESIAN_POINT('Ctrl Pts',(105.051878837344,-4.82287988160151,334.02483459894));
#37045=CARTESIAN_POINT('Ctrl Pts',(105.043495998419,-4.84784917077349,334.170818789449));
#37046=CARTESIAN_POINT('Ctrl Pts',(105.035140929155,-4.87273574468608,334.316319381081));
#37047=CARTESIAN_POINT('Ctrl Pts',(105.026785859891,-4.8910975567269,334.463115997978));
#37048=CARTESIAN_POINT('Ctrl Pts',(105.018430790627,-4.90281261842756,334.610626797163));
#37049=CARTESIAN_POINT('Ctrl Pts',(105.011132609926,-4.91304576366047,334.739477969274));
#37050=CARTESIAN_POINT('Ctrl Pts',(105.003834429225,-4.9182080748459,334.868873698525));
#37051=CARTESIAN_POINT('Ctrl Pts',(104.996536248525,-4.91824974554793,334.998417938773));
#37052=CARTESIAN_POINT('',(108.496536248524,-4.9182486817404,335.003600980256));
#37053=CARTESIAN_POINT('Ctrl Pts',(108.49653624849,-4.91824868173996,335.003600980854));
#37054=CARTESIAN_POINT('Ctrl Pts',(108.483686675037,-4.91808315126232,335.22968384175));
#37055=CARTESIAN_POINT('Ctrl Pts',(108.470837101584,-4.9023277300516,335.455205193581));
#37056=CARTESIAN_POINT('Ctrl Pts',(108.45798752813,-4.87121828787386,335.678539206224));
#37057=CARTESIAN_POINT('Ctrl Pts',(108.450212449352,-4.85239444406579,335.813675173851));
#37058=CARTESIAN_POINT('Ctrl Pts',(108.442437370574,-4.82791323807937,335.948240780144));
#37059=CARTESIAN_POINT('Ctrl Pts',(108.434662291795,-4.79781766449557,336.081724882192));
#37060=CARTESIAN_POINT('Ctrl Pts',(108.426896780746,-4.76775912543104,336.215044723556));
#37061=CARTESIAN_POINT('Ctrl Pts',(108.419131269697,-4.73210005052074,336.347285331047));
#37062=CARTESIAN_POINT('Ctrl Pts',(108.411365758648,-4.69093508627443,336.477941500486));
#37063=CARTESIAN_POINT('Ctrl Pts',(108.403607947126,-4.64981093720996,336.608468123953));
#37064=CARTESIAN_POINT('Ctrl Pts',(108.395850135604,-4.60319187943937,336.737413065289));
#37065=CARTESIAN_POINT('Ctrl Pts',(108.388092324081,-4.55122334285371,336.864282474831));
#37066=CARTESIAN_POINT('Ctrl Pts',(108.380340350558,-4.49929391423994,336.99105641112));
#37067=CARTESIAN_POINT('Ctrl Pts',(108.372588377035,-4.44202316724143,337.115757564259));
#37068=CARTESIAN_POINT('Ctrl Pts',(108.364836403512,-4.3796058697932,337.237908730885));
#37069=CARTESIAN_POINT('Ctrl Pts',(108.357087712955,-4.31721500610749,337.36000816642));
#37070=CARTESIAN_POINT('Ctrl Pts',(108.349339022397,-4.24968210446359,337.479559415987));
#37071=CARTESIAN_POINT('Ctrl Pts',(108.341590331839,-4.17724933325099,337.596106906573));
#37072=CARTESIAN_POINT('Ctrl Pts',(108.333843253462,-4.10483163228136,337.71263014848));
#37073=CARTESIAN_POINT('Ctrl Pts',(108.326096175084,-4.02751629571281,337.826150542714));
#37074=CARTESIAN_POINT('Ctrl Pts',(108.318349096706,-3.94559035808407,337.9362390551));
#37075=CARTESIAN_POINT('Ctrl Pts',(108.3106019534,-3.86366373383718,338.046328490133));
#37076=CARTESIAN_POINT('Ctrl Pts',(108.302854810094,-3.77712666481263,338.152985672376));
#37077=CARTESIAN_POINT('Ctrl Pts',(108.295107666788,-3.68630799867523,338.255812709817));
#37078=CARTESIAN_POINT('Ctrl Pts',(108.28735878176,-3.59546891457343,338.358662864958));
#37079=CARTESIAN_POINT('Ctrl Pts',(108.279609896732,-3.50034657660713,338.4576808689));
#37080=CARTESIAN_POINT('Ctrl Pts',(108.271861011704,-3.40130810991624,338.55250421589));
#37081=CARTESIAN_POINT('Ctrl Pts',(108.264103901929,-3.30216452277361,338.647428209361));
#37082=CARTESIAN_POINT('Ctrl Pts',(108.256346792155,-3.19909678644762,338.738148381346));
#37083=CARTESIAN_POINT('Ctrl Pts',(108.24858968238,-3.0925070844845,338.824340857574));
#37084=CARTESIAN_POINT('Ctrl Pts',(108.240828427454,-2.98586042439274,338.910579392306));
#37085=CARTESIAN_POINT('Ctrl Pts',(108.233067172527,-2.87568836235641,338.992285177577));
#37086=CARTESIAN_POINT('Ctrl Pts',(108.225305917601,-2.76242292537484,339.069177145795));
#37087=CARTESIAN_POINT('Ctrl Pts',(108.217532247197,-2.64897630060723,339.146192116104));
#37088=CARTESIAN_POINT('Ctrl Pts',(108.209758576792,-2.53242674501801,339.218377675484));
#37089=CARTESIAN_POINT('Ctrl Pts',(108.201984906387,-2.41323255949811,339.285497832957));
#37090=CARTESIAN_POINT('Ctrl Pts',(108.19457310221,-2.29958689199112,339.349493530951));
#37091=CARTESIAN_POINT('Ctrl Pts',(108.187161298033,-2.18353752487874,339.408884672028));
#37092=CARTESIAN_POINT('Ctrl Pts',(108.179749493856,-2.06549763150288,339.463507880217));
#37093=CARTESIAN_POINT('Ctrl Pts',(108.171974415078,-1.94167225132945,339.520808334552));
#37094=CARTESIAN_POINT('Ctrl Pts',(108.164199336299,-1.81526497687633,339.573042737093));
#37095=CARTESIAN_POINT('Ctrl Pts',(108.156424257521,-1.68672890595508,339.61997063414));
#37096=CARTESIAN_POINT('Ctrl Pts',(108.148658746472,-1.55835100685203,339.666840783422));
#37097=CARTESIAN_POINT('Ctrl Pts',(108.140893235423,-1.42784988723146,339.708417287256));
#37098=CARTESIAN_POINT('Ctrl Pts',(108.133127724374,-1.29570160272429,339.744506340938));
#37099=CARTESIAN_POINT('Ctrl Pts',(108.125369912851,-1.16368434362604,339.780559612218));
#37100=CARTESIAN_POINT('Ctrl Pts',(108.117612101329,-1.03002354437659,339.811136158581));
#37101=CARTESIAN_POINT('Ctrl Pts',(108.109854289807,-0.895213194151686,
339.836091024734));
#37102=CARTESIAN_POINT('Ctrl Pts',(108.102102316284,-0.760504292990412,
339.86102711156));
#37103=CARTESIAN_POINT('Ctrl Pts',(108.094350342761,-0.624647945537534,
339.880349867905));
#37104=CARTESIAN_POINT('Ctrl Pts',(108.086598369238,-0.488150842387499,
339.893964836161));
#37105=CARTESIAN_POINT('Ctrl Pts',(108.07884967868,-0.351711545841687,339.907574038469));
#37106=CARTESIAN_POINT('Ctrl Pts',(108.071100988123,-0.214632421450255,
339.915480221715));
#37107=CARTESIAN_POINT('Ctrl Pts',(108.063352297565,-0.0774276214902788,
339.917640493766));
#37108=CARTESIAN_POINT('Ctrl Pts',(108.055605219187,0.0597486318650154,
339.919800316355));
#37109=CARTESIAN_POINT('Ctrl Pts',(108.047858140809,0.197050118198452,339.916216599503));
#37110=CARTESIAN_POINT('Ctrl Pts',(108.040111062432,0.333960722659175,339.906898541668));
#37111=CARTESIAN_POINT('Ctrl Pts',(108.032363919126,0.470872474562539,339.897580405738));
#37112=CARTESIAN_POINT('Ctrl Pts',(108.02461677582,0.607392948086891,339.882527859507));
#37113=CARTESIAN_POINT('Ctrl Pts',(108.016869632514,0.743009589010084,339.861802115794));
#37114=CARTESIAN_POINT('Ctrl Pts',(108.009120747486,0.878656719433565,339.841071712494));
#37115=CARTESIAN_POINT('Ctrl Pts',(108.001371862458,1.01339922659645,339.814665632736));
#37116=CARTESIAN_POINT('Ctrl Pts',(107.99362297743,1.14673359920081,339.782696427222));
#37117=CARTESIAN_POINT('Ctrl Pts',(107.985865867655,1.28020949428575,339.750693289263));
#37118=CARTESIAN_POINT('Ctrl Pts',(107.97810875788,1.4122738884897,339.713115321516));
#37119=CARTESIAN_POINT('Ctrl Pts',(107.970351648106,1.54243678443367,339.670125461754));
#37120=CARTESIAN_POINT('Ctrl Pts',(107.96259039318,1.67266923526742,339.627112629586));
#37121=CARTESIAN_POINT('Ctrl Pts',(107.954829138253,1.80099779765773,339.578682280889));
#37122=CARTESIAN_POINT('Ctrl Pts',(107.947067883327,1.92695232127111,339.525045614582));
#37123=CARTESIAN_POINT('Ctrl Pts',(107.939294212923,2.05310833107378,339.471323147089));
#37124=CARTESIAN_POINT('Ctrl Pts',(107.931520542518,2.17688236010878,339.412377887506));
#37125=CARTESIAN_POINT('Ctrl Pts',(107.923746872113,2.29782794561957,339.348467522568));
#37126=CARTESIAN_POINT('Ctrl Pts',(107.916335067936,2.41314348502651,339.287532200495));
#37127=CARTESIAN_POINT('Ctrl Pts',(107.908923263759,2.52588773406848,339.222083766185));
#37128=CARTESIAN_POINT('Ctrl Pts',(107.901511459582,2.63569971460231,339.152381253804));
#37129=CARTESIAN_POINT('Ctrl Pts',(107.893736380804,2.7508939074156,339.079262413658));
#37130=CARTESIAN_POINT('Ctrl Pts',(107.885961302025,2.86322516033814,339.001230872214));
#37131=CARTESIAN_POINT('Ctrl Pts',(107.878186223247,2.97224607350173,338.918537525794));
#37132=CARTESIAN_POINT('Ctrl Pts',(107.870420712198,3.08113282949107,338.835945938801));
#37133=CARTESIAN_POINT('Ctrl Pts',(107.862655201149,3.18671704253944,338.748704195076));
#37134=CARTESIAN_POINT('Ctrl Pts',(107.8548896901,3.28857811712067,338.657107741111));
#37135=CARTESIAN_POINT('Ctrl Pts',(107.847131878578,3.39033819614996,338.565602105297));
#37136=CARTESIAN_POINT('Ctrl Pts',(107.839374067055,3.48838219423739,338.469750611398));
#37137=CARTESIAN_POINT('Ctrl Pts',(107.831616255533,3.58232088949783,338.369890221827));
#37138=CARTESIAN_POINT('Ctrl Pts',(107.82386428201,3.67618889291106,338.270104980366));
#37139=CARTESIAN_POINT('Ctrl Pts',(107.816112308487,3.76595747599722,338.166317131623));
#37140=CARTESIAN_POINT('Ctrl Pts',(107.808360334964,3.85127300798222,338.058901646096));
#37141=CARTESIAN_POINT('Ctrl Pts',(107.800611644407,3.93655240878877,337.95153165109));
#37142=CARTESIAN_POINT('Ctrl Pts',(107.792862953849,4.01738226675829,337.840537380346));
#37143=CARTESIAN_POINT('Ctrl Pts',(107.785114263291,4.0934482756819,337.726327984087));
#37144=CARTESIAN_POINT('Ctrl Pts',(107.777367184913,4.16949845843704,337.612142350047));
#37145=CARTESIAN_POINT('Ctrl Pts',(107.769620106536,4.24078654709393,337.494743246168));
#37146=CARTESIAN_POINT('Ctrl Pts',(107.761873028158,4.3070409774704,337.374569662253));
#37147=CARTESIAN_POINT('Ctrl Pts',(107.754125884852,4.37329596312276,337.254395071167));
#37148=CARTESIAN_POINT('Ctrl Pts',(107.746378741546,4.43451701763259,337.131446295963));
#37149=CARTESIAN_POINT('Ctrl Pts',(107.73863159824,4.4904782436648,337.006187480191));
#37150=CARTESIAN_POINT('Ctrl Pts',(107.730882713212,4.5464520509687,336.880900503577));
#37151=CARTESIAN_POINT('Ctrl Pts',(107.723133828184,4.59716351730095,336.753302809761));
#37152=CARTESIAN_POINT('Ctrl Pts',(107.715384943156,4.6424348100919,336.623878719778));
#37153=CARTESIAN_POINT('Ctrl Pts',(107.707627833381,4.68775415430075,336.494317257728));
#37154=CARTESIAN_POINT('Ctrl Pts',(107.699870723607,4.72762166108901,336.362925896601));
#37155=CARTESIAN_POINT('Ctrl Pts',(107.692113613832,4.7619091826073,336.230204860623));
#37156=CARTESIAN_POINT('Ctrl Pts',(107.684352358906,4.79621502628079,336.097412902767));
#37157=CARTESIAN_POINT('Ctrl Pts',(107.67659110398,4.82493486144602,335.96329023627));
#37158=CARTESIAN_POINT('Ctrl Pts',(107.668829849053,4.847991864457,335.828346512432));
#37159=CARTESIAN_POINT('Ctrl Pts',(107.661056178649,4.87108575115853,335.693186922614));
#37160=CARTESIAN_POINT('Ctrl Pts',(107.653282508244,4.88849865409562,335.557204038756));
#37161=CARTESIAN_POINT('Ctrl Pts',(107.645508837839,4.90020566092802,335.420912749996));
#37162=CARTESIAN_POINT('Ctrl Pts',(107.638097033662,4.91136770377592,335.290965853516));
#37163=CARTESIAN_POINT('Ctrl Pts',(107.630685229485,4.91734310150411,335.160738905966));
#37164=CARTESIAN_POINT('Ctrl Pts',(107.623273425308,4.91815433548213,335.03067563982));
#37165=CARTESIAN_POINT('Ctrl Pts',(107.615498346529,4.91900533045394,334.894237585561));
#37166=CARTESIAN_POINT('Ctrl Pts',(107.607723267751,4.91417582904538,334.757548493972));
#37167=CARTESIAN_POINT('Ctrl Pts',(107.599948188973,4.90363470158705,334.621120367542));
#37168=CARTESIAN_POINT('Ctrl Pts',(107.592182677924,4.89310654565713,334.484860124608));
#37169=CARTESIAN_POINT('Ctrl Pts',(107.584417166875,4.87688077823922,334.348860593855));
#37170=CARTESIAN_POINT('Ctrl Pts',(107.576651655826,4.85497823821829,334.213635346085));
#37171=CARTESIAN_POINT('Ctrl Pts',(107.568893844303,4.83309741462955,334.078544174542));
#37172=CARTESIAN_POINT('Ctrl Pts',(107.561136032781,4.80555108163696,333.944226141567));
#37173=CARTESIAN_POINT('Ctrl Pts',(107.553378221259,4.77241196782509,333.811190901843));
#37174=CARTESIAN_POINT('Ctrl Pts',(107.545626247736,4.73929779224731,333.678255775357));
#37175=CARTESIAN_POINT('Ctrl Pts',(107.537874274213,4.70059930725059,333.54660189841));
#37176=CARTESIAN_POINT('Ctrl Pts',(107.53012230069,4.65644046362301,333.416729564719));
#37177=CARTESIAN_POINT('Ctrl Pts',(107.522373610132,4.61230032129189,333.286912232038));
#37178=CARTESIAN_POINT('Ctrl Pts',(107.514624919575,4.56270454522748,333.158875311293));
#37179=CARTESIAN_POINT('Ctrl Pts',(107.506876229017,4.50782710945783,333.033104523942));
#37180=CARTESIAN_POINT('Ctrl Pts',(107.499129150639,4.45296109139705,332.907359904254));
#37181=CARTESIAN_POINT('Ctrl Pts',(107.491382072261,4.39281575562719,332.78388083817));
#37182=CARTESIAN_POINT('Ctrl Pts',(107.483634993883,4.32761329907645,332.663133252375));
#37183=CARTESIAN_POINT('Ctrl Pts',(107.475887850578,4.26241029606638,332.542384654598));
#37184=CARTESIAN_POINT('Ctrl Pts',(107.468140707272,4.19215027345905,332.424367926705));
#37185=CARTESIAN_POINT('Ctrl Pts',(107.460393563966,4.11710129345659,332.30952420529));
#37186=CARTESIAN_POINT('Ctrl Pts',(107.452644678938,4.04203544085009,332.194654664569));
#37187=CARTESIAN_POINT('Ctrl Pts',(107.44489579391,3.96217870219855,332.082959876971));
#37188=CARTESIAN_POINT('Ctrl Pts',(107.437146908882,3.87784211798493,331.974851479599));
#37189=CARTESIAN_POINT('Ctrl Pts',(107.429389799107,3.79341601804948,331.866628334858));
#37190=CARTESIAN_POINT('Ctrl Pts',(107.421632689332,3.70450081488571,331.761999493123));
#37191=CARTESIAN_POINT('Ctrl Pts',(107.413875579558,3.6114478095638,331.661343416687));
#37192=CARTESIAN_POINT('Ctrl Pts',(107.406114324631,3.51834507969104,331.560633552862));
#37193=CARTESIAN_POINT('Ctrl Pts',(107.398353069705,3.42110041880388,331.463900959963));
#37194=CARTESIAN_POINT('Ctrl Pts',(107.390591814779,3.32010082986982,331.371486042193));
#37195=CARTESIAN_POINT('Ctrl Pts',(107.382818144374,3.21893967450923,331.278923290673));
#37196=CARTESIAN_POINT('Ctrl Pts',(107.37504447397,3.11401188733686,331.190692267954));
#37197=CARTESIAN_POINT('Ctrl Pts',(107.367270803565,3.00573696811573,331.10709255941));
#37198=CARTESIAN_POINT('Ctrl Pts',(107.359858999388,2.90250227243516,331.027384437412));
#37199=CARTESIAN_POINT('Ctrl Pts',(107.352447195211,2.79622528455195,330.951886324245));
#37200=CARTESIAN_POINT('Ctrl Pts',(107.345035391034,2.68729131452731,330.880819443947));
#37201=CARTESIAN_POINT('Ctrl Pts',(107.337260312256,2.57301816613274,330.806269364147));
#37202=CARTESIAN_POINT('Ctrl Pts',(107.329485233477,2.45545987255247,330.736360284237));
#37203=CARTESIAN_POINT('Ctrl Pts',(107.321710154699,2.33503014155402,330.671395455746));
#37204=CARTESIAN_POINT('Ctrl Pts',(107.31394464365,2.21474860700649,330.606510570613));
#37205=CARTESIAN_POINT('Ctrl Pts',(107.306179132601,2.09160300638987,330.546558014855));
#37206=CARTESIAN_POINT('Ctrl Pts',(107.298413621552,1.96603648946314,330.491798187237));
#37207=CARTESIAN_POINT('Ctrl Pts',(107.290655810029,1.84059447210359,330.437092654148));
#37208=CARTESIAN_POINT('Ctrl Pts',(107.282897998507,1.71273667123535,330.387569758427));
#37209=CARTESIAN_POINT('Ctrl Pts',(107.275140186985,1.5829310239641,330.343444144448));
#37210=CARTESIAN_POINT('Ctrl Pts',(107.267388213462,1.45322305955879,330.299351736394));
#37211=CARTESIAN_POINT('Ctrl Pts',(107.259636239939,1.32157053497217,330.26064865091));
#37212=CARTESIAN_POINT('Ctrl Pts',(107.251884266416,1.18846123474575,330.227501392771));
#37213=CARTESIAN_POINT('Ctrl Pts',(107.244135575858,1.05540830638701,330.194368172515));
#37214=CARTESIAN_POINT('Ctrl Pts',(107.236386885301,0.920900207950748,330.166786194114));
#37215=CARTESIAN_POINT('Ctrl Pts',(107.228638194743,0.785439540304255,330.14487201085));
#37216=CARTESIAN_POINT('Ctrl Pts',(107.220891116365,0.650007056381056,330.122962387015));
#37217=CARTESIAN_POINT('Ctrl Pts',(107.213144037988,0.513622783076975,330.106718275122));
#37218=CARTESIAN_POINT('Ctrl Pts',(107.20539695961,0.376798771589208,330.0962049647));
#37219=CARTESIAN_POINT('Ctrl Pts',(107.197649816304,0.23997361338444,330.085691566167));
#37220=CARTESIAN_POINT('Ctrl Pts',(107.189902672998,0.102709099370616,330.080909094847));
#37221=CARTESIAN_POINT('Ctrl Pts',(107.182155529692,-0.0344787454392194,
330.081870855842));
#37222=CARTESIAN_POINT('Ctrl Pts',(107.174406644664,-0.171697432989055,
330.082832833062));
#37223=CARTESIAN_POINT('Ctrl Pts',(107.166657759636,-0.308839026247162,
330.089541609647));
#37224=CARTESIAN_POINT('Ctrl Pts',(107.158908874608,-0.445389048938188,
330.101958385478));
#37225=CARTESIAN_POINT('Ctrl Pts',(107.151151764833,-0.582084007234216,
330.114388340604));
#37226=CARTESIAN_POINT('Ctrl Pts',(107.143394655059,-0.718185750792701,
330.132538362002));
#37227=CARTESIAN_POINT('Ctrl Pts',(107.135637545284,-0.853185913430837,
330.156317840772));
#37228=CARTESIAN_POINT('Ctrl Pts',(107.127876290358,-0.988258215839419,
330.180110026535));
#37229=CARTESIAN_POINT('Ctrl Pts',(107.120115035431,-1.12222738281142,330.209537579966));
#37230=CARTESIAN_POINT('Ctrl Pts',(107.112353780505,-1.25459773167696,330.24445927426));
#37231=CARTESIAN_POINT('Ctrl Pts',(107.104580110101,-1.38717982996129,330.279436831884));
#37232=CARTESIAN_POINT('Ctrl Pts',(107.096806439696,-1.51815762568644,330.319925977565));
#37233=CARTESIAN_POINT('Ctrl Pts',(107.089032769291,-1.64705217572689,330.365736067838));
#37234=CARTESIAN_POINT('Ctrl Pts',(107.081620965114,-1.76994665345263,330.409413687388));
#37235=CARTESIAN_POINT('Ctrl Pts',(107.074209160937,-1.89094720381393,330.457927912704));
#37236=CARTESIAN_POINT('Ctrl Pts',(107.06679735676,-2.00965928141386,330.511074445357));
#37237=CARTESIAN_POINT('Ctrl Pts',(107.059022277982,-2.134189791562,330.56682584789));
#37238=CARTESIAN_POINT('Ctrl Pts',(107.051247199203,-2.25659536645293,330.627851310436));
#37239=CARTESIAN_POINT('Ctrl Pts',(107.043472120425,-2.37639711439414,330.693967044111));
#37240=CARTESIAN_POINT('Ctrl Pts',(107.035706609376,-2.49605143865748,330.760001418167));
#37241=CARTESIAN_POINT('Ctrl Pts',(107.027941098327,-2.61310797241295,330.831113412924));
#37242=CARTESIAN_POINT('Ctrl Pts',(107.020175587278,-2.72710792702054,330.907071291009));
#37243=CARTESIAN_POINT('Ctrl Pts',(107.012417775756,-2.84099485034124,330.982953856637));
#37244=CARTESIAN_POINT('Ctrl Pts',(107.004659964234,-2.95183090240648,331.063672528616));
#37245=CARTESIAN_POINT('Ctrl Pts',(106.996902152711,-3.05918235656461,331.148949965038));
#37246=CARTESIAN_POINT('Ctrl Pts',(106.989150179188,-3.16645302534911,331.234163227484));
#37247=CARTESIAN_POINT('Ctrl Pts',(106.981398205665,-3.27024401090058,331.323928183754));
#37248=CARTESIAN_POINT('Ctrl Pts',(106.973646232142,-3.37015132759812,331.417924750708));
#37249=CARTESIAN_POINT('Ctrl Pts',(106.965897541585,-3.47001633348772,331.511881510061));
#37250=CARTESIAN_POINT('Ctrl Pts',(106.958148851027,-3.56600065769723,331.610066048474));
#37251=CARTESIAN_POINT('Ctrl Pts',(106.95040016047,-3.65773430191766,331.712118791824));
#37252=CARTESIAN_POINT('Ctrl Pts',(106.942653082092,-3.74944886018737,331.814150302249));
#37253=CARTESIAN_POINT('Ctrl Pts',(106.934906003714,-3.83691423644332,331.92004812627));
#37254=CARTESIAN_POINT('Ctrl Pts',(106.927158925336,-3.91979842704514,332.029417001019));
#37255=CARTESIAN_POINT('Ctrl Pts',(106.91941178203,-4.00268331229625,332.138786792385));
#37256=CARTESIAN_POINT('Ctrl Pts',(106.911664638725,-4.08098669922714,332.25162738098));
#37257=CARTESIAN_POINT('Ctrl Pts',(106.903917495419,-4.15441814855179,332.367512030515));
#37258=CARTESIAN_POINT('Ctrl Pts',(106.896168610391,-4.2278661068252,332.483422733379));
#37259=CARTESIAN_POINT('Ctrl Pts',(106.888419725363,-4.29643973876372,332.602378528898));
#37260=CARTESIAN_POINT('Ctrl Pts',(106.880670840335,-4.35989325958387,332.723925786022));
#37261=CARTESIAN_POINT('Ctrl Pts',(106.87291373056,-4.42341413062661,332.845602054661));
#37262=CARTESIAN_POINT('Ctrl Pts',(106.865156620785,-4.48180385337479,332.969874932449));
#37263=CARTESIAN_POINT('Ctrl Pts',(106.85739951101,-4.53486351667543,333.096267889742));
#37264=CARTESIAN_POINT('Ctrl Pts',(106.849638256084,-4.58795153336361,333.22272838739));
#37265=CARTESIAN_POINT('Ctrl Pts',(106.841877001158,-4.63570367927216,333.351310855718));
#37266=CARTESIAN_POINT('Ctrl Pts',(106.834115746232,-4.67797047269869,333.481522038665));
#37267=CARTESIAN_POINT('Ctrl Pts',(106.826342075827,-4.72030487921998,333.61194151707));
#37268=CARTESIAN_POINT('Ctrl Pts',(106.818568405423,-4.75713629359026,333.743994539778));
#37269=CARTESIAN_POINT('Ctrl Pts',(106.810794735018,-4.78836584835855,333.877175185181));
#37270=CARTESIAN_POINT('Ctrl Pts',(106.803382930841,-4.81814165983935,334.0041562395));
#37271=CARTESIAN_POINT('Ctrl Pts',(106.795971126664,-4.84282535357643,334.132162014798));
#37272=CARTESIAN_POINT('Ctrl Pts',(106.788559322486,-4.86237521732448,334.26075017183));
#37273=CARTESIAN_POINT('Ctrl Pts',(106.775427117146,-4.89701358862873,334.488582160125));
#37274=CARTESIAN_POINT('Ctrl Pts',(106.762294911805,-4.91564487213602,334.718907368115));
#37275=CARTESIAN_POINT('Ctrl Pts',(106.749162706464,-4.91799551195798,334.949967941666));
#37276=CARTESIAN_POINT('Ctrl Pts',(106.748287220473,-4.91815222228817,334.965372079057));
#37277=CARTESIAN_POINT('Ctrl Pts',(106.747411734481,-4.91823658492966,334.980779468144));
#37278=CARTESIAN_POINT('Ctrl Pts',(106.74653624849,-4.91824852393596,334.996189579852));
#37279=CARTESIAN_POINT('',(110.24653624849,-4.91461063079939,335.001894868956));
#37280=CARTESIAN_POINT('Ctrl Pts',(110.24653624849,-4.9182496344383,335.001896272004));
#37281=CARTESIAN_POINT('Ctrl Pts',(110.238131601278,-4.91819212410279,335.151057460917));
#37282=CARTESIAN_POINT('Ctrl Pts',(110.229726954067,-4.91134478705064,335.300008991737));
#37283=CARTESIAN_POINT('Ctrl Pts',(110.221322306855,-4.89778963213231,335.448151516652));
#37284=CARTESIAN_POINT('Ctrl Pts',(110.212881585518,-4.8841762962643,335.596929893597));
#37285=CARTESIAN_POINT('Ctrl Pts',(110.204440864181,-4.86379752081166,335.744892036098));
#37286=CARTESIAN_POINT('Ctrl Pts',(110.196000142844,-4.8367869983973,335.891445228062));
#37287=CARTESIAN_POINT('Ctrl Pts',(110.187541124662,-4.80971792561422,336.038316101532));
#37288=CARTESIAN_POINT('Ctrl Pts',(110.17908210648,-4.77598844349376,336.183771654938));
#37289=CARTESIAN_POINT('Ctrl Pts',(110.170623088298,-4.73578228833357,336.327233656899));
#37290=CARTESIAN_POINT('Ctrl Pts',(110.162136028151,-4.69544284825189,336.471171240811));
#37291=CARTESIAN_POINT('Ctrl Pts',(110.153648968005,-4.64858385138581,336.613101785076));
#37292=CARTESIAN_POINT('Ctrl Pts',(110.145161907858,-4.59543845833362,336.752463534048));
#37293=CARTESIAN_POINT('Ctrl Pts',(110.139246516497,-4.55839668019884,336.849597202452));
#37294=CARTESIAN_POINT('Ctrl Pts',(110.133331125135,-4.51830200299678,336.945483427693));
#37295=CARTESIAN_POINT('Ctrl Pts',(110.127415733774,-4.47524643769942,337.039939308989));
#37296=CARTESIAN_POINT('Ctrl Pts',(110.119640654995,-4.41865501515803,337.164090336922));
#37297=CARTESIAN_POINT('Ctrl Pts',(110.111865576217,-4.35680400840861,337.286080848059));
#37298=CARTESIAN_POINT('Ctrl Pts',(110.104090497439,-4.2898804373959,337.40543320326));
#37299=CARTESIAN_POINT('Ctrl Pts',(110.09632498639,-4.22303922009794,337.52463868779));
#37300=CARTESIAN_POINT('Ctrl Pts',(110.088559475341,-4.15113804789479,337.641212138151));
#37301=CARTESIAN_POINT('Ctrl Pts',(110.080793964292,-4.07441175231475,337.754696341723));
#37302=CARTESIAN_POINT('Ctrl Pts',(110.073036152769,-3.99776153108016,337.868068025376));
#37303=CARTESIAN_POINT('Ctrl Pts',(110.065278341247,-3.91629592466286,337.978356236054));
#37304=CARTESIAN_POINT('Ctrl Pts',(110.057520529725,-3.83029519877422,338.085129130644));
#37305=CARTESIAN_POINT('Ctrl Pts',(110.049768556202,-3.74435919115911,338.191821675245));
#37306=CARTESIAN_POINT('Ctrl Pts',(110.042016582679,-3.65389510132756,338.295003866086));
#37307=CARTESIAN_POINT('Ctrl Pts',(110.034264609156,-3.55922573432606,338.394273889157));
#37308=CARTESIAN_POINT('Ctrl Pts',(110.026515918598,-3.46459645985764,338.493501871314));
#37309=CARTESIAN_POINT('Ctrl Pts',(110.018767228041,-3.36576571957422,338.58882069869));
#37310=CARTESIAN_POINT('Ctrl Pts',(110.011018537483,-3.26309557899603,338.6798628106));
#37311=CARTESIAN_POINT('Ctrl Pts',(110.003271459105,-3.1604467997981,338.770885980438));
#37312=CARTESIAN_POINT('Ctrl Pts',(109.995524380728,-3.05396050148425,338.857633945528));
#37313=CARTESIAN_POINT('Ctrl Pts',(109.98777730235,-2.94403418082203,338.939777380088));
#37314=CARTESIAN_POINT('Ctrl Pts',(109.980030159044,-2.83410693887145,339.021921503089));
#37315=CARTESIAN_POINT('Ctrl Pts',(109.972283015738,-2.72073993017841,339.099460784613));
#37316=CARTESIAN_POINT('Ctrl Pts',(109.964535872432,-2.60436184341858,339.17210767491));
#37317=CARTESIAN_POINT('Ctrl Pts',(109.956786987404,-2.48795759239406,339.244770897771));
#37318=CARTESIAN_POINT('Ctrl Pts',(109.949038102376,-2.36854124774976,339.31253933376));
#37319=CARTESIAN_POINT('Ctrl Pts',(109.941289217348,-2.24656809063275,339.375170268304));
#37320=CARTESIAN_POINT('Ctrl Pts',(109.933532107573,-2.12446546994647,339.437867679969));
#37321=CARTESIAN_POINT('Ctrl Pts',(109.925774997799,-1.99980096392575,339.495416518489));
#37322=CARTESIAN_POINT('Ctrl Pts',(109.918017888024,-1.87305243512715,339.547621096548));
#37323=CARTESIAN_POINT('Ctrl Pts',(109.910256633098,-1.74623617596738,339.599853571063));
#37324=CARTESIAN_POINT('Ctrl Pts',(109.902495378172,-1.61733404215803,339.646735961142));
#37325=CARTESIAN_POINT('Ctrl Pts',(109.894734123245,-1.48684028835761,339.688122120787));
#37326=CARTESIAN_POINT('Ctrl Pts',(109.886960452841,-1.35613778707902,339.729574484801));
#37327=CARTESIAN_POINT('Ctrl Pts',(109.879186782436,-1.22383895540408,339.765512946487));
#37328=CARTESIAN_POINT('Ctrl Pts',(109.871413112032,-1.09045037131715,339.795842058512));
#37329=CARTESIAN_POINT('Ctrl Pts',(109.864001307854,-0.963271057909453,
339.824759343076));
#37330=CARTESIAN_POINT('Ctrl Pts',(109.856589503677,-0.835101447788344,
339.848577703379));
#37331=CARTESIAN_POINT('Ctrl Pts',(109.8491776995,-0.706384151899945,339.867258416444));
#37332=CARTESIAN_POINT('Ctrl Pts',(109.841402620722,-0.571358037912271,
339.886854726903));
#37333=CARTESIAN_POINT('Ctrl Pts',(109.833627541943,-0.435302485781498,
339.900858961184));
#37334=CARTESIAN_POINT('Ctrl Pts',(109.825852463165,-0.298720359673227,
339.909169910404));
#37335=CARTESIAN_POINT('Ctrl Pts',(109.818086952116,-0.162306306566375,
339.917470632472));
#37336=CARTESIAN_POINT('Ctrl Pts',(109.810321441067,-0.0253673552049586,
339.920091985795));
#37337=CARTESIAN_POINT('Ctrl Pts',(109.802555930018,0.111584933750508,339.916984021233));
#37338=CARTESIAN_POINT('Ctrl Pts',(109.794798118495,0.24840143411275,339.913879138227));
#37339=CARTESIAN_POINT('Ctrl Pts',(109.787040306973,0.385230857495597,339.905056250932));
#37340=CARTESIAN_POINT('Ctrl Pts',(109.779282495451,0.521558389955213,339.890517345677));
#37341=CARTESIAN_POINT('Ctrl Pts',(109.771530521928,0.657783331623366,339.875989381409));
#37342=CARTESIAN_POINT('Ctrl Pts',(109.763778548405,0.793506747034172,339.85575400236));
#37343=CARTESIAN_POINT('Ctrl Pts',(109.756026574882,0.928216053879054,339.829865217563));
#37344=CARTESIAN_POINT('Ctrl Pts',(109.748277884324,1.06286831125251,339.80398739668));
#37345=CARTESIAN_POINT('Ctrl Pts',(109.740529193767,1.1965069312056,339.772461005601));
#37346=CARTESIAN_POINT('Ctrl Pts',(109.732780503209,1.32862688968728,339.735391604767));
#37347=CARTESIAN_POINT('Ctrl Pts',(109.725033424831,1.4607193595082,339.698329916532));
#37348=CARTESIAN_POINT('Ctrl Pts',(109.717286346453,1.59129342023932,339.655727618001));
#37349=CARTESIAN_POINT('Ctrl Pts',(109.709539268076,1.71985702649545,339.607740755611));
#37350=CARTESIAN_POINT('Ctrl Pts',(109.70179212477,1.84842171023827,339.559753491044));
#37351=CARTESIAN_POINT('Ctrl Pts',(109.694044981464,1.97497553970162,339.506381709291));
#37352=CARTESIAN_POINT('Ctrl Pts',(109.686297838158,2.09904472012501,339.447830294134));
#37353=CARTESIAN_POINT('Ctrl Pts',(109.67854895313,2.22314179393413,339.389265715376));
#37354=CARTESIAN_POINT('Ctrl Pts',(109.670800068102,2.34475275372905,339.325519352794));
#37355=CARTESIAN_POINT('Ctrl Pts',(109.663051183074,2.46342711689372,339.256842715235));
#37356=CARTESIAN_POINT('Ctrl Pts',(109.655294073299,2.58222744225374,339.188093183584));
#37357=CARTESIAN_POINT('Ctrl Pts',(109.647536963524,2.69808460577164,339.114403119545));
#37358=CARTESIAN_POINT('Ctrl Pts',(109.63977985375,2.81057545095884,339.036068470302));
#37359=CARTESIAN_POINT('Ctrl Pts',(109.632018598824,2.92312640765686,338.957691961528));
#37360=CARTESIAN_POINT('Ctrl Pts',(109.624257343897,3.0323071506728,338.874666158583));
#37361=CARTESIAN_POINT('Ctrl Pts',(109.616496088971,3.13772731316523,338.787327602772));
#37362=CARTESIAN_POINT('Ctrl Pts',(109.608722418567,3.24331611356129,338.699849333735));
#37363=CARTESIAN_POINT('Ctrl Pts',(109.600948748162,3.34513202183141,338.608044787474));
#37364=CARTESIAN_POINT('Ctrl Pts',(109.593175077757,3.44282063586128,338.512288304195));
#37365=CARTESIAN_POINT('Ctrl Pts',(109.58576327358,3.53596182140487,338.420989308252));
#37366=CARTESIAN_POINT('Ctrl Pts',(109.578351469403,3.62535111913162,338.326098230181));
#37367=CARTESIAN_POINT('Ctrl Pts',(109.570939665226,3.71071644388418,338.227966315746));
#37368=CARTESIAN_POINT('Ctrl Pts',(109.563164586448,3.80026577749375,338.125024663863));
#37369=CARTESIAN_POINT('Ctrl Pts',(109.555389507669,3.88566970299204,338.018191142191));
#37370=CARTESIAN_POINT('Ctrl Pts',(109.547614428891,3.96657098301511,337.907833849999));
#37371=CARTESIAN_POINT('Ctrl Pts',(109.539848917842,4.04737270886268,337.797612359482));
#37372=CARTESIAN_POINT('Ctrl Pts',(109.532083406793,4.12368258493346,337.683876038514));
#37373=CARTESIAN_POINT('Ctrl Pts',(109.524317895744,4.19518177310224,337.567028039023));
#37374=CARTESIAN_POINT('Ctrl Pts',(109.516560084222,4.26661006961778,337.450295894664));
#37375=CARTESIAN_POINT('Ctrl Pts',(109.508802272699,4.33323696772656,337.330458542841));
#37376=CARTESIAN_POINT('Ctrl Pts',(109.501044461177,4.39478554240987,337.2079499765));
#37377=CARTESIAN_POINT('Ctrl Pts',(109.493292487654,4.45628779983887,337.08553360174));
#37378=CARTESIAN_POINT('Ctrl Pts',(109.485540514131,4.51271916578058,336.96045036148));
#37379=CARTESIAN_POINT('Ctrl Pts',(109.477788540608,4.56384766988322,336.833160524504));
#37380=CARTESIAN_POINT('Ctrl Pts',(109.47003985005,4.61495452103402,336.705924594851));
#37381=CARTESIAN_POINT('Ctrl Pts',(109.462291159493,4.66076283162849,336.57648428908));
#37382=CARTESIAN_POINT('Ctrl Pts',(109.454542468935,4.70108807220229,336.445321417505));
#37383=CARTESIAN_POINT('Ctrl Pts',(109.446795390557,4.741404922773,336.314185835459));
#37384=CARTESIAN_POINT('Ctrl Pts',(109.43904831218,4.77624085765821,336.181328773861));
#37385=CARTESIAN_POINT('Ctrl Pts',(109.431301233802,4.80546082564253,336.047248449851));
#37386=CARTESIAN_POINT('Ctrl Pts',(109.423554090496,4.8346810385183,335.913167002119));
#37387=CARTESIAN_POINT('Ctrl Pts',(109.41580694719,4.85828510738479,335.777862653436));
#37388=CARTESIAN_POINT('Ctrl Pts',(109.408059803884,4.87618892585517,335.641844702298));
#37389=CARTESIAN_POINT('Ctrl Pts',(109.400310918856,4.89409676948403,335.505796171436));
#37390=CARTESIAN_POINT('Ctrl Pts',(109.392562033828,4.90630176160053,335.36903410633));
#37391=CARTESIAN_POINT('Ctrl Pts',(109.3848131488,4.91277161936732,335.23207343329));
#37392=CARTESIAN_POINT('Ctrl Pts',(109.377056039025,4.91924834430799,335.094967388777));
#37393=CARTESIAN_POINT('Ctrl Pts',(109.369298929251,4.91997775641148,334.957662706284));
#37394=CARTESIAN_POINT('Ctrl Pts',(109.361541819476,4.91497972972099,334.820675381133));
#37395=CARTESIAN_POINT('Ctrl Pts',(109.35378056455,4.90997903224484,334.683614854335));
#37396=CARTESIAN_POINT('Ctrl Pts',(109.346019309623,4.89924482810669,334.546872412271));
#37397=CARTESIAN_POINT('Ctrl Pts',(109.338258054697,4.88284887217082,334.410958444556));
#37398=CARTESIAN_POINT('Ctrl Pts',(109.330484384293,4.86642668804888,334.274827058786));
#37399=CARTESIAN_POINT('Ctrl Pts',(109.322710713888,4.84432471669487,334.139527181649));
#37400=CARTESIAN_POINT('Ctrl Pts',(109.314937043483,4.81666596145387,334.005559414408));
#37401=CARTESIAN_POINT('Ctrl Pts',(109.307525239306,4.7902947279236,333.877827878963));
#37402=CARTESIAN_POINT('Ctrl Pts',(109.300113435129,4.75887247411791,333.751307504273));
#37403=CARTESIAN_POINT('Ctrl Pts',(109.292701630952,4.72254732920113,333.626417171789));
#37404=CARTESIAN_POINT('Ctrl Pts',(109.284926552173,4.68444178072505,333.495405592081));
#37405=CARTESIAN_POINT('Ctrl Pts',(109.277151473395,4.64082015772091,333.365773860434));
#37406=CARTESIAN_POINT('Ctrl Pts',(109.269376394617,4.5917986810825,333.238021585005));
#37407=CARTESIAN_POINT('Ctrl Pts',(109.261610883568,4.54283752849195,333.110426516883));
#37408=CARTESIAN_POINT('Ctrl Pts',(109.253845372519,4.48848988233381,332.984706664631));
#37409=CARTESIAN_POINT('Ctrl Pts',(109.24607986147,4.42892222005965,332.861348314671));
#37410=CARTESIAN_POINT('Ctrl Pts',(109.238322049947,4.36941361929606,332.738112274873));
#37411=CARTESIAN_POINT('Ctrl Pts',(109.230564238425,4.30469547114769,332.617233427494));
#37412=CARTESIAN_POINT('Ctrl Pts',(109.222806426903,4.23498286952324,332.499179503174));
#37413=CARTESIAN_POINT('Ctrl Pts',(109.21505445338,4.16532272884222,332.381214418176));
#37414=CARTESIAN_POINT('Ctrl Pts',(109.207302479857,4.09067581371561,332.266070360066));
#37415=CARTESIAN_POINT('Ctrl Pts',(109.199550506334,4.01130364151637,332.15419147551));
#37416=CARTESIAN_POINT('Ctrl Pts',(109.191801815776,3.93196508347924,332.042359971729));
#37417=CARTESIAN_POINT('Ctrl Pts',(109.184053125219,3.84790547421205,331.933791209337));
#37418=CARTESIAN_POINT('Ctrl Pts',(109.176304434661,3.75943011880288,331.828901098304));
#37419=CARTESIAN_POINT('Ctrl Pts',(109.168557356283,3.67097317143031,331.724032810534));
#37420=CARTESIAN_POINT('Ctrl Pts',(109.160810277905,3.57810255720293,331.62284195033));
#37421=CARTESIAN_POINT('Ctrl Pts',(109.153063199527,3.48116415358215,331.525711699022));
#37422=CARTESIAN_POINT('Ctrl Pts',(109.145316056222,3.38422493752432,331.428580633669));
#37423=CARTESIAN_POINT('Ctrl Pts',(109.137568912916,3.28321814019055,331.335510521755));
#37424=CARTESIAN_POINT('Ctrl Pts',(109.12982176961,3.17852652675748,331.246847700772));
#37425=CARTESIAN_POINT('Ctrl Pts',(109.122072884582,3.07381137642705,331.158164946505));
#37426=CARTESIAN_POINT('Ctrl Pts',(109.114323999554,2.96541005974504,331.073891707418));
#37427=CARTESIAN_POINT('Ctrl Pts',(109.106575114526,2.85373811913615,330.99433378701));
#37428=CARTESIAN_POINT('Ctrl Pts',(109.098818004751,2.74194764877562,330.914691423003));
#37429=CARTESIAN_POINT('Ctrl Pts',(109.091060894976,2.62687993874335,330.839774602566));
#37430=CARTESIAN_POINT('Ctrl Pts',(109.083303785202,2.5089796554982,330.769845847868));
#37431=CARTESIAN_POINT('Ctrl Pts',(109.075542530275,2.39101637011147,330.69987972548));
#37432=CARTESIAN_POINT('Ctrl Pts',(109.067781275349,2.27021783952015,330.634907165063));
#37433=CARTESIAN_POINT('Ctrl Pts',(109.060020020423,2.14705209191434,330.57514402753));
#37434=CARTESIAN_POINT('Ctrl Pts',(109.052246350018,2.02368931925198,330.515285288453));
#37435=CARTESIAN_POINT('Ctrl Pts',(109.044472679614,1.89795212116079,330.460652780665));
#37436=CARTESIAN_POINT('Ctrl Pts',(109.036699009209,1.77032802809097,330.411413972098));
#37437=CARTESIAN_POINT('Ctrl Pts',(109.029287205032,1.64864486725917,330.364467241917));
#37438=CARTESIAN_POINT('Ctrl Pts',(109.021875400855,1.5252468004473,330.322423451024));
#37439=CARTESIAN_POINT('Ctrl Pts',(109.014463596678,1.40056623519365,330.285384715235));
#37440=CARTESIAN_POINT('Ctrl Pts',(109.006688517899,1.26977470403156,330.246530600672));
#37441=CARTESIAN_POINT('Ctrl Pts',(108.998913439121,1.13715845210191,330.213061785822));
#37442=CARTESIAN_POINT('Ctrl Pts',(108.991138360343,1.00320050435739,330.185150904695));
#37443=CARTESIAN_POINT('Ctrl Pts',(108.983372849294,0.869407400395848,330.157274369685));
#37444=CARTESIAN_POINT('Ctrl Pts',(108.975607338245,0.734276264718385,330.134942238938));
#37445=CARTESIAN_POINT('Ctrl Pts',(108.967841827196,0.598306116453239,330.118277675501));
#37446=CARTESIAN_POINT('Ctrl Pts',(108.960084015673,0.462470782985871,330.101629635026));
#37447=CARTESIAN_POINT('Ctrl Pts',(108.952326204151,0.325798477897935,330.090638026161));
#37448=CARTESIAN_POINT('Ctrl Pts',(108.944568392629,0.188798925520283,330.085375087738));
#37449=CARTESIAN_POINT('Ctrl Pts',(108.936816419106,0.0519024696503939,
330.080116109843));
#37450=CARTESIAN_POINT('Ctrl Pts',(108.929064445583,-0.0853203543193356,
330.080577236487));
#37451=CARTESIAN_POINT('Ctrl Pts',(108.92131247206,-0.222354531924368,330.086778905379));
#37452=CARTESIAN_POINT('Ctrl Pts',(108.913563781502,-0.359330675473921,
330.09297794786));
#37453=CARTESIAN_POINT('Ctrl Pts',(108.905815090945,-0.496117941896057,
330.104912679621));
#37454=CARTESIAN_POINT('Ctrl Pts',(108.898066400387,-0.632201365523266,
330.12255143585));
#37455=CARTESIAN_POINT('Ctrl Pts',(108.890319322009,-0.768256475857506,
330.140186522188));
#37456=CARTESIAN_POINT('Ctrl Pts',(108.882572243631,-0.903607647288817,
330.163523222213));
#37457=CARTESIAN_POINT('Ctrl Pts',(108.874825165254,-1.03774548032018,330.192478041592));
#37458=CARTESIAN_POINT('Ctrl Pts',(108.867078021948,-1.1718844375557,330.221433103641));
#37459=CARTESIAN_POINT('Ctrl Pts',(108.859330878642,-1.30480965403428,330.256006296485));
#37460=CARTESIAN_POINT('Ctrl Pts',(108.851583735336,-1.43602275096882,330.296063167814));
#37461=CARTESIAN_POINT('Ctrl Pts',(108.843834850308,-1.56726534739338,330.336129044777));
#37462=CARTESIAN_POINT('Ctrl Pts',(108.83608596528,-1.69679468455561,330.381680939348));
#37463=CARTESIAN_POINT('Ctrl Pts',(108.828337080252,-1.82412873191852,330.432534900857));
#37464=CARTESIAN_POINT('Ctrl Pts',(108.820579970477,-1.95159793295482,330.483442839286));
#37465=CARTESIAN_POINT('Ctrl Pts',(108.812822860702,-2.07686682602267,330.53966394125));
#37466=CARTESIAN_POINT('Ctrl Pts',(108.805065750928,-2.19947401609355,330.600966343044));
#37467=CARTESIAN_POINT('Ctrl Pts',(108.797304496001,-2.32214672352659,330.662301502882));
#37468=CARTESIAN_POINT('Ctrl Pts',(108.789543241075,-2.44215455203073,330.728723183814));
#37469=CARTESIAN_POINT('Ctrl Pts',(108.781781986149,-2.559062702652,330.799954625674));
#37470=CARTESIAN_POINT('Ctrl Pts',(108.774008315744,-2.67615786821398,330.871300014627));
#37471=CARTESIAN_POINT('Ctrl Pts',(108.76623464534,-2.790143122232,330.947470322211));
#37472=CARTESIAN_POINT('Ctrl Pts',(108.758460974935,-2.90061380664893,331.028146200176));
#37473=CARTESIAN_POINT('Ctrl Pts',(108.751049170758,-3.00594205412869,331.105066596612));
#37474=CARTESIAN_POINT('Ctrl Pts',(108.743637366581,-3.10807534938728,331.186082355853));
#37475=CARTESIAN_POINT('Ctrl Pts',(108.736225562404,-3.20669382052801,331.270885117902));
#37476=CARTESIAN_POINT('Ctrl Pts',(108.728562913846,-3.30864992563361,331.358557936397));
#37477=CARTESIAN_POINT('Ctrl Pts',(108.720900265287,-3.40719142055373,331.450573305663));
#37478=CARTESIAN_POINT('Ctrl Pts',(108.713237616729,-3.50191761917469,331.546631202577));
#37479=CARTESIAN_POINT('Ctrl Pts',(108.705584462041,-3.59652645390365,331.642570085651));
#37480=CARTESIAN_POINT('Ctrl Pts',(108.697931307353,-3.68732911260994,331.742541251977));
#37481=CARTESIAN_POINT('Ctrl Pts',(108.690278152666,-3.77395733333042,331.846204015999));
#37482=CARTESIAN_POINT('Ctrl Pts',(108.682632523285,-3.86050037297028,331.949764848962));
#37483=CARTESIAN_POINT('Ctrl Pts',(108.674986893905,-3.94287688229336,332.057009752153));
#37484=CARTESIAN_POINT('Ctrl Pts',(108.667341264524,-4.02075527324775,332.167561104781));
#37485=CARTESIAN_POINT('Ctrl Pts',(108.659701345131,-4.0985755022631,332.278029894313));
#37486=CARTESIAN_POINT('Ctrl Pts',(108.652061425738,-4.17190406617584,332.391799891288));
#37487=CARTESIAN_POINT('Ctrl Pts',(108.644421506345,-4.24044987896429,332.508460739524));
#37488=CARTESIAN_POINT('Ctrl Pts',(108.636784588332,-4.30896876319232,332.625075756972));
#37489=CARTESIAN_POINT('Ctrl Pts',(108.629147670319,-4.37270842827463,332.744579020613));
#37490=CARTESIAN_POINT('Ctrl Pts',(108.621510752306,-4.43142153970922,332.866531884489));
#37491=CARTESIAN_POINT('Ctrl Pts',(108.613875070075,-4.49012515037309,332.988465014337));
#37492=CARTESIAN_POINT('Ctrl Pts',(108.606239387844,-4.54380365076244,333.112846592724));
#37493=CARTESIAN_POINT('Ctrl Pts',(108.598603705613,-4.59225629740001,333.239214617993));
#37494=CARTESIAN_POINT('Ctrl Pts',(108.590967494843,-4.6407122979124,333.365591390411));
#37495=CARTESIAN_POINT('Ctrl Pts',(108.583331284073,-4.68394158254028,333.493954506195));
#37496=CARTESIAN_POINT('Ctrl Pts',(108.575695073302,-4.72179226687599,333.623823829966));
#37497=CARTESIAN_POINT('Ctrl Pts',(108.568053090257,-4.75967156285829,333.753791323037));
#37498=CARTESIAN_POINT('Ctrl Pts',(108.560411107212,-4.79216402805422,333.885266909895));
#37499=CARTESIAN_POINT('Ctrl Pts',(108.552769124166,-4.81916817768044,334.017757088225));
#37500=CARTESIAN_POINT('Ctrl Pts',(108.545123862112,-4.84618391420262,334.150304115222));
#37501=CARTESIAN_POINT('Ctrl Pts',(108.537478600057,-4.86770658117338,334.283866203063));
#37502=CARTESIAN_POINT('Ctrl Pts',(108.529833338002,-4.88368637289488,334.417942894811));
#37503=CARTESIAN_POINT('Ctrl Pts',(108.522178982304,-4.89968517175085,334.552179063838));
#37504=CARTESIAN_POINT('Ctrl Pts',(108.514524626606,-4.91012790262292,334.68693065758));
#37505=CARTESIAN_POINT('Ctrl Pts',(108.506870270908,-4.91501683048537,334.821695152771));
#37506=CARTESIAN_POINT('Ctrl Pts',(108.50342559678,-4.91721698474864,334.882342944469));
#37507=CARTESIAN_POINT('Ctrl Pts',(108.499980922652,-4.91829305663433,334.942993382303));
#37508=CARTESIAN_POINT('Ctrl Pts',(108.496536248524,-4.9182486817404,335.003600980256));
#37509=CARTESIAN_POINT('',(111.99653624849,-4.91682066856926,334.995613600539));
#37510=CARTESIAN_POINT('Ctrl Pts',(111.99653624849,-4.91583883843042,334.99561447645));
#37511=CARTESIAN_POINT('Ctrl Pts',(111.929972145466,-4.90575025587869,336.172136823171));
#37512=CARTESIAN_POINT('Ctrl Pts',(111.770662031017,-3.8923044058229,339.00355018297));
#37513=CARTESIAN_POINT('Ctrl Pts',(111.518605905143,0.841275660426242,340.754711472316));
#37514=CARTESIAN_POINT('Ctrl Pts',(111.240367870869,5.29452218069954,337.406757932263));
#37515=CARTESIAN_POINT('Ctrl Pts',(110.962129836596,4.88906384276416,331.850158161461));
#37516=CARTESIAN_POINT('Ctrl Pts',(110.683891802322,-0.00301622121185956,
329.184121754297));
#37517=CARTESIAN_POINT('Ctrl Pts',(110.445360606286,-4.19458360114431,331.474041886394));
#37518=CARTESIAN_POINT('Ctrl Pts',(110.299575421676,-4.90756129070927,334.062005703542));
#37519=CARTESIAN_POINT('Ctrl Pts',(110.24653624849,-4.91080622874904,335.001893402137));
#37520=CARTESIAN_POINT('',(113.746536248529,-4.91824999495766,335.000222708279));
#37521=CARTESIAN_POINT('Ctrl Pts',(113.74653624849,-4.91824999495763,335.000222708968));
#37522=CARTESIAN_POINT('Ctrl Pts',(113.745860892105,-4.91824945829249,335.012074289756));
#37523=CARTESIAN_POINT('Ctrl Pts',(113.74518553572,-4.91820608331596,335.023925756962));
#37524=CARTESIAN_POINT('Ctrl Pts',(113.744510179335,-4.91811987196888,335.035776912175));
#37525=CARTESIAN_POINT('Ctrl Pts',(113.736735100557,-4.91712735893421,335.172214010356));
#37526=CARTESIAN_POINT('Ctrl Pts',(113.728960021778,-4.91045147623641,335.308825373111));
#37527=CARTESIAN_POINT('Ctrl Pts',(113.721184943,-4.89806801477245,335.445098624086));
#37528=CARTESIAN_POINT('Ctrl Pts',(113.713419431951,-4.88569979194618,335.58120418215));
#37529=CARTESIAN_POINT('Ctrl Pts',(113.705653920902,-4.86763800021826,335.716972070743));
#37530=CARTESIAN_POINT('Ctrl Pts',(113.697888409853,-4.84391041548599,335.851889047498));
#37531=CARTESIAN_POINT('Ctrl Pts',(113.69013059833,-4.82020635672306,335.986672253677));
#37532=CARTESIAN_POINT('Ctrl Pts',(113.682372786808,-4.79084775166455,336.120605844507));
#37533=CARTESIAN_POINT('Ctrl Pts',(113.674614975286,-4.75591420825975,336.25318119447));
#37534=CARTESIAN_POINT('Ctrl Pts',(113.666863001763,-4.72100695345425,336.385656777277));
#37535=CARTESIAN_POINT('Ctrl Pts',(113.65911102824,-4.68053321007231,336.516775777246));
#37536=CARTESIAN_POINT('Ctrl Pts',(113.651359054717,-4.63462367711408,336.64603962104));
#37537=CARTESIAN_POINT('Ctrl Pts',(113.643610364159,-4.58873358687026,336.77524872152));
#37538=CARTESIAN_POINT('Ctrl Pts',(113.635861673602,-4.53741241623104,336.902603860881));
#37539=CARTESIAN_POINT('Ctrl Pts',(113.628112983044,-4.48084068598308,337.027621712583));
#37540=CARTESIAN_POINT('Ctrl Pts',(113.620365904666,-4.42428072595613,337.152613553277));
#37541=CARTESIAN_POINT('Ctrl Pts',(113.612618826288,-4.36247254026919,337.275268717693));
#37542=CARTESIAN_POINT('Ctrl Pts',(113.60487174791,-4.29564460075782,337.395124323805));
#37543=CARTESIAN_POINT('Ctrl Pts',(113.597124604605,-4.22881610116395,337.514980934421));
#37544=CARTESIAN_POINT('Ctrl Pts',(113.589377461299,-4.15696795418387,337.632037598542));
#37545=CARTESIAN_POINT('Ctrl Pts',(113.581630317993,-4.08037415779872,337.745856841656));
#37546=CARTESIAN_POINT('Ctrl Pts',(113.573881432965,-4.00376314150208,337.859701673752));
#37547=CARTESIAN_POINT('Ctrl Pts',(113.566132547937,-3.92240457092562,337.9703073123));
#37548=CARTESIAN_POINT('Ctrl Pts',(113.558383662909,-3.83661501983729,338.077266360272));
#37549=CARTESIAN_POINT('Ctrl Pts',(113.550626553134,-3.75073441083301,338.184338935682));
#37550=CARTESIAN_POINT('Ctrl Pts',(113.542869443359,-3.66041367140612,338.287756883379));
#37551=CARTESIAN_POINT('Ctrl Pts',(113.535112333584,-3.56600918400808,338.387146522085));
#37552=CARTESIAN_POINT('Ctrl Pts',(113.527351078658,-3.47155424987037,338.486589271435));
#37553=CARTESIAN_POINT('Ctrl Pts',(113.519589823732,-3.37301150015818,338.581999150794));
#37554=CARTESIAN_POINT('Ctrl Pts',(113.511828568806,-3.27077250175421,338.673041015871));
#37555=CARTESIAN_POINT('Ctrl Pts',(113.504054898401,-3.16836995427248,338.764228518261));
#37556=CARTESIAN_POINT('Ctrl Pts',(113.496281227997,-3.06225964528318,338.851033795849));
#37557=CARTESIAN_POINT('Ctrl Pts',(113.488507557592,-2.95286508399031,338.933162958517));
#37558=CARTESIAN_POINT('Ctrl Pts',(113.481095753415,-2.84856286584562,339.011468988903));
#37559=CARTESIAN_POINT('Ctrl Pts',(113.473683949238,-2.74127551511268,339.085524289983));
#37560=CARTESIAN_POINT('Ctrl Pts',(113.466272145061,-2.63139129566544,339.155112863882));
#37561=CARTESIAN_POINT('Ctrl Pts',(113.458497066283,-2.51612132329367,339.228112181081));
#37562=CARTESIAN_POINT('Ctrl Pts',(113.450721987504,-2.39762921068808,339.296426536042));
#37563=CARTESIAN_POINT('Ctrl Pts',(113.442946908726,-2.27633272511975,339.359758294567));
#37564=CARTESIAN_POINT('Ctrl Pts',(113.435181397677,-2.15518550259894,339.423012119332));
#37565=CARTESIAN_POINT('Ctrl Pts',(113.427415886628,-2.0312411167115,339.481295368214));
#37566=CARTESIAN_POINT('Ctrl Pts',(113.419650375579,-1.90494619504383,339.534353653663));
#37567=CARTESIAN_POINT('Ctrl Pts',(113.411892564056,-1.77877649515877,339.587359331668));
#37568=CARTESIAN_POINT('Ctrl Pts',(113.404134752534,-1.65026125548881,339.635150205442));
#37569=CARTESIAN_POINT('Ctrl Pts',(113.396376941012,-1.51987127051161,339.677517972555));
#37570=CARTESIAN_POINT('Ctrl Pts',(113.388624967489,-1.38957940813319,339.71985385658));
#37571=CARTESIAN_POINT('Ctrl Pts',(113.380872993966,-1.25741597883199,339.75677463679));
#37572=CARTESIAN_POINT('Ctrl Pts',(113.373121020443,-1.12387097229015,339.788120414123));
#37573=CARTESIAN_POINT('Ctrl Pts',(113.365372329885,-0.990382522137781,
339.819452916501));
#37574=CARTESIAN_POINT('Ctrl Pts',(113.357623639328,-0.855514038205416,
339.845215022766));
#37575=CARTESIAN_POINT('Ctrl Pts',(113.34987494877,-0.719769650248154,339.865296980975));
#37576=CARTESIAN_POINT('Ctrl Pts',(113.342127870392,-0.584053505044566,
339.885374760964));
#37577=CARTESIAN_POINT('Ctrl Pts',(113.334380792014,-0.44746220472576,339.899774686417));
#37578=CARTESIAN_POINT('Ctrl Pts',(113.326633713637,-0.310508635883616,
339.908438392151));
#37579=CARTESIAN_POINT('Ctrl Pts',(113.318886570331,-0.173553919238654,
339.917102170495));
#37580=CARTESIAN_POINT('Ctrl Pts',(113.311139427025,-0.0362373181090265,
339.920029608552));
#37581=CARTESIAN_POINT('Ctrl Pts',(113.303392283719,0.10092500982788,339.91721437451));
#37582=CARTESIAN_POINT('Ctrl Pts',(113.295643398691,0.238118174767959,339.914398507545));
#37583=CARTESIAN_POINT('Ctrl Pts',(113.287894513663,0.375156606782635,339.905837407406));
#37584=CARTESIAN_POINT('Ctrl Pts',(113.280145628635,0.511526400790512,339.891576821823));
#37585=CARTESIAN_POINT('Ctrl Pts',(113.27238851886,0.648040939106898,339.877301099907));
#37586=CARTESIAN_POINT('Ctrl Pts',(113.264631409085,0.783885032357087,339.857313848833));
#37587=CARTESIAN_POINT('Ctrl Pts',(113.256874299311,0.918551584988934,339.831712537829));
#37588=CARTESIAN_POINT('Ctrl Pts',(113.249113044385,1.05329009912071,339.806097546303));
#37589=CARTESIAN_POINT('Ctrl Pts',(113.241351789458,1.1868494384051,339.774862606091));
#37590=CARTESIAN_POINT('Ctrl Pts',(113.233590534532,1.31873587354948,339.738155628334));
#37591=CARTESIAN_POINT('Ctrl Pts',(113.225816864128,1.45083328400832,339.701389931375));
#37592=CARTESIAN_POINT('Ctrl Pts',(113.218043193723,1.581252070644,339.659134825371));
#37593=CARTESIAN_POINT('Ctrl Pts',(113.210269523318,1.70951590985447,339.61158740744));
#37594=CARTESIAN_POINT('Ctrl Pts',(113.202857719141,1.83180903649128,339.566253333252));
#37595=CARTESIAN_POINT('Ctrl Pts',(113.195445914964,1.95214306070018,339.516108683852));
#37596=CARTESIAN_POINT('Ctrl Pts',(113.188034110787,2.0701262333978,339.461363069769));
#37597=CARTESIAN_POINT('Ctrl Pts',(113.180259032009,2.19389211284315,339.403934210061));
#37598=CARTESIAN_POINT('Ctrl Pts',(113.17248395323,2.31546199255914,339.341260481999));
#37599=CARTESIAN_POINT('Ctrl Pts',(113.164708874452,2.43435950775904,339.273532128051));
#37600=CARTESIAN_POINT('Ctrl Pts',(113.156943363403,2.55311071199701,339.205887118154));
#37601=CARTESIAN_POINT('Ctrl Pts',(113.149177852354,2.66919575853113,339.133200050086));
#37602=CARTESIAN_POINT('Ctrl Pts',(113.141412341305,2.78215903162971,339.055708838812));
#37603=CARTESIAN_POINT('Ctrl Pts',(113.133654529782,2.8950103013142,338.9782944603));
#37604=CARTESIAN_POINT('Ctrl Pts',(113.12589671826,3.00474563703244,338.896085637548));
#37605=CARTESIAN_POINT('Ctrl Pts',(113.118138906738,3.11093509892163,338.809365547279));
#37606=CARTESIAN_POINT('Ctrl Pts',(113.110386933215,3.21704464987322,338.722710716628));
#37607=CARTESIAN_POINT('Ctrl Pts',(113.102634959692,3.31961333675318,338.631551622032));
#37608=CARTESIAN_POINT('Ctrl Pts',(113.094882986169,3.41824153549645,338.536213775708));
#37609=CARTESIAN_POINT('Ctrl Pts',(113.087134295611,3.51682796513898,338.440916305019));
#37610=CARTESIAN_POINT('Ctrl Pts',(113.079385605054,3.61147694531549,338.341443873517));
#37611=CARTESIAN_POINT('Ctrl Pts',(113.071636914496,3.70182336973774,338.238161021593));
#37612=CARTESIAN_POINT('Ctrl Pts',(113.063889836118,3.79215099683179,338.134899658529));
#37613=CARTESIAN_POINT('Ctrl Pts',(113.05614275774,3.87817759156433,338.027829745974));
#37614=CARTESIAN_POINT('Ctrl Pts',(113.048395679363,3.95957652104232,337.917350996454));
#37615=CARTESIAN_POINT('Ctrl Pts',(113.040648536057,4.04097613272173,337.806871321016));
#37616=CARTESIAN_POINT('Ctrl Pts',(113.032901392751,4.11774776993411,337.692983066313));
#37617=CARTESIAN_POINT('Ctrl Pts',(113.025154249445,4.18960678558787,337.576116853843));
#37618=CARTESIAN_POINT('Ctrl Pts',(113.017405364417,4.26148195667391,337.459224367368));
#37619=CARTESIAN_POINT('Ctrl Pts',(113.009656479389,4.32844210375113,337.339352923779));
#37620=CARTESIAN_POINT('Ctrl Pts',(113.001907594361,4.39024759353263,337.216959433544));
#37621=CARTESIAN_POINT('Ctrl Pts',(112.994150484586,4.4521186842996,337.094436033594));
#37622=CARTESIAN_POINT('Ctrl Pts',(112.986393374811,4.50882401205307,336.96938558905));
#37623=CARTESIAN_POINT('Ctrl Pts',(112.978636265037,4.56017112224367,336.842287273569));
#37624=CARTESIAN_POINT('Ctrl Pts',(112.970875010111,4.61154567068816,336.715121040813));
#37625=CARTESIAN_POINT('Ctrl Pts',(112.963113755184,4.65755616521626,336.585905124636));
#37626=CARTESIAN_POINT('Ctrl Pts',(112.955352500258,4.69805980220984,336.455134755739));
#37627=CARTESIAN_POINT('Ctrl Pts',(112.947578829854,4.7386282318225,336.32415519687));
#37628=CARTESIAN_POINT('Ctrl Pts',(112.939805159449,4.77367210058735,336.191616594369));
#37629=CARTESIAN_POINT('Ctrl Pts',(112.932031489044,4.80309938564335,336.058026159475));
#37630=CARTESIAN_POINT('Ctrl Pts',(112.924619684867,4.8311568235,335.930654391466));
#37631=CARTESIAN_POINT('Ctrl Pts',(112.91720788069,4.85410876329437,335.802326796206));
#37632=CARTESIAN_POINT('Ctrl Pts',(112.909796076513,4.8719194730853,335.673486236142));
#37633=CARTESIAN_POINT('Ctrl Pts',(112.902020997735,4.89060313881857,335.538330816432));
#37634=CARTESIAN_POINT('Ctrl Pts',(112.894245918956,4.90368790139807,335.402183760527));
#37635=CARTESIAN_POINT('Ctrl Pts',(112.886470840178,4.91107595145501,335.265548604855));
#37636=CARTESIAN_POINT('Ctrl Pts',(112.878705329129,4.91845491004601,335.12908158744));
#37637=CARTESIAN_POINT('Ctrl Pts',(112.87093981808,4.92015108343508,334.992128051929));
#37638=CARTESIAN_POINT('Ctrl Pts',(112.863174307031,4.91611797957733,334.85519988475));
#37639=CARTESIAN_POINT('Ctrl Pts',(112.855416495509,4.9120888745538,334.718407482247));
#37640=CARTESIAN_POINT('Ctrl Pts',(112.847658683986,4.90234180842258,334.581640786208));
#37641=CARTESIAN_POINT('Ctrl Pts',(112.839900872464,4.88688224540193,334.445414585411));
#37642=CARTESIAN_POINT('Ctrl Pts',(112.832148898941,4.87143431619271,334.309290899149));
#37643=CARTESIAN_POINT('Ctrl Pts',(112.824396925418,4.85028249061291,334.173707285351));
#37644=CARTESIAN_POINT('Ctrl Pts',(112.816644951895,4.82348423932062,334.039175949757));
#37645=CARTESIAN_POINT('Ctrl Pts',(112.808896261338,4.79669733710367,333.904701588264));
#37646=CARTESIAN_POINT('Ctrl Pts',(112.80114757078,4.76426884143297,333.771279001173));
#37647=CARTESIAN_POINT('Ctrl Pts',(112.793398880222,4.72630772213892,333.639412487875));
#37648=CARTESIAN_POINT('Ctrl Pts',(112.785651801844,4.6883545009728,333.507573410507));
#37649=CARTESIAN_POINT('Ctrl Pts',(112.777904723467,4.64487105388345,333.377290138345));
#37650=CARTESIAN_POINT('Ctrl Pts',(112.770157645089,4.59601674786154,333.249053651343));
#37651=CARTESIAN_POINT('Ctrl Pts',(112.762410501783,4.54716203239348,333.120816089595));
#37652=CARTESIAN_POINT('Ctrl Pts',(112.754663358477,4.49293650736629,332.994625712486));
#37653=CARTESIAN_POINT('Ctrl Pts',(112.746916215171,4.43354825270876,332.870954919828));
#37654=CARTESIAN_POINT('Ctrl Pts',(112.739167330143,4.37414664631077,332.747256323351));
#37655=CARTESIAN_POINT('Ctrl Pts',(112.731418445115,4.30958016980779,332.626078790794));
#37656=CARTESIAN_POINT('Ctrl Pts',(112.723669560087,4.24010336963785,332.507871095371));
#37657=CARTESIAN_POINT('Ctrl Pts',(112.715912450312,4.17055282607434,332.389537933079));
#37658=CARTESIAN_POINT('Ctrl Pts',(112.708155340538,4.09608174602097,332.27418124228));
#37659=CARTESIAN_POINT('Ctrl Pts',(112.700398230763,4.01698892863049,332.162222170472));
#37660=CARTESIAN_POINT('Ctrl Pts',(112.692636975837,3.93785384656735,332.050203271316));
#37661=CARTESIAN_POINT('Ctrl Pts',(112.68487572091,3.85409234462456,331.941585918225));
#37662=CARTESIAN_POINT('Ctrl Pts',(112.677114465984,3.7660435936311,331.836758195558));
#37663=CARTESIAN_POINT('Ctrl Pts',(112.66934079558,3.67785399333106,331.731762782697));
#37664=CARTESIAN_POINT('Ctrl Pts',(112.661567125175,3.58536370310621,331.630569402948));
#37665=CARTESIAN_POINT('Ctrl Pts',(112.65379345477,3.48894944885784,331.533529921402));
#37666=CARTESIAN_POINT('Ctrl Pts',(112.646381650593,3.39702330134008,331.441007651068));
#37667=CARTESIAN_POINT('Ctrl Pts',(112.638969846416,3.30153050034026,331.352261450004));
#37668=CARTESIAN_POINT('Ctrl Pts',(112.631558042239,3.20282412173445,331.267561024245));
#37669=CARTESIAN_POINT('Ctrl Pts',(112.62378296346,3.09927984948263,331.17870917831));
#37670=CARTESIAN_POINT('Ctrl Pts',(112.616007884682,2.99187180143713,331.094028938239));
#37671=CARTESIAN_POINT('Ctrl Pts',(112.608232805904,2.88097048186124,331.013875046471));
#37672=CARTESIAN_POINT('Ctrl Pts',(112.600467294855,2.77020563341941,330.93381978917));
#37673=CARTESIAN_POINT('Ctrl Pts',(112.592701783806,2.65595638037961,330.858280024324));
#37674=CARTESIAN_POINT('Ctrl Pts',(112.584936272757,2.53862801944713,330.787571859203));
#37675=CARTESIAN_POINT('Ctrl Pts',(112.577178461234,2.42141598992611,330.716933801434));
#37676=CARTESIAN_POINT('Ctrl Pts',(112.569420649712,2.30113126066751,330.65111801039));
#37677=CARTESIAN_POINT('Ctrl Pts',(112.56166283819,2.17820968553823,330.59039847284));
#37678=CARTESIAN_POINT('Ctrl Pts',(112.553910864667,2.05538061279238,330.529724628668));
#37679=CARTESIAN_POINT('Ctrl Pts',(112.546158891144,1.92991899288691,330.47413957684));
#37680=CARTESIAN_POINT('Ctrl Pts',(112.538406917621,1.8022866512284,330.423872172972));
#37681=CARTESIAN_POINT('Ctrl Pts',(112.530658227063,1.67470836194228,330.373626057378));
#37682=CARTESIAN_POINT('Ctrl Pts',(112.522909536506,1.54496154225741,330.328693253558));
#37683=CARTESIAN_POINT('Ctrl Pts',(112.515160845948,1.41352923811787,330.289255031793));
#37684=CARTESIAN_POINT('Ctrl Pts',(112.50741376757,1.28212427956694,330.24982501548));
#37685=CARTESIAN_POINT('Ctrl Pts',(112.499666689192,1.14903490823484,330.215887419597));
#37686=CARTESIAN_POINT('Ctrl Pts',(112.491919610814,1.01476024226081,330.187573926466));
#37687=CARTESIAN_POINT('Ctrl Pts',(112.484172467509,0.880484450935939,330.159260196042));
#37688=CARTESIAN_POINT('Ctrl Pts',(112.476425324203,0.745023727619236,330.136570743032));
#37689=CARTESIAN_POINT('Ctrl Pts',(112.468678180897,0.608887927380469,330.119586231231));
#37690=CARTESIAN_POINT('Ctrl Pts',(112.460929295869,0.472721520923564,330.102597900951));
#37691=CARTESIAN_POINT('Ctrl Pts',(112.453180410841,0.335880123327505,330.091317112476));
#37692=CARTESIAN_POINT('Ctrl Pts',(112.445431525813,0.198878867246145,330.085772669212));
#37693=CARTESIAN_POINT('Ctrl Pts',(112.437674416038,0.0617321966159992,
330.080222341019));
#37694=CARTESIAN_POINT('Ctrl Pts',(112.429917306263,-0.0755742802706099,
330.08042053645));
#37695=CARTESIAN_POINT('Ctrl Pts',(112.422160196489,-0.212524714131034,
330.086343895999));
#37696=CARTESIAN_POINT('Ctrl Pts',(112.414398941562,-0.349548329924487,
330.092270420803));
#37697=CARTESIAN_POINT('Ctrl Pts',(112.406637686636,-0.486215134323129,
330.10392817254));
#37698=CARTESIAN_POINT('Ctrl Pts',(112.39887643171,-0.622015234114492,330.12124194994));
#37699=CARTESIAN_POINT('Ctrl Pts',(112.391102761305,-0.758032569808371,
330.13858342374));
#37700=CARTESIAN_POINT('Ctrl Pts',(112.383329090901,-0.893180044838139,
330.161598937727));
#37701=CARTESIAN_POINT('Ctrl Pts',(112.375555420496,-1.02695790033932,330.190162109444));
#37702=CARTESIAN_POINT('Ctrl Pts',(112.368143616319,-1.15450836448048,330.217395658645));
#37703=CARTESIAN_POINT('Ctrl Pts',(112.360731812142,-1.2808135722666,330.249671930603));
#37704=CARTESIAN_POINT('Ctrl Pts',(112.353320007965,-1.40545565252448,330.286839969693));
#37705=CARTESIAN_POINT('Ctrl Pts',(112.345544929187,-1.53620681242671,330.325829725096));
#37706=CARTESIAN_POINT('Ctrl Pts',(112.337769850408,-1.66554089074588,330.370326107294));
#37707=CARTESIAN_POINT('Ctrl Pts',(112.32999477163,-1.79295907588046,330.420209522836));
#37708=CARTESIAN_POINT('Ctrl Pts',(112.322229260581,-1.92022046482639,330.47003155366));
#37709=CARTESIAN_POINT('Ctrl Pts',(112.314463749532,-2.0455702910965,330.525227286713));
#37710=CARTESIAN_POINT('Ctrl Pts',(112.306698238483,-2.1685234040396,330.585626963131));
#37711=CARTESIAN_POINT('Ctrl Pts',(112.29894042696,-2.29135460861308,330.645966753095));
#37712=CARTESIAN_POINT('Ctrl Pts',(112.291182615438,-2.41179348035784,330.711500047047));
#37713=CARTESIAN_POINT('Ctrl Pts',(112.283424803916,-2.52937375241882,330.782008596135));
#37714=CARTESIAN_POINT('Ctrl Pts',(112.275672830393,-2.64686554159646,330.852464085305));
#37715=CARTESIAN_POINT('Ctrl Pts',(112.26792085687,-2.76150267905072,330.927887177076));
#37716=CARTESIAN_POINT('Ctrl Pts',(112.260168883347,-2.87284279498562,331.008013359516));
#37717=CARTESIAN_POINT('Ctrl Pts',(112.252420192789,-2.98413575831538,331.088105608471));
#37718=CARTESIAN_POINT('Ctrl Pts',(112.244671502232,-3.09213416064943,331.172896758781));
#37719=CARTESIAN_POINT('Ctrl Pts',(112.236922811674,-3.19642416406312,331.262078702555));
#37720=CARTESIAN_POINT('Ctrl Pts',(112.229175733296,-3.3006924690705,331.351242091281));
#37721=CARTESIAN_POINT('Ctrl Pts',(112.221428654918,-3.40125361296962,331.4447942025));
#37722=CARTESIAN_POINT('Ctrl Pts',(112.213681576541,-3.49772675982205,331.542386577981));
#37723=CARTESIAN_POINT('Ctrl Pts',(112.205934433235,-3.59420071521237,331.63997977138));
#37724=CARTESIAN_POINT('Ctrl Pts',(112.198187289929,-3.68658633042788,331.741613018601));
#37725=CARTESIAN_POINT('Ctrl Pts',(112.190440146623,-3.77453986172993,331.846901223445));
#37726=CARTESIAN_POINT('Ctrl Pts',(112.182691261595,-3.86251316685307,331.952213099313));
#37727=CARTESIAN_POINT('Ctrl Pts',(112.174942376567,-3.94605215474399,332.061181267999));
#37728=CARTESIAN_POINT('Ctrl Pts',(112.167193491539,-4.02485383616609,332.173388130641));
#37729=CARTESIAN_POINT('Ctrl Pts',(112.159436381764,-4.10373915850704,332.285714090807));
#37730=CARTESIAN_POINT('Ctrl Pts',(112.151679271989,-4.17787690502825,332.401285291446));
#37731=CARTESIAN_POINT('Ctrl Pts',(112.143922162215,-4.24700756358994,332.519655302723));
#37732=CARTESIAN_POINT('Ctrl Pts',(112.136160907288,-4.31617516336514,332.638088567149));
#37733=CARTESIAN_POINT('Ctrl Pts',(112.128399652362,-4.38033016102159,332.759323277013));
#37734=CARTESIAN_POINT('Ctrl Pts',(112.120638397436,-4.43925986243837,332.882889956511));
#37735=CARTESIAN_POINT('Ctrl Pts',(112.112864727032,-4.49828383217231,333.006654302425));
#37736=CARTESIAN_POINT('Ctrl Pts',(112.105091056627,-4.55206564894555,333.132757712671));
#37737=CARTESIAN_POINT('Ctrl Pts',(112.097317386222,-4.60044114226395,333.260711536557));
#37738=CARTESIAN_POINT('Ctrl Pts',(112.089905582045,-4.64656474473003,333.382709079158));
#37739=CARTESIAN_POINT('Ctrl Pts',(112.082493777868,-4.68777393438105,333.506388365759));
#37740=CARTESIAN_POINT('Ctrl Pts',(112.075081973691,-4.72396951895452,333.631316308825));
#37741=CARTESIAN_POINT('Ctrl Pts',(112.065386055773,-4.77131958496133,333.794743600301));
#37742=CARTESIAN_POINT('Ctrl Pts',(112.055690137855,-4.8102122349805,333.960723810202));
#37743=CARTESIAN_POINT('Ctrl Pts',(112.045994219937,-4.84041651357817,334.128477746939));
#37744=CARTESIAN_POINT('Ctrl Pts',(112.036441766059,-4.87017387958176,334.2937495404));
#37745=CARTESIAN_POINT('Ctrl Pts',(112.026889312181,-4.89149809061967,334.460743035106));
#37746=CARTESIAN_POINT('Ctrl Pts',(112.017336858303,-4.90421385269992,334.628692109583));
#37747=CARTESIAN_POINT('Ctrl Pts',(112.010403321699,-4.91344343945979,334.750595975379));
#37748=CARTESIAN_POINT('Ctrl Pts',(112.003469785094,-4.91813866033305,334.873002852249));
#37749=CARTESIAN_POINT('Ctrl Pts',(111.99653624849,-4.91824804283262,334.995612327148));
#37750=CARTESIAN_POINT('',(115.496536248451,-4.91824814755885,335.004268668875));
#37751=CARTESIAN_POINT('Ctrl Pts',(115.496536248451,-4.91824814755885,335.004268668875));
#37752=CARTESIAN_POINT('Ctrl Pts',(115.48716948192,-4.91810431769546,335.169985659309));
#37753=CARTESIAN_POINT('Ctrl Pts',(115.477802715389,-4.90958118452984,335.335335957126));
#37754=CARTESIAN_POINT('Ctrl Pts',(115.468435948858,-4.89281220431308,335.499571612309));
#37755=CARTESIAN_POINT('Ctrl Pts',(115.458942508385,-4.87581644436368,335.66602835175));
#37756=CARTESIAN_POINT('Ctrl Pts',(115.449449067914,-4.85035035781784,335.831340101219));
#37757=CARTESIAN_POINT('Ctrl Pts',(115.439955627442,-4.8166019771811,335.994750449065));
#37758=CARTESIAN_POINT('Ctrl Pts',(115.431283213287,-4.78577227589518,336.144028491924));
#37759=CARTESIAN_POINT('Ctrl Pts',(115.422610799133,-4.74803152286972,336.291720084277));
#37760=CARTESIAN_POINT('Ctrl Pts',(115.413938384978,-4.70355762201091,336.437264331612));
#37761=CARTESIAN_POINT('Ctrl Pts',(115.4061633062,-4.66368543917903,336.567749104204));
#37762=CARTESIAN_POINT('Ctrl Pts',(115.398388227421,-4.61831632860917,336.696779626366));
#37763=CARTESIAN_POINT('Ctrl Pts',(115.390613148643,-4.56757325085014,336.823857905819));
#37764=CARTESIAN_POINT('Ctrl Pts',(115.382847637594,-4.51689261567874,336.950779807359));
#37765=CARTESIAN_POINT('Ctrl Pts',(115.375082126545,-4.46085131487353,337.07575388666));
#37766=CARTESIAN_POINT('Ctrl Pts',(115.367316615496,-4.39962238096218,337.198296150985));
#37767=CARTESIAN_POINT('Ctrl Pts',(115.359558803974,-4.33845415571703,337.320716914299));
#37768=CARTESIAN_POINT('Ctrl Pts',(115.351800992452,-4.27210870691022,337.440710313559));
#37769=CARTESIAN_POINT('Ctrl Pts',(115.344043180929,-4.20080742837961,337.557811566979));
#37770=CARTESIAN_POINT('Ctrl Pts',(115.336291207406,-4.12955980632228,337.674824697992));
#37771=CARTESIAN_POINT('Ctrl Pts',(115.328539233883,-4.05336398022909,337.788949682732));
#37772=CARTESIAN_POINT('Ctrl Pts',(115.32078726036,-3.97248744451886,337.899745948465));
#37773=CARTESIAN_POINT('Ctrl Pts',(115.313038569803,-3.89164516006953,338.010495291914));
#37774=CARTESIAN_POINT('Ctrl Pts',(115.305289879245,-3.80612633860054,338.117918405125));
#37775=CARTESIAN_POINT('Ctrl Pts',(115.297541188688,-3.71624187673964,338.221603541106));
#37776=CARTESIAN_POINT('Ctrl Pts',(115.28979411031,-3.62637611609182,338.325267104528));
#37777=CARTESIAN_POINT('Ctrl Pts',(115.282047031932,-3.53214677761466,338.425193942495));
#37778=CARTESIAN_POINT('Ctrl Pts',(115.274299953554,-3.4339048844054,338.521005581841));
#37779=CARTESIAN_POINT('Ctrl Pts',(115.266552810248,-3.33566216783445,338.616818024181));
#37780=CARTESIAN_POINT('Ctrl Pts',(115.258805666943,-3.233407109285,338.708514926203));
#37781=CARTESIAN_POINT('Ctrl Pts',(115.251058523637,-3.12752711840107,338.795755153611));
#37782=CARTESIAN_POINT('Ctrl Pts',(115.243309638609,-3.02162332344737,338.883014994474));
#37783=CARTESIAN_POINT('Ctrl Pts',(115.235560753581,-2.91209327608224,338.965815918435));
#37784=CARTESIAN_POINT('Ctrl Pts',(115.227811868553,-2.7993566125464,339.04385776435));
#37785=CARTESIAN_POINT('Ctrl Pts',(115.220054758778,-2.68650028915093,339.121982444686));
#37786=CARTESIAN_POINT('Ctrl Pts',(115.212297649003,-2.57043087259344,339.195337733633));
#37787=CARTESIAN_POINT('Ctrl Pts',(115.204540539228,-2.45159653571134,339.263667140923));
#37788=CARTESIAN_POINT('Ctrl Pts',(115.196779284302,-2.3326986975592,339.332033061264));
#37789=CARTESIAN_POINT('Ctrl Pts',(115.189018029376,-2.21103334159486,339.395367568116));
#37790=CARTESIAN_POINT('Ctrl Pts',(115.18125677445,-2.08707136980889,339.453461143855));
#37791=CARTESIAN_POINT('Ctrl Pts',(115.173483104045,-1.96291109926726,339.511647650382));
#37792=CARTESIAN_POINT('Ctrl Pts',(115.165709433641,-1.83644723224796,339.56457632153));
#37793=CARTESIAN_POINT('Ctrl Pts',(115.157935763236,-1.70816951737834,339.612086291734));
#37794=CARTESIAN_POINT('Ctrl Pts',(115.150523959059,-1.58586316099757,339.657384661395));
#37795=CARTESIAN_POINT('Ctrl Pts',(115.143112154882,-1.4619082993518,339.69775736901));
#37796=CARTESIAN_POINT('Ctrl Pts',(115.135700350705,-1.33673868020804,339.733108150395));
#37797=CARTESIAN_POINT('Ctrl Pts',(115.127925271926,-1.20543412516908,339.77019157888));
#37798=CARTESIAN_POINT('Ctrl Pts',(115.120150193148,-1.07237777732891,339.801865545206));
#37799=CARTESIAN_POINT('Ctrl Pts',(115.11237511437,-0.938054950028191,339.827963957325));
#37800=CARTESIAN_POINT('Ctrl Pts',(115.104609603321,-0.803897415517961,
339.854030253686));
#37801=CARTESIAN_POINT('Ctrl Pts',(115.096844092272,-0.668476882513542,
339.874534573571));
#37802=CARTESIAN_POINT('Ctrl Pts',(115.089078581223,-0.5322939886632,339.889360507483));
#37803=CARTESIAN_POINT('Ctrl Pts',(115.0813207697,-0.396246120548597,339.904171741438));
#37804=CARTESIAN_POINT('Ctrl Pts',(115.073562958178,-0.259437781913177,
339.913315751678));
#37805=CARTESIAN_POINT('Ctrl Pts',(115.065805146656,-0.122379626587724,
339.91672719291));
#37806=CARTESIAN_POINT('Ctrl Pts',(115.058053173133,0.0145753881293899,
339.920136066923));
#37807=CARTESIAN_POINT('Ctrl Pts',(115.05030119961,0.151779456161817,339.917820948928));
#37808=CARTESIAN_POINT('Ctrl Pts',(115.042549226087,0.288717333918926,339.909768361501));
#37809=CARTESIAN_POINT('Ctrl Pts',(115.034800535529,0.425597218403598,339.901719184349));
#37810=CARTESIAN_POINT('Ctrl Pts',(115.027051844972,0.562210747440298,339.887937393407));
#37811=CARTESIAN_POINT('Ctrl Pts',(115.019303154414,0.698043430194164,339.868461608359));
#37812=CARTESIAN_POINT('Ctrl Pts',(115.011556076036,0.833847851823886,339.84898987541));
#37813=CARTESIAN_POINT('Ctrl Pts',(115.003808997659,0.968871363643894,339.823826560214));
#37814=CARTESIAN_POINT('Ctrl Pts',(114.996061919281,1.10260574075635,339.793062032037));
#37815=CARTESIAN_POINT('Ctrl Pts',(114.988314775975,1.23634123869161,339.762297246023));
#37816=CARTESIAN_POINT('Ctrl Pts',(114.980567632669,1.36878719944449,339.725931241024));
#37817=CARTESIAN_POINT('Ctrl Pts',(114.972820489363,1.49944710632027,339.684105190733));
#37818=CARTESIAN_POINT('Ctrl Pts',(114.965071604335,1.63013638831711,339.642269737057));
#37819=CARTESIAN_POINT('Ctrl Pts',(114.957322719307,1.75903844521842,339.594971914578));
#37820=CARTESIAN_POINT('Ctrl Pts',(114.949573834279,1.8856737758654,339.542402169944));
#37821=CARTESIAN_POINT('Ctrl Pts',(114.941816724504,2.01244351856081,339.48977662724));
#37822=CARTESIAN_POINT('Ctrl Pts',(114.93405961473,2.13694136736339,339.431868134599));
#37823=CARTESIAN_POINT('Ctrl Pts',(114.926302504955,2.25870910209775,339.368914768521));
#37824=CARTESIAN_POINT('Ctrl Pts',(114.918541250029,2.3805419056161,339.305927762177));
#37825=CARTESIAN_POINT('Ctrl Pts',(114.910779995102,2.49964134887912,339.237890704521));
#37826=CARTESIAN_POINT('Ctrl Pts',(114.903018740176,2.61557641195957,339.165086205074));
#37827=CARTESIAN_POINT('Ctrl Pts',(114.895245069772,2.73169693335781,339.092165242156));
#37828=CARTESIAN_POINT('Ctrl Pts',(114.887471399367,2.84464263704903,339.014461819395));
#37829=CARTESIAN_POINT('Ctrl Pts',(114.879697728962,2.95401321666414,338.932300723276));
#37830=CARTESIAN_POINT('Ctrl Pts',(114.872285924785,3.0582925694855,338.853964245947));
#37831=CARTESIAN_POINT('Ctrl Pts',(114.864874120608,3.15932192879822,338.771575947004));
#37832=CARTESIAN_POINT('Ctrl Pts',(114.857462316431,3.25678561819087,338.685448480124));
#37833=CARTESIAN_POINT('Ctrl Pts',(114.849687237653,3.35902629332978,338.595099649532));
#37834=CARTESIAN_POINT('Ctrl Pts',(114.841912158874,3.45766603193587,338.500350328631));
#37835=CARTESIAN_POINT('Ctrl Pts',(114.834137080096,3.55230253276615,338.401518745826));
#37836=CARTESIAN_POINT('Ctrl Pts',(114.826371569047,3.64682257735731,338.302808781575));
#37837=CARTESIAN_POINT('Ctrl Pts',(114.818606057998,3.73734891822672,338.200026830329));
#37838=CARTESIAN_POINT('Ctrl Pts',(114.810840546949,3.82351274038597,338.093530893107));
#37839=CARTESIAN_POINT('Ctrl Pts',(114.803082735426,3.90959113086463,337.987140546917));
#37840=CARTESIAN_POINT('Ctrl Pts',(114.795324923904,3.99131536625086,337.877043844904));
#37841=CARTESIAN_POINT('Ctrl Pts',(114.787567112382,4.0683541522042,337.763634844682));
#37842=CARTESIAN_POINT('Ctrl Pts',(114.779815138859,4.14533496402801,337.65031118833));
#37843=CARTESIAN_POINT('Ctrl Pts',(114.772063165336,4.21763712589514,337.533680517212));
#37844=CARTESIAN_POINT('Ctrl Pts',(114.764311191813,4.28497047648131,337.41416881725));
#37845=CARTESIAN_POINT('Ctrl Pts',(114.756562501255,4.35227531135357,337.294707730564));
#37846=CARTESIAN_POINT('Ctrl Pts',(114.748813810698,4.41461532877343,337.172368381598));
#37847=CARTESIAN_POINT('Ctrl Pts',(114.74106512014,4.47174458434419,337.047604315997));
#37848=CARTESIAN_POINT('Ctrl Pts',(114.733318041762,4.52886195369618,336.922866208601));
#37849=CARTESIAN_POINT('Ctrl Pts',(114.725570963384,4.58077055500555,336.795704743189));
#37850=CARTESIAN_POINT('Ctrl Pts',(114.717823885007,4.62727135206123,336.666596200912));
#37851=CARTESIAN_POINT('Ctrl Pts',(114.710076741701,4.67377253883835,336.537486576581));
#37852=CARTESIAN_POINT('Ctrl Pts',(114.702329598395,4.71486569851094,336.406430210587));
#37853=CARTESIAN_POINT('Ctrl Pts',(114.694582455089,4.75040085337575,336.273921031598));
#37854=CARTESIAN_POINT('Ctrl Pts',(114.686833570061,4.78594399729778,336.141382061731));
#37855=CARTESIAN_POINT('Ctrl Pts',(114.679084685033,4.8159265487081,336.007390006387));
#37856=CARTESIAN_POINT('Ctrl Pts',(114.671335800005,4.84024917266582,335.872451149926));
#37857=CARTESIAN_POINT('Ctrl Pts',(114.66357869023,4.86459761290791,335.73736906797));
#37858=CARTESIAN_POINT('Ctrl Pts',(114.655821580455,4.88327405569469,335.60133856271));
#37859=CARTESIAN_POINT('Ctrl Pts',(114.648064470681,4.89623073540441,335.464873798123));
#37860=CARTESIAN_POINT('Ctrl Pts',(114.640303215755,4.90919433874949,335.328336111129));
#37861=CARTESIAN_POINT('Ctrl Pts',(114.632541960828,4.9164320681337,335.191364092551));
#37862=CARTESIAN_POINT('Ctrl Pts',(114.624780705902,4.91794832631852,335.054473132468));
#37863=CARTESIAN_POINT('Ctrl Pts',(114.617007035498,4.91946701002228,334.917363191462));
#37864=CARTESIAN_POINT('Ctrl Pts',(114.609233365093,4.91524594518383,334.780334958961));
#37865=CARTESIAN_POINT('Ctrl Pts',(114.601459694688,4.90534162293875,334.64390082173));
#37866=CARTESIAN_POINT('Ctrl Pts',(114.594047890511,4.89589834927706,334.513817726412));
#37867=CARTESIAN_POINT('Ctrl Pts',(114.586636086334,4.88128905440621,334.384274946802));
#37868=CARTESIAN_POINT('Ctrl Pts',(114.579224282157,4.86160582485375,334.255707136775));
#37869=CARTESIAN_POINT('Ctrl Pts',(114.571449203379,4.84095786158752,334.120837835393));
#37870=CARTESIAN_POINT('Ctrl Pts',(114.5636741246,4.81466075876088,333.986615280559));
#37871=CARTESIAN_POINT('Ctrl Pts',(114.555899045822,4.78276441314124,333.853549987618));
#37872=CARTESIAN_POINT('Ctrl Pts',(114.548133534773,4.7509073180055,333.720648439992));
#37873=CARTESIAN_POINT('Ctrl Pts',(114.540368023724,4.71346477989057,333.588901697214));
#37874=CARTESIAN_POINT('Ctrl Pts',(114.532602512675,4.67053826253905,333.45881363857));
#37875=CARTESIAN_POINT('Ctrl Pts',(114.524844701153,4.62765430695445,333.328854562614));
#37876=CARTESIAN_POINT('Ctrl Pts',(114.51708688963,4.57929731452527,333.200551266761));
#37877=CARTESIAN_POINT('Ctrl Pts',(114.509329078108,4.52561937432772,333.074395590676));
#37878=CARTESIAN_POINT('Ctrl Pts',(114.501577104585,4.47198182848235,332.948334850737));
#37879=CARTESIAN_POINT('Ctrl Pts',(114.493825131062,4.41303145741679,332.824418871915));
#37880=CARTESIAN_POINT('Ctrl Pts',(114.486073157539,4.3489694588376,332.703122182484));
#37881=CARTESIAN_POINT('Ctrl Pts',(114.478324466982,4.28493459055289,332.581876862273));
#37882=CARTESIAN_POINT('Ctrl Pts',(114.470575776424,4.21579258250683,332.463248970102));
#37883=CARTESIAN_POINT('Ctrl Pts',(114.462827085866,4.1417917362836,332.347690765436));
#37884=CARTESIAN_POINT('Ctrl Pts',(114.455080007488,4.06780628655445,332.23215660362));
#37885=CARTESIAN_POINT('Ctrl Pts',(114.447332929111,3.9889642201012,332.119691187899));
#37886=CARTESIAN_POINT('Ctrl Pts',(114.439585850733,3.90555834199266,332.010719635131));
#37887=CARTESIAN_POINT('Ctrl Pts',(114.431838707427,3.82215176486263,331.901747169077));
#37888=CARTESIAN_POINT('Ctrl Pts',(114.424091564121,3.73418153735742,331.796268934772));
#37889=CARTESIAN_POINT('Ctrl Pts',(114.416344420815,3.64198185308981,331.694678344811));
#37890=CARTESIAN_POINT('Ctrl Pts',(114.408595535787,3.54976144037567,331.593064915128));
#37891=CARTESIAN_POINT('Ctrl Pts',(114.400846650759,3.45330994140741,331.495341158387));
#37892=CARTESIAN_POINT('Ctrl Pts',(114.393097765731,3.35299934567111,331.40186458698));
#37893=CARTESIAN_POINT('Ctrl Pts',(114.385340655956,3.2525822792321,331.308288798574));
#37894=CARTESIAN_POINT('Ctrl Pts',(114.377583546182,3.14829822012146,331.218969467565));
#37895=CARTESIAN_POINT('Ctrl Pts',(114.369826436407,3.04055369107716,331.134225004714));
#37896=CARTESIAN_POINT('Ctrl Pts',(114.362065181481,2.93275158680162,331.049435257132));
#37897=CARTESIAN_POINT('Ctrl Pts',(114.354303926554,2.8214856448798,330.969225477377));
#37898=CARTESIAN_POINT('Ctrl Pts',(114.346542671628,2.70719165041267,330.893870870219));
#37899=CARTESIAN_POINT('Ctrl Pts',(114.338769001224,2.59271482280271,330.818395720248));
#37900=CARTESIAN_POINT('Ctrl Pts',(114.330995330819,2.47520059833398,330.747791464438));
#37901=CARTESIAN_POINT('Ctrl Pts',(114.323221660414,2.35511042456542,330.682287880068));
#37902=CARTESIAN_POINT('Ctrl Pts',(114.315809856237,2.24061047727715,330.61983350331));
#37903=CARTESIAN_POINT('Ctrl Pts',(114.30839805206,2.12376926249241,330.562015739833));
#37904=CARTESIAN_POINT('Ctrl Pts',(114.300986247883,2.00500212323059,330.508992368261));
#37905=CARTESIAN_POINT('Ctrl Pts',(114.293211169104,1.88041385268503,330.4533701633));
#37906=CARTESIAN_POINT('Ctrl Pts',(114.285436090326,1.7533123715449,330.402848431981));
#37907=CARTESIAN_POINT('Ctrl Pts',(114.277661011548,1.62415398506101,330.357661484197));
#37908=CARTESIAN_POINT('Ctrl Pts',(114.269895500499,1.49515453619431,330.312530141828));
#37909=CARTESIAN_POINT('Ctrl Pts',(114.26212998945,1.36410358367196,330.272720648787));
#37910=CARTESIAN_POINT('Ctrl Pts',(114.254364478401,1.2314797581886,330.238420360041));
#37911=CARTESIAN_POINT('Ctrl Pts',(114.246606666878,1.09898742961442,330.204154080132));
#37912=CARTESIAN_POINT('Ctrl Pts',(114.238848855356,0.964925707573891,330.175386231289));
#37913=CARTESIAN_POINT('Ctrl Pts',(114.231091043834,0.829790494659489,330.152255081229));
#37914=CARTESIAN_POINT('Ctrl Pts',(114.223339070311,0.694756975278188,330.129141338092));
#37915=CARTESIAN_POINT('Ctrl Pts',(114.215587096788,0.558651956700592,330.111655916335));
#37916=CARTESIAN_POINT('Ctrl Pts',(114.207835123265,0.421983359498487,330.099886418989));
#37917=CARTESIAN_POINT('Ctrl Pts',(114.200086432707,0.285372641528438,330.088121906033));
#37918=CARTESIAN_POINT('Ctrl Pts',(114.19233774215,0.148199208265827,330.082068536358));
#37919=CARTESIAN_POINT('Ctrl Pts',(114.184589051592,0.0109777445768436,
330.081762251413));
#37920=CARTESIAN_POINT('Ctrl Pts',(114.176841973214,-0.12621516904043,330.081456030193));
#37921=CARTESIAN_POINT('Ctrl Pts',(114.169094894836,-0.263455702579121,
330.086894516185));
#37922=CARTESIAN_POINT('Ctrl Pts',(114.161347816458,-0.400227912580374,
330.098061538484));
#37923=CARTESIAN_POINT('Ctrl Pts',(114.153600673153,-0.537001268864482,
330.109228654373));
#37924=CARTESIAN_POINT('Ctrl Pts',(114.145853529847,-0.673305904204498,
330.126124370523));
#37925=CARTESIAN_POINT('Ctrl Pts',(114.138106386541,-0.808630138217336,
330.148680554523));
#37926=CARTESIAN_POINT('Ctrl Pts',(114.130357501513,-0.943984795990994,
330.171241809632));
#37927=CARTESIAN_POINT('Ctrl Pts',(114.122608616485,-1.07835822835649,330.199466000656));
#37928=CARTESIAN_POINT('Ctrl Pts',(114.114859731457,-1.21124849066157,330.233233784171));
#37929=CARTESIAN_POINT('Ctrl Pts',(114.107102621682,-1.34427980406407,330.26703740916));
#37930=CARTESIAN_POINT('Ctrl Pts',(114.099345511907,-1.47582442325646,330.306396284118));
#37931=CARTESIAN_POINT('Ctrl Pts',(114.091588402132,-1.60539459705742,330.351140865735));
#37932=CARTESIAN_POINT('Ctrl Pts',(114.083827147206,-1.73503400901633,330.395909357426));
#37933=CARTESIAN_POINT('Ctrl Pts',(114.07606589228,-1.86269650962508,330.446069147481));
#37934=CARTESIAN_POINT('Ctrl Pts',(114.068304637354,-1.98791484499822,330.501402704005));
#37935=CARTESIAN_POINT('Ctrl Pts',(114.060530966949,-2.11333348889947,330.556824776186));
#37936=CARTESIAN_POINT('Ctrl Pts',(114.052757296545,-2.23629980371065,330.617436980507));
#37937=CARTESIAN_POINT('Ctrl Pts',(114.04498362614,-2.35637084906335,330.682975621544));
#37938=CARTESIAN_POINT('Ctrl Pts',(114.037571821963,-2.470852558366,330.745463423072));
#37939=CARTESIAN_POINT('Ctrl Pts',(114.030160017786,-2.58270223482796,330.812429183881));
#37940=CARTESIAN_POINT('Ctrl Pts',(114.022748213609,-2.69156243309646,330.883609016232));
#37941=CARTESIAN_POINT('Ctrl Pts',(114.014983182136,-2.80561062507305,330.958181094127));
#37942=CARTESIAN_POINT('Ctrl Pts',(114.007218150664,-2.91673988008223,331.037615837191));
#37943=CARTESIAN_POINT('Ctrl Pts',(113.999453119191,-3.02450689708768,331.121657429782));
#37944=CARTESIAN_POINT('Ctrl Pts',(113.99169765018,-3.13214120143334,331.205595527039));
#37945=CARTESIAN_POINT('Ctrl Pts',(113.983942181169,-3.23642119965978,331.294128947552));
#37946=CARTESIAN_POINT('Ctrl Pts',(113.976186712158,-3.33693093749876,331.386957655816));
#37947=CARTESIAN_POINT('Ctrl Pts',(113.968438926609,-3.43734109880006,331.479694397257));
#37948=CARTESIAN_POINT('Ctrl Pts',(113.960691141061,-3.53398814660308,331.576717694108));
#37949=CARTESIAN_POINT('Ctrl Pts',(113.952943355512,-3.62648801736549,331.677686390118));
#37950=CARTESIAN_POINT('Ctrl Pts',(113.945201381181,-3.71891850869959,331.778579354667));
#37951=CARTESIAN_POINT('Ctrl Pts',(113.93745940685,-3.80720775043846,331.883411540521));
#37952=CARTESIAN_POINT('Ctrl Pts',(113.92971743252,-3.89100775402714,331.991804241642));
#37953=CARTESIAN_POINT('Ctrl Pts',(113.921978697296,-3.97477269715578,332.100151593148));
#37954=CARTESIAN_POINT('Ctrl Pts',(113.914239962072,-4.05405189823505,332.212056187804));
#37955=CARTESIAN_POINT('Ctrl Pts',(113.906501226849,-4.12853713695404,332.327105656542));
#37956=CARTESIAN_POINT('Ctrl Pts',(113.898764059831,-4.20300728171342,332.442131811236));
#37957=CARTESIAN_POINT('Ctrl Pts',(113.891026892812,-4.27268518341832,332.560301243582));
#37958=CARTESIAN_POINT('Ctrl Pts',(113.883289725794,-4.33730575999222,332.681172320581));
#37959=CARTESIAN_POINT('Ctrl Pts',(113.875552440266,-4.40192732635598,332.802045248957));
#37960=CARTESIAN_POINT('Ctrl Pts',(113.867815154738,-4.4614912284773,332.925619558689));
#37961=CARTESIAN_POINT('Ctrl Pts',(113.860077869211,-4.51577839106033,333.051429091531));
#37962=CARTESIAN_POINT('Ctrl Pts',(113.85233877873,-4.57007821774068,333.177267973193));
#37963=CARTESIAN_POINT('Ctrl Pts',(113.84459968825,-4.61909870032521,333.305342755621));
#37964=CARTESIAN_POINT('Ctrl Pts',(113.83686059777,-4.66266910488782,333.435167778698));
#37965=CARTESIAN_POINT('Ctrl Pts',(113.829113285313,-4.70628579846462,333.565130727332));
#37966=CARTESIAN_POINT('Ctrl Pts',(113.821365972855,-4.74444072371911,333.69684725854));
#37967=CARTESIAN_POINT('Ctrl Pts',(113.813618660398,-4.77701305493719,333.829816537692));
#37968=CARTESIAN_POINT('Ctrl Pts',(113.805867127408,-4.8096031307091,333.962858255028));
#37969=CARTESIAN_POINT('Ctrl Pts',(113.798115594417,-4.83660447590441,334.097153696005));
#37970=CARTESIAN_POINT('Ctrl Pts',(113.790364061427,-4.8579477161762,334.232193351554));
#37971=CARTESIAN_POINT('Ctrl Pts',(113.782600302031,-4.8793246208999,334.367446003626));
#37972=CARTESIAN_POINT('Ctrl Pts',(113.774836542635,-4.8950255443115,334.503444826225));
#37973=CARTESIAN_POINT('Ctrl Pts',(113.767072783239,-4.90503308943813,334.639675904196));
#37974=CARTESIAN_POINT('Ctrl Pts',(113.760227271669,-4.91385700610772,334.759794441221));
#37975=CARTESIAN_POINT('Ctrl Pts',(113.753381760099,-4.91825543465756,334.880093343675));
#37976=CARTESIAN_POINT('Ctrl Pts',(113.746536248529,-4.91824999495766,335.000222708279));
#37977=CARTESIAN_POINT('',(117.246536248536,-4.9182494855724,334.997750518554));
#37978=CARTESIAN_POINT('Ctrl Pts',(117.24653624849,-4.91824948557278,334.997750519371));
#37979=CARTESIAN_POINT('Ctrl Pts',(117.238656580834,-4.91831343288592,335.137564499501));
#37980=CARTESIAN_POINT('Ctrl Pts',(117.230776913178,-4.91241116676489,335.277359185831));
#37981=CARTESIAN_POINT('Ctrl Pts',(117.222897245522,-4.90057407742763,335.416601457204));
#37982=CARTESIAN_POINT('Ctrl Pts',(117.215014674906,-4.88873262717076,335.555895027028));
#37983=CARTESIAN_POINT('Ctrl Pts',(117.20713210429,-4.87095202893947,335.694635405755));
#37984=CARTESIAN_POINT('Ctrl Pts',(117.199249533674,-4.84731549143901,335.832295373624));
#37985=CARTESIAN_POINT('Ctrl Pts',(117.191362594417,-4.82366585420909,335.970031634745));
#37986=CARTESIAN_POINT('Ctrl Pts',(117.18347565516,-4.79415387465817,336.106685925741));
#37987=CARTESIAN_POINT('Ctrl Pts',(117.175588715903,-4.75891369292042,336.241742133389));
#37988=CARTESIAN_POINT('Ctrl Pts',(117.167690165343,-4.72362162991005,336.376997173382));
#37989=CARTESIAN_POINT('Ctrl Pts',(117.159791614782,-4.68258460953353,336.510649068882));
#37990=CARTESIAN_POINT('Ctrl Pts',(117.151893064222,-4.63598670297276,336.642196806829));
#37991=CARTESIAN_POINT('Ctrl Pts',(117.14398847896,-4.58935319438067,336.773845050722));
#37992=CARTESIAN_POINT('Ctrl Pts',(117.136083893698,-4.5371504680916,336.903385587463));
#37993=CARTESIAN_POINT('Ctrl Pts',(117.128179308437,-4.47961018621695,337.030338799817));
#37994=CARTESIAN_POINT('Ctrl Pts',(117.120260085878,-4.42196335426404,337.157527097476));
#37995=CARTESIAN_POINT('Ctrl Pts',(117.11234086332,-4.35895937967084,337.282118162656));
#37996=CARTESIAN_POINT('Ctrl Pts',(117.104421640762,-4.29087578559953,337.40365722495));
#37997=CARTESIAN_POINT('Ctrl Pts',(117.097403290715,-4.23053722432006,337.511370283553));
#37998=CARTESIAN_POINT('Ctrl Pts',(117.090384940669,-4.16620974209067,337.616686482591));
#37999=CARTESIAN_POINT('Ctrl Pts',(117.083366590622,-4.09811362679982,337.71931016332));
#38000=CARTESIAN_POINT('Ctrl Pts',(117.075591511844,-4.02267528910245,337.832998878889));
#38001=CARTESIAN_POINT('Ctrl Pts',(117.067816433065,-3.94238327911094,337.943725682216));
#38002=CARTESIAN_POINT('Ctrl Pts',(117.060041354287,-3.85749750858327,338.051048349957));
#38003=CARTESIAN_POINT('Ctrl Pts',(117.052275843238,-3.77271619540029,338.158238950323));
#38004=CARTESIAN_POINT('Ctrl Pts',(117.044510332189,-3.68335260952253,338.262033446382));
#38005=CARTESIAN_POINT('Ctrl Pts',(117.03674482114,-3.58971066051248,338.362017316479));
#38006=CARTESIAN_POINT('Ctrl Pts',(117.028987009617,-3.49616155776767,338.461902052277));
#38007=CARTESIAN_POINT('Ctrl Pts',(117.021229198095,-3.39834279920199,338.557983397584));
#38008=CARTESIAN_POINT('Ctrl Pts',(117.013471386573,-3.29659916595578,338.6498790393));
#38009=CARTESIAN_POINT('Ctrl Pts',(117.00571941305,-3.19493209802014,338.741705526631));
#38010=CARTESIAN_POINT('Ctrl Pts',(116.997967439527,-3.08934632328922,338.829352319102));
#38011=CARTESIAN_POINT('Ctrl Pts',(116.990215466004,-2.98022390189834,338.91247345768));
#38012=CARTESIAN_POINT('Ctrl Pts',(116.982466775446,-2.87114769391747,338.995559394408));
#38013=CARTESIAN_POINT('Ctrl Pts',(116.974718084889,-2.75853812853333,339.074123252902));
#38014=CARTESIAN_POINT('Ctrl Pts',(116.966969394331,-2.64281064164036,339.147859083302));
#38015=CARTESIAN_POINT('Ctrl Pts',(116.959222315953,-2.52710723281754,339.221579572347));
#38016=CARTESIAN_POINT('Ctrl Pts',(116.951475237575,-2.40828752225627,339.29047382144));
#38017=CARTESIAN_POINT('Ctrl Pts',(116.943728159198,-2.28679591309402,339.354279218695));
#38018=CARTESIAN_POINT('Ctrl Pts',(116.935981015892,-2.16530328571512,339.4180851507));
#38019=CARTESIAN_POINT('Ctrl Pts',(116.928233872586,-2.04113906112369,339.476801964059));
#38020=CARTESIAN_POINT('Ctrl Pts',(116.92048672928,-1.91477186555856,339.530213214118));
#38021=CARTESIAN_POINT('Ctrl Pts',(116.912737844252,-1.78837625996547,339.583636472159));
#38022=CARTESIAN_POINT('Ctrl Pts',(116.904988959224,-1.65977705782248,339.631751641209));
#38023=CARTESIAN_POINT('Ctrl Pts',(116.897240074196,-1.52946208463444,339.674390740424));
#38024=CARTESIAN_POINT('Ctrl Pts',(116.889482964421,-1.39900879378701,339.71707509722));
#38025=CARTESIAN_POINT('Ctrl Pts',(116.881725854646,-1.26683646608281,339.754271651707));
#38026=CARTESIAN_POINT('Ctrl Pts',(116.873968744872,-1.13344782004771,339.78586241985));
#38027=CARTESIAN_POINT('Ctrl Pts',(116.866207489946,-0.999987895385022,
339.817470069089));
#38028=CARTESIAN_POINT('Ctrl Pts',(116.858446235019,-0.865310740879716,
339.843465889031));
#38029=CARTESIAN_POINT('Ctrl Pts',(116.850684980093,-0.729927460062221,
339.863783400353));
#38030=CARTESIAN_POINT('Ctrl Pts',(116.842911309689,-0.59432761011691,339.884133413071));
#38031=CARTESIAN_POINT('Ctrl Pts',(116.835137639284,-0.458019765479544,
339.898786923957));
#38032=CARTESIAN_POINT('Ctrl Pts',(116.827363968879,-0.321519214412819,
339.90772946048));
#38033=CARTESIAN_POINT('Ctrl Pts',(116.819952164702,-0.191372796838107,
339.916255719777));
#38034=CARTESIAN_POINT('Ctrl Pts',(116.812540360525,-0.0610514977543804,
339.91959072367));
#38035=CARTESIAN_POINT('Ctrl Pts',(116.805128556348,0.0690014971030674,
339.917765941553));
#38036=CARTESIAN_POINT('Ctrl Pts',(116.79735347757,0.205428776646209,339.915851721428));
#38037=CARTESIAN_POINT('Ctrl Pts',(116.789578398791,0.341991921577325,339.908253084054));
#38038=CARTESIAN_POINT('Ctrl Pts',(116.781803320013,0.478178403686709,339.894949282347));
#38039=CARTESIAN_POINT('Ctrl Pts',(116.774037808964,0.614197299659894,339.881661851815));
#38040=CARTESIAN_POINT('Ctrl Pts',(116.766272297915,0.749840069754946,339.862683263506));
#38041=CARTESIAN_POINT('Ctrl Pts',(116.758506786866,0.884593670964688,339.838044760003));
#38042=CARTESIAN_POINT('Ctrl Pts',(116.750748975343,1.01921366358614,339.813430685647));
#38043=CARTESIAN_POINT('Ctrl Pts',(116.742991163821,1.15294585975989,339.78316793379));
#38044=CARTESIAN_POINT('Ctrl Pts',(116.735233352299,1.28528218338405,339.747339546691));
#38045=CARTESIAN_POINT('Ctrl Pts',(116.727481378776,1.41751891972823,339.711538121589));
#38046=CARTESIAN_POINT('Ctrl Pts',(116.719729405253,1.54836149859689,339.670179499622));
#38047=CARTESIAN_POINT('Ctrl Pts',(116.71197743173,1.6773122409977,339.623397745025));
#38048=CARTESIAN_POINT('Ctrl Pts',(116.704228741172,1.80620837268263,339.576635802528));
#38049=CARTESIAN_POINT('Ctrl Pts',(116.696480050615,1.93321389474144,339.524455428401));
#38050=CARTESIAN_POINT('Ctrl Pts',(116.688731360057,2.05784671120971,339.467040404526));
#38051=CARTESIAN_POINT('Ctrl Pts',(116.680984281679,2.18245359677939,339.409637326325));
#38052=CARTESIAN_POINT('Ctrl Pts',(116.673237203301,2.30468840389376,339.347001928142));
#38053=CARTESIAN_POINT('Ctrl Pts',(116.665490124924,2.42408980457841,339.279365803696));
#38054=CARTESIAN_POINT('Ctrl Pts',(116.657742981618,2.54349220596179,339.211729112393));
#38055=CARTESIAN_POINT('Ctrl Pts',(116.649995838312,2.66006081345148,339.139091803885));
#38056=CARTESIAN_POINT('Ctrl Pts',(116.642248695006,2.77336001357305,339.061730825352));
#38057=CARTESIAN_POINT('Ctrl Pts',(116.634499809978,2.88668468576037,338.984352454428));
#38058=CARTESIAN_POINT('Ctrl Pts',(116.62675092495,2.99673816520765,338.902248520623));
#38059=CARTESIAN_POINT('Ctrl Pts',(116.619002039922,3.10311520286695,338.815738342737));
#38060=CARTESIAN_POINT('Ctrl Pts',(116.611244930147,3.20960515021311,338.729136342055));
#38061=CARTESIAN_POINT('Ctrl Pts',(116.603487820372,3.31241055700217,338.638119001886));
#38062=CARTESIAN_POINT('Ctrl Pts',(116.595730710598,3.4111601581012,338.543045221033));
#38063=CARTESIAN_POINT('Ctrl Pts',(116.587969455671,3.50996252782953,338.447920635791));
#38064=CARTESIAN_POINT('Ctrl Pts',(116.580208200745,3.6047045034919,338.348735573167));
#38065=CARTESIAN_POINT('Ctrl Pts',(116.572446945819,3.69505359375842,338.245883855247));
#38066=CARTESIAN_POINT('Ctrl Pts',(116.564673275414,3.78554721312473,338.142867608097));
#38067=CARTESIAN_POINT('Ctrl Pts',(116.55689960501,3.87163365912346,338.0361732891));
#38068=CARTESIAN_POINT('Ctrl Pts',(116.549125934605,3.95302190944854,337.926226383231));
#38069=CARTESIAN_POINT('Ctrl Pts',(116.541714130428,4.0306215171394,337.821397532284));
#38070=CARTESIAN_POINT('Ctrl Pts',(116.534302326251,4.10395032583083,337.713612333572));
#38071=CARTESIAN_POINT('Ctrl Pts',(116.526890522074,4.17279496557417,337.603260501329));
#38072=CARTESIAN_POINT('Ctrl Pts',(116.519115443296,4.24501388618956,337.487499997065));
#38073=CARTESIAN_POINT('Ctrl Pts',(116.511340364517,4.31252618362558,337.368549076353));
#38074=CARTESIAN_POINT('Ctrl Pts',(116.503565285739,4.37503705279395,337.246827507661));
#38075=CARTESIAN_POINT('Ctrl Pts',(116.49579977469,4.43747099835817,337.125255725107));
#38076=CARTESIAN_POINT('Ctrl Pts',(116.488034263641,4.4949155846381,337.000920422798));
#38077=CARTESIAN_POINT('Ctrl Pts',(116.480268752592,4.54711944717708,336.874269936696));
#38078=CARTESIAN_POINT('Ctrl Pts',(116.47251094107,4.5992715494343,336.74774502492));
#38079=CARTESIAN_POINT('Ctrl Pts',(116.464753129547,4.64619312067145,336.6189098566));
#38080=CARTESIAN_POINT('Ctrl Pts',(116.456995318025,4.68767904376461,336.488236622702));
#38081=CARTESIAN_POINT('Ctrl Pts',(116.449243344502,4.72913374738513,336.357661724555));
#38082=CARTESIAN_POINT('Ctrl Pts',(116.441491370979,4.76516082699687,336.225251885076));
#38083=CARTESIAN_POINT('Ctrl Pts',(116.433739397456,4.79560369741601,336.091498162999));
#38084=CARTESIAN_POINT('Ctrl Pts',(116.425990706898,4.8260336752614,335.957801085702));
#38085=CARTESIAN_POINT('Ctrl Pts',(116.418242016341,4.85088406099985,335.82276163811));
#38086=CARTESIAN_POINT('Ctrl Pts',(116.410493325783,4.87004851094776,335.686884679925));
#38087=CARTESIAN_POINT('Ctrl Pts',(116.402746247405,4.88920897357179,335.551035992076));
#38088=CARTESIAN_POINT('Ctrl Pts',(116.394999169028,4.90268579893338,335.414350527033));
#38089=CARTESIAN_POINT('Ctrl Pts',(116.38725209065,4.91042408809411,335.277341553982));
#38090=CARTESIAN_POINT('Ctrl Pts',(116.379504947344,4.91816244210915,335.140331432664));
#38091=CARTESIAN_POINT('Ctrl Pts',(116.371757804038,4.9201621419538,335.002998188182));
#38092=CARTESIAN_POINT('Ctrl Pts',(116.364010660732,4.91642034297385,334.865858009211));
#38093=CARTESIAN_POINT('Ctrl Pts',(116.356261775704,4.91267770275806,334.728686998216));
#38094=CARTESIAN_POINT('Ctrl Pts',(116.348512890676,4.9031910058071,334.591709529757));
#38095=CARTESIAN_POINT('Ctrl Pts',(116.340764005648,4.88800947059981,334.455439188128));
#38096=CARTESIAN_POINT('Ctrl Pts',(116.333006895873,4.87281182155416,334.31902420775));
#38097=CARTESIAN_POINT('Ctrl Pts',(116.325249786099,4.85190730302309,334.183318242585));
#38098=CARTESIAN_POINT('Ctrl Pts',(116.317492676324,4.82539680779922,334.048827718139));
#38099=CARTESIAN_POINT('Ctrl Pts',(116.309731421398,4.79887214621431,333.914265326256));
#38100=CARTESIAN_POINT('Ctrl Pts',(116.301970166472,4.76673563035788,333.780920049067));
#38101=CARTESIAN_POINT('Ctrl Pts',(116.294208911545,4.72913850348643,333.649284605351));
#38102=CARTESIAN_POINT('Ctrl Pts',(116.286435241141,4.69148123346491,333.517438587825));
#38103=CARTESIAN_POINT('Ctrl Pts',(116.278661570736,4.64834601996584,333.387308240683));
#38104=CARTESIAN_POINT('Ctrl Pts',(116.270887900331,4.59993317351458,333.259368545125));
#38105=CARTESIAN_POINT('Ctrl Pts',(116.263476096154,4.55377395671318,333.137384473176));
#38106=CARTESIAN_POINT('Ctrl Pts',(116.256064291977,4.50281750960875,333.017391957809));
#38107=CARTESIAN_POINT('Ctrl Pts',(116.2486524878,4.44727608449179,332.899781323098));
#38108=CARTESIAN_POINT('Ctrl Pts',(116.240877409022,4.38901240868031,332.776406240836));
#38109=CARTESIAN_POINT('Ctrl Pts',(116.233102330243,4.32551881974418,332.655262541011));
#38110=CARTESIAN_POINT('Ctrl Pts',(116.225327251465,4.25698877399473,332.536825292314));
#38111=CARTESIAN_POINT('Ctrl Pts',(116.217561740416,4.1885430588296,332.418533788193));
#38112=CARTESIAN_POINT('Ctrl Pts',(116.209796229367,4.11507341234639,332.302942443626));
#38113=CARTESIAN_POINT('Ctrl Pts',(116.202030718318,4.03682082209073,332.190505256664));
#38114=CARTESIAN_POINT('Ctrl Pts',(116.194272906796,3.95864581950602,332.078179551499));
#38115=CARTESIAN_POINT('Ctrl Pts',(116.186515095274,3.87569753244349,331.96900209908));
#38116=CARTESIAN_POINT('Ctrl Pts',(116.178757283752,3.78826203571425,331.863400916396));
#38117=CARTESIAN_POINT('Ctrl Pts',(116.171005310229,3.70089233696875,331.757879201951));
#38118=CARTESIAN_POINT('Ctrl Pts',(116.163253336706,3.60904239812246,331.655928700284));
#38119=CARTESIAN_POINT('Ctrl Pts',(116.155501363183,3.51304042371204,331.557946827275));
#38120=CARTESIAN_POINT('Ctrl Pts',(116.147752672625,3.41707910619497,331.460006449648));
#38121=CARTESIAN_POINT('Ctrl Pts',(116.140003982067,3.316969523412,331.366031636466));
#38122=CARTESIAN_POINT('Ctrl Pts',(116.13225529151,3.21307867398919,331.276385022957));
#38123=CARTESIAN_POINT('Ctrl Pts',(116.124508213132,3.10920943992531,331.186757061175));
#38124=CARTESIAN_POINT('Ctrl Pts',(116.116761134754,3.00156079981723,331.101455763068));
#38125=CARTESIAN_POINT('Ctrl Pts',(116.109014056376,2.89053466370803,331.020805053732));
#38126=CARTESIAN_POINT('Ctrl Pts',(116.10126691307,2.77950759709302,330.940153668466));
#38127=CARTESIAN_POINT('Ctrl Pts',(116.093519769765,2.6651032942607,330.864153179436));
#38128=CARTESIAN_POINT('Ctrl Pts',(116.085772626459,2.54775428987424,330.793085318083));
#38129=CARTESIAN_POINT('Ctrl Pts',(116.078023741431,2.4303789029403,330.722001479166));
#38130=CARTESIAN_POINT('Ctrl Pts',(116.070274856403,2.31005783135975,330.655852677073));
#38131=CARTESIAN_POINT('Ctrl Pts',(116.062525971375,2.18724959406665,330.594875452867));
#38132=CARTESIAN_POINT('Ctrl Pts',(116.0547688616,2.06431100684147,330.533833506805));
#38133=CARTESIAN_POINT('Ctrl Pts',(116.047011751825,1.93888033109602,330.477974277858));
#38134=CARTESIAN_POINT('Ctrl Pts',(116.03925464205,1.81143802972191,330.427486979026));
#38135=CARTESIAN_POINT('Ctrl Pts',(116.031493387124,1.68392762725658,330.376972701395));
#38136=CARTESIAN_POINT('Ctrl Pts',(116.023732132198,1.55440382614832,330.331836202344));
#38137=CARTESIAN_POINT('Ctrl Pts',(116.015970877272,1.42336281053587,330.292216936595));
#38138=CARTESIAN_POINT('Ctrl Pts',(116.008197206867,1.29211217200488,330.252534292933));
#38139=CARTESIAN_POINT('Ctrl Pts',(116.000423536463,1.15933984776138,330.218386616497));
#38140=CARTESIAN_POINT('Ctrl Pts',(115.992649866058,1.02555365914964,330.189862501476));
#38141=CARTESIAN_POINT('Ctrl Pts',(115.985238061881,0.897995249804329,330.162666190872));
#38142=CARTESIAN_POINT('Ctrl Pts',(115.977826257704,0.769515526294496,330.140581719116));
#38143=CARTESIAN_POINT('Ctrl Pts',(115.970414453527,0.640557582355683,330.123641825482));
#38144=CARTESIAN_POINT('Ctrl Pts',(115.962639374748,0.505279025439115,330.105871657201));
#38145=CARTESIAN_POINT('Ctrl Pts',(115.95486429597,0.36904667953373,330.093706963514));
#38146=CARTESIAN_POINT('Ctrl Pts',(115.947089217191,0.232364730348951,330.087242149811));
#38147=CARTESIAN_POINT('Ctrl Pts',(115.939323706142,0.0958509770039653,
330.080785291474));
#38148=CARTESIAN_POINT('Ctrl Pts',(115.931558195093,-0.0411108920754093,
330.080014375433));
#38149=CARTESIAN_POINT('Ctrl Pts',(115.923792684044,-0.178008688054912,
330.084972434515));
#38150=CARTESIAN_POINT('Ctrl Pts',(115.916034872522,-0.314770749470483,
330.089925577667));
#38151=CARTESIAN_POINT('Ctrl Pts',(115.908277061,-0.451468476109896,330.100596377777));
#38152=CARTESIAN_POINT('Ctrl Pts',(115.900519249478,-0.587587127858695,
330.116975892987));
#38153=CARTESIAN_POINT('Ctrl Pts',(115.892767275955,-0.723603346005389,
330.133343082091));
#38154=CARTESIAN_POINT('Ctrl Pts',(115.885015302432,-0.859040970132618,
330.155410388829));
#38155=CARTESIAN_POINT('Ctrl Pts',(115.877263328909,-0.993388194442216,
330.183116883539));
#38156=CARTESIAN_POINT('Ctrl Pts',(115.869514638351,-1.12767852262311,330.210811644533));
#38157=CARTESIAN_POINT('Ctrl Pts',(115.861765947794,-1.26087898742259,330.244140764753));
#38158=CARTESIAN_POINT('Ctrl Pts',(115.854017257236,-1.39248603712727,330.282991869956));
#38159=CARTESIAN_POINT('Ctrl Pts',(115.846270178858,-1.52406570488586,330.321834891861));
#38160=CARTESIAN_POINT('Ctrl Pts',(115.83852310048,-1.65405224232759,330.366197502918));
#38161=CARTESIAN_POINT('Ctrl Pts',(115.830776022102,-1.78195575734221,330.415917022852));
#38162=CARTESIAN_POINT('Ctrl Pts',(115.823028878797,-1.9098603443114,330.465636959484));
#38163=CARTESIAN_POINT('Ctrl Pts',(115.815281735491,-2.03568150971615,330.520713752924));
#38164=CARTESIAN_POINT('Ctrl Pts',(115.807534592185,-2.15894827025205,330.580936136592));
#38165=CARTESIAN_POINT('Ctrl Pts',(115.799785707157,-2.28224274377249,330.641172059531));
#38166=CARTESIAN_POINT('Ctrl Pts',(115.792036822129,-2.40298131852899,330.706555703131));
#38167=CARTESIAN_POINT('Ctrl Pts',(115.784287937101,-2.52071695119039,330.776829494979));
#38168=CARTESIAN_POINT('Ctrl Pts',(115.776530827326,-2.63857754966897,330.847177876156));
#38169=CARTESIAN_POINT('Ctrl Pts',(115.768773717551,-2.75342850285078,330.922426573351));
#38170=CARTESIAN_POINT('Ctrl Pts',(115.761016607776,-2.86485069144925,331.00227394908));
#38171=CARTESIAN_POINT('Ctrl Pts',(115.75325535285,-2.97633242050287,331.082163992694));
#38172=CARTESIAN_POINT('Ctrl Pts',(115.745494097924,-3.08438142635394,331.166657370746));
#38173=CARTESIAN_POINT('Ctrl Pts',(115.737732842998,-3.18861192484192,331.255412298362));
#38174=CARTESIAN_POINT('Ctrl Pts',(115.729959172593,-3.2930091581587,331.344309204937));
#38175=CARTESIAN_POINT('Ctrl Pts',(115.722185502189,-3.39357539090462,331.437481017854));
#38176=CARTESIAN_POINT('Ctrl Pts',(115.714411831784,-3.48996131106872,331.53454864271));
#38177=CARTESIAN_POINT('Ctrl Pts',(115.707000027607,-3.58186044346053,331.627097746276));
#38178=CARTESIAN_POINT('Ctrl Pts',(115.69958822343,-3.66995949746807,331.723187911896));
#38179=CARTESIAN_POINT('Ctrl Pts',(115.692176419253,-3.75399115849184,331.822464249695));
#38180=CARTESIAN_POINT('Ctrl Pts',(115.684448837586,-3.84160296090546,331.925970223344));
#38181=CARTESIAN_POINT('Ctrl Pts',(115.67672125592,-3.92508001115426,332.03327892309));
#38182=CARTESIAN_POINT('Ctrl Pts',(115.668993674254,-4.0040708182706,332.144023819292));
#38183=CARTESIAN_POINT('Ctrl Pts',(115.66127857742,-4.08293400629399,332.254589793873));
#38184=CARTESIAN_POINT('Ctrl Pts',(115.653563480586,-4.15732515638901,332.368580590616));
#38185=CARTESIAN_POINT('Ctrl Pts',(115.645848383752,-4.22693171934945,332.485595238937));
#38186=CARTESIAN_POINT('Ctrl Pts',(115.638140515054,-4.29647306917115,332.602500258335));
#38187=CARTESIAN_POINT('Ctrl Pts',(115.630432646356,-4.36123854570563,332.722423157182));
#38188=CARTESIAN_POINT('Ctrl Pts',(115.622724777658,-4.42095763075255,332.844932323663));
#38189=CARTESIAN_POINT('Ctrl Pts',(115.615022409018,-4.48063410240012,332.967354071993));
#38190=CARTESIAN_POINT('Ctrl Pts',(115.607320040379,-4.53527117295905,333.092358062275));
#38191=CARTESIAN_POINT('Ctrl Pts',(115.599617671739,-4.58464343942483,333.219486704391));
#38192=CARTESIAN_POINT('Ctrl Pts',(115.591919079466,-4.63399149934459,333.346553017076));
#38193=CARTESIAN_POINT('Ctrl Pts',(115.584220487192,-4.67807974880975,333.475741540178));
#38194=CARTESIAN_POINT('Ctrl Pts',(115.576521894919,-4.71673045205952,333.606573681491));
#38195=CARTESIAN_POINT('Ctrl Pts',(115.568824079112,-4.75537725706688,333.737392627302));
#38196=CARTESIAN_POINT('Ctrl Pts',(115.561126263305,-4.78858748724757,333.869854484083));
#38197=CARTESIAN_POINT('Ctrl Pts',(115.553428447498,-4.81623300248729,334.003464637731));
#38198=CARTESIAN_POINT('Ctrl Pts',(115.545731117604,-4.84387677264664,334.137066357445));
#38199=CARTESIAN_POINT('Ctrl Pts',(115.53803378771,-4.86595645195465,334.271815840756));
#38200=CARTESIAN_POINT('Ctrl Pts',(115.530336457815,-4.88239499323559,334.407208137262));
#38201=CARTESIAN_POINT('Ctrl Pts',(115.522635710278,-4.89884083328964,334.542660548449));
#38202=CARTESIAN_POINT('Ctrl Pts',(115.514934962741,-4.90964049051541,334.678755948844));
#38203=CARTESIAN_POINT('Ctrl Pts',(115.507234215204,-4.91476878400503,334.814984156706));
#38204=CARTESIAN_POINT('Ctrl Pts',(115.503668226299,-4.91714354536363,334.878067419128));
#38205=CARTESIAN_POINT('Ctrl Pts',(115.500102237395,-4.91830290451448,334.941179132723));
#38206=CARTESIAN_POINT('Ctrl Pts',(115.49653624849,-4.91824814755945,335.004268668182));
#38207=CARTESIAN_POINT('',(118.996536248454,-4.91824887548736,334.996674151641));
#38208=CARTESIAN_POINT('Ctrl Pts',(118.996536248454,-4.91824887548736,334.996674151641));
#38209=CARTESIAN_POINT('Ctrl Pts',(118.988875843359,-4.91833997688369,335.131394467091));
#38210=CARTESIAN_POINT('Ctrl Pts',(118.981215438265,-4.9128915405517,335.266331852603));
#38211=CARTESIAN_POINT('Ctrl Pts',(118.97355503317,-4.9018765637506,335.400985306779));
#38212=CARTESIAN_POINT('Ctrl Pts',(118.965902782214,-4.89087331186996,335.535495428738));
#38213=CARTESIAN_POINT('Ctrl Pts',(118.958250531257,-4.87431533657838,335.669721822289));
#38214=CARTESIAN_POINT('Ctrl Pts',(118.950598280301,-4.85222765334842,335.803162413576));
#38215=CARTESIAN_POINT('Ctrl Pts',(118.942952224206,-4.83015785115041,335.936494978346));
#38216=CARTESIAN_POINT('Ctrl Pts',(118.935306168111,-4.80256731158553,336.069042610921));
#38217=CARTESIAN_POINT('Ctrl Pts',(118.927660112016,-4.76953291471938,336.200307809651));
#38218=CARTESIAN_POINT('Ctrl Pts',(118.92001772895,-4.73651438698541,336.331509950932));
#38219=CARTESIAN_POINT('Ctrl Pts',(118.912375345883,-4.69805729946584,336.461430493612));
#38220=CARTESIAN_POINT('Ctrl Pts',(118.904732962817,-4.65428965003596,336.589581994132));
#38221=CARTESIAN_POINT('Ctrl Pts',(118.897092344035,-4.61053210459963,336.7177039102));
#38222=CARTESIAN_POINT('Ctrl Pts',(118.889451725253,-4.5614665646002,336.844057215134));
#38223=CARTESIAN_POINT('Ctrl Pts',(118.881811106471,-4.50727077723995,336.968170013779));
#38224=CARTESIAN_POINT('Ctrl Pts',(118.874170489986,-4.45307500616858,337.092282775121));
#38225=CARTESIAN_POINT('Ctrl Pts',(118.8665298735,-4.39374915218029,337.214154662487));
#38226=CARTESIAN_POINT('Ctrl Pts',(118.858889257015,-4.32951872896555,337.333334660531));
#38227=CARTESIAN_POINT('Ctrl Pts',(118.851246881055,-4.26527351482691,337.452542103237));
#38228=CARTESIAN_POINT('Ctrl Pts',(118.843604505096,-4.19612167703267,337.569056069762));
#38229=CARTESIAN_POINT('Ctrl Pts',(118.835962129136,-4.12233392781025,337.682451500051));
#38230=CARTESIAN_POINT('Ctrl Pts',(118.828311845355,-4.04846982794068,337.795964264376));
#38231=CARTESIAN_POINT('Ctrl Pts',(118.820661561574,-3.9699604592865,337.906351712053));
#38232=CARTESIAN_POINT('Ctrl Pts',(118.813011277792,-3.88711916257599,338.013218823523));
#38233=CARTESIAN_POINT('Ctrl Pts',(118.805356671563,-3.80423106012154,338.120146315441));
#38234=CARTESIAN_POINT('Ctrl Pts',(118.797702065333,-3.71700641623412,338.22354920428));
#38235=CARTESIAN_POINT('Ctrl Pts',(118.790047459104,-3.62579696872232,338.323067770014));
#38236=CARTESIAN_POINT('Ctrl Pts',(118.782381461024,-3.53445178014621,338.42273444273));
#38237=CARTESIAN_POINT('Ctrl Pts',(118.774715462944,-3.43911023079049,338.518504965712));
#38238=CARTESIAN_POINT('Ctrl Pts',(118.767049464864,-3.3401591307308,338.610058177356));
#38239=CARTESIAN_POINT('Ctrl Pts',(118.762297908664,-3.27882703698147,338.666804895242));
#38240=CARTESIAN_POINT('Ctrl Pts',(118.757546352465,-3.21610887156023,338.721932217824));
#38241=CARTESIAN_POINT('Ctrl Pts',(118.752794796265,-3.15210235561836,338.775372008452));
#38242=CARTESIAN_POINT('Ctrl Pts',(118.745019717487,-3.04736704724914,338.862816745418));
#38243=CARTESIAN_POINT('Ctrl Pts',(118.737244638709,-2.93882467881816,338.946038053379));
#38244=CARTESIAN_POINT('Ctrl Pts',(118.72946955993,-2.82685051373547,339.024686228204));
#38245=CARTESIAN_POINT('Ctrl Pts',(118.721704048881,-2.71501413999145,339.103237621442));
#38246=CARTESIAN_POINT('Ctrl Pts',(118.713938537832,-2.59975468904415,339.177226856203));
#38247=CARTESIAN_POINT('Ctrl Pts',(118.706173026783,-2.48148169156554,339.246343330081));
#38248=CARTESIAN_POINT('Ctrl Pts',(118.698415215261,-2.3633259621084,339.315391274774));
#38249=CARTESIAN_POINT('Ctrl Pts',(118.690657403739,-2.24216296759089,339.379575877312));
#38250=CARTESIAN_POINT('Ctrl Pts',(118.682899592217,-2.11843222396238,339.43862906481));
#38251=CARTESIAN_POINT('Ctrl Pts',(118.675147618694,-1.99479459164251,339.497637812912));
#38252=CARTESIAN_POINT('Ctrl Pts',(118.667395645171,-1.86859340772187,339.551522664521));
#38253=CARTESIAN_POINT('Ctrl Pts',(118.659643671648,-1.74029354754665,339.60006102469));
#38254=CARTESIAN_POINT('Ctrl Pts',(118.65189498109,-1.61204802243807,339.648578828834));
#38255=CARTESIAN_POINT('Ctrl Pts',(118.644146290532,-1.48170595364246,339.691754506935));
#38256=CARTESIAN_POINT('Ctrl Pts',(118.636397599975,-1.3497527921755,339.729413331748));
#38257=CARTESIAN_POINT('Ctrl Pts',(118.628650521597,-1.21782708466583,339.767064321327));
#38258=CARTESIAN_POINT('Ctrl Pts',(118.620903443219,-1.08429132685455,339.799200633525));
#38259=CARTESIAN_POINT('Ctrl Pts',(118.613156364841,-0.949646370496838,
339.82569734168));
#38260=CARTESIAN_POINT('Ctrl Pts',(118.605409221535,-0.815000285684848,
339.852194271904));
#38261=CARTESIAN_POINT('Ctrl Pts',(118.59766207823,-0.679245367303301,339.87305142834));
#38262=CARTESIAN_POINT('Ctrl Pts',(118.589914934924,-0.542892513740601,
339.888195043267));
#38263=CARTESIAN_POINT('Ctrl Pts',(118.582166049896,-0.406509005161195,
339.903342062801));
#38264=CARTESIAN_POINT('Ctrl Pts',(118.574417164868,-0.269527682312667,
339.912772941627));
#38265=CARTESIAN_POINT('Ctrl Pts',(118.56666827984,-0.132464019994088,339.916465838985));
#38266=CARTESIAN_POINT('Ctrl Pts',(118.558911170065,0.00474512311143449,
339.920162656022));
#38267=CARTESIAN_POINT('Ctrl Pts',(118.55115406029,0.142036388918992,339.918109314995));
#38268=CARTESIAN_POINT('Ctrl Pts',(118.543396950515,0.278894290845277,339.910336142978));
#38269=CARTESIAN_POINT('Ctrl Pts',(118.535635695589,0.415825325258531,339.902558817225));
#38270=CARTESIAN_POINT('Ctrl Pts',(118.527874440663,0.552322145576616,339.889055608601));
#38271=CARTESIAN_POINT('Ctrl Pts',(118.520113185737,0.68787592118284,339.86990860074));
#38272=CARTESIAN_POINT('Ctrl Pts',(118.512339515332,0.823646538653116,339.850730963905));
#38273=CARTESIAN_POINT('Ctrl Pts',(118.504565844928,0.958470712246472,339.825891557595));
#38274=CARTESIAN_POINT('Ctrl Pts',(118.496792174523,1.09185043628403,339.795523505029));
#38275=CARTESIAN_POINT('Ctrl Pts',(118.489380370346,1.21902130207793,339.766569092616));
#38276=CARTESIAN_POINT('Ctrl Pts',(118.481968566169,1.34487889237259,339.732589242545));
#38277=CARTESIAN_POINT('Ctrl Pts',(118.474556761992,1.46900741371671,339.693740542568));
#38278=CARTESIAN_POINT('Ctrl Pts',(118.466781683213,1.59921984365208,339.652987752081));
#38279=CARTESIAN_POINT('Ctrl Pts',(118.459006604435,1.7279409206832,339.606747983793));
#38280=CARTESIAN_POINT('Ctrl Pts',(118.451231525657,1.85467349458063,339.555147559739));
#38281=CARTESIAN_POINT('Ctrl Pts',(118.443466014608,1.9812501159779,339.503610633293));
#38282=CARTESIAN_POINT('Ctrl Pts',(118.435700503559,2.1058427444732,339.44672632247));
#38283=CARTESIAN_POINT('Ctrl Pts',(118.42793499251,2.22796856733121,339.384670925564));
#38284=CARTESIAN_POINT('Ctrl Pts',(118.420177180987,2.34997330207991,339.322677056765));
#38285=CARTESIAN_POINT('Ctrl Pts',(118.412419369465,2.46951575233738,339.255522481121));
#38286=CARTESIAN_POINT('Ctrl Pts',(118.404661557943,2.58613264259454,339.183431727351));
#38287=CARTESIAN_POINT('Ctrl Pts',(118.39690958442,2.70266177494385,339.111395224159));
#38288=CARTESIAN_POINT('Ctrl Pts',(118.389157610897,2.81626939828716,339.034430141333));
#38289=CARTESIAN_POINT('Ctrl Pts',(118.381405637374,2.92651675705899,338.952806943572));
#38290=CARTESIAN_POINT('Ctrl Pts',(118.373656946816,3.03671742600892,338.871218313284));
#38291=CARTESIAN_POINT('Ctrl Pts',(118.365908256259,3.14356034728874,338.784975723748));
#38292=CARTESIAN_POINT('Ctrl Pts',(118.358159565701,3.24663588362999,338.694392846142));
#38293=CARTESIAN_POINT('Ctrl Pts',(118.350412487323,3.349689974245,338.603828815061));
#38294=CARTESIAN_POINT('Ctrl Pts',(118.342665408945,3.44897794560169,338.508926549968));
#38295=CARTESIAN_POINT('Ctrl Pts',(118.334918330568,3.5441237045835,338.410039622806));
#38296=CARTESIAN_POINT('Ctrl Pts',(118.327171187262,3.6392702609785,338.311151866877));
#38297=CARTESIAN_POINT('Ctrl Pts',(118.319424043956,3.7302742647451,338.208279663936));
#38298=CARTESIAN_POINT('Ctrl Pts',(118.31167690065,3.81679720660061,338.101812719393));
#38299=CARTESIAN_POINT('Ctrl Pts',(118.303928015622,3.90333960065008,337.99532183882));
#38300=CARTESIAN_POINT('Ctrl Pts',(118.296179130594,3.98539868163359,337.885234911745));
#38301=CARTESIAN_POINT('Ctrl Pts',(118.288430245566,4.06267713019773,337.771973592635));
#38302=CARTESIAN_POINT('Ctrl Pts',(118.280673135791,4.14003760290573,337.658592056791));
#38303=CARTESIAN_POINT('Ctrl Pts',(118.272916026017,4.21260708633004,337.542029721743));
#38304=CARTESIAN_POINT('Ctrl Pts',(118.265158916242,4.28013212378407,337.422736482875));
#38305=CARTESIAN_POINT('Ctrl Pts',(118.257397661316,4.34769324445904,337.303379497514));
#38306=CARTESIAN_POINT('Ctrl Pts',(118.249636406389,4.41020436990875,337.181289048276));
#38307=CARTESIAN_POINT('Ctrl Pts',(118.241875151463,4.46745916856873,337.056937441847));
#38308=CARTESIAN_POINT('Ctrl Pts',(118.234101481059,4.52480555624725,336.932386913373));
#38309=CARTESIAN_POINT('Ctrl Pts',(118.226327810654,4.57687866609643,336.805568361412));
#38310=CARTESIAN_POINT('Ctrl Pts',(118.218554140249,4.62352094482344,336.676972610176));
#38311=CARTESIAN_POINT('Ctrl Pts',(118.211142336072,4.66799201425439,336.554363022097));
#38312=CARTESIAN_POINT('Ctrl Pts',(118.203730531895,4.70752639721672,336.430138242727));
#38313=CARTESIAN_POINT('Ctrl Pts',(118.196318727718,4.74203076199793,336.304732660266));
#38314=CARTESIAN_POINT('Ctrl Pts',(118.18854364894,4.7782262884802,336.173180576646));
#38315=CARTESIAN_POINT('Ctrl Pts',(118.180768570161,4.80900064164011,336.039913284969));
#38316=CARTESIAN_POINT('Ctrl Pts',(118.172993491383,4.83419101185646,335.90541720957));
#38317=CARTESIAN_POINT('Ctrl Pts',(118.165227980334,4.85935038371852,335.771086640156));
#38318=CARTESIAN_POINT('Ctrl Pts',(118.157462469285,4.87893937357584,335.63553067618));
#38319=CARTESIAN_POINT('Ctrl Pts',(118.149696958236,4.89284495675063,335.499250730295));
#38320=CARTESIAN_POINT('Ctrl Pts',(118.141939146713,4.90673675249929,335.363105906373));
#38321=CARTESIAN_POINT('Ctrl Pts',(118.134181335191,4.9149563163394,335.226238915415));
#38322=CARTESIAN_POINT('Ctrl Pts',(118.126423523669,4.91744175429895,335.089160841053));
#38323=CARTESIAN_POINT('Ctrl Pts',(118.118671550146,4.91992532188761,334.95218592229));
#38324=CARTESIAN_POINT('Ctrl Pts',(118.110919576623,4.91668334555691,334.815000625536));
#38325=CARTESIAN_POINT('Ctrl Pts',(118.1031676031,4.90770582902847,334.678120273674));
#38326=CARTESIAN_POINT('Ctrl Pts',(118.095418912542,4.89873211448361,334.541297890722));
#38327=CARTESIAN_POINT('Ctrl Pts',(118.087670221985,4.88402771638807,334.404780585027));
#38328=CARTESIAN_POINT('Ctrl Pts',(118.079921531427,4.86363472929568,334.269082574781));
#38329=CARTESIAN_POINT('Ctrl Pts',(118.072174453049,4.84324598513459,334.133412797639));
#38330=CARTESIAN_POINT('Ctrl Pts',(118.064427374672,4.81717106421079,333.998562363177));
#38331=CARTESIAN_POINT('Ctrl Pts',(118.056680296294,4.78550376714829,333.865038874186));
#38332=CARTESIAN_POINT('Ctrl Pts',(118.048933152988,4.75383620468341,333.73151426614));
#38333=CARTESIAN_POINT('Ctrl Pts',(118.041186009682,4.71657626279533,333.59931700607));
#38334=CARTESIAN_POINT('Ctrl Pts',(118.033438866376,4.6738684662794,333.468942645614));
#38335=CARTESIAN_POINT('Ctrl Pts',(118.025689981348,4.63115106814392,333.338538974233));
#38336=CARTESIAN_POINT('Ctrl Pts',(118.01794109632,4.58298349983442,333.209959389353));
#38337=CARTESIAN_POINT('Ctrl Pts',(118.010192211292,4.52955944302532,333.083682094589));
#38338=CARTESIAN_POINT('Ctrl Pts',(118.002435101517,4.47607868137037,332.957270767799));
#38339=CARTESIAN_POINT('Ctrl Pts',(117.994677991743,4.41733043859673,332.833166973145));
#38340=CARTESIAN_POINT('Ctrl Pts',(117.986920881968,4.35355588137484,332.71182731197));
#38341=CARTESIAN_POINT('Ctrl Pts',(117.979159627042,4.28974724506864,332.59042281076));
#38342=CARTESIAN_POINT('Ctrl Pts',(117.971398372115,4.22090713848748,332.471785724121));
#38343=CARTESIAN_POINT('Ctrl Pts',(117.963637117189,4.14732107655037,332.356345152918));
#38344=CARTESIAN_POINT('Ctrl Pts',(117.955863446785,4.07361730089588,332.240719914422));
#38345=CARTESIAN_POINT('Ctrl Pts',(117.94808977638,3.99515262269015,332.128301730106));
#38346=CARTESIAN_POINT('Ctrl Pts',(117.940316105975,3.91225452535773,332.019488703038));
#38347=CARTESIAN_POINT('Ctrl Pts',(117.932904301798,3.8332153544005,331.915740948559));
#38348=CARTESIAN_POINT('Ctrl Pts',(117.925492497621,3.7501464103122,331.815270486364));
#38349=CARTESIAN_POINT('Ctrl Pts',(117.918080693444,3.66336247225411,331.718390873462));
#38350=CARTESIAN_POINT('Ctrl Pts',(117.910305614666,3.57232499487551,331.616762902141));
#38351=CARTESIAN_POINT('Ctrl Pts',(117.902530535887,3.47691145449798,331.518765513625));
#38352=CARTESIAN_POINT('Ctrl Pts',(117.894755457109,3.37744279009486,331.424798850115));
#38353=CARTESIAN_POINT('Ctrl Pts',(117.88698994606,3.27809652821564,331.330947818568));
#38354=CARTESIAN_POINT('Ctrl Pts',(117.879224435011,3.17470535257591,331.241117908777));
#38355=CARTESIAN_POINT('Ctrl Pts',(117.871458923962,3.06762974763401,331.155675508762));
#38356=CARTESIAN_POINT('Ctrl Pts',(117.863701112439,2.96066030846611,331.070317825136));
#38357=CARTESIAN_POINT('Ctrl Pts',(117.855943300917,2.85001401347286,330.989339236313));
#38358=CARTESIAN_POINT('Ctrl Pts',(117.848185489395,2.73608714940386,330.913068366933));
#38359=CARTESIAN_POINT('Ctrl Pts',(117.840433515872,2.6222460189125,330.8368548938));
#38360=CARTESIAN_POINT('Ctrl Pts',(117.832681542349,2.50512955673429,330.765342305097));
#38361=CARTESIAN_POINT('Ctrl Pts',(117.824929568826,2.38516569931506,330.698817877686));
#38362=CARTESIAN_POINT('Ctrl Pts',(117.817180878268,2.26525264666126,330.632321623411));
#38363=CARTESIAN_POINT('Ctrl Pts',(117.809432187711,2.14249493828591,330.570809518001));
#38364=CARTESIAN_POINT('Ctrl Pts',(117.801683497153,2.01734777101439,330.514524436218));
#38365=CARTESIAN_POINT('Ctrl Pts',(117.793936418775,1.89222664165648,330.458251065017));
#38366=CARTESIAN_POINT('Ctrl Pts',(117.786189340397,1.76471739851877,330.407202714502));
#38367=CARTESIAN_POINT('Ctrl Pts',(117.778442262019,1.63529765651769,330.361575198724));
#38368=CARTESIAN_POINT('Ctrl Pts',(117.770695118714,1.50587682985473,330.315947300545));
#38369=CARTESIAN_POINT('Ctrl Pts',(117.762947975408,1.37454584102702,330.275740457684));
#38370=CARTESIAN_POINT('Ctrl Pts',(117.755200832102,1.24179962063643,330.241101307583));
#38371=CARTESIAN_POINT('Ctrl Pts',(117.747451947074,1.10902355607731,330.206454369866));
#38372=CARTESIAN_POINT('Ctrl Pts',(117.739703062046,0.974832004960463,330.177377714394));
#38373=CARTESIAN_POINT('Ctrl Pts',(117.731954177018,0.839731911174272,330.15396725353));
#38374=CARTESIAN_POINT('Ctrl Pts',(117.724197067243,0.70448842075237,330.130531944562));
#38375=CARTESIAN_POINT('Ctrl Pts',(117.716439957468,0.568334847051531,330.112774910888));
#38376=CARTESIAN_POINT('Ctrl Pts',(117.708682847694,0.431785665005347,330.100740443496));
#38377=CARTESIAN_POINT('Ctrl Pts',(117.700921592768,0.295163515442321,330.08869954527));
#38378=CARTESIAN_POINT('Ctrl Pts',(117.693160337841,0.15814572656161,330.082387324559));
#38379=CARTESIAN_POINT('Ctrl Pts',(117.685399082915,0.0212476469387261,
330.081795896875));
#38380=CARTESIAN_POINT('Ctrl Pts',(117.677625412511,-0.115869424996714,
330.081203523099));
#38381=CARTESIAN_POINT('Ctrl Pts',(117.669851742106,-0.252866014204814,
330.086350214885));
#38382=CARTESIAN_POINT('Ctrl Pts',(117.662078071701,-0.389230127248695,
330.097176020849));
#38383=CARTESIAN_POINT('Ctrl Pts',(117.654666267524,-0.519246458023034,
330.10749788294));
#38384=CARTESIAN_POINT('Ctrl Pts',(117.647254463347,-0.648687585267904,
330.122981998134));
#38385=CARTESIAN_POINT('Ctrl Pts',(117.63984265917,-0.777119487138416,330.143533345609));
#38386=CARTESIAN_POINT('Ctrl Pts',(117.632067580392,-0.911846219098311,
330.165091975843));
#38387=CARTESIAN_POINT('Ctrl Pts',(117.624292501613,-1.04588805531016,330.19229524749));
#38388=CARTESIAN_POINT('Ctrl Pts',(117.616517422835,-1.17873482916488,330.225089816027));
#38389=CARTESIAN_POINT('Ctrl Pts',(117.608751911786,-1.31141812660662,330.257844028759));
#38390=CARTESIAN_POINT('Ctrl Pts',(117.600986400737,-1.44290891190943,330.296175755481));
#38391=CARTESIAN_POINT('Ctrl Pts',(117.593220889688,-1.57270400274552,330.339980130702));
#38392=CARTESIAN_POINT('Ctrl Pts',(117.585463078166,-1.70237040137199,330.383741073759));
#38393=CARTESIAN_POINT('Ctrl Pts',(117.577705266643,-1.83034408342,330.432963742791));
#38394=CARTESIAN_POINT('Ctrl Pts',(117.569947455121,-1.95613424791927,330.487492729467));
#38395=CARTESIAN_POINT('Ctrl Pts',(117.562195481598,-2.08182975132995,330.54198068135));
#38396=CARTESIAN_POINT('Ctrl Pts',(117.554443508075,-2.20534465064975,330.601766847826));
#38397=CARTESIAN_POINT('Ctrl Pts',(117.546691534552,-2.3262057876686,330.666646830004));
#38398=CARTESIAN_POINT('Ctrl Pts',(117.538942843994,-2.44701573992453,330.73149933547));
#38399=CARTESIAN_POINT('Ctrl Pts',(117.531194153437,-2.56517382150425,330.801441181563));
#38400=CARTESIAN_POINT('Ctrl Pts',(117.523445462879,-2.6802294607188,330.876221017029));
#38401=CARTESIAN_POINT('Ctrl Pts',(117.515698384501,-2.79526116164669,330.950985293925));
#38402=CARTESIAN_POINT('Ctrl Pts',(117.507951306124,-2.90719137660424,331.030585345153));
#38403=CARTESIAN_POINT('Ctrl Pts',(117.500204227746,-3.01559697654182,331.114725500358));
#38404=CARTESIAN_POINT('Ctrl Pts',(117.49245708444,-3.12400348502271,331.198866360738));
#38405=CARTESIAN_POINT('Ctrl Pts',(117.484709941134,-3.22888501078524,331.287547161327));
#38406=CARTESIAN_POINT('Ctrl Pts',(117.476962797828,-3.32985040792915,331.380431058356));
#38407=CARTESIAN_POINT('Ctrl Pts',(117.4692139128,-3.4308385042377,331.473335837657));
#38408=CARTESIAN_POINT('Ctrl Pts',(117.461465027772,-3.52790843236624,331.570445329149));
#38409=CARTESIAN_POINT('Ctrl Pts',(117.453716142744,-3.6207052011363,331.671385136582));
#38410=CARTESIAN_POINT('Ctrl Pts',(117.445959032969,-3.71360046535553,331.772432082571));
#38411=CARTESIAN_POINT('Ctrl Pts',(117.438201923195,-3.8022132450217,331.877317177585));
#38412=CARTESIAN_POINT('Ctrl Pts',(117.43044481342,-3.88622788299097,331.985631757074));
#38413=CARTESIAN_POINT('Ctrl Pts',(117.422683558494,-3.97028741569659,332.09400421641));
#38414=CARTESIAN_POINT('Ctrl Pts',(117.414922303568,-4.04974368440043,332.205809493404));
#38415=CARTESIAN_POINT('Ctrl Pts',(117.407161048642,-4.12432443465167,332.320609953696));
#38416=CARTESIAN_POINT('Ctrl Pts',(117.399387378237,-4.19902448979746,332.43559405731));
#38417=CARTESIAN_POINT('Ctrl Pts',(117.391613707832,-4.26883324215789,332.553582582111));
#38418=CARTESIAN_POINT('Ctrl Pts',(117.383840037428,-4.33352403710379,332.674112538762));
#38419=CARTESIAN_POINT('Ctrl Pts',(117.37642823325,-4.39520345998145,332.789031796933));
#38420=CARTESIAN_POINT('Ctrl Pts',(117.369016429073,-4.45223055845808,332.906260945549));
#38421=CARTESIAN_POINT('Ctrl Pts',(117.361604624896,-4.50445036344607,333.025383585161));
#38422=CARTESIAN_POINT('Ctrl Pts',(117.353031950123,-4.56484907261539,333.163163756249));
#38423=CARTESIAN_POINT('Ctrl Pts',(117.344459275349,-4.61898103881594,333.303850835865));
#38424=CARTESIAN_POINT('Ctrl Pts',(117.335886600575,-4.66658497031551,333.446884493244));
#38425=CARTESIAN_POINT('Ctrl Pts',(117.327347485539,-4.71400254510683,333.589358211965));
#38426=CARTESIAN_POINT('Ctrl Pts',(117.318808370503,-4.75494297021422,333.734159945722));
#38427=CARTESIAN_POINT('Ctrl Pts',(117.310269255467,-4.78919382292977,333.88071201699));
#38428=CARTESIAN_POINT('Ctrl Pts',(117.301751804726,-4.82335777898218,334.026892276026));
#38429=CARTESIAN_POINT('Ctrl Pts',(117.293234353986,-4.85086593947895,334.174813772444));
#38430=CARTESIAN_POINT('Ctrl Pts',(117.284716903245,-4.87155504716373,334.323882787563));
#38431=CARTESIAN_POINT('Ctrl Pts',(117.276233683062,-4.89216100794231,334.472352713171));
#38432=CARTESIAN_POINT('Ctrl Pts',(117.267750462878,-4.90600251753535,334.6219607101));
#38433=CARTESIAN_POINT('Ctrl Pts',(117.259267242695,-4.9129671501702,334.772103436076));
#38434=CARTESIAN_POINT('Ctrl Pts',(117.255023577975,-4.91645115331497,334.847211163488));
#38435=CARTESIAN_POINT('Ctrl Pts',(117.250779913256,-4.91821504616872,334.922452462763));
#38436=CARTESIAN_POINT('Ctrl Pts',(117.246536248536,-4.9182494855724,334.997750518554));
#38437=CARTESIAN_POINT('',(120.746536248543,-4.91824835509349,335.00402245201));
#38438=CARTESIAN_POINT('Ctrl Pts',(120.74653624849,-4.91824835509272,335.004022452949));
#38439=CARTESIAN_POINT('Ctrl Pts',(120.734143493174,-4.91806986260446,335.222265002467));
#38440=CARTESIAN_POINT('Ctrl Pts',(120.721750737859,-4.90336218246484,335.439931562694));
#38441=CARTESIAN_POINT('Ctrl Pts',(120.709357982543,-4.87436982771678,335.655516472062));
#38442=CARTESIAN_POINT('Ctrl Pts',(120.706392333757,-4.86743181115095,335.707107027073));
#38443=CARTESIAN_POINT('Ctrl Pts',(120.70342668497,-4.85967592412588,335.758578543016));
#38444=CARTESIAN_POINT('Ctrl Pts',(120.700461036184,-4.85110583398809,335.809910643186));
#38445=CARTESIAN_POINT('Ctrl Pts',(120.692685957405,-4.82863752072631,335.944488656775));
#38446=CARTESIAN_POINT('Ctrl Pts',(120.684910878627,-4.80052932182094,336.078343656673));
#38447=CARTESIAN_POINT('Ctrl Pts',(120.677135799848,-4.76683802711673,336.210965848294));
#38448=CARTESIAN_POINT('Ctrl Pts',(120.669370288799,-4.73318819169556,336.343424839865));
#38449=CARTESIAN_POINT('Ctrl Pts',(120.66160477775,-4.6939690258323,336.474653666432));
#38450=CARTESIAN_POINT('Ctrl Pts',(120.653839266701,-4.64928879197929,336.604149865591));
#38451=CARTESIAN_POINT('Ctrl Pts',(120.646081455179,-4.60465285870828,336.733517668892));
#38452=CARTESIAN_POINT('Ctrl Pts',(120.638323643657,-4.55456675960404,336.861155896394));
#38453=CARTESIAN_POINT('Ctrl Pts',(120.630565832134,-4.49918921516278,336.986574808222));
#38454=CARTESIAN_POINT('Ctrl Pts',(120.622813858611,-4.44385334407982,337.111899338342));
#38455=CARTESIAN_POINT('Ctrl Pts',(120.615061885088,-4.38323411084305,337.23500752092));
#38456=CARTESIAN_POINT('Ctrl Pts',(120.607309911565,-4.31753910620023,337.355427589405));
#38457=CARTESIAN_POINT('Ctrl Pts',(120.599561221008,-4.25187192343088,337.47579665992));
#38458=CARTESIAN_POINT('Ctrl Pts',(120.59181253045,-4.1811334314492,337.593479538154));
#38459=CARTESIAN_POINT('Ctrl Pts',(120.584063839892,-4.1055780197045,337.708027360759));
#38460=CARTESIAN_POINT('Ctrl Pts',(120.576316761515,-4.03003832789429,337.822551350732));
#38461=CARTESIAN_POINT('Ctrl Pts',(120.568569683137,-3.94968392485187,337.933941256413));
#38462=CARTESIAN_POINT('Ctrl Pts',(120.560822604759,-3.86481333272204,338.041775955871));
#38463=CARTESIAN_POINT('Ctrl Pts',(120.553075461453,-3.77994202929487,338.149611559087));
#38464=CARTESIAN_POINT('Ctrl Pts',(120.545328318147,-3.69055470302849,338.253891589497));
#38465=CARTESIAN_POINT('Ctrl Pts',(120.537581174841,-3.59699083247381,338.354227185746));
#38466=CARTESIAN_POINT('Ctrl Pts',(120.529832289813,-3.50340592677465,338.454585339567));
#38467=CARTESIAN_POINT('Ctrl Pts',(120.522083404785,-3.40564287485283,338.550997008797));
#38468=CARTESIAN_POINT('Ctrl Pts',(120.514334519757,-3.30407846263076,338.64310973967));
#38469=CARTESIAN_POINT('Ctrl Pts',(120.506577409982,-3.20240624889218,338.735320239948));
#38470=CARTESIAN_POINT('Ctrl Pts',(120.498820300208,-3.09692490494641,338.82322242397));
#38471=CARTESIAN_POINT('Ctrl Pts',(120.491063190433,-2.98804521850892,338.906503402615));
#38472=CARTESIAN_POINT('Ctrl Pts',(120.483301935507,-2.87910735024845,338.989828883953));
#38473=CARTESIAN_POINT('Ctrl Pts',(120.475540680581,-2.76676784099327,339.068528015209));
#38474=CARTESIAN_POINT('Ctrl Pts',(120.467779425654,-2.65146615438967,339.142331504675));
#38475=CARTESIAN_POINT('Ctrl Pts',(120.46000575525,-2.53598002266411,339.216253055673));
#38476=CARTESIAN_POINT('Ctrl Pts',(120.452232084845,-2.41752258254548,339.285263118501));
#38477=CARTESIAN_POINT('Ctrl Pts',(120.44445841444,-2.2965583440195,339.349138171525));
#38478=CARTESIAN_POINT('Ctrl Pts',(120.437046610263,-2.18122501989955,339.410039825463));
#38479=CARTESIAN_POINT('Ctrl Pts',(120.429634806086,-2.06361328781059,339.466273656212));
#38480=CARTESIAN_POINT('Ctrl Pts',(120.422223001909,-1.94414058462504,339.517687511295));
#38481=CARTESIAN_POINT('Ctrl Pts',(120.414447923131,-1.81881216836524,339.57162131257));
#38482=CARTESIAN_POINT('Ctrl Pts',(120.406672844352,-1.69103968400412,339.620421149492));
#38483=CARTESIAN_POINT('Ctrl Pts',(120.398897765574,-1.56128256092932,339.663858898749));
#38484=CARTESIAN_POINT('Ctrl Pts',(120.391132254525,-1.43168511225526,339.70724319509));
#38485=CARTESIAN_POINT('Ctrl Pts',(120.383366743476,-1.300108251307,339.745278409775));
#38486=CARTESIAN_POINT('Ctrl Pts',(120.375601232427,-1.16703309646476,339.777783671773));
#38487=CARTESIAN_POINT('Ctrl Pts',(120.367843420905,-1.03408988602594,339.810256704708));
#38488=CARTESIAN_POINT('Ctrl Pts',(120.360085609382,-0.899651715311847,
339.837210604213));
#38489=CARTESIAN_POINT('Ctrl Pts',(120.35232779786,-0.764216309800422,339.85851381539));
#38490=CARTESIAN_POINT('Ctrl Pts',(120.344575824337,-0.628882823726594,
339.879800995225));
#38491=CARTESIAN_POINT('Ctrl Pts',(120.336823850814,-0.492553981163142,
339.895445890281));
#38492=CARTESIAN_POINT('Ctrl Pts',(120.329071877291,-0.35573883993393,339.905367768095));
#38493=CARTESIAN_POINT('Ctrl Pts',(120.321323186733,-0.218981639998256,
339.915285443987));
#38494=CARTESIAN_POINT('Ctrl Pts',(120.313574496176,-0.0817389400515719,
339.919484894995));
#38495=CARTESIAN_POINT('Ctrl Pts',(120.305825805618,0.0554741364109582,
339.917937136919));
#38496=CARTESIAN_POINT('Ctrl Pts',(120.29807872724,0.192658664546857,339.916389700867));
#38497=CARTESIAN_POINT('Ctrl Pts',(120.290331648863,0.329813190854032,339.909097438578));
#38498=CARTESIAN_POINT('Ctrl Pts',(120.282584570485,0.466422037455538,339.896083490452));
#38499=CARTESIAN_POINT('Ctrl Pts',(120.274837427179,0.603032028970757,339.883069433256));
#38500=CARTESIAN_POINT('Ctrl Pts',(120.267090283873,0.739095942545852,339.864333631646));
#38501=CARTESIAN_POINT('Ctrl Pts',(120.259343140567,0.874103065048431,339.839951125184));
#38502=CARTESIAN_POINT('Ctrl Pts',(120.251594255539,1.00914054001834,339.815563137018));
#38503=CARTESIAN_POINT('Ctrl Pts',(120.243845370511,1.14312036656365,339.785525987294));
#38504=CARTESIAN_POINT('Ctrl Pts',(120.236096485483,1.27554225831209,339.749965790378));
#38505=CARTESIAN_POINT('Ctrl Pts',(120.228339375708,1.40810470402469,339.714367849501));
#38506=CARTESIAN_POINT('Ctrl Pts',(120.220582265934,1.53910553360685,339.673235252632));
#38507=CARTESIAN_POINT('Ctrl Pts',(120.212825156159,1.66805933111811,339.626744117667));
#38508=CARTESIAN_POINT('Ctrl Pts',(120.205063901233,1.79708203741562,339.580228139327));
#38509=CARTESIAN_POINT('Ctrl Pts',(120.197302646307,1.92405517035841,339.528348065013));
#38510=CARTESIAN_POINT('Ctrl Pts',(120.18954139138,2.04851445781022,339.471327719888));
#38511=CARTESIAN_POINT('Ctrl Pts',(120.181767720976,2.17317283956069,339.414216160794));
#38512=CARTESIAN_POINT('Ctrl Pts',(120.173994050571,2.29530899159242,339.351948077013));
#38513=CARTESIAN_POINT('Ctrl Pts',(120.166220380166,2.41448357678769,339.284793124519));
#38514=CARTESIAN_POINT('Ctrl Pts',(120.158808575989,2.52811055637085,339.220764251219));
#38515=CARTESIAN_POINT('Ctrl Pts',(120.151396771812,2.63904524113767,339.152293389084));
#38516=CARTESIAN_POINT('Ctrl Pts',(120.143984967635,2.74693378378046,339.079649231248));
#38517=CARTESIAN_POINT('Ctrl Pts',(120.136209888857,2.86011026528116,339.003444566842));
#38518=CARTESIAN_POINT('Ctrl Pts',(120.128434810078,2.9702921121187,338.922406350728));
#38519=CARTESIAN_POINT('Ctrl Pts',(120.1206597313,3.07703886693046,338.836797476268));
#38520=CARTESIAN_POINT('Ctrl Pts',(120.112894220251,3.18365426306458,338.751293948978));
#38521=CARTESIAN_POINT('Ctrl Pts',(120.105128709202,3.28684267587705,338.661231196664));
#38522=CARTESIAN_POINT('Ctrl Pts',(120.097363198153,3.38619164629601,338.566915922342));
#38523=CARTESIAN_POINT('Ctrl Pts',(120.089605386631,3.48544211192153,338.472694161888));
#38524=CARTESIAN_POINT('Ctrl Pts',(120.081847575109,3.5808604292853,338.374228537659));
#38525=CARTESIAN_POINT('Ctrl Pts',(120.074089763586,3.67206662325238,338.271866405723));
#38526=CARTESIAN_POINT('Ctrl Pts',(120.066337790063,3.76320418166611,338.169581304537));
#38527=CARTESIAN_POINT('Ctrl Pts',(120.05858581654,3.8501356669462,338.063405822796));
#38528=CARTESIAN_POINT('Ctrl Pts',(120.050833843017,3.93251770904395,337.953724349115));
#38529=CARTESIAN_POINT('Ctrl Pts',(120.04308515246,4.01486486229801,337.844089325604));
#38530=CARTESIAN_POINT('Ctrl Pts',(120.035336461902,4.09266617016763,337.730951575179));
#38531=CARTESIAN_POINT('Ctrl Pts',(120.027587771345,4.16561849634008,337.614728591164));
#38532=CARTESIAN_POINT('Ctrl Pts',(120.019840692967,4.23855564417176,337.498529788311));
#38533=CARTESIAN_POINT('Ctrl Pts',(120.012093614589,4.30664560934917,337.379247359521));
#38534=CARTESIAN_POINT('Ctrl Pts',(120.004346536211,4.3696287882395,337.257327471921));
#38535=CARTESIAN_POINT('Ctrl Pts',(119.996599392905,4.43261249498949,337.135406562514));
#38536=CARTESIAN_POINT('Ctrl Pts',(119.9888522496,4.49048915068558,337.010848497481));
#38537=CARTESIAN_POINT('Ctrl Pts',(119.981105106294,4.54304548151737,336.884123354604));
#38538=CARTESIAN_POINT('Ctrl Pts',(119.973356221266,4.59561362812812,336.757369721224));
#38539=CARTESIAN_POINT('Ctrl Pts',(119.965607336238,4.64285892001542,336.628448401501));
#38540=CARTESIAN_POINT('Ctrl Pts',(119.95785845121,4.68461667577673,336.497848344638));
#38541=CARTESIAN_POINT('Ctrl Pts',(119.950101341435,4.72641875365148,336.367109667525));
#38542=CARTESIAN_POINT('Ctrl Pts',(119.94234423166,4.76272154113165,336.234689066795));
#38543=CARTESIAN_POINT('Ctrl Pts',(119.934587121886,4.79341045309562,336.101090046569));
#38544=CARTESIAN_POINT('Ctrl Pts',(119.926825866959,4.82411576423291,335.967419635298));
#38545=CARTESIAN_POINT('Ctrl Pts',(119.919064612033,4.84920115088203,335.832569933865));
#38546=CARTESIAN_POINT('Ctrl Pts',(119.911303357107,4.86860358810352,335.69705248325));
#38547=CARTESIAN_POINT('Ctrl Pts',(119.903529686702,4.88803706290132,335.56131824888));
#38548=CARTESIAN_POINT('Ctrl Pts',(119.895756016298,4.90176938285342,335.4249145199));
#38549=CARTESIAN_POINT('Ctrl Pts',(119.887982345893,4.9097895568984,335.288356670586));
#38550=CARTESIAN_POINT('Ctrl Pts',(119.880570541716,4.91743638991207,335.158155622011));
#38551=CARTESIAN_POINT('Ctrl Pts',(119.873158737539,4.91989090453877,335.027814766544));
#38552=CARTESIAN_POINT('Ctrl Pts',(119.865746933362,4.91718756348704,334.897777067209));
#38553=CARTESIAN_POINT('Ctrl Pts',(119.857971854583,4.91435172363754,334.761365832868));
#38554=CARTESIAN_POINT('Ctrl Pts',(119.850196775805,4.90583067839006,334.624857138524));
#38555=CARTESIAN_POINT('Ctrl Pts',(119.842421697027,4.89160714362751,334.488763640855));
#38556=CARTESIAN_POINT('Ctrl Pts',(119.834656185978,4.87740111182999,334.352837614898));
#38557=CARTESIAN_POINT('Ctrl Pts',(119.826890674929,4.85750659312705,334.217326154058));
#38558=CARTESIAN_POINT('Ctrl Pts',(119.81912516388,4.83195829535756,334.08274207857));
#38559=CARTESIAN_POINT('Ctrl Pts',(119.811367352357,4.80643532879969,333.948291443585));
#38560=CARTESIAN_POINT('Ctrl Pts',(119.803609540835,4.77526981134047,333.814766745626));
#38561=CARTESIAN_POINT('Ctrl Pts',(119.795851729313,4.7385482157608,333.682675488192));
#38562=CARTESIAN_POINT('Ctrl Pts',(119.78809975579,4.70185425434634,333.550683633618));
#38563=CARTESIAN_POINT('Ctrl Pts',(119.780347782267,4.65961264140815,333.420123447526));
#38564=CARTESIAN_POINT('Ctrl Pts',(119.772595808744,4.61196080029828,333.291491691852));
#38565=CARTESIAN_POINT('Ctrl Pts',(119.764847118186,4.56432913977141,333.162914411802));
#38566=CARTESIAN_POINT('Ctrl Pts',(119.757098427629,4.51129194367738,333.036264303599));
#38567=CARTESIAN_POINT('Ctrl Pts',(119.749349737071,4.4530362466058,332.912022210627));
#38568=CARTESIAN_POINT('Ctrl Pts',(119.741602658693,4.39479267011855,332.78780596726));
#38569=CARTESIAN_POINT('Ctrl Pts',(119.733855580315,4.33133291812902,332.665997096264));
#38570=CARTESIAN_POINT('Ctrl Pts',(119.726108501938,4.2628916956706,332.547055350506));
#38571=CARTESIAN_POINT('Ctrl Pts',(119.718361358632,4.19444989960887,332.428112607901));
#38572=CARTESIAN_POINT('Ctrl Pts',(119.710614215326,4.12102674475167,332.312037377252));
#38573=CARTESIAN_POINT('Ctrl Pts',(119.70286707202,4.04290211483849,332.199263391118));
#38574=CARTESIAN_POINT('Ctrl Pts',(119.695118186992,3.96475992084993,332.086464050997));
#38575=CARTESIAN_POINT('Ctrl Pts',(119.687369301964,3.88191437105357,331.976967753509));
#38576=CARTESIAN_POINT('Ctrl Pts',(119.679620416936,3.79468751470903,331.871177581228));
#38577=CARTESIAN_POINT('Ctrl Pts',(119.671863307161,3.70736807487786,331.765275122165));
#38578=CARTESIAN_POINT('Ctrl Pts',(119.664106197386,3.61565828801369,331.66308694834));
#38579=CARTESIAN_POINT('Ctrl Pts',(119.656349087612,3.51991955288857,331.564981891796));
#38580=CARTESIAN_POINT('Ctrl Pts',(119.648587832686,3.42412965804449,331.466824411046));
#38581=CARTESIAN_POINT('Ctrl Pts',(119.640826577759,3.32430680933164,331.372754663119));
#38582=CARTESIAN_POINT('Ctrl Pts',(119.633065322833,3.22084706606405,331.28310247121));
#38583=CARTESIAN_POINT('Ctrl Pts',(119.625291652429,3.11722182092475,331.193306865011));
#38584=CARTESIAN_POINT('Ctrl Pts',(119.617517982024,3.00994836146576,331.107943179601));
#38585=CARTESIAN_POINT('Ctrl Pts',(119.609744311619,2.89945412901684,331.027299556193));
#38586=CARTESIAN_POINT('Ctrl Pts',(119.602332507442,2.79410342967243,330.950409912856));
#38587=CARTESIAN_POINT('Ctrl Pts',(119.594920703265,2.6858253023157,330.877810943292));
#38588=CARTESIAN_POINT('Ctrl Pts',(119.587508899088,2.57501089375246,330.809713379785));
#38589=CARTESIAN_POINT('Ctrl Pts',(119.57973382031,2.45876514092566,330.738278151837));
#38590=CARTESIAN_POINT('Ctrl Pts',(119.571958741531,2.33936084104629,330.671570993198));
#38591=CARTESIAN_POINT('Ctrl Pts',(119.564183662753,2.21721974462194,330.609883866393));
#38592=CARTESIAN_POINT('Ctrl Pts',(119.556418151704,2.09522895059262,330.548272649525));
#38593=CARTESIAN_POINT('Ctrl Pts',(119.548652640655,1.9705084065453,330.491669347627));
#38594=CARTESIAN_POINT('Ctrl Pts',(119.540887129606,1.84350813635811,330.440322290591));
#38595=CARTESIAN_POINT('Ctrl Pts',(119.533129318084,1.71663378730865,330.389026144312));
#38596=CARTESIAN_POINT('Ctrl Pts',(119.525371506561,1.58748457039647,330.342976017119));
#38597=CARTESIAN_POINT('Ctrl Pts',(119.517613695039,1.45653405152368,330.302373831471));
#38598=CARTESIAN_POINT('Ctrl Pts',(119.509861721516,1.32568207706911,330.261802200254));
#38599=CARTESIAN_POINT('Ctrl Pts',(119.502109747993,1.19303187062088,330.226670465523));
#38600=CARTESIAN_POINT('Ctrl Pts',(119.49435777447,1.05907553754994,330.197131891436));
#38601=CARTESIAN_POINT('Ctrl Pts',(119.486609083912,0.925175935065453,330.167605826952));
#38602=CARTESIAN_POINT('Ctrl Pts',(119.478860393355,0.789971687035495,330.143668295916));
#38603=CARTESIAN_POINT('Ctrl Pts',(119.471111702797,0.653968360069763,330.125422228897));
#38604=CARTESIAN_POINT('Ctrl Pts',(119.463364624419,0.517993329732128,330.107179958125));
#38605=CARTESIAN_POINT('Ctrl Pts',(119.455617546042,0.38121993831201,330.09462684794));
#38606=CARTESIAN_POINT('Ctrl Pts',(119.447870467664,0.24416181416412,330.087814328529));
#38607=CARTESIAN_POINT('Ctrl Pts',(119.440123324358,0.107102541337231,330.081001752022));
#38608=CARTESIAN_POINT('Ctrl Pts',(119.432376181052,-0.0302410785848208,
330.079929881657));
#38609=CARTESIAN_POINT('Ctrl Pts',(119.424629037746,-0.167352849489318,
330.084598074799));
#38610=CARTESIAN_POINT('Ctrl Pts',(119.416880152718,-0.30449544603088,330.089267317451));
#38611=CARTESIAN_POINT('Ctrl Pts',(119.40913126769,-0.441405699261192,330.09967917824));
#38612=CARTESIAN_POINT('Ctrl Pts',(119.401382382662,-0.577570369110589,
330.115780970183));
#38613=CARTESIAN_POINT('Ctrl Pts',(119.393625272887,-0.713879565547455,
330.131899852735));
#38614=CARTESIAN_POINT('Ctrl Pts',(119.385868163113,-0.849441208984974,
330.153720684638));
#38615=CARTESIAN_POINT('Ctrl Pts',(119.378111053338,-0.983749567076295,
330.181139154138));
#38616=CARTESIAN_POINT('Ctrl Pts',(119.370349798412,-1.11812969525979,330.208572275192));
#38617=CARTESIAN_POINT('Ctrl Pts',(119.362588543485,-1.25125482445359,330.241608899978));
#38618=CARTESIAN_POINT('Ctrl Pts',(119.354827288559,-1.38263326887683,330.280094460024));
#38619=CARTESIAN_POINT('Ctrl Pts',(119.347053618155,-1.51422187599501,330.318641584424));
#38620=CARTESIAN_POINT('Ctrl Pts',(119.33927994775,-1.64405784447323,330.36265493672));
#38621=CARTESIAN_POINT('Ctrl Pts',(119.331506277345,-1.77166755718988,330.411931002121));
#38622=CARTESIAN_POINT('Ctrl Pts',(119.324094473168,-1.89333700707897,330.458913254822));
#38623=CARTESIAN_POINT('Ctrl Pts',(119.316682668991,-2.01298253712763,330.510679173971));
#38624=CARTESIAN_POINT('Ctrl Pts',(119.309270864814,-2.13021526608317,330.567013875203));
#38625=CARTESIAN_POINT('Ctrl Pts',(119.301495786035,-2.25319392030266,330.626109707954));
#38626=CARTESIAN_POINT('Ctrl Pts',(119.293720707257,-2.37390591121925,330.690420259906));
#38627=CARTESIAN_POINT('Ctrl Pts',(119.285945628478,-2.49187748791643,330.759748869735));
#38628=CARTESIAN_POINT('Ctrl Pts',(119.278180117429,-2.60970389307808,330.828992166295));
#38629=CARTESIAN_POINT('Ctrl Pts',(119.27041460638,-2.72479626006984,330.903241038027));
#38630=CARTESIAN_POINT('Ctrl Pts',(119.262649095331,-2.83670222924492,330.982251435804));
#38631=CARTESIAN_POINT('Ctrl Pts',(119.254891283809,-2.94849724332576,331.061183494542));
#38632=CARTESIAN_POINT('Ctrl Pts',(119.247133472287,-3.05711182957005,331.144867460142));
#38633=CARTESIAN_POINT('Ctrl Pts',(119.239375660765,-3.16211991339303,331.233014372761));
#38634=CARTESIAN_POINT('Ctrl Pts',(119.231623687242,-3.26704897530287,331.321094952034));
#38635=CARTESIAN_POINT('Ctrl Pts',(119.223871713719,-3.36837663871759,331.413631543083));
#38636=CARTESIAN_POINT('Ctrl Pts',(119.216119740196,-3.46570771408276,331.510293264034));
#38637=CARTESIAN_POINT('Ctrl Pts',(119.208371049638,-3.56299756967973,331.606914048689));
#38638=CARTESIAN_POINT('Ctrl Pts',(119.20062235908,-3.65629392683993,331.707656213734));
#38639=CARTESIAN_POINT('Ctrl Pts',(119.192873668523,-3.74523663794914,331.812150319061));
#38640=CARTESIAN_POINT('Ctrl Pts',(119.185126590145,-3.83416084378441,331.916622683516));
#38641=CARTESIAN_POINT('Ctrl Pts',(119.177379511767,-3.91873295210075,332.024845138075));
#38642=CARTESIAN_POINT('Ctrl Pts',(119.169632433389,-3.99863176038211,332.136413593522));
#38643=CARTESIAN_POINT('Ctrl Pts',(119.161885290083,-4.07853123829235,332.247982984021));
#38644=CARTESIAN_POINT('Ctrl Pts',(119.154138146778,-4.15375711046519,332.362898113552));
#38645=CARTESIAN_POINT('Ctrl Pts',(119.146391003472,-4.22403057396825,332.480724554027));
#38646=CARTESIAN_POINT('Ctrl Pts',(119.138642118444,-4.29431983643781,332.598577484388));
#38647=CARTESIAN_POINT('Ctrl Pts',(119.130893233416,-4.35965427450441,332.719342692487));
#38648=CARTESIAN_POINT('Ctrl Pts',(119.123144348387,-4.41980045012489,332.84256007185));
#38649=CARTESIAN_POINT('Ctrl Pts',(119.115387238613,-4.48001046551765,332.965908235413));
#38650=CARTESIAN_POINT('Ctrl Pts',(119.107630128838,-4.53502104623235,333.091713417683));
#38651=CARTESIAN_POINT('Ctrl Pts',(119.099873019063,-4.58464622945744,333.219493888463));
#38652=CARTESIAN_POINT('Ctrl Pts',(119.092111764137,-4.63429793079373,333.347342641041));
#38653=CARTESIAN_POINT('Ctrl Pts',(119.084350509211,-4.67855837433095,333.477168415593));
#38654=CARTESIAN_POINT('Ctrl Pts',(119.076589254285,-4.71729146060522,333.608474097186));
#38655=CARTESIAN_POINT('Ctrl Pts',(119.06881558388,-4.75608650719445,333.739989825079));
#38656=CARTESIAN_POINT('Ctrl Pts',(119.061041913475,-4.78933643279507,333.872989811314));
#38657=CARTESIAN_POINT('Ctrl Pts',(119.053268243071,-4.8169560759355,334.006965647619));
#38658=CARTESIAN_POINT('Ctrl Pts',(119.045856438894,-4.84329001804257,334.134704876511));
#38659=CARTESIAN_POINT('Ctrl Pts',(119.038444634717,-4.8645060138211,334.263330864432));
#38660=CARTESIAN_POINT('Ctrl Pts',(119.03103283054,-4.88057431815725,334.39240030658));
#38661=CARTESIAN_POINT('Ctrl Pts',(119.019533969856,-4.90550309238889,334.592641907449));
#38662=CARTESIAN_POINT('Ctrl Pts',(119.008035109173,-4.91811212521678,334.794448535063));
#38663=CARTESIAN_POINT('Ctrl Pts',(118.99653624849,-4.91824887548693,334.996674151001));
#38664=CARTESIAN_POINT('',(122.496536248438,-4.9182498524359,335.001204788044));
#38665=CARTESIAN_POINT('Ctrl Pts',(122.496536248438,-4.9182498524359,335.001204788045));
#38666=CARTESIAN_POINT('Ctrl Pts',(122.488252845916,-4.91821382984681,335.148258117707));
#38667=CARTESIAN_POINT('Ctrl Pts',(122.479969443393,-4.91157834180379,335.295134724896));
#38668=CARTESIAN_POINT('Ctrl Pts',(122.471686040871,-4.89841612088684,335.441251140662));
#38669=CARTESIAN_POINT('Ctrl Pts',(122.463202974284,-4.88493663631842,335.590889562927));
#38670=CARTESIAN_POINT('Ctrl Pts',(122.454719907697,-4.86461188669965,335.739730340687));
#38671=CARTESIAN_POINT('Ctrl Pts',(122.44623684111,-4.83757469627169,335.887160707252));
#38672=CARTESIAN_POINT('Ctrl Pts',(122.437909913463,-4.8110351511475,336.031877477161));
#38673=CARTESIAN_POINT('Ctrl Pts',(122.429582985816,-4.77802828235813,336.175235047038));
#38674=CARTESIAN_POINT('Ctrl Pts',(122.421256058168,-4.73872973127174,336.31667140793));
#38675=CARTESIAN_POINT('Ctrl Pts',(122.412694922111,-4.69832584439482,336.462085896959));
#38676=CARTESIAN_POINT('Ctrl Pts',(122.404133786055,-4.65127130310775,336.605469186264));
#38677=CARTESIAN_POINT('Ctrl Pts',(122.395572649998,-4.59780918123002,336.746234175446));
#38678=CARTESIAN_POINT('Ctrl Pts',(122.387011513941,-4.54434705935229,336.886999164629));
#38679=CARTESIAN_POINT('Ctrl Pts',(122.378450377884,-4.48447755795471,337.025145573085));
#38680=CARTESIAN_POINT('Ctrl Pts',(122.369889241827,-4.4184938428861,337.160114631884));
#38681=CARTESIAN_POINT('Ctrl Pts',(122.362114163048,-4.35856855033833,337.282691245294));
#38682=CARTESIAN_POINT('Ctrl Pts',(122.35433908427,-4.29344397051479,337.402966017987));
#38683=CARTESIAN_POINT('Ctrl Pts',(122.346564005492,-4.22331996077631,337.520466538443));
#38684=CARTESIAN_POINT('Ctrl Pts',(122.338798494443,-4.15328224309601,337.637822467028));
#38685=CARTESIAN_POINT('Ctrl Pts',(122.331032983394,-4.07825753484646,337.75241060361));
#38686=CARTESIAN_POINT('Ctrl Pts',(122.323267472345,-3.99849293559624,337.86378024759));
#38687=CARTESIAN_POINT('Ctrl Pts',(122.315509660822,-3.91880742317863,337.975039468244));
#38688=CARTESIAN_POINT('Ctrl Pts',(122.3077518493,-3.8343915983921,338.083086231125));
#38689=CARTESIAN_POINT('Ctrl Pts',(122.299994037778,-3.74553729292212,338.187496423501));
#38690=CARTESIAN_POINT('Ctrl Pts',(122.292242064255,-3.65674985313468,338.291828043896));
#38691=CARTESIAN_POINT('Ctrl Pts',(122.284490090732,-3.56353083326843,338.392528244447));
#38692=CARTESIAN_POINT('Ctrl Pts',(122.276738117209,-3.46621377743365,338.489204079963));
#38693=CARTESIAN_POINT('Ctrl Pts',(122.268989426651,-3.36893793542969,338.585838973204));
#38694=CARTESIAN_POINT('Ctrl Pts',(122.261240736094,-3.26756778601032,338.678452616282));
#38695=CARTESIAN_POINT('Ctrl Pts',(122.253492045536,-3.16247519390871,338.766687365632));
#38696=CARTESIAN_POINT('Ctrl Pts',(122.245744967158,-3.05740446719868,338.854903757005));
#38697=CARTESIAN_POINT('Ctrl Pts',(122.23799788878,-2.94861313747918,338.938742815646));
#38698=CARTESIAN_POINT('Ctrl Pts',(122.230250810403,-2.83650745469667,339.017886076278));
#38699=CARTESIAN_POINT('Ctrl Pts',(122.222503667097,-2.72440083236055,339.097030000207));
#38700=CARTESIAN_POINT('Ctrl Pts',(122.214756523791,-2.6089801208757,339.171477822202));
#38701=CARTESIAN_POINT('Ctrl Pts',(122.207009380485,-2.49068162192992,339.240953680563));
#38702=CARTESIAN_POINT('Ctrl Pts',(122.199260495457,-2.37235652697011,339.310445158572));
#38703=CARTESIAN_POINT('Ctrl Pts',(122.191511610429,-2.2511526940969,339.374962250738));
#38704=CARTESIAN_POINT('Ctrl Pts',(122.183762725401,-2.12753179632469,339.434274632691));
#38705=CARTESIAN_POINT('Ctrl Pts',(122.176005615626,-2.00377968605431,339.49364996942));
#38706=CARTESIAN_POINT('Ctrl Pts',(122.168248505851,-1.87760573903,339.547809391211));
#38707=CARTESIAN_POINT('Ctrl Pts',(122.160491396077,-1.74949293076574,339.596570193927));
#38708=CARTESIAN_POINT('Ctrl Pts',(122.15273014115,-1.621311663113,339.645357052858));
#38709=CARTESIAN_POINT('Ctrl Pts',(122.144968886224,-1.49118984038717,339.688739420827));
#38710=CARTESIAN_POINT('Ctrl Pts',(122.137207631298,-1.35962548562458,339.726584559842));
#38711=CARTESIAN_POINT('Ctrl Pts',(122.129433960893,-1.22785067077109,339.764490238746));
#38712=CARTESIAN_POINT('Ctrl Pts',(122.121660290489,-1.09462909268573,339.79684089598));
#38713=CARTESIAN_POINT('Ctrl Pts',(122.113886620084,-0.960469723365517,
339.823554806675));
#38714=CARTESIAN_POINT('Ctrl Pts',(122.106474815907,-0.832555504965305,
339.8490251784));
#38715=CARTESIAN_POINT('Ctrl Pts',(122.09906301173,-0.703789123143303,339.8693717299));
#38716=CARTESIAN_POINT('Ctrl Pts',(122.091651207553,-0.574614073533863,
339.884567711579));
#38717=CARTESIAN_POINT('Ctrl Pts',(122.083876128775,-0.43910776994924,339.900508493586));
#38718=CARTESIAN_POINT('Ctrl Pts',(122.076101049996,-0.302723500652418,
339.91083142591));
#38719=CARTESIAN_POINT('Ctrl Pts',(122.068325971218,-0.165966680853271,
339.915448923887));
#38720=CARTESIAN_POINT('Ctrl Pts',(122.060560460169,-0.0293781490272524,
339.92006073974));
#38721=CARTESIAN_POINT('Ctrl Pts',(122.05279494912,0.107581634205588,339.918981077761));
#38722=CARTESIAN_POINT('Ctrl Pts',(122.045029438071,0.244399945341746,339.912173829296));
#38723=CARTESIAN_POINT('Ctrl Pts',(122.037271626548,0.381082600724122,339.905373330236));
#38724=CARTESIAN_POINT('Ctrl Pts',(122.029513815026,0.517623675278446,339.892856565358));
#38725=CARTESIAN_POINT('Ctrl Pts',(122.021756003504,0.653508596689846,339.874639430415));
#38726=CARTESIAN_POINT('Ctrl Pts',(122.014004029981,0.789291260388541,339.856436004443));
#38727=CARTESIAN_POINT('Ctrl Pts',(122.006252056458,0.924418367932922,339.832540798592));
#38728=CARTESIAN_POINT('Ctrl Pts',(121.998500082935,1.05837898346981,339.803021652028));
#38729=CARTESIAN_POINT('Ctrl Pts',(121.990751392377,1.19228286660657,339.77351500684));
#38730=CARTESIAN_POINT('Ctrl Pts',(121.98300270182,1.32502085936485,339.738389241995));
#38731=CARTESIAN_POINT('Ctrl Pts',(121.975254011262,1.45609097429646,339.697763525027));
#38732=CARTESIAN_POINT('Ctrl Pts',(121.967506932884,1.58713381899593,339.657146260578));
#38733=CARTESIAN_POINT('Ctrl Pts',(121.959759854507,1.71650910299104,339.611031435771));
#38734=CARTESIAN_POINT('Ctrl Pts',(121.952012776129,1.84372917688055,339.559588335017));
#38735=CARTESIAN_POINT('Ctrl Pts',(121.944265632823,1.97095031699678,339.50814480312));
#38736=CARTESIAN_POINT('Ctrl Pts',(121.936518489517,2.09601584861001,339.451373052736));
#38737=CARTESIAN_POINT('Ctrl Pts',(121.928771346211,2.21845768585406,339.389490694668));
#38738=CARTESIAN_POINT('Ctrl Pts',(121.921022461183,2.34092705062267,339.327594424132));
#38739=CARTESIAN_POINT('Ctrl Pts',(121.913273576155,2.46077119847885,339.260585435859));
#38740=CARTESIAN_POINT('Ctrl Pts',(121.905524691127,2.57754660698784,339.188727318805));
#38741=CARTESIAN_POINT('Ctrl Pts',(121.897767581352,2.6944459621219,339.116792930803));
#38742=CARTESIAN_POINT('Ctrl Pts',(121.890010471578,2.80826973794107,339.039999337746));
#38743=CARTESIAN_POINT('Ctrl Pts',(121.882253361803,2.91860292887465,338.958653812354));
#38744=CARTESIAN_POINT('Ctrl Pts',(121.874492106877,3.0289950783377,338.877264818514));
#38745=CARTESIAN_POINT('Ctrl Pts',(121.86673085195,3.13589262175083,338.791319290345));
#38746=CARTESIAN_POINT('Ctrl Pts',(121.858969597024,3.23891442806256,338.701164193897));
#38747=CARTESIAN_POINT('Ctrl Pts',(121.85119592662,3.34210103568965,338.610864878677));
#38748=CARTESIAN_POINT('Ctrl Pts',(121.843422256215,3.44139923368296,338.516342808417));
#38749=CARTESIAN_POINT('Ctrl Pts',(121.83564858581,3.53646486390482,338.417981762512));
#38750=CARTESIAN_POINT('Ctrl Pts',(121.828236781633,3.62710516616851,338.324199446958));
#38751=CARTESIAN_POINT('Ctrl Pts',(121.820824977456,3.71389789321751,338.226927735874));
#38752=CARTESIAN_POINT('Ctrl Pts',(121.813413173279,3.79658054981075,338.12652509846));
#38753=CARTESIAN_POINT('Ctrl Pts',(121.805638094501,3.88331572970239,338.021201428702));
#38754=CARTESIAN_POINT('Ctrl Pts',(121.797863015722,3.96580185756734,337.912099318029));
#38755=CARTESIAN_POINT('Ctrl Pts',(121.790087936944,4.04369177242485,337.799596383789));
#38756=CARTESIAN_POINT('Ctrl Pts',(121.782322425895,4.12148583878341,337.687231891572));
#38757=CARTESIAN_POINT('Ctrl Pts',(121.774556914846,4.19469472545002,337.571475220895));
#38758=CARTESIAN_POINT('Ctrl Pts',(121.766791403797,4.26301060377761,337.452737991425));
#38759=CARTESIAN_POINT('Ctrl Pts',(121.759033592274,4.33125874671298,337.334118490264));
#38760=CARTESIAN_POINT('Ctrl Pts',(121.751275780752,4.39462334225948,337.212524648007));
#38761=CARTESIAN_POINT('Ctrl Pts',(121.74351796923,4.45283929289114,337.088397781598));
#38762=CARTESIAN_POINT('Ctrl Pts',(121.735765995707,4.51101143417379,336.964364324592));
#38763=CARTESIAN_POINT('Ctrl Pts',(121.728014022184,4.56404247727582,336.837801990055));
#38764=CARTESIAN_POINT('Ctrl Pts',(121.720262048661,4.61171297289221,336.709177146512));
#38765=CARTESIAN_POINT('Ctrl Pts',(121.712513358103,4.65936328002541,336.580606775666));
#38766=CARTESIAN_POINT('Ctrl Pts',(121.704764667546,4.70165741937806,336.449975998841));
#38767=CARTESIAN_POINT('Ctrl Pts',(121.697015976988,4.73842394725883,336.317771436382));
#38768=CARTESIAN_POINT('Ctrl Pts',(121.68926889861,4.7751828255564,336.185594380186));
#38769=CARTESIAN_POINT('Ctrl Pts',(121.681521820233,4.80641627528101,336.051844566003));
#38770=CARTESIAN_POINT('Ctrl Pts',(121.673774741855,4.83200275623447,335.917023678125));
#38771=CARTESIAN_POINT('Ctrl Pts',(121.666027598549,4.85758945162727,335.782201660319));
#38772=CARTESIAN_POINT('Ctrl Pts',(121.658280455243,4.87752901097182,335.646308934934));
#38773=CARTESIAN_POINT('Ctrl Pts',(121.650533311937,4.89175111971402,335.509856887054));
#38774=CARTESIAN_POINT('Ctrl Pts',(121.642784426909,4.9059764258882,335.373374161857));
#38775=CARTESIAN_POINT('Ctrl Pts',(121.635035541881,4.91448168313653,335.236332252633));
#38776=CARTESIAN_POINT('Ctrl Pts',(121.627286656853,4.91724853359589,335.099246769968));
#38777=CARTESIAN_POINT('Ctrl Pts',(121.619529547078,4.92001832081892,334.962015783355));
#38778=CARTESIAN_POINT('Ctrl Pts',(121.611772437304,4.91703752640005,334.824741522326));
#38779=CARTESIAN_POINT('Ctrl Pts',(121.604015327529,4.90833995919861,334.68793925682));
#38780=CARTESIAN_POINT('Ctrl Pts',(121.596254072603,4.89963774429536,334.551063888557));
#38781=CARTESIAN_POINT('Ctrl Pts',(121.588492817677,4.88521271061089,334.414661406896));
#38782=CARTESIAN_POINT('Ctrl Pts',(121.58073156275,4.86515037741903,334.279240076309));
#38783=CARTESIAN_POINT('Ctrl Pts',(121.572957892346,4.84505595103237,334.143602115726));
#38784=CARTESIAN_POINT('Ctrl Pts',(121.565184221941,4.81930627827437,334.008948826707));
#38785=CARTESIAN_POINT('Ctrl Pts',(121.557410551536,4.78803784370988,333.875777304222));
#38786=CARTESIAN_POINT('Ctrl Pts',(121.549998747359,4.75822496229697,333.748804948148));
#38787=CARTESIAN_POINT('Ctrl Pts',(121.542586943182,4.72339563001726,333.623179788013));
#38788=CARTESIAN_POINT('Ctrl Pts',(121.535175139005,4.68370924003127,333.499316549919));
#38789=CARTESIAN_POINT('Ctrl Pts',(121.527400060227,4.64207770185253,333.369382405557));
#38790=CARTESIAN_POINT('Ctrl Pts',(121.519624981448,4.59496938623718,333.240976648509));
#38791=CARTESIAN_POINT('Ctrl Pts',(121.51184990267,4.54251397094156,333.114595564262));
#38792=CARTESIAN_POINT('Ctrl Pts',(121.504084391621,4.49012310537392,332.988369999985));
#38793=CARTESIAN_POINT('Ctrl Pts',(121.496318880572,4.43239838074171,332.864164508724));
#38794=CARTESIAN_POINT('Ctrl Pts',(121.488553369523,4.36951935306018,332.742460701176));
#38795=CARTESIAN_POINT('Ctrl Pts',(121.480795558,4.30670267011765,332.620877563308));
#38796=CARTESIAN_POINT('Ctrl Pts',(121.473037746478,4.23874203258317,332.50179151799));
#38797=CARTESIAN_POINT('Ctrl Pts',(121.465279934956,4.1658650938064,332.385664313309));
#38798=CARTESIAN_POINT('Ctrl Pts',(121.457527961433,4.09304299723716,332.269624498032));
#38799=CARTESIAN_POINT('Ctrl Pts',(121.44977598791,4.01531217037886,332.156539421157));
#38800=CARTESIAN_POINT('Ctrl Pts',(121.442024014387,3.9329460358628,332.046846001054));
#38801=CARTESIAN_POINT('Ctrl Pts',(121.434275323829,3.85061478345361,331.93719903618));
#38802=CARTESIAN_POINT('Ctrl Pts',(121.426526633272,3.76365236197711,331.83094118316));
#38803=CARTESIAN_POINT('Ctrl Pts',(121.418777942714,3.67237520284385,331.728479950843));
#38804=CARTESIAN_POINT('Ctrl Pts',(121.411030864336,3.58111703468588,331.626040036441));
#38805=CARTESIAN_POINT('Ctrl Pts',(121.403283785958,3.48554617433257,331.527395463213));
#38806=CARTESIAN_POINT('Ctrl Pts',(121.395536707581,3.38601872643472,331.432919927065));
#38807=CARTESIAN_POINT('Ctrl Pts',(121.387789564275,3.28649044440102,331.33844359912));
#38808=CARTESIAN_POINT('Ctrl Pts',(121.380042420969,3.1830057921737,331.248136647046));
#38809=CARTESIAN_POINT('Ctrl Pts',(121.372295277663,3.07595675313919,331.162334939665));
#38810=CARTESIAN_POINT('Ctrl Pts',(121.364546392635,2.96888364720807,331.076513942238));
#38811=CARTESIAN_POINT('Ctrl Pts',(121.356797507607,2.85824486480913,330.995200449422));
#38812=CARTESIAN_POINT('Ctrl Pts',(121.349048622579,2.74446405939093,330.918688925209));
#38813=CARTESIAN_POINT('Ctrl Pts',(121.341291512804,2.63056248585021,330.842096190874));
#38814=CARTESIAN_POINT('Ctrl Pts',(121.333534403029,2.5135125522349,330.770315825055));
#38815=CARTESIAN_POINT('Ctrl Pts',(121.325777293255,2.39376585594316,330.703598239291));
#38816=CARTESIAN_POINT('Ctrl Pts',(121.318016038328,2.27395517084569,330.636845001783));
#38817=CARTESIAN_POINT('Ctrl Pts',(121.310254783402,2.15144520056255,330.575160110753));
#38818=CARTESIAN_POINT('Ctrl Pts',(121.302493528476,2.02670963491755,330.518746702291));
#38819=CARTESIAN_POINT('Ctrl Pts',(121.294719858071,1.90177453301879,330.462243050759));
#38820=CARTESIAN_POINT('Ctrl Pts',(121.286946187667,1.77460708413481,330.411027878834));
#38821=CARTESIAN_POINT('Ctrl Pts',(121.279172517262,1.6456991656623,330.365255420345));
#38822=CARTESIAN_POINT('Ctrl Pts',(121.271760713085,1.52279194180933,330.321613680812));
#38823=CARTESIAN_POINT('Ctrl Pts',(121.264348908908,1.39830291435526,330.282919426859));
#38824=CARTESIAN_POINT('Ctrl Pts',(121.256937104731,1.27266709211144,330.249263053467));
#38825=CARTESIAN_POINT('Ctrl Pts',(121.249162025953,1.14087348396843,330.213957080957));
#38826=CARTESIAN_POINT('Ctrl Pts',(121.241386947174,1.00740133079538,330.18408374551));
#38827=CARTESIAN_POINT('Ctrl Pts',(121.233611868396,0.87273814572275,330.159802566888));
#38828=CARTESIAN_POINT('Ctrl Pts',(121.225846357347,0.738240672272432,330.135551267803));
#38829=CARTESIAN_POINT('Ctrl Pts',(121.218080846298,0.602555464120857,330.116878502018));
#38830=CARTESIAN_POINT('Ctrl Pts',(121.210315335249,0.466184686040631,330.103893904234));
#38831=CARTESIAN_POINT('Ctrl Pts',(121.202557523727,0.329949119983904,330.090922180715));
#38832=CARTESIAN_POINT('Ctrl Pts',(121.194799712204,0.19302972333652,330.083627438418));
#38833=CARTESIAN_POINT('Ctrl Pts',(121.187041900682,0.0559379862049669,
330.082068117166));
#38834=CARTESIAN_POINT('Ctrl Pts',(121.179289927159,-0.0810505850469661,
330.080509969352));
#38835=CARTESIAN_POINT('Ctrl Pts',(121.171537953636,-0.218210849362863,
330.084678656054));
#38836=CARTESIAN_POINT('Ctrl Pts',(121.163785980113,-0.355027428088145,
330.094580691948));
#38837=CARTESIAN_POINT('Ctrl Pts',(121.156037289555,-0.491786064911109,
330.104478534325));
#38838=CARTESIAN_POINT('Ctrl Pts',(121.148288598998,-0.628200916591018,
330.120104868463));
#38839=CARTESIAN_POINT('Ctrl Pts',(121.14053990844,-0.763758061050371,330.14141412686));
#38840=CARTESIAN_POINT('Ctrl Pts',(121.132792830062,-0.899287001713625,
330.162718951687));
#38841=CARTESIAN_POINT('Ctrl Pts',(121.125045751684,-1.03395820422216,330.189704288275));
#38842=CARTESIAN_POINT('Ctrl Pts',(121.117298673307,-1.16726471105814,330.222272908922));
#38843=CARTESIAN_POINT('Ctrl Pts',(121.109551530001,-1.30057233513105,330.254841802526));
#38844=CARTESIAN_POINT('Ctrl Pts',(121.101804386695,-1.43251486101219,330.292993980753));
#38845=CARTESIAN_POINT('Ctrl Pts',(121.094057243389,-1.56259772474264,330.336581574303));
#38846=CARTESIAN_POINT('Ctrl Pts',(121.086308358361,-1.69270983386246,330.38017896727));
#38847=CARTESIAN_POINT('Ctrl Pts',(121.078559473333,-1.82096107832683,330.429214083034));
#38848=CARTESIAN_POINT('Ctrl Pts',(121.070810588305,-1.94687457389216,330.483490013735));
#38849=CARTESIAN_POINT('Ctrl Pts',(121.06305347853,-2.07292171534266,330.53782355347));
#38850=CARTESIAN_POINT('Ctrl Pts',(121.055296368755,-2.1966257917297,330.597408865097));
#38851=CARTESIAN_POINT('Ctrl Pts',(121.047539258981,-2.317531841383,330.662001702781));
#38852=CARTESIAN_POINT('Ctrl Pts',(121.039778004055,-2.43850249936338,330.726629056812));
#38853=CARTESIAN_POINT('Ctrl Pts',(121.032016749128,-2.55667181476036,330.796269070445));
#38854=CARTESIAN_POINT('Ctrl Pts',(121.024255494202,-2.67161262535982,330.870633336392));
#38855=CARTESIAN_POINT('Ctrl Pts',(121.016481823798,-2.78673730379719,330.94511656093));
#38856=CARTESIAN_POINT('Ctrl Pts',(121.008708153393,-2.8986228379547,331.02433891344));
#38857=CARTESIAN_POINT('Ctrl Pts',(121.000934482988,-3.00687334623065,331.107970228502));
#38858=CARTESIAN_POINT('Ctrl Pts',(120.993522678811,-3.11008476730356,331.187708485728));
#38859=CARTESIAN_POINT('Ctrl Pts',(120.986110874634,-3.20999174689452,331.271454283682));
#38860=CARTESIAN_POINT('Ctrl Pts',(120.978699070457,-3.30628286170681,331.358890732087));
#38861=CARTESIAN_POINT('Ctrl Pts',(120.971039942796,-3.40578710161219,331.449244835427));
#38862=CARTESIAN_POINT('Ctrl Pts',(120.963380815135,-3.50176462688324,331.543844415688));
#38863=CARTESIAN_POINT('Ctrl Pts',(120.955721687474,-3.59382317637695,331.642379110228));
#38864=CARTESIAN_POINT('Ctrl Pts',(120.948072075932,-3.68576734729001,331.74079137987));
#38865=CARTESIAN_POINT('Ctrl Pts',(120.94042246439,-3.7738019527125,331.843128749123));
#38866=CARTESIAN_POINT('Ctrl Pts',(120.932772852849,-3.85756823507023,331.949041072994));
#38867=CARTESIAN_POINT('Ctrl Pts',(120.925012994336,-3.94254176551617,332.056479815931));
#38868=CARTESIAN_POINT('Ctrl Pts',(120.917253135823,-4.02312265110909,332.167597105007));
#38869=CARTESIAN_POINT('Ctrl Pts',(120.90949327731,-4.09897502778376,332.281988450336));
#38870=CARTESIAN_POINT('Ctrl Pts',(120.901857084696,-4.17361857412897,332.394556784526));
#38871=CARTESIAN_POINT('Ctrl Pts',(120.894220892082,-4.24368296867924,332.510295247593));
#38872=CARTESIAN_POINT('Ctrl Pts',(120.886584699468,-4.30888915332716,332.628785685173));
#38873=CARTESIAN_POINT('Ctrl Pts',(120.878951511157,-4.37406968393813,332.747229505119));
#38874=CARTESIAN_POINT('Ctrl Pts',(120.871318322847,-4.43439561110258,332.868422793726));
#38875=CARTESIAN_POINT('Ctrl Pts',(120.863685134536,-4.48963242435178,332.991920380884));
#38876=CARTESIAN_POINT('Ctrl Pts',(120.856053182759,-4.5448602895486,333.115397962129));
#38877=CARTESIAN_POINT('Ctrl Pts',(120.848421230982,-4.59500051666463,333.241178730914));
#38878=CARTESIAN_POINT('Ctrl Pts',(120.840789279205,-4.63986583957253,333.368795520706));
#38879=CARTESIAN_POINT('Ctrl Pts',(120.832934859983,-4.68603896342454,333.500132273877));
#38880=CARTESIAN_POINT('Ctrl Pts',(120.825080440761,-4.72662478170577,333.633413309007));
#38881=CARTESIAN_POINT('Ctrl Pts',(120.817226021539,-4.76147380476872,333.768111097135));
#38882=CARTESIAN_POINT('Ctrl Pts',(120.809588196785,-4.79536182671955,333.89909444185));
#38883=CARTESIAN_POINT('Ctrl Pts',(120.801950372031,-4.82382525267203,334.031417014512));
#38884=CARTESIAN_POINT('Ctrl Pts',(120.794312547278,-4.84677845086613,334.164582912121));
#38885=CARTESIAN_POINT('Ctrl Pts',(120.786349830822,-4.87070801391076,334.303413314547));
#38886=CARTESIAN_POINT('Ctrl Pts',(120.778387114366,-4.88864816190976,334.443159882849));
#38887=CARTESIAN_POINT('Ctrl Pts',(120.77042439791,-4.90056191064571,334.583255447032));
#38888=CARTESIAN_POINT('Ctrl Pts',(120.762461681455,-4.91247565938166,334.723351011215));
#38889=CARTESIAN_POINT('Ctrl Pts',(120.754498964999,-4.91836304183632,334.863795077535));
#38890=CARTESIAN_POINT('Ctrl Pts',(120.746536248543,-4.91824835509349,335.00402245201));
#38891=CARTESIAN_POINT('',(124.246536248521,-4.91824792744739,334.995484841147));
#38892=CARTESIAN_POINT('Ctrl Pts',(124.24653624849,-4.91824792744789,334.995484841695));
#38893=CARTESIAN_POINT('Ctrl Pts',(124.238867278053,-4.91837231136742,335.130973104362));
#38894=CARTESIAN_POINT('Ctrl Pts',(124.231198307617,-4.91289382317161,335.266601363009));
#38895=CARTESIAN_POINT('Ctrl Pts',(124.22352933718,-4.90180460816653,335.401863964368));
#38896=CARTESIAN_POINT('Ctrl Pts',(124.215853841775,-4.89070595815681,335.537241650814));
#38897=CARTESIAN_POINT('Ctrl Pts',(124.208178346371,-4.87398701663746,335.672252655387));
#38898=CARTESIAN_POINT('Ctrl Pts',(124.200502850966,-4.85169222915224,335.806390461305));
#38899=CARTESIAN_POINT('Ctrl Pts',(124.192840454809,-4.82943549066893,335.940299343326));
#38900=CARTESIAN_POINT('Ctrl Pts',(124.185178058652,-4.80162198093284,336.073337607823));
#38901=CARTESIAN_POINT('Ctrl Pts',(124.177515662495,-4.76834765888175,336.205007745426));
#38902=CARTESIAN_POINT('Ctrl Pts',(124.169853753625,-4.73507545289661,336.336669509525));
#38903=CARTESIAN_POINT('Ctrl Pts',(124.162191844755,-4.69634322324669,336.466962931612));
#38904=CARTESIAN_POINT('Ctrl Pts',(124.154529935884,-4.65229756023208,336.595402918876));
#38905=CARTESIAN_POINT('Ctrl Pts',(124.14686676733,-4.60824465572831,336.723864022789));
#38906=CARTESIAN_POINT('Ctrl Pts',(124.139203598775,-4.55887671063673,336.850470707267));
#38907=CARTESIAN_POINT('Ctrl Pts',(124.13154043022,-4.50438929995784,336.974755705632));
#38908=CARTESIAN_POINT('Ctrl Pts',(124.123855181658,-4.44974489384719,337.099398808313));
#38909=CARTESIAN_POINT('Ctrl Pts',(124.116169933095,-4.38995164429082,337.221706458019));
#38910=CARTESIAN_POINT('Ctrl Pts',(124.108484684533,-4.3252537414127,337.341231115225));
#38911=CARTESIAN_POINT('Ctrl Pts',(124.100809883398,-4.26064378971032,337.460593289047));
#38912=CARTESIAN_POINT('Ctrl Pts',(124.093135082263,-4.19114275147848,337.577179708469));
#38913=CARTESIAN_POINT('Ctrl Pts',(124.085460281128,-4.1170374390443,337.690573505409));
#38914=CARTESIAN_POINT('Ctrl Pts',(124.077769808852,-4.04278081131301,337.804198840622));
#38915=CARTESIAN_POINT('Ctrl Pts',(124.070079336575,-3.96390134438794,337.914618191908));
#38916=CARTESIAN_POINT('Ctrl Pts',(124.062388864299,-3.8807277299219,338.021445903655));
#38917=CARTESIAN_POINT('Ctrl Pts',(124.054698392023,-3.7975541154559,338.128273615403));
#38918=CARTESIAN_POINT('Ctrl Pts',(124.047007919747,-3.71008665864779,338.231509425653));
#38919=CARTESIAN_POINT('Ctrl Pts',(124.039317447471,-3.61868988274723,338.330805697576));
#38920=CARTESIAN_POINT('Ctrl Pts',(124.031542368692,-3.52628760793234,338.431194374483));
#38921=CARTESIAN_POINT('Ctrl Pts',(124.023767289914,-3.42955872278655,338.52789367449));
#38922=CARTESIAN_POINT('Ctrl Pts',(124.015992211135,-3.32882954335569,338.620507828162));
#38923=CARTESIAN_POINT('Ctrl Pts',(124.008226700086,-3.22822431759288,338.713008014222));
#38924=CARTESIAN_POINT('Ctrl Pts',(124.000461189037,-3.12362887712746,338.801432794272));
#38925=CARTESIAN_POINT('Ctrl Pts',(123.992695677988,-3.01540862382393,338.885420684285));
#38926=CARTESIAN_POINT('Ctrl Pts',(123.984937866466,-2.90729567121673,338.96932530006));
#38927=CARTESIAN_POINT('Ctrl Pts',(123.977180054944,-2.79556536486126,339.048801542328));
#38928=CARTESIAN_POINT('Ctrl Pts',(123.969422243422,-2.68061839541984,339.123526170723));
#38929=CARTESIAN_POINT('Ctrl Pts',(123.961670269899,-2.56575792721845,339.198194566465));
#38930=CARTESIAN_POINT('Ctrl Pts',(123.953918296376,-2.44768594049332,339.268118253486));
#38931=CARTESIAN_POINT('Ctrl Pts',(123.946166322853,-2.3268342140595,339.333015763043));
#38932=CARTESIAN_POINT('Ctrl Pts',(123.938417632295,-2.20603366840316,339.397885788467));
#38933=CARTESIAN_POINT('Ctrl Pts',(123.930668941738,-2.08245606809512,339.457733685502));
#38934=CARTESIAN_POINT('Ctrl Pts',(123.92292025118,-1.95655984991967,339.512322751775));
#38935=CARTESIAN_POINT('Ctrl Pts',(123.915173172802,-1.83068982550396,339.566900460336));
#38936=CARTESIAN_POINT('Ctrl Pts',(123.907426094424,-1.70250250115246,339.616221359065));
#38937=CARTESIAN_POINT('Ctrl Pts',(123.899679016047,-1.57247809385156,339.660096104895));
#38938=CARTESIAN_POINT('Ctrl Pts',(123.891931872741,-1.44245259682079,339.703971218438));
#38939=CARTESIAN_POINT('Ctrl Pts',(123.884184729435,-1.3105903564888,339.74239996307));
#38940=CARTESIAN_POINT('Ctrl Pts',(123.876437586129,-1.17738823951595,339.7752424018));
#38941=CARTESIAN_POINT('Ctrl Pts',(123.868688701101,-1.04415617587965,339.808092224208));
#38942=CARTESIAN_POINT('Ctrl Pts',(123.860939816073,-0.909584015617764,
339.835353148018));
#38943=CARTESIAN_POINT('Ctrl Pts',(123.853190931045,-0.774179952228243,
339.856936119002));
#38944=CARTESIAN_POINT('Ctrl Pts',(123.84543382127,-0.638632169566438,339.878541998374));
#38945=CARTESIAN_POINT('Ctrl Pts',(123.837676711495,-0.502251106531569,
339.894457824521));
#38946=CARTESIAN_POINT('Ctrl Pts',(123.829919601721,-0.36555178951698,339.904646261626));
#38947=CARTESIAN_POINT('Ctrl Pts',(123.822158346795,-0.228779424758129,
339.914840143106));
#38948=CARTESIAN_POINT('Ctrl Pts',(123.814397091868,-0.0916888576196233,
339.919300524453));
#38949=CARTESIAN_POINT('Ctrl Pts',(123.806635836942,0.0452047168919196,
339.918042252367));
#38950=CARTESIAN_POINT('Ctrl Pts',(123.798862166538,0.182317276508983,339.916781967457));
#38951=CARTESIAN_POINT('Ctrl Pts',(123.791088496133,0.319231823217834,339.909784768699));
#38952=CARTESIAN_POINT('Ctrl Pts',(123.783314825728,0.455437220326082,339.897117519607));
#38953=CARTESIAN_POINT('Ctrl Pts',(123.775903021551,0.585302223430506,339.885039934008));
#38954=CARTESIAN_POINT('Ctrl Pts',(123.768491217374,0.714522327711021,339.867808338154));
#38955=CARTESIAN_POINT('Ctrl Pts',(123.761079413197,0.842664834777234,339.845523608314));
#38956=CARTESIAN_POINT('Ctrl Pts',(123.753304334418,0.977087987830924,339.822146637482));
#38957=CARTESIAN_POINT('Ctrl Pts',(123.74552925564,1.1107500422505,339.793134794181));
#38958=CARTESIAN_POINT('Ctrl Pts',(123.737754176862,1.24314159873856,339.758548310986));
#38959=CARTESIAN_POINT('Ctrl Pts',(123.729988665813,1.37537023898794,339.72400438866));
#38960=CARTESIAN_POINT('Ctrl Pts',(123.722223154764,1.50633111751356,339.683899573625));
#38961=CARTESIAN_POINT('Ctrl Pts',(123.714457643715,1.63552251476752,339.638345520354));
#38962=CARTESIAN_POINT('Ctrl Pts',(123.706699832192,1.76458581837474,339.59283663406));
#38963=CARTESIAN_POINT('Ctrl Pts',(123.69894202067,1.89188276590224,339.541889390821));
#38964=CARTESIAN_POINT('Ctrl Pts',(123.691184209148,2.01692470091968,339.485665816055));
#38965=CARTESIAN_POINT('Ctrl Pts',(123.683432235625,2.141872537916,339.429484551311));
#38966=CARTESIAN_POINT('Ctrl Pts',(123.675680262102,2.26456838507538,339.368035017985));
#38967=CARTESIAN_POINT('Ctrl Pts',(123.667928288579,2.38454188903436,339.301527989208));
#38968=CARTESIAN_POINT('Ctrl Pts',(123.660179598021,2.50446458414293,339.235049126197));
#38969=CARTESIAN_POINT('Ctrl Pts',(123.652430907464,2.62166688796647,339.163517216843));
#38970=CARTESIAN_POINT('Ctrl Pts',(123.644682216906,2.73570166597968,339.087189677181));
#38971=CARTESIAN_POINT('Ctrl Pts',(123.636935138528,2.84971271810498,339.010878018101));
#38972=CARTESIAN_POINT('Ctrl Pts',(123.629188060151,2.96055723065519,338.929772930632));
#38973=CARTESIAN_POINT('Ctrl Pts',(123.621440981773,3.06781610803996,338.844175775085));
#38974=CARTESIAN_POINT('Ctrl Pts',(123.613693838467,3.1750758843574,338.758577902151));
#38975=CARTESIAN_POINT('Ctrl Pts',(123.605946695161,3.27874966005724,338.66848812986));
#38976=CARTESIAN_POINT('Ctrl Pts',(123.598199551855,3.37845087607788,338.57424855605));
#38977=CARTESIAN_POINT('Ctrl Pts',(123.590450666827,3.4781745070483,338.479987795184));
#38978=CARTESIAN_POINT('Ctrl Pts',(123.582701781799,3.5739235171337,338.381575644755));
#38979=CARTESIAN_POINT('Ctrl Pts',(123.574952896771,3.66534800606997,338.279391263161));
#38980=CARTESIAN_POINT('Ctrl Pts',(123.567195786996,3.75686953390367,338.177098422009));
#38981=CARTESIAN_POINT('Ctrl Pts',(123.559438677222,3.84405711041111,338.071025643319));
#38982=CARTESIAN_POINT('Ctrl Pts',(123.551681567447,3.92660062877545,337.961585819219));
#38983=CARTESIAN_POINT('Ctrl Pts',(123.543920312521,4.00918825575675,337.852087513977));
#38984=CARTESIAN_POINT('Ctrl Pts',(123.536159057595,4.08712665772259,337.739218899655));
#38985=CARTESIAN_POINT('Ctrl Pts',(123.528397802668,4.16014951800182,337.623421249127));
#38986=CARTESIAN_POINT('Ctrl Pts',(123.520624132264,4.23328919105941,337.507438360096));
#38987=CARTESIAN_POINT('Ctrl Pts',(123.512850461859,4.3014974147242,337.388517411078));
#38988=CARTESIAN_POINT('Ctrl Pts',(123.505076791454,4.36455381055837,337.267124411505));
#38989=CARTESIAN_POINT('Ctrl Pts',(123.497664987277,4.42467491599633,337.151382285266));
#38990=CARTESIAN_POINT('Ctrl Pts',(123.4902531831,4.48011291249718,337.033393337522));
#38991=CARTESIAN_POINT('Ctrl Pts',(123.482841378923,4.53071847113989,336.913576023515));
#38992=CARTESIAN_POINT('Ctrl Pts',(123.475066300145,4.58380435895752,336.787886106033));
#38993=CARTESIAN_POINT('Ctrl Pts',(123.467291221366,4.63173988815878,336.659786859807));
#38994=CARTESIAN_POINT('Ctrl Pts',(123.459516142588,4.67430004441115,336.529739244877));
#38995=CARTESIAN_POINT('Ctrl Pts',(123.451750631539,4.71680782768174,336.399851661817));
#38996=CARTESIAN_POINT('Ctrl Pts',(123.44398512049,4.75395327902397,336.268020848508));
#38997=CARTESIAN_POINT('Ctrl Pts',(123.436219609441,4.78555878183027,336.134729134264));
#38998=CARTESIAN_POINT('Ctrl Pts',(123.428461797919,4.81713294768859,336.001569579142));
#38999=CARTESIAN_POINT('Ctrl Pts',(123.420703986396,4.84317800654216,335.866952383536));
#39000=CARTESIAN_POINT('Ctrl Pts',(123.412946174874,4.86356576898616,335.731376150313));
#39001=CARTESIAN_POINT('Ctrl Pts',(123.405194201351,4.88393818899236,335.595901942504));
#39002=CARTESIAN_POINT('Ctrl Pts',(123.397442227828,4.89866172863496,335.459470518571));
#39003=CARTESIAN_POINT('Ctrl Pts',(123.389690254305,4.90765909634135,335.322591470126));
#39004=CARTESIAN_POINT('Ctrl Pts',(123.381941563747,4.91665265365717,335.185770390039));
#39005=CARTESIAN_POINT('Ctrl Pts',(123.37419287319,4.91992483668058,335.048502451701));
#39006=CARTESIAN_POINT('Ctrl Pts',(123.366444182632,4.91745014189946,334.91130296266));
#39007=CARTESIAN_POINT('Ctrl Pts',(123.358697104254,4.91497596199927,334.774132019118));
#39008=CARTESIAN_POINT('Ctrl Pts',(123.350950025877,4.90675728964313,334.637029887112));
#39009=CARTESIAN_POINT('Ctrl Pts',(123.343202947499,4.89282074847415,334.500512076421));
#39010=CARTESIAN_POINT('Ctrl Pts',(123.335455804193,4.87888409050351,334.363993121579));
#39011=CARTESIAN_POINT('Ctrl Pts',(123.327708660887,4.85922950783392,334.228058886673));
#39012=CARTESIAN_POINT('Ctrl Pts',(123.319961517581,4.83393548854778,334.093219566235));
#39013=CARTESIAN_POINT('Ctrl Pts',(123.312212632553,4.80863578262904,333.958349931055));
#39014=CARTESIAN_POINT('Ctrl Pts',(123.304463747525,4.7776941892355,333.824576084272));
#39015=CARTESIAN_POINT('Ctrl Pts',(123.296714862497,4.74124019964471,333.69239744885));
#39016=CARTESIAN_POINT('Ctrl Pts',(123.288957752722,4.70474751741284,333.56007851766));
#39017=CARTESIAN_POINT('Ctrl Pts',(123.281200642947,4.66273085531849,333.429358557505));
#39018=CARTESIAN_POINT('Ctrl Pts',(123.273443533173,4.61536960656995,333.300721783447));
#39019=CARTESIAN_POINT('Ctrl Pts',(123.265682278247,4.56798304948439,333.172016270011));
#39020=CARTESIAN_POINT('Ctrl Pts',(123.25792102332,4.5152463651625,333.045396521445));
#39021=CARTESIAN_POINT('Ctrl Pts',(123.250159768394,4.45738651014688,332.921325287194));
#39022=CARTESIAN_POINT('Ctrl Pts',(123.24238609799,4.39943409821974,332.797055579402));
#39023=CARTESIAN_POINT('Ctrl Pts',(123.234612427585,4.33634231873491,332.675342879767));
#39024=CARTESIAN_POINT('Ctrl Pts',(123.22683875718,4.26838378954875,332.556624693663));
#39025=CARTESIAN_POINT('Ctrl Pts',(123.219426953003,4.2035887462465,332.443432867685));
#39026=CARTESIAN_POINT('Ctrl Pts',(123.212015148826,4.13437000384308,332.332963283882));
#39027=CARTESIAN_POINT('Ctrl Pts',(123.204603344649,4.06099863983351,332.225567966273));
#39028=CARTESIAN_POINT('Ctrl Pts',(123.196828265871,3.98403112671128,332.112908884233));
#39029=CARTESIAN_POINT('Ctrl Pts',(123.189053187092,3.90225040307346,332.003277022603));
#39030=CARTESIAN_POINT('Ctrl Pts',(123.181278108314,3.81592233188421,331.89711105266));
#39031=CARTESIAN_POINT('Ctrl Pts',(123.173512597265,3.72970049288233,331.791075726701));
#39032=CARTESIAN_POINT('Ctrl Pts',(123.165747086216,3.63894268461023,331.688498106672));
#39033=CARTESIAN_POINT('Ctrl Pts',(123.157981575167,3.54395838953981,331.589788570233));
#39034=CARTESIAN_POINT('Ctrl Pts',(123.150223763644,3.44906827167421,331.491176904587));
#39035=CARTESIAN_POINT('Ctrl Pts',(123.142465952122,3.34996027576758,331.396425970075));
#39036=CARTESIAN_POINT('Ctrl Pts',(123.1347081406,3.24698431696538,331.305913386522));
#39037=CARTESIAN_POINT('Ctrl Pts',(123.126956167077,3.14408585083783,331.215468916558));
#39038=CARTESIAN_POINT('Ctrl Pts',(123.119204193554,3.03732550795233,331.129256706036));
#39039=CARTESIAN_POINT('Ctrl Pts',(123.111452220031,2.92708998786247,331.047617520349));
#39040=CARTESIAN_POINT('Ctrl Pts',(123.103703529473,2.81690115258131,330.966012908906));
#39041=CARTESIAN_POINT('Ctrl Pts',(123.095954838916,2.70324038074115,330.888977702525));
#39042=CARTESIAN_POINT('Ctrl Pts',(123.088206148358,2.58652720403971,330.816812210137));
#39043=CARTESIAN_POINT('Ctrl Pts',(123.08045906998,2.46983831048941,330.744661732382));
#39044=CARTESIAN_POINT('Ctrl Pts',(123.072711991602,2.35009860754055,330.677379158757));
#39045=CARTESIAN_POINT('Ctrl Pts',(123.064964913224,2.22775600594537,330.615221072793));
#39046=CARTESIAN_POINT('Ctrl Pts',(123.057217769919,2.10541237900115,330.553062465886));
#39047=CARTESIAN_POINT('Ctrl Pts',(123.049470626613,1.98046615837642,330.496028609352));
#39048=CARTESIAN_POINT('Ctrl Pts',(123.041723483307,1.85338885194286,330.444329596427));
#39049=CARTESIAN_POINT('Ctrl Pts',(123.033974598279,1.72628297583324,330.392618960466));
#39050=CARTESIAN_POINT('Ctrl Pts',(123.026225713251,1.5970454225206,330.346245702025));
#39051=CARTESIAN_POINT('Ctrl Pts',(123.018476828223,1.46616624259004,330.305371195548));
#39052=CARTESIAN_POINT('Ctrl Pts',(123.010719718448,1.3351481461455,330.264453304448));
#39053=CARTESIAN_POINT('Ctrl Pts',(123.002962608673,1.20248531608825,330.22904594084));
#39054=CARTESIAN_POINT('Ctrl Pts',(122.995205498898,1.06868201915229,330.199260285702));
#39055=CARTESIAN_POINT('Ctrl Pts',(122.987444243972,0.93480722201275,330.169458714062));
#39056=CARTESIAN_POINT('Ctrl Pts',(122.979682989046,0.799791128213023,330.145284905607));
#39057=CARTESIAN_POINT('Ctrl Pts',(122.97192173412,0.664145692840228,330.126798428017));
#39058=CARTESIAN_POINT('Ctrl Pts',(122.964148063715,0.52828326897758,330.108282378086));
#39059=CARTESIAN_POINT('Ctrl Pts',(122.95637439331,0.391789881143109,330.095471875814));
#39060=CARTESIAN_POINT('Ctrl Pts',(122.948600722906,0.255180966104411,330.088374430289));
#39061=CARTESIAN_POINT('Ctrl Pts',(122.941188918729,0.124931228928863,330.081607372561));
#39062=CARTESIAN_POINT('Ctrl Pts',(122.933777114552,-0.00542323414057583,
330.080033459226));
#39063=CARTESIAN_POINT('Ctrl Pts',(122.926365310375,-0.135439703008916,
330.083615235831));
#39064=CARTESIAN_POINT('Ctrl Pts',(122.918590231596,-0.271828666317511,
330.087372565977));
#39065=CARTESIAN_POINT('Ctrl Pts',(122.910815152818,-0.408276679793586,
330.096815630196));
#39066=CARTESIAN_POINT('Ctrl Pts',(122.903040074039,-0.544270981694427,
330.11195824885));
#39067=CARTESIAN_POINT('Ctrl Pts',(122.89527456299,-0.680097933948819,330.127082233547));
#39068=CARTESIAN_POINT('Ctrl Pts',(122.887509051941,-0.815471900766772,
330.147891774656));
#39069=CARTESIAN_POINT('Ctrl Pts',(122.879743540892,-0.949880308093416,
330.174348700663));
#39070=CARTESIAN_POINT('Ctrl Pts',(122.87198572937,-1.0841554490931,330.20077939455));
#39071=CARTESIAN_POINT('Ctrl Pts',(122.864227917848,-1.21746655474758,330.232846255212));
#39072=CARTESIAN_POINT('Ctrl Pts',(122.856470106326,-1.34930671732538,330.270459383293));
#39073=CARTESIAN_POINT('Ctrl Pts',(122.848718132803,-1.48104766599924,330.308044206302));
#39074=CARTESIAN_POINT('Ctrl Pts',(122.84096615928,-1.6113195005258,330.351166882297));
#39075=CARTESIAN_POINT('Ctrl Pts',(122.833214185757,-1.73962639869795,330.399686635081));
#39076=CARTESIAN_POINT('Ctrl Pts',(122.825465495199,-1.86787895882302,330.448185839721));
#39077=CARTESIAN_POINT('Ctrl Pts',(122.817716804641,-1.99416787283916,330.502077437156));
#39078=CARTESIAN_POINT('Ctrl Pts',(122.809968114084,-2.11801357188558,330.561171148624));
#39079=CARTESIAN_POINT('Ctrl Pts',(122.802221035706,-2.24183350380001,330.620252565152));
#39080=CARTESIAN_POINT('Ctrl Pts',(122.794473957328,-2.36321087930042,330.684533774634));
#39081=CARTESIAN_POINT('Ctrl Pts',(122.78672687895,-2.4816875416116,330.753776971436));
#39082=CARTESIAN_POINT('Ctrl Pts',(122.778979735645,-2.60016519687084,330.823020748561));
#39083=CARTESIAN_POINT('Ctrl Pts',(122.771232592339,-2.71574175298579,330.897226398723));
#39084=CARTESIAN_POINT('Ctrl Pts',(122.763485449033,-2.82798537810988,330.976111114395));
#39085=CARTESIAN_POINT('Ctrl Pts',(122.755736564005,-2.94025423798401,331.055013565026));
#39086=CARTESIAN_POINT('Ctrl Pts',(122.747987678977,-3.04918835608372,331.138596949729));
#39087=CARTESIAN_POINT('Ctrl Pts',(122.740238793949,-3.15438683470517,331.226536503484));
#39088=CARTESIAN_POINT('Ctrl Pts',(122.732481684174,-3.25969697207885,331.31456939719));
#39089=CARTESIAN_POINT('Ctrl Pts',(122.724724574399,-3.36126324905533,331.4069674451));
#39090=CARTESIAN_POINT('Ctrl Pts',(122.716967464625,-3.4587192835137,331.503366764965));
#39091=CARTESIAN_POINT('Ctrl Pts',(122.709206209698,-3.55622739536091,331.599817597545));
#39092=CARTESIAN_POINT('Ctrl Pts',(122.701444954772,-3.6496206221926,331.700273676415));
#39093=CARTESIAN_POINT('Ctrl Pts',(122.693683699846,-3.73857182400419,331.80433672311));
#39094=CARTESIAN_POINT('Ctrl Pts',(122.685910029441,-3.82766531874958,331.908566236766));
#39095=CARTESIAN_POINT('Ctrl Pts',(122.678136359037,-3.912302347557,332.016413940708));
#39096=CARTESIAN_POINT('Ctrl Pts',(122.670362688632,-3.9921976634614,332.127450456763));
#39097=CARTESIAN_POINT('Ctrl Pts',(122.662950884455,-4.06837383318914,332.233318196282));
#39098=CARTESIAN_POINT('Ctrl Pts',(122.655539080278,-4.14023965019631,332.342084310452));
#39099=CARTESIAN_POINT('Ctrl Pts',(122.648127276101,-4.2075870294846,332.453356237749));
#39100=CARTESIAN_POINT('Ctrl Pts',(122.640098530856,-4.28054024550361,332.573890177372));
#39101=CARTESIAN_POINT('Ctrl Pts',(122.632069785611,-4.348409418628,332.697724738684));
#39102=CARTESIAN_POINT('Ctrl Pts',(122.624041040366,-4.41089340609883,332.824407569756));
#39103=CARTESIAN_POINT('Ctrl Pts',(122.616024308214,-4.47328390125301,332.950900850324));
#39104=CARTESIAN_POINT('Ctrl Pts',(122.608007576063,-4.53030510255302,333.080233596217));
#39105=CARTESIAN_POINT('Ctrl Pts',(122.599990843912,-4.58169993115081,333.211925951368));
#39106=CARTESIAN_POINT('Ctrl Pts',(122.591984868597,-4.63302579826329,333.343441601961));
#39107=CARTESIAN_POINT('Ctrl Pts',(122.583978893282,-4.67874020175239,333.47731022567));
#39108=CARTESIAN_POINT('Ctrl Pts',(122.575972917967,-4.71863265997295,333.613028881794));
#39109=CARTESIAN_POINT('Ctrl Pts',(122.567979254774,-4.7584637689112,333.748538820719));
#39110=CARTESIAN_POINT('Ctrl Pts',(122.559985591582,-4.79249068257633,333.885892779966));
#39111=CARTESIAN_POINT('Ctrl Pts',(122.551991928389,-4.82055175829656,334.024569936857));
#39112=CARTESIAN_POINT('Ctrl Pts',(122.544005574865,-4.84858717404663,334.163120282796));
#39113=CARTESIAN_POINT('Ctrl Pts',(122.536019221341,-4.87066754613693,334.302991069189));
#39114=CARTESIAN_POINT('Ctrl Pts',(122.528032867817,-4.88668140797001,334.443647701991));
#39115=CARTESIAN_POINT('Ctrl Pts',(122.520054174503,-4.90267990991051,334.584169422253));
#39116=CARTESIAN_POINT('Ctrl Pts',(122.512075481188,-4.91262346031404,334.725475133635));
#39117=CARTESIAN_POINT('Ctrl Pts',(122.504096787873,-4.91645195726336,334.867021752075));
#39118=CARTESIAN_POINT('Ctrl Pts',(122.501576608079,-4.91766124057254,334.911731194296));
#39119=CARTESIAN_POINT('Ctrl Pts',(122.499056428284,-4.91826081210291,334.956464617952));
#39120=CARTESIAN_POINT('Ctrl Pts',(122.49653624849,-4.91824985243613,335.001204787119));
#39121=CARTESIAN_POINT('',(125.996536248531,-4.91824989020686,335.001039220942));
#39122=CARTESIAN_POINT('Ctrl Pts',(125.99653624849,-4.91824989020671,335.001039221667));
#39123=CARTESIAN_POINT('Ctrl Pts',(125.993352061456,-4.91823808096415,335.056927977462));
#39124=CARTESIAN_POINT('Ctrl Pts',(125.990167874422,-4.91727366286132,335.112805554363));
#39125=CARTESIAN_POINT('Ctrl Pts',(125.986983687388,-4.91535758023749,335.168650291734));
#39126=CARTESIAN_POINT('Ctrl Pts',(125.97920860861,-4.91067893128005,335.305010759195));
#39127=CARTESIAN_POINT('Ctrl Pts',(125.971433529831,-4.90031427907279,335.441391864294));
#39128=CARTESIAN_POINT('Ctrl Pts',(125.963658451053,-4.88425326763991,335.577280763623));
#39129=CARTESIAN_POINT('Ctrl Pts',(125.955892940004,-4.86821202030407,335.71300244301));
#39130=CARTESIAN_POINT('Ctrl Pts',(125.948127428955,-4.84648840654108,335.848232737317));
#39131=CARTESIAN_POINT('Ctrl Pts',(125.940361917906,-4.81912405979518,335.982459342061));
#39132=CARTESIAN_POINT('Ctrl Pts',(125.932604106383,-4.79178684487883,336.116552860735));
#39133=CARTESIAN_POINT('Ctrl Pts',(125.924846294861,-4.7588201045514,336.249644289744));
#39134=CARTESIAN_POINT('Ctrl Pts',(125.917088483339,-4.72031716063909,336.381227340258));
#39135=CARTESIAN_POINT('Ctrl Pts',(125.909336509816,-4.68184319141301,336.512711370354));
#39136=CARTESIAN_POINT('Ctrl Pts',(125.901584536293,-4.63784142048731,336.642688907688));
#39137=CARTESIAN_POINT('Ctrl Pts',(125.89383256277,-4.58845597047808,336.770665092411));
#39138=CARTESIAN_POINT('Ctrl Pts',(125.886083872212,-4.53909143523628,336.898587079144));
#39139=CARTESIAN_POINT('Ctrl Pts',(125.878335181655,-4.48434789608241,337.024509035126));
#39140=CARTESIAN_POINT('Ctrl Pts',(125.870586491097,-4.42441886726431,337.147952687909));
#39141=CARTESIAN_POINT('Ctrl Pts',(125.862839412719,-4.36450230718121,337.271370657209));
#39142=CARTESIAN_POINT('Ctrl Pts',(125.855092334341,-4.2994025740111,337.39231099753));
#39143=CARTESIAN_POINT('Ctrl Pts',(125.847345255964,-4.22936056313782,337.510317169099));
#39144=CARTESIAN_POINT('Ctrl Pts',(125.839598112658,-4.15931796524507,337.628324329674));
#39145=CARTESIAN_POINT('Ctrl Pts',(125.831850969352,-4.08433320653738,337.743396936323));
#39146=CARTESIAN_POINT('Ctrl Pts',(125.824103826046,-4.0046920054174,337.855105077619));
#39147=CARTESIAN_POINT('Ctrl Pts',(125.816354941018,-3.9250328992646,337.966838333277));
#39148=CARTESIAN_POINT('Ctrl Pts',(125.80860605599,-3.84071549441394,338.075205300218));
#39149=CARTESIAN_POINT('Ctrl Pts',(125.800857170962,-3.75206725682389,338.179807283904));
#39150=CARTESIAN_POINT('Ctrl Pts',(125.793100061187,-3.66332492707852,338.284520293217));
#39151=CARTESIAN_POINT('Ctrl Pts',(125.785342951412,-3.57024283518527,338.385460037843));
#39152=CARTESIAN_POINT('Ctrl Pts',(125.777585841638,-3.47318733026035,338.482262602306));
#39153=CARTESIAN_POINT('Ctrl Pts',(125.769824586712,-3.3760799619769,338.579116894964));
#39154=CARTESIAN_POINT('Ctrl Pts',(125.762063331785,-3.27499523778071,338.671829338219));
#39155=CARTESIAN_POINT('Ctrl Pts',(125.754302076859,-3.17033363711312,338.760075490185));
#39156=CARTESIAN_POINT('Ctrl Pts',(125.746528406455,-3.06550461199349,338.848462807235));
#39157=CARTESIAN_POINT('Ctrl Pts',(125.73875473605,-2.95708758575487,338.932369316592));
#39158=CARTESIAN_POINT('Ctrl Pts',(125.730981065645,-2.84551385381968,339.011512678557));
#39159=CARTESIAN_POINT('Ctrl Pts',(125.723569261468,-2.73913390594905,339.086971897981));
#39160=CARTESIAN_POINT('Ctrl Pts',(125.716157457291,-2.62988476906911,339.158101282463));
#39161=CARTESIAN_POINT('Ctrl Pts',(125.708745653114,-2.51816040151034,339.224695403785));
#39162=CARTESIAN_POINT('Ctrl Pts',(125.700970574336,-2.40096008988791,339.294553501367));
#39163=CARTESIAN_POINT('Ctrl Pts',(125.693195495557,-2.280665401014,339.359641285721));
#39164=CARTESIAN_POINT('Ctrl Pts',(125.685420416779,-2.15770199163858,339.419672519291));
#39165=CARTESIAN_POINT('Ctrl Pts',(125.67765490573,-2.03488989656664,339.479629880607));
#39166=CARTESIAN_POINT('Ctrl Pts',(125.669889394681,-1.90941596316459,339.534542902102));
#39167=CARTESIAN_POINT('Ctrl Pts',(125.662123883632,-1.78173352944661,339.584169356879));
#39168=CARTESIAN_POINT('Ctrl Pts',(125.654366072109,-1.6541776932334,339.633746606881));
#39169=CARTESIAN_POINT('Ctrl Pts',(125.646608260587,-1.52441807637631,339.678047580646));
#39170=CARTESIAN_POINT('Ctrl Pts',(125.638850449065,-1.39293092974834,339.716876772553));
#39171=CARTESIAN_POINT('Ctrl Pts',(125.631098475542,-1.26154273136795,339.755676744262));
#39172=CARTESIAN_POINT('Ctrl Pts',(125.623346502019,-1.1284299642057,339.789013019915));
#39173=CARTESIAN_POINT('Ctrl Pts',(125.615594528496,-0.994086759483296,
339.816738998235));
#39174=CARTESIAN_POINT('Ctrl Pts',(125.607845837938,-0.859800449187851,
339.844453234588));
#39175=CARTESIAN_POINT('Ctrl Pts',(125.600097147381,-0.724285119755702,
339.866561820393));
#39176=CARTESIAN_POINT('Ctrl Pts',(125.592348456823,-0.588047682355619,
339.882968665246));
#39177=CARTESIAN_POINT('Ctrl Pts',(125.584601378445,-0.451838590292264,
339.899372096518));
#39178=CARTESIAN_POINT('Ctrl Pts',(125.576854300067,-0.314908076926829,
339.910076099757));
#39179=CARTESIAN_POINT('Ctrl Pts',(125.56910722169,-0.177770418609592,339.915036189162));
#39180=CARTESIAN_POINT('Ctrl Pts',(125.561360078384,-0.0406316109467381,
339.919996320137));
#39181=CARTESIAN_POINT('Ctrl Pts',(125.553612935078,0.0967139545117735,
339.919212427132));
#39182=CARTESIAN_POINT('Ctrl Pts',(125.545865791772,0.233750137453922,339.912692127107));
#39183=CARTESIAN_POINT('Ctrl Pts',(125.538116906744,0.370817129039309,339.90617036118));
#39184=CARTESIAN_POINT('Ctrl Pts',(125.530368021716,0.507574209343861,339.893909640515));
#39185=CARTESIAN_POINT('Ctrl Pts',(125.522619136688,0.643508897006027,339.875969581732));
#39186=CARTESIAN_POINT('Ctrl Pts',(125.514862026913,0.779587867150193,339.858010481185));
#39187=CARTESIAN_POINT('Ctrl Pts',(125.507104917139,0.914842312834073,339.834360052031));
#39188=CARTESIAN_POINT('Ctrl Pts',(125.499347807364,1.04876795724189,339.805129429512));
#39189=CARTESIAN_POINT('Ctrl Pts',(125.491586552438,1.18276516723197,339.775883187083));
#39190=CARTESIAN_POINT('Ctrl Pts',(125.483825297511,1.31543178320089,339.741050908843));
#39191=CARTESIAN_POINT('Ctrl Pts',(125.476064042585,1.44627825264097,339.700793792376));
#39192=CARTESIAN_POINT('Ctrl Pts',(125.468290372181,1.5773340337894,339.660472277642));
#39193=CARTESIAN_POINT('Ctrl Pts',(125.460516701776,1.70656348144028,339.61470871407));
#39194=CARTESIAN_POINT('Ctrl Pts',(125.452743031371,1.8334957714153,339.563712996969));
#39195=CARTESIAN_POINT('Ctrl Pts',(125.445331227194,1.95451933275402,339.515091142767));
#39196=CARTESIAN_POINT('Ctrl Pts',(125.437919423017,2.07345452632375,339.461713404183));
#39197=CARTESIAN_POINT('Ctrl Pts',(125.43050761884,2.18991540969609,339.403799900186));
#39198=CARTESIAN_POINT('Ctrl Pts',(125.422732540062,2.31208438788146,339.343047882842));
#39199=CARTESIAN_POINT('Ctrl Pts',(125.414957461283,2.43191645298921,339.277112247443));
#39200=CARTESIAN_POINT('Ctrl Pts',(125.407182382505,2.54894055446037,339.206196038266));
#39201=CARTESIAN_POINT('Ctrl Pts',(125.399416871456,2.66582065032452,339.135367096));
#39202=CARTESIAN_POINT('Ctrl Pts',(125.391651360407,2.77989932667487,339.059569975373));
#39203=CARTESIAN_POINT('Ctrl Pts',(125.383885849358,2.89072756253167,338.979054815119));
#39204=CARTESIAN_POINT('Ctrl Pts',(125.376128037835,3.00144591186995,338.898619485881));
#39205=CARTESIAN_POINT('Ctrl Pts',(125.368370226313,3.10891992011577,338.813475654659));
#39206=CARTESIAN_POINT('Ctrl Pts',(125.360612414791,3.21272745574601,338.723918011664));
#39207=CARTESIAN_POINT('Ctrl Pts',(125.352860441268,3.31645687291369,338.634427763635));
#39208=CARTESIAN_POINT('Ctrl Pts',(125.345108467745,3.41652501462897,338.540530569483));
#39209=CARTESIAN_POINT('Ctrl Pts',(125.337356494222,3.5125411979933,338.442562620331));
#39210=CARTESIAN_POINT('Ctrl Pts',(125.329607803664,3.60851671844701,338.344636160663));
#39211=CARTESIAN_POINT('Ctrl Pts',(125.321859113107,3.7004434205406,338.242642653421));
#39212=CARTESIAN_POINT('Ctrl Pts',(125.314110422549,3.78796618108195,338.136956370988));
#39213=CARTESIAN_POINT('Ctrl Pts',(125.306363344171,3.87547073178196,338.031292077468));
#39214=CARTESIAN_POINT('Ctrl Pts',(125.298616265794,3.95857291431835,337.921936837842));
#39215=CARTESIAN_POINT('Ctrl Pts',(125.290869187416,4.03695701519037,337.809299044247));
#39216=CARTESIAN_POINT('Ctrl Pts',(125.28312204411,4.11534177299659,337.696660306638));
#39217=CARTESIAN_POINT('Ctrl Pts',(125.275374900804,4.18900814700185,337.58073928102));
#39218=CARTESIAN_POINT('Ctrl Pts',(125.267627757498,4.25768322933087,337.461974122767));
#39219=CARTESIAN_POINT('Ctrl Pts',(125.25987887247,4.32637375127644,337.343182263585));
#39220=CARTESIAN_POINT('Ctrl Pts',(125.252129987442,4.3900705529706,337.221545337701));
#39221=CARTESIAN_POINT('Ctrl Pts',(125.244381102414,4.44854643423001,337.097526563598));
#39222=CARTESIAN_POINT('Ctrl Pts',(125.236623992639,4.50708438239397,336.973376154687));
#39223=CARTESIAN_POINT('Ctrl Pts',(125.228866882865,4.5603901734167,336.846839201508));
#39224=CARTESIAN_POINT('Ctrl Pts',(125.22110977309,4.6082843701736,336.71839990285));
#39225=CARTESIAN_POINT('Ctrl Pts',(125.213348518164,4.65620416005789,336.589891970337));
#39226=CARTESIAN_POINT('Ctrl Pts',(125.205587263238,4.69870647248079,336.459480038218));
#39227=CARTESIAN_POINT('Ctrl Pts',(125.197826008311,4.73566193697881,336.327663014906));
#39228=CARTESIAN_POINT('Ctrl Pts',(125.190052337907,4.77267651817627,336.195635127316));
#39229=CARTESIAN_POINT('Ctrl Pts',(125.182278667502,4.8041264305537,336.062198037635));
#39230=CARTESIAN_POINT('Ctrl Pts',(125.174504997097,4.82993338957599,335.927861258357));
#39231=CARTESIAN_POINT('Ctrl Pts',(125.16709319292,4.85453902844704,335.799777888472));
#39232=CARTESIAN_POINT('Ctrl Pts',(125.159681388743,4.87401520704816,335.670876989667));
#39233=CARTESIAN_POINT('Ctrl Pts',(125.152269584566,4.88833817252304,335.541602228166));
#39234=CARTESIAN_POINT('Ctrl Pts',(125.144494505788,4.90336314920172,335.405991325514));
#39235=CARTESIAN_POINT('Ctrl Pts',(125.136719427009,4.91276447311226,335.26954042976));
#39236=CARTESIAN_POINT('Ctrl Pts',(125.128944348231,4.91645797603193,335.132755536276));
#39237=CARTESIAN_POINT('Ctrl Pts',(125.121178837182,4.92014693386112,334.996138965312));
#39238=CARTESIAN_POINT('Ctrl Pts',(125.113413326133,4.91814203567155,334.859189601398));
#39239=CARTESIAN_POINT('Ctrl Pts',(125.105647815084,4.91041063744346,334.722420400277));
#39240=CARTESIAN_POINT('Ctrl Pts',(125.097890003562,4.90268690491922,334.585786806218));
#39241=CARTESIAN_POINT('Ctrl Pts',(125.09013219204,4.88924799350033,334.4493334072));
#39242=CARTESIAN_POINT('Ctrl Pts',(125.082374380517,4.87011327488168,334.313574656411));
#39243=CARTESIAN_POINT('Ctrl Pts',(125.074622406994,4.8509929557456,334.177918068387));
#39244=CARTESIAN_POINT('Ctrl Pts',(125.066870433471,4.82618541536519,334.042955473583));
#39245=CARTESIAN_POINT('Ctrl Pts',(125.059118459948,4.79576194309461,333.90919733789));
#39246=CARTESIAN_POINT('Ctrl Pts',(125.051369769391,4.76535135518257,333.775495848848));
#39247=CARTESIAN_POINT('Ctrl Pts',(125.043621078833,4.72932965226221,333.642998184732));
#39248=CARTESIAN_POINT('Ctrl Pts',(125.035872388276,4.68781939042985,333.512205516474));
#39249=CARTESIAN_POINT('Ctrl Pts',(125.028125309898,4.64631776515417,333.381440060723));
#39250=CARTESIAN_POINT('Ctrl Pts',(125.02037823152,4.59932997053408,333.252379267558));
#39251=CARTESIAN_POINT('Ctrl Pts',(125.012631153142,4.54702858153806,333.125509631613));
#39252=CARTESIAN_POINT('Ctrl Pts',(125.004884009836,4.49472675420606,332.998638932379));
#39253=CARTESIAN_POINT('Ctrl Pts',(124.997136866531,4.43711139264739,332.873959788366));
#39254=CARTESIAN_POINT('Ctrl Pts',(124.989389723225,4.37440326495255,332.751938804642));
#39255=CARTESIAN_POINT('Ctrl Pts',(124.981640838197,4.31168103913931,332.629890388012));
#39256=CARTESIAN_POINT('Ctrl Pts',(124.973891953169,4.24386394747163,332.510501668434));
#39257=CARTESIAN_POINT('Ctrl Pts',(124.966143068141,4.17121856919917,332.394214377492));
#39258=CARTESIAN_POINT('Ctrl Pts',(124.958385958366,4.09849608437156,332.277803658018));
#39259=CARTESIAN_POINT('Ctrl Pts',(124.950628848591,4.02093528310379,332.164501275064));
#39260=CARTESIAN_POINT('Ctrl Pts',(124.942871738816,3.93884623476317,332.054720148884));
#39261=CARTESIAN_POINT('Ctrl Pts',(124.93511048389,3.85671332065985,331.94488035918));
#39262=CARTESIAN_POINT('Ctrl Pts',(124.927349228964,3.77004758475939,331.838565878412));
#39263=CARTESIAN_POINT('Ctrl Pts',(124.919587974038,3.67919856000733,331.736155484932));
#39264=CARTESIAN_POINT('Ctrl Pts',(124.911814303633,3.58820420642329,331.633581268198));
#39265=CARTESIAN_POINT('Ctrl Pts',(124.904040633229,3.49301346313851,331.53492390008));
#39266=CARTESIAN_POINT('Ctrl Pts',(124.896266962824,3.39401242582346,331.440524938161));
#39267=CARTESIAN_POINT('Ctrl Pts',(124.888855158647,3.29961991061364,331.350520270629));
#39268=CARTESIAN_POINT('Ctrl Pts',(124.88144335447,3.20176407261195,331.264386663862));
#39269=CARTESIAN_POINT('Ctrl Pts',(124.874031550293,3.10080514617983,331.182384185395));
#39270=CARTESIAN_POINT('Ctrl Pts',(124.866256471514,2.99489792202207,331.096362521185));
#39271=CARTESIAN_POINT('Ctrl Pts',(124.858481392736,2.88524104854596,331.014615338097));
#39272=CARTESIAN_POINT('Ctrl Pts',(124.850706313957,2.77221447980072,330.937487238114));
#39273=CARTESIAN_POINT('Ctrl Pts',(124.842940802908,2.65932699744387,330.860454049169));
#39274=CARTESIAN_POINT('Ctrl Pts',(124.835175291859,2.54307839019052,330.788028851863));
#39275=CARTESIAN_POINT('Ctrl Pts',(124.82740978081,2.42388234791601,330.720516687033));
#39276=CARTESIAN_POINT('Ctrl Pts',(124.819651969288,2.30480448886452,330.653071460712));
#39277=CARTESIAN_POINT('Ctrl Pts',(124.811894157766,2.18278534843191,330.590529764128));
#39278=CARTESIAN_POINT('Ctrl Pts',(124.804136346244,2.0582680244126,330.533153707348));
#39279=CARTESIAN_POINT('Ctrl Pts',(124.796384372721,1.93384440362837,330.47582082787));
#39280=CARTESIAN_POINT('Ctrl Pts',(124.788632399198,1.80692669480055,330.423646013621));
#39281=CARTESIAN_POINT('Ctrl Pts',(124.780880425675,1.6779827383479,330.376845558246));
#39282=CARTESIAN_POINT('Ctrl Pts',(124.773131735117,1.54909338973727,330.330064922892));
#39283=CARTESIAN_POINT('Ctrl Pts',(124.765383044559,1.41817986689333,330.2886542526));
#39284=CARTESIAN_POINT('Ctrl Pts',(124.757634354002,1.28572993728018,330.252781699681));
#39285=CARTESIAN_POINT('Ctrl Pts',(124.749887275624,1.15330756498117,330.216916610347));
#39286=CARTESIAN_POINT('Ctrl Pts',(124.742140197246,1.0193497987886,330.186587448595));
#39287=CARTESIAN_POINT('Ctrl Pts',(124.734393118868,0.884359132638813,330.161912362615));
#39288=CARTESIAN_POINT('Ctrl Pts',(124.726645975562,0.749367335137269,330.137237069834));
#39289=CARTESIAN_POINT('Ctrl Pts',(124.718898832256,0.613343004915525,330.118216017625));
#39290=CARTESIAN_POINT('Ctrl Pts',(124.711151688951,0.476797990411733,330.104916064168));
#39291=CARTESIAN_POINT('Ctrl Pts',(124.703402803923,0.340222277689887,330.091613120599));
#39292=CARTESIAN_POINT('Ctrl Pts',(124.695653918894,0.203126036705078,330.08403387311));
#39293=CARTESIAN_POINT('Ctrl Pts',(124.687905033866,0.0660249902972504,
330.082193195828));
#39294=CARTESIAN_POINT('Ctrl Pts',(124.680147924092,-0.0712215765778929,
330.080350564833));
#39295=CARTESIAN_POINT('Ctrl Pts',(124.672390814317,-0.208472567608445,
330.0842586766));
#39296=CARTESIAN_POINT('Ctrl Pts',(124.664633704542,-0.345212953016926,
330.093880242027));
#39297=CARTESIAN_POINT('Ctrl Pts',(124.656872449616,-0.482026408115212,
330.103506948911));
#39298=CARTESIAN_POINT('Ctrl Pts',(124.64911119469,-0.618328325687482,330.118853149295));
#39299=CARTESIAN_POINT('Ctrl Pts',(124.641349939764,-0.75361103060421,330.139829892169));
#39300=CARTESIAN_POINT('Ctrl Pts',(124.633576269359,-0.889110143760274,
330.160840190995));
#39301=CARTESIAN_POINT('Ctrl Pts',(124.625802598954,-1.02358640260804,330.187498954982));
#39302=CARTESIAN_POINT('Ctrl Pts',(124.61802892855,-1.15654364556947,330.219666344449));
#39303=CARTESIAN_POINT('Ctrl Pts',(124.610617124372,-1.28331169688312,330.250336334197));
#39304=CARTESIAN_POINT('Ctrl Pts',(124.603205320195,-1.40869869330304,330.286013559068));
#39305=CARTESIAN_POINT('Ctrl Pts',(124.595793516018,-1.53229099500652,330.32653582777));
#39306=CARTESIAN_POINT('Ctrl Pts',(124.58801843724,-1.66194092357931,330.369044213569));
#39307=CARTESIAN_POINT('Ctrl Pts',(124.580243358461,-1.79002550018592,330.417018926481));
#39308=CARTESIAN_POINT('Ctrl Pts',(124.572468279683,-1.91604932672805,330.470326938945));
#39309=CARTESIAN_POINT('Ctrl Pts',(124.564702768634,-2.0419180729286,330.523569352506));
#39310=CARTESIAN_POINT('Ctrl Pts',(124.556937257585,-2.16573075819596,330.582131856382));
#39311=CARTESIAN_POINT('Ctrl Pts',(124.549171746536,-2.28700699585225,330.64583164503));
#39312=CARTESIAN_POINT('Ctrl Pts',(124.541413935014,-2.40816298776578,330.709468275152));
#39313=CARTESIAN_POINT('Ctrl Pts',(124.533656123492,-2.52678719303667,330.778231872843));
#39314=CARTESIAN_POINT('Ctrl Pts',(124.525898311969,-2.6424194120768,330.851891670511));
#39315=CARTESIAN_POINT('Ctrl Pts',(124.518146338446,-2.75796461420512,330.925496036844));
#39316=CARTESIAN_POINT('Ctrl Pts',(124.510394364923,-2.87052198339134,331.003989060088));
#39317=CARTESIAN_POINT('Ctrl Pts',(124.5026423914,-2.97965645839908,331.087094372155));
#39318=CARTESIAN_POINT('Ctrl Pts',(124.494893700843,-3.08874471489186,331.170164489073));
#39319=CARTESIAN_POINT('Ctrl Pts',(124.487145010285,-3.19441265002579,331.257842773511));
#39320=CARTESIAN_POINT('Ctrl Pts',(124.479396319727,-3.29625490197135,331.349810048267));
#39321=CARTESIAN_POINT('Ctrl Pts',(124.47164924135,-3.39807596478578,331.441758188464));
#39322=CARTESIAN_POINT('Ctrl Pts',(124.463902162972,-3.49607263772918,331.537993282208));
#39323=CARTESIAN_POINT('Ctrl Pts',(124.456155084594,-3.5898736391659,331.638156708393));
#39324=CARTESIAN_POINT('Ctrl Pts',(124.448407941288,-3.6836754267453,331.738320974044));
#39325=CARTESIAN_POINT('Ctrl Pts',(124.440660797982,-3.77328120550124,331.842413352502));
#39326=CARTESIAN_POINT('Ctrl Pts',(124.432913654677,-3.85835776240475,331.950039600291));
#39327=CARTESIAN_POINT('Ctrl Pts',(124.425164769648,-3.94345344632432,332.057690044746));
#39328=CARTESIAN_POINT('Ctrl Pts',(124.41741588462,-4.02401763981144,332.168875632897));
#39329=CARTESIAN_POINT('Ctrl Pts',(124.409666999592,-4.09975874767403,332.283170731649));
#39330=CARTESIAN_POINT('Ctrl Pts',(124.401909889818,-4.17558024793119,332.397587144399));
#39331=CARTESIAN_POINT('Ctrl Pts',(124.394152780043,-4.24656822007687,332.515119334403));
#39332=CARTESIAN_POINT('Ctrl Pts',(124.386395670268,-4.31247530914839,332.635314022859));
#39333=CARTESIAN_POINT('Ctrl Pts',(124.378634415342,-4.37841761686099,332.755572939514));
#39334=CARTESIAN_POINT('Ctrl Pts',(124.370873160416,-4.43927345816176,332.878496839467));
#39335=CARTESIAN_POINT('Ctrl Pts',(124.363111905489,-4.49484290171026,333.003610671376));
#39336=CARTESIAN_POINT('Ctrl Pts',(124.355338235085,-4.55050123825842,333.128924644641));
#39337=CARTESIAN_POINT('Ctrl Pts',(124.34756456468,-4.60085613479065,333.256435186504));
#39338=CARTESIAN_POINT('Ctrl Pts',(124.339790894275,-4.64575668397817,333.385649388834));
#39339=CARTESIAN_POINT('Ctrl Pts',(124.332379090098,-4.68856710179801,333.508848638956));
#39340=CARTESIAN_POINT('Ctrl Pts',(124.324967285921,-4.72641946073029,333.633596232795));
#39341=CARTESIAN_POINT('Ctrl Pts',(124.317555481744,-4.75922630665098,333.759456560784));
#39342=CARTESIAN_POINT('Ctrl Pts',(124.307455587595,-4.80393143690577,333.930963519126));
#39343=CARTESIAN_POINT('Ctrl Pts',(124.297355693447,-4.83938417614909,334.104974579676));
#39344=CARTESIAN_POINT('Ctrl Pts',(124.287255799298,-4.86535496713038,334.280622417419));
#39345=CARTESIAN_POINT('Ctrl Pts',(124.277360004687,-4.8908009381128,334.452720748408));
#39346=CARTESIAN_POINT('Ctrl Pts',(124.267464210076,-4.90714435346763,334.626390601291));
#39347=CARTESIAN_POINT('Ctrl Pts',(124.257568415465,-4.91421409236322,334.800794284924));
#39348=CARTESIAN_POINT('Ctrl Pts',(124.253891026484,-4.91684128714015,334.865604662434));
#39349=CARTESIAN_POINT('Ctrl Pts',(124.250213637502,-4.91818828344244,334.930516140544));
#39350=CARTESIAN_POINT('Ctrl Pts',(124.246536248521,-4.91824792744739,334.995484841147));
#39351=CARTESIAN_POINT('',(127.746536248441,-4.91824840624245,335.003959418342));
#39352=CARTESIAN_POINT('Ctrl Pts',(127.746536248441,-4.91824840624245,335.003959418342));
#39353=CARTESIAN_POINT('Ctrl Pts',(127.737429000281,-4.9181185842084,335.165219724011));
#39354=CARTESIAN_POINT('Ctrl Pts',(127.728321752122,-4.91005377499314,335.326144681731));
#39355=CARTESIAN_POINT('Ctrl Pts',(127.719214503963,-4.89417593406791,335.486029823046));
#39356=CARTESIAN_POINT('Ctrl Pts',(127.71004726698,-4.87819350688481,335.646968116909));
#39357=CARTESIAN_POINT('Ctrl Pts',(127.700880029996,-4.85429488696353,335.806852778631));
#39358=CARTESIAN_POINT('Ctrl Pts',(127.691712793013,-4.82265339123684,335.964985663361));
#39359=CARTESIAN_POINT('Ctrl Pts',(127.682478322858,-4.79077983451745,336.124278305977));
#39360=CARTESIAN_POINT('Ctrl Pts',(127.673243852703,-4.75104948174692,336.28179331331));
#39361=CARTESIAN_POINT('Ctrl Pts',(127.664009382549,-4.70368766144363,336.4368386987));
#39362=CARTESIAN_POINT('Ctrl Pts',(127.661476886043,-4.69069897422996,336.479358939727));
#39363=CARTESIAN_POINT('Ctrl Pts',(127.658944389537,-4.67713660103905,336.52169356915));
#39364=CARTESIAN_POINT('Ctrl Pts',(127.656411893031,-4.6630058067537,336.563828605916));
#39365=CARTESIAN_POINT('Ctrl Pts',(127.648636814253,-4.61962251342256,336.693188401455));
#39366=CARTESIAN_POINT('Ctrl Pts',(127.640861735474,-4.5707835927889,336.820945951818));
#39367=CARTESIAN_POINT('Ctrl Pts',(127.633086656696,-4.51662541614281,336.946606768907));
#39368=CARTESIAN_POINT('Ctrl Pts',(127.625321145647,-4.46253388458095,337.07211295236));
#39369=CARTESIAN_POINT('Ctrl Pts',(127.617555634598,-4.40313627426551,337.195527180802));
#39370=CARTESIAN_POINT('Ctrl Pts',(127.609790123549,-4.33861863191982,337.316370313499));
#39371=CARTESIAN_POINT('Ctrl Pts',(127.602032312027,-4.27416495900428,337.437093629878));
#39372=CARTESIAN_POINT('Ctrl Pts',(127.594274500505,-4.20460153953952,337.555250581073));
#39373=CARTESIAN_POINT('Ctrl Pts',(127.586516688982,-4.13016224482694,337.670382536998));
#39374=CARTESIAN_POINT('Ctrl Pts',(127.578764715459,-4.05577896804424,337.785427852476));
#39375=CARTESIAN_POINT('Ctrl Pts',(127.571012741937,-3.97652733085012,337.897452376836));
#39376=CARTESIAN_POINT('Ctrl Pts',(127.563260768414,-3.89268663417267,338.006022925833));
#39377=CARTESIAN_POINT('Ctrl Pts',(127.555512077856,-3.80888144408013,338.114547495138));
#39378=CARTESIAN_POINT('Ctrl Pts',(127.547763387298,-3.72049129833228,338.219620689684));
#39379=CARTESIAN_POINT('Ctrl Pts',(127.540014696741,-3.62783810535521,338.320839313161));
#39380=CARTESIAN_POINT('Ctrl Pts',(127.532267618363,-3.53520418964882,338.422036877257));
#39381=CARTESIAN_POINT('Ctrl Pts',(127.524520539985,-3.43830925470008,338.519381177332));
#39382=CARTESIAN_POINT('Ctrl Pts',(127.516773461607,-3.33751442170336,338.612503362963));
#39383=CARTESIAN_POINT('Ctrl Pts',(127.509026318302,-3.23671874394886,338.705626329048));
#39384=CARTESIAN_POINT('Ctrl Pts',(127.501279174996,-3.13202339005494,338.794526844864));
#39385=CARTESIAN_POINT('Ctrl Pts',(127.49353203169,-3.02382484559053,338.878874368382));
#39386=CARTESIAN_POINT('Ctrl Pts',(127.485783146662,-2.91560197579636,338.963240855013));
#39387=CARTESIAN_POINT('Ctrl Pts',(127.478034261634,-2.80387465642282,339.043052072208));
#39388=CARTESIAN_POINT('Ctrl Pts',(127.470285376606,-2.68907048078475,339.118019306884));
#39389=CARTESIAN_POINT('Ctrl Pts',(127.462528266831,-2.57414445080831,339.193066112558));
#39390=CARTESIAN_POINT('Ctrl Pts',(127.454771157056,-2.45613536860487,339.263258451128));
#39391=CARTESIAN_POINT('Ctrl Pts',(127.447014047282,-2.33549817369035,339.328352035497));
#39392=CARTESIAN_POINT('Ctrl Pts',(127.439252792356,-2.21479651411619,339.393480403796));
#39393=CARTESIAN_POINT('Ctrl Pts',(127.431491537429,-2.09146429476056,339.453504417898));
#39394=CARTESIAN_POINT('Ctrl Pts',(127.423730282503,-1.96597790680437,339.508227360333));
#39395=CARTESIAN_POINT('Ctrl Pts',(127.415956612099,-1.84029078152338,339.563037841643));
#39396=CARTESIAN_POINT('Ctrl Pts',(127.408182941694,-1.71244296628371,339.612530164576));
#39397=CARTESIAN_POINT('Ctrl Pts',(127.400409271289,-1.58292837745497,339.656556755195));
#39398=CARTESIAN_POINT('Ctrl Pts',(127.392997467112,-1.45944272389427,339.698533897428));
#39399=CARTESIAN_POINT('Ctrl Pts',(127.385585662935,-1.3344422571681,339.735542633752));
#39400=CARTESIAN_POINT('Ctrl Pts',(127.378173858758,-1.20836316771759,339.767498454893));
#39401=CARTESIAN_POINT('Ctrl Pts',(127.370398779979,-1.07610456652419,339.801020526018));
#39402=CARTESIAN_POINT('Ctrl Pts',(127.362623701201,-0.942240974504719,
339.829087776953));
#39403=CARTESIAN_POINT('Ctrl Pts',(127.354848622423,-0.807262015579741,
339.85154728934));
#39404=CARTESIAN_POINT('Ctrl Pts',(127.347083111374,-0.672449156856947,
339.873979163867));
#39405=CARTESIAN_POINT('Ctrl Pts',(127.339317600325,-0.536524044056986,
339.890816966678));
#39406=CARTESIAN_POINT('Ctrl Pts',(127.331552089276,-0.399990277402321,
339.901957857885));
#39407=CARTESIAN_POINT('Ctrl Pts',(127.323794277753,-0.263591884374801,
339.913087702867));
#39408=CARTESIAN_POINT('Ctrl Pts',(127.316036466231,-0.12658642552593,339.918531845505));
#39409=CARTESIAN_POINT('Ctrl Pts',(127.308278654709,0.0105138661390176,
339.91823876211));
#39410=CARTESIAN_POINT('Ctrl Pts',(127.300526681186,0.147510985486694,339.917945899269));
#39411=CARTESIAN_POINT('Ctrl Pts',(127.292774707663,0.284602406302951,339.91192440489));
#39412=CARTESIAN_POINT('Ctrl Pts',(127.28502273414,0.421272708956044,339.900174728231));
#39413=CARTESIAN_POINT('Ctrl Pts',(127.277274043582,0.557885131654915,339.888430027566));
#39414=CARTESIAN_POINT('Ctrl Pts',(127.269525353025,0.694076402276577,339.870962002953));
#39415=CARTESIAN_POINT('Ctrl Pts',(127.261776662467,0.829333261321776,339.847823161396));
#39416=CARTESIAN_POINT('Ctrl Pts',(127.254029584089,0.964561979047763,339.824689134068));
#39417=CARTESIAN_POINT('Ctrl Pts',(127.246282505712,1.09885628686149,339.795886702492));
#39418=CARTESIAN_POINT('Ctrl Pts',(127.238535427334,1.23171058717457,339.761519935057));
#39419=CARTESIAN_POINT('Ctrl Pts',(127.230788284028,1.36456600093455,339.727152879595));
#39420=CARTESIAN_POINT('Ctrl Pts',(127.223041140722,1.49598100470378,339.687221493146));
#39421=CARTESIAN_POINT('Ctrl Pts',(127.215293997416,1.625463077546,339.641880313627));
#39422=CARTESIAN_POINT('Ctrl Pts',(127.207545112388,1.75497426070709,339.596528940447));
#39423=CARTESIAN_POINT('Ctrl Pts',(127.19979622736,1.88255127936962,339.545765483179));
#39424=CARTESIAN_POINT('Ctrl Pts',(127.192047342332,2.00771995326452,339.489793274947));
#39425=CARTESIAN_POINT('Ctrl Pts',(127.184290232557,2.13302148248321,339.433761657236));
#39426=CARTESIAN_POINT('Ctrl Pts',(127.176533122783,2.25590920321444,339.372510404433));
#39427=CARTESIAN_POINT('Ctrl Pts',(127.168776013008,2.37593149535021,339.306289887119));
#39428=CARTESIAN_POINT('Ctrl Pts',(127.161014758082,2.49601792356133,339.240033983678));
#39429=CARTESIAN_POINT('Ctrl Pts',(127.153253503156,2.6132355382701,339.168803727451));
#39430=CARTESIAN_POINT('Ctrl Pts',(127.145492248229,2.72716111295764,339.092893270838));
#39431=CARTESIAN_POINT('Ctrl Pts',(127.137718577825,2.84126893143643,339.016861382233));
#39432=CARTESIAN_POINT('Ctrl Pts',(127.12994490742,2.95207387039609,338.936134562693));
#39433=CARTESIAN_POINT('Ctrl Pts',(127.122171237015,3.0591845452739,338.851048296303));
#39434=CARTESIAN_POINT('Ctrl Pts',(127.114759432838,3.16130919246735,338.769922816083));
#39435=CARTESIAN_POINT('Ctrl Pts',(127.107347628661,3.26007555345974,338.684834807632));
#39436=CARTESIAN_POINT('Ctrl Pts',(127.099935824484,3.35517651492205,338.596105339978));
#39437=CARTESIAN_POINT('Ctrl Pts',(127.092160745706,3.45493865779627,338.503026976803));
#39438=CARTESIAN_POINT('Ctrl Pts',(127.084385666927,3.55098227862865,338.405647026398));
#39439=CARTESIAN_POINT('Ctrl Pts',(127.076610588149,3.6429138215132,338.304294471068));
#39440=CARTESIAN_POINT('Ctrl Pts',(127.0688450771,3.73473223678157,338.203066636509));
#39441=CARTESIAN_POINT('Ctrl Pts',(127.061079566051,3.8224483823009,338.097876210574));
#39442=CARTESIAN_POINT('Ctrl Pts',(127.053314055002,3.90570325084063,337.98909102887));
#39443=CARTESIAN_POINT('Ctrl Pts',(127.045556243479,3.98887557193586,337.880413707991));
#39444=CARTESIAN_POINT('Ctrl Pts',(127.037798431957,4.0675951827806,337.768149032728));
#39445=CARTESIAN_POINT('Ctrl Pts',(127.030040620435,4.14154155733407,337.652699868318));
#39446=CARTESIAN_POINT('Ctrl Pts',(127.022288646912,4.21543228489564,337.537337583066));
#39447=CARTESIAN_POINT('Ctrl Pts',(127.014536673389,4.28455671591711,337.418795906462));
#39448=CARTESIAN_POINT('Ctrl Pts',(127.006784699866,4.34863630505158,337.297508508991));
#39449=CARTESIAN_POINT('Ctrl Pts',(126.999036009308,4.41268875644203,337.176272476805));
#39450=CARTESIAN_POINT('Ctrl Pts',(126.991287318751,4.47170043306779,337.052293381393));
#39451=CARTESIAN_POINT('Ctrl Pts',(126.983538628193,4.52543773502323,336.92603124817));
#39452=CARTESIAN_POINT('Ctrl Pts',(126.975791549815,4.57916385648417,336.799795384839));
#39453=CARTESIAN_POINT('Ctrl Pts',(126.968044471437,4.62761763306284,336.671277787946));
#39454=CARTESIAN_POINT('Ctrl Pts',(126.96029739306,4.67061297022109,336.540959942666));
#39455=CARTESIAN_POINT('Ctrl Pts',(126.952550249754,4.71360866772167,336.410641005198));
#39456=CARTESIAN_POINT('Ctrl Pts',(126.944803106448,4.75114571208938,336.278522160442));
#39457=CARTESIAN_POINT('Ctrl Pts',(126.937055963142,4.7830875262143,336.145101209096));
#39458=CARTESIAN_POINT('Ctrl Pts',(126.929307078114,4.81503652153716,336.011650261887));
#39459=CARTESIAN_POINT('Ctrl Pts',(126.921558193086,4.84138769249563,335.876897005623));
#39460=CARTESIAN_POINT('Ctrl Pts',(126.913809308058,4.86205542010043,335.741350223829));
#39461=CARTESIAN_POINT('Ctrl Pts',(126.906052198283,4.88274508464486,335.605659571281));
#39462=CARTESIAN_POINT('Ctrl Pts',(126.898295088508,4.89773919640854,335.469174097736));
#39463=CARTESIAN_POINT('Ctrl Pts',(126.890537978734,4.90700389979862,335.332409070064));
#39464=CARTESIAN_POINT('Ctrl Pts',(126.882776723808,4.91627355394997,335.195570959535));
#39465=CARTESIAN_POINT('Ctrl Pts',(126.875015468881,4.91980768912263,335.058453387763));
#39466=CARTESIAN_POINT('Ctrl Pts',(126.867254213955,4.91762463218933,334.921571437698));
#39467=CARTESIAN_POINT('Ctrl Pts',(126.859480543551,4.9154380830764,334.784470521123));
#39468=CARTESIAN_POINT('Ctrl Pts',(126.851706873146,4.90751608875082,334.647606369875));
#39469=CARTESIAN_POINT('Ctrl Pts',(126.843933202741,4.89392896429312,334.511489657271));
#39470=CARTESIAN_POINT('Ctrl Pts',(126.836521398564,4.88097432374781,334.381709210387));
#39471=CARTESIAN_POINT('Ctrl Pts',(126.829109594387,4.86287014731348,334.25260846662));
#39472=CARTESIAN_POINT('Ctrl Pts',(126.82169779021,4.83972023214225,334.124619432993));
#39473=CARTESIAN_POINT('Ctrl Pts',(126.813922711432,4.81543567066841,333.990357275569));
#39474=CARTESIAN_POINT('Ctrl Pts',(126.806147632653,4.78552150707733,333.856894266986));
#39475=CARTESIAN_POINT('Ctrl Pts',(126.798372553875,4.75004141392361,333.724739388003));
#39476=CARTESIAN_POINT('Ctrl Pts',(126.790607042826,4.7146049812833,333.592747134012));
#39477=CARTESIAN_POINT('Ctrl Pts',(126.782841531777,4.67361634746703,333.462060180604));
#39478=CARTESIAN_POINT('Ctrl Pts',(126.775076020728,4.62719055387269,333.333179481572));
#39479=CARTESIAN_POINT('Ctrl Pts',(126.767318209205,4.58081079158786,333.204426568129));
#39480=CARTESIAN_POINT('Ctrl Pts',(126.759560397683,4.52900472945568,333.07747671043));
#39481=CARTESIAN_POINT('Ctrl Pts',(126.751802586161,4.47193769041654,332.952817459157));
#39482=CARTESIAN_POINT('Ctrl Pts',(126.744050612638,4.414913596134,332.828252017924));
#39483=CARTESIAN_POINT('Ctrl Pts',(126.736298639115,4.35263656728711,332.705974106043));
#39484=CARTESIAN_POINT('Ctrl Pts',(126.728546665592,4.28532054976733,332.586452642221));
#39485=CARTESIAN_POINT('Ctrl Pts',(126.720797975034,4.21803304062094,332.46698179581));
#39486=CARTESIAN_POINT('Ctrl Pts',(126.713049284477,4.14571097862224,332.35026541553));
#39487=CARTESIAN_POINT('Ctrl Pts',(126.705300593919,4.06861479464466,332.236748886674));
#39488=CARTESIAN_POINT('Ctrl Pts',(126.697553515541,3.99153465117209,332.12325597588));
#39489=CARTESIAN_POINT('Ctrl Pts',(126.689806437164,3.90968258092601,332.012961915422));
#39490=CARTESIAN_POINT('Ctrl Pts',(126.682059358786,3.82336276862943,331.906283755423));
#39491=CARTESIAN_POINT('Ctrl Pts',(126.67431221548,3.73704223288972,331.799604701359));
#39492=CARTESIAN_POINT('Ctrl Pts',(126.666565072174,3.64625412628549,331.696541912057));
#39493=CARTESIAN_POINT('Ctrl Pts',(126.658817928868,3.55134315033103,331.597479626645));
#39494=CARTESIAN_POINT('Ctrl Pts',(126.65106904384,3.45641083637419,331.498395069927));
#39495=CARTESIAN_POINT('Ctrl Pts',(126.643320158812,3.35735407898259,331.403313088986));
#39496=CARTESIAN_POINT('Ctrl Pts',(126.635571273784,3.25455439172946,331.312581014615));
#39497=CARTESIAN_POINT('Ctrl Pts',(126.627814164009,3.15164559182608,331.221752636283));
#39498=CARTESIAN_POINT('Ctrl Pts',(126.620057054235,3.04498621956935,331.135283646546));
#39499=CARTESIAN_POINT('Ctrl Pts',(126.61229994446,2.93499125265941,331.053481355763));
#39500=CARTESIAN_POINT('Ctrl Pts',(126.604538689534,2.82493750795619,330.971635352451));
#39501=CARTESIAN_POINT('Ctrl Pts',(126.596777434607,2.71154493990857,330.894461236896));
#39502=CARTESIAN_POINT('Ctrl Pts',(126.589016179681,2.59525661048028,330.82222233858));
#39503=CARTESIAN_POINT('Ctrl Pts',(126.581242509277,2.47878225762314,330.749867881569));
#39504=CARTESIAN_POINT('Ctrl Pts',(126.573468838872,2.35940322727646,330.682464610102));
#39505=CARTESIAN_POINT('Ctrl Pts',(126.565695168467,2.23758700705245,330.620229749362));
#39506=CARTESIAN_POINT('Ctrl Pts',(126.55828336429,2.1214413611875,330.560891936363));
#39507=CARTESIAN_POINT('Ctrl Pts',(126.550871560113,2.00308058282386,330.50625230431));
#39508=CARTESIAN_POINT('Ctrl Pts',(126.543459755936,1.88292412648035,330.456457351755));
#39509=CARTESIAN_POINT('Ctrl Pts',(126.535684677158,1.75687844428347,330.404221800244));
#39510=CARTESIAN_POINT('Ctrl Pts',(126.527909598379,1.62845828266413,330.357152766548));
#39511=CARTESIAN_POINT('Ctrl Pts',(126.520134519601,1.49812611127402,330.315472145753));
#39512=CARTESIAN_POINT('Ctrl Pts',(126.512369008552,1.36795432191816,330.273842815615));
#39513=CARTESIAN_POINT('Ctrl Pts',(126.504603497503,1.23587557302824,330.23758882294));
#39514=CARTESIAN_POINT('Ctrl Pts',(126.496837986454,1.10237338283778,330.206884521805));
#39515=CARTESIAN_POINT('Ctrl Pts',(126.489080174932,0.969003560457524,330.176210664074));
#39516=CARTESIAN_POINT('Ctrl Pts',(126.481322363409,0.83421348391091,330.151075634573));
#39517=CARTESIAN_POINT('Ctrl Pts',(126.473564551887,0.698502610697266,330.131604251363));
#39518=CARTESIAN_POINT('Ctrl Pts',(126.465812578364,0.562893864219401,330.112147520986));
#39519=CARTESIAN_POINT('Ctrl Pts',(126.458060604841,0.426366085669455,330.098346008742));
#39520=CARTESIAN_POINT('Ctrl Pts',(126.450308631318,0.289429377190495,330.090273561784));
#39521=CARTESIAN_POINT('Ctrl Pts',(126.442559940761,0.152550661488875,330.082204533512));
#39522=CARTESIAN_POINT('Ctrl Pts',(126.434811250203,0.015263749689991,330.079859767816));
#39523=CARTESIAN_POINT('Ctrl Pts',(126.427062559645,-0.121915890122222,
330.083261286357));
#39524=CARTESIAN_POINT('Ctrl Pts',(126.419315481267,-0.259066988564671,
330.086662097183));
#39525=CARTESIAN_POINT('Ctrl Pts',(126.41156840289,-0.396110468905335,330.095806804505));
#39526=CARTESIAN_POINT('Ctrl Pts',(126.403821324512,-0.532531012990603,
330.110665302651));
#39527=CARTESIAN_POINT('Ctrl Pts',(126.396074181206,-0.668952700411195,
330.125523925325));
#39528=CARTESIAN_POINT('Ctrl Pts',(126.3883270379,-0.804751052586834,330.146096392015));
#39529=CARTESIAN_POINT('Ctrl Pts',(126.380579894594,-0.939416416870888,
330.172300769703));
#39530=CARTESIAN_POINT('Ctrl Pts',(126.372831009566,-1.07411205678781,330.198511038691));
#39531=CARTESIAN_POINT('Ctrl Pts',(126.365082124538,-1.20767381834649,330.230355663574));
#39532=CARTESIAN_POINT('Ctrl Pts',(126.35733323951,-1.33960316478618,330.267701782073));
#39533=CARTESIAN_POINT('Ctrl Pts',(126.349576129735,-1.47167254239741,330.305087540128));
#39534=CARTESIAN_POINT('Ctrl Pts',(126.341819019961,-1.60210566704428,330.3479863498));
#39535=CARTESIAN_POINT('Ctrl Pts',(126.334061910186,-1.73041954664402,330.396215550757));
#39536=CARTESIAN_POINT('Ctrl Pts',(126.32630065526,-1.8588019930783,330.444470523857));
#39537=CARTESIAN_POINT('Ctrl Pts',(126.318539400334,-1.98506257832049,330.498061411276));
#39538=CARTESIAN_POINT('Ctrl Pts',(126.310778145408,-2.10874009674039,330.556758135449));
#39539=CARTESIAN_POINT('Ctrl Pts',(126.303004475003,-2.23261545888335,330.615548755251));
#39540=CARTESIAN_POINT('Ctrl Pts',(126.295230804598,-2.35389915113358,330.67946135092));
#39541=CARTESIAN_POINT('Ctrl Pts',(126.287457134194,-2.47215551982878,330.74822035516));
#39542=CARTESIAN_POINT('Ctrl Pts',(126.280045330016,-2.58490702611154,330.81377861121));
#39543=CARTESIAN_POINT('Ctrl Pts',(126.272633525839,-2.69490646710385,330.883742074728));
#39544=CARTESIAN_POINT('Ctrl Pts',(126.265221721662,-2.801803658141,330.957837296233));
#39545=CARTESIAN_POINT('Ctrl Pts',(126.257489796435,-2.91331781424917,331.03513274261));
#39546=CARTESIAN_POINT('Ctrl Pts',(126.249757871209,-3.02181683019522,331.117175227558));
#39547=CARTESIAN_POINT('Ctrl Pts',(126.242025945982,-3.12686658200773,331.203700691354));
#39548=CARTESIAN_POINT('Ctrl Pts',(126.234303559797,-3.23178673168168,331.290119406825));
#39549=CARTESIAN_POINT('Ctrl Pts',(126.226581173613,-3.33326578005632,331.38100984988));
#39550=CARTESIAN_POINT('Ctrl Pts',(126.218858787429,-3.43089795556801,331.476064376158));
#39551=CARTESIAN_POINT('Ctrl Pts',(126.211144028533,-3.52843370120097,331.571025018465));
#39552=CARTESIAN_POINT('Ctrl Pts',(126.203429269637,-3.62212985195588,331.670141286756));
#39553=CARTESIAN_POINT('Ctrl Pts',(126.195714510741,-3.71161349914195,331.773065185739));
#39554=CARTESIAN_POINT('Ctrl Pts',(126.188005474514,-3.80103076898046,331.87591273764));
#39555=CARTESIAN_POINT('Ctrl Pts',(126.180296438286,-3.88624149514754,331.982562001969));
#39556=CARTESIAN_POINT('Ctrl Pts',(126.172587402058,-3.966909764782,332.092628338073));
#39557=CARTESIAN_POINT('Ctrl Pts',(126.164881483907,-4.04754540649268,332.202650155607));
#39558=CARTESIAN_POINT('Ctrl Pts',(126.157175565757,-4.1236420114915,332.31608597817));
#39559=CARTESIAN_POINT('Ctrl Pts',(126.149469647606,-4.19490428962288,332.432518536892));
#39560=CARTESIAN_POINT('Ctrl Pts',(126.141765161666,-4.26615332304912,332.548929455625));
#39561=CARTESIAN_POINT('Ctrl Pts',(126.134060675726,-4.33256961003524,332.668335665489));
#39562=CARTESIAN_POINT('Ctrl Pts',(126.126356189786,-4.39390176642594,332.79029179992));
#39563=CARTESIAN_POINT('Ctrl Pts',(126.118651420408,-4.45523617914033,332.912252420947));
#39564=CARTESIAN_POINT('Ctrl Pts',(126.110946651031,-4.51148591145028,333.036762799581));
#39565=CARTESIAN_POINT('Ctrl Pts',(126.103241881654,-4.56244624654336,333.163354331968));
#39566=CARTESIAN_POINT('Ctrl Pts',(126.095535113322,-4.61341980298235,333.28997870775));
#39567=CARTESIAN_POINT('Ctrl Pts',(126.087828344989,-4.65910108471449,333.418684944373));
#39568=CARTESIAN_POINT('Ctrl Pts',(126.080121576657,-4.69933425155995,333.548986335483));
#39569=CARTESIAN_POINT('Ctrl Pts',(126.072406696856,-4.73960976431207,333.679424870421));
#39570=CARTESIAN_POINT('Ctrl Pts',(126.064691817054,-4.77442559528901,333.811461533829));
#39571=CARTESIAN_POINT('Ctrl Pts',(126.056976937253,-4.80367624537959,333.944596005278));
#39572=CARTESIAN_POINT('Ctrl Pts',(126.049257603452,-4.8329437826263,334.077807338697));
#39573=CARTESIAN_POINT('Ctrl Pts',(126.041538269651,-4.85663967119378,334.212117353458));
#39574=CARTESIAN_POINT('Ctrl Pts',(126.03381893585,-4.87471008483557,334.347018643986));
#39575=CARTESIAN_POINT('Ctrl Pts',(126.026088189024,-4.89280721556078,334.482119385898));
#39576=CARTESIAN_POINT('Ctrl Pts',(126.018357442198,-4.90526222560895,334.617812756118));
#39577=CARTESIAN_POINT('Ctrl Pts',(126.010626695372,-4.91207334932376,334.753588812423));
#39578=CARTESIAN_POINT('Ctrl Pts',(126.005929879758,-4.91621144787085,334.836079562092));
#39579=CARTESIAN_POINT('Ctrl Pts',(126.001233064145,-4.91826730934574,334.918600853459));
#39580=CARTESIAN_POINT('Ctrl Pts',(125.996536248531,-4.91824989020686,335.001039220942));
#39581=CARTESIAN_POINT('',(129.496536248543,-4.91824916909057,334.997141112125));
#39582=CARTESIAN_POINT('Ctrl Pts',(129.49653624849,-4.91824916909112,334.997141113067));
#39583=CARTESIAN_POINT('Ctrl Pts',(129.488710570362,-4.9183298433808,335.13592808418));
#39584=CARTESIAN_POINT('Ctrl Pts',(129.480884892233,-4.91253157919313,335.274726350522));
#39585=CARTESIAN_POINT('Ctrl Pts',(129.473059214105,-4.90087810992756,335.413009460101));
#39586=CARTESIAN_POINT('Ctrl Pts',(129.465232246285,-4.88922272014096,335.551315359084));
#39587=CARTESIAN_POINT('Ctrl Pts',(129.457405278465,-4.87171023496562,335.689105553739));
#39588=CARTESIAN_POINT('Ctrl Pts',(129.449578310645,-4.84841629440405,335.825858643266));
#39589=CARTESIAN_POINT('Ctrl Pts',(129.441748490757,-4.82511386576545,335.96266156424));
#39590=CARTESIAN_POINT('Ctrl Pts',(129.433918670869,-4.79602584993982,336.098426253253));
#39591=CARTESIAN_POINT('Ctrl Pts',(129.426088850981,-4.76127898355548,336.232641676747));
#39592=CARTESIAN_POINT('Ctrl Pts',(129.418254615085,-4.72651251998405,336.366932797563));
#39593=CARTESIAN_POINT('Ctrl Pts',(129.410420379188,-4.68608094482974,336.499672545629));
#39594=CARTESIAN_POINT('Ctrl Pts',(129.402586143292,-4.64016072426206,336.630365454589));
#39595=CARTESIAN_POINT('Ctrl Pts',(129.394741224013,-4.59417788325398,336.761236586723));
#39596=CARTESIAN_POINT('Ctrl Pts',(129.386896304734,-4.54269157665094,336.890054947805));
#39597=CARTESIAN_POINT('Ctrl Pts',(129.379051385455,-4.48592650900079,337.016344816331));
#39598=CARTESIAN_POINT('Ctrl Pts',(129.371200172618,-4.42911590178636,337.142736000434));
#39599=CARTESIAN_POINT('Ctrl Pts',(129.363348959782,-4.36701826387414,337.266594311415));
#39600=CARTESIAN_POINT('Ctrl Pts',(129.355497746946,-4.29990366529128,337.387469692313));
#39601=CARTESIAN_POINT('Ctrl Pts',(129.347634273421,-4.23268425855185,337.508533835807));
#39602=CARTESIAN_POINT('Ctrl Pts',(129.339770799897,-4.16043244475512,337.626605425462));
#39603=CARTESIAN_POINT('Ctrl Pts',(129.331907326373,-4.08346121829752,337.741263858362));
#39604=CARTESIAN_POINT('Ctrl Pts',(129.32988491714,-4.06366496432108,337.770752896833));
#39605=CARTESIAN_POINT('Ctrl Pts',(129.327862507908,-4.04355673962888,337.80001634081));
#39606=CARTESIAN_POINT('Ctrl Pts',(129.325840098675,-4.02314228273049,337.829047407769));
#39607=CARTESIAN_POINT('Ctrl Pts',(129.318065019897,-3.94465964526313,337.940656289398));
#39608=CARTESIAN_POINT('Ctrl Pts',(129.310289941118,-3.86140513775162,338.049173195096));
#39609=CARTESIAN_POINT('Ctrl Pts',(129.30251486234,-3.77365052583071,338.154163085732));
#39610=CARTESIAN_POINT('Ctrl Pts',(129.294749351291,-3.68600390154654,338.259023779624));
#39611=CARTESIAN_POINT('Ctrl Pts',(129.286983840242,-3.59386843949686,338.360365797199));
#39612=CARTESIAN_POINT('Ctrl Pts',(129.279218329193,-3.49755913856428,338.457782979706));
#39613=CARTESIAN_POINT('Ctrl Pts',(129.271460517671,-3.40134532858401,338.555103572794));
#39614=CARTESIAN_POINT('Ctrl Pts',(129.263702706148,-3.30096618835245,338.648506798915));
#39615=CARTESIAN_POINT('Ctrl Pts',(129.255944894626,-3.19677670314018,338.737619800456));
#39616=CARTESIAN_POINT('Ctrl Pts',(129.248192921103,-3.09266562381965,338.826665741638));
#39617=CARTESIAN_POINT('Ctrl Pts',(129.24044094758,-2.98475020279728,338.911427631432));
#39618=CARTESIAN_POINT('Ctrl Pts',(129.232688974057,-2.87342170844965,338.991569960293));
#39619=CARTESIAN_POINT('Ctrl Pts',(129.2249402835,-2.76214036178536,339.071678348829));
#39620=CARTESIAN_POINT('Ctrl Pts',(129.217191592942,-2.64744913323816,339.14717083966));
#39621=CARTESIAN_POINT('Ctrl Pts',(129.209442902384,-2.52977157371988,339.217752819607));
#39622=CARTESIAN_POINT('Ctrl Pts',(129.201695824007,-2.41211849800069,339.288320114383));
#39623=CARTESIAN_POINT('Ctrl Pts',(129.193948745629,-2.29148066217425,339.35397872953));
#39624=CARTESIAN_POINT('Ctrl Pts',(129.186201667251,-2.16830940283761,339.41447815671));
#39625=CARTESIAN_POINT('Ctrl Pts',(129.178454523945,-2.04513711120714,339.474978090933));
#39626=CARTESIAN_POINT('Ctrl Pts',(129.170707380639,-1.919431704554,339.530318578621));
#39627=CARTESIAN_POINT('Ctrl Pts',(129.162960237334,-1.79166748630491,339.580295916316));
#39628=CARTESIAN_POINT('Ctrl Pts',(129.155211352306,-1.66387454394753,339.630284489976));
#39629=CARTESIAN_POINT('Ctrl Pts',(129.147462467278,-1.53402223288998,339.674907371972));
#39630=CARTESIAN_POINT('Ctrl Pts',(129.139713582249,-1.40260273933468,339.714009823718));
#39631=CARTESIAN_POINT('Ctrl Pts',(129.131956472475,-1.2710437557708,339.753153779211));
#39632=CARTESIAN_POINT('Ctrl Pts',(129.1241993627,-1.13791464209848,339.786765488022));
#39633=CARTESIAN_POINT('Ctrl Pts',(129.116442252925,-1.00372112120168,339.81474059253));
#39634=CARTESIAN_POINT('Ctrl Pts',(129.108680997999,-0.869455891578076,
339.842730646039));
#39635=CARTESIAN_POINT('Ctrl Pts',(129.100919743073,-0.734125506830217,
339.865078029869));
#39636=CARTESIAN_POINT('Ctrl Pts',(129.093158488147,-0.598242680140097,
339.881730098864));
#39637=CARTESIAN_POINT('Ctrl Pts',(129.085384817742,-0.462142485211244,
339.898408805743));
#39638=CARTESIAN_POINT('Ctrl Pts',(129.077611147338,-0.325488472218683,
339.909373960736));
#39639=CARTESIAN_POINT('Ctrl Pts',(129.069837476933,-0.188796132337487,
339.914625019563));
#39640=CARTESIAN_POINT('Ctrl Pts',(129.062425672756,-0.0584668537638033,
339.919631640338));
#39641=CARTESIAN_POINT('Ctrl Pts',(129.055013868579,0.0718969759700748,
339.919444175783));
#39642=CARTESIAN_POINT('Ctrl Pts',(129.047602064402,0.201853183231733,339.914106058575));
#39643=CARTESIAN_POINT('Ctrl Pts',(129.039826985623,0.338178931330607,339.90850630434));
#39644=CARTESIAN_POINT('Ctrl Pts',(129.032051906845,0.474486903596368,339.897220537189));
#39645=CARTESIAN_POINT('Ctrl Pts',(129.024276828066,0.610264198362322,339.880241866004));
#39646=CARTESIAN_POINT('Ctrl Pts',(129.016511317017,0.745874410522877,339.863284088155));
#39647=CARTESIAN_POINT('Ctrl Pts',(129.008745805968,0.880954860385049,339.840647393207));
#39648=CARTESIAN_POINT('Ctrl Pts',(129.000980294919,1.01499353642109,339.812376874635));
#39649=CARTESIAN_POINT('Ctrl Pts',(128.993222483397,1.14889931271969,339.784134386365));
#39650=CARTESIAN_POINT('Ctrl Pts',(128.985464671875,1.28176499076853,339.75026927098));
#39651=CARTESIAN_POINT('Ctrl Pts',(128.977706860353,1.41308492374687,339.710878268516));
#39652=CARTESIAN_POINT('Ctrl Pts',(128.96995488683,1.5443060343113,339.671516909032));
#39653=CARTESIAN_POINT('Ctrl Pts',(128.962202913307,1.67398334225606,339.626638051423));
#39654=CARTESIAN_POINT('Ctrl Pts',(128.954450939784,1.80162297267577,339.576389158149));
#39655=CARTESIAN_POINT('Ctrl Pts',(128.946702249226,1.92920854763621,339.526161545312));
#39656=CARTESIAN_POINT('Ctrl Pts',(128.938953558668,2.05475779848533,339.470568562943));
#39657=CARTESIAN_POINT('Ctrl Pts',(128.931204868111,2.1777937710154,339.409806951945));
#39658=CARTESIAN_POINT('Ctrl Pts',(128.923457789733,2.30080414488376,339.349057982909));
#39659=CARTESIAN_POINT('Ctrl Pts',(128.915710711355,2.42130193028902,339.283142697214));
#39660=CARTESIAN_POINT('Ctrl Pts',(128.907963632977,2.53883222529564,339.212305068997));
#39661=CARTESIAN_POINT('Ctrl Pts',(128.900216489671,2.65636350531941,339.141466847093));
#39662=CARTESIAN_POINT('Ctrl Pts',(128.892469346366,2.77092691056876,339.065706402156));
#39663=CARTESIAN_POINT('Ctrl Pts',(128.88472220306,2.88209446965961,338.985312350426));
#39664=CARTESIAN_POINT('Ctrl Pts',(128.876973318032,2.99328702157801,338.904900224406));
#39665=CARTESIAN_POINT('Ctrl Pts',(128.869224433003,3.10108189147329,338.819852647668));
#39666=CARTESIAN_POINT('Ctrl Pts',(128.861475547975,3.20508260617299,338.730499772163));
#39667=CARTESIAN_POINT('Ctrl Pts',(128.853718438201,3.30919370830552,338.641052056593));
#39668=CARTESIAN_POINT('Ctrl Pts',(128.845961328426,3.40950231367455,338.547290168998));
#39669=CARTESIAN_POINT('Ctrl Pts',(128.838204218651,3.50564699005738,338.449582908643));
#39670=CARTESIAN_POINT('Ctrl Pts',(128.830442963725,3.60184304308115,338.351823436652));
#39671=CARTESIAN_POINT('Ctrl Pts',(128.822681708799,3.6938704713474,338.250114680653));
#39672=CARTESIAN_POINT('Ctrl Pts',(128.814920453873,3.78140754589906,338.144859302786));
#39673=CARTESIAN_POINT('Ctrl Pts',(128.807146783468,3.86908465124167,338.039435550616));
#39674=CARTESIAN_POINT('Ctrl Pts',(128.799373113063,3.952256811642,337.930454150252));
#39675=CARTESIAN_POINT('Ctrl Pts',(128.791599442659,4.03064460755032,337.81834829468));
#39676=CARTESIAN_POINT('Ctrl Pts',(128.784187638482,4.10538343270009,337.711460993656));
#39677=CARTESIAN_POINT('Ctrl Pts',(128.776775834304,4.17577313830021,337.601733820215));
#39678=CARTESIAN_POINT('Ctrl Pts',(128.769364030127,4.24161096229037,337.489562111512));
#39679=CARTESIAN_POINT('Ctrl Pts',(128.761588951349,4.31067569415507,337.371892533224));
#39680=CARTESIAN_POINT('Ctrl Pts',(128.75381387257,4.3749493169291,337.25116087516));
#39681=CARTESIAN_POINT('Ctrl Pts',(128.746038793792,4.4341484752029,337.127794718096));
#39682=CARTESIAN_POINT('Ctrl Pts',(128.738273282743,4.49327478514374,337.004580370941));
#39683=CARTESIAN_POINT('Ctrl Pts',(128.730507771694,4.54733888776425,336.878738324307));
#39684=CARTESIAN_POINT('Ctrl Pts',(128.722742260645,4.59610162431328,336.750723542278));
#39685=CARTESIAN_POINT('Ctrl Pts',(128.714984449123,4.644816012467,336.622835687277));
#39686=CARTESIAN_POINT('Ctrl Pts',(128.707226637601,4.68823935668187,336.492779746926));
#39687=CARTESIAN_POINT('Ctrl Pts',(128.699468826078,4.7261793732111,336.361033282008));
#39688=CARTESIAN_POINT('Ctrl Pts',(128.691716852555,4.76409083867489,336.229385960483));
#39689=CARTESIAN_POINT('Ctrl Pts',(128.683964879032,4.79652708207503,336.096051020687));
#39690=CARTESIAN_POINT('Ctrl Pts',(128.676212905509,4.82334484368842,335.961523572963));
#39691=CARTESIAN_POINT('Ctrl Pts',(128.668464214952,4.85015124796372,335.827053097694));
#39692=CARTESIAN_POINT('Ctrl Pts',(128.660715524394,4.87134382671436,335.691391501495));
#39693=CARTESIAN_POINT('Ctrl Pts',(128.652966833837,4.88682991627327,335.555046333126));
#39694=CARTESIAN_POINT('Ctrl Pts',(128.645219755459,4.90231278382191,335.418729532508));
#39695=CARTESIAN_POINT('Ctrl Pts',(128.637472677081,4.91209147968396,335.281729830745));
#39696=CARTESIAN_POINT('Ctrl Pts',(128.629725598703,4.91612499337729,335.144561792985));
#39697=CARTESIAN_POINT('Ctrl Pts',(128.621978455397,4.92015854087534,335.007392605625));
#39698=CARTESIAN_POINT('Ctrl Pts',(128.614231312092,4.91844679867661,334.870055470159));
#39699=CARTESIAN_POINT('Ctrl Pts',(128.606484168786,4.91100087046202,334.733066463663));
#39700=CARTESIAN_POINT('Ctrl Pts',(128.598735283758,4.90355326824466,334.59604665913));
#39701=CARTESIAN_POINT('Ctrl Pts',(128.59098639873,4.89036893592378,334.45937552953));
#39702=CARTESIAN_POINT('Ctrl Pts',(128.583237513701,4.87151095093534,334.323565141779));
#39703=CARTESIAN_POINT('Ctrl Pts',(128.575480403927,4.85263294988685,334.187610603479));
#39704=CARTESIAN_POINT('Ctrl Pts',(128.567723294152,4.82806932035802,334.0525190198));
#39705=CARTESIAN_POINT('Ctrl Pts',(128.559966184377,4.79793460180347,333.918793905253));
#39706=CARTESIAN_POINT('Ctrl Pts',(128.552204929451,4.76778378021887,333.784997332281));
#39707=CARTESIAN_POINT('Ctrl Pts',(128.544443674525,4.73205603940615,333.652569060615));
#39708=CARTESIAN_POINT('Ctrl Pts',(128.536682419599,4.69091588054836,333.521997542587));
#39709=CARTESIAN_POINT('Ctrl Pts',(128.528908749194,4.64970991084394,333.391217152683));
#39710=CARTESIAN_POINT('Ctrl Pts',(128.52113507879,4.60307435467188,333.262299819513));
#39711=CARTESIAN_POINT('Ctrl Pts',(128.513361408385,4.5512222833044,333.135714938521));
#39712=CARTESIAN_POINT('Ctrl Pts',(128.505949604208,4.50178393833409,333.015022614194));
#39713=CARTESIAN_POINT('Ctrl Pts',(128.498537800031,4.44760392592213,332.896450739364));
#39714=CARTESIAN_POINT('Ctrl Pts',(128.491125995854,4.38890496733028,332.780383760592));
#39715=CARTESIAN_POINT('Ctrl Pts',(128.483350917075,4.32732899792243,332.658627993444));
#39716=CARTESIAN_POINT('Ctrl Pts',(128.475575838297,4.26058531626217,332.539244105077));
#39717=CARTESIAN_POINT('Ctrl Pts',(128.467800759519,4.18888014427416,332.422701763589));
#39718=CARTESIAN_POINT('Ctrl Pts',(128.46003524847,4.11726321006525,332.306302834873));
#39719=CARTESIAN_POINT('Ctrl Pts',(128.452269737421,4.04069713645387,332.192738825323));
#39720=CARTESIAN_POINT('Ctrl Pts',(128.444504226372,3.95943508992144,332.082457055809));
#39721=CARTESIAN_POINT('Ctrl Pts',(128.436746414849,3.87825361494438,331.97228463099));
#39722=CARTESIAN_POINT('Ctrl Pts',(128.428988603327,3.79238566326635,331.86538828251));
#39723=CARTESIAN_POINT('Ctrl Pts',(128.421230791805,3.70212877017079,331.762188141418));
#39724=CARTESIAN_POINT('Ctrl Pts',(128.413478818282,3.61193979825039,331.659065661706));
#39725=CARTESIAN_POINT('Ctrl Pts',(128.405726844759,3.51736871529613,331.559634145954));
#39726=CARTESIAN_POINT('Ctrl Pts',(128.397974871236,3.41875434410055,331.464281996936));
#39727=CARTESIAN_POINT('Ctrl Pts',(128.390226180678,3.32018173614913,331.368970229608));
#39728=CARTESIAN_POINT('Ctrl Pts',(128.382477490121,3.21756952608372,331.277734664049));
#39729=CARTESIAN_POINT('Ctrl Pts',(128.374728799563,3.11129437685753,331.190927886869));
#39730=CARTESIAN_POINT('Ctrl Pts',(128.366981721185,3.00504133906383,331.104139170564));
#39731=CARTESIAN_POINT('Ctrl Pts',(128.359234642807,2.89512718052339,331.021777656929));
#39732=CARTESIAN_POINT('Ctrl Pts',(128.35148756443,2.78196241692162,330.944156293281));
#39733=CARTESIAN_POINT('Ctrl Pts',(128.343740421124,2.66879670489037,330.866534279091));
#39734=CARTESIAN_POINT('Ctrl Pts',(128.335993277818,2.55238065579436,330.79365271522));
#39735=CARTESIAN_POINT('Ctrl Pts',(128.328246134512,2.43315425869544,330.725781543265));
#39736=CARTESIAN_POINT('Ctrl Pts',(128.320497249484,2.31390105697087,330.65789511243));
#39737=CARTESIAN_POINT('Ctrl Pts',(128.312748364456,2.19183658960441,330.59502150834));
#39738=CARTESIAN_POINT('Ctrl Pts',(128.304999479428,2.06742559940844,330.537384796623));
#39739=CARTESIAN_POINT('Ctrl Pts',(128.297242369653,1.94288255810227,330.479686908705));
#39740=CARTESIAN_POINT('Ctrl Pts',(128.289485259878,1.81598837393559,330.427237181336));
#39741=CARTESIAN_POINT('Ctrl Pts',(128.281728150104,1.68722844687343,330.380211776438));
#39742=CARTESIAN_POINT('Ctrl Pts',(128.273966895177,1.55839971462311,330.333161242667));
#39743=CARTESIAN_POINT('Ctrl Pts',(128.266205640251,1.42770362513454,330.291540925603));
#39744=CARTESIAN_POINT('Ctrl Pts',(128.258444385325,1.29563994942319,330.255476822276));
#39745=CARTESIAN_POINT('Ctrl Pts',(128.25067071492,1.16336501487029,330.219355028137));
#39746=CARTESIAN_POINT('Ctrl Pts',(128.242897044516,1.02971850368519,330.188807295995));
#39747=CARTESIAN_POINT('Ctrl Pts',(128.235123374111,0.895210445600456,330.16390846648));
#39748=CARTESIAN_POINT('Ctrl Pts',(128.227711569934,0.766963769981202,330.140168683468));
#39749=CARTESIAN_POINT('Ctrl Pts',(128.220299765757,0.637934237252592,330.121563766662));
#39750=CARTESIAN_POINT('Ctrl Pts',(128.21288796158,0.508565663983887,330.108114471094));
#39751=CARTESIAN_POINT('Ctrl Pts',(128.205112882802,0.372856351569223,330.094005985487));
#39752=CARTESIAN_POINT('Ctrl Pts',(128.197337804023,0.236345056999165,330.085526699067));
#39753=CARTESIAN_POINT('Ctrl Pts',(128.189562725245,0.0995383327161246,
330.082757359778));
#39754=CARTESIAN_POINT('Ctrl Pts',(128.181797214196,-0.0371000421829576,
330.079991428337));
#39755=CARTESIAN_POINT('Ctrl Pts',(128.174031703147,-0.174032736386184,
330.082921471233));
#39756=CARTESIAN_POINT('Ctrl Pts',(128.166266192098,-0.310746585322844,
330.091576666361));
#39757=CARTESIAN_POINT('Ctrl Pts',(128.158508380576,-0.447324882079973,
330.100223279838));
#39758=CARTESIAN_POINT('Ctrl Pts',(128.150750569053,-0.583684377803953,
330.114583724443));
#39759=CARTESIAN_POINT('Ctrl Pts',(128.142992757531,-0.719310761919096,
330.134635153425));
#39760=CARTESIAN_POINT('Ctrl Pts',(128.135240784008,-0.854835082879417,
330.154671493071));
#39761=CARTESIAN_POINT('Ctrl Pts',(128.127488810485,-0.989627005227994,
330.180390235761));
#39762=CARTESIAN_POINT('Ctrl Pts',(128.119736836962,-1.12317655633233,330.211716645205));
#39763=CARTESIAN_POINT('Ctrl Pts',(128.111988146404,-1.25666954912299,330.243029787897));
#39764=CARTESIAN_POINT('Ctrl Pts',(128.104239455847,-1.38892083738134,330.279945784856));
#39765=CARTESIAN_POINT('Ctrl Pts',(128.096490765289,-1.51943008956658,330.322338697018));
#39766=CARTESIAN_POINT('Ctrl Pts',(128.088743686911,-1.64991218821143,330.364722788979));
#39767=CARTESIAN_POINT('Ctrl Pts',(128.080996608534,-1.77865260019195,330.412581408881));
#39768=CARTESIAN_POINT('Ctrl Pts',(128.073249530156,-1.90516600784046,330.465738699075));
#39769=CARTESIAN_POINT('Ctrl Pts',(128.06550238685,-2.03168047579345,330.518896434778));
#39770=CARTESIAN_POINT('Ctrl Pts',(128.057755243544,-2.15596754182973,330.577352777937));
#39771=CARTESIAN_POINT('Ctrl Pts',(128.050008100238,-2.27756210297438,330.640883813249));
#39772=CARTESIAN_POINT('Ctrl Pts',(128.04225921521,-2.39918400115769,330.704429131687));
#39773=CARTESIAN_POINT('Ctrl Pts',(128.034510330182,-2.51811184353597,330.773051231566));
#39774=CARTESIAN_POINT('Ctrl Pts',(128.026761445154,-2.6339057095397,330.84648055551));
#39775=CARTESIAN_POINT('Ctrl Pts',(128.019004335379,-2.74982248034938,330.919987818097));
#39776=CARTESIAN_POINT('Ctrl Pts',(128.011247225604,-2.86259829929943,330.998312287688));
#39777=CARTESIAN_POINT('Ctrl Pts',(128.00349011583,-2.97182235029787,331.081141112419));
#39778=CARTESIAN_POINT('Ctrl Pts',(127.995728860904,-3.0811047671369,331.164014198227));
#39779=CARTESIAN_POINT('Ctrl Pts',(127.987967605977,-3.18683133304892,331.25139618642));
#39780=CARTESIAN_POINT('Ctrl Pts',(127.980206351051,-3.28862563967027,331.342934993112));
#39781=CARTESIAN_POINT('Ctrl Pts',(127.972432680646,-3.39058278400735,331.434620232063));
#39782=CARTESIAN_POINT('Ctrl Pts',(127.964659010242,-3.48859481951027,331.530475303851));
#39783=CARTESIAN_POINT('Ctrl Pts',(127.956885339837,-3.58232280474365,331.630111814153));
#39784=CARTESIAN_POINT('Ctrl Pts',(127.94947353566,-3.67168772971594,331.72511022093));
#39785=CARTESIAN_POINT('Ctrl Pts',(127.942061731483,-3.75715828505088,331.823545719694));
#39786=CARTESIAN_POINT('Ctrl Pts',(127.934649927306,-3.83847684278656,331.925056327363));
#39787=CARTESIAN_POINT('Ctrl Pts',(127.926811857355,-3.92447217247712,332.032404986963));
#39788=CARTESIAN_POINT('Ctrl Pts',(127.918973787404,-4.00610492627406,332.14354388457));
#39789=CARTESIAN_POINT('Ctrl Pts',(127.911135717454,-4.08302188865518,332.258081817548));
#39790=CARTESIAN_POINT('Ctrl Pts',(127.903388132755,-4.1590508963803,332.371297487038));
#39791=CARTESIAN_POINT('Ctrl Pts',(127.895640548056,-4.23047215722734,332.487833817112));
#39792=CARTESIAN_POINT('Ctrl Pts',(127.887892963357,-4.29698302741908,332.607277716789));
#39793=CARTESIAN_POINT('Ctrl Pts',(127.880152880545,-4.36342949598585,332.726605960467));
#39794=CARTESIAN_POINT('Ctrl Pts',(127.872412797734,-4.42497484252336,332.848835833053));
#39795=CARTESIAN_POINT('Ctrl Pts',(127.864672714922,-4.48135934721705,332.973524867261));
#39796=CARTESIAN_POINT('Ctrl Pts',(127.85693843481,-4.53770158073825,333.098120422742));
#39797=CARTESIAN_POINT('Ctrl Pts',(127.849204154699,-4.58889050980646,333.225171115613));
#39798=CARTESIAN_POINT('Ctrl Pts',(127.841469874587,-4.63471225796807,333.354209810352));
#39799=CARTESIAN_POINT('Ctrl Pts',(127.833558739079,-4.6815817860558,333.486199159736));
#39800=CARTESIAN_POINT('Ctrl Pts',(127.825647603571,-4.7228355025048,333.620268161879));
#39801=CARTESIAN_POINT('Ctrl Pts',(127.817736468063,-4.75829647276027,333.755894803557));
#39802=CARTESIAN_POINT('Ctrl Pts',(127.810007972526,-4.79293877538075,333.88839030863));
#39803=CARTESIAN_POINT('Ctrl Pts',(127.80227947699,-4.82205279167517,334.022371915563));
#39804=CARTESIAN_POINT('Ctrl Pts',(127.794550981453,-4.84552409401785,334.157337958139));
#39805=CARTESIAN_POINT('Ctrl Pts',(127.786548525959,-4.86982740783749,334.297088281315));
#39806=CARTESIAN_POINT('Ctrl Pts',(127.778546070465,-4.88808046340052,334.43789369095));
#39807=CARTESIAN_POINT('Ctrl Pts',(127.770543614972,-4.90021423700222,334.579187103357));
#39808=CARTESIAN_POINT('Ctrl Pts',(127.762541159478,-4.91234801060392,334.720480515765));
#39809=CARTESIAN_POINT('Ctrl Pts',(127.754538703984,-4.91836247964961,334.862261464752));
#39810=CARTESIAN_POINT('Ctrl Pts',(127.74653624849,-4.91824840624315,335.00395941747));
#39811=CARTESIAN_POINT('',(131.246536248453,-4.91824924060785,334.99726691378));
#39812=CARTESIAN_POINT('Ctrl Pts',(131.246536248453,-4.91824924060785,334.99726691378));
#39813=CARTESIAN_POINT('Ctrl Pts',(131.238860999982,-4.91832419279384,335.132145034037));
#39814=CARTESIAN_POINT('Ctrl Pts',(131.231185751512,-4.91284661490259,335.267247101451));
#39815=CARTESIAN_POINT('Ctrl Pts',(131.223510503042,-4.90178762207131,335.402071101434));
#39816=CARTESIAN_POINT('Ctrl Pts',(131.215843894781,-4.8907410786093,335.536743326858));
#39817=CARTESIAN_POINT('Ctrl Pts',(131.208177286519,-4.87412564910301,335.671137710913));
#39818=CARTESIAN_POINT('Ctrl Pts',(131.200510678257,-4.85196444990179,335.804750917607));
#39819=CARTESIAN_POINT('Ctrl Pts',(131.192850758201,-4.82982258371629,335.938247562638));
#39820=CARTESIAN_POINT('Ctrl Pts',(131.185190838145,-4.80214463739249,336.070963992175));
#39821=CARTESIAN_POINT('Ctrl Pts',(131.177530918089,-4.76900560663304,336.202401175317));
#39822=CARTESIAN_POINT('Ctrl Pts',(131.169875333428,-4.73588533204745,336.333763967066));
#39823=CARTESIAN_POINT('Ctrl Pts',(131.162219748767,-4.69731021811577,336.463848564326));
#39824=CARTESIAN_POINT('Ctrl Pts',(131.154564164106,-4.65340641976804,336.592165743559));
#39825=CARTESIAN_POINT('Ctrl Pts',(131.146910803518,-4.60951537619533,336.720445644541));
#39826=CARTESIAN_POINT('Ctrl Pts',(131.139257442931,-4.56029885568008,336.846958768903));
#39827=CARTESIAN_POINT('Ctrl Pts',(131.131604082343,-4.50593285082086,336.971231139769));
#39828=CARTESIAN_POINT('Ctrl Pts',(131.123951191523,-4.45157018297827,337.095495882725));
#39829=CARTESIAN_POINT('Ctrl Pts',(131.116298300703,-4.39205882023487,337.217519777963));
#39830=CARTESIAN_POINT('Ctrl Pts',(131.108645409882,-4.32762265436903,337.336849422597));
#39831=CARTESIAN_POINT('Ctrl Pts',(131.100991235131,-4.26317567800085,337.456199087252));
#39832=CARTESIAN_POINT('Ctrl Pts',(131.09333706038,-4.19380244644444,337.572853249405));
#39833=CARTESIAN_POINT('Ctrl Pts',(131.085682885629,-4.11977222899054,337.686384157886));
#39834=CARTESIAN_POINT('Ctrl Pts',(131.078021004012,-4.04566747169431,337.800029378823));
#39835=CARTESIAN_POINT('Ctrl Pts',(131.070359122394,-3.96689658280152,337.910544728399));
#39836=CARTESIAN_POINT('Ctrl Pts',(131.062697240777,-3.88377171888825,338.017532153609));
#39837=CARTESIAN_POINT('Ctrl Pts',(131.055031479518,-3.80060476418162,338.124573752569));
#39838=CARTESIAN_POINT('Ctrl Pts',(131.047365718259,-3.71307970316364,338.228083563571));
#39839=CARTESIAN_POINT('Ctrl Pts',(131.039699957,-3.62154737670412,338.327698553173));
#39840=CARTESIAN_POINT('Ctrl Pts',(131.032022091977,-3.52987052633862,338.427470828708));
#39841=CARTESIAN_POINT('Ctrl Pts',(131.024344226953,-3.43417405392277,338.52333571341));
#39842=CARTESIAN_POINT('Ctrl Pts',(131.016666361929,-3.33484438255584,338.614968327197));
#39843=CARTESIAN_POINT('Ctrl Pts',(131.009533676059,-3.24256777425054,338.700094419875));
#39844=CARTESIAN_POINT('Ctrl Pts',(131.002400990189,-3.14715616375519,338.781568205919));
#39845=CARTESIAN_POINT('Ctrl Pts',(130.995268304319,-3.04894185816097,338.859162682248));
#39846=CARTESIAN_POINT('Ctrl Pts',(130.987493225541,-2.94188205248691,338.943745569709));
#39847=CARTESIAN_POINT('Ctrl Pts',(130.979718146762,-2.83113069276856,339.024003704274));
#39848=CARTESIAN_POINT('Ctrl Pts',(130.971943067984,-2.71707235433044,339.099597649018));
#39849=CARTESIAN_POINT('Ctrl Pts',(130.964177556935,-2.60315437193928,339.1750985706));
#39850=CARTESIAN_POINT('Ctrl Pts',(130.956412045886,-2.4859378305606,339.24594650861));
#39851=CARTESIAN_POINT('Ctrl Pts',(130.948646534837,-2.36584050375049,339.311842039467));
#39852=CARTESIAN_POINT('Ctrl Pts',(130.940888723315,-2.24586225378951,339.377672234713));
#39853=CARTESIAN_POINT('Ctrl Pts',(130.933130911793,-2.12300924308282,339.438559607818));
#39854=CARTESIAN_POINT('Ctrl Pts',(130.92537310027,-1.99772807037857,339.494248059389));
#39855=CARTESIAN_POINT('Ctrl Pts',(130.917621126747,-1.87254117572994,339.549894603634));
#39856=CARTESIAN_POINT('Ctrl Pts',(130.909869153224,-1.74493011191208,339.600349855562));
#39857=CARTESIAN_POINT('Ctrl Pts',(130.902117179701,-1.61536559900807,339.645403862318));
#39858=CARTESIAN_POINT('Ctrl Pts',(130.894368489144,-1.4858559567518,339.690438788676));
#39859=CARTESIAN_POINT('Ctrl Pts',(130.886619798586,-1.35439487924633,339.730076891286));
#39860=CARTESIAN_POINT('Ctrl Pts',(130.878871108028,-1.221472361358,339.764156623468));
#39861=CARTESIAN_POINT('Ctrl Pts',(130.871124029651,-1.08857749910972,339.798229265078));
#39862=CARTESIAN_POINT('Ctrl Pts',(130.863376951273,-0.954222179675249,
339.826745739536));
#39863=CARTESIAN_POINT('Ctrl Pts',(130.855629872895,-0.818910447437517,
339.849594698692));
#39864=CARTESIAN_POINT('Ctrl Pts',(130.847882729589,-0.683597581157139,
339.872443849343));
#39865=CARTESIAN_POINT('Ctrl Pts',(130.840135586283,-0.547328671503624,
339.889625324869));
#39866=CARTESIAN_POINT('Ctrl Pts',(130.832388442977,-0.410616423522549,
339.901079188835));
#39867=CARTESIAN_POINT('Ctrl Pts',(130.824639557949,-0.273873439725831,
339.912535627873));
#39868=CARTESIAN_POINT('Ctrl Pts',(130.816890672921,-0.136687308699211,
339.918261860369));
#39869=CARTESIAN_POINT('Ctrl Pts',(130.809141787893,0.000426092826129061,
339.918249981543));
#39870=CARTESIAN_POINT('Ctrl Pts',(130.801384678118,0.137685027932541,339.918238090108));
#39871=CARTESIAN_POINT('Ctrl Pts',(130.793627568344,0.274870687840066,339.912475921059));
#39872=CARTESIAN_POINT('Ctrl Pts',(130.785870458569,0.411468593600158,339.901007718723));
#39873=CARTESIAN_POINT('Ctrl Pts',(130.778109203643,0.548139492913627,339.889533388146));
#39874=CARTESIAN_POINT('Ctrl Pts',(130.770347948717,0.684221624655794,339.872346997582));
#39875=CARTESIAN_POINT('Ctrl Pts',(130.76258669379,0.819208561864751,339.84954434918));
#39876=CARTESIAN_POINT('Ctrl Pts',(130.754813023386,0.954411434181009,339.826705223973));
#39877=CARTESIAN_POINT('Ctrl Pts',(130.747039352981,1.08851522848843,339.798231969095));
#39878=CARTESIAN_POINT('Ctrl Pts',(130.739265682576,1.22102571788834,339.764271115161));
#39879=CARTESIAN_POINT('Ctrl Pts',(130.731853878399,1.34736781212674,339.731891147147));
#39880=CARTESIAN_POINT('Ctrl Pts',(130.724442074222,1.47226132420035,339.69452306066));
#39881=CARTESIAN_POINT('Ctrl Pts',(130.717030270045,1.5952948434285,339.652334620922));
#39882=CARTESIAN_POINT('Ctrl Pts',(130.709255191267,1.7243586019316,339.60807840008));
#39883=CARTESIAN_POINT('Ctrl Pts',(130.701480112488,1.85178329517504,339.558377500741));
#39884=CARTESIAN_POINT('Ctrl Pts',(130.69370503371,1.97707536763083,339.503371631701));
#39885=CARTESIAN_POINT('Ctrl Pts',(130.685939522661,2.10221326021498,339.448433450885));
#39886=CARTESIAN_POINT('Ctrl Pts',(130.678174011612,2.22522339918631,339.388203445045));
#39887=CARTESIAN_POINT('Ctrl Pts',(130.670408500563,2.3456279116231,339.322870893598));
#39888=CARTESIAN_POINT('Ctrl Pts',(130.662650689041,2.46591304263514,339.257603119565));
#39889=CARTESIAN_POINT('Ctrl Pts',(130.654892877518,2.58359734705257,339.187243053212));
#39890=CARTESIAN_POINT('Ctrl Pts',(130.647135065996,2.69822378522158,339.112027658876));
#39891=CARTESIAN_POINT('Ctrl Pts',(130.639383092473,2.81276396336065,339.03686886651));
#39892=CARTESIAN_POINT('Ctrl Pts',(130.63163111895,2.92425053007613,338.956862232423));
#39893=CARTESIAN_POINT('Ctrl Pts',(130.623879145427,3.03225219788486,338.872289977639));
#39894=CARTESIAN_POINT('Ctrl Pts',(130.61613045487,3.14020812692348,338.787753539254));
#39895=CARTESIAN_POINT('Ctrl Pts',(130.608381764312,3.24468178532352,338.698655566337));
#39896=CARTESIAN_POINT('Ctrl Pts',(130.600633073754,3.3452721606967,338.605320683846));
#39897=CARTESIAN_POINT('Ctrl Pts',(130.592885995377,3.44584160740214,338.512005220457));
#39898=CARTESIAN_POINT('Ctrl Pts',(130.585138916999,3.54252909179903,338.414454866604));
#39899=CARTESIAN_POINT('Ctrl Pts',(130.577391838621,3.63496821151331,338.313033227088));
#39900=CARTESIAN_POINT('Ctrl Pts',(130.569644695315,3.72740810595632,338.211610737561));
#39901=CARTESIAN_POINT('Ctrl Pts',(130.561897552009,3.81559930139824,338.106317186544));
#39902=CARTESIAN_POINT('Ctrl Pts',(130.554150408703,3.8992139418947,337.997551283604));
#39903=CARTESIAN_POINT('Ctrl Pts',(130.546401523675,3.98284738073777,337.888760927779));
#39904=CARTESIAN_POINT('Ctrl Pts',(130.538652638647,4.06190197904431,337.776496976435));
#39905=CARTESIAN_POINT('Ctrl Pts',(130.530903753619,4.13609191901683,337.661188963592));
#39906=CARTESIAN_POINT('Ctrl Pts',(130.523146643844,4.21036060495799,337.545758561633));
#39907=CARTESIAN_POINT('Ctrl Pts',(130.51538953407,4.27975410636193,337.427277973183));
#39908=CARTESIAN_POINT('Ctrl Pts',(130.507632424295,4.34403121514666,337.306203777712));
#39909=CARTESIAN_POINT('Ctrl Pts',(130.499871169369,4.40834267156309,337.185064884061));
#39910=CARTESIAN_POINT('Ctrl Pts',(130.492109914443,4.46753211895922,337.061329974206));
#39911=CARTESIAN_POINT('Ctrl Pts',(130.484348659517,4.52140606271786,336.935476757421));
#39912=CARTESIAN_POINT('Ctrl Pts',(130.476574989112,4.57536618722908,336.809422216505));
#39913=CARTESIAN_POINT('Ctrl Pts',(130.468801318707,4.62399367772629,336.681242962884));
#39914=CARTESIAN_POINT('Ctrl Pts',(130.461027648303,4.66714430039421,336.551433898623));
#39915=CARTESIAN_POINT('Ctrl Pts',(130.453615844125,4.70828625119613,336.427667477532));
#39916=CARTESIAN_POINT('Ctrl Pts',(130.446204039948,4.74444967582734,336.302419842963));
#39917=CARTESIAN_POINT('Ctrl Pts',(130.438792235771,4.77555301371775,336.176127746323));
#39918=CARTESIAN_POINT('Ctrl Pts',(130.431017156993,4.80818081884981,336.043645697824));
#39919=CARTESIAN_POINT('Ctrl Pts',(130.423242078214,4.83534308541445,335.909595546319));
#39920=CARTESIAN_POINT('Ctrl Pts',(130.415466999436,4.85689020630341,335.774467937628));
#39921=CARTESIAN_POINT('Ctrl Pts',(130.407701488387,4.87841081208837,335.639506612062));
#39922=CARTESIAN_POINT('Ctrl Pts',(130.399935977338,4.89432995974505,335.503470849738));
#39923=CARTESIAN_POINT('Ctrl Pts',(130.392170466289,4.90454821391293,335.366864934143));
#39924=CARTESIAN_POINT('Ctrl Pts',(130.384412654766,4.91475633665202,335.230394463711));
#39925=CARTESIAN_POINT('Ctrl Pts',(130.376654843244,4.9192747856339,335.093355352278));
#39926=CARTESIAN_POINT('Ctrl Pts',(130.368897031722,4.91805549884353,334.956260169241));
#39927=CARTESIAN_POINT('Ctrl Pts',(130.361145058199,4.91683712960514,334.819268154675));
#39928=CARTESIAN_POINT('Ctrl Pts',(130.353393084676,4.90988962248244,334.682220541777));
#39929=CARTESIAN_POINT('Ctrl Pts',(130.345641111153,4.89721690874973,334.545632735383));
#39930=CARTESIAN_POINT('Ctrl Pts',(130.337892420595,4.88454956191884,334.409102774006));
#39931=CARTESIAN_POINT('Ctrl Pts',(130.330143730038,4.86616186692838,334.273032620223));
#39932=CARTESIAN_POINT('Ctrl Pts',(130.32239503948,4.84210979701792,334.1379351671));
#39933=CARTESIAN_POINT('Ctrl Pts',(130.314647961102,4.81806273134149,334.00286582213));
#39934=CARTESIAN_POINT('Ctrl Pts',(130.306900882724,4.78835370337467,333.868769159856));
#39935=CARTESIAN_POINT('Ctrl Pts',(130.299153804347,4.75309019480281,333.736150063271));
#39936=CARTESIAN_POINT('Ctrl Pts',(130.291406661041,4.71782639068884,333.603529855211));
#39937=CARTESIAN_POINT('Ctrl Pts',(130.283659517735,4.67700811356214,333.472387615289));
#39938=CARTESIAN_POINT('Ctrl Pts',(130.275912374429,4.63079322514058,333.343214809189));
#39939=CARTESIAN_POINT('Ctrl Pts',(130.268163489401,4.58456794663097,333.214012962299));
#39940=CARTESIAN_POINT('Ctrl Pts',(130.260414604373,4.53294377419524,333.086781798251));
#39941=CARTESIAN_POINT('Ctrl Pts',(130.252665719345,4.47612723974367,332.961994112834));
#39942=CARTESIAN_POINT('Ctrl Pts',(130.24490860957,4.41925039963531,332.837073976477));
#39943=CARTESIAN_POINT('Ctrl Pts',(130.237151499795,4.3571703505436,332.714602855877));
#39944=CARTESIAN_POINT('Ctrl Pts',(130.229394390021,4.2901405083497,332.595030669402));
#39945=CARTESIAN_POINT('Ctrl Pts',(130.221633135095,4.2230748475513,332.475394587374));
#39946=CARTESIAN_POINT('Ctrl Pts',(130.213871880168,4.15105432836077,332.358660858676));
#39947=CARTESIAN_POINT('Ctrl Pts',(130.206110625242,4.07437595565987,332.245250712961));
#39948=CARTESIAN_POINT('Ctrl Pts',(130.198336954837,3.99757492255209,332.131659147973));
#39949=CARTESIAN_POINT('Ctrl Pts',(130.190563284433,3.91610137895022,332.021402104734));
#39950=CARTESIAN_POINT('Ctrl Pts',(130.182789614028,3.83029344536577,331.91486869244));
#39951=CARTESIAN_POINT('Ctrl Pts',(130.175377809851,3.74847989173427,331.813294436119));
#39952=CARTESIAN_POINT('Ctrl Pts',(130.167966005674,3.66272658791024,331.715105159063));
#39953=CARTESIAN_POINT('Ctrl Pts',(130.160554201497,3.57335667036554,331.620605798541));
#39954=CARTESIAN_POINT('Ctrl Pts',(130.152779122719,3.47960646694233,331.521474742861));
#39955=CARTESIAN_POINT('Ctrl Pts',(130.14500404394,3.38157989571606,331.42609118465));
#39956=CARTESIAN_POINT('Ctrl Pts',(130.137228965162,3.27960859023327,331.334846448323));
#39957=CARTESIAN_POINT('Ctrl Pts',(130.129463454113,3.17776276693348,331.243713994454));
#39958=CARTESIAN_POINT('Ctrl Pts',(130.121697943064,3.07198215643688,331.156710486845));
#39959=CARTESIAN_POINT('Ctrl Pts',(130.113932432015,2.96263701130687,331.074192439544));
#39960=CARTESIAN_POINT('Ctrl Pts',(130.106174620492,2.8534002822066,330.991756209127));
#39961=CARTESIAN_POINT('Ctrl Pts',(130.09841680897,2.74060636181404,330.913796822482));
#39962=CARTESIAN_POINT('Ctrl Pts',(130.090658997448,2.62466027155475,330.840632076695));
#39963=CARTESIAN_POINT('Ctrl Pts',(130.082907023925,2.50880143440497,330.767522389698));
#39964=CARTESIAN_POINT('Ctrl Pts',(130.075155050402,2.3897954781847,330.699200369527));
#39965=CARTESIAN_POINT('Ctrl Pts',(130.067403076879,2.2680779452533,330.635941625418));
#39966=CARTESIAN_POINT('Ctrl Pts',(130.059654386321,2.14641195976986,330.572709671426));
#39967=CARTESIAN_POINT('Ctrl Pts',(130.051905695764,2.0220370276797,330.514536908512));
#39968=CARTESIAN_POINT('Ctrl Pts',(130.044157005206,1.89541474203446,330.461653823453));
#39969=CARTESIAN_POINT('Ctrl Pts',(130.036409926828,1.76881880121349,330.408781741162));
#39970=CARTESIAN_POINT('Ctrl Pts',(130.02866284845,1.63997679734376,330.361197298172));
#39971=CARTESIAN_POINT('Ctrl Pts',(130.020915770073,1.50937146181384,330.319083332));
#39972=CARTESIAN_POINT('Ctrl Pts',(130.013168626767,1.37876503168533,330.276969012872));
#39973=CARTESIAN_POINT('Ctrl Pts',(130.005421483461,1.24639561243237,330.240325381966));
#39974=CARTESIAN_POINT('Ctrl Pts',(129.997674340155,1.11276191606658,330.209285650276));
#39975=CARTESIAN_POINT('Ctrl Pts',(129.989925455127,0.979098176008767,330.178238940195));
#39976=CARTESIAN_POINT('Ctrl Pts',(129.982176570099,0.844169973903678,330.152798724761));
#39977=CARTESIAN_POINT('Ctrl Pts',(129.974427685071,0.708486660083692,330.133047183814));
#39978=CARTESIAN_POINT('Ctrl Pts',(129.966670575296,0.572659330592638,330.113274678377));
#39979=CARTESIAN_POINT('Ctrl Pts',(129.958913465521,0.436075675756878,330.099202965329));
#39980=CARTESIAN_POINT('Ctrl Pts',(129.951156355747,0.299251179407041,330.090862418497));
#39981=CARTESIAN_POINT('Ctrl Pts',(129.943395100821,0.162353568421154,330.082517414743));
#39982=CARTESIAN_POINT('Ctrl Pts',(129.935633845894,0.0252152500842124,
330.079909687043));
#39983=CARTESIAN_POINT('Ctrl Pts',(129.927872590968,-0.111648828219296,
330.083017429189));
#39984=CARTESIAN_POINT('Ctrl Pts',(129.920098920564,-0.248731844444331,
330.08613014271));
#39985=CARTESIAN_POINT('Ctrl Pts',(129.912325250159,-0.385539353729229,
330.094976571042));
#39986=CARTESIAN_POINT('Ctrl Pts',(129.904551579754,-0.521561169438464,
330.109482950747));
#39987=CARTESIAN_POINT('Ctrl Pts',(129.897139775577,-0.651251136900461,
330.123314054987));
#39988=CARTESIAN_POINT('Ctrl Pts',(129.8897279714,-0.780226627975906,330.142289985724));
#39989=CARTESIAN_POINT('Ctrl Pts',(129.882316167223,-0.908056346721781,
330.16630402966));
#39990=CARTESIAN_POINT('Ctrl Pts',(129.874541088445,-1.04215138076962,330.191495073424));
#39991=CARTESIAN_POINT('Ctrl Pts',(129.866766009666,-1.17540925224237,330.222310192018));
#39992=CARTESIAN_POINT('Ctrl Pts',(129.858990930888,-1.30732142214948,330.258682275813));
#39993=CARTESIAN_POINT('Ctrl Pts',(129.851225419839,-1.43907126573354,330.295009601443));
#39994=CARTESIAN_POINT('Ctrl Pts',(129.84345990879,-1.56947832944978,330.336880183313));
#39995=CARTESIAN_POINT('Ctrl Pts',(129.835694397741,-1.69804244812341,330.38417559835));
#39996=CARTESIAN_POINT('Ctrl Pts',(129.827936586219,-1.82647909509925,330.431424119845));
#39997=CARTESIAN_POINT('Ctrl Pts',(129.820178774696,-1.95307606895754,330.484086636434));
#39998=CARTESIAN_POINT('Ctrl Pts',(129.812420963174,-2.07734694701626,330.541994535196));
#39999=CARTESIAN_POINT('Ctrl Pts',(129.804668989651,-2.20152430729843,330.599858856428));
#40000=CARTESIAN_POINT('Ctrl Pts',(129.796917016128,-2.32337870311768,330.662960538463));
#40001=CARTESIAN_POINT('Ctrl Pts',(129.789165042605,-2.44244267182418,330.731082472412));
#40002=CARTESIAN_POINT('Ctrl Pts',(129.781416352048,-2.5614562168692,330.79917555668));
#40003=CARTESIAN_POINT('Ctrl Pts',(129.77366766149,-2.67768134665106,330.872284470533));
#40004=CARTESIAN_POINT('Ctrl Pts',(129.765918970932,-2.79067444543647,330.950145780144));
#40005=CARTESIAN_POINT('Ctrl Pts',(129.758171892554,-2.90364403506375,331.027990890059));
#40006=CARTESIAN_POINT('Ctrl Pts',(129.750424814177,-3.01338260959016,331.11058620734));
#40007=CARTESIAN_POINT('Ctrl Pts',(129.742677735799,-3.1194751833941,331.197624736735));
#40008=CARTESIAN_POINT('Ctrl Pts',(129.734930592493,-3.22556864635589,331.284663995597));
#40009=CARTESIAN_POINT('Ctrl Pts',(129.727183449187,-3.32801574545603,331.37614629293));
#40010=CARTESIAN_POINT('Ctrl Pts',(129.719436305881,-3.4264345790412,331.471724339277));
#40011=CARTESIAN_POINT('Ctrl Pts',(129.711687420853,-3.52487553926979,331.567323873598));
#40012=CARTESIAN_POINT('Ctrl Pts',(129.703938535825,-3.61928615150944,331.667020716984));
#40013=CARTESIAN_POINT('Ctrl Pts',(129.696189650797,-3.70932167028769,331.770431018103));
#40014=CARTESIAN_POINT('Ctrl Pts',(129.688432541022,-3.79945275369569,331.873951079983));
#40015=CARTESIAN_POINT('Ctrl Pts',(129.680675431248,-3.88519921020425,331.981192177854));
#40016=CARTESIAN_POINT('Ctrl Pts',(129.672918321473,-3.96625653993615,332.091737267386));
#40017=CARTESIAN_POINT('Ctrl Pts',(129.665157066547,-4.0473571841136,332.202341428679));
#40018=CARTESIAN_POINT('Ctrl Pts',(129.657395811621,-4.12376349101779,332.316252775197));
#40019=CARTESIAN_POINT('Ctrl Pts',(129.649634556695,-4.19521513037563,332.433026476107));
#40020=CARTESIAN_POINT('Ctrl Pts',(129.64186088629,-4.26678106907022,332.549986976882));
#40021=CARTESIAN_POINT('Ctrl Pts',(129.634087215885,-4.33337631204293,332.669818640078));
#40022=CARTESIAN_POINT('Ctrl Pts',(129.626313545481,-4.39478679727931,332.792052521241));
#40023=CARTESIAN_POINT('Ctrl Pts',(129.618901741304,-4.45333860965332,332.908596385827));
#40024=CARTESIAN_POINT('Ctrl Pts',(129.611489937126,-4.50717738349597,333.027323592805));
#40025=CARTESIAN_POINT('Ctrl Pts',(129.604078132949,-4.55615945731404,333.147813707526));
#40026=CARTESIAN_POINT('Ctrl Pts',(129.595116309249,-4.61538507897874,333.29350173975));
#40027=CARTESIAN_POINT('Ctrl Pts',(129.586154485548,-4.66767254577,333.442165238511));
#40028=CARTESIAN_POINT('Ctrl Pts',(129.577192661848,-4.71274877049981,333.593165934215));
#40029=CARTESIAN_POINT('Ctrl Pts',(129.568494161544,-4.75650052992046,333.739729807974));
#40030=CARTESIAN_POINT('Ctrl Pts',(129.55979566124,-4.79345868248545,333.888495249248));
#40031=CARTESIAN_POINT('Ctrl Pts',(129.551097160936,-4.82342038277065,334.038855435654));
#40032=CARTESIAN_POINT('Ctrl Pts',(129.542003675537,-4.85474259631828,334.196043239511));
#40033=CARTESIAN_POINT('Ctrl Pts',(129.532910190138,-4.87841796184014,334.354973856826));
#40034=CARTESIAN_POINT('Ctrl Pts',(129.52381670474,-4.8942712126928,334.514930562593));
#40035=CARTESIAN_POINT('Ctrl Pts',(129.515189481392,-4.90931159928784,334.666685601074));
#40036=CARTESIAN_POINT('Ctrl Pts',(129.506562258044,-4.91731175971941,334.819363839407));
#40037=CARTESIAN_POINT('Ctrl Pts',(129.497935034696,-4.91817219910754,334.972336261538));
#40038=CARTESIAN_POINT('Ctrl Pts',(129.497468772645,-4.91821870192979,334.980603722854));
#40039=CARTESIAN_POINT('Ctrl Pts',(129.497002510594,-4.91824436243081,334.988872039881));
#40040=CARTESIAN_POINT('Ctrl Pts',(129.496536248543,-4.91824916909057,334.997141112125));
#40041=CARTESIAN_POINT('',(132.996536248523,-4.91824810241123,335.004320373636));
#40042=CARTESIAN_POINT('Ctrl Pts',(132.99653624849,-4.91824810241071,335.004320374226));
#40043=CARTESIAN_POINT('Ctrl Pts',(132.985166312015,-4.91807204458086,335.204741921598));
#40044=CARTESIAN_POINT('Ctrl Pts',(132.973796375539,-4.90564181988563,335.404646016326));
#40045=CARTESIAN_POINT('Ctrl Pts',(132.962426439064,-4.88116543082435,335.602832563342));
#40046=CARTESIAN_POINT('Ctrl Pts',(132.955929140788,-4.86717851007207,335.716085360572));
#40047=CARTESIAN_POINT('Ctrl Pts',(132.949431842512,-4.84925871495562,335.828778013465));
#40048=CARTESIAN_POINT('Ctrl Pts',(132.942934544237,-4.82745109785408,335.940690682598));
#40049=CARTESIAN_POINT('Ctrl Pts',(132.935159465458,-4.80135472152312,336.07461247315));
#40050=CARTESIAN_POINT('Ctrl Pts',(132.92738438668,-4.76964005433339,336.207659125601));
#40051=CARTESIAN_POINT('Ctrl Pts',(132.919609307901,-4.73237763992542,336.339322565939));
#40052=CARTESIAN_POINT('Ctrl Pts',(132.911843796852,-4.69516107929066,336.470823986032));
#40053=CARTESIAN_POINT('Ctrl Pts',(132.904078285803,-4.65241046034805,336.600945208256));
#40054=CARTESIAN_POINT('Ctrl Pts',(132.896312774754,-4.6042475824392,336.729186878883));
#40055=CARTESIAN_POINT('Ctrl Pts',(132.888554963232,-4.55613245816402,336.857301397521));
#40056=CARTESIAN_POINT('Ctrl Pts',(132.88079715171,-4.50261589064495,336.983539709631));
#40057=CARTESIAN_POINT('Ctrl Pts',(132.873039340188,-4.44386977508548,337.107416542732));
#40058=CARTESIAN_POINT('Ctrl Pts',(132.865287366665,-4.38516786784091,337.231200154588));
#40059=CARTESIAN_POINT('Ctrl Pts',(132.857535393142,-4.32124441258973,337.35262547289));
#40060=CARTESIAN_POINT('Ctrl Pts',(132.849783419619,-4.25231967130944,337.471226512381));
#40061=CARTESIAN_POINT('Ctrl Pts',(132.842034729061,-4.18342411969796,337.589777324261));
#40062=CARTESIAN_POINT('Ctrl Pts',(132.834286038504,-4.10953169069499,337.705505899011));
#40063=CARTESIAN_POINT('Ctrl Pts',(132.826537347946,-4.03090880905422,337.817970410701));
#40064=CARTESIAN_POINT('Ctrl Pts',(132.818790269568,-3.95230228556062,337.930411523211));
#40065=CARTESIAN_POINT('Ctrl Pts',(132.81104319119,-3.86896749090839,338.03958960332));
#40066=CARTESIAN_POINT('Ctrl Pts',(132.803296112813,-3.78121421686721,338.145091748846));
#40067=CARTESIAN_POINT('Ctrl Pts',(132.795548969507,-3.69346020736914,338.250594778582));
#40068=CARTESIAN_POINT('Ctrl Pts',(132.787801826201,-3.60128789457463,338.352421511779));
#40069=CARTESIAN_POINT('Ctrl Pts',(132.780054682895,-3.50504714003312,338.450192401685));
#40070=CARTESIAN_POINT('Ctrl Pts',(132.772305797867,-3.4087847485269,338.547985272563));
#40071=CARTESIAN_POINT('Ctrl Pts',(132.764556912839,-3.30845236932635,338.641720207185));
#40072=CARTESIAN_POINT('Ctrl Pts',(132.756808027811,-3.20443617400694,338.731055061134));
#40073=CARTESIAN_POINT('Ctrl Pts',(132.749050918036,-3.10030957482292,338.820484736021));
#40074=CARTESIAN_POINT('Ctrl Pts',(132.741293808261,-2.99249164583852,338.905504745818));
#40075=CARTESIAN_POINT('Ctrl Pts',(132.733536698487,-2.88140147898083,338.985813415029));
#40076=CARTESIAN_POINT('Ctrl Pts',(132.725775443561,-2.77025194908991,339.066164998625));
#40077=CARTESIAN_POINT('Ctrl Pts',(132.718014188634,-2.65582702303574,339.141800009682));
#40078=CARTESIAN_POINT('Ctrl Pts',(132.710252933708,-2.53857328021474,339.212461129017));
#40079=CARTESIAN_POINT('Ctrl Pts',(132.702479263304,-2.4211319696182,339.283235283114));
#40080=CARTESIAN_POINT('Ctrl Pts',(132.694705592899,-2.30085314270943,339.349019458175));
#40081=CARTESIAN_POINT('Ctrl Pts',(132.686931922494,-2.1782071793833,339.409602765123));
#40082=CARTESIAN_POINT('Ctrl Pts',(132.679520118317,-2.06127041515641,339.467365904558));
#40083=CARTESIAN_POINT('Ctrl Pts',(132.67210831414,-1.9421821982926,339.520401362981));
#40084=CARTESIAN_POINT('Ctrl Pts',(132.664696509963,-1.821363924382,339.568568322512));
#40085=CARTESIAN_POINT('Ctrl Pts',(132.656921431184,-1.69462398696847,339.619096088212));
#40086=CARTESIAN_POINT('Ctrl Pts',(132.649146352406,-1.56557959229293,339.664425725826));
#40087=CARTESIAN_POINT('Ctrl Pts',(132.641371273628,-1.4346961658433,339.704341609005));
#40088=CARTESIAN_POINT('Ctrl Pts',(132.633605762579,-1.30397379978233,339.744208373149));
#40089=CARTESIAN_POINT('Ctrl Pts',(132.62584025153,-1.17141727505926,339.778674525335));
#40090=CARTESIAN_POINT('Ctrl Pts',(132.618074740481,-1.0375124214905,339.807572260274));
#40091=CARTESIAN_POINT('Ctrl Pts',(132.610316928958,-0.903740334973862,
339.836441343024));
#40092=CARTESIAN_POINT('Ctrl Pts',(132.602559117436,-0.768622959679355,
339.859752913907));
#40093=CARTESIAN_POINT('Ctrl Pts',(132.594801305914,-0.632661393947455,
339.877388914482));
#40094=CARTESIAN_POINT('Ctrl Pts',(132.587049332391,-0.496802143605495,
339.895011643407));
#40095=CARTESIAN_POINT('Ctrl Pts',(132.579297358868,-0.360100353386185,
339.906967253255));
#40096=CARTESIAN_POINT('Ctrl Pts',(132.571545385345,-0.223067076628279,
339.913188795663));
#40097=CARTESIAN_POINT('Ctrl Pts',(132.563796694787,-0.0860918335444363,
339.919407703243));
#40098=CARTESIAN_POINT('Ctrl Pts',(132.55604800423,0.0512142272032169,339.919897355569));
#40099=CARTESIAN_POINT('Ctrl Pts',(132.548299313672,0.188335387045108,339.91464269754));
#40100=CARTESIAN_POINT('Ctrl Pts',(132.540552235294,0.325428017684436,339.909389132787));
#40101=CARTESIAN_POINT('Ctrl Pts',(132.532805156916,0.462335433595527,339.898393649877));
#40102=CARTESIAN_POINT('Ctrl Pts',(132.525058078539,0.598542770423849,339.881693314258));
#40103=CARTESIAN_POINT('Ctrl Pts',(132.517310935233,0.734751248800706,339.864992838674));
#40104=CARTESIAN_POINT('Ctrl Pts',(132.509563791927,0.870259248422978,339.842587462585));
#40105=CARTESIAN_POINT('Ctrl Pts',(132.501816648621,1.00455827017125,339.814565997505));
#40106=CARTESIAN_POINT('Ctrl Pts',(132.494067763593,1.13888748519099,339.786538232605));
#40107=CARTESIAN_POINT('Ctrl Pts',(132.486318878565,1.27200679891804,339.752891946071));
#40108=CARTESIAN_POINT('Ctrl Pts',(132.478569993537,1.40341951521538,339.713766723843));
#40109=CARTESIAN_POINT('Ctrl Pts',(132.470812883762,1.53497171432755,339.674599973701));
#40110=CARTESIAN_POINT('Ctrl Pts',(132.463055773987,1.66481332235345,339.629942782771));
#40111=CARTESIAN_POINT('Ctrl Pts',(132.455298664213,1.79246385924236,339.579984320476));
#40112=CARTESIAN_POINT('Ctrl Pts',(132.447537409287,1.92018260849663,339.529999161977));
#40113=CARTESIAN_POINT('Ctrl Pts',(132.43977615436,2.04570759608539,339.474707244928));
#40114=CARTESIAN_POINT('Ctrl Pts',(132.432014899434,2.16858076708155,339.414344857297));
#40115=CARTESIAN_POINT('Ctrl Pts',(132.42424122903,2.29165049510703,339.353885909518));
#40116=CARTESIAN_POINT('Ctrl Pts',(132.416467558625,2.41205958619735,339.288340469755));
#40117=CARTESIAN_POINT('Ctrl Pts',(132.40869388822,2.52937614967794,339.217989966316));
#40118=CARTESIAN_POINT('Ctrl Pts',(132.401282084043,2.64123159890342,339.150914295738));
#40119=CARTESIAN_POINT('Ctrl Pts',(132.393870279866,2.75027571477758,339.079471003268));
#40120=CARTESIAN_POINT('Ctrl Pts',(132.386458475689,2.85616203920789,339.003938244814));
#40121=CARTESIAN_POINT('Ctrl Pts',(132.378683396911,2.96723816781801,338.924703400868));
#40122=CARTESIAN_POINT('Ctrl Pts',(132.370908318132,3.07519015367777,338.840717684271));
#40123=CARTESIAN_POINT('Ctrl Pts',(132.363133239354,3.17958480355244,338.752255793455));
#40124=CARTESIAN_POINT('Ctrl Pts',(132.355367728305,3.28385098916439,338.663902760628));
#40125=CARTESIAN_POINT('Ctrl Pts',(132.347602217256,3.38456825346058,338.571084763634));
#40126=CARTESIAN_POINT('Ctrl Pts',(132.339836706207,3.48133257500152,338.47411953806));
#40127=CARTESIAN_POINT('Ctrl Pts',(132.332078894684,3.57800095443589,338.37725045379));
#40128=CARTESIAN_POINT('Ctrl Pts',(132.324321083162,3.67072391652706,338.276242598925));
#40129=CARTESIAN_POINT('Ctrl Pts',(132.31656327164,3.75913101034844,338.171453469552));
#40130=CARTESIAN_POINT('Ctrl Pts',(132.308811298117,3.84747157502812,338.066743197323));
#40131=CARTESIAN_POINT('Ctrl Pts',(132.301059324594,3.93150248504629,337.958257612025));
#40132=CARTESIAN_POINT('Ctrl Pts',(132.293307351071,4.01089088180881,337.846390239711));
#40133=CARTESIAN_POINT('Ctrl Pts',(132.285558660513,4.09024565753819,337.734570243296));
#40134=CARTESIAN_POINT('Ctrl Pts',(132.277809969956,4.16496160471648,337.619371626487));
#40135=CARTESIAN_POINT('Ctrl Pts',(132.270061279398,4.23474697827753,337.501219920852));
#40136=CARTESIAN_POINT('Ctrl Pts',(132.26231420102,4.30451783240876,337.383092797667));
#40137=CARTESIAN_POINT('Ctrl Pts',(132.254567122642,4.36935995474722,337.262014144113));
#40138=CARTESIAN_POINT('Ctrl Pts',(132.246820044265,4.4290258917723,337.138436978849));
#40139=CARTESIAN_POINT('Ctrl Pts',(132.239072900959,4.48869232885536,337.01485877789));
#40140=CARTESIAN_POINT('Ctrl Pts',(132.231325757653,4.54318232414685,336.888782375449));
#40141=CARTESIAN_POINT('Ctrl Pts',(132.223578614347,4.59229538309382,336.760683440291));
#40142=CARTESIAN_POINT('Ctrl Pts',(132.215829729319,4.64141948369911,336.632555705773));
#40143=CARTESIAN_POINT('Ctrl Pts',(132.208080844291,4.68516410258287,336.502404898617));
#40144=CARTESIAN_POINT('Ctrl Pts',(132.200331959263,4.72337782976025,336.370724239163));
#40145=CARTESIAN_POINT('Ctrl Pts',(132.192574849488,4.76163211738251,336.238903812497));
#40146=CARTESIAN_POINT('Ctrl Pts',(132.184817739713,4.79434367722345,336.105550665818));
#40147=CARTESIAN_POINT('Ctrl Pts',(132.177060629939,4.82141157055939,335.97117121548));
#40148=CARTESIAN_POINT('Ctrl Pts',(132.169299375013,4.84849392811207,335.83671995706));
#40149=CARTESIAN_POINT('Ctrl Pts',(132.161538120086,4.86992654887105,335.701241688073));
#40150=CARTESIAN_POINT('Ctrl Pts',(132.15377686516,4.88566025262429,335.565249465658));
#40151=CARTESIAN_POINT('Ctrl Pts',(132.146003194756,4.90141912517593,335.429039700007));
#40152=CARTESIAN_POINT('Ctrl Pts',(132.138229524351,4.91146083478947,335.292314728042));
#40153=CARTESIAN_POINT('Ctrl Pts',(132.130455853946,4.91578831970801,335.15559003285));
#40154=CARTESIAN_POINT('Ctrl Pts',(132.123044049769,4.91991435916246,335.025229905114));
#40155=CARTESIAN_POINT('Ctrl Pts',(132.115632245592,4.91884619839865,334.89487031675));
#40156=CARTESIAN_POINT('Ctrl Pts',(132.108220441415,4.91263025629944,334.764953137883));
#40157=CARTESIAN_POINT('Ctrl Pts',(132.100445362637,4.90610965236161,334.628668331075));
#40158=CARTESIAN_POINT('Ctrl Pts',(132.092670283858,4.89390328535079,334.492439712761));
#40159=CARTESIAN_POINT('Ctrl Pts',(132.08489520508,4.87600772932303,334.356780219457));
#40160=CARTESIAN_POINT('Ctrl Pts',(132.077129694031,4.85813419491626,334.221287663795));
#40161=CARTESIAN_POINT('Ctrl Pts',(132.069364182982,4.83458545192537,334.086363223471));
#40162=CARTESIAN_POINT('Ctrl Pts',(132.061598671933,4.80541005179943,333.95251859369));
#40163=CARTESIAN_POINT('Ctrl Pts',(132.05384086041,4.77626357916766,333.818806671249));
#40164=CARTESIAN_POINT('Ctrl Pts',(132.046083048888,4.74150163433323,333.686172808172));
#40165=CARTESIAN_POINT('Ctrl Pts',(132.038325237366,4.7012243711309,333.555121986192));
#40166=CARTESIAN_POINT('Ctrl Pts',(132.030573263843,4.66097741784642,333.424169784113));
#40167=CARTESIAN_POINT('Ctrl Pts',(132.02282129032,4.61522352183404,333.294798624051));
#40168=CARTESIAN_POINT('Ctrl Pts',(132.015069316797,4.56411347866309,333.167501373429));
#40169=CARTESIAN_POINT('Ctrl Pts',(132.007320626239,4.51302508062575,333.040258033268));
#40170=CARTESIAN_POINT('Ctrl Pts',(131.999571935682,4.45658519231475,332.91508721764));
#40171=CARTESIAN_POINT('Ctrl Pts',(131.991823245124,4.39499377230843,332.792464540745));
#40172=CARTESIAN_POINT('Ctrl Pts',(131.984076166746,4.33341516691146,332.669867376521));
#40173=CARTESIAN_POINT('Ctrl Pts',(131.976329088368,4.26668733707546,332.549817645571));
#40174=CARTESIAN_POINT('Ctrl Pts',(131.968582009991,4.19505732455719,332.432768591229));
#40175=CARTESIAN_POINT('Ctrl Pts',(131.960834866685,4.12342671171045,332.315718555904));
#40176=CARTESIAN_POINT('Ctrl Pts',(131.953087723379,4.04689403826312,332.201669580747));
#40177=CARTESIAN_POINT('Ctrl Pts',(131.945340580073,3.96575080512067,332.091047677568));
#40178=CARTESIAN_POINT('Ctrl Pts',(131.937591695045,3.88458932925674,331.980400904236));
#40179=CARTESIAN_POINT('Ctrl Pts',(131.929842810017,3.79881546221727,331.873183051162));
#40180=CARTESIAN_POINT('Ctrl Pts',(131.922093924989,3.70876202687786,331.76978835206));
#40181=CARTESIAN_POINT('Ctrl Pts',(131.914336815214,3.61861300789172,331.666283908755));
#40182=CARTESIAN_POINT('Ctrl Pts',(131.90657970544,3.5241756039036,331.566611020744));
#40183=CARTESIAN_POINT('Ctrl Pts',(131.898822595665,3.42582104749373,331.471128620501));
#40184=CARTESIAN_POINT('Ctrl Pts',(131.891061340739,3.32741393355371,331.375595197515));
#40185=CARTESIAN_POINT('Ctrl Pts',(131.883300085812,3.2250857877574,331.284256984384));
#40186=CARTESIAN_POINT('Ctrl Pts',(131.875538830886,3.1192414365625,331.197432982454));
#40187=CARTESIAN_POINT('Ctrl Pts',(131.867765160482,3.01322776890029,331.110470090416));
#40188=CARTESIAN_POINT('Ctrl Pts',(131.859991490077,2.90368696834014,331.028036074963));
#40189=CARTESIAN_POINT('Ctrl Pts',(131.852217819672,2.79105410566051,330.950407422743));
#40190=CARTESIAN_POINT('Ctrl Pts',(131.844806015495,2.68366432983633,330.87639240296));
#40191=CARTESIAN_POINT('Ctrl Pts',(131.837394211318,2.57346412780097,330.806745588839));
#40192=CARTESIAN_POINT('Ctrl Pts',(131.829982407141,2.46085019748905,330.74166706703));
#40193=CARTESIAN_POINT('Ctrl Pts',(131.822207328363,2.342716722993,330.673398853008));
#40194=CARTESIAN_POINT('Ctrl Pts',(131.814432249584,2.22155360595167,330.609942325273));
#40195=CARTESIAN_POINT('Ctrl Pts',(131.806657170806,2.0977903316501,330.551577944154));
#40196=CARTESIAN_POINT('Ctrl Pts',(131.798891659757,1.97417935593668,330.493285384122));
#40197=CARTESIAN_POINT('Ctrl Pts',(131.791126148708,1.84797493952248,330.440072667872));
#40198=CARTESIAN_POINT('Ctrl Pts',(131.783360637659,1.71963365179694,330.392175875089));
#40199=CARTESIAN_POINT('Ctrl Pts',(131.775602826136,1.59141961483201,330.344326572117));
#40200=CARTESIAN_POINT('Ctrl Pts',(131.767845014614,1.4610732867611,330.301782839301));
#40201=CARTESIAN_POINT('Ctrl Pts',(131.760087203092,1.32907351648444,330.264733729738));
#40202=CARTESIAN_POINT('Ctrl Pts',(131.752335229569,1.19717308022083,330.227712500805));
#40203=CARTESIAN_POINT('Ctrl Pts',(131.744583256046,1.06362205322197,330.196177770053));
#40204=CARTESIAN_POINT('Ctrl Pts',(131.736831282523,0.928916502352443,330.170269449114));
#40205=CARTESIAN_POINT('Ctrl Pts',(131.729082591965,0.794267999363639,330.144372100365));
#40206=CARTESIAN_POINT('Ctrl Pts',(131.721333901408,0.658466328014882,330.124096495902));
#40207=CARTESIAN_POINT('Ctrl Pts',(131.71358521085,0.522019651493034,330.109531868425));
#40208=CARTESIAN_POINT('Ctrl Pts',(131.705838132472,0.385601363841908,330.09497027124));
#40209=CARTESIAN_POINT('Ctrl Pts',(131.698091054094,0.248538726370752,330.086117329055));
#40210=CARTESIAN_POINT('Ctrl Pts',(131.690343975717,0.111346569539857,330.083010575164));
#40211=CARTESIAN_POINT('Ctrl Pts',(131.682596832411,-0.0258467370934059,
330.079903795234));
#40212=CARTESIAN_POINT('Ctrl Pts',(131.674849689105,-0.163169174477405,
330.082543308503));
#40213=CARTESIAN_POINT('Ctrl Pts',(131.667102545799,-0.300104752326663,
330.090914525074));
#40214=CARTESIAN_POINT('Ctrl Pts',(131.659353660771,-0.437071116201,330.099287623672));
#40215=CARTESIAN_POINT('Ctrl Pts',(131.651604775743,-0.573650057401876,
330.113394965913));
#40216=CARTESIAN_POINT('Ctrl Pts',(131.643855890715,-0.70932994683372,330.133170016425));
#40217=CARTESIAN_POINT('Ctrl Pts',(131.63609878094,-0.845153848302135,330.15296605638));
#40218=CARTESIAN_POINT('Ctrl Pts',(131.628341671165,-0.980076404373335,
330.178441765195));
#40219=CARTESIAN_POINT('Ctrl Pts',(131.620584561391,-1.11359488582268,330.209479204432));
#40220=CARTESIAN_POINT('Ctrl Pts',(131.612823306464,-1.24718471527936,330.240533229084));
#40221=CARTESIAN_POINT('Ctrl Pts',(131.605062051538,-1.37936859859475,330.277154801849));
#40222=CARTESIAN_POINT('Ctrl Pts',(131.597300796612,-1.5096592059064,330.319176125454));
#40223=CARTESIAN_POINT('Ctrl Pts',(131.589527126207,-1.64015823572809,330.361264669482));
#40224=CARTESIAN_POINT('Ctrl Pts',(131.581753455803,-1.7687575706075,330.4087700898));
#40225=CARTESIAN_POINT('Ctrl Pts',(131.573979785398,-1.89498926526261,330.461476148896));
#40226=CARTESIAN_POINT('Ctrl Pts',(131.566567981221,-2.01534484416103,330.511728728261));
#40227=CARTESIAN_POINT('Ctrl Pts',(131.559156177044,-2.13354798861138,330.566708541716));
#40228=CARTESIAN_POINT('Ctrl Pts',(131.551744372867,-2.24921576546666,330.626190275872));
#40229=CARTESIAN_POINT('Ctrl Pts',(131.543969294089,-2.37055276462297,330.688587387006));
#40230=CARTESIAN_POINT('Ctrl Pts',(131.53619421531,-2.48948302755049,330.756136068736));
#40231=CARTESIAN_POINT('Ctrl Pts',(131.528419136532,-2.60553829004209,330.828626930899));
#40232=CARTESIAN_POINT('Ctrl Pts',(131.520653625483,-2.72145073914472,330.901028588441));
#40233=CARTESIAN_POINT('Ctrl Pts',(131.512888114434,-2.83449489881281,330.978360120548));
#40234=CARTESIAN_POINT('Ctrl Pts',(131.505122603385,-2.94422516870629,331.060365344546));
#40235=CARTESIAN_POINT('Ctrl Pts',(131.497364791862,-3.05384664071762,331.142289260125));
#40236=CARTESIAN_POINT('Ctrl Pts',(131.48960698034,-3.16016045066288,331.228877413231));
#40237=CARTESIAN_POINT('Ctrl Pts',(131.481849168818,-3.2627484871443,331.319829437086));
#40238=CARTESIAN_POINT('Ctrl Pts',(131.474097195295,-3.36525932287509,331.410713016659));
#40239=CARTESIAN_POINT('Ctrl Pts',(131.466345221772,-3.46404967459343,331.505953672176));
#40240=CARTESIAN_POINT('Ctrl Pts',(131.458593248249,-3.55873343737917,331.60520996464));
#40241=CARTESIAN_POINT('Ctrl Pts',(131.450844557691,-3.65337710153515,331.704424222005));
#40242=CARTESIAN_POINT('Ctrl Pts',(131.443095867134,-3.7439173665542,331.807650451655));
#40243=CARTESIAN_POINT('Ctrl Pts',(131.435347176576,-3.83000419849704,331.914509617258));
#40244=CARTESIAN_POINT('Ctrl Pts',(131.427600098198,-3.91607311935545,332.021346549919));
#40245=CARTESIAN_POINT('Ctrl Pts',(131.419853019821,-3.99769020509566,332.131814610874));
#40246=CARTESIAN_POINT('Ctrl Pts',(131.412105941443,-4.07454528886835,332.245501179623));
#40247=CARTESIAN_POINT('Ctrl Pts',(131.404358798137,-4.15140101676064,332.359188701174));
#40248=CARTESIAN_POINT('Ctrl Pts',(131.396611654831,-4.22349444416985,332.476094460501));
#40249=CARTESIAN_POINT('Ctrl Pts',(131.388864511525,-4.29055860809946,332.595776654933));
#40250=CARTESIAN_POINT('Ctrl Pts',(131.381115626497,-4.35763784947678,332.715485756464));
#40251=CARTESIAN_POINT('Ctrl Pts',(131.373366741469,-4.41968538640075,332.837972194269));
#40252=CARTESIAN_POINT('Ctrl Pts',(131.365617856441,-4.47648029802522,332.962769722419));
#40253=CARTESIAN_POINT('Ctrl Pts',(131.357860746666,-4.53333549235583,333.087699711956));
#40254=CARTESIAN_POINT('Ctrl Pts',(131.350103636892,-4.58492676225724,333.214945335638));
#40255=CARTESIAN_POINT('Ctrl Pts',(131.342346527117,-4.63108122904954,333.344020014479));
#40256=CARTESIAN_POINT('Ctrl Pts',(131.334585272191,-4.67726035931314,333.473163666702));
#40257=CARTESIAN_POINT('Ctrl Pts',(131.326824017265,-4.71799678146001,333.604137948569));
#40258=CARTESIAN_POINT('Ctrl Pts',(131.319062762338,-4.75316787764475,333.736442249271));
#40259=CARTESIAN_POINT('Ctrl Pts',(131.311289091934,-4.78839523612117,333.868958193737));
#40260=CARTESIAN_POINT('Ctrl Pts',(131.303515421529,-4.81803939382419,334.002808026778));
#40261=CARTESIAN_POINT('Ctrl Pts',(131.295741751124,-4.84202895744665,334.137481224698));
#40262=CARTESIAN_POINT('Ctrl Pts',(131.288329946947,-4.86490180111146,334.265885352858));
#40263=CARTESIAN_POINT('Ctrl Pts',(131.28091814277,-4.88263460699182,334.395037630585));
#40264=CARTESIAN_POINT('Ctrl Pts',(131.273506338593,-4.89520961882523,334.524494111224));
#40265=CARTESIAN_POINT('Ctrl Pts',(131.264516308558,-4.91046227949477,334.681516291147));
#40266=CARTESIAN_POINT('Ctrl Pts',(131.255526278524,-4.91816144897856,334.83928396875));
#40267=CARTESIAN_POINT('Ctrl Pts',(131.24653624849,-4.91824924060749,334.997266913122));
#40268=CARTESIAN_POINT('',(134.746536248449,-4.91824997633412,335.000482482528));
#40269=CARTESIAN_POINT('Ctrl Pts',(134.746536248449,-4.91824997633412,335.000482482528));
#40270=CARTESIAN_POINT('Ctrl Pts',(134.73835890364,-4.91823573273552,335.145676503863));
#40271=CARTESIAN_POINT('Ctrl Pts',(134.730181558832,-4.91178769478722,335.290726823761));
#40272=CARTESIAN_POINT('Ctrl Pts',(134.722004214023,-4.89896956597948,335.435063505832));
#40273=CARTESIAN_POINT('Ctrl Pts',(134.713813828826,-4.88613099613821,335.579630361199));
#40274=CARTESIAN_POINT('Ctrl Pts',(134.705623443629,-4.86690208535552,335.723480987154));
#40275=CARTESIAN_POINT('Ctrl Pts',(134.697433058432,-4.84139785573774,335.866054192853));
#40276=CARTESIAN_POINT('Ctrl Pts',(134.689221195481,-4.81582674604515,336.009001270133));
#40277=CARTESIAN_POINT('Ctrl Pts',(134.68100933253,-4.78394746694061,336.150663910874));
#40278=CARTESIAN_POINT('Ctrl Pts',(134.672797469578,-4.74592579345992,336.290492706478));
#40279=CARTESIAN_POINT('Ctrl Pts',(134.664573976314,-4.70785027056847,336.430519539084));
#40280=CARTESIAN_POINT('Ctrl Pts',(134.656350483049,-4.66361508511763,336.568707036158));
#40281=CARTESIAN_POINT('Ctrl Pts',(134.648126989784,-4.61343476530339,336.704524194252));
#40282=CARTESIAN_POINT('Ctrl Pts',(134.639884397592,-4.5631379025238,336.840656785456));
#40283=CARTESIAN_POINT('Ctrl Pts',(134.6316418054,-4.50686842177647,336.974407733546));
#40284=CARTESIAN_POINT('Ctrl Pts',(134.623399213208,-4.44488829345144,337.105267470237));
#40285=CARTESIAN_POINT('Ctrl Pts',(134.619720392099,-4.41722541760802,337.163672587277));
#40286=CARTESIAN_POINT('Ctrl Pts',(134.616041570989,-4.38842557466354,337.221502133846));
#40287=CARTESIAN_POINT('Ctrl Pts',(134.61236274988,-4.35851485952536,337.27871263695));
#40288=CARTESIAN_POINT('Ctrl Pts',(134.604587671102,-4.29529945447882,337.399625330275));
#40289=CARTESIAN_POINT('Ctrl Pts',(134.596812592323,-4.22694885561345,337.518096539765));
#40290=CARTESIAN_POINT('Ctrl Pts',(134.589037513545,-4.15367561177011,337.63365942648));
#40291=CARTESIAN_POINT('Ctrl Pts',(134.581272002496,-4.08049253531808,337.749080105705));
#40292=CARTESIAN_POINT('Ctrl Pts',(134.573506491447,-4.0023990741382,337.861599256138));
#40293=CARTESIAN_POINT('Ctrl Pts',(134.565740980398,-3.91965441540698,337.970773018304));
#40294=CARTESIAN_POINT('Ctrl Pts',(134.557983168875,-3.83699179824588,338.079838534366));
#40295=CARTESIAN_POINT('Ctrl Pts',(134.550225357353,-3.74968739560838,338.185564953597));
#40296=CARTESIAN_POINT('Ctrl Pts',(134.542467545831,-3.65804439205829,338.287536203334));
#40297=CARTESIAN_POINT('Ctrl Pts',(134.534715572308,-3.56647035277456,338.389430716471));
#40298=CARTESIAN_POINT('Ctrl Pts',(134.526963598785,-3.4705644714938,338.487575395348));
#40299=CARTESIAN_POINT('Ctrl Pts',(134.519211625262,-3.37067078783581,338.581586450517));
#40300=CARTESIAN_POINT('Ctrl Pts',(134.511462934704,-3.27081940921213,338.67555769195));
#40301=CARTESIAN_POINT('Ctrl Pts',(134.503714244147,-3.16698387123994,338.765398524156));
#40302=CARTESIAN_POINT('Ctrl Pts',(134.495965553589,-3.05954556632937,338.850761481844));
#40303=CARTESIAN_POINT('Ctrl Pts',(134.488218475211,-2.95212961485544,338.936106679056));
#40304=CARTESIAN_POINT('Ctrl Pts',(134.480471396834,-2.84111269326651,339.016975611885));
#40305=CARTESIAN_POINT('Ctrl Pts',(134.472724318456,-2.72690950804375,339.093060908103));
#40306=CARTESIAN_POINT('Ctrl Pts',(134.46497717515,-2.61270536568846,339.169146841989));
#40307=CARTESIAN_POINT('Ctrl Pts',(134.457230031844,-2.49531523172932,339.240448842581));
#40308=CARTESIAN_POINT('Ctrl Pts',(134.449482888538,-2.37518270227838,339.306702937666));
#40309=CARTESIAN_POINT('Ctrl Pts',(134.44173400351,-2.25502316448436,339.372971928077));
#40310=CARTESIAN_POINT('Ctrl Pts',(134.433985118482,-2.13212034654061,339.434190565976));
#40311=CARTESIAN_POINT('Ctrl Pts',(134.426236233454,-2.00694197621473,339.490141085379));
#40312=CARTESIAN_POINT('Ctrl Pts',(134.418479123679,-1.88163074027313,339.546150991242));
#40313=CARTESIAN_POINT('Ctrl Pts',(134.410722013905,-1.75403948458573,339.596881449041));
#40314=CARTESIAN_POINT('Ctrl Pts',(134.40296490413,-1.62465594495468,339.64216287123));
#40315=CARTESIAN_POINT('Ctrl Pts',(134.395203649204,-1.49520326689706,339.687468490363));
#40316=CARTESIAN_POINT('Ctrl Pts',(134.387442394278,-1.36395677033809,339.727319158375));
#40317=CARTESIAN_POINT('Ctrl Pts',(134.379681139351,-1.23141788303495,339.761595642203));
#40318=CARTESIAN_POINT('Ctrl Pts',(134.371907468947,-1.09866697670641,339.795926957233));
#40319=CARTESIAN_POINT('Ctrl Pts',(134.364133798542,-0.964619930738429,
339.824666187533));
#40320=CARTESIAN_POINT('Ctrl Pts',(134.356360128137,-0.829787739488795,
339.847745390374));
#40321=CARTESIAN_POINT('Ctrl Pts',(134.34894832396,-0.701232019180494,339.869750250771));
#40322=CARTESIAN_POINT('Ctrl Pts',(134.341536519783,-0.571962890992541,
339.886610136396));
#40323=CARTESIAN_POINT('Ctrl Pts',(134.334124715606,-0.442424411406601,
339.898310290569));
#40324=CARTESIAN_POINT('Ctrl Pts',(134.326349636828,-0.30653686506098,339.91058390415));
#40325=CARTESIAN_POINT('Ctrl Pts',(134.318574558049,-0.169923466525491,
339.9172179967));
#40326=CARTESIAN_POINT('Ctrl Pts',(134.310799479271,-0.0330918129995932,
339.918138671735));
#40327=CARTESIAN_POINT('Ctrl Pts',(134.303033968222,0.103571460465418,339.91905821382));
#40328=CARTESIAN_POINT('Ctrl Pts',(134.295268457173,0.240452067401368,339.91427832491));
#40329=CARTESIAN_POINT('Ctrl Pts',(134.287502946124,0.37703649585296,339.903776763199));
#40330=CARTESIAN_POINT('Ctrl Pts',(134.279745134602,0.513485500446227,339.893285613818));
#40331=CARTESIAN_POINT('Ctrl Pts',(134.27198732308,0.64963852374524,339.87708411111));
#40332=CARTESIAN_POINT('Ctrl Pts',(134.264229511557,0.784981610805304,339.855202048648));
#40333=CARTESIAN_POINT('Ctrl Pts',(134.256477538034,0.920222847900195,339.833336453133));
#40334=CARTESIAN_POINT('Ctrl Pts',(134.248725564511,1.05465497763155,339.805798868782));
#40335=CARTESIAN_POINT('Ctrl Pts',(134.240973590988,1.18776908368744,339.772670915361));
#40336=CARTESIAN_POINT('Ctrl Pts',(134.233224900431,1.32082681584048,339.739556991649));
#40337=CARTESIAN_POINT('Ctrl Pts',(134.225476209873,1.45256725599122,339.700857501906));
#40338=CARTESIAN_POINT('Ctrl Pts',(134.217727519316,1.58249181984603,339.656705133742));
#40339=CARTESIAN_POINT('Ctrl Pts',(134.209980440938,1.71238935181019,339.612561951847));
#40340=CARTESIAN_POINT('Ctrl Pts',(134.20223336256,1.84047138910986,339.562968273852));
#40341=CARTESIAN_POINT('Ctrl Pts',(134.194486284182,1.96625503440986,339.508106498538));
#40342=CARTESIAN_POINT('Ctrl Pts',(134.186739140876,2.09203973389788,339.453244263429));
#40343=CARTESIAN_POINT('Ctrl Pts',(134.178991997571,2.21552564468682,339.393113999202));
#40344=CARTESIAN_POINT('Ctrl Pts',(134.171244854265,2.33625073160155,339.327945884781));
#40345=CARTESIAN_POINT('Ctrl Pts',(134.163495969237,2.45700296007889,339.262763119184));
#40346=CARTESIAN_POINT('Ctrl Pts',(134.155747084209,2.57499278568155,339.19254043525));
#40347=CARTESIAN_POINT('Ctrl Pts',(134.147998199181,2.68978397001657,339.117553309569));
#40348=CARTESIAN_POINT('Ctrl Pts',(134.140241089406,2.8046969949007,339.042486591778));
#40349=CARTESIAN_POINT('Ctrl Pts',(134.132483979631,2.91640426878821,338.962645544458));
#40350=CARTESIAN_POINT('Ctrl Pts',(134.124726869856,3.02449924006377,338.8783485415));
#40351=CARTESIAN_POINT('Ctrl Pts',(134.11696561493,3.13265197383574,338.794006492918));
#40352=CARTESIAN_POINT('Ctrl Pts',(134.109204360004,3.23718826095472,338.705203997033));
#40353=CARTESIAN_POINT('Ctrl Pts',(134.101443105078,3.33773648446146,338.61229819129));
#40354=CARTESIAN_POINT('Ctrl Pts',(134.093669434673,3.43844555235721,338.519243766535));
#40355=CARTESIAN_POINT('Ctrl Pts',(134.085895764269,3.53515353243187,338.422073192384));
#40356=CARTESIAN_POINT('Ctrl Pts',(134.078122093864,3.62752676182902,338.321179407186));
#40357=CARTESIAN_POINT('Ctrl Pts',(134.070710289687,3.71559999517437,338.224982251961));
#40358=CARTESIAN_POINT('Ctrl Pts',(134.06329848551,3.79973277541043,338.125400935764));
#40359=CARTESIAN_POINT('Ctrl Pts',(134.055886681333,3.87967238888669,338.022800889475));
#40360=CARTESIAN_POINT('Ctrl Pts',(134.048111602554,3.96353008094701,337.915172109288));
#40361=CARTESIAN_POINT('Ctrl Pts',(134.040336523776,4.04303817972715,337.803881076083));
#40362=CARTESIAN_POINT('Ctrl Pts',(134.032561444997,4.11785985412688,337.689314649547));
#40363=CARTESIAN_POINT('Ctrl Pts',(134.024795933948,4.19258945569285,337.574889204293));
#40364=CARTESIAN_POINT('Ctrl Pts',(134.017030422899,4.2626438957544,337.457196709542));
#40365=CARTESIAN_POINT('Ctrl Pts',(134.00926491185,4.32772657991942,337.336656952135));
#40366=CARTESIAN_POINT('Ctrl Pts',(134.001507100328,4.39274473441363,337.216236710248));
#40367=CARTESIAN_POINT('Ctrl Pts',(133.993749288806,4.45280075850798,337.092975165501));
#40368=CARTESIAN_POINT('Ctrl Pts',(133.985991477284,4.50764157574367,336.967320636583));
#40369=CARTESIAN_POINT('Ctrl Pts',(133.978239503761,4.56244112352525,336.841760666684));
#40370=CARTESIAN_POINT('Ctrl Pts',(133.970487530238,4.61203312046782,336.713811653811));
#40371=CARTESIAN_POINT('Ctrl Pts',(133.962735556715,4.65621079855521,336.583945725686));
#40372=CARTESIAN_POINT('Ctrl Pts',(133.954986866157,4.70036976736972,336.454134795858));
#40373=CARTESIAN_POINT('Ctrl Pts',(133.947238175599,4.73911885225843,336.322408934701));
#40374=CARTESIAN_POINT('Ctrl Pts',(133.939489485042,4.77229982049138,336.18925921726));
#40375=CARTESIAN_POINT('Ctrl Pts',(133.931742406664,4.80547388514676,336.05613720273));
#40376=CARTESIAN_POINT('Ctrl Pts',(133.923995328286,4.8330820430151,335.921592300207));
#40377=CARTESIAN_POINT('Ctrl Pts',(133.916248249908,4.85501635366416,335.786129294807));
#40378=CARTESIAN_POINT('Ctrl Pts',(133.908501106602,4.87695084814386,335.650665154096));
#40379=CARTESIAN_POINT('Ctrl Pts',(133.900753963296,4.89321133808062,335.514283281011));
#40380=CARTESIAN_POINT('Ctrl Pts',(133.893006819991,4.90374135209681,335.377496773808));
#40381=CARTESIAN_POINT('Ctrl Pts',(133.885257934962,4.91427373348371,335.240679514095));
#40382=CARTESIAN_POINT('Ctrl Pts',(133.877509049934,4.9190730453166,335.10345782889));
#40383=CARTESIAN_POINT('Ctrl Pts',(133.869760164906,4.91813486811154,334.966347636554));
#40384=CARTESIAN_POINT('Ctrl Pts',(133.862003055132,4.91719569511549,334.829091914042));
#40385=CARTESIAN_POINT('Ctrl Pts',(133.854245945357,4.91050687075318,334.691948312277));
#40386=CARTESIAN_POINT('Ctrl Pts',(133.846488835582,4.89811611401281,334.555430999565));
#40387=CARTESIAN_POINT('Ctrl Pts',(133.838727580656,4.88571873604822,334.418840736365));
#40388=CARTESIAN_POINT('Ctrl Pts',(133.83096632573,4.86761340599107,334.282877816333));
#40389=CARTESIAN_POINT('Ctrl Pts',(133.823205070804,4.84389934507849,334.148048007662));
#40390=CARTESIAN_POINT('Ctrl Pts',(133.815431400399,4.82014734939685,334.013002515239));
#40391=CARTESIAN_POINT('Ctrl Pts',(133.807657729994,4.79076877767103,333.8790941383));
#40392=CARTESIAN_POINT('Ctrl Pts',(133.799884059589,4.75591349602446,333.746816102548));
#40393=CARTESIAN_POINT('Ctrl Pts',(133.792472255412,4.72268073612439,333.620695641186));
#40394=CARTESIAN_POINT('Ctrl Pts',(133.785060451235,4.68446975778355,333.496057427223));
#40395=CARTESIAN_POINT('Ctrl Pts',(133.777648647058,4.64145110176964,333.373311728578));
#40396=CARTESIAN_POINT('Ctrl Pts',(133.76987356828,4.59632397327837,333.244549897602));
#40397=CARTESIAN_POINT('Ctrl Pts',(133.762098489501,4.54576336359021,333.117463877162));
#40398=CARTESIAN_POINT('Ctrl Pts',(133.754323410723,4.48991231263323,332.99254626769));
#40399=CARTESIAN_POINT('Ctrl Pts',(133.746557899674,4.43412998995011,332.86778237729));
#40400=CARTESIAN_POINT('Ctrl Pts',(133.738792388625,4.37307033749456,332.745181941992));
#40401=CARTESIAN_POINT('Ctrl Pts',(133.731026877576,4.30692585873355,332.625221545097));
#40402=CARTESIAN_POINT('Ctrl Pts',(133.723269066054,4.24084696241581,332.505380089284));
#40403=CARTESIAN_POINT('Ctrl Pts',(133.715511254532,4.16969346041965,332.388173802776));
#40404=CARTESIAN_POINT('Ctrl Pts',(133.70775344301,4.09370539930299,332.274058113932));
#40405=CARTESIAN_POINT('Ctrl Pts',(133.700001469487,4.017774521612,332.160028300764));
#40406=CARTESIAN_POINT('Ctrl Pts',(133.692249495964,3.93701654214815,332.049084779957));
#40407=CARTESIAN_POINT('Ctrl Pts',(133.684497522441,3.8517165891476,331.94165692255));
#40408=CARTESIAN_POINT('Ctrl Pts',(133.676748831883,3.76645276072784,331.834274560905));
#40409=CARTESIAN_POINT('Ctrl Pts',(133.669000141325,3.67665102708774,331.730405206846));
#40410=CARTESIAN_POINT('Ctrl Pts',(133.661251450768,3.58263871490179,331.630447670537));
#40411=CARTESIAN_POINT('Ctrl Pts',(133.65350437239,3.48864596276259,331.530510931229));
#40412=CARTESIAN_POINT('Ctrl Pts',(133.645757294012,3.39044464221962,331.434484675344));
#40413=CARTESIAN_POINT('Ctrl Pts',(133.638010215634,3.28840082508506,331.342732840483));
#40414=CARTESIAN_POINT('Ctrl Pts',(133.630263072328,3.1863561527251,331.250980236654));
#40415=CARTESIAN_POINT('Ctrl Pts',(133.622515929023,3.08046921019923,331.163502386647));
#40416=CARTESIAN_POINT('Ctrl Pts',(133.614768785717,2.97114091287707,331.080624445358));
#40417=CARTESIAN_POINT('Ctrl Pts',(133.607019900689,2.86178803623268,330.997727871348));
#40418=CARTESIAN_POINT('Ctrl Pts',(133.599271015661,2.74899257666471,330.919433499995));
#40419=CARTESIAN_POINT('Ctrl Pts',(133.591522130633,2.6331859892934,330.846024240768));
#40420=CARTESIAN_POINT('Ctrl Pts',(133.583765020858,2.5172564836136,330.772537064194));
#40421=CARTESIAN_POINT('Ctrl Pts',(133.576007911083,2.398309796392,330.703945567087));
#40422=CARTESIAN_POINT('Ctrl Pts',(133.568250801309,2.2768041262092,330.640487867504));
#40423=CARTESIAN_POINT('Ctrl Pts',(133.560489546382,2.15523352728129,330.576996258156));
#40424=CARTESIAN_POINT('Ctrl Pts',(133.552728291456,2.03110157420737,330.518644078881));
#40425=CARTESIAN_POINT('Ctrl Pts',(133.54496703653,1.90488727255615,330.465621592616));
#40426=CARTESIAN_POINT('Ctrl Pts',(133.537193366126,1.77847106915543,330.412514287652));
#40427=CARTESIAN_POINT('Ctrl Pts',(133.529419695721,1.64996622727507,330.364753848958));
#40428=CARTESIAN_POINT('Ctrl Pts',(133.521646025316,1.51986861208891,330.322481163642));
#40429=CARTESIAN_POINT('Ctrl Pts',(133.514234221139,1.39582707218824,330.282176281997));
#40430=CARTESIAN_POINT('Ctrl Pts',(133.506822416962,1.27033798609995,330.246859819564));
#40431=CARTESIAN_POINT('Ctrl Pts',(133.499410612785,1.14383864626459,330.216610384486));
#40432=CARTESIAN_POINT('Ctrl Pts',(133.491635534006,1.01113919696284,330.184878334485));
#40433=CARTESIAN_POINT('Ctrl Pts',(133.483860455228,0.876908604043832,330.158622291981));
#40434=CARTESIAN_POINT('Ctrl Pts',(133.47608537645,0.741638512833184,330.137988546005));
#40435=CARTESIAN_POINT('Ctrl Pts',(133.468319865401,0.606534880081532,330.117380191166));
#40436=CARTESIAN_POINT('Ctrl Pts',(133.460554354352,0.470394676928328,330.102380425216));
#40437=CARTESIAN_POINT('Ctrl Pts',(133.452788843303,0.333722847109352,330.09308527445));
#40438=CARTESIAN_POINT('Ctrl Pts',(133.44503103178,0.197186527807458,330.083799339854));
#40439=CARTESIAN_POINT('Ctrl Pts',(133.437273220258,0.0601200182785917,
330.080206790751));
#40440=CARTESIAN_POINT('Ctrl Pts',(133.429515408736,-0.0769637990857087,
330.082352225288));
#40441=CARTESIAN_POINT('Ctrl Pts',(133.421763435213,-0.213944456530078,
330.084496045318));
#40442=CARTESIAN_POINT('Ctrl Pts',(133.41401146169,-0.350942006632094,330.092369248098));
#40443=CARTESIAN_POINT('Ctrl Pts',(133.406259488167,-0.487441082877129,
330.105964420519));
#40444=CARTESIAN_POINT('Ctrl Pts',(133.398510797609,-0.623882351682428,
330.119553835376));
#40445=CARTESIAN_POINT('Ctrl Pts',(133.390762107052,-0.759825178361284,
330.138860361527));
#40446=CARTESIAN_POINT('Ctrl Pts',(133.383013416494,-0.89475705969261,330.16382456205));
#40447=CARTESIAN_POINT('Ctrl Pts',(133.375266338116,-1.0296608673191,330.188783568563));
#40448=CARTESIAN_POINT('Ctrl Pts',(133.367519259738,-1.16355376386032,330.219397836996));
#40449=CARTESIAN_POINT('Ctrl Pts',(133.359772181361,-1.29593160395851,330.255556477271));
#40450=CARTESIAN_POINT('Ctrl Pts',(133.352025038055,-1.42831055351028,330.291715420591));
#40451=CARTESIAN_POINT('Ctrl Pts',(133.344277894749,-1.55917404423149,330.333418725443));
#40452=CARTESIAN_POINT('Ctrl Pts',(133.336530751443,-1.6880316881225,330.380505213512));
#40453=CARTESIAN_POINT('Ctrl Pts',(133.328781866415,-1.81691830194784,330.427602287622));
#40454=CARTESIAN_POINT('Ctrl Pts',(133.321032981387,-1.9437978045298,330.48008481909));
#40455=CARTESIAN_POINT('Ctrl Pts',(133.313284096359,-2.06819880613954,330.537743086645));
#40456=CARTESIAN_POINT('Ctrl Pts',(133.305526986584,-2.19273184825761,330.595462553282));
#40457=CARTESIAN_POINT('Ctrl Pts',(133.297769876809,-2.31478077912562,330.658368565319));
#40458=CARTESIAN_POINT('Ctrl Pts',(133.290012767035,-2.43389740264501,330.726204673139));
#40459=CARTESIAN_POINT('Ctrl Pts',(133.282251512108,-2.55307767827928,330.794077030407));
#40460=CARTESIAN_POINT('Ctrl Pts',(133.274490257182,-2.66932219321876,330.866884525533));
#40461=CARTESIAN_POINT('Ctrl Pts',(133.266729002256,-2.78221173390346,330.944327314707));
#40462=CARTESIAN_POINT('Ctrl Pts',(133.258955331851,-2.8952818610627,331.021893987106));
#40463=CARTESIAN_POINT('Ctrl Pts',(133.251181661447,-3.00498597643254,331.104110536303));
#40464=CARTESIAN_POINT('Ctrl Pts',(133.243407991042,-3.11093726393982,331.190636220793));
#40465=CARTESIAN_POINT('Ctrl Pts',(133.235996186865,-3.21195649352298,331.273134113854));
#40466=CARTESIAN_POINT('Ctrl Pts',(133.228584382688,-3.30956420526994,331.359548799256));
#40467=CARTESIAN_POINT('Ctrl Pts',(133.221172578511,-3.40345765188556,331.449555087835));
#40468=CARTESIAN_POINT('Ctrl Pts',(133.213511082815,-3.5005142146269,331.542593540564));
#40469=CARTESIAN_POINT('Ctrl Pts',(133.205849587119,-3.59392796942943,331.639782791326));
#40470=CARTESIAN_POINT('Ctrl Pts',(133.198188091422,-3.6833150462342,331.740801734677));
#40471=CARTESIAN_POINT('Ctrl Pts',(133.190536156553,-3.77259057636755,331.84169461588));
#40472=CARTESIAN_POINT('Ctrl Pts',(133.182884221683,-3.85784915697961,331.946407386533));
#40473=CARTESIAN_POINT('Ctrl Pts',(133.175232286814,-3.93874150010774,332.05458008803));
#40474=CARTESIAN_POINT('Ctrl Pts',(133.167589038231,-4.01954201625486,332.16262999456));
#40475=CARTESIAN_POINT('Ctrl Pts',(133.159945789648,-4.09598592049617,332.274131693386));
#40476=CARTESIAN_POINT('Ctrl Pts',(133.152302541065,-4.16776268013728,332.388690500045));
#40477=CARTESIAN_POINT('Ctrl Pts',(133.144664156999,-4.23949375773086,332.503176396185));
#40478=CARTESIAN_POINT('Ctrl Pts',(133.137025772933,-4.30656338277509,332.620715191685));
#40479=CARTESIAN_POINT('Ctrl Pts',(133.129387388867,-4.36870312452959,332.74088157189));
#40480=CARTESIAN_POINT('Ctrl Pts',(133.121752099894,-4.43081768709791,332.860999260363));
#40481=CARTESIAN_POINT('Ctrl Pts',(133.114116810921,-4.48800615405122,332.983742058596));
#40482=CARTESIAN_POINT('Ctrl Pts',(133.106481521948,-4.54004531548502,333.108658783867));
#40483=CARTESIAN_POINT('Ctrl Pts',(133.098847561528,-4.592075422017,333.233553773417));
#40484=CARTESIAN_POINT('Ctrl Pts',(133.091213601108,-4.63895785133504,333.360621565049));
#40485=CARTESIAN_POINT('Ctrl Pts',(133.083579640688,-4.68051717966776,333.489390191567));
#40486=CARTESIAN_POINT('Ctrl Pts',(133.075942212416,-4.7220953870101,333.618217313355));
#40487=CARTESIAN_POINT('Ctrl Pts',(133.068304784144,-4.75834553472749,333.748746430563));
#40488=CARTESIAN_POINT('Ctrl Pts',(133.060667355872,-4.78914182396789,333.880489547873));
#40489=CARTESIAN_POINT('Ctrl Pts',(133.053028265726,-4.81994481435949,334.012261331966));
#40490=CARTESIAN_POINT('Ctrl Pts',(133.04538917558,-4.84529150255409,334.145247246808));
#40491=CARTESIAN_POINT('Ctrl Pts',(133.037750085433,-4.86510731614558,334.278949471336));
#40492=CARTESIAN_POINT('Ctrl Pts',(133.030103040723,-4.88494376388924,334.412790919622));
#40493=CARTESIAN_POINT('Ctrl Pts',(133.022455996013,-4.89923778582828,334.547349766649));
#40494=CARTESIAN_POINT('Ctrl Pts',(133.014808951304,-4.90796672328694,334.682123128227));
#40495=CARTESIAN_POINT('Ctrl Pts',(133.008718050377,-4.91491935600626,334.789470636196));
#40496=CARTESIAN_POINT('Ctrl Pts',(133.00262714945,-4.91834241697973,334.896954093159));
#40497=CARTESIAN_POINT('Ctrl Pts',(132.996536248523,-4.91824810241123,335.004320373636));
#40498=CARTESIAN_POINT('',(136.49653624846,-4.91824792654204,334.995483855083));
#40499=CARTESIAN_POINT('Ctrl Pts',(136.49653624846,-4.91824792654204,334.995483855083));
#40500=CARTESIAN_POINT('Ctrl Pts',(136.488880220191,-4.91837200760644,335.130612698127));
#40501=CARTESIAN_POINT('Ctrl Pts',(136.481224191922,-4.91292290562032,335.265902532329));
#40502=CARTESIAN_POINT('Ctrl Pts',(136.473568163653,-4.9018876379854,335.400849905907));
#40503=CARTESIAN_POINT('Ctrl Pts',(136.465577446647,-4.89036995575505,335.541696600172));
#40504=CARTESIAN_POINT('Ctrl Pts',(136.457586729642,-4.87276658776302,335.682169772044));
#40505=CARTESIAN_POINT('Ctrl Pts',(136.449596012637,-4.84912339044322,335.821696663469));
#40506=CARTESIAN_POINT('Ctrl Pts',(136.441948571372,-4.82649588872065,335.955229575002));
#40507=CARTESIAN_POINT('Ctrl Pts',(136.434301130108,-4.79833678172102,336.087895379985));
#40508=CARTESIAN_POINT('Ctrl Pts',(136.426653688844,-4.76473917465448,336.219197957681));
#40509=CARTESIAN_POINT('Ctrl Pts',(136.419007402992,-4.73114664367949,336.350480697538));
#40510=CARTESIAN_POINT('Ctrl Pts',(136.411361117141,-4.69211734596046,336.480400230189));
#40511=CARTESIAN_POINT('Ctrl Pts',(136.40371483129,-4.64779509938816,336.608472497932));
#40512=CARTESIAN_POINT('Ctrl Pts',(136.396067943003,-4.60346936075534,336.736554856231));
#40513=CARTESIAN_POINT('Ctrl Pts',(136.388421054716,-4.55384997580059,336.862789280302));
#40514=CARTESIAN_POINT('Ctrl Pts',(136.380774166429,-4.49912986394917,336.986709221255));
#40515=CARTESIAN_POINT('Ctrl Pts',(136.373124917608,-4.44439286042653,337.110667415327));
#40516=CARTESIAN_POINT('Ctrl Pts',(136.365475668787,-4.38455216153253,337.232309338066));
#40517=CARTESIAN_POINT('Ctrl Pts',(136.357826419965,-4.31984757795824,337.35119118017));
#40518=CARTESIAN_POINT('Ctrl Pts',(136.350168933632,-4.25507331371344,337.470201046688));
#40519=CARTESIAN_POINT('Ctrl Pts',(136.342511447298,-4.18542490274012,337.586444546877));
#40520=CARTESIAN_POINT('Ctrl Pts',(136.334853960964,-4.1111867358577,337.699504896348));
#40521=CARTESIAN_POINT('Ctrl Pts',(136.327191619778,-4.03690150191032,337.812636926184));
#40522=CARTESIAN_POINT('Ctrl Pts',(136.319529278591,-3.95802095341253,337.922581462587));
#40523=CARTESIAN_POINT('Ctrl Pts',(136.311866937404,-3.87487022793623,338.028954238537));
#40524=CARTESIAN_POINT('Ctrl Pts',(136.304193797532,-3.79160231653885,338.135476927692));
#40525=CARTESIAN_POINT('Ctrl Pts',(136.29652065766,-3.70405247838207,338.238417506861));
#40526=CARTESIAN_POINT('Ctrl Pts',(136.288847517788,-3.6125833477282,338.337427844646));
#40527=CARTESIAN_POINT('Ctrl Pts',(136.286495330367,-3.58454364792289,338.367779288125));
#40528=CARTESIAN_POINT('Ctrl Pts',(136.284143142945,-3.55613588360524,338.397761682906));
#40529=CARTESIAN_POINT('Ctrl Pts',(136.281790955524,-3.52737111106981,338.427365767946));
#40530=CARTESIAN_POINT('Ctrl Pts',(136.274015876745,-3.43229009394204,338.525221105175));
#40531=CARTESIAN_POINT('Ctrl Pts',(136.266240797967,-3.33298373222669,338.619271508503));
#40532=CARTESIAN_POINT('Ctrl Pts',(136.258465719188,-3.22978891642843,338.709130169975));
#40533=CARTESIAN_POINT('Ctrl Pts',(136.250700208139,-3.12672108842059,338.798878254643));
#40534=CARTESIAN_POINT('Ctrl Pts',(136.24293469709,-3.01977461905091,338.884444606572));
#40535=CARTESIAN_POINT('Ctrl Pts',(136.235169186041,-2.90932454398892,338.965477746785));
#40536=CARTESIAN_POINT('Ctrl Pts',(136.227411374519,-2.79898398049803,339.046430542402));
#40537=CARTESIAN_POINT('Ctrl Pts',(136.219653562997,-2.68514703756664,339.122858841268));
#40538=CARTESIAN_POINT('Ctrl Pts',(136.211895751475,-2.56822299344343,339.194450347596));
#40539=CARTESIAN_POINT('Ctrl Pts',(136.204143777952,-2.45138693837106,339.265987979046));
#40540=CARTESIAN_POINT('Ctrl Pts',(136.196391804429,-2.33146873821512,339.332695859595));
#40541=CARTESIAN_POINT('Ctrl Pts',(136.188639830906,-2.20890761936723,339.394304289828));
#40542=CARTESIAN_POINT('Ctrl Pts',(136.180891140348,-2.08639840522611,339.455886628854));
#40543=CARTESIAN_POINT('Ctrl Pts',(136.173142449791,-1.96124884706467,339.512373637709));
#40544=CARTESIAN_POINT('Ctrl Pts',(136.165393759233,-1.83392360993417,339.563541087295));
#40545=CARTESIAN_POINT('Ctrl Pts',(136.157646680855,-1.70662486388266,339.614697891065));
#40546=CARTESIAN_POINT('Ctrl Pts',(136.149899602477,-1.57715170170746,339.660537191367));
#40547=CARTESIAN_POINT('Ctrl Pts',(136.142152524099,-1.4459892810726,339.700882689615));
#40548=CARTESIAN_POINT('Ctrl Pts',(136.134405380794,-1.31482576117042,339.741228525997));
#40549=CARTESIAN_POINT('Ctrl Pts',(136.126658237488,-1.18197332816933,339.776080353569));
#40550=CARTESIAN_POINT('Ctrl Pts',(136.118911094182,-1.04793244838807,339.805311711649));
#40551=CARTESIAN_POINT('Ctrl Pts',(136.111162209154,-0.913861433370988,
339.83454964156));
#40552=CARTESIAN_POINT('Ctrl Pts',(136.103413324126,-0.778601821723289,
339.858164504288));
#40553=CARTESIAN_POINT('Ctrl Pts',(136.095664439098,-0.642664027625574,
339.876081009386));
#40554=CARTESIAN_POINT('Ctrl Pts',(136.087907329323,-0.50658194774898,339.894016531247));
#40555=CARTESIAN_POINT('Ctrl Pts',(136.080150219548,-0.369820635629727,
339.906241562284));
#40556=CARTESIAN_POINT('Ctrl Pts',(136.072393109773,-0.232895938429691,
339.912732696205));
#40557=CARTESIAN_POINT('Ctrl Pts',(136.064631854847,-0.0958980730494751,
339.91922729878));
#40558=CARTESIAN_POINT('Ctrl Pts',(136.056870599921,0.0412629607100064,
339.919981896772));
#40559=CARTESIAN_POINT('Ctrl Pts',(136.049109344995,0.178072557094469,339.91502525191));
#40560=CARTESIAN_POINT('Ctrl Pts',(136.04133567459,0.31510100424691,339.910060678031));
#40561=CARTESIAN_POINT('Ctrl Pts',(136.033562004186,0.451776500723456,339.899366635117));
#40562=CARTESIAN_POINT('Ctrl Pts',(136.025788333781,0.587589903084384,339.883023773062));
#40563=CARTESIAN_POINT('Ctrl Pts',(136.018376529604,0.717081158889626,339.867441675169));
#40564=CARTESIAN_POINT('Ctrl Pts',(136.010964725427,0.845788491179478,339.846724873767));
#40565=CARTESIAN_POINT('Ctrl Pts',(136.00355292125,0.973282085195013,339.820985899703));
#40566=CARTESIAN_POINT('Ctrl Pts',(135.995777842472,1.10702452003798,339.793985381848));
#40567=CARTESIAN_POINT('Ctrl Pts',(135.988002763693,1.23985388119609,339.761372613526));
#40568=CARTESIAN_POINT('Ctrl Pts',(135.980227684915,1.37126258282383,339.723221569167));
#40569=CARTESIAN_POINT('Ctrl Pts',(135.972462173866,1.50250957767816,339.685117472098));
#40570=CARTESIAN_POINT('Ctrl Pts',(135.964696662817,1.63233901965662,339.641488767228));
#40571=CARTESIAN_POINT('Ctrl Pts',(135.956931151768,1.76025238926696,339.592460624609));
#40572=CARTESIAN_POINT('Ctrl Pts',(135.949173340245,1.88803893239909,339.543481093536));
#40573=CARTESIAN_POINT('Ctrl Pts',(135.941415528723,2.01391282122397,339.489112917591));
#40574=CARTESIAN_POINT('Ctrl Pts',(135.933657717201,2.13738995560857,339.429531266417));
#40575=CARTESIAN_POINT('Ctrl Pts',(135.925905743678,2.26077416953356,339.369994452325));
#40576=CARTESIAN_POINT('Ctrl Pts',(135.918153770155,2.38176486844677,339.305252141334));
#40577=CARTESIAN_POINT('Ctrl Pts',(135.910401796632,2.49989756575133,339.235527738458));
#40578=CARTESIAN_POINT('Ctrl Pts',(135.902653106075,2.61798023378877,339.165832863909));
#40579=CARTESIAN_POINT('Ctrl Pts',(135.894904415517,2.73320697163412,339.091160292218));
#40580=CARTESIAN_POINT('Ctrl Pts',(135.887155724959,2.84513776333188,339.011779426908));
#40581=CARTESIAN_POINT('Ctrl Pts',(135.879408646581,2.95704526689345,338.932415077451));
#40582=CARTESIAN_POINT('Ctrl Pts',(135.871661568204,3.06565786967789,338.848344608841));
#40583=CARTESIAN_POINT('Ctrl Pts',(135.863914489826,3.17056477179156,338.759880595228));
#40584=CARTESIAN_POINT('Ctrl Pts',(135.85616734652,3.2754725531259,338.671415840202));
#40585=CARTESIAN_POINT('Ctrl Pts',(135.848420203214,3.37667427302956,338.578557718706));
#40586=CARTESIAN_POINT('Ctrl Pts',(135.840673059908,3.47379275697694,338.481658648414));
#40587=CARTESIAN_POINT('Ctrl Pts',(135.83292417488,3.57093307522166,338.384737793153));
#40588=CARTESIAN_POINT('Ctrl Pts',(135.825175289852,3.66398805414817,338.283774457325));
#40589=CARTESIAN_POINT('Ctrl Pts',(135.817426404824,3.75261816601189,338.17915711512));
#40590=CARTESIAN_POINT('Ctrl Pts',(135.809669295049,3.84134235079202,338.074428730987));
#40591=CARTESIAN_POINT('Ctrl Pts',(135.801912185275,3.92563203355077,337.966038891718));
#40592=CARTESIAN_POINT('Ctrl Pts',(135.7941550755,4.00518837693964,337.854408717708));
#40593=CARTESIAN_POINT('Ctrl Pts',(135.786393820574,4.08478723269454,337.742718892103));
#40594=CARTESIAN_POINT('Ctrl Pts',(135.778632565648,4.15964749591002,337.627785608884));
#40595=CARTESIAN_POINT('Ctrl Pts',(135.770871310722,4.22951487023652,337.510057175633));
#40596=CARTESIAN_POINT('Ctrl Pts',(135.763097640317,4.29949400959234,337.392140415256));
#40597=CARTESIAN_POINT('Ctrl Pts',(135.755323969912,4.36446411434039,337.271419914181));
#40598=CARTESIAN_POINT('Ctrl Pts',(135.747550299508,4.42421747796838,337.148367466273));
#40599=CARTESIAN_POINT('Ctrl Pts',(135.74013849533,4.48118930814455,337.031043139418));
#40600=CARTESIAN_POINT('Ctrl Pts',(135.732726691153,4.53341903060046,336.911599347874));
#40601=CARTESIAN_POINT('Ctrl Pts',(135.725314886976,4.58076867749739,336.790458428939));
#40602=CARTESIAN_POINT('Ctrl Pts',(135.717539808198,4.63043907163535,336.663380032709));
#40603=CARTESIAN_POINT('Ctrl Pts',(135.709764729419,4.67489588805964,336.534032348861));
#40604=CARTESIAN_POINT('Ctrl Pts',(135.701989650641,4.7139266496224,336.402882248972));
#40605=CARTESIAN_POINT('Ctrl Pts',(135.694224139592,4.75290938134819,336.27189353763));
#40606=CARTESIAN_POINT('Ctrl Pts',(135.686458628543,4.78647923331155,336.13910719446));
#40607=CARTESIAN_POINT('Ctrl Pts',(135.678693117494,4.81447168617738,336.005010171837));
#40608=CARTESIAN_POINT('Ctrl Pts',(135.670935305971,4.84243638444472,335.871046106802));
#40609=CARTESIAN_POINT('Ctrl Pts',(135.663177494449,4.8648346092841,335.735774328639));
#40610=CARTESIAN_POINT('Ctrl Pts',(135.655419682927,4.88155169022486,335.599696721821));
#40611=CARTESIAN_POINT('Ctrl Pts',(135.647667709404,4.89825619103208,335.463721517717));
#40612=CARTESIAN_POINT('Ctrl Pts',(135.639915735881,4.90928801013023,335.326942078388));
#40613=CARTESIAN_POINT('Ctrl Pts',(135.632163762358,4.91458365321138,335.189869897792));
#40614=CARTESIAN_POINT('Ctrl Pts',(135.6244150718,4.91987705358453,335.052855767346));
#40615=CARTESIAN_POINT('Ctrl Pts',(135.616666381243,4.91943909453702,334.915549531984));
#40616=CARTESIAN_POINT('Ctrl Pts',(135.608917690685,4.91325820535681,334.778467000214));
#40617=CARTESIAN_POINT('Ctrl Pts',(135.601170612307,4.90707860216221,334.641412989611));
#40618=CARTESIAN_POINT('Ctrl Pts',(135.593423533929,4.89515846310018,334.504582980254));
#40619=CARTESIAN_POINT('Ctrl Pts',(135.585676455552,4.87753833104645,334.368491574346));
#40620=CARTESIAN_POINT('Ctrl Pts',(135.577929312246,4.85991805131904,334.23239902786));
#40621=CARTESIAN_POINT('Ctrl Pts',(135.57018216894,4.83659773350489,334.097045484809));
#40622=CARTESIAN_POINT('Ctrl Pts',(135.562435025634,4.80766962236658,333.962938832723));
#40623=CARTESIAN_POINT('Ctrl Pts',(135.554686140606,4.77873500757465,333.828802030614));
#40624=CARTESIAN_POINT('Ctrl Pts',(135.546937255578,4.74419017310846,333.695913059302));
#40625=CARTESIAN_POINT('Ctrl Pts',(135.53918837055,4.70417805725921,333.564767660586));
#40626=CARTESIAN_POINT('Ctrl Pts',(135.531431260775,4.66412347213697,333.433483062789));
#40627=CARTESIAN_POINT('Ctrl Pts',(135.523674151,4.61859012778119,333.303946108879));
#40628=CARTESIAN_POINT('Ctrl Pts',(135.515917041226,4.56777043528063,333.176635989969));
#40629=CARTESIAN_POINT('Ctrl Pts',(135.5081557863,4.51692358636127,333.049257840602));
#40630=CARTESIAN_POINT('Ctrl Pts',(135.500394531373,4.46078492041568,332.92410925377));
#40631=CARTESIAN_POINT('Ctrl Pts',(135.492633276447,4.39959381450564,332.801646677655));
#40632=CARTESIAN_POINT('Ctrl Pts',(135.484859606043,4.33830482276827,332.678988201329));
#40633=CARTESIAN_POINT('Ctrl Pts',(135.477085935638,4.27194742961757,332.559024664097));
#40634=CARTESIAN_POINT('Ctrl Pts',(135.469312265233,4.20080597466927,332.44218604553));
#40635=CARTESIAN_POINT('Ctrl Pts',(135.461900461056,4.13297617156452,332.330786292766));
#40636=CARTESIAN_POINT('Ctrl Pts',(135.454488656879,4.06079783879632,332.222227315595));
#40637=CARTESIAN_POINT('Ctrl Pts',(135.447076852702,3.98455146649534,332.11685368506));
#40638=CARTESIAN_POINT('Ctrl Pts',(135.439301773924,3.90456803236149,332.006315379001));
#40639=CARTESIAN_POINT('Ctrl Pts',(135.431526695145,3.81985493980073,331.898933239927));
#40640=CARTESIAN_POINT('Ctrl Pts',(135.423751616367,3.73068980750526,331.795138595403));
#40641=CARTESIAN_POINT('Ctrl Pts',(135.415986105318,3.64163439858168,331.691471676797));
#40642=CARTESIAN_POINT('Ctrl Pts',(135.408220594269,3.54813810287312,331.591383762532));
#40643=CARTESIAN_POINT('Ctrl Pts',(135.40045508322,3.45052137816715,331.495276718297));
#40644=CARTESIAN_POINT('Ctrl Pts',(135.392697271697,3.35300144072778,331.399264964476));
#40645=CARTESIAN_POINT('Ctrl Pts',(135.384939460175,3.25136948124354,331.307226498306));
#40646=CARTESIAN_POINT('Ctrl Pts',(135.377181648653,3.14598549030458,331.219529347119));
#40647=CARTESIAN_POINT('Ctrl Pts',(135.36942967513,3.04068080416094,331.13189819082));
#40648=CARTESIAN_POINT('Ctrl Pts',(135.361677701607,2.93163000588674,331.048602095762));
#40649=CARTESIAN_POINT('Ctrl Pts',(135.353925728084,2.81922886125216,330.969971254397));
#40650=CARTESIAN_POINT('Ctrl Pts',(135.346177037526,2.70687531856899,330.891373713241));
#40651=CARTESIAN_POINT('Ctrl Pts',(135.338428346969,2.5911745711822,330.817437719762));
#40652=CARTESIAN_POINT('Ctrl Pts',(135.330679656411,2.47255411189487,330.748452137603));
#40653=CARTESIAN_POINT('Ctrl Pts',(135.322932578033,2.35395833258491,330.67948090847));
#40654=CARTESIAN_POINT('Ctrl Pts',(135.315185499655,2.2324443873526,330.615458238345));
#40655=CARTESIAN_POINT('Ctrl Pts',(135.307438421278,2.10846695624441,330.556628514638));
#40656=CARTESIAN_POINT('Ctrl Pts',(135.299691277972,1.98448848608576,330.497798297881));
#40657=CARTESIAN_POINT('Ctrl Pts',(135.291944134666,1.85804684200413,330.444161281919));
#40658=CARTESIAN_POINT('Ctrl Pts',(135.28419699136,1.72961903639317,330.395914743247));
#40659=CARTESIAN_POINT('Ctrl Pts',(135.276448106332,1.60116235748504,330.34765735773));
#40660=CARTESIAN_POINT('Ctrl Pts',(135.268699221304,1.47071899433501,330.30479299847));
#40661=CARTESIAN_POINT('Ctrl Pts',(135.260950336276,1.33878317890999,330.267469739942));
#40662=CARTESIAN_POINT('Ctrl Pts',(135.253193226501,1.20670732544751,330.230106866122));
#40663=CARTESIAN_POINT('Ctrl Pts',(135.245436116726,1.07313623202158,330.198296948212));
#40664=CARTESIAN_POINT('Ctrl Pts',(135.237679006952,0.938576985342084,330.172137501431));
#40665=CARTESIAN_POINT('Ctrl Pts',(135.229917752026,0.803945834503438,330.145964075878));
#40666=CARTESIAN_POINT('Ctrl Pts',(135.222156497099,0.668325864529675,330.125447196379));
#40667=CARTESIAN_POINT('Ctrl Pts',(135.214395242173,0.532230453097473,330.110632575957));
#40668=CARTESIAN_POINT('Ctrl Pts',(135.206621571769,0.395917333360418,330.09579425697));
#40669=CARTESIAN_POINT('Ctrl Pts',(135.198847901364,0.259127642572011,330.086676451041));
#40670=CARTESIAN_POINT('Ctrl Pts',(135.191074230959,0.122376832207485,330.083272737538));
#40671=CARTESIAN_POINT('Ctrl Pts',(135.183662426782,-0.00800819503385429,
330.080027467717));
#40672=CARTESIAN_POINT('Ctrl Pts',(135.176250622605,-0.138357592394053,
330.081976275939));
#40673=CARTESIAN_POINT('Ctrl Pts',(135.168838818428,-0.268229813425918,
330.089069759232));
#40674=CARTESIAN_POINT('Ctrl Pts',(135.16106373965,-0.404467458880331,330.096510915272));
#40675=CARTESIAN_POINT('Ctrl Pts',(135.153288660871,-0.540610505746174,
330.109637325042));
#40676=CARTESIAN_POINT('Ctrl Pts',(135.145513582093,-0.676146006067357,
330.128448949156));
#40677=CARTESIAN_POINT('Ctrl Pts',(135.137748071044,-0.811514721326461,
330.147237424369));
#40678=CARTESIAN_POINT('Ctrl Pts',(135.129982559995,-0.94627699413789,330.171697140634));
#40679=CARTESIAN_POINT('Ctrl Pts',(135.122217048946,-1.07992146897312,330.201776090745));
#40680=CARTESIAN_POINT('Ctrl Pts',(135.114459237424,-1.21343343492265,330.231825217488));
#40681=CARTESIAN_POINT('Ctrl Pts',(135.106701425902,-1.34582942959668,330.26748240523));
#40682=CARTESIAN_POINT('Ctrl Pts',(135.098943614379,-1.47660515939545,330.308644090911));
#40683=CARTESIAN_POINT('Ctrl Pts',(135.091191640856,-1.6072824763105,330.349774801117));
#40684=CARTESIAN_POINT('Ctrl Pts',(135.083439667333,-1.73634158396792,330.396401647318));
#40685=CARTESIAN_POINT('Ctrl Pts',(135.07568769381,-1.86329064492519,330.448370507715));
#40686=CARTESIAN_POINT('Ctrl Pts',(135.067939003253,-1.99018594287999,330.500317359269));
#40687=CARTESIAN_POINT('Ctrl Pts',(135.060190312695,-2.11497261046951,330.557601577597));
#40688=CARTESIAN_POINT('Ctrl Pts',(135.052441622138,-2.23717639521115,330.62001999557));
#40689=CARTESIAN_POINT('Ctrl Pts',(135.04469454376,-2.35935475443446,330.682425426869));
#40690=CARTESIAN_POINT('Ctrl Pts',(135.036947465382,-2.47895095184019,330.749962755377));
#40691=CARTESIAN_POINT('Ctrl Pts',(135.029200387004,-2.59551342337868,330.822381882991));
#40692=CARTESIAN_POINT('Ctrl Pts',(135.021453243698,-2.71207687182351,330.894801617548));
#40693=CARTESIAN_POINT('Ctrl Pts',(135.013706100392,-2.8256062116748,330.972103026542));
#40694=CARTESIAN_POINT('Ctrl Pts',(135.005958957087,-2.9356774101408,331.053991737706));
#40695=CARTESIAN_POINT('Ctrl Pts',(134.998210072058,-3.04577335494865,331.135898859191));
#40696=CARTESIAN_POINT('Ctrl Pts',(134.99046118703,-3.15240929776071,331.222395101799));
#40697=CARTESIAN_POINT('Ctrl Pts',(134.982712302002,-3.25519326231551,331.31314498692));
#40698=CARTESIAN_POINT('Ctrl Pts',(134.974955192228,-3.35808632283232,331.403991194906));
#40699=CARTESIAN_POINT('Ctrl Pts',(134.967198082453,-3.4571189443977,331.499099805149));
#40700=CARTESIAN_POINT('Ctrl Pts',(134.959440972678,-3.55193471066977,331.598097168695));
#40701=CARTESIAN_POINT('Ctrl Pts',(134.951679717752,-3.64680114345565,331.697147433267));
#40702=CARTESIAN_POINT('Ctrl Pts',(134.943918462826,-3.73744597276019,331.800090298588));
#40703=CARTESIAN_POINT('Ctrl Pts',(134.9361572079,-3.82355293940824,331.906518792357));
#40704=CARTESIAN_POINT('Ctrl Pts',(134.928383537495,-3.90979764914072,332.01311753703));
#40705=CARTESIAN_POINT('Ctrl Pts',(134.92060986709,-3.99148975734294,332.123212738326));
#40706=CARTESIAN_POINT('Ctrl Pts',(134.912836196686,-4.0683557228909,332.236367467531));
#40707=CARTESIAN_POINT('Ctrl Pts',(134.905424392509,-4.1416435592496,332.344254816868));
#40708=CARTESIAN_POINT('Ctrl Pts',(134.898012588332,-4.21054430319857,332.454923017942));
#40709=CARTESIAN_POINT('Ctrl Pts',(134.890600784154,-4.2748605526315,332.567974030144));
#40710=CARTESIAN_POINT('Ctrl Pts',(134.882487617091,-4.34526290867109,332.691722813412));
#40711=CARTESIAN_POINT('Ctrl Pts',(134.874374450027,-4.41037836836449,332.81868940777));
#40712=CARTESIAN_POINT('Ctrl Pts',(134.866261282963,-4.46991427174387,332.948403191229));
#40713=CARTESIAN_POINT('Ctrl Pts',(134.858161266845,-4.52935367107875,333.077906716607));
#40714=CARTESIAN_POINT('Ctrl Pts',(134.850061250727,-4.58323139045913,333.210148250226));
#40715=CARTESIAN_POINT('Ctrl Pts',(134.841961234609,-4.63129969921503,333.344631111036));
#40716=CARTESIAN_POINT('Ctrl Pts',(134.833878080244,-4.67926794447111,333.478834019709));
#40717=CARTESIAN_POINT('Ctrl Pts',(134.825794925879,-4.7214507781199,333.615268631362));
#40718=CARTESIAN_POINT('Ctrl Pts',(134.817711771514,-4.7576480650366,333.753417490997));
#40719=CARTESIAN_POINT('Ctrl Pts',(134.809638480598,-4.79380118230602,333.891397774836));
#40720=CARTESIAN_POINT('Ctrl Pts',(134.801565189681,-4.82398321470201,334.031087810636));
#40721=CARTESIAN_POINT('Ctrl Pts',(134.793491898765,-4.84804299991267,334.17195281928));
#40722=CARTESIAN_POINT('Ctrl Pts',(134.785431051445,-4.87206570108183,334.31260070862));
#40723=CARTESIAN_POINT('Ctrl Pts',(134.777370204125,-4.88998491290346,334.454419623487));
#40724=CARTESIAN_POINT('Ctrl Pts',(134.769309356805,-4.90170006679297,334.596862904582));
#40725=CARTESIAN_POINT('Ctrl Pts',(134.7617183207,-4.91273242513222,334.731004148896));
#40726=CARTESIAN_POINT('Ctrl Pts',(134.754127284595,-4.91826319865876,334.865698748933));
#40727=CARTESIAN_POINT('Ctrl Pts',(134.74653624849,-4.9182499763342,335.000482481796));
#40728=CARTESIAN_POINT('',(138.246536248522,-4.91824966475132,335.001815949749));
#40729=CARTESIAN_POINT('Ctrl Pts',(138.24653624849,-4.91824966475112,335.001815950303));
#40730=CARTESIAN_POINT('Ctrl Pts',(138.240843230807,-4.91821275526505,335.101780176863));
#40731=CARTESIAN_POINT('Ctrl Pts',(138.235150213124,-4.91512839652291,335.201684563828));
#40732=CARTESIAN_POINT('Ctrl Pts',(138.229457195442,-4.90900608956926,335.30140052268));
#40733=CARTESIAN_POINT('Ctrl Pts',(138.221682116663,-4.90064472104323,335.437584788873));
#40734=CARTESIAN_POINT('Ctrl Pts',(138.213907037885,-4.88659886760582,335.5736360507));
#40735=CARTESIAN_POINT('Ctrl Pts',(138.206131959106,-4.86687203397043,335.709041372176));
#40736=CARTESIAN_POINT('Ctrl Pts',(138.198366448057,-4.8471694754597,335.844280068783));
#40737=CARTESIAN_POINT('Ctrl Pts',(138.190600937008,-4.82179990226589,335.97887402351));
#40738=CARTESIAN_POINT('Ctrl Pts',(138.182835425959,-4.7908187749794,336.112312243844));
#40739=CARTESIAN_POINT('Ctrl Pts',(138.175077614437,-4.75986836557079,336.245618159794));
#40740=CARTESIAN_POINT('Ctrl Pts',(138.167319802915,-4.72331756232056,336.37777024349));
#40741=CARTESIAN_POINT('Ctrl Pts',(138.159561991393,-4.68127333278809,336.508264912483));
#40742=CARTESIAN_POINT('Ctrl Pts',(138.15181001787,-4.63926074287154,336.638661380099));
#40743=CARTESIAN_POINT('Ctrl Pts',(138.144058044347,-4.59176307453842,336.767402545074));
#40744=CARTESIAN_POINT('Ctrl Pts',(138.136306070824,-4.53893776878225,336.893997622391));
#40745=CARTESIAN_POINT('Ctrl Pts',(138.128557380266,-4.48613483457457,337.020539086617));
#40746=CARTESIAN_POINT('Ctrl Pts',(138.120808689709,-4.42800890069209,337.144935910884));
#40747=CARTESIAN_POINT('Ctrl Pts',(138.113059999151,-4.3647663335395,337.266715226071));
#40748=CARTESIAN_POINT('Ctrl Pts',(138.105312920773,-4.3015369245312,337.388469204054));
#40749=CARTESIAN_POINT('Ctrl Pts',(138.097565842395,-4.23319317976694,337.507606409525));
#40750=CARTESIAN_POINT('Ctrl Pts',(138.089818764018,-4.1599882422768,337.62367697833));
#40751=CARTESIAN_POINT('Ctrl Pts',(138.082071620712,-4.08678269125879,337.739748519918));
#40752=CARTESIAN_POINT('Ctrl Pts',(138.074324477406,-4.00871607476777,337.852753042965));
#40753=CARTESIAN_POINT('Ctrl Pts',(138.0665773341,-3.92608562299602,337.962268513049));
#40754=CARTESIAN_POINT('Ctrl Pts',(138.058828449072,-3.8434365941445,338.071808604536));
#40755=CARTESIAN_POINT('Ctrl Pts',(138.051079564044,-3.75622192367133,338.177857770205));
#40756=CARTESIAN_POINT('Ctrl Pts',(138.043330679016,-3.66477973060957,338.280026309134));
#40757=CARTESIAN_POINT('Ctrl Pts',(138.035573569241,-3.57324047985925,338.382303290807));
#40758=CARTESIAN_POINT('Ctrl Pts',(138.027816459466,-3.47746500413433,338.480691126062));
#40759=CARTESIAN_POINT('Ctrl Pts',(138.020059349692,-3.37782935170732,338.574835930955));
#40760=CARTESIAN_POINT('Ctrl Pts',(138.012298094765,-3.27814045717343,338.669031043821));
#40761=CARTESIAN_POINT('Ctrl Pts',(138.004536839839,-3.1745875706577,338.758978352254));
#40762=CARTESIAN_POINT('Ctrl Pts',(137.996775584913,-3.06757979172964,338.844364353683));
#40763=CARTESIAN_POINT('Ctrl Pts',(137.989001914508,-2.96040083522901,338.929886944888));
#40764=CARTESIAN_POINT('Ctrl Pts',(137.981228244104,-2.84975625795989,339.010833417398));
#40765=CARTESIAN_POINT('Ctrl Pts',(137.973454573699,-2.7360848266308,339.086933188098));
#40766=CARTESIAN_POINT('Ctrl Pts',(137.966042769522,-2.62770482777796,339.159490496164));
#40767=CARTESIAN_POINT('Ctrl Pts',(137.958630965345,-2.51657367857949,339.2276420253));
#40768=CARTESIAN_POINT('Ctrl Pts',(137.951219161168,-2.40309074415355,339.291193066953));
#40769=CARTESIAN_POINT('Ctrl Pts',(137.943444082389,-2.2840456730631,339.357858934466));
#40770=CARTESIAN_POINT('Ctrl Pts',(137.935669003611,-2.16203624722082,339.419672621049));
#40771=CARTESIAN_POINT('Ctrl Pts',(137.927893924833,-2.03749570204059,339.476359494798));
#40772=CARTESIAN_POINT('Ctrl Pts',(137.920128413784,-1.91310841192979,339.532976611739));
#40773=CARTESIAN_POINT('Ctrl Pts',(137.912362902735,-1.78619655220239,339.584479308307));
#40774=CARTESIAN_POINT('Ctrl Pts',(137.904597391686,-1.65721984027246,339.630637695124));
#40775=CARTESIAN_POINT('Ctrl Pts',(137.896839580163,-1.52837100912795,339.676750315767));
#40776=CARTESIAN_POINT('Ctrl Pts',(137.889081768641,-1.39746176568338,339.71752904091));
#40777=CARTESIAN_POINT('Ctrl Pts',(137.881323957119,-1.26497346944824,339.752791304496));
#40778=CARTESIAN_POINT('Ctrl Pts',(137.873571983596,-1.1325848748576,339.788027032111));
#40779=CARTESIAN_POINT('Ctrl Pts',(137.865820010073,-0.998619968907839,
339.817754461025));
#40780=CARTESIAN_POINT('Ctrl Pts',(137.85806803655,-0.86357666354513,339.841840394796));
#40781=CARTESIAN_POINT('Ctrl Pts',(137.850319345992,-0.728590549102326,
339.86591612816));
#40782=CARTESIAN_POINT('Ctrl Pts',(137.842570655435,-0.592527327597096,
339.884355049795));
#40783=CARTESIAN_POINT('Ctrl Pts',(137.834821964877,-0.455896321464846,
339.897074800999));
#40784=CARTESIAN_POINT('Ctrl Pts',(137.827074886499,-0.319293742554587,
339.909791905752));
#40785=CARTESIAN_POINT('Ctrl Pts',(137.819327808121,-0.182124002937933,
339.916792170701));
#40786=CARTESIAN_POINT('Ctrl Pts',(137.811580729744,-0.0449023931984699,
339.918045021915));
#40787=CARTESIAN_POINT('Ctrl Pts',(137.803833586438,0.0923203665902042,
339.919297883629));
#40788=CARTESIAN_POINT('Ctrl Pts',(137.796086443132,0.229594606510773,339.914803231962));
#40789=CARTESIAN_POINT('Ctrl Pts',(137.788339299826,0.366404580502749,339.904582627083));
#40790=CARTESIAN_POINT('Ctrl Pts',(137.780590414798,0.503245312281391,339.894359724395));
#40791=CARTESIAN_POINT('Ctrl Pts',(137.77284152977,0.63962118072128,339.878408335994));
#40792=CARTESIAN_POINT('Ctrl Pts',(137.765092644742,0.775021502395107,339.856801903859));
#40793=CARTESIAN_POINT('Ctrl Pts',(137.757335534967,0.910565539369398,339.835172538433));
#40794=CARTESIAN_POINT('Ctrl Pts',(137.749578425192,1.04513157455788,339.807876200765));
#40795=CARTESIAN_POINT('Ctrl Pts',(137.741821315418,1.17821851810457,339.775037610961));
#40796=CARTESIAN_POINT('Ctrl Pts',(137.734060060491,1.31137657905856,339.742181473265));
#40797=CARTESIAN_POINT('Ctrl Pts',(137.726298805565,1.44305359841864,339.703777291559));
#40798=CARTESIAN_POINT('Ctrl Pts',(137.718537550639,1.57276455793385,339.659999432168));
#40799=CARTESIAN_POINT('Ctrl Pts',(137.710763880234,1.70268301271159,339.61615154247));
#40800=CARTESIAN_POINT('Ctrl Pts',(137.70299020983,1.83062875790791,339.566912937929));
#40801=CARTESIAN_POINT('Ctrl Pts',(137.695216539425,1.95613681256451,339.51250615878));
#40802=CARTESIAN_POINT('Ctrl Pts',(137.687804735248,2.0758024370805,339.460632028291));
#40803=CARTESIAN_POINT('Ctrl Pts',(137.680392931071,2.19325195341466,339.404060177001));
#40804=CARTESIAN_POINT('Ctrl Pts',(137.672981126894,2.30810550760913,339.343021071587));
#40805=CARTESIAN_POINT('Ctrl Pts',(137.665206048116,2.42858837662648,339.278990257789));
#40806=CARTESIAN_POINT('Ctrl Pts',(137.657430969337,2.54659512563419,339.209840861321));
#40807=CARTESIAN_POINT('Ctrl Pts',(137.649655890559,2.66166036226265,339.13578858));
#40808=CARTESIAN_POINT('Ctrl Pts',(137.64189037951,2.77658400379202,339.061827424726));
#40809=CARTESIAN_POINT('Ctrl Pts',(137.634124868461,2.88857300959695,338.982975598673));
#40810=CARTESIAN_POINT('Ctrl Pts',(137.626359357412,2.99718528132519,338.899495281688));
#40811=CARTESIAN_POINT('Ctrl Pts',(137.618601545889,3.10568986366975,338.816097735681));
#40812=CARTESIAN_POINT('Ctrl Pts',(137.610843734367,3.21082406681668,338.7280810681));
#40813=CARTESIAN_POINT('Ctrl Pts',(137.603085922845,3.31217387582342,338.635751267457));
#40814=CARTESIAN_POINT('Ctrl Pts',(137.595333949322,3.41344741588479,338.543490947917));
#40815=CARTESIAN_POINT('Ctrl Pts',(137.587581975799,3.51094194257992,338.446924218033));
#40816=CARTESIAN_POINT('Ctrl Pts',(137.579830002276,3.60427599945385,338.346397702345));
#40817=CARTESIAN_POINT('Ctrl Pts',(137.572081311718,3.69757052929937,338.245913759696));
#40818=CARTESIAN_POINT('Ctrl Pts',(137.564332621161,3.78670782834184,338.141473652473));
#40819=CARTESIAN_POINT('Ctrl Pts',(137.556583930603,3.87134301579653,338.033461111757));
#40820=CARTESIAN_POINT('Ctrl Pts',(137.548836852225,3.95596059419359,337.925471043953));
#40821=CARTESIAN_POINT('Ctrl Pts',(137.541089773848,4.0360776832385,337.813910328561));
#40822=CARTESIAN_POINT('Ctrl Pts',(137.53334269547,4.11138971935707,337.699195739117));
#40823=CARTESIAN_POINT('Ctrl Pts',(137.525595552164,4.18670238666302,337.584480188254));
#40824=CARTESIAN_POINT('Ctrl Pts',(137.517848408858,4.25720970620255,337.466611037367));
#40825=CARTESIAN_POINT('Ctrl Pts',(137.510101265552,4.32265070859431,337.346033655767));
#40826=CARTESIAN_POINT('Ctrl Pts',(137.502352380524,4.38810642351268,337.22542916581));
#40827=CARTESIAN_POINT('Ctrl Pts',(137.494603495496,4.44849336835652,337.102115577034));
#40828=CARTESIAN_POINT('Ctrl Pts',(137.486854610468,4.50359694194783,336.976562077694));
#40829=CARTESIAN_POINT('Ctrl Pts',(137.479097500693,4.55875900304154,336.850875314573));
#40830=CARTESIAN_POINT('Ctrl Pts',(137.471340390919,4.60862633339258,336.722944250167));
#40831=CARTESIAN_POINT('Ctrl Pts',(137.463583281144,4.6530326443263,336.593257754833));
#40832=CARTESIAN_POINT('Ctrl Pts',(137.455822026218,4.69746268457272,336.463501959182));
#40833=CARTESIAN_POINT('Ctrl Pts',(137.448060771292,4.73642577966011,336.331989238043));
#40834=CARTESIAN_POINT('Ctrl Pts',(137.440299516365,4.76980608674607,336.199221813236));
#40835=CARTESIAN_POINT('Ctrl Pts',(137.432525845961,4.80323979144476,336.066242003817));
#40836=CARTESIAN_POINT('Ctrl Pts',(137.424752175556,4.83107278267786,335.932003862852));
#40837=CARTESIAN_POINT('Ctrl Pts',(137.416978505151,4.85324057139962,335.797018832036));
#40838=CARTESIAN_POINT('Ctrl Pts',(137.409566700974,4.8743764442233,335.66831738688));
#40839=CARTESIAN_POINT('Ctrl Pts',(137.402154896797,4.89036264010635,335.538937308092));
#40840=CARTESIAN_POINT('Ctrl Pts',(137.39474309262,4.90118740262167,335.409322741712));
#40841=CARTESIAN_POINT('Ctrl Pts',(137.386968013842,4.91254271899308,335.273355379333));
#40842=CARTESIAN_POINT('Ctrl Pts',(137.379192935063,4.91825373937873,335.136700280308));
#40843=CARTESIAN_POINT('Ctrl Pts',(137.371417856285,4.91824999816171,334.999865529476));
#40844=CARTESIAN_POINT('Ctrl Pts',(137.363652345236,4.91824626154849,334.863199162517));
#40845=CARTESIAN_POINT('Ctrl Pts',(137.355886834187,4.91254175575894,334.72635397076));
#40846=CARTESIAN_POINT('Ctrl Pts',(137.348121323138,4.90111770863511,334.589843604703));
#40847=CARTESIAN_POINT('Ctrl Pts',(137.340363511615,4.88970498848726,334.45346858907));
#40848=CARTESIAN_POINT('Ctrl Pts',(137.332605700093,4.87258404488704,334.317428125481));
#40849=CARTESIAN_POINT('Ctrl Pts',(137.324847888571,4.84978814286073,334.182235955873));
#40850=CARTESIAN_POINT('Ctrl Pts',(137.317095915048,4.8270093954736,334.047145522659));
#40851=CARTESIAN_POINT('Ctrl Pts',(137.309343941525,4.79856425478291,333.912902496669));
#40852=CARTESIAN_POINT('Ctrl Pts',(137.301591968002,4.76453777678333,333.7800152312));
#40853=CARTESIAN_POINT('Ctrl Pts',(137.293843277444,4.73052570901736,333.647184243566));
#40854=CARTESIAN_POINT('Ctrl Pts',(137.286094586887,4.69093710193018,333.51570825235));
#40855=CARTESIAN_POINT('Ctrl Pts',(137.278345896329,4.64590800839346,333.386084934067));
#40856=CARTESIAN_POINT('Ctrl Pts',(137.270598817951,4.60088828353574,333.256488584998));
#40857=CARTESIAN_POINT('Ctrl Pts',(137.262851739573,4.55043045191868,333.128744511146));
#40858=CARTESIAN_POINT('Ctrl Pts',(137.255104661196,4.49472017047414,333.003334366592));
#40859=CARTESIAN_POINT('Ctrl Pts',(137.24735751789,4.43900942212383,332.87792317098));
#40860=CARTESIAN_POINT('Ctrl Pts',(137.239610374584,4.3780462948272,332.754846300897));
#40861=CARTESIAN_POINT('Ctrl Pts',(137.231863231278,4.3120640836314,332.63456422595));
#40862=CARTESIAN_POINT('Ctrl Pts',(137.22411434625,4.24606703823373,332.514255109039));
#40863=CARTESIAN_POINT('Ctrl Pts',(137.216365461222,4.17504885150819,332.396742380201));
#40864=CARTESIAN_POINT('Ctrl Pts',(137.208616576194,4.09928794085967,332.282460406834));
#40865=CARTESIAN_POINT('Ctrl Pts',(137.200859466419,4.02344661679774,332.1680571334));
#40866=CARTESIAN_POINT('Ctrl Pts',(137.193102356644,3.94285272928874,332.056891791802));
#40867=CARTESIAN_POINT('Ctrl Pts',(137.18534524687,3.85782739150161,331.949368773536));
#40868=CARTESIAN_POINT('Ctrl Pts',(137.177583991943,3.77275661889258,331.841788298406));
#40869=CARTESIAN_POINT('Ctrl Pts',(137.169822737017,3.68324993243985,331.7378543209));
#40870=CARTESIAN_POINT('Ctrl Pts',(137.162061482091,3.58966697197622,331.637936036777));
#40871=CARTESIAN_POINT('Ctrl Pts',(137.154287811686,3.49593430927446,331.537857915963));
#40872=CARTESIAN_POINT('Ctrl Pts',(137.146514141282,3.3981126213039,331.441808599185));
#40873=CARTESIAN_POINT('Ctrl Pts',(137.138740470877,3.29659709157677,331.350119087106));
#40874=CARTESIAN_POINT('Ctrl Pts',(137.1313286667,3.19980713418204,331.262697743874));
#40875=CARTESIAN_POINT('Ctrl Pts',(137.123916862523,3.09965971360733,331.179239626247));
#40876=CARTESIAN_POINT('Ctrl Pts',(137.116505058346,2.99652195965593,331.099994973362));
#40877=CARTESIAN_POINT('Ctrl Pts',(137.108729979568,2.88832911715145,331.016866303982));
#40878=CARTESIAN_POINT('Ctrl Pts',(137.100954900789,2.77650348980156,330.93811186975));
#40879=CARTESIAN_POINT('Ctrl Pts',(137.093179822011,2.66143420399861,330.864065880567));
#40880=CARTESIAN_POINT('Ctrl Pts',(137.085414310962,2.54650651827747,330.790111009689));
#40881=CARTESIAN_POINT('Ctrl Pts',(137.077648799913,2.42834344165802,330.720853264873));
#40882=CARTESIAN_POINT('Ctrl Pts',(137.069883288864,2.30736675510891,330.656586397784));
#40883=CARTESIAN_POINT('Ctrl Pts',(137.062125477341,2.1865100172968,330.59238325148));
#40884=CARTESIAN_POINT('Ctrl Pts',(137.054367665819,2.06284556418658,330.533161317365));
#40885=CARTESIAN_POINT('Ctrl Pts',(137.046609854297,1.93682341394976,330.479170637408));
#40886=CARTESIAN_POINT('Ctrl Pts',(137.038857880774,1.81089609937739,330.42522058715));
#40887=CARTESIAN_POINT('Ctrl Pts',(137.031105907251,1.68261497706301,330.37649410858));
#40888=CARTESIAN_POINT('Ctrl Pts',(137.023353933728,1.55245356082002,330.333194775438));
#40889=CARTESIAN_POINT('Ctrl Pts',(137.01560524317,1.42234726801413,330.289913779589));
#40890=CARTESIAN_POINT('Ctrl Pts',(137.007856552613,1.29036263519437,330.252055480937));
#40891=CARTESIAN_POINT('Ctrl Pts',(137.000107862055,1.15699179517662,330.219774791038));
#40892=CARTESIAN_POINT('Ctrl Pts',(136.992360783677,1.02364870407606,330.187500817407));
#40893=CARTESIAN_POINT('Ctrl Pts',(136.984613705299,0.888920359115701,330.160802236169));
#40894=CARTESIAN_POINT('Ctrl Pts',(136.976866626922,0.75331226310739,330.139783575112));
#40895=CARTESIAN_POINT('Ctrl Pts',(136.969119483616,0.617703030572713,330.118764737898));
#40896=CARTESIAN_POINT('Ctrl Pts',(136.96137234031,0.481214418545881,330.103425975681));
#40897=CARTESIAN_POINT('Ctrl Pts',(136.953625197004,0.344359895081198,330.093820292207));
#40898=CARTESIAN_POINT('Ctrl Pts',(136.945876311976,0.207474603814183,330.084212449171));
#40899=CARTESIAN_POINT('Ctrl Pts',(136.938127426948,0.070223627250653,330.080340277042));
#40900=CARTESIAN_POINT('Ctrl Pts',(136.93037854192,-0.0668770981646875,
330.082204709807));
#40901=CARTESIAN_POINT('Ctrl Pts',(136.922621432145,-0.204123343706593,
330.084071121501));
#40902=CARTESIAN_POINT('Ctrl Pts',(136.914864322371,-0.341218628072329,
330.091686295898));
#40903=CARTESIAN_POINT('Ctrl Pts',(136.907107212596,-0.47764911706483,330.104999041525));
#40904=CARTESIAN_POINT('Ctrl Pts',(136.89934595767,-0.614152510148492,330.118318901059));
#40905=CARTESIAN_POINT('Ctrl Pts',(136.891584702743,-0.74999001310014,330.137342344279));
#40906=CARTESIAN_POINT('Ctrl Pts',(136.883823447817,-0.884656539578058,
330.161966735389));
#40907=CARTESIAN_POINT('Ctrl Pts',(136.876049777413,-1.01953848861058,330.1866305175));
#40908=CARTESIAN_POINT('Ctrl Pts',(136.868276107008,-1.15324533657983,330.216913065231));
#40909=CARTESIAN_POINT('Ctrl Pts',(136.860502436603,-1.28528488149189,330.252661183789));
#40910=CARTESIAN_POINT('Ctrl Pts',(136.853090632426,-1.41117795382149,330.286745218827));
#40911=CARTESIAN_POINT('Ctrl Pts',(136.845678828249,-1.53555518116635,330.325797345066));
#40912=CARTESIAN_POINT('Ctrl Pts',(136.838267024072,-1.65800745709441,330.369644253978));
#40913=CARTESIAN_POINT('Ctrl Pts',(136.830491945294,-1.78646148383199,330.415640230509));
#40914=CARTESIAN_POINT('Ctrl Pts',(136.822716866515,-1.91320303124183,330.467058242951));
#40915=CARTESIAN_POINT('Ctrl Pts',(136.814941787737,-2.03774047646905,330.523751926774));
#40916=CARTESIAN_POINT('Ctrl Pts',(136.807176276688,-2.16212467044152,330.580375845409));
#40917=CARTESIAN_POINT('Ctrl Pts',(136.799410765639,-2.2843098065612,330.642262357709));
#40918=CARTESIAN_POINT('Ctrl Pts',(136.79164525459,-2.40382061290231,330.709215744938));
#40919=CARTESIAN_POINT('Ctrl Pts',(136.783887443068,-2.5232129239311,330.776102747689));
#40920=CARTESIAN_POINT('Ctrl Pts',(136.776129631545,-2.63993584321648,330.848046437871));
#40921=CARTESIAN_POINT('Ctrl Pts',(136.768371820023,-2.75353557447544,330.924803697661));
#40922=CARTESIAN_POINT('Ctrl Pts',(136.7606198465,-2.86704981833406,331.001503195178));
#40923=CARTESIAN_POINT('Ctrl Pts',(136.752867872977,-2.97744522975045,331.083008834211));
#40924=CARTESIAN_POINT('Ctrl Pts',(136.745115899454,-3.08429437372997,331.169032592324));
#40925=CARTESIAN_POINT('Ctrl Pts',(136.737367208897,-3.19109826703358,331.255019919323));
#40926=CARTESIAN_POINT('Ctrl Pts',(136.729618518339,-3.29435857613724,331.34552131512));
#40927=CARTESIAN_POINT('Ctrl Pts',(136.721869827781,-3.39367871130215,331.440206766264));
#40928=CARTESIAN_POINT('Ctrl Pts',(136.714122749403,-3.49297818208337,331.534872517308));
#40929=CARTESIAN_POINT('Ctrl Pts',(136.706375671026,-3.58833882680404,331.633720322616));
#40930=CARTESIAN_POINT('Ctrl Pts',(136.698628592648,-3.67939918924155,331.736381660073));
#40931=CARTESIAN_POINT('Ctrl Pts',(136.690881449342,-3.77046031485257,331.83904385793));
#40932=CARTESIAN_POINT('Ctrl Pts',(136.683134306036,-3.85722082692128,331.945519359267));
#40933=CARTESIAN_POINT('Ctrl Pts',(136.67538716273,-3.93935828644084,332.05540506121));
#40934=CARTESIAN_POINT('Ctrl Pts',(136.667638277702,-4.02151421220511,332.165315467791));
#40935=CARTESIAN_POINT('Ctrl Pts',(136.659889392674,-4.09904478323544,332.27863728758));
#40936=CARTESIAN_POINT('Ctrl Pts',(136.652140507646,-4.17167001130741,332.394937164048));
#40937=CARTESIAN_POINT('Ctrl Pts',(136.644383397872,-4.2443723245468,332.511360482406));
#40938=CARTESIAN_POINT('Ctrl Pts',(136.636626288097,-4.31215868682998,332.630767839654));
#40939=CARTESIAN_POINT('Ctrl Pts',(136.628869178322,-4.37479408099023,332.752699439008));
#40940=CARTESIAN_POINT('Ctrl Pts',(136.621107923396,-4.43746294550244,332.874696194711));
#40941=CARTESIAN_POINT('Ctrl Pts',(136.61334666847,-4.49497519345254,332.999219525601));
#40942=CARTESIAN_POINT('Ctrl Pts',(136.605585413544,-4.54714380227066,333.125789151677));
#40943=CARTESIAN_POINT('Ctrl Pts',(136.597811743139,-4.59939586386118,333.252561247906));
#40944=CARTESIAN_POINT('Ctrl Pts',(136.590038072734,-4.64628707095768,333.381385813063));
#40945=CARTESIAN_POINT('Ctrl Pts',(136.58226440233,-4.68767988958946,333.511766041498));
#40946=CARTESIAN_POINT('Ctrl Pts',(136.574852598153,-4.72714586255579,333.636077038933));
#40947=CARTESIAN_POINT('Ctrl Pts',(136.567440793975,-4.76161375094119,333.761801849198));
#40948=CARTESIAN_POINT('Ctrl Pts',(136.560028989798,-4.79100790261916,333.888502658779));
#40949=CARTESIAN_POINT('Ctrl Pts',(136.549446866247,-4.83297508595386,334.069398374451));
#40950=CARTESIAN_POINT('Ctrl Pts',(136.538864742696,-4.86471113811121,334.252750046396));
#40951=CARTESIAN_POINT('Ctrl Pts',(136.528282619144,-4.88598650972011,334.437577659287));
#40952=CARTESIAN_POINT('Ctrl Pts',(136.517700495593,-4.907261881329,334.622405272178));
#40953=CARTESIAN_POINT('Ctrl Pts',(136.507118372042,-4.91807642230174,334.808709451141));
#40954=CARTESIAN_POINT('Ctrl Pts',(136.49653624849,-4.91824792654155,334.995483854551));
#40955=CARTESIAN_POINT('',(139.996536248436,-4.91824872290583,335.003544310248));
#40956=CARTESIAN_POINT('Ctrl Pts',(139.996536248436,-4.91824872290583,335.003544310248));
#40957=CARTESIAN_POINT('Ctrl Pts',(139.987647616362,-4.91813521599565,335.161051745276));
#40958=CARTESIAN_POINT('Ctrl Pts',(139.978758984289,-4.91045146808829,335.318255606896));
#40959=CARTESIAN_POINT('Ctrl Pts',(139.969870352215,-4.89530859694114,335.474485830362));
#40960=CARTESIAN_POINT('Ctrl Pts',(139.960938083389,-4.88009138525247,335.631483031193));
#40961=CARTESIAN_POINT('Ctrl Pts',(139.952005814563,-4.85734174321484,335.787496869337));
#40962=CARTESIAN_POINT('Ctrl Pts',(139.943073545737,-4.82722190234324,335.941866109401));
#40963=CARTESIAN_POINT('Ctrl Pts',(139.934085617475,-4.79691437641931,336.097197266861));
#40964=CARTESIAN_POINT('Ctrl Pts',(139.925097689213,-4.75914460223028,336.250863127016));
#40965=CARTESIAN_POINT('Ctrl Pts',(139.916109760952,-4.71412634167529,336.402211074419));
#40966=CARTESIAN_POINT('Ctrl Pts',(139.910368307663,-4.68536885356579,336.498891549057));
#40967=CARTESIAN_POINT('Ctrl Pts',(139.904626854374,-4.65365451630116,336.594626606268));
#40968=CARTESIAN_POINT('Ctrl Pts',(139.898885401086,-4.61904906007375,336.689250971032));
#40969=CARTESIAN_POINT('Ctrl Pts',(139.891110322307,-4.57218633476673,336.817391330868));
#40970=CARTESIAN_POINT('Ctrl Pts',(139.883335243529,-4.51991326629705,336.943782620743));
#40971=CARTESIAN_POINT('Ctrl Pts',(139.87556016475,-4.46237953711759,337.067934217816));
#40972=CARTESIAN_POINT('Ctrl Pts',(139.867794653701,-4.40491660685465,337.191933038445));
#40973=CARTESIAN_POINT('Ctrl Pts',(139.860029142652,-4.34220605922225,337.313697298837));
#40974=CARTESIAN_POINT('Ctrl Pts',(139.852263631603,-4.27444681928786,337.432753060132));
#40975=CARTESIAN_POINT('Ctrl Pts',(139.844505820081,-4.2067547628372,337.551690777292));
#40976=CARTESIAN_POINT('Ctrl Pts',(139.836748008559,-4.13402416799171,337.667925002101));
#40977=CARTESIAN_POINT('Ctrl Pts',(139.828990197037,-4.05650121274327,337.781003591064));
#40978=CARTESIAN_POINT('Ctrl Pts',(139.821238223514,-3.97903659597706,337.893997084804));
#40979=CARTESIAN_POINT('Ctrl Pts',(139.813486249991,-3.89678701730541,338.003839348365));
#40980=CARTESIAN_POINT('Ctrl Pts',(139.805734276467,-3.81004338021991,338.110104902305));
#40981=CARTESIAN_POINT('Ctrl Pts',(139.79798558591,-3.72333647911625,338.21632545272));
#40982=CARTESIAN_POINT('Ctrl Pts',(139.790236895352,-3.63213955166073,338.31897200405));
#40983=CARTESIAN_POINT('Ctrl Pts',(139.782488204795,-3.53678528301995,338.417650205084));
#40984=CARTESIAN_POINT('Ctrl Pts',(139.774741126417,-3.44145085363118,338.516307875295));
#40985=CARTESIAN_POINT('Ctrl Pts',(139.766994048039,-3.34196107498748,338.610998556575));
#40986=CARTESIAN_POINT('Ctrl Pts',(139.759246969661,-3.23868690268931,338.701363290579));
#40987=CARTESIAN_POINT('Ctrl Pts',(139.751499826355,-3.13541186485413,338.791728781928));
#40988=CARTESIAN_POINT('Ctrl Pts',(139.743752683049,-3.02835266426594,338.877767996294));
#40989=CARTESIAN_POINT('Ctrl Pts',(139.736005539744,-2.91791457290447,338.959161225276));
#40990=CARTESIAN_POINT('Ctrl Pts',(139.728256654715,-2.80745165271555,339.040572753185));
#40991=CARTESIAN_POINT('Ctrl Pts',(139.720507769687,-2.69360864473185,339.117335985385));
#40992=CARTESIAN_POINT('Ctrl Pts',(139.712758884659,-2.57682078711325,339.189173867674));
#40993=CARTESIAN_POINT('Ctrl Pts',(139.705001774885,-2.45990896965572,339.261087999433));
#40994=CARTESIAN_POINT('Ctrl Pts',(139.69724466511,-2.34004639215398,339.328066133112));
#40995=CARTESIAN_POINT('Ctrl Pts',(139.689487555335,-2.21769442860519,339.38987636316));
#40996=CARTESIAN_POINT('Ctrl Pts',(139.681726300409,-2.09527708407922,339.451719622619));
#40997=CARTESIAN_POINT('Ctrl Pts',(139.673965045483,-1.97036805863983,339.508389314376));
#40998=CARTESIAN_POINT('Ctrl Pts',(139.666203790557,-1.843448884797,339.559701664763));
#40999=CARTESIAN_POINT('Ctrl Pts',(139.658430120152,-1.71632668163883,339.611096098187));
#41000=CARTESIAN_POINT('Ctrl Pts',(139.650656449747,-1.58718827277892,339.657115933564));
#41001=CARTESIAN_POINT('Ctrl Pts',(139.642882779343,-1.4565313816709,339.697626996336));
#41002=CARTESIAN_POINT('Ctrl Pts',(139.635470975165,-1.33195660027659,339.736252259391));
#41003=CARTESIAN_POINT('Ctrl Pts',(139.628059170988,-1.20600180393444,339.769870000609));
#41004=CARTESIAN_POINT('Ctrl Pts',(139.620647366811,-1.07910530725297,339.798407527332));
#41005=CARTESIAN_POINT('Ctrl Pts',(139.612872288033,-0.945989235265604,
339.828343763249));
#41006=CARTESIAN_POINT('Ctrl Pts',(139.605097209254,-0.811416146393164,
339.852783804057));
#41007=CARTESIAN_POINT('Ctrl Pts',(139.597322130476,-0.675879617612291,
339.871588016756));
#41008=CARTESIAN_POINT('Ctrl Pts',(139.589556619427,-0.540509875158715,
339.890369089673));
#41009=CARTESIAN_POINT('Ctrl Pts',(139.581791108378,-0.404179435214022,
339.903528080428));
#41010=CARTESIAN_POINT('Ctrl Pts',(139.574025597329,-0.26739449284549,339.910975793841));
#41011=CARTESIAN_POINT('Ctrl Pts',(139.566267785806,-0.130745173145602,
339.918416122825));
#41012=CARTESIAN_POINT('Ctrl Pts',(139.558509974284,0.00635736439610471,
339.920156422543));
#41013=CARTESIAN_POINT('Ctrl Pts',(139.550752162762,0.143399681632911,339.916159028531));
#41014=CARTESIAN_POINT('Ctrl Pts',(139.543000189239,0.280338870180042,339.912164642685));
#41015=CARTESIAN_POINT('Ctrl Pts',(139.535248215716,0.417217539489989,339.902441168823));
#41016=CARTESIAN_POINT('Ctrl Pts',(139.527496242193,0.553520470249815,339.887002982556));
#41017=CARTESIAN_POINT('Ctrl Pts',(139.519747551635,0.689765676637587,339.871571334371));
#41018=CARTESIAN_POINT('Ctrl Pts',(139.511998861078,0.825435241844567,339.850429831255));
#41019=CARTESIAN_POINT('Ctrl Pts',(139.50425017052,0.960017512489698,339.823644829194));
#41020=CARTESIAN_POINT('Ctrl Pts',(139.496503092142,1.09457178216941,339.796865399977));
#41021=CARTESIAN_POINT('Ctrl Pts',(139.488756013764,1.22803882414136,339.764444883585));
#41022=CARTESIAN_POINT('Ctrl Pts',(139.481008935387,1.35991603731443,339.726500971539));
#41023=CARTESIAN_POINT('Ctrl Pts',(139.473261792081,1.49179435574552,339.688556741486));
#41024=CARTESIAN_POINT('Ctrl Pts',(139.465514648775,1.62208244316626,339.645089131526));
#41025=CARTESIAN_POINT('Ctrl Pts',(139.457767505469,1.75029213403813,339.596265930951));
#41026=CARTESIAN_POINT('Ctrl Pts',(139.450018620441,1.87853064917044,339.547431753885));
#41027=CARTESIAN_POINT('Ctrl Pts',(139.442269735413,2.00468947272995,339.493239729354));
#41028=CARTESIAN_POINT('Ctrl Pts',(139.434520850385,2.12830009158425,339.433905928486));
#41029=CARTESIAN_POINT('Ctrl Pts',(139.42676374061,2.25204191202657,339.374509150109));
#41030=CARTESIAN_POINT('Ctrl Pts',(139.419006630835,2.37322977195209,339.309959862869));
#41031=CARTESIAN_POINT('Ctrl Pts',(139.411249521061,2.49141898109368,339.240520548606));
#41032=CARTESIAN_POINT('Ctrl Pts',(139.403488266134,2.60967134676968,339.171044128193));
#41033=CARTESIAN_POINT('Ctrl Pts',(139.395727011208,2.72492154050674,339.096672685799));
#41034=CARTESIAN_POINT('Ctrl Pts',(139.387965756282,2.83675443823476,339.017711701909));
#41035=CARTESIAN_POINT('Ctrl Pts',(139.380192085877,2.94876623215281,338.938624406178));
#41036=CARTESIAN_POINT('Ctrl Pts',(139.372418415473,3.05734949650549,338.85493313666));
#41037=CARTESIAN_POINT('Ctrl Pts',(139.364644745068,3.16212205432583,338.766983830075));
#41038=CARTESIAN_POINT('Ctrl Pts',(139.357232940891,3.26201742437199,338.683128584872));
#41039=CARTESIAN_POINT('Ctrl Pts',(139.349821136714,3.35844866774865,338.59540299826));
#41040=CARTESIAN_POINT('Ctrl Pts',(139.342409332537,3.45111745846367,338.504136320178));
#41041=CARTESIAN_POINT('Ctrl Pts',(139.334634253759,3.54832822265841,338.408396390332));
#41042=CARTESIAN_POINT('Ctrl Pts',(139.32685917498,3.64170559457075,338.308456917359));
#41043=CARTESIAN_POINT('Ctrl Pts',(139.319084096202,3.73086505100657,338.204657397239));
#41044=CARTESIAN_POINT('Ctrl Pts',(139.311318585153,3.81991479105509,338.100985609036));
#41045=CARTESIAN_POINT('Ctrl Pts',(139.303553074104,3.90475669080866,337.993463518565));
#41046=CARTESIAN_POINT('Ctrl Pts',(139.295787563055,3.98504181294203,337.882468527426));
#41047=CARTESIAN_POINT('Ctrl Pts',(139.288029751532,4.06524733214306,337.771583588145));
#41048=CARTESIAN_POINT('Ctrl Pts',(139.28027194001,4.14090483730894,337.657232915407));
#41049=CARTESIAN_POINT('Ctrl Pts',(139.272514128488,4.21170480474704,337.539827887903));
#41050=CARTESIAN_POINT('Ctrl Pts',(139.264762154965,4.28245149296448,337.422511211405));
#41051=CARTESIAN_POINT('Ctrl Pts',(139.257010181442,4.34834771841282,337.302145088565));
#41052=CARTESIAN_POINT('Ctrl Pts',(139.249258207919,4.40912675511663,337.179170557762));
#41053=CARTESIAN_POINT('Ctrl Pts',(139.241509517361,4.46988005186227,337.056248106745));
#41054=CARTESIAN_POINT('Ctrl Pts',(139.233760826804,4.52552029730964,336.930719794544));
#41055=CARTESIAN_POINT('Ctrl Pts',(139.226012136246,4.57582640661904,336.803051790434));
#41056=CARTESIAN_POINT('Ctrl Pts',(139.218265057868,4.62612204932223,336.675410348718));
#41057=CARTESIAN_POINT('Ctrl Pts',(139.210517979491,4.67108562017492,336.545630464021));
#41058=CARTESIAN_POINT('Ctrl Pts',(139.202770901113,4.7105441021983,336.414198473958));
#41059=CARTESIAN_POINT('Ctrl Pts',(139.195023757807,4.75000291492175,336.282765382368));
#41060=CARTESIAN_POINT('Ctrl Pts',(139.187276614501,4.78395643439791,336.149680532161));
#41061=CARTESIAN_POINT('Ctrl Pts',(139.179529471195,4.81228158383889,336.015445232568));
#41062=CARTESIAN_POINT('Ctrl Pts',(139.171780586167,4.84061310137481,335.88117975403));
#41063=CARTESIAN_POINT('Ctrl Pts',(139.164031701139,4.86331365023053,335.745763693807));
#41064=CARTESIAN_POINT('Ctrl Pts',(139.156282816111,4.88031138988746,335.609707963073));
#41065=CARTESIAN_POINT('Ctrl Pts',(139.148525706336,4.8973271711209,335.473507821381));
#41066=CARTESIAN_POINT('Ctrl Pts',(139.140768596562,4.90862800314639,335.336667041378));
#41067=CARTESIAN_POINT('Ctrl Pts',(139.133011486787,4.9141939651214,335.199701616579));
#41068=CARTESIAN_POINT('Ctrl Pts',(139.125250231861,4.91976290136852,335.062663001838));
#41069=CARTESIAN_POINT('Ctrl Pts',(139.117488976935,4.91959086170075,334.925500000258));
#41070=CARTESIAN_POINT('Ctrl Pts',(139.109727722008,4.91371008371975,334.788727011545));
#41071=CARTESIAN_POINT('Ctrl Pts',(139.101954051604,4.90781989841053,334.651735230624));
#41072=CARTESIAN_POINT('Ctrl Pts',(139.094180381199,4.89620275924597,334.515135098968));
#41073=CARTESIAN_POINT('Ctrl Pts',(139.086406710795,4.87894275390741,334.379435203549));
#41074=CARTESIAN_POINT('Ctrl Pts',(139.078994906617,4.8624862059697,334.250052170908));
#41075=CARTESIAN_POINT('Ctrl Pts',(139.07158310244,4.84090036765922,334.121487732471));
#41076=CARTESIAN_POINT('Ctrl Pts',(139.064171298263,4.81430067095986,333.994170932964));
#41077=CARTESIAN_POINT('Ctrl Pts',(139.056396219485,4.78639724388913,333.860613957856));
#41078=CARTESIAN_POINT('Ctrl Pts',(139.048621140706,4.75288786288529,333.728007950344));
#41079=CARTESIAN_POINT('Ctrl Pts',(139.040846061928,4.71384992979645,333.596859984942));
#41080=CARTESIAN_POINT('Ctrl Pts',(139.033080550879,4.67486003536955,333.465873405459));
#41081=CARTESIAN_POINT('Ctrl Pts',(139.02531503983,4.63035523579267,333.336341669164));
#41082=CARTESIAN_POINT('Ctrl Pts',(139.017549528781,4.58046406611567,333.208762438557));
#41083=CARTESIAN_POINT('Ctrl Pts',(139.009791717258,4.53062236367866,333.08130970313));
#41084=CARTESIAN_POINT('Ctrl Pts',(139.002033905736,4.47540506068098,332.955805982495));
#41085=CARTESIAN_POINT('Ctrl Pts',(138.994276094214,4.41499059320829,332.832734182344));
#41086=CARTESIAN_POINT('Ctrl Pts',(138.986524120691,4.35462158953825,332.709754997625));
#41087=CARTESIAN_POINT('Ctrl Pts',(138.978772147168,4.28906337765768,332.589204440135));
#41088=CARTESIAN_POINT('Ctrl Pts',(138.971020173645,4.21854249541944,332.471545476612));
#41089=CARTESIAN_POINT('Ctrl Pts',(138.963271483087,4.14805147881671,332.35393634173));
#41090=CARTESIAN_POINT('Ctrl Pts',(138.95552279253,4.07260217250614,332.239216699756));
#41091=CARTESIAN_POINT('Ctrl Pts',(138.947774101972,3.99246694648356,332.127824736591));
#41092=CARTESIAN_POINT('Ctrl Pts',(138.940027023594,3.91234839326405,332.016455949455));
#41093=CARTESIAN_POINT('Ctrl Pts',(138.932279945216,3.82754608768726,331.908413781091));
#41094=CARTESIAN_POINT('Ctrl Pts',(138.924532866839,3.73837537201439,331.804106910359));
#41095=CARTESIAN_POINT('Ctrl Pts',(138.916785723533,3.64920390900509,331.699799165434));
#41096=CARTESIAN_POINT('Ctrl Pts',(138.909038580227,3.55566421686661,331.599227077686));
#41097=CARTESIAN_POINT('Ctrl Pts',(138.901291436921,3.4581112533133,331.502765432201));
#41098=CARTESIAN_POINT('Ctrl Pts',(138.893542551893,3.36053635778264,331.40628210009));
#41099=CARTESIAN_POINT('Ctrl Pts',(138.885793666865,3.25894667330923,331.313911323904));
#41100=CARTESIAN_POINT('Ctrl Pts',(138.878044781837,3.15373295897183,331.225989999219));
#41101=CARTESIAN_POINT('Ctrl Pts',(138.870287672062,3.04840756971094,331.137975353932));
#41102=CARTESIAN_POINT('Ctrl Pts',(138.862530562288,2.93945076708657,331.054419845207));
#41103=CARTESIAN_POINT('Ctrl Pts',(138.854773452513,2.82728568074394,330.975619458605));
#41104=CARTESIAN_POINT('Ctrl Pts',(138.847012197587,2.71506065696551,330.896776963596));
#41105=CARTESIAN_POINT('Ctrl Pts',(138.83925094266,2.59962426215665,330.822694864856));
#41106=CARTESIAN_POINT('Ctrl Pts',(138.831489687734,2.48142651161956,330.753624424296));
#41107=CARTESIAN_POINT('Ctrl Pts',(138.82371601733,2.36303968320221,330.684443493542));
#41108=CARTESIAN_POINT('Ctrl Pts',(138.815942346925,2.24188301766289,330.620290424353));
#41109=CARTESIAN_POINT('Ctrl Pts',(138.80816867652,2.11842970130722,330.561369731199));
#41110=CARTESIAN_POINT('Ctrl Pts',(138.800756872343,2.0007231665291,330.505191810486));
#41111=CARTESIAN_POINT('Ctrl Pts',(138.793345068166,1.88092925174198,330.453770207772));
#41112=CARTESIAN_POINT('Ctrl Pts',(138.785933263989,1.75947121667798,330.407240034556));
#41113=CARTESIAN_POINT('Ctrl Pts',(138.778158185211,1.63206016151062,330.358429278945));
#41114=CARTESIAN_POINT('Ctrl Pts',(138.770383106432,1.50241509194013,330.314847312727));
#41115=CARTESIAN_POINT('Ctrl Pts',(138.762608027654,1.37100430432327,330.276703454151));
#41116=CARTESIAN_POINT('Ctrl Pts',(138.754842516605,1.23975522604655,330.238606534022));
#41117=CARTESIAN_POINT('Ctrl Pts',(138.747077005556,1.10674512482111,330.205934514415));
#41118=CARTESIAN_POINT('Ctrl Pts',(138.739311494507,0.972462053353817,330.178848621202));
#41119=CARTESIAN_POINT('Ctrl Pts',(138.731553682985,0.838312123942887,330.151789583731));
#41120=CARTESIAN_POINT('Ctrl Pts',(138.723795871462,0.702892116736589,330.130305727194));
#41121=CARTESIAN_POINT('Ctrl Pts',(138.71603805994,0.566704679436738,330.114508328857));
#41122=CARTESIAN_POINT('Ctrl Pts',(138.708286086417,0.430619727502208,330.098722818564));
#41123=CARTESIAN_POINT('Ctrl Pts',(138.700534112894,0.293768881697937,330.08861529371));
#41124=CARTESIAN_POINT('Ctrl Pts',(138.692782139371,0.156664053261195,330.084245791649));
#41125=CARTESIAN_POINT('Ctrl Pts',(138.685033448814,0.0196172888007414,
330.079878140075));
#41126=CARTESIAN_POINT('Ctrl Pts',(138.677284758256,-0.117682854496473,
330.081243690508));
#41127=CARTESIAN_POINT('Ctrl Pts',(138.669536067698,-0.254720501724082,
330.088350528743));
#41128=CARTESIAN_POINT('Ctrl Pts',(138.66178898932,-0.391729637124671,330.09545588834));
#41129=CARTESIAN_POINT('Ctrl Pts',(138.654041910943,-0.528475994983113,
330.108300139518));
#41130=CARTESIAN_POINT('Ctrl Pts',(138.646294832565,-0.664445258736857,
330.12683926382));
#41131=CARTESIAN_POINT('Ctrl Pts',(138.638547689259,-0.800415662043992,
330.145378543499));
#41132=CARTESIAN_POINT('Ctrl Pts',(138.630800545953,-0.935608570965312,
330.169612738694));
#41133=CARTESIAN_POINT('Ctrl Pts',(138.623053402647,-1.0695167327395,330.199446175607));
#41134=CARTESIAN_POINT('Ctrl Pts',(138.615304517619,-1.2034549999114,330.229286319711));
#41135=CARTESIAN_POINT('Ctrl Pts',(138.607555632591,-1.33610756373403,330.264728125477));
#41136=CARTESIAN_POINT('Ctrl Pts',(138.599806747563,-1.46697965937024,330.305625308788));
#41137=CARTESIAN_POINT('Ctrl Pts',(138.592049637788,-1.59799066400087,330.346565900792));
#41138=CARTESIAN_POINT('Ctrl Pts',(138.584292528014,-1.72721705170641,330.392973320425));
#41139=CARTESIAN_POINT('Ctrl Pts',(138.576535418239,-1.85418094218393,330.444651923712));
#41140=CARTESIAN_POINT('Ctrl Pts',(138.568774163313,-1.98121267810497,330.496358142392));
#41141=CARTESIAN_POINT('Ctrl Pts',(138.561012908387,-2.10597915237709,330.553340995057));
#41142=CARTESIAN_POINT('Ctrl Pts',(138.553251653461,-2.22802554439818,330.615358026474));
#41143=CARTESIAN_POINT('Ctrl Pts',(138.545477983056,-2.35026717087167,330.67747426493));
#41144=CARTESIAN_POINT('Ctrl Pts',(138.537704312651,-2.46977967908966,330.744640582905));
#41145=CARTESIAN_POINT('Ctrl Pts',(138.529930642247,-2.5861350202107,330.816569742455));
#41146=CARTESIAN_POINT('Ctrl Pts',(138.52251883807,-2.69707399220891,330.885150582323));
#41147=CARTESIAN_POINT('Ctrl Pts',(138.515107033892,-2.80514287602787,330.958060661159));
#41148=CARTESIAN_POINT('Ctrl Pts',(138.507695229715,-2.90999900339613,331.03501716741));
#41149=CARTESIAN_POINT('Ctrl Pts',(138.499989985559,-3.01900647894815,331.115020450807));
#41150=CARTESIAN_POINT('Ctrl Pts',(138.492284741403,-3.12489967861004,331.199660154725));
#41151=CARTESIAN_POINT('Ctrl Pts',(138.484579497247,-3.22725339229766,331.288663501594));
#41152=CARTESIAN_POINT('Ctrl Pts',(138.47688376838,-3.32948070828308,331.377556937271));
#41153=CARTESIAN_POINT('Ctrl Pts',(138.469188039513,-3.42817693442612,331.470803038781));
#41154=CARTESIAN_POINT('Ctrl Pts',(138.461492310646,-3.52294624608198,331.568086130201));
#41155=CARTESIAN_POINT('Ctrl Pts',(138.453804161778,-3.6176222135787,331.665273401485));
#41156=CARTESIAN_POINT('Ctrl Pts',(138.446116012911,-3.70837868497844,331.766489468646));
#41157=CARTESIAN_POINT('Ctrl Pts',(138.438427864043,-3.79485368309668,331.871379123897));
#41158=CARTESIAN_POINT('Ctrl Pts',(138.430432380063,-3.88478553457888,331.980461761692));
#41159=CARTESIAN_POINT('Ctrl Pts',(138.422436896083,-3.97008616230015,332.093517512434));
#41160=CARTESIAN_POINT('Ctrl Pts',(138.414441412103,-4.05039117206293,332.210104945383));
#41161=CARTESIAN_POINT('Ctrl Pts',(138.406762059569,-4.12752102208044,332.322082656909));
#41162=CARTESIAN_POINT('Ctrl Pts',(138.399082707035,-4.20004250895292,332.437317741729));
#41163=CARTESIAN_POINT('Ctrl Pts',(138.391403354502,-4.26767479704982,332.555386556299));
#41164=CARTESIAN_POINT('Ctrl Pts',(138.383725265561,-4.33529595664338,332.673435943325));
#41165=CARTESIAN_POINT('Ctrl Pts',(138.37604717662,-4.39802931932651,332.794317787035));
#41166=CARTESIAN_POINT('Ctrl Pts',(138.36836908768,-4.45563881475275,332.917581738706));
#41167=CARTESIAN_POINT('Ctrl Pts',(138.360690526208,-4.51325185562625,333.040853276381));
#41168=CARTESIAN_POINT('Ctrl Pts',(138.353011964737,-4.56574023362412,333.166506852295));
#41169=CARTESIAN_POINT('Ctrl Pts',(138.345333403266,-4.61291526543899,333.294070395245));
#41170=CARTESIAN_POINT('Ctrl Pts',(138.337652633093,-4.66010386692659,333.421670631239));
#41171=CARTESIAN_POINT('Ctrl Pts',(138.32997186292,-4.70197594459933,333.551181553172));
#41172=CARTESIAN_POINT('Ctrl Pts',(138.322291092747,-4.73839225483785,333.682114609766));
#41173=CARTESIAN_POINT('Ctrl Pts',(138.314602413885,-4.77484606200135,333.813182484714));
#41174=CARTESIAN_POINT('Ctrl Pts',(138.306913735024,-4.80583278181753,333.945675033012));
#41175=CARTESIAN_POINT('Ctrl Pts',(138.299225056162,-4.83126394489471,334.079091884464));
#41176=CARTESIAN_POINT('Ctrl Pts',(138.29153168722,-4.8567106209356,334.212590119955));
#41177=CARTESIAN_POINT('Ctrl Pts',(138.283838318278,-4.87659493447119,334.347013388021));
#41178=CARTESIAN_POINT('Ctrl Pts',(138.276144949336,-4.89088027700115,334.481856025278));
#41179=CARTESIAN_POINT('Ctrl Pts',(138.268441174777,-4.90518494107916,334.616881043074));
#41180=CARTESIAN_POINT('Ctrl Pts',(138.260737400219,-4.91387549554807,334.752326166009));
#41181=CARTESIAN_POINT('Ctrl Pts',(138.25303362566,-4.91696740557989,334.887685286071));
#41182=CARTESIAN_POINT('Ctrl Pts',(138.250867833281,-4.91783664638312,334.925739326789));
#41183=CARTESIAN_POINT('Ctrl Pts',(138.248702040901,-4.91826370620767,334.963786600083));
#41184=CARTESIAN_POINT('Ctrl Pts',(138.246536248522,-4.91824966475132,335.001815949749));
#41185=CARTESIAN_POINT('',(141.746536248545,-4.91824882895472,334.996606036901));
#41186=CARTESIAN_POINT('Ctrl Pts',(141.74653624849,-4.91824882895539,334.996606037877));
#41187=CARTESIAN_POINT('Ctrl Pts',(141.738756538685,-4.91834398132713,335.134492974708));
#41188=CARTESIAN_POINT('Ctrl Pts',(141.730976828881,-4.91263616094097,335.272420682955));
#41189=CARTESIAN_POINT('Ctrl Pts',(141.723197119076,-4.90114179516215,335.409868474288));
#41190=CARTESIAN_POINT('Ctrl Pts',(141.715417497372,-4.88964755954944,335.547314709114));
#41191=CARTESIAN_POINT('Ctrl Pts',(141.707637875667,-4.87236694027544,335.684280653093));
#41192=CARTESIAN_POINT('Ctrl Pts',(141.699858253963,-4.84936833957404,335.820249821479));
#41193=CARTESIAN_POINT('Ctrl Pts',(141.692077090379,-4.82636518067306,335.956245938228));
#41194=CARTESIAN_POINT('Ctrl Pts',(141.684295926795,-4.7976418484734,336.091244505456));
#41195=CARTESIAN_POINT('Ctrl Pts',(141.676514763211,-4.76331799226883,336.224738652541));
#41196=CARTESIAN_POINT('Ctrl Pts',(141.668730427127,-4.72898014169905,336.358287227248));
#41197=CARTESIAN_POINT('Ctrl Pts',(141.660946091043,-4.68903731748926,336.490329787161));
#41198=CARTESIAN_POINT('Ctrl Pts',(141.653161754958,-4.64365911135693,336.620374376498));
#41199=CARTESIAN_POINT('Ctrl Pts',(141.645367727005,-4.59822440719476,336.750580877548));
#41200=CARTESIAN_POINT('Ctrl Pts',(141.637573699051,-4.54734093321821,336.878784075261));
#41201=CARTESIAN_POINT('Ctrl Pts',(141.629779671097,-4.49122678197054,337.004511176175));
#41202=CARTESIAN_POINT('Ctrl Pts',(141.621980325694,-4.43507434702874,337.130324053988));
#41203=CARTESIAN_POINT('Ctrl Pts',(141.61418098029,-4.37368429609552,337.253657124271));
#41204=CARTESIAN_POINT('Ctrl Pts',(141.606381634887,-4.30732038762834,337.374062792097));
#41205=CARTESIAN_POINT('Ctrl Pts',(141.598569673064,-4.24084912721982,337.494663231185));
#41206=CARTESIAN_POINT('Ctrl Pts',(141.590757711242,-4.16938813773808,337.612326479504));
#41207=CARTESIAN_POINT('Ctrl Pts',(141.582945749419,-4.0932445566266,337.726633833529));
#41208=CARTESIAN_POINT('Ctrl Pts',(141.578068368523,-4.04570448201125,337.798001374432));
#41209=CARTESIAN_POINT('Ctrl Pts',(141.573190987626,-3.99633990974758,337.868061389034));
#41210=CARTESIAN_POINT('Ctrl Pts',(141.568313606729,-3.94523323621345,337.936718879017));
#41211=CARTESIAN_POINT('Ctrl Pts',(141.560538527951,-3.86376360707521,338.046166429791));
#41212=CARTESIAN_POINT('Ctrl Pts',(141.552763449172,-3.77760739456703,338.15239419871));
#41213=CARTESIAN_POINT('Ctrl Pts',(141.544988370394,-3.68704801975687,338.25497464852));
#41214=CARTESIAN_POINT('Ctrl Pts',(141.537222859345,-3.59660008402268,338.357428866555));
#41215=CARTESIAN_POINT('Ctrl Pts',(141.529457348296,-3.501760023206,338.456244405604));
#41216=CARTESIAN_POINT('Ctrl Pts',(141.521691837247,-3.40285369549707,338.551023766401));
#41217=CARTESIAN_POINT('Ctrl Pts',(141.513934025724,-3.30404543369986,338.645709153185));
#41218=CARTESIAN_POINT('Ctrl Pts',(141.506176214202,-3.20117920874914,338.736366056992));
#41219=CARTESIAN_POINT('Ctrl Pts',(141.49841840268,-3.09461995083519,338.822631347958));
#41220=CARTESIAN_POINT('Ctrl Pts',(141.490666429157,-2.98814088214216,338.908831721557));
#41221=CARTESIAN_POINT('Ctrl Pts',(141.482914455634,-2.87797461477476,338.99064681546));
#41222=CARTESIAN_POINT('Ctrl Pts',(141.475162482111,-2.76452133964631,339.067751814595));
#41223=CARTESIAN_POINT('Ctrl Pts',(141.467413791553,-2.65111611204728,339.144824159717));
#41224=CARTESIAN_POINT('Ctrl Pts',(141.459665100996,-2.5344269679848,339.217190158193));
#41225=CARTESIAN_POINT('Ctrl Pts',(141.451916410438,-2.41488526411081,339.284566748655));
#41226=CARTESIAN_POINT('Ctrl Pts',(141.44416933206,-2.29536843188661,339.351929320855));
#41227=CARTESIAN_POINT('Ctrl Pts',(141.436422253683,-2.17300056066116,339.414304358071));
#41228=CARTESIAN_POINT('Ctrl Pts',(141.428675175305,-2.04823959092459,339.471453638434));
#41229=CARTESIAN_POINT('Ctrl Pts',(141.420928031999,-1.92347757557131,339.528603397764));
#41230=CARTESIAN_POINT('Ctrl Pts',(141.413180888693,-1.79632277706827,339.580527150103));
#41231=CARTESIAN_POINT('Ctrl Pts',(141.405433745387,-1.66725482969334,339.627034081932));
#41232=CARTESIAN_POINT('Ctrl Pts',(141.397684860359,-1.53815786510339,339.673551469507));
#41233=CARTESIAN_POINT('Ctrl Pts',(141.389935975331,-1.40714726341605,339.714649480776));
#41234=CARTESIAN_POINT('Ctrl Pts',(141.382187090303,-1.27471921213646,339.750186732404));
#41235=CARTESIAN_POINT('Ctrl Pts',(141.374429980528,-1.14215060035509,339.785761703639));
#41236=CARTESIAN_POINT('Ctrl Pts',(141.366672870753,-1.00816191172415,339.815764023472));
#41237=CARTESIAN_POINT('Ctrl Pts',(141.358915760979,-0.873261504206372,
339.840103036896));
#41238=CARTESIAN_POINT('Ctrl Pts',(141.351154506053,-0.738289010224137,
339.86445505631));
#41239=CARTESIAN_POINT('Ctrl Pts',(141.343393251126,-0.602404213613322,
339.883137685947));
#41240=CARTESIAN_POINT('Ctrl Pts',(141.3356319962,-0.466121062823814,339.896112153259));
#41241=CARTESIAN_POINT('Ctrl Pts',(141.327858325796,-0.329619903407525,
339.909107375491));
#41242=CARTESIAN_POINT('Ctrl Pts',(141.320084655391,-0.192719506954368,
339.916376167823));
#41243=CARTESIAN_POINT('Ctrl Pts',(141.312310984986,-0.0559351911396397,
339.917931914626));
#41244=CARTESIAN_POINT('Ctrl Pts',(141.304899180809,0.0744817818656994,
339.91941524104));
#41245=CARTESIAN_POINT('Ctrl Pts',(141.297487376632,0.204792950453107,339.915705444923));
#41246=CARTESIAN_POINT('Ctrl Pts',(141.290075572455,0.334557475968693,339.906857890522));
#41247=CARTESIAN_POINT('Ctrl Pts',(141.282300493676,0.470682147428127,339.897576691123));
#41248=CARTESIAN_POINT('Ctrl Pts',(141.274525414898,0.606635414813306,339.882612035073));
#41249=CARTESIAN_POINT('Ctrl Pts',(141.26675033612,0.741904377521809,339.861970892253));
#41250=CARTESIAN_POINT('Ctrl Pts',(141.258984825071,0.877006883160056,339.841355149673));
#41251=CARTESIAN_POINT('Ctrl Pts',(141.251219314022,1.01142637691261,339.815076877422));
#41252=CARTESIAN_POINT('Ctrl Pts',(141.243453802973,1.14465225260247,339.783194986943));
#41253=CARTESIAN_POINT('Ctrl Pts',(141.23569599145,1.2777460344488,339.751344707451));
#41254=CARTESIAN_POINT('Ctrl Pts',(141.227938179928,1.40964817572406,339.713901956877));
#41255=CARTESIAN_POINT('Ctrl Pts',(141.220180368406,1.53985582811249,339.670977102398));
#41256=CARTESIAN_POINT('Ctrl Pts',(141.212428394883,1.66996549511275,339.628084550234));
#41257=CARTESIAN_POINT('Ctrl Pts',(141.20467642136,1.79838284163539,339.57971822757));
#41258=CARTESIAN_POINT('Ctrl Pts',(141.196924447837,1.92461815748993,339.526038887411));
#41259=CARTESIAN_POINT('Ctrl Pts',(141.189175757279,2.05080001261378,339.472382280485));
#41260=CARTESIAN_POINT('Ctrl Pts',(141.181427066722,2.17480131606695,339.413417283924));
#41261=CARTESIAN_POINT('Ctrl Pts',(141.173678376164,2.29615060367084,339.349353453993));
#41262=CARTESIAN_POINT('Ctrl Pts',(141.165931297786,2.41747464354182,339.285302953077));
#41263=CARTESIAN_POINT('Ctrl Pts',(141.158184219408,2.53614741963648,339.216155911276));
#41264=CARTESIAN_POINT('Ctrl Pts',(141.150437141031,2.651720788228,339.142168504996));
#41265=CARTESIAN_POINT('Ctrl Pts',(141.142689997725,2.7672951254357,339.06818047863));
#41266=CARTESIAN_POINT('Ctrl Pts',(141.134942854419,2.87976967413334,338.989352217615));
#41267=CARTESIAN_POINT('Ctrl Pts',(141.127195711113,2.98872441753231,338.905983796503));
#41268=CARTESIAN_POINT('Ctrl Pts',(141.119446826085,3.0977036562707,338.822596632401));
#41269=CARTESIAN_POINT('Ctrl Pts',(141.111697941057,3.20316120469366,338.734667514554));
#41270=CARTESIAN_POINT('Ctrl Pts',(141.103949056029,3.30470965500933,338.642537186988));
#41271=CARTESIAN_POINT('Ctrl Pts',(141.096191946254,3.40636588989946,338.55030907134));
#41272=CARTESIAN_POINT('Ctrl Pts',(141.088434836479,3.5041044484065,338.453871101341));
#41273=CARTESIAN_POINT('Ctrl Pts',(141.080677726705,3.5975739951362,338.353601707421));
#41274=CARTESIAN_POINT('Ctrl Pts',(141.072916471778,3.69109348900298,338.253278732743));
#41275=CARTESIAN_POINT('Ctrl Pts',(141.065155216852,3.78033917135454,338.149120551204));
#41276=CARTESIAN_POINT('Ctrl Pts',(141.057393961926,3.86500031053346,338.041538370969));
#41277=CARTESIAN_POINT('Ctrl Pts',(141.049620291521,3.94979687994415,337.933784094307));
#41278=CARTESIAN_POINT('Ctrl Pts',(141.041846621117,4.02999402235305,337.822595190901));
#41279=CARTESIAN_POINT('Ctrl Pts',(141.034072950712,4.10532412499918,337.708412245431));
#41280=CARTESIAN_POINT('Ctrl Pts',(141.026661146535,4.17714759324341,337.599544543543));
#41281=CARTESIAN_POINT('Ctrl Pts',(141.019249342358,4.24454679711922,337.487955518265));
#41282=CARTESIAN_POINT('Ctrl Pts',(141.011837538181,4.30732973051173,337.374045840996));
#41283=CARTESIAN_POINT('Ctrl Pts',(141.004062459403,4.37318984249072,337.254553111124));
#41284=CARTESIAN_POINT('Ctrl Pts',(140.996287380624,4.43417785794029,337.132128874084));
#41285=CARTESIAN_POINT('Ctrl Pts',(140.988512301846,4.49002207803601,337.007208210737));
#41286=CARTESIAN_POINT('Ctrl Pts',(140.980746790797,4.5457975782636,336.882441270219));
#41287=CARTESIAN_POINT('Ctrl Pts',(140.972981279748,4.59644171956362,336.755184369247));
#41288=CARTESIAN_POINT('Ctrl Pts',(140.965215768699,4.6417277235244,336.62589876781));
#41289=CARTESIAN_POINT('Ctrl Pts',(140.957457957177,4.68696882628041,336.496741353423));
#41290=CARTESIAN_POINT('Ctrl Pts',(140.949700145654,4.7268622357043,336.365559608016));
#41291=CARTESIAN_POINT('Ctrl Pts',(140.941942334132,4.7612286418322,336.232836113478));
#41292=CARTESIAN_POINT('Ctrl Pts',(140.934190360609,4.7955691861499,336.100212497579));
#41293=CARTESIAN_POINT('Ctrl Pts',(140.926438387086,4.82439090836163,335.966049818771));
#41294=CARTESIAN_POINT('Ctrl Pts',(140.918686413563,4.84756397881346,335.830846877475));
#41295=CARTESIAN_POINT('Ctrl Pts',(140.910937723005,4.87072723545608,335.695701194706));
#41296=CARTESIAN_POINT('Ctrl Pts',(140.903189032448,4.88824653237722,335.559516510131));
#41297=CARTESIAN_POINT('Ctrl Pts',(140.89544034189,4.90004295358947,335.422802690954));
#41298=CARTESIAN_POINT('Ctrl Pts',(140.887693263512,4.91183692045776,335.286117316229));
#41299=CARTESIAN_POINT('Ctrl Pts',(140.879946185135,4.9179103464071,335.148903415064));
#41300=CARTESIAN_POINT('Ctrl Pts',(140.872199106757,4.91823613935751,335.011676472831));
#41301=CARTESIAN_POINT('Ctrl Pts',(140.864451963451,4.91856193503837,334.874448380504));
#41302=CARTESIAN_POINT('Ctrl Pts',(140.856704820145,4.91314000071226,334.737207637765));
#41303=CARTESIAN_POINT('Ctrl Pts',(140.848957676839,4.90199538028729,334.600469833252));
#41304=CARTESIAN_POINT('Ctrl Pts',(140.841208791811,4.89084825431497,334.463701287175));
#41305=CARTESIAN_POINT('Ctrl Pts',(140.833459906783,4.87397591383677,334.327436293829));
#41306=CARTESIAN_POINT('Ctrl Pts',(140.825711021755,4.85145524918657,334.192185028834));
#41307=CARTESIAN_POINT('Ctrl Pts',(140.81795391198,4.82891068087031,334.056790206749));
#41308=CARTESIAN_POINT('Ctrl Pts',(140.810196802205,4.80070587673029,333.922411648564));
#41309=CARTESIAN_POINT('Ctrl Pts',(140.802439692431,4.7669689392463,333.789549590127));
#41310=CARTESIAN_POINT('Ctrl Pts',(140.794678437505,4.73321397382166,333.656616534455));
#41311=CARTESIAN_POINT('Ctrl Pts',(140.786917182578,4.69392109648418,333.525201967566));
#41312=CARTESIAN_POINT('Ctrl Pts',(140.779155927652,4.64926794622451,333.395789718675));
#41313=CARTESIAN_POINT('Ctrl Pts',(140.771382257248,4.60454336547684,333.266170452361));
#41314=CARTESIAN_POINT('Ctrl Pts',(140.763608586843,4.55444151996085,333.138560268728));
#41315=CARTESIAN_POINT('Ctrl Pts',(140.755834916438,4.49918808611068,333.013422634706));
#41316=CARTESIAN_POINT('Ctrl Pts',(140.748423112261,4.44650671289935,332.894110187653));
#41317=CARTESIAN_POINT('Ctrl Pts',(140.741011308084,4.38914269747793,332.77704553466));
#41318=CARTESIAN_POINT('Ctrl Pts',(140.733599503907,4.32732906744816,332.662606964048));
#41319=CARTESIAN_POINT('Ctrl Pts',(140.725824425129,4.26248576727736,332.542559418195));
#41320=CARTESIAN_POINT('Ctrl Pts',(140.71804934635,4.19254072919499,332.425022515518));
#41321=CARTESIAN_POINT('Ctrl Pts',(140.710274267572,4.11771279015552,332.310460180572));
#41322=CARTESIAN_POINT('Ctrl Pts',(140.702508756523,4.04297693165904,332.196038821873));
#41323=CARTESIAN_POINT('Ctrl Pts',(140.694743245474,3.9633703395422,332.084585071893));
#41324=CARTESIAN_POINT('Ctrl Pts',(140.686977734425,3.87915817435981,331.976539247684));
#41325=CARTESIAN_POINT('Ctrl Pts',(140.679219922903,3.79502950578445,331.868600551224));
#41326=CARTESIAN_POINT('Ctrl Pts',(140.67146211138,3.706304590355,331.764063362504));
#41327=CARTESIAN_POINT('Ctrl Pts',(140.663704299858,3.61329220656668,331.66333961985));
#41328=CARTESIAN_POINT('Ctrl Pts',(140.655952326335,3.52034981754666,331.562691675005));
#41329=CARTESIAN_POINT('Ctrl Pts',(140.648200352812,3.42312664638137,331.465851750158));
#41330=CARTESIAN_POINT('Ctrl Pts',(140.640448379289,3.32197188671056,331.373198951362));
#41331=CARTESIAN_POINT('Ctrl Pts',(140.632699688732,3.22085996614025,331.28058539108));
#41332=CARTESIAN_POINT('Ctrl Pts',(140.624950998174,3.11582005632932,331.192155693442));
#41333=CARTESIAN_POINT('Ctrl Pts',(140.617202307616,3.00723820951844,331.108252138985));
#41334=CARTESIAN_POINT('Ctrl Pts',(140.609455229239,2.89867895406761,331.024366041364));
#41335=CARTESIAN_POINT('Ctrl Pts',(140.601708150861,2.78657953652146,330.945004452659));
#41336=CARTESIAN_POINT('Ctrl Pts',(140.593961072483,2.67135877844877,330.870469113894));
#41337=CARTESIAN_POINT('Ctrl Pts',(140.586213929177,2.55613705471535,330.795933150451));
#41338=CARTESIAN_POINT('Ctrl Pts',(140.578466785871,2.43779426646905,330.726223729929));
#41339=CARTESIAN_POINT('Ctrl Pts',(140.570719642565,2.31677753588989,330.661598806969));
#41340=CARTESIAN_POINT('Ctrl Pts',(140.562970757537,2.1957335981806,330.596959354953));
#41341=CARTESIAN_POINT('Ctrl Pts',(140.555221872509,2.07201486662305,330.537406859234));
#41342=CARTESIAN_POINT('Ctrl Pts',(140.547472987481,1.94609196855235,330.483152746391));
#41343=CARTESIAN_POINT('Ctrl Pts',(140.539715877706,1.82003541461648,330.428841047672));
#41344=CARTESIAN_POINT('Ctrl Pts',(140.531958767932,1.69177038028666,330.379839120722));
#41345=CARTESIAN_POINT('Ctrl Pts',(140.524201658157,1.56178684816186,330.336309947755));
#41346=CARTESIAN_POINT('Ctrl Pts',(140.516440403231,1.43173385699337,330.292757514189));
#41347=CARTESIAN_POINT('Ctrl Pts',(140.508679148305,1.29996091353737,330.254683770309));
#41348=CARTESIAN_POINT('Ctrl Pts',(140.500917893378,1.16697101075282,330.222201163447));
#41349=CARTESIAN_POINT('Ctrl Pts',(140.493144222974,1.03376836746512,330.189666595001));
#41350=CARTESIAN_POINT('Ctrl Pts',(140.485370552569,0.899345258152152,330.162741113136));
#41351=CARTESIAN_POINT('Ctrl Pts',(140.477596882164,0.764213548510509,330.141485750276));
#41352=CARTESIAN_POINT('Ctrl Pts',(140.470185077987,0.635372252462299,330.12121982967));
#41353=CARTESIAN_POINT('Ctrl Pts',(140.46277327381,0.505887128002858,330.106108053142));
#41354=CARTESIAN_POINT('Ctrl Pts',(140.455361469633,0.37620239045995,330.096159176328));
#41355=CARTESIAN_POINT('Ctrl Pts',(140.447586390855,0.240161417620565,330.085722675425));
#41356=CARTESIAN_POINT('Ctrl Pts',(140.439811312076,0.10347085506739,330.080934987856));
#41357=CARTESIAN_POINT('Ctrl Pts',(140.432036233298,-0.0333607479093066,
330.081863145154));
#41358=CARTESIAN_POINT('Ctrl Pts',(140.424270722249,-0.170023970887461,
330.082790160295));
#41359=CARTESIAN_POINT('Ctrl Pts',(140.4165052112,-0.306827501827269,330.089419022609));
#41360=CARTESIAN_POINT('Ctrl Pts',(140.408739700151,-0.443257575134837,
330.101765033751));
#41361=CARTESIAN_POINT('Ctrl Pts',(140.400981888628,-0.579552377627468,
330.114098803787));
#41362=CARTESIAN_POINT('Ctrl Pts',(140.393224077106,-0.715474072598671,
330.132138406876));
#41363=CARTESIAN_POINT('Ctrl Pts',(140.385466265584,-0.850509154561626,
330.155847108058));
#41364=CARTESIAN_POINT('Ctrl Pts',(140.377714292061,-0.985442618342828,
330.179537967691));
#41365=CARTESIAN_POINT('Ctrl Pts',(140.369962318538,-1.11949041371819,330.208889366481));
#41366=CARTESIAN_POINT('Ctrl Pts',(140.362210345015,-1.25214477360342,330.243812816085));
#41367=CARTESIAN_POINT('Ctrl Pts',(140.354461654457,-1.38474295428892,330.278721475588));
#41368=CARTESIAN_POINT('Ctrl Pts',(140.3467129639,-1.51594849598507,330.319197393189));
#41369=CARTESIAN_POINT('Ctrl Pts',(140.338964273342,-1.64526465266629,330.365101156963));
#41370=CARTESIAN_POINT('Ctrl Pts',(140.331217194964,-1.77455390404073,330.410995370075));
#41371=CARTESIAN_POINT('Ctrl Pts',(140.323470116586,-1.90195418418469,330.462315052411));
#41372=CARTESIAN_POINT('Ctrl Pts',(140.315723038209,-2.02698510425249,330.518871297358));
#41373=CARTESIAN_POINT('Ctrl Pts',(140.307975894903,-2.15201707220025,330.575428016302));
#41374=CARTESIAN_POINT('Ctrl Pts',(140.300228751597,-2.27467928433013,330.637221224301));
#41375=CARTESIAN_POINT('Ctrl Pts',(140.292481608291,-2.3945128576153,330.704014520833));
#41376=CARTESIAN_POINT('Ctrl Pts',(140.284732723263,-2.51437337203151,330.770822833915));
#41377=CARTESIAN_POINT('Ctrl Pts',(140.276983838235,-2.63140364080378,330.84263328215));
#41378=CARTESIAN_POINT('Ctrl Pts',(140.269234953207,-2.74517118735471,330.919164520026));
#41379=CARTESIAN_POINT('Ctrl Pts',(140.261477843432,-2.85905948795526,330.995776988948));
#41380=CARTESIAN_POINT('Ctrl Pts',(140.253720733657,-2.9696778236595,331.077120038328));
#41381=CARTESIAN_POINT('Ctrl Pts',(140.245963623883,-3.07662398154829,331.162869830373));
#41382=CARTESIAN_POINT('Ctrl Pts',(140.238202368957,-3.18362728804423,331.248665444365));
#41383=CARTESIAN_POINT('Ctrl Pts',(140.23044111403,-3.28695421237456,331.338872236285));
#41384=CARTESIAN_POINT('Ctrl Pts',(140.222679859104,-3.38623799682626,331.433128080327));
#41385=CARTESIAN_POINT('Ctrl Pts',(140.2149061887,-3.48568060297654,331.527534703002));
#41386=CARTESIAN_POINT('Ctrl Pts',(140.207132518295,-3.5810668727517,331.626003040194));
#41387=CARTESIAN_POINT('Ctrl Pts',(140.19935884789,-3.67206848278731,331.728135681264));
#41388=CARTESIAN_POINT('Ctrl Pts',(140.191947043713,-3.75883394598241,331.82551402332));
#41389=CARTESIAN_POINT('Ctrl Pts',(140.184535239536,-3.84161359195973,331.926222977529));
#41390=CARTESIAN_POINT('Ctrl Pts',(140.177123435359,-3.9201596675152,332.02989373192));
#41391=CARTESIAN_POINT('Ctrl Pts',(140.169326540512,-4.00278671446171,332.138950845589));
#41392=CARTESIAN_POINT('Ctrl Pts',(140.161529645666,-4.0809922521438,332.25163379844));
#41393=CARTESIAN_POINT('Ctrl Pts',(140.15373275082,-4.15444223853103,332.367550048109));
#41394=CARTESIAN_POINT('Ctrl Pts',(140.145945417238,-4.22780215383955,332.483324150692));
#41395=CARTESIAN_POINT('Ctrl Pts',(140.138158083656,-4.29641791378443,332.602323338621));
#41396=CARTESIAN_POINT('Ctrl Pts',(140.130370750073,-4.3599959443122,332.724122492734));
#41397=CARTESIAN_POINT('Ctrl Pts',(140.122591313883,-4.42350949825989,332.845798126302));
#41398=CARTESIAN_POINT('Ctrl Pts',(140.114811877693,-4.48199531007374,332.970267735069));
#41399=CARTESIAN_POINT('Ctrl Pts',(140.107032441503,-4.5352035263831,333.097078026617));
#41400=CARTESIAN_POINT('Ctrl Pts',(140.0992592446,-4.58836906848031,333.223786613398));
#41401=CARTESIAN_POINT('Ctrl Pts',(140.091486047697,-4.63626528978345,333.352831791015));
#41402=CARTESIAN_POINT('Ctrl Pts',(140.083712850793,-4.67868881687082,333.483736824496));
#41403=CARTESIAN_POINT('Ctrl Pts',(140.075944143033,-4.72108784370571,333.614566258267));
#41404=CARTESIAN_POINT('Ctrl Pts',(140.068175435273,-4.75802034867188,333.747253041976));
#41405=CARTESIAN_POINT('Ctrl Pts',(140.060406727513,-4.78933166584142,333.881301981289));
#41406=CARTESIAN_POINT('Ctrl Pts',(140.052640748718,-4.82063198407799,334.015303832346));
#41407=CARTESIAN_POINT('Ctrl Pts',(140.044874769923,-4.84631495845551,334.150666509196));
#41408=CARTESIAN_POINT('Ctrl Pts',(140.037108791128,-4.86627631122856,334.286881548916));
#41409=CARTESIAN_POINT('Ctrl Pts',(140.029342347225,-4.88623885949439,334.423104746606));
#41410=CARTESIAN_POINT('Ctrl Pts',(140.021575903323,-4.9004790384385,334.560180026654));
#41411=CARTESIAN_POINT('Ctrl Pts',(140.013809459421,-4.90894404984525,334.69759071114));
#41412=CARTESIAN_POINT('Ctrl Pts',(140.008051722444,-4.91521967737826,334.799461604568));
#41413=CARTESIAN_POINT('Ctrl Pts',(140.002293985467,-4.91832224859098,334.901516643467));
#41414=CARTESIAN_POINT('Ctrl Pts',(139.99653624849,-4.91824872290653,335.003544309289));
#41415=CARTESIAN_POINT('',(143.496536248456,-4.91824957381542,334.997952522408));
#41416=CARTESIAN_POINT('Ctrl Pts',(143.496536248456,-4.91824957381541,334.997952522409));
#41417=CARTESIAN_POINT('Ctrl Pts',(143.488840527635,-4.91830583800652,335.133104836198));
#41418=CARTESIAN_POINT('Ctrl Pts',(143.481144806814,-4.9127869647833,335.268484246378));
#41419=CARTESIAN_POINT('Ctrl Pts',(143.473449085993,-4.90166304579241,335.403586977011));
#41420=CARTESIAN_POINT('Ctrl Pts',(143.465762407207,-4.89055219677536,335.538530969599));
#41421=CARTESIAN_POINT('Ctrl Pts',(143.458075728422,-4.87384943324171,335.673198534926));
#41422=CARTESIAN_POINT('Ctrl Pts',(143.450389049636,-4.85157683415553,335.807084434731));
#41423=CARTESIAN_POINT('Ctrl Pts',(143.442709473782,-4.82932481622644,335.940846616298));
#41424=CARTESIAN_POINT('Ctrl Pts',(143.435029897928,-4.80151326699133,336.073828177672));
#41425=CARTESIAN_POINT('Ctrl Pts',(143.427350322074,-4.76821615087756,336.205528017514));
#41426=CARTESIAN_POINT('Ctrl Pts',(143.419449967503,-4.73396178208414,336.341014071878));
#41427=CARTESIAN_POINT('Ctrl Pts',(143.411549612932,-4.69390170447446,336.475143167105));
#41428=CARTESIAN_POINT('Ctrl Pts',(143.403649258361,-4.6481732473492,336.60737939676));
#41429=CARTESIAN_POINT('Ctrl Pts',(143.395977266379,-4.60376658771376,336.735793290665));
#41430=CARTESIAN_POINT('Ctrl Pts',(143.388305274396,-4.55401486860619,336.862421837089));
#41431=CARTESIAN_POINT('Ctrl Pts',(143.380633282414,-4.49909457980441,336.986789124309));
#41432=CARTESIAN_POINT('Ctrl Pts',(143.372962119359,-4.44418022491634,337.111142974151));
#41433=CARTESIAN_POINT('Ctrl Pts',(143.365290956305,-4.38409857211948,337.233235685312));
#41434=CARTESIAN_POINT('Ctrl Pts',(143.35761979325,-4.31907404683682,337.35261183378));
#41435=CARTESIAN_POINT('Ctrl Pts',(143.349947717993,-4.25404178928833,337.472002177632));
#41436=CARTESIAN_POINT('Ctrl Pts',(143.342275642737,-4.18406568151538,337.58867496567));
#41437=CARTESIAN_POINT('Ctrl Pts',(143.334603567481,-4.10941558937893,337.70220032127));
#41438=CARTESIAN_POINT('Ctrl Pts',(143.326531754555,-4.03087600804304,337.821640681551));
#41439=CARTESIAN_POINT('Ctrl Pts',(143.318459941629,-3.9471625706808,337.937596400006));
#41440=CARTESIAN_POINT('Ctrl Pts',(143.310388128704,-3.85863976017585,338.049603624029));
#41441=CARTESIAN_POINT('Ctrl Pts',(143.302704741091,-3.774376773414,338.156220926182));
#41442=CARTESIAN_POINT('Ctrl Pts',(143.295021353478,-3.68575677496038,338.259260601928));
#41443=CARTESIAN_POINT('Ctrl Pts',(143.287337965865,-3.59313334160412,338.358359101102));
#41444=CARTESIAN_POINT('Ctrl Pts',(143.27964941016,-3.50044760677403,338.457524257085));
#41445=CARTESIAN_POINT('Ctrl Pts',(143.271960854456,-3.40375335973002,338.552742679942));
#41446=CARTESIAN_POINT('Ctrl Pts',(143.264272298752,-3.30343869949283,338.643689863475));
#41447=CARTESIAN_POINT('Ctrl Pts',(143.256573199342,-3.20298647268547,338.734761767485));
#41448=CARTESIAN_POINT('Ctrl Pts',(143.248874099932,-3.09890423223411,338.82155049195));
#41449=CARTESIAN_POINT('Ctrl Pts',(143.241175000522,-2.99161071287561,338.903773610893));
#41450=CARTESIAN_POINT('Ctrl Pts',(143.240030604472,-2.97566257749354,338.915995275727));
#41451=CARTESIAN_POINT('Ctrl Pts',(143.238886208422,-2.95964353913426,338.928116149807));
#41452=CARTESIAN_POINT('Ctrl Pts',(143.237741812373,-2.94355502036444,338.940135391657));
#41453=CARTESIAN_POINT('Ctrl Pts',(143.229966733594,-2.834248892561,339.021794667106));
#41454=CARTESIAN_POINT('Ctrl Pts',(143.222191654816,-2.72136941230709,339.099031023707));
#41455=CARTESIAN_POINT('Ctrl Pts',(143.214416576037,-2.6053101860245,339.171515539597));
#41456=CARTESIAN_POINT('Ctrl Pts',(143.206651064988,-2.48939377800862,339.243910858676));
#41457=CARTESIAN_POINT('Ctrl Pts',(143.198885553939,-2.370305737832,339.311565766702));
#41458=CARTESIAN_POINT('Ctrl Pts',(143.19112004289,-2.24847177687613,339.374192237556));
#41459=CARTESIAN_POINT('Ctrl Pts',(143.183362231368,-2.12675861464739,339.436756614081));
#41460=CARTESIAN_POINT('Ctrl Pts',(143.175604419846,-2.00230529514067,339.494302297735));
#41461=CARTESIAN_POINT('Ctrl Pts',(143.167846608324,-1.87556517379614,339.546585349616));
#41462=CARTESIAN_POINT('Ctrl Pts',(143.160094634801,-1.74892042841222,339.598829056843));
#41463=CARTESIAN_POINT('Ctrl Pts',(143.152342661278,-1.6199926664213,339.645817866616));
#41464=CARTESIAN_POINT('Ctrl Pts',(143.144590687755,-1.48925810892312,339.68735462148));
#41465=CARTESIAN_POINT('Ctrl Pts',(143.136841997197,-1.3585789175874,339.728873785503));
#41466=CARTESIAN_POINT('Ctrl Pts',(143.12909330664,-1.22609482438024,339.764945368841));
#41467=CARTESIAN_POINT('Ctrl Pts',(143.121344616082,-1.09230001022392,339.795421123339));
#41468=CARTESIAN_POINT('Ctrl Pts',(143.113597537704,-0.958533033196216,
339.825890537102));
#41469=CARTESIAN_POINT('Ctrl Pts',(143.105850459327,-0.823456258525038,
339.850766351064));
#41470=CARTESIAN_POINT('Ctrl Pts',(143.098103380949,-0.687576555167322,
339.869950876886));
#41471=CARTESIAN_POINT('Ctrl Pts',(143.090356237643,-0.551695713006862,
339.889135563493));
#41472=CARTESIAN_POINT('Ctrl Pts',(143.082609094337,-0.41501231577349,339.902628812179));
#41473=CARTESIAN_POINT('Ctrl Pts',(143.074861951031,-0.278040500792239,
339.910384561561));
#41474=CARTESIAN_POINT('Ctrl Pts',(143.067113066003,-0.141037891639126,
339.918142054601));
#41475=CARTESIAN_POINT('Ctrl Pts',(143.059364180975,-0.00374712588186016,
339.920159459465));
#41476=CARTESIAN_POINT('Ctrl Pts',(143.051615295947,0.133315894509946,339.916442813129));
#41477=CARTESIAN_POINT('Ctrl Pts',(143.043858186172,0.270524395008002,339.912722221906));
#41478=CARTESIAN_POINT('Ctrl Pts',(143.036101076398,0.407504275911864,339.903255432377));
#41479=CARTESIAN_POINT('Ctrl Pts',(143.028343966623,0.5437424415808,339.888100573814));
#41480=CARTESIAN_POINT('Ctrl Pts',(143.020582711697,0.680053408569185,339.87293761698));
#41481=CARTESIAN_POINT('Ctrl Pts',(143.012821456771,0.815621484428806,339.852080593996));
#41482=CARTESIAN_POINT('Ctrl Pts',(143.005060201844,0.949943015645992,339.825638955571));
#41483=CARTESIAN_POINT('Ctrl Pts',(142.99728653144,1.08447941753802,339.799155019142));
#41484=CARTESIAN_POINT('Ctrl Pts',(142.989512861035,1.21776490983714,339.767068706896));
#41485=CARTESIAN_POINT('Ctrl Pts',(142.98173919063,1.34930940530986,339.729539849842));
#41486=CARTESIAN_POINT('Ctrl Pts',(142.974327386453,1.47473047287291,339.693757970112));
#41487=CARTESIAN_POINT('Ctrl Pts',(142.966915582276,1.59856870936171,339.653028933421));
#41488=CARTESIAN_POINT('Ctrl Pts',(142.959503778099,1.72041738727867,339.607531559962));
#41489=CARTESIAN_POINT('Ctrl Pts',(142.95172869932,1.84823823186638,339.559804224702));
#41490=CARTESIAN_POINT('Ctrl Pts',(142.943953620542,1.97427349568604,339.506678485956));
#41491=CARTESIAN_POINT('Ctrl Pts',(142.936178541763,2.09803357830588,339.448307337269));
#41492=CARTESIAN_POINT('Ctrl Pts',(142.928413030714,2.2216413662652,339.390008017996));
#41493=CARTESIAN_POINT('Ctrl Pts',(142.920647519665,2.3429791935886,339.32647629715));
#41494=CARTESIAN_POINT('Ctrl Pts',(142.912882008616,2.46157447611125,339.257914297054));
#41495=CARTESIAN_POINT('Ctrl Pts',(142.905124197094,2.58005217106592,339.18942027638));
#41496=CARTESIAN_POINT('Ctrl Pts',(142.897366385572,2.69579239644874,339.115906096308));
#41497=CARTESIAN_POINT('Ctrl Pts',(142.88960857405,2.80834468219192,339.037620983761));
#41498=CARTESIAN_POINT('Ctrl Pts',(142.881856600527,2.92081226877096,338.959394783243));
#41499=CARTESIAN_POINT('Ctrl Pts',(142.874104627004,3.03009637125878,338.876405018817));
#41500=CARTESIAN_POINT('Ctrl Pts',(142.866352653481,3.13577348518116,338.788945461753));
#41501=CARTESIAN_POINT('Ctrl Pts',(142.858603962923,3.24140584478293,338.701522943862));
#41502=CARTESIAN_POINT('Ctrl Pts',(142.850855272365,3.3434339535351,338.609634646991));
#41503=CARTESIAN_POINT('Ctrl Pts',(142.843106581808,3.44146571674916,338.513615912837));
#41504=CARTESIAN_POINT('Ctrl Pts',(142.83535950343,3.53947708363611,338.417617156183));
#41505=CARTESIAN_POINT('Ctrl Pts',(142.827612425052,3.633493479777,338.317489944933));
#41506=CARTESIAN_POINT('Ctrl Pts',(142.819865346674,3.72315846108758,338.213607651244));
#41507=CARTESIAN_POINT('Ctrl Pts',(142.812118203368,3.81282419387709,338.10972448692));
#41508=CARTESIAN_POINT('Ctrl Pts',(142.804371060062,3.89813818369696,338.00208647328));
#41509=CARTESIAN_POINT('Ctrl Pts',(142.796623916757,3.97878346734188,337.891101032912));
#41510=CARTESIAN_POINT('Ctrl Pts',(142.788875031728,4.05944688175883,337.780090640661));
#41511=CARTESIAN_POINT('Ctrl Pts',(142.7811261467,4.13543927164257,337.665731640296));
#41512=CARTESIAN_POINT('Ctrl Pts',(142.773377261672,4.20648652945596,337.548461131743));
#41513=CARTESIAN_POINT('Ctrl Pts',(142.765620151897,4.27760919756266,337.431066151061));
#41514=CARTESIAN_POINT('Ctrl Pts',(142.757863042123,4.34377604574314,337.310753823853));
#41515=CARTESIAN_POINT('Ctrl Pts',(142.750105932348,4.4047582906504,337.187987080274));
#41516=CARTESIAN_POINT('Ctrl Pts',(142.742344677422,4.46577312251947,337.065154734073));
#41517=CARTESIAN_POINT('Ctrl Pts',(142.734583422496,4.52159767166923,336.939865714952));
#41518=CARTESIAN_POINT('Ctrl Pts',(142.726822167569,4.57205142171969,336.812602785955));
#41519=CARTESIAN_POINT('Ctrl Pts',(142.719048497165,4.62258588132743,336.685136277746));
#41520=CARTESIAN_POINT('Ctrl Pts',(142.71127482676,4.6677322446311,336.555689919082));
#41521=CARTESIAN_POINT('Ctrl Pts',(142.703501156355,4.70735970261259,336.424762328502));
#41522=CARTESIAN_POINT('Ctrl Pts',(142.696089352178,4.74514249289104,336.299929448764));
#41523=CARTESIAN_POINT('Ctrl Pts',(142.688677548001,4.77790855262165,336.173750414946));
#41524=CARTESIAN_POINT('Ctrl Pts',(142.681265743824,4.80558815193244,336.046664022744));
#41525=CARTESIAN_POINT('Ctrl Pts',(142.673490665046,4.83462441085886,335.913348747889));
#41526=CARTESIAN_POINT('Ctrl Pts',(142.665715586267,4.85815475691442,335.778613620109));
#41527=CARTESIAN_POINT('Ctrl Pts',(142.657940507489,4.87604289474714,335.642953148438));
#41528=CARTESIAN_POINT('Ctrl Pts',(142.65017499644,4.89390902008739,335.507459615614));
#41529=CARTESIAN_POINT('Ctrl Pts',(142.642409485391,4.90614670136614,335.37104338839));
#41530=CARTESIAN_POINT('Ctrl Pts',(142.634643974342,4.9126701651479,335.234211252859));
#41531=CARTESIAN_POINT('Ctrl Pts',(142.62688616282,4.91918716089635,335.097514786788));
#41532=CARTESIAN_POINT('Ctrl Pts',(142.619128351298,4.92000119564422,334.960403620974));
#41533=CARTESIAN_POINT('Ctrl Pts',(142.611370539776,4.91507807442839,334.823391436297));
#41534=CARTESIAN_POINT('Ctrl Pts',(142.603618566252,4.91015865801739,334.686482357633));
#41535=CARTESIAN_POINT('Ctrl Pts',(142.595866592729,4.8995106931793,334.549672500894));
#41536=CARTESIAN_POINT('Ctrl Pts',(142.588114619206,4.88315203587047,334.413476976518));
#41537=CARTESIAN_POINT('Ctrl Pts',(142.580365928649,4.86680030646277,334.277339131028));
#41538=CARTESIAN_POINT('Ctrl Pts',(142.572617238091,4.84474274129044,334.141815487718));
#41539=CARTESIAN_POINT('Ctrl Pts',(142.564868547534,4.81704915140712,334.007417240011));
#41540=CARTESIAN_POINT('Ctrl Pts',(142.557121469156,4.78936132340645,333.873046954981));
#41541=CARTESIAN_POINT('Ctrl Pts',(142.549374390778,4.75603988195816,333.739801982409));
#41542=CARTESIAN_POINT('Ctrl Pts',(142.5416273124,4.71720591132571,333.608184116827));
#41543=CARTESIAN_POINT('Ctrl Pts',(142.533880169094,4.67837161522723,333.476565148159));
#41544=CARTESIAN_POINT('Ctrl Pts',(142.526133025789,4.63402480840819,333.346573688577));
#41545=CARTESIAN_POINT('Ctrl Pts',(142.518385882483,4.58433657423815,333.218696758942));
#41546=CARTESIAN_POINT('Ctrl Pts',(142.510636997455,4.53463716909814,333.090791079859));
#41547=CARTESIAN_POINT('Ctrl Pts',(142.502888112427,4.47959408855751,332.965001240964));
#41548=CARTESIAN_POINT('Ctrl Pts',(142.495139227399,4.4194265639526,332.841794284983));
#41549=CARTESIAN_POINT('Ctrl Pts',(142.487382117624,4.35919517691543,332.718456555867));
#41550=CARTESIAN_POINT('Ctrl Pts',(142.479625007849,4.29382865241851,332.597707537852));
#41551=CARTESIAN_POINT('Ctrl Pts',(142.471867898074,4.22359247050929,332.479990137806));
#41552=CARTESIAN_POINT('Ctrl Pts',(142.464106643148,4.15331875663018,332.362209833344));
#41553=CARTESIAN_POINT('Ctrl Pts',(142.456345388222,4.07817041428427,332.247464701671));
#41554=CARTESIAN_POINT('Ctrl Pts',(142.448584133296,3.99845572144275,332.136167793644));
#41555=CARTESIAN_POINT('Ctrl Pts',(142.440810462891,3.91861351107166,332.024692846836));
#41556=CARTESIAN_POINT('Ctrl Pts',(142.433036792487,3.83419059413541,331.916677454475));
#41557=CARTESIAN_POINT('Ctrl Pts',(142.425263122082,3.74553548133648,331.812501447757));
#41558=CARTESIAN_POINT('Ctrl Pts',(142.417851317905,3.6610072853676,331.713174859216));
#41559=CARTESIAN_POINT('Ctrl Pts',(142.410439513728,3.57263223895412,331.617338465204));
#41560=CARTESIAN_POINT('Ctrl Pts',(142.403027709551,3.48074159992395,331.525288360589));
#41561=CARTESIAN_POINT('Ctrl Pts',(142.395252630772,3.38434712694685,331.428726606143));
#41562=CARTESIAN_POINT('Ctrl Pts',(142.387477551994,3.28377910397054,331.336026527406));
#41563=CARTESIAN_POINT('Ctrl Pts',(142.379702473216,3.1793796169556,331.247570345258));
#41564=CARTESIAN_POINT('Ctrl Pts',(142.371936962167,3.07510860015578,331.159223014074));
#41565=CARTESIAN_POINT('Ctrl Pts',(142.364171451118,2.96701579590837,331.075109438695));
#41566=CARTESIAN_POINT('Ctrl Pts',(142.356405940069,2.855480954523,330.995575998866));
#41567=CARTESIAN_POINT('Ctrl Pts',(142.348648128546,2.74405670025762,330.916121416675));
#41568=CARTESIAN_POINT('Ctrl Pts',(142.340890317024,2.6291975166976,330.84123815823));
#41569=CARTESIAN_POINT('Ctrl Pts',(142.333132505502,2.51131686419744,330.771232961004));
#41570=CARTESIAN_POINT('Ctrl Pts',(142.325380531979,2.39352492062629,330.701280444909));
#41571=CARTESIAN_POINT('Ctrl Pts',(142.317628558456,2.2727163686305,330.636198882077));
#41572=CARTESIAN_POINT('Ctrl Pts',(142.309876584933,2.14933403844941,330.576252012867));
#41573=CARTESIAN_POINT('Ctrl Pts',(142.302127894375,2.02600396075849,330.516330531192));
#41574=CARTESIAN_POINT('Ctrl Pts',(142.294379203818,1.90010262365113,330.461539588583));
#41575=CARTESIAN_POINT('Ctrl Pts',(142.28663051326,1.77209767934956,330.412097115528));
#41576=CARTESIAN_POINT('Ctrl Pts',(142.278883434882,1.64411936754582,330.362664929393));
#41577=CARTESIAN_POINT('Ctrl Pts',(142.271136356505,1.51403868350181,330.318579140135));
#41578=CARTESIAN_POINT('Ctrl Pts',(142.263389278127,1.3823431225873,330.280009475228));
#41579=CARTESIAN_POINT('Ctrl Pts',(142.255642134821,1.25064645793736,330.24143948707));
#41580=CARTESIAN_POINT('Ctrl Pts',(142.247894991515,1.11733526453966,330.208385825334));
#41581=CARTESIAN_POINT('Ctrl Pts',(142.240147848209,0.982911671655583,330.180968177297));
#41582=CARTESIAN_POINT('Ctrl Pts',(142.232398963181,0.848457857494069,330.153544365191));
#41583=CARTESIAN_POINT('Ctrl Pts',(142.224650078153,0.712891529107122,330.131759166265));
#41584=CARTESIAN_POINT('Ctrl Pts',(142.216901193125,0.576724071343072,330.115680967828));
#41585=CARTESIAN_POINT('Ctrl Pts',(142.20914408335,0.440412084032061,330.099585703826));
#41586=CARTESIAN_POINT('Ctrl Pts',(142.201386973576,0.303498081580096,330.089209586584));
#41587=CARTESIAN_POINT('Ctrl Pts',(142.193629863801,0.166498180307998,330.084569050586));
#41588=CARTESIAN_POINT('Ctrl Pts',(142.185868608875,0.0294250706691604,
330.079926034835));
#41589=CARTESIAN_POINT('Ctrl Pts',(142.178107353948,-0.107733638589367,
330.08102470431));
#41590=CARTESIAN_POINT('Ctrl Pts',(142.170346099022,-0.244463777289203,
330.08782934701));
#41591=CARTESIAN_POINT('Ctrl Pts',(142.162572428618,-0.381412639650758,
330.094644874921));
#41592=CARTESIAN_POINT('Ctrl Pts',(142.154798758213,-0.517931172034827,
330.107184580128));
#41593=CARTESIAN_POINT('Ctrl Pts',(142.147025087808,-0.653511367146012,
330.125360941002));
#41594=CARTESIAN_POINT('Ctrl Pts',(142.139613283631,-0.782780271556707,
330.142691187904));
#41595=CARTESIAN_POINT('Ctrl Pts',(142.132201479454,-0.911195948435113,
330.165145077941));
#41596=CARTESIAN_POINT('Ctrl Pts',(142.124789675277,-1.03833014267276,330.192604283261));
#41597=CARTESIAN_POINT('Ctrl Pts',(142.117014596498,-1.17169556248273,330.221409346031));
#41598=CARTESIAN_POINT('Ctrl Pts',(142.10923951772,-1.30407216418749,330.255813810342));
#41599=CARTESIAN_POINT('Ctrl Pts',(142.101464438941,-1.43495340775072,330.295736850464));
#41600=CARTESIAN_POINT('Ctrl Pts',(142.093698927892,-1.56567359361126,330.335610762743));
#41601=CARTESIAN_POINT('Ctrl Pts',(142.085933416843,-1.69490171237429,330.38098962582));
#41602=CARTESIAN_POINT('Ctrl Pts',(142.078167905794,-1.82214098123911,330.431741545513));
#41603=CARTESIAN_POINT('Ctrl Pts',(142.070410094272,-1.94925409199845,330.482443144531));
#41604=CARTESIAN_POINT('Ctrl Pts',(142.06265228275,-2.07438191643226,330.538507054455));
#41605=CARTESIAN_POINT('Ctrl Pts',(142.054894471228,-2.19704276533312,330.599751580899));
#41606=CARTESIAN_POINT('Ctrl Pts',(142.047142497705,-2.31961130805555,330.660950018896));
#41607=CARTESIAN_POINT('Ctrl Pts',(142.039390524182,-2.43971622217395,330.727321139579));
#41608=CARTESIAN_POINT('Ctrl Pts',(142.031638550659,-2.55689608194047,330.798635282595));
#41609=CARTESIAN_POINT('Ctrl Pts',(142.023889860101,-2.67402631596664,330.869919224029));
#41610=CARTESIAN_POINT('Ctrl Pts',(142.016141169543,-2.78823362624632,330.94614182144));
#41611=CARTESIAN_POINT('Ctrl Pts',(142.008392478986,-2.89908167693048,331.027027750791));
#41612=CARTESIAN_POINT('Ctrl Pts',(142.000645400608,-3.00990666475198,331.107896851148));
#41613=CARTESIAN_POINT('Ctrl Pts',(141.99289832223,-3.11737346763247,331.193427123301));
#41614=CARTESIAN_POINT('Ctrl Pts',(141.985151243852,-3.22107554640128,331.283300471268));
#41615=CARTESIAN_POINT('Ctrl Pts',(141.977404100546,-3.32477849429333,331.37317457246));
#41616=CARTESIAN_POINT('Ctrl Pts',(141.969656957241,-3.42471635975889,331.467391566074));
#41617=CARTESIAN_POINT('Ctrl Pts',(141.961909813935,-3.52051676425655,331.565593970555));
#41618=CARTESIAN_POINT('Ctrl Pts',(141.954160928907,-3.61633870671897,331.663818453022));
#41619=CARTESIAN_POINT('Ctrl Pts',(141.946412043878,-3.70802106434763,331.76602984957));
#41620=CARTESIAN_POINT('Ctrl Pts',(141.93866315885,-3.7952295891095,331.871835134069));
#41621=CARTESIAN_POINT('Ctrl Pts',(141.930906049076,-3.88253067790056,331.977752721389));
#41622=CARTESIAN_POINT('Ctrl Pts',(141.923148939301,-3.96534819910468,332.087271514562));
#41623=CARTESIAN_POINT('Ctrl Pts',(141.915391829526,-4.04338903245736,332.199966394005));
#41624=CARTESIAN_POINT('Ctrl Pts',(141.9076305746,-4.12147156833623,332.312721493987));
#41625=CARTESIAN_POINT('Ctrl Pts',(141.899869319674,-4.19477212148012,332.428655731851));
#41626=CARTESIAN_POINT('Ctrl Pts',(141.892108064748,-4.26304247588702,332.547317405109));
#41627=CARTESIAN_POINT('Ctrl Pts',(141.884334394343,-4.33142204061157,332.666168898372));
#41628=CARTESIAN_POINT('Ctrl Pts',(141.876560723938,-4.39475514628468,332.787756198764));
#41629=CARTESIAN_POINT('Ctrl Pts',(141.868787053534,-4.45284047981482,332.911604749138));
#41630=CARTESIAN_POINT('Ctrl Pts',(141.861375249357,-4.5082219270939,333.029688119694));
#41631=CARTESIAN_POINT('Ctrl Pts',(141.85396344518,-4.55883306317671,333.14982669031));
#41632=CARTESIAN_POINT('Ctrl Pts',(141.846551641003,-4.6045416390662,333.271596298139));
#41633=CARTESIAN_POINT('Ctrl Pts',(141.837634724743,-4.65953223701258,333.418093611081));
#41634=CARTESIAN_POINT('Ctrl Pts',(141.828717808484,-4.70757175041617,333.567334854595));
#41635=CARTESIAN_POINT('Ctrl Pts',(141.819800892224,-4.748414626951,333.718695355094));
#41636=CARTESIAN_POINT('Ctrl Pts',(141.810916116168,-4.78911028909658,333.8695102906));
#41637=CARTESIAN_POINT('Ctrl Pts',(141.802031340113,-4.82266099798843,334.022429090279));
#41638=CARTESIAN_POINT('Ctrl Pts',(141.793146564057,-4.84887039270233,334.176811699989));
#41639=CARTESIAN_POINT('Ctrl Pts',(141.784323191418,-4.87489865213825,334.330127358813));
#41640=CARTESIAN_POINT('Ctrl Pts',(141.775499818779,-4.89368663649289,334.484886506641));
#41641=CARTESIAN_POINT('Ctrl Pts',(141.766676446139,-4.90508935650447,334.64044267883));
#41642=CARTESIAN_POINT('Ctrl Pts',(141.759963046941,-4.91376529194467,334.758799992338));
#41643=CARTESIAN_POINT('Ctrl Pts',(141.753249647743,-4.91816671843185,334.877618301574));
#41644=CARTESIAN_POINT('Ctrl Pts',(141.746536248545,-4.91824882895472,334.996606036901));
#41645=CARTESIAN_POINT('',(145.246536248534,-4.91824795069328,335.004489766291));
#41646=CARTESIAN_POINT('Ctrl Pts',(145.24653624849,-4.91824795069257,335.004489767066));
#41647=CARTESIAN_POINT('Ctrl Pts',(145.235878849129,-4.91807628812392,335.192534951623));
#41648=CARTESIAN_POINT('Ctrl Pts',(145.225221449767,-4.9071165282921,335.380107035918));
#41649=CARTESIAN_POINT('Ctrl Pts',(145.214564050406,-4.88555165495592,335.566187327002));
#41650=CARTESIAN_POINT('Ctrl Pts',(145.204845384367,-4.86588627553186,335.735877149449));
#41651=CARTESIAN_POINT('Ctrl Pts',(145.195126718329,-4.83740238492614,335.904327231285));
#41652=CARTESIAN_POINT('Ctrl Pts',(145.18540805229,-4.80027135218314,336.070783828749));
#41653=CARTESIAN_POINT('Ctrl Pts',(145.177632973512,-4.77056596838255,336.203951606441));
#41654=CARTESIAN_POINT('Ctrl Pts',(145.169857894733,-4.73526799098947,336.336092760649));
#41655=CARTESIAN_POINT('Ctrl Pts',(145.162082815955,-4.69446166592918,336.466701308932));
#41656=CARTESIAN_POINT('Ctrl Pts',(145.154317304906,-4.65370555564978,336.59714913508));
#41657=CARTESIAN_POINT('Ctrl Pts',(145.146551793857,-4.60745470017155,336.726067738318));
#41658=CARTESIAN_POINT('Ctrl Pts',(145.138786282808,-4.55584434678735,336.85296123822));
#41659=CARTESIAN_POINT('Ctrl Pts',(145.131028471285,-4.5042851652188,336.979728922848));
#41660=CARTESIAN_POINT('Ctrl Pts',(145.123270659763,-4.44737720713481,337.104475140226));
#41661=CARTESIAN_POINT('Ctrl Pts',(145.115512848241,-4.38530541692814,337.226719439615));
#41662=CARTESIAN_POINT('Ctrl Pts',(145.107760874718,-4.32328033771178,337.348871746293));
#41663=CARTESIAN_POINT('Ctrl Pts',(145.100008901195,-4.25609933741541,337.468525535432));
#41664=CARTESIAN_POINT('Ctrl Pts',(145.092256927672,-4.18399518841079,337.585220943334));
#41665=CARTESIAN_POINT('Ctrl Pts',(145.084508237114,-4.11192157555631,337.701866930662));
#41666=CARTESIAN_POINT('Ctrl Pts',(145.076759546556,-4.03492916585593,337.815556696807));
#41667=CARTESIAN_POINT('Ctrl Pts',(145.069010855999,-3.95329622482413,337.925855775887));
#41668=CARTESIAN_POINT('Ctrl Pts',(145.061263777621,-3.87168026820744,338.036131906323));
#41669=CARTESIAN_POINT('Ctrl Pts',(145.053516699243,-3.78542593309394,338.143018438918));
#41670=CARTESIAN_POINT('Ctrl Pts',(145.045769620865,-3.69485405466793,338.246110992743));
#41671=CARTESIAN_POINT('Ctrl Pts',(145.038022477559,-3.6042814171625,338.349204410582));
#41672=CARTESIAN_POINT('Ctrl Pts',(145.030275334254,-3.5093914221528,338.448503492585));
#41673=CARTESIAN_POINT('Ctrl Pts',(145.022528190948,-3.41054405871756,338.543638283748));
#41674=CARTESIAN_POINT('Ctrl Pts',(145.01477930592,-3.31167447229633,338.638794463233));
#41675=CARTESIAN_POINT('Ctrl Pts',(145.007030420891,-3.20884602861807,338.729784217906));
#41676=CARTESIAN_POINT('Ctrl Pts',(144.999281535863,-3.10245400292844,338.816275962534));
#41677=CARTESIAN_POINT('Ctrl Pts',(144.991524426089,-2.99594905164362,338.902859510393));
#41678=CARTESIAN_POINT('Ctrl Pts',(144.983767316314,-2.88587326637787,338.984935264271));
#41679=CARTESIAN_POINT('Ctrl Pts',(144.976010206539,-2.77265373724858,339.062212982578));
#41680=CARTESIAN_POINT('Ctrl Pts',(144.968248951613,-2.65937370722299,339.139531995626));
#41681=CARTESIAN_POINT('Ctrl Pts',(144.960487696687,-2.5429469175631,339.212047657725));
#41682=CARTESIAN_POINT('Ctrl Pts',(144.952726441761,-2.42382673732278,339.279514810109));
#41683=CARTESIAN_POINT('Ctrl Pts',(144.944952771356,-2.30451600361524,339.347089887949));
#41684=CARTESIAN_POINT('Ctrl Pts',(144.937179100951,-2.18250361763352,339.409600139572));
#41685=CARTESIAN_POINT('Ctrl Pts',(144.929405430547,-2.05826548570975,339.466847462454));
#41686=CARTESIAN_POINT('Ctrl Pts',(144.92199362637,-1.93981066872105,339.521429908682));
#41687=CARTESIAN_POINT('Ctrl Pts',(144.914581822193,-1.81933292542051,339.571228268232));
#41688=CARTESIAN_POINT('Ctrl Pts',(144.907170018016,-1.69725730241249,339.616113160648));
#41689=CARTESIAN_POINT('Ctrl Pts',(144.899394939238,-1.56919838947214,339.663197995348));
#41690=CARTESIAN_POINT('Ctrl Pts',(144.891619860459,-1.43897631282604,339.705024333909));
#41691=CARTESIAN_POINT('Ctrl Pts',(144.883844781681,-1.30706215420824,339.741389204393));
#41692=CARTESIAN_POINT('Ctrl Pts',(144.876079270632,-1.17531032436078,339.777709325589));
#41693=CARTESIAN_POINT('Ctrl Pts',(144.868313759583,-1.0418709287678,339.808581248059));
#41694=CARTESIAN_POINT('Ctrl Pts',(144.860548248534,-0.907234153928469,
339.833850354784));
#41695=CARTESIAN_POINT('Ctrl Pts',(144.852790437012,-0.77273087184328,339.859094407116));
#41696=CARTESIAN_POINT('Ctrl Pts',(144.845032625489,-0.637032954808813,
339.878746627246));
#41697=CARTESIAN_POINT('Ctrl Pts',(144.837274813967,-0.500644508125581,
339.892702539393));
#41698=CARTESIAN_POINT('Ctrl Pts',(144.829522840444,-0.364358698073604,
339.906647949274));
#41699=CARTESIAN_POINT('Ctrl Pts',(144.821770866921,-0.227383779979994,
339.914905543918));
#41700=CARTESIAN_POINT('Ctrl Pts',(144.814018893398,-0.0902324295267442,
339.917422207942));
#41701=CARTESIAN_POINT('Ctrl Pts',(144.80627020284,0.0468608372481148,339.919937806158));
#41702=CARTESIAN_POINT('Ctrl Pts',(144.798521512283,0.184129997776206,339.916717302258));
#41703=CARTESIAN_POINT('Ctrl Pts',(144.790772821725,0.321059114991753,339.907759581233));
#41704=CARTESIAN_POINT('Ctrl Pts',(144.783025743347,0.457959742960808,339.898803723936));
#41705=CARTESIAN_POINT('Ctrl Pts',(144.77527866497,0.594520078546099,339.884113049318));
#41706=CARTESIAN_POINT('Ctrl Pts',(144.767531586592,0.730226446869954,339.863738520808));
#41707=CARTESIAN_POINT('Ctrl Pts',(144.759784443286,0.865933952543838,339.84336382154));
#41708=CARTESIAN_POINT('Ctrl Pts',(144.75203729998,1.00078709013895,339.817305231398));
#41709=CARTESIAN_POINT('Ctrl Pts',(144.744290156674,1.1342799458554,339.785665269002));
#41710=CARTESIAN_POINT('Ctrl Pts',(144.736541271646,1.26780281359986,339.75401819327));
#41711=CARTESIAN_POINT('Ctrl Pts',(144.728792386618,1.39996441065466,339.716787338477));
#41712=CARTESIAN_POINT('Ctrl Pts',(144.72104350159,1.53027199380604,339.674125660214));
#41713=CARTESIAN_POINT('Ctrl Pts',(144.713286391815,1.66071788677265,339.631418700405));
#41714=CARTESIAN_POINT('Ctrl Pts',(144.70552928204,1.78930546277245,339.583269524141));
#41715=CARTESIAN_POINT('Ctrl Pts',(144.697772172266,1.91555952849149,339.529880214234));
#41716=CARTESIAN_POINT('Ctrl Pts',(144.69001091734,2.04188106034638,339.476462374787));
#41717=CARTESIAN_POINT('Ctrl Pts',(144.682249662413,2.16586624411189,339.417798989215));
#41718=CARTESIAN_POINT('Ctrl Pts',(144.674488407487,2.28706357654228,339.354138635753));
#41719=CARTESIAN_POINT('Ctrl Pts',(144.666714737083,2.40845478520644,339.290376446472));
#41720=CARTESIAN_POINT('Ctrl Pts',(144.658941066678,2.52704889251869,339.221601512071));
#41721=CARTESIAN_POINT('Ctrl Pts',(144.651167396273,2.64242176961468,339.148106827695));
#41722=CARTESIAN_POINT('Ctrl Pts',(144.643755592096,2.7524240115249,339.078033338557));
#41723=CARTESIAN_POINT('Ctrl Pts',(144.636343787919,2.85949793438714,339.003669783716));
#41724=CARTESIAN_POINT('Ctrl Pts',(144.628931983742,2.96330472230804,338.925303578737));
#41725=CARTESIAN_POINT('Ctrl Pts',(144.621156904963,3.07219939012918,338.843096412612));
#41726=CARTESIAN_POINT('Ctrl Pts',(144.613381826185,3.17784268836485,338.756224521984));
#41727=CARTESIAN_POINT('Ctrl Pts',(144.605606747407,3.27980900422639,338.664974209772));
#41728=CARTESIAN_POINT('Ctrl Pts',(144.597841236358,3.38164984404481,338.573836186879));
#41729=CARTESIAN_POINT('Ctrl Pts',(144.590075725309,3.47982241597921,338.478330720999));
#41730=CARTESIAN_POINT('Ctrl Pts',(144.58231021426,3.57393143123928,338.378786348277));
#41731=CARTESIAN_POINT('Ctrl Pts',(144.574552402737,3.66794713713673,338.27934067409));
#41732=CARTESIAN_POINT('Ctrl Pts',(144.566794591215,3.75790703755715,338.175864344624));
#41733=CARTESIAN_POINT('Ctrl Pts',(144.559036779693,3.84345047628596,338.068724734941));
#41734=CARTESIAN_POINT('Ctrl Pts',(144.55128480617,3.92892954086429,337.961665751212));
#41735=CARTESIAN_POINT('Ctrl Pts',(144.543532832647,4.00999851616736,337.850949278638));
#41736=CARTESIAN_POINT('Ctrl Pts',(144.535780859124,4.0863352981092,337.736977693356));
#41737=CARTESIAN_POINT('Ctrl Pts',(144.528032168566,4.1626397513786,337.623054375108));
#41738=CARTESIAN_POINT('Ctrl Pts',(144.520283478009,4.23421578020743,337.505879010058));
#41739=CARTESIAN_POINT('Ctrl Pts',(144.512534787451,4.30078324380866,337.385884857296));
#41740=CARTESIAN_POINT('Ctrl Pts',(144.504787709073,4.36733685749311,337.26591567032));
#41741=CARTESIAN_POINT('Ctrl Pts',(144.497040630695,4.42888378921111,337.143129203753));
#41742=CARTESIAN_POINT('Ctrl Pts',(144.489293552318,4.48518891624504,337.017984996994));
#41743=CARTESIAN_POINT('Ctrl Pts',(144.481546409012,4.54149451517015,336.892839741406));
#41744=CARTESIAN_POINT('Ctrl Pts',(144.473799265706,4.5925580614089,336.76533706267));
#41745=CARTESIAN_POINT('Ctrl Pts',(144.4660521224,4.63819198606711,336.635957873199));
#41746=CARTESIAN_POINT('Ctrl Pts',(144.458303237372,4.68383617020041,336.50654959654));
#41747=CARTESIAN_POINT('Ctrl Pts',(144.450554352344,4.72404817371695,336.375264338199));
#41748=CARTESIAN_POINT('Ctrl Pts',(144.442805467316,4.75868996860927,336.242599229501));
#41749=CARTESIAN_POINT('Ctrl Pts',(144.435048357541,4.79336853266061,336.109793308687));
#41750=CARTESIAN_POINT('Ctrl Pts',(144.427291247766,4.82246497884918,335.975604990658));
#41751=CARTESIAN_POINT('Ctrl Pts',(144.419534137992,4.84589208855476,335.840543234214));
#41752=CARTESIAN_POINT('Ctrl Pts',(144.411772883066,4.86933171695872,335.705409305085));
#41753=CARTESIAN_POINT('Ctrl Pts',(144.404011628139,4.88709592170682,335.569401394912));
#41754=CARTESIAN_POINT('Ctrl Pts',(144.396250373213,4.89914940322585,335.433033702351));
#41755=CARTESIAN_POINT('Ctrl Pts',(144.388476702809,4.91122216638709,335.296447865924));
#41756=CARTESIAN_POINT('Ctrl Pts',(144.380703032404,4.91756593319584,335.159501487682));
#41757=CARTESIAN_POINT('Ctrl Pts',(144.372929361999,4.9181975690542,335.022709783119));
#41758=CARTESIAN_POINT('Ctrl Pts',(144.365517557822,4.9187998021114,334.892285765315));
#41759=CARTESIAN_POINT('Ctrl Pts',(144.358105753645,4.91420974592913,334.762002632754));
#41760=CARTESIAN_POINT('Ctrl Pts',(144.350693949468,4.90448574166947,334.632300840005));
#41761=CARTESIAN_POINT('Ctrl Pts',(144.34291887069,4.89428513499471,334.496241976032));
#41762=CARTESIAN_POINT('Ctrl Pts',(144.335143791911,4.8784023593217,334.360392908018));
#41763=CARTESIAN_POINT('Ctrl Pts',(144.327368713133,4.85684784938132,334.225266477774));
#41764=CARTESIAN_POINT('Ctrl Pts',(144.319603202084,4.83531986363765,334.090306329206));
#41765=CARTESIAN_POINT('Ctrl Pts',(144.311837691035,4.80813409167404,333.956067431356));
#41766=CARTESIAN_POINT('Ctrl Pts',(144.304072179986,4.77535289309746,333.823059980761));
#41767=CARTESIAN_POINT('Ctrl Pts',(144.296314368463,4.7426041971747,333.690184407441));
#41768=CARTESIAN_POINT('Ctrl Pts',(144.288556556941,4.70427120817129,333.558538228622));
#41769=CARTESIAN_POINT('Ctrl Pts',(144.280798745419,4.66046768784341,333.428623535537));
#41770=CARTESIAN_POINT('Ctrl Pts',(144.273046771896,4.61669713105369,333.298806607379));
#41771=CARTESIAN_POINT('Ctrl Pts',(144.265294798373,4.56746436150689,333.170718940296));
#41772=CARTESIAN_POINT('Ctrl Pts',(144.25754282485,4.51293343687854,333.044849147303));
#41773=CARTESIAN_POINT('Ctrl Pts',(144.249794134292,4.45842560612914,332.919032660242));
#41774=CARTESIAN_POINT('Ctrl Pts',(144.242045443735,4.39862423806305,332.795432537042));
#41775=CARTESIAN_POINT('Ctrl Pts',(144.234296753177,4.33374206923738,332.674518815423));
#41776=CARTESIAN_POINT('Ctrl Pts',(144.226549674799,4.26887339968883,332.553630250913));
#41777=CARTESIAN_POINT('Ctrl Pts',(144.218802596422,4.19892621673326,332.43542732044));
#41778=CARTESIAN_POINT('Ctrl Pts',(144.211055518044,4.12415971846065,332.32035642685));
#41779=CARTESIAN_POINT('Ctrl Pts',(144.203308374738,4.04939259357281,332.205284568854));
#41780=CARTESIAN_POINT('Ctrl Pts',(144.195561231432,3.96980628576874,332.093345127863));
#41781=CARTESIAN_POINT('Ctrl Pts',(144.187814088126,3.88570370026562,331.984956083862));
#41782=CARTESIAN_POINT('Ctrl Pts',(144.180065203098,3.80158220671579,331.876542671703));
#41783=CARTESIAN_POINT('Ctrl Pts',(144.17231631807,3.71294265459526,331.771681553625));
#41784=CARTESIAN_POINT('Ctrl Pts',(144.164567433042,3.620128397368,331.670757826611));
#41785=CARTESIAN_POINT('Ctrl Pts',(144.156810323267,3.52721562612911,331.569726978111));
#41786=CARTESIAN_POINT('Ctrl Pts',(144.149053213492,3.4301195633022,331.472642157156));
#41787=CARTESIAN_POINT('Ctrl Pts',(144.141296103718,3.32922100420126,331.379852134555));
#41788=CARTESIAN_POINT('Ctrl Pts',(144.133534848792,3.22826852813645,331.287012527933));
#41789=CARTESIAN_POINT('Ctrl Pts',(144.125773593865,3.12350980536916,331.198472544851));
#41790=CARTESIAN_POINT('Ctrl Pts',(144.118012338939,3.01535813389604,331.11454013187));
#41791=CARTESIAN_POINT('Ctrl Pts',(144.110238668535,2.90703345499511,331.030473454383));
#41792=CARTESIAN_POINT('Ctrl Pts',(144.10246499813,2.79530530013393,330.951029302286));
#41793=CARTESIAN_POINT('Ctrl Pts',(144.094691327725,2.68061605185049,330.876472305772));
#41794=CARTESIAN_POINT('Ctrl Pts',(144.087279523548,2.57126561566729,330.805385955384));
#41795=CARTESIAN_POINT('Ctrl Pts',(144.079867719371,2.45922380725008,330.738742152878));
#41796=CARTESIAN_POINT('Ctrl Pts',(144.072455915194,2.34489258599307,330.676730193169));
#41797=CARTESIAN_POINT('Ctrl Pts',(144.064680836416,2.22495765100707,330.611678842591));
#41798=CARTESIAN_POINT('Ctrl Pts',(144.056905757637,2.10212419023106,330.551519281778));
#41799=CARTESIAN_POINT('Ctrl Pts',(144.049130678859,1.97682911011694,330.496520264074));
#41800=CARTESIAN_POINT('Ctrl Pts',(144.04136516781,1.85168821357553,330.441588926163));
#41801=CARTESIAN_POINT('Ctrl Pts',(144.033599656761,1.72409207938351,330.391805651538));
#41802=CARTESIAN_POINT('Ctrl Pts',(144.025834145712,1.59450348905423,330.347394097294));
#41803=CARTESIAN_POINT('Ctrl Pts',(144.018076334189,1.46504338618959,330.303026577236));
#41804=CARTESIAN_POINT('Ctrl Pts',(144.010318522667,1.33359512597675,330.264020304272));
#41805=CARTESIAN_POINT('Ctrl Pts',(144.002560711145,1.20064249065815,330.230551324091));
#41806=CARTESIAN_POINT('Ctrl Pts',(143.994808737622,1.0677899064138,330.197107530379));
#41807=CARTESIAN_POINT('Ctrl Pts',(143.987056764099,0.93343557795561,330.169192830299));
#41808=CARTESIAN_POINT('Ctrl Pts',(143.979304790576,0.798079171413243,330.146933680789));
#41809=CARTESIAN_POINT('Ctrl Pts',(143.971556100018,0.662780088389454,330.124683958043));
#41810=CARTESIAN_POINT('Ctrl Pts',(143.963807409461,0.526480156235899,330.108085085419));
#41811=CARTESIAN_POINT('Ctrl Pts',(143.956058718903,0.389689763655344,330.097212532589));
#41812=CARTESIAN_POINT('Ctrl Pts',(143.948311640525,0.252927831458461,330.086342241884));
#41813=CARTESIAN_POINT('Ctrl Pts',(143.940564562147,0.115676031208867,330.081195932127));
#41814=CARTESIAN_POINT('Ctrl Pts',(143.93281748377,-0.0215499804572701,
330.08179721231));
#41815=CARTESIAN_POINT('Ctrl Pts',(143.925070340464,-0.158777142209558,
330.082398497532));
#41816=CARTESIAN_POINT('Ctrl Pts',(143.917323197158,-0.295978124076759,
330.088747467059));
#41817=CARTESIAN_POINT('Ctrl Pts',(143.909576053852,-0.432637518377247,
330.100815594388));
#41818=CARTESIAN_POINT('Ctrl Pts',(143.901827168824,-0.569327636610888,
330.112886434888));
#41819=CARTESIAN_POINT('Ctrl Pts',(143.894078283796,-0.705475535705275,
330.130678957386));
#41820=CARTESIAN_POINT('Ctrl Pts',(143.886329398768,-0.840571571131002,
330.154112826705));
#41821=CARTESIAN_POINT('Ctrl Pts',(143.878572288993,-0.975810998884487,
330.177571568974));
#41822=CARTESIAN_POINT('Ctrl Pts',(143.870815179218,-1.10999594700619,330.206683552314));
#41823=CARTESIAN_POINT('Ctrl Pts',(143.863058069444,-1.24262705648704,330.241317297719));
#41824=CARTESIAN_POINT('Ctrl Pts',(143.855296814518,-1.37532903979217,330.27596955029));
#41825=CARTESIAN_POINT('Ctrl Pts',(143.847535559591,-1.50647515642764,330.316149329926));
#41826=CARTESIAN_POINT('Ctrl Pts',(143.839774304665,-1.6355827882982,330.361675733077));
#41827=CARTESIAN_POINT('Ctrl Pts',(143.832000634261,-1.76489695030359,330.407274963637));
#41828=CARTESIAN_POINT('Ctrl Pts',(143.824226963856,-1.89216574822349,330.458237763472));
#41829=CARTESIAN_POINT('Ctrl Pts',(143.816453293451,-2.01692725030957,330.514335330248));
#41830=CARTESIAN_POINT('Ctrl Pts',(143.809041489274,-2.13588107445724,330.567821541795));
#41831=CARTESIAN_POINT('Ctrl Pts',(143.801629685097,-2.25255552125887,330.625975103243));
#41832=CARTESIAN_POINT('Ctrl Pts',(143.79421788092,-2.36657388529132,330.688560436704));
#41833=CARTESIAN_POINT('Ctrl Pts',(143.786442802142,-2.48618062898853,330.754213263789));
#41834=CARTESIAN_POINT('Ctrl Pts',(143.778667723363,-2.60324232093219,330.824950751182));
#41835=CARTESIAN_POINT('Ctrl Pts',(143.770892644585,-2.71729652555157,330.900550932781));
#41836=CARTESIAN_POINT('Ctrl Pts',(143.763127133536,-2.83121037921096,330.976058083543));
#41837=CARTESIAN_POINT('Ctrl Pts',(143.755361622487,-2.94212378659893,331.056415808465));
#41838=CARTESIAN_POINT('Ctrl Pts',(143.747596111438,-3.04959823205991,331.141355978389));
#41839=CARTESIAN_POINT('Ctrl Pts',(143.739838299915,-3.15696611629546,331.226211929886));
#41840=CARTESIAN_POINT('Ctrl Pts',(143.732080488393,-3.26090151949346,331.315641043745));
#41841=CARTESIAN_POINT('Ctrl Pts',(143.724322676871,-3.36099459874852,331.409331765579));
#41842=CARTESIAN_POINT('Ctrl Pts',(143.716570703348,-3.46101235478711,331.502951982173));
#41843=CARTESIAN_POINT('Ctrl Pts',(143.708818729825,-3.55719325799698,331.600827157338));
#41844=CARTESIAN_POINT('Ctrl Pts',(143.701066756302,-3.64916057002648,331.702605544272));
#41845=CARTESIAN_POINT('Ctrl Pts',(143.693318065745,-3.74108893384489,331.804340827999));
#41846=CARTESIAN_POINT('Ctrl Pts',(143.685569375187,-3.82880699413227,331.909975746359));
#41847=CARTESIAN_POINT('Ctrl Pts',(143.677820684629,-3.91197508621941,332.019121943571));
#41848=CARTESIAN_POINT('Ctrl Pts',(143.670073606251,-3.99512587449037,332.128245432006));
#41849=CARTESIAN_POINT('Ctrl Pts',(143.662326527874,-4.07372834077822,332.24087843547));
#41850=CARTESIAN_POINT('Ctrl Pts',(143.654579449496,-4.1474835803845,332.356600103476));
#41851=CARTESIAN_POINT('Ctrl Pts',(143.64683230619,-4.22123943813074,332.472322741342));
#41852=CARTESIAN_POINT('Ctrl Pts',(143.639085162884,-4.29014777808469,332.591133765764));
#41853=CARTESIAN_POINT('Ctrl Pts',(143.631338019578,-4.35395367212233,332.712584322098));
#41854=CARTESIAN_POINT('Ctrl Pts',(143.62358913455,-4.4177739110794,332.834062183095));
#41855=CARTESIAN_POINT('Ctrl Pts',(143.615840249522,-4.47648923968823,332.95818041089));
#41856=CARTESIAN_POINT('Ctrl Pts',(143.608091364494,-4.52989141561629,333.08446696055));
#41857=CARTESIAN_POINT('Ctrl Pts',(143.600334254719,-4.58335027316575,333.210887552058));
#41858=CARTESIAN_POINT('Ctrl Pts',(143.592577144945,-4.63148456025762,333.339480702275));
#41859=CARTESIAN_POINT('Ctrl Pts',(143.58482003517,-4.67413460857986,333.46975533872));
#41860=CARTESIAN_POINT('Ctrl Pts',(143.577058780244,-4.71680744772426,333.600099589766));
#41861=CARTESIAN_POINT('Ctrl Pts',(143.569297525318,-4.75399010270507,333.7321267414));
#41862=CARTESIAN_POINT('Ctrl Pts',(143.561536270392,-4.78557352683102,333.86533305248));
#41863=CARTESIAN_POINT('Ctrl Pts',(143.553762599987,-4.81720747414253,333.998752450246));
#41864=CARTESIAN_POINT('Ctrl Pts',(143.545988929582,-4.84322421775455,334.133354392813));
#41865=CARTESIAN_POINT('Ctrl Pts',(143.538215259178,-4.86356618465578,334.268626613847));
#41866=CARTESIAN_POINT('Ctrl Pts',(143.530803455,-4.88296122810408,334.39760188045));
#41867=CARTESIAN_POINT('Ctrl Pts',(143.523391650823,-4.89719789557304,334.527186140858));
#41868=CARTESIAN_POINT('Ctrl Pts',(143.515979846646,-4.90627043261721,334.656935130732));
#41869=CARTESIAN_POINT('Ctrl Pts',(143.509498647261,-4.91420384803269,334.770393211023));
#41870=CARTESIAN_POINT('Ctrl Pts',(143.503017447875,-4.91820218909899,334.884129643691));
#41871=CARTESIAN_POINT('Ctrl Pts',(143.49653624849,-4.91824957381517,334.997952521813));
#41872=CARTESIAN_POINT('',(146.996536248541,-4.91824999353705,334.999747863625));
#41873=CARTESIAN_POINT('Ctrl Pts',(146.99653624849,-4.9182499935371,334.999747864535));
#41874=CARTESIAN_POINT('Ctrl Pts',(146.988451747308,-4.91825735260103,335.143296556126));
#41875=CARTESIAN_POINT('Ctrl Pts',(146.980367246126,-4.91197577165588,335.286734459456));
#41876=CARTESIAN_POINT('Ctrl Pts',(146.972282744944,-4.8994601760364,335.429503254858));
#41877=CARTESIAN_POINT('Ctrl Pts',(146.96418868747,-4.88692978634548,335.572440810247));
#41878=CARTESIAN_POINT('Ctrl Pts',(146.956094629996,-4.86815071007839,335.714707342739));
#41879=CARTESIAN_POINT('Ctrl Pts',(146.948000572523,-4.84322933887771,335.855752670772));
#41880=CARTESIAN_POINT('Ctrl Pts',(146.939888459662,-4.81825237565734,335.997112628149));
#41881=CARTESIAN_POINT('Ctrl Pts',(146.9317763468,-4.78710578379308,336.137245600314));
#41882=CARTESIAN_POINT('Ctrl Pts',(146.92366423394,-4.74994683805557,336.275612832385));
#41883=CARTESIAN_POINT('Ctrl Pts',(146.915542734325,-4.71274489465739,336.41414017307));
#41884=CARTESIAN_POINT('Ctrl Pts',(146.90742123471,-4.66951681702968,336.550897374038));
#41885=CARTESIAN_POINT('Ctrl Pts',(146.899299735095,-4.62046882424643,336.685363731266));
#41886=CARTESIAN_POINT('Ctrl Pts',(146.891159808995,-4.5713095487968,336.820135172839));
#41887=CARTESIAN_POINT('Ctrl Pts',(146.883019882894,-4.51630408411138,336.952605063933));
#41888=CARTESIAN_POINT('Ctrl Pts',(146.874879956794,-4.45570635164289,337.082273750118));
#41889=CARTESIAN_POINT('Ctrl Pts',(146.86819872384,-4.40596786973402,337.188705514793));
#41890=CARTESIAN_POINT('Ctrl Pts',(146.861517490887,-4.3524627314102,337.293250469534));
#41891=CARTESIAN_POINT('Ctrl Pts',(146.854836257933,-4.2953532843308,337.395646723807));
#41892=CARTESIAN_POINT('Ctrl Pts',(146.847061179155,-4.22889392673633,337.514807206478));
#41893=CARTESIAN_POINT('Ctrl Pts',(146.839286100376,-4.15736721850354,337.631388344973));
#41894=CARTESIAN_POINT('Ctrl Pts',(146.831511021598,-4.08099824474996,337.744929213814));
#41895=CARTESIAN_POINT('Ctrl Pts',(146.823745510549,-4.00472324788034,337.858330363387));
#41896=CARTESIAN_POINT('Ctrl Pts',(146.8159799995,-3.92361805769198,337.968698366077));
#41897=CARTESIAN_POINT('Ctrl Pts',(146.808214488451,-3.83795375971063,338.075596527639));
#41898=CARTESIAN_POINT('Ctrl Pts',(146.800456676929,-3.75237439813021,338.182388699362));
#41899=CARTESIAN_POINT('Ctrl Pts',(146.792698865406,-3.66224516740222,338.285717573409));
#41900=CARTESIAN_POINT('Ctrl Pts',(146.784941053884,-3.56788038358312,338.385175421));
#41901=CARTESIAN_POINT('Ctrl Pts',(146.777189080361,-3.47358661225655,338.484558423406));
#41902=CARTESIAN_POINT('Ctrl Pts',(146.769437106838,-3.37506390012999,338.580075915266));
#41903=CARTESIAN_POINT('Ctrl Pts',(146.761685133315,-3.27266653111475,338.671353543126));
#41904=CARTESIAN_POINT('Ctrl Pts',(146.753936442757,-3.17031252744598,338.762592514856));
#41905=CARTESIAN_POINT('Ctrl Pts',(146.7461877522,-3.06408742173266,338.849594934326));
#41906=CARTESIAN_POINT('Ctrl Pts',(146.738439061642,-2.95438185556877,338.932023768238));
#41907=CARTESIAN_POINT('Ctrl Pts',(146.730691983264,-2.84469911456428,339.014435452142));
#41908=CARTESIAN_POINT('Ctrl Pts',(146.722944904887,-2.73153766577113,339.092275208584));
#41909=CARTESIAN_POINT('Ctrl Pts',(146.715197826509,-2.61532036938624,339.16524698283));
#41910=CARTESIAN_POINT('Ctrl Pts',(146.707450683203,-2.49910209898838,339.23821936865));
#41911=CARTESIAN_POINT('Ctrl Pts',(146.699703539897,-2.37982826094574,339.306323483048));
#41912=CARTESIAN_POINT('Ctrl Pts',(146.691956396591,-2.25794942188029,339.369307436051));
#41913=CARTESIAN_POINT('Ctrl Pts',(146.684207511563,-2.13604318186429,339.432305549184));
#41914=CARTESIAN_POINT('Ctrl Pts',(146.676458626535,-2.01153112260807,339.490181030905));
#41915=CARTESIAN_POINT('Ctrl Pts',(146.668709741507,-1.88488668509718,339.542728832634));
#41916=CARTESIAN_POINT('Ctrl Pts',(146.660952631732,-1.75810782587179,339.595332409143));
#41917=CARTESIAN_POINT('Ctrl Pts',(146.653195521957,-1.62919242878137,339.64259685952));
#41918=CARTESIAN_POINT('Ctrl Pts',(146.645438412183,-1.49863263377112,339.684365836642));
#41919=CARTESIAN_POINT('Ctrl Pts',(146.637677157257,-1.36800307178104,339.726157133769));
#41920=CARTESIAN_POINT('Ctrl Pts',(146.62991590233,-1.23572773770935,339.762447002828));
#41921=CARTESIAN_POINT('Ctrl Pts',(146.622154647404,-1.10231109789111,339.793129802745));
#41922=CARTESIAN_POINT('Ctrl Pts',(146.614380977,-0.968681034929487,339.823861685143));
#41923=CARTESIAN_POINT('Ctrl Pts',(146.606607306595,-0.833906402363296,
339.848968503094));
#41924=CARTESIAN_POINT('Ctrl Pts',(146.59883363619,-0.698499843782523,339.868396145625));
#41925=CARTESIAN_POINT('Ctrl Pts',(146.591421832013,-0.569396493082272,
339.886919426722));
#41926=CARTESIAN_POINT('Ctrl Pts',(146.584010027836,-0.439719010975681,
339.900280335367));
#41927=CARTESIAN_POINT('Ctrl Pts',(146.576598223659,-0.309911690541216,
339.908476118569));
#41928=CARTESIAN_POINT('Ctrl Pts',(146.568823144881,-0.173742126654373,
339.91707360152));
#41929=CARTESIAN_POINT('Ctrl Pts',(146.561048066102,-0.0369993541179618,
339.920014010076));
#41930=CARTESIAN_POINT('Ctrl Pts',(146.553272987324,0.0998072185269236,
339.917237189889));
#41931=CARTESIAN_POINT('Ctrl Pts',(146.545507476275,0.236445441974683,339.914463786757));
#41932=CARTESIAN_POINT('Ctrl Pts',(146.537741965226,0.37314692226037,339.905987161194));
#41933=CARTESIAN_POINT('Ctrl Pts',(146.529976454177,0.509397733943853,339.89179895449));
#41934=CARTESIAN_POINT('Ctrl Pts',(146.522218642655,0.645513452550358,339.877624815435));
#41935=CARTESIAN_POINT('Ctrl Pts',(146.514460831133,0.781179005522254,339.85775040525));
#41936=CARTESIAN_POINT('Ctrl Pts',(146.506703019611,0.915881430575405,339.832219393573));
#41937=CARTESIAN_POINT('Ctrl Pts',(146.498951046088,1.05048248778232,339.806707594793));
#41938=CARTESIAN_POINT('Ctrl Pts',(146.491199072565,1.18412147722747,339.775547739914));
#41939=CARTESIAN_POINT('Ctrl Pts',(146.483447099042,1.31629187375136,339.738835169701));
#41940=CARTESIAN_POINT('Ctrl Pts',(146.475698408484,1.44840629603409,339.702138147283));
#41941=CARTESIAN_POINT('Ctrl Pts',(146.467949717926,1.5790529865786,339.659893191049));
#41942=CARTESIAN_POINT('Ctrl Pts',(146.460201027369,1.7077371283126,339.612246411791));
#41943=CARTESIAN_POINT('Ctrl Pts',(146.452453948991,1.83639449623608,339.564609545844));
#41944=CARTESIAN_POINT('Ctrl Pts',(146.444706870613,1.96308976121095,339.511573228015));
#41945=CARTESIAN_POINT('Ctrl Pts',(146.436959792235,2.08734513058017,339.453332838262));
#41946=CARTESIAN_POINT('Ctrl Pts',(146.429212648929,2.21160154132905,339.395091960398));
#41947=CARTESIAN_POINT('Ctrl Pts',(146.421465505624,2.33341766176053,339.331647089507));
#41948=CARTESIAN_POINT('Ctrl Pts',(146.413718362318,2.45233784476907,339.263240804554));
#41949=CARTESIAN_POINT('Ctrl Pts',(146.40596947729,2.57128476355967,339.194819140416));
#41950=CARTESIAN_POINT('Ctrl Pts',(146.398220592262,2.68733411062261,339.121434037493));
#41951=CARTESIAN_POINT('Ctrl Pts',(146.390471707234,2.80005725014844,339.043372658857));
#41952=CARTESIAN_POINT('Ctrl Pts',(146.382714597459,2.91290003517898,338.965228425067));
#41953=CARTESIAN_POINT('Ctrl Pts',(146.374957487684,3.02240923837369,338.882398223497));
#41954=CARTESIAN_POINT('Ctrl Pts',(146.367200377909,3.128187058937,338.795211296726));
#41955=CARTESIAN_POINT('Ctrl Pts',(146.359439122983,3.23402140378546,338.707977780049));
#41956=CARTESIAN_POINT('Ctrl Pts',(146.351677868057,3.33612010211076,338.616383160118));
#41957=CARTESIAN_POINT('Ctrl Pts',(146.343916613131,3.43412132240092,338.520794484989));
#41958=CARTESIAN_POINT('Ctrl Pts',(146.336142942726,3.53227931270499,338.425052899133));
#41959=CARTESIAN_POINT('Ctrl Pts',(146.328369272322,3.62632645859891,338.32530477514));
#41960=CARTESIAN_POINT('Ctrl Pts',(146.320595601917,3.71593983614847,338.221951923388));
#41961=CARTESIAN_POINT('Ctrl Pts',(146.31318379774,3.80138168941324,338.123410171751));
#41962=CARTESIAN_POINT('Ctrl Pts',(146.305771993563,3.88279308899692,338.021591964816));
#41963=CARTESIAN_POINT('Ctrl Pts',(146.298360189386,3.95993128737131,337.916869428308));
#41964=CARTESIAN_POINT('Ctrl Pts',(146.290585110607,4.04085025863102,337.807014128333));
#41965=CARTESIAN_POINT('Ctrl Pts',(146.282810031829,4.11732227143436,337.693615437419));
#41966=CARTESIAN_POINT('Ctrl Pts',(146.27503495305,4.18902107051601,337.577069175104));
#41967=CARTESIAN_POINT('Ctrl Pts',(146.267269442001,4.2606316396608,337.460666330386));
#41968=CARTESIAN_POINT('Ctrl Pts',(146.259503930952,4.32748047929625,337.341123950735));
#41969=CARTESIAN_POINT('Ctrl Pts',(146.251738419903,4.38928244585868,337.21886968364));
#41970=CARTESIAN_POINT('Ctrl Pts',(146.243980608381,4.45102313559127,337.096736632007));
#41971=CARTESIAN_POINT('Ctrl Pts',(146.236222796859,4.50772673526551,336.971897390471));
#41972=CARTESIAN_POINT('Ctrl Pts',(146.228464985337,4.55915237428648,336.844806952106));
#41973=CARTESIAN_POINT('Ctrl Pts',(146.220713011814,4.61053931388351,336.717812153326));
#41974=CARTESIAN_POINT('Ctrl Pts',(146.212961038291,4.65665605254184,336.588569890611));
#41975=CARTESIAN_POINT('Ctrl Pts',(146.205209064768,4.69730865451637,336.457557706132));
#41976=CARTESIAN_POINT('Ctrl Pts',(146.19746037421,4.73794404008971,336.326601005392));
#41977=CARTESIAN_POINT('Ctrl Pts',(146.189711683653,4.77311977589454,336.193876246255));
#41978=CARTESIAN_POINT('Ctrl Pts',(146.181962993095,4.80269095570401,336.059878599887));
#41979=CARTESIAN_POINT('Ctrl Pts',(146.174215914717,4.83225598298247,335.925908832849));
#41980=CARTESIAN_POINT('Ctrl Pts',(146.166468836339,4.85621868949043,335.790667086807));
#41981=CARTESIAN_POINT('Ctrl Pts',(146.158721757961,4.87448481337984,335.654660879104));
#41982=CARTESIAN_POINT('Ctrl Pts',(146.150974614656,4.89275109035697,335.518653531538));
#41983=CARTESIAN_POINT('Ctrl Pts',(146.14322747135,4.90532063746016,335.381882096929));
#41984=CARTESIAN_POINT('Ctrl Pts',(146.135480328044,4.91215086772375,335.244861012047));
#41985=CARTESIAN_POINT('Ctrl Pts',(146.127731443016,4.91898263356812,335.107809121916));
#41986=CARTESIAN_POINT('Ctrl Pts',(146.119982557988,4.92007249552335,334.970507860139));
#41987=CARTESIAN_POINT('Ctrl Pts',(146.11223367296,4.91542997571179,334.833473076129));
#41988=CARTESIAN_POINT('Ctrl Pts',(146.104476563185,4.91078252828173,334.696292841983));
#41989=CARTESIAN_POINT('Ctrl Pts',(146.09671945341,4.90039055816213,334.559380041875));
#41990=CARTESIAN_POINT('Ctrl Pts',(146.088962343636,4.88431565962564,334.423247367032));
#41991=CARTESIAN_POINT('Ctrl Pts',(146.081201088709,4.86823217117733,334.28704194724));
#41992=CARTESIAN_POINT('Ctrl Pts',(146.073439833783,4.84645976527734,334.151617869095));
#41993=CARTESIAN_POINT('Ctrl Pts',(146.065678578857,4.81911129267469,334.0174780352));
#41994=CARTESIAN_POINT('Ctrl Pts',(146.057904908452,4.79171907142872,333.883123621286));
#41995=CARTESIAN_POINT('Ctrl Pts',(146.050131238048,4.75873305299711,333.750057936457));
#41996=CARTESIAN_POINT('Ctrl Pts',(146.042357567643,4.7203163756295,333.61876997699));
#41997=CARTESIAN_POINT('Ctrl Pts',(146.034945763466,4.6836880038361,333.493593503623));
#41998=CARTESIAN_POINT('Ctrl Pts',(146.027533959289,4.64212328112795,333.370033246777));
#41999=CARTESIAN_POINT('Ctrl Pts',(146.020122155112,4.59580377135082,333.248494716612));
#42000=CARTESIAN_POINT('Ctrl Pts',(146.012347076334,4.54721400442055,333.120999221037));
#42001=CARTESIAN_POINT('Ctrl Pts',(146.004571997555,4.49323802006642,332.995325735542));
#42002=CARTESIAN_POINT('Ctrl Pts',(145.996796918777,4.43403211594032,332.871962815807));
#42003=CARTESIAN_POINT('Ctrl Pts',(145.989031407728,4.37489906844865,332.748751701998));
#42004=CARTESIAN_POINT('Ctrl Pts',(145.981265896679,4.31054907398809,332.627845845622));
#42005=CARTESIAN_POINT('Ctrl Pts',(145.97350038563,4.24118744291114,332.509716454579));
#42006=CARTESIAN_POINT('Ctrl Pts',(145.965742574108,4.17189458409309,332.391704189172));
#42007=CARTESIAN_POINT('Ctrl Pts',(145.957984762585,4.09760017399217,332.276463245618));
#42008=CARTESIAN_POINT('Ctrl Pts',(145.950226951063,4.01855647709236,332.1644424));
#42009=CARTESIAN_POINT('Ctrl Pts',(145.94247497754,3.93957226308123,332.052505853621));
#42010=CARTESIAN_POINT('Ctrl Pts',(145.934723004017,3.85584610056792,331.943784899952));
#42011=CARTESIAN_POINT('Ctrl Pts',(145.926971030494,3.76767461519253,331.838701049168));
#42012=CARTESIAN_POINT('Ctrl Pts',(145.919222339937,3.67954047049339,331.733661701457));
#42013=CARTESIAN_POINT('Ctrl Pts',(145.911473649379,3.58696499800371,331.632256691863));
#42014=CARTESIAN_POINT('Ctrl Pts',(145.903724958821,3.49028618064765,331.534875840654));
#42015=CARTESIAN_POINT('Ctrl Pts',(145.895977880443,3.39362747812715,331.437515250346));
#42016=CARTESIAN_POINT('Ctrl Pts',(145.888230802066,3.29286740409521,331.344177430268));
#42017=CARTESIAN_POINT('Ctrl Pts',(145.880483723688,3.18838173021944,331.255216293976));
#42018=CARTESIAN_POINT('Ctrl Pts',(145.872736580382,3.08389518065287,331.166254412104));
#42019=CARTESIAN_POINT('Ctrl Pts',(145.864989437076,2.97568326657754,331.081669540575));
#42020=CARTESIAN_POINT('Ctrl Pts',(145.85724229377,2.86415554259743,331.001775882931));
#42021=CARTESIAN_POINT('Ctrl Pts',(145.849493408742,2.75260274481735,330.921864263498));
#42022=CARTESIAN_POINT('Ctrl Pts',(145.841744523714,2.63773297143534,330.846646184236));
#42023=CARTESIAN_POINT('Ctrl Pts',(145.833995638686,2.51998516419439,330.776392793507));
#42024=CARTESIAN_POINT('Ctrl Pts',(145.826238528911,2.40211237821431,330.706064835103));
#42025=CARTESIAN_POINT('Ctrl Pts',(145.818481419137,2.28135579237415,330.640712292286));
#42026=CARTESIAN_POINT('Ctrl Pts',(145.810724309362,2.15817987185988,330.58056081576));
#42027=CARTESIAN_POINT('Ctrl Pts',(145.802963054436,2.03493813007217,330.520377196207));
#42028=CARTESIAN_POINT('Ctrl Pts',(145.79520179951,1.90927483548139,330.465400337506));
#42029=CARTESIAN_POINT('Ctrl Pts',(145.787440544583,1.78167395963085,330.415807490509));
#42030=CARTESIAN_POINT('Ctrl Pts',(145.779666874179,1.65386896396384,330.366135311119));
#42031=CARTESIAN_POINT('Ctrl Pts',(145.771893203774,1.52412056344867,330.321864480375));
#42032=CARTESIAN_POINT('Ctrl Pts',(145.764119533369,1.392928248955,330.283122435788));
#42033=CARTESIAN_POINT('Ctrl Pts',(145.756707729192,1.26784296826336,330.246183842697));
#42034=CARTESIAN_POINT('Ctrl Pts',(145.749295925015,1.14144545579727,330.214270959902));
#42035=CARTESIAN_POINT('Ctrl Pts',(145.741884120838,1.0141749683151,330.187450551304));
#42036=CARTESIAN_POINT('Ctrl Pts',(145.73410904206,0.880666575122889,330.159315594587));
#42037=CARTESIAN_POINT('Ctrl Pts',(145.726333963281,0.745775557768737,330.136696017214));
#42038=CARTESIAN_POINT('Ctrl Pts',(145.718558884503,0.609997334773571,330.119724770664));
#42039=CARTESIAN_POINT('Ctrl Pts',(145.710793373454,0.474386195525958,330.102774408314));
#42040=CARTESIAN_POINT('Ctrl Pts',(145.703027862405,0.337890407081227,330.091458595041));
#42041=CARTESIAN_POINT('Ctrl Pts',(145.695262351356,0.201017323427911,330.085859678623));
#42042=CARTESIAN_POINT('Ctrl Pts',(145.687504539833,0.0642799498357178,
330.080266313547));
#42043=CARTESIAN_POINT('Ctrl Pts',(145.679746728311,-0.0728335864743402,
330.080378580922));
#42044=CARTESIAN_POINT('Ctrl Pts',(145.671988916789,-0.209809385332896,
330.08622720465));
#42045=CARTESIAN_POINT('Ctrl Pts',(145.664236943266,-0.346682105559385,
330.092071427103));
#42046=CARTESIAN_POINT('Ctrl Pts',(145.656484969743,-0.483416905702162,
330.103643396942));
#42047=CARTESIAN_POINT('Ctrl Pts',(145.64873299622,-0.619498807707696,330.120921778681));
#42048=CARTESIAN_POINT('Ctrl Pts',(145.640984305662,-0.755523078946614,
330.138192843015));
#42049=CARTESIAN_POINT('Ctrl Pts',(145.633235615105,-0.89089461503863,330.161165463533));
#42050=CARTESIAN_POINT('Ctrl Pts',(145.625486924547,-1.02510270584944,330.189766377299));
#42051=CARTESIAN_POINT('Ctrl Pts',(145.617739846169,-1.15928287354639,330.218361340406));
#42052=CARTESIAN_POINT('Ctrl Pts',(145.609992767792,-1.29229969539579,330.252582186115));
#42053=CARTESIAN_POINT('Ctrl Pts',(145.602245689414,-1.42365220632738,330.292304442945));
#42054=CARTESIAN_POINT('Ctrl Pts',(145.594498546108,-1.55500581811904,330.332027032685));
#42055=CARTESIAN_POINT('Ctrl Pts',(145.586751402802,-1.68469471703088,330.377251012368));
#42056=CARTESIAN_POINT('Ctrl Pts',(145.579004259496,-1.81223304910432,330.427802012354));
#42057=CARTESIAN_POINT('Ctrl Pts',(145.571255374468,-1.93980005450287,330.478364377279));
#42058=CARTESIAN_POINT('Ctrl Pts',(145.56350648944,-2.06521516766474,330.534256001654));
#42059=CARTESIAN_POINT('Ctrl Pts',(145.555757604412,-2.18801283758504,330.59525450394));
#42060=CARTESIAN_POINT('Ctrl Pts',(145.548000494637,-2.31094084622089,330.656317750666));
#42061=CARTESIAN_POINT('Ctrl Pts',(145.540243384862,-2.43124551132059,330.722498529082));
#42062=CARTESIAN_POINT('Ctrl Pts',(145.532486275088,-2.54848572963048,330.793528373046));
#42063=CARTESIAN_POINT('Ctrl Pts',(145.524725020162,-2.66578859736462,330.864596173088));
#42064=CARTESIAN_POINT('Ctrl Pts',(145.516963765235,-2.78002342998789,330.940517985603));
#42065=CARTESIAN_POINT('Ctrl Pts',(145.509202510309,-2.89077926870459,331.020982749205));
#42066=CARTESIAN_POINT('Ctrl Pts',(145.501428839905,-3.00171228066773,331.101576230204));
#42067=CARTESIAN_POINT('Ctrl Pts',(145.4936551695,-3.10915487119704,331.186726941483));
#42068=CARTESIAN_POINT('Ctrl Pts',(145.485881499095,-3.21272957220138,331.276083814262));
#42069=CARTESIAN_POINT('Ctrl Pts',(145.478469694918,-3.31148284595504,331.361281103115));
#42070=CARTESIAN_POINT('Ctrl Pts',(145.471057890741,-3.40672001661188,331.450301575878));
#42071=CARTESIAN_POINT('Ctrl Pts',(145.463646086564,-3.49814723394469,331.54281198195));
#42072=CARTESIAN_POINT('Ctrl Pts',(145.455976271731,-3.59275710367367,331.63854274706));
#42073=CARTESIAN_POINT('Ctrl Pts',(145.448306456898,-3.68360372780343,331.73833168146));
#42074=CARTESIAN_POINT('Ctrl Pts',(145.440636642065,-3.77031161777008,331.841846525672));
#42075=CARTESIAN_POINT('Ctrl Pts',(145.432976460366,-3.8569106043599,331.945231357309));
#42076=CARTESIAN_POINT('Ctrl Pts',(145.425316278667,-3.93938093917433,332.052332486302));
#42077=CARTESIAN_POINT('Ctrl Pts',(145.417656096968,-4.0173827889169,332.162779777702));
#42078=CARTESIAN_POINT('Ctrl Pts',(145.410004775819,-4.09529441373516,332.273099314459));
#42079=CARTESIAN_POINT('Ctrl Pts',(145.40235345467,-4.16874761186798,332.386756982264));
#42080=CARTESIAN_POINT('Ctrl Pts',(145.394702133522,-4.2374422648968,332.503349020354));
#42081=CARTESIAN_POINT('Ctrl Pts',(145.387055773642,-4.306092374942,332.619865457841));
#42082=CARTESIAN_POINT('Ctrl Pts',(145.379409413763,-4.36998987136978,332.739312137212));
#42083=CARTESIAN_POINT('Ctrl Pts',(145.371763053884,-4.42887756327229,332.861255837637));
#42084=CARTESIAN_POINT('Ctrl Pts',(145.364119890709,-4.48774063606745,332.983148557203));
#42085=CARTESIAN_POINT('Ctrl Pts',(145.356476727534,-4.54159789544213,333.107535859778));
#42086=CARTESIAN_POINT('Ctrl Pts',(145.348833564359,-4.59023805793477,333.233959900232));
#42087=CARTESIAN_POINT('Ctrl Pts',(145.341191836263,-4.63886908776217,333.36036020334));
#42088=CARTESIAN_POINT('Ctrl Pts',(145.333550108167,-4.68228482634771,333.488796107685));
#42089=CARTESIAN_POINT('Ctrl Pts',(145.32590838007,-4.72032231776672,333.618790284246));
#42090=CARTESIAN_POINT('Ctrl Pts',(145.318263816003,-4.75837392552262,333.748832703777));
#42091=CARTESIAN_POINT('Ctrl Pts',(145.310619251937,-4.7910431831734,333.880434165006));
#42092=CARTESIAN_POINT('Ctrl Pts',(145.30297468787,-4.8182171885484,334.013102747761));
#42093=CARTESIAN_POINT('Ctrl Pts',(145.295328537929,-4.84539683120244,334.145798852768));
#42094=CARTESIAN_POINT('Ctrl Pts',(145.287682387988,-4.86707888188329,334.279562123726));
#42095=CARTESIAN_POINT('Ctrl Pts',(145.280036238048,-4.88320188790053,334.413892173312));
#42096=CARTESIAN_POINT('Ctrl Pts',(145.272383494346,-4.89933879781132,334.548338064244));
#42097=CARTESIAN_POINT('Ctrl Pts',(145.264730750644,-4.90990705633585,334.683351308939));
#42098=CARTESIAN_POINT('Ctrl Pts',(145.257078006942,-4.91489722135088,334.818428069192));
#42099=CARTESIAN_POINT('Ctrl Pts',(145.253564087473,-4.91718856138322,334.880451426591));
#42100=CARTESIAN_POINT('Ctrl Pts',(145.250050168003,-4.91830455064958,334.942488182909));
#42101=CARTESIAN_POINT('Ctrl Pts',(145.246536248534,-4.91824795069328,335.004489766291));
#42102=CARTESIAN_POINT('',(148.746536238457,-4.91925759883339,334.995611705565));
#42103=CARTESIAN_POINT('Ctrl Pts',(148.746536220508,-4.91824804336388,334.995612922681));
#42104=CARTESIAN_POINT('Ctrl Pts',(148.73888721855,-4.91836834981328,335.130485621825));
#42105=CARTESIAN_POINT('Ctrl Pts',(148.731238216592,-4.91293658427382,335.265537890568));
#42106=CARTESIAN_POINT('Ctrl Pts',(148.723589214634,-4.90193520133637,335.400267840826));
#42107=CARTESIAN_POINT('Ctrl Pts',(148.715946577363,-4.89094297258105,335.534885683133));
#42108=CARTESIAN_POINT('Ctrl Pts',(148.708303940092,-4.87439037787505,335.669181340703));
#42109=CARTESIAN_POINT('Ctrl Pts',(148.700661302821,-4.85231193471425,335.802653069968));
#42110=CARTESIAN_POINT('Ctrl Pts',(148.693022560317,-4.83024474295622,335.936056780662));
#42111=CARTESIAN_POINT('Ctrl Pts',(148.685383817813,-4.80265736764482,336.068637001217));
#42112=CARTESIAN_POINT('Ctrl Pts',(148.677745075309,-4.76963611017469,336.199897678562));
#42113=CARTESIAN_POINT('Ctrl Pts',(148.670108245621,-4.73662312154852,336.331125486957));
#42114=CARTESIAN_POINT('Ctrl Pts',(148.662471415932,-4.69817905405275,336.461034018351));
#42115=CARTESIAN_POINT('Ctrl Pts',(148.654834586243,-4.65444109706652,336.589138488754));
#42116=CARTESIAN_POINT('Ctrl Pts',(148.647197904936,-4.61070398989816,336.717240470118));
#42117=CARTESIAN_POINT('Ctrl Pts',(148.639561223629,-4.56167332821842,336.843538078707));
#42118=CARTESIAN_POINT('Ctrl Pts',(148.631924542323,-4.50753566578765,336.967563285933));
#42119=CARTESIAN_POINT('Ctrl Pts',(148.624286245292,-4.4533865492329,337.091614733674));
#42120=CARTESIAN_POINT('Ctrl Pts',(148.616647948262,-4.39412844508063,337.213392454829));
#42121=CARTESIAN_POINT('Ctrl Pts',(148.609009651231,-4.32999514183211,337.332450456968));
#42122=CARTESIAN_POINT('Ctrl Pts',(148.601363531302,-4.2657961553142,337.451630394489));
#42123=CARTESIAN_POINT('Ctrl Pts',(148.593717411373,-4.19671219166365,337.568084696027));
#42124=CARTESIAN_POINT('Ctrl Pts',(148.586071291445,-4.12302206393855,337.681393690374));
#42125=CARTESIAN_POINT('Ctrl Pts',(148.57842097385,-4.04929148085525,337.794764890556));
#42126=CARTESIAN_POINT('Ctrl Pts',(148.570770656255,-3.97094993260759,337.904987017903));
#42127=CARTESIAN_POINT('Ctrl Pts',(148.563120338661,-3.88831747903655,338.011672333558));
#42128=CARTESIAN_POINT('Ctrl Pts',(148.555458493911,-3.8055605185951,338.118518397856));
#42129=CARTESIAN_POINT('Ctrl Pts',(148.547796649162,-3.71850000186133,338.221816701511));
#42130=CARTESIAN_POINT('Ctrl Pts',(148.540134804412,-3.62749423183861,338.32121493741));
#42131=CARTESIAN_POINT('Ctrl Pts',(148.5348446908,-3.56465938220769,338.389844357334));
#42132=CARTESIAN_POINT('Ctrl Pts',(148.529554577189,-3.49994452278994,338.45661531508));
#42133=CARTESIAN_POINT('Ctrl Pts',(148.524264463577,-3.43347664954062,338.521423172463));
#42134=CARTESIAN_POINT('Ctrl Pts',(148.516489384798,-3.33578631835186,338.616673715949));
#42135=CARTESIAN_POINT('Ctrl Pts',(148.50871430602,-3.23397499366961,338.708006546902));
#42136=CARTESIAN_POINT('Ctrl Pts',(148.500939227242,-3.1283898944596,338.795044101291));
#42137=CARTESIAN_POINT('Ctrl Pts',(148.493173716193,-3.02293472443598,338.881974550428));
#42138=CARTESIAN_POINT('Ctrl Pts',(148.485408205144,-2.91371531857904,338.964619993602));
#42139=CARTESIAN_POINT('Ctrl Pts',(148.477642694094,-2.80111607251189,339.042639213536));
#42140=CARTESIAN_POINT('Ctrl Pts',(148.469884882572,-2.68862846892532,339.120581077185));
#42141=CARTESIAN_POINT('Ctrl Pts',(148.46212707105,-2.57276801326575,339.193905624628));
#42142=CARTESIAN_POINT('Ctrl Pts',(148.454369259528,-2.45395227251279,339.262311732702));
#42143=CARTESIAN_POINT('Ctrl Pts',(148.446617286005,-2.33522594437226,339.33066636301));
#42144=CARTESIAN_POINT('Ctrl Pts',(148.438865312482,-2.21354909517373,339.394109726928));
#42145=CARTESIAN_POINT('Ctrl Pts',(148.431113338959,-2.08936807816185,339.4523840913));
#42146=CARTESIAN_POINT('Ctrl Pts',(148.423364648401,-1.96523965188457,339.510633776443));
#42147=CARTESIAN_POINT('Ctrl Pts',(148.415615957844,-1.83860952020017,339.56371865025));
#42148=CARTESIAN_POINT('Ctrl Pts',(148.407867267286,-1.70994823712798,339.611427120626));
#42149=CARTESIAN_POINT('Ctrl Pts',(148.400120188908,-1.58131372311037,339.659125664856));
#42150=CARTESIAN_POINT('Ctrl Pts',(148.39237311053,-1.45064926454198,339.70144989483));
#42151=CARTESIAN_POINT('Ctrl Pts',(148.384626032152,-1.31844460550187,339.738236685173));
#42152=CARTESIAN_POINT('Ctrl Pts',(148.376878888847,-1.18623883845948,339.775023783825));
#42153=CARTESIAN_POINT('Ctrl Pts',(148.369131745541,-1.05249322176654,339.806273245497));
#42154=CARTESIAN_POINT('Ctrl Pts',(148.361384602235,-0.917711455959071,
339.831872178163));
#42155=CARTESIAN_POINT('Ctrl Pts',(148.353635717207,-0.782899388349155,
339.857476866011));
#42156=CARTESIAN_POINT('Ctrl Pts',(148.345886832179,-0.647051092018016,
339.877428424061));
#42157=CARTESIAN_POINT('Ctrl Pts',(148.338137947151,-0.510678829123992,
339.891665380623));
#42158=CARTESIAN_POINT('Ctrl Pts',(148.330380837376,-0.374161819301003,
339.905917448438));
#42159=CARTESIAN_POINT('Ctrl Pts',(148.322623727601,-0.237120121341795,
339.914442757636));
#42160=CARTESIAN_POINT('Ctrl Pts',(148.314866617827,-0.100070026504685,
339.91723184854));
#42161=CARTESIAN_POINT('Ctrl Pts',(148.3071053629,0.0370533035209075,339.920022429845));
#42162=CARTESIAN_POINT('Ctrl Pts',(148.299344107974,0.174184648779658,339.917070693474));
#42163=CARTESIAN_POINT('Ctrl Pts',(148.291582853048,0.310810368535273,339.908419295182));
#42164=CARTESIAN_POINT('Ctrl Pts',(148.283809182643,0.447654644916372,339.899754057471));
#42165=CARTESIAN_POINT('Ctrl Pts',(148.276035512239,0.583991290578826,339.885370979202));
#42166=CARTESIAN_POINT('Ctrl Pts',(148.268261841834,0.719313527112632,339.865364437759));
#42167=CARTESIAN_POINT('Ctrl Pts',(148.260850037657,0.848336480977584,339.846289205634));
#42168=CARTESIAN_POINT('Ctrl Pts',(148.25343823348,0.976437059057399,339.822102326113));
#42169=CARTESIAN_POINT('Ctrl Pts',(148.246026429303,1.10318864407574,339.79292790245));
#42170=CARTESIAN_POINT('Ctrl Pts',(148.238251350525,1.23615270185096,339.762323553377));
#42171=CARTESIAN_POINT('Ctrl Pts',(148.230476271746,1.36805237761787,339.726133673908));
#42172=CARTESIAN_POINT('Ctrl Pts',(148.222701192968,1.49838226962256,339.684445926316));
#42173=CARTESIAN_POINT('Ctrl Pts',(148.214935681919,1.62855178239806,339.642809478152));
#42174=CARTESIAN_POINT('Ctrl Pts',(148.20717017087,1.75715498624406,339.595688741169));
#42175=CARTESIAN_POINT('Ctrl Pts',(148.199404659821,1.88369692574338,339.5432223096));
#42176=CARTESIAN_POINT('Ctrl Pts',(148.191646848298,2.01011339854131,339.49080789865));
#42177=CARTESIAN_POINT('Ctrl Pts',(148.183889036776,2.1344723154265,339.433058489694));
#42178=CARTESIAN_POINT('Ctrl Pts',(148.176131225254,2.25629448605361,339.370162268693));
#42179=CARTESIAN_POINT('Ctrl Pts',(148.168379251731,2.37802498163404,339.307313379092));
#42180=CARTESIAN_POINT('Ctrl Pts',(148.160627278208,2.49722218477479,339.239325565334));
#42181=CARTESIAN_POINT('Ctrl Pts',(148.152875304685,2.6134278148142,339.166434701187));
#42182=CARTESIAN_POINT('Ctrl Pts',(148.145126614127,2.72958423170021,339.093574706364));
#42183=CARTESIAN_POINT('Ctrl Pts',(148.13737792357,2.84275126489012,339.015815998321));
#42184=CARTESIAN_POINT('Ctrl Pts',(148.129629233012,2.95249633829824,338.93343977135));
#42185=CARTESIAN_POINT('Ctrl Pts',(148.121882154634,3.06221857832727,338.85108068344));
#42186=CARTESIAN_POINT('Ctrl Pts',(148.114135076256,3.16851996231689,338.764106222029));
#42187=CARTESIAN_POINT('Ctrl Pts',(148.106387997879,3.27099828603664,338.672839946859));
#42188=CARTESIAN_POINT('Ctrl Pts',(148.098640854573,3.37347746862351,338.581572906791));
#42189=CARTESIAN_POINT('Ctrl Pts',(148.090893711267,3.47213323513621,338.48601424118));
#42190=CARTESIAN_POINT('Ctrl Pts',(148.083146567961,3.56659807099842,338.386526430201));
#42191=CARTESIAN_POINT('Ctrl Pts',(148.075397682933,3.66108414456091,338.28701625225));
#42192=CARTESIAN_POINT('Ctrl Pts',(148.067648797905,3.75137714349083,338.18357545455));
#42193=CARTESIAN_POINT('Ctrl Pts',(148.059899912877,3.83714816048657,338.07660154342));
#42194=CARTESIAN_POINT('Ctrl Pts',(148.052142803102,3.92301021572605,337.969514089075));
#42195=CARTESIAN_POINT('Ctrl Pts',(148.044385693327,4.00434045632674,337.858886335594));
#42196=CARTESIAN_POINT('Ctrl Pts',(148.036628583553,4.08085153261982,337.745147324137));
#42197=CARTESIAN_POINT('Ctrl Pts',(148.028867328626,4.15740349398574,337.631347534188));
#42198=CARTESIAN_POINT('Ctrl Pts',(148.0211060737,4.22913095541315,337.51443350647));
#42199=CARTESIAN_POINT('Ctrl Pts',(148.013344818774,4.29579182656153,337.394860255912));
#42200=CARTESIAN_POINT('Ctrl Pts',(148.005571148369,4.36255933337902,337.275095727122));
#42201=CARTESIAN_POINT('Ctrl Pts',(147.997797477965,4.42424387797575,337.152663824218));
#42202=CARTESIAN_POINT('Ctrl Pts',(147.99002380756,4.48065057743245,337.028041780993));
#42203=CARTESIAN_POINT('Ctrl Pts',(147.982612003383,4.53443153145845,336.909220923864));
#42204=CARTESIAN_POINT('Ctrl Pts',(147.975200199206,4.58341484167304,336.788409506498));
#42205=CARTESIAN_POINT('Ctrl Pts',(147.967788395029,4.62747400206407,336.666033439857));
#42206=CARTESIAN_POINT('Ctrl Pts',(147.96001331625,4.67369263315157,336.537659357649));
#42207=CARTESIAN_POINT('Ctrl Pts',(147.952238237472,4.71463827438773,336.407157685985));
#42208=CARTESIAN_POINT('Ctrl Pts',(147.944463158694,4.75011114096031,336.275000867068));
#42209=CARTESIAN_POINT('Ctrl Pts',(147.936697647645,4.78554035591227,336.14300667553));
#42210=CARTESIAN_POINT('Ctrl Pts',(147.928932136596,4.81551009575784,336.009361763219));
#42211=CARTESIAN_POINT('Ctrl Pts',(147.921166625547,4.8398690585666,335.874557349995));
#42212=CARTESIAN_POINT('Ctrl Pts',(147.913408814024,4.86420386939277,335.739886595739));
#42213=CARTESIAN_POINT('Ctrl Pts',(147.905651002502,4.88293890501215,335.604059010603));
#42214=CARTESIAN_POINT('Ctrl Pts',(147.89789319098,4.89597309762072,335.467579394193));
#42215=CARTESIAN_POINT('Ctrl Pts',(147.890141217457,4.90899748158607,335.331202483022));
#42216=CARTESIAN_POINT('Ctrl Pts',(147.882389243934,4.91632952469463,335.194174904776));
#42217=CARTESIAN_POINT('Ctrl Pts',(147.874637270411,4.91791957626672,335.057009682271));
#42218=CARTESIAN_POINT('Ctrl Pts',(147.866888579853,4.91950895445101,334.919902549318));
#42219=CARTESIAN_POINT('Ctrl Pts',(147.859139889296,4.91536117313067,334.782658278081));
#42220=CARTESIAN_POINT('Ctrl Pts',(147.851391198738,4.90547860284268,334.645792801382));
#42221=CARTESIAN_POINT('Ctrl Pts',(147.84364412036,4.89559808870599,334.50895580069));
#42222=CARTESIAN_POINT('Ctrl Pts',(147.835897041982,4.87998518703533,334.372497827389));
#42223=CARTESIAN_POINT('Ctrl Pts',(147.828149963605,4.85869433033462,334.236932200342));
#42224=CARTESIAN_POINT('Ctrl Pts',(147.820402820299,4.83740329519608,334.101365437126));
#42225=CARTESIAN_POINT('Ctrl Pts',(147.812655676993,4.81043427075645,333.96669142122));
#42226=CARTESIAN_POINT('Ctrl Pts',(147.804908533687,4.77789319110129,333.833415362296));
#42227=CARTESIAN_POINT('Ctrl Pts',(147.797159648659,4.74534479552042,333.700109340083));
#42228=CARTESIAN_POINT('Ctrl Pts',(147.789410763631,4.70722194465379,333.568202279898));
#42229=CARTESIAN_POINT('Ctrl Pts',(147.781661878603,4.66368091943255,333.438185880388));
#42230=CARTESIAN_POINT('Ctrl Pts',(147.773904768828,4.62009367931724,333.308031480127));
#42231=CARTESIAN_POINT('Ctrl Pts',(147.766147659054,4.57107690119268,333.179772120473));
#42232=CARTESIAN_POINT('Ctrl Pts',(147.758390549279,4.51683587352932,333.053881618683));
#42233=CARTESIAN_POINT('Ctrl Pts',(147.750629294353,4.46256586119521,332.927923845035));
#42234=CARTESIAN_POINT('Ctrl Pts',(147.742868039426,4.403066206135,332.804337803558));
#42235=CARTESIAN_POINT('Ctrl Pts',(147.7351067845,4.3385885311362,332.683573307874));
#42236=CARTESIAN_POINT('Ctrl Pts',(147.727333114096,4.27400771287057,332.562615628354));
#42237=CARTESIAN_POINT('Ctrl Pts',(147.719559443691,4.20443316028766,332.444488851017));
#42238=CARTESIAN_POINT('Ctrl Pts',(147.711785773286,4.13016072713749,332.32961511566));
#42239=CARTESIAN_POINT('Ctrl Pts',(147.704373969109,4.05934569361944,332.220088780321));
#42240=CARTESIAN_POINT('Ctrl Pts',(147.696962164932,3.98426047517631,332.113519679653));
#42241=CARTESIAN_POINT('Ctrl Pts',(147.689550360755,3.90519476976026,332.010244680122));
#42242=CARTESIAN_POINT('Ctrl Pts',(147.681775281977,3.82225381859714,331.901907865224));
#42243=CARTESIAN_POINT('Ctrl Pts',(147.674000203198,3.73467021469701,331.79685385925));
#42244=CARTESIAN_POINT('Ctrl Pts',(147.66622512442,3.64273312976269,331.695506331096));
#42245=CARTESIAN_POINT('Ctrl Pts',(147.658459613371,3.55090917926433,331.594283517527));
#42246=CARTESIAN_POINT('Ctrl Pts',(147.650694102322,3.4547426672061,331.496758393319));
#42247=CARTESIAN_POINT('Ctrl Pts',(147.642928591273,3.35456479269266,331.403324018746));
#42248=CARTESIAN_POINT('Ctrl Pts',(147.635170779751,3.25448624483407,331.309982284629));
#42249=CARTESIAN_POINT('Ctrl Pts',(147.627412968229,3.15040453352937,331.22072349338));
#42250=CARTESIAN_POINT('Ctrl Pts',(147.619655156706,3.04268946194786,331.135905811105));
#42251=CARTESIAN_POINT('Ctrl Pts',(147.611903183183,2.93505544937278,331.051151956825));
#42252=CARTESIAN_POINT('Ctrl Pts',(147.60415120966,2.82379382470928,330.970832800123));
#42253=CARTESIAN_POINT('Ctrl Pts',(147.596399236137,2.70930913095551,330.895267719397));
#42254=CARTESIAN_POINT('Ctrl Pts',(147.58865054558,2.59487292153776,330.819734640528));
#42255=CARTESIAN_POINT('Ctrl Pts',(147.580901855022,2.47721668340389,330.748951848088));
#42256=CARTESIAN_POINT('Ctrl Pts',(147.573153164465,2.35677555830677,330.683196549498));
#42257=CARTESIAN_POINT('Ctrl Pts',(147.565406086087,2.23635949199171,330.617454931846));
#42258=CARTESIAN_POINT('Ctrl Pts',(147.557659007709,2.11316003407813,330.556738914638));
#42259=CARTESIAN_POINT('Ctrl Pts',(147.549911929331,1.98763830189889,330.501280510709));
#42260=CARTESIAN_POINT('Ctrl Pts',(147.542164786025,1.86211551772689,330.445821641986));
#42261=CARTESIAN_POINT('Ctrl Pts',(147.53441764272,1.73427077800145,330.395620632396));
#42262=CARTESIAN_POINT('Ctrl Pts',(147.526670499414,1.60458625132328,330.350861797648));
#42263=CARTESIAN_POINT('Ctrl Pts',(147.518921614386,1.47487256881032,330.306092900165));
#42264=CARTESIAN_POINT('Ctrl Pts',(147.511172729358,1.34331864569536,330.266768739683));
#42265=CARTESIAN_POINT('Ctrl Pts',(147.50342384433,1.21042253443848,330.233023982584));
#42266=CARTESIAN_POINT('Ctrl Pts',(147.495666734555,1.07738536587563,330.199243408451));
#42267=CARTESIAN_POINT('Ctrl Pts',(147.48790962478,0.943003542824317,330.171054163873));
#42268=CARTESIAN_POINT('Ctrl Pts',(147.480152515006,0.807786601694979,330.148540027103));
#42269=CARTESIAN_POINT('Ctrl Pts',(147.472391260079,0.672497404955977,330.126013859498));
#42270=CARTESIAN_POINT('Ctrl Pts',(147.464630005153,0.536372588643611,330.109168890399));
#42271=CARTESIAN_POINT('Ctrl Pts',(147.456868750227,0.399926578155264,330.098036944796));
#42272=CARTESIAN_POINT('Ctrl Pts',(147.449095079823,0.263262298517647,330.086887191708));
#42273=CARTESIAN_POINT('Ctrl Pts',(147.441321409418,0.12627618874179,330.081468739953));
#42274=CARTESIAN_POINT('Ctrl Pts',(147.433547739013,-0.0105166613726054,
330.081761243866));
#42275=CARTESIAN_POINT('Ctrl Pts',(147.426135934836,-0.140941771405292,
330.082040131652));
#42276=CARTESIAN_POINT('Ctrl Pts',(147.418724130659,-0.271190921798768,
330.087510238409));
#42277=CARTESIAN_POINT('Ctrl Pts',(147.411312326482,-0.400824062171299,
330.098110248722));
#42278=CARTESIAN_POINT('Ctrl Pts',(147.403537247703,-0.536810908909002,
330.109229797116));
#42279=CARTESIAN_POINT('Ctrl Pts',(147.395762168925,-0.672549577378057,
330.12602996752));
#42280=CARTESIAN_POINT('Ctrl Pts',(147.387987090146,-0.807527307964116,
330.148496860828));
#42281=CARTESIAN_POINT('Ctrl Pts',(147.380221579097,-0.94233893985986,330.170936107195));
#42282=CARTESIAN_POINT('Ctrl Pts',(147.372456068048,-1.07639111512157,330.199028138108));
#42283=CARTESIAN_POINT('Ctrl Pts',(147.364690556999,-1.20917407013934,330.232707148643));
#42284=CARTESIAN_POINT('Ctrl Pts',(147.356932745477,-1.34182537047099,330.266352766341));
#42285=CARTESIAN_POINT('Ctrl Pts',(147.349174933955,-1.47320957848017,330.30557424425));
#42286=CARTESIAN_POINT('Ctrl Pts',(147.341417122433,-1.60282538293446,330.350254431227));
#42287=CARTESIAN_POINT('Ctrl Pts',(147.33366514891,-1.7323436473856,330.394900994947));
#42288=CARTESIAN_POINT('Ctrl Pts',(147.325913175387,-1.86009578908672,330.444997964386));
#42289=CARTESIAN_POINT('Ctrl Pts',(147.318161201864,-1.98559431450014,330.500377984683));
#42290=CARTESIAN_POINT('Ctrl Pts',(147.310412511306,-2.1110396912131,330.555734551509));
#42291=CARTESIAN_POINT('Ctrl Pts',(147.302663820748,-2.23423299302842,330.616369561736));
#42292=CARTESIAN_POINT('Ctrl Pts',(147.294915130191,-2.35470563014128,330.682067108224));
#42293=CARTESIAN_POINT('Ctrl Pts',(147.287168051813,-2.47515320191574,330.747750985788));
#42294=CARTESIAN_POINT('Ctrl Pts',(147.279420973435,-2.5928808919661,330.818495117497));
#42295=CARTESIAN_POINT('Ctrl Pts',(147.271673895057,-2.70744405870082,330.894037295407));
#42296=CARTESIAN_POINT('Ctrl Pts',(147.263926751751,-2.82200818558557,330.969580106434));
#42297=CARTESIAN_POINT('Ctrl Pts',(147.256179608446,-2.93340740993668,331.049920828695));
#42298=CARTESIAN_POINT('Ctrl Pts',(147.24843246514,-3.04122580764633,331.134753740134));
#42299=CARTESIAN_POINT('Ctrl Pts',(147.240683580112,-3.14906844522087,331.219605723813));
#42300=CARTESIAN_POINT('Ctrl Pts',(147.232934695083,-3.25332834707508,331.308951664684));
#42301=CARTESIAN_POINT('Ctrl Pts',(147.225185810055,-3.35362274461133,331.402445615515));
#42302=CARTESIAN_POINT('Ctrl Pts',(147.21742870028,-3.45402359565694,331.496038801791));
#42303=CARTESIAN_POINT('Ctrl Pts',(147.209671590506,-3.55045024809324,331.593788525966));
#42304=CARTESIAN_POINT('Ctrl Pts',(147.201914480731,-3.64255651161291,331.695311645222));
#42305=CARTESIAN_POINT('Ctrl Pts',(147.194153225805,-3.73471199377463,331.796889015186));
#42306=CARTESIAN_POINT('Ctrl Pts',(147.186391970879,-3.82254223660822,331.902243497975));
#42307=CARTESIAN_POINT('Ctrl Pts',(147.178630715953,-3.90574209270071,332.010959724626));
#42308=CARTESIAN_POINT('Ctrl Pts',(147.170857045548,-3.98907504144831,332.11984986181));
#42309=CARTESIAN_POINT('Ctrl Pts',(147.163083375143,-4.06776257738746,332.232112168836));
#42310=CARTESIAN_POINT('Ctrl Pts',(147.155309704739,-4.14154306497522,332.347302485496));
#42311=CARTESIAN_POINT('Ctrl Pts',(147.147897900562,-4.21188905311404,332.457130665201));
#42312=CARTESIAN_POINT('Ctrl Pts',(147.140486096385,-4.27777441261324,332.569620143148));
#42313=CARTESIAN_POINT('Ctrl Pts',(147.133074292208,-4.33901256840172,332.684367690295));
#42314=CARTESIAN_POINT('Ctrl Pts',(147.124864295878,-4.40684558479657,332.811472632412));
#42315=CARTESIAN_POINT('Ctrl Pts',(147.116654299549,-4.46917147454035,332.94171328728));
#42316=CARTESIAN_POINT('Ctrl Pts',(147.108444303219,-4.52570597472449,333.074599134507));
#42317=CARTESIAN_POINT('Ctrl Pts',(147.100248947627,-4.58213965795952,333.207248008811));
#42318=CARTESIAN_POINT('Ctrl Pts',(147.092053592035,-4.63280240618409,333.342532376197));
#42319=CARTESIAN_POINT('Ctrl Pts',(147.083858236443,-4.67745572456991,333.479937169987));
#42320=CARTESIAN_POINT('Ctrl Pts',(147.07568251851,-4.72200204495912,333.617012715286));
#42321=CARTESIAN_POINT('Ctrl Pts',(147.067506800577,-4.76056755098082,333.756198245452));
#42322=CARTESIAN_POINT('Ctrl Pts',(147.059331082644,-4.79296201278595,333.896959562622));
#42323=CARTESIAN_POINT('Ctrl Pts',(147.051167168358,-4.82530970526421,334.037517656411));
#42324=CARTESIAN_POINT('Ctrl Pts',(147.043003254073,-4.85150403160578,334.179646688232));
#42325=CARTESIAN_POINT('Ctrl Pts',(147.034839339788,-4.87140414900122,334.322796426771));
#42326=CARTESIAN_POINT('Ctrl Pts',(147.026691107238,-4.89126604106112,334.465671194733));
#42327=CARTESIAN_POINT('Ctrl Pts',(147.018542874687,-4.90485778798851,334.609562437749));
#42328=CARTESIAN_POINT('Ctrl Pts',(147.010394642137,-4.91208942193594,334.753909420324));
#42329=CARTESIAN_POINT('Ctrl Pts',(147.005775177605,-4.91618924067846,334.835743825784));
#42330=CARTESIAN_POINT('Ctrl Pts',(147.001155713073,-4.91824578857046,334.917724486486));
#42331=CARTESIAN_POINT('Ctrl Pts',(146.996536248541,-4.91824999353705,334.999747863625));
#42332=CARTESIAN_POINT('',(150.496536287082,-4.92151798553658,335.002527853233));
#42333=CARTESIAN_POINT('Ctrl Pts',(150.49653624849,-4.92474948212452,335.002530191525));
#42334=CARTESIAN_POINT('Ctrl Pts',(150.488334400158,-4.92565302976486,335.146822327));
#42335=CARTESIAN_POINT('Ctrl Pts',(150.387386540402,-4.85438643557772,336.921856051074));
#42336=CARTESIAN_POINT('Ctrl Pts',(150.193692669221,-2.70353245624263,340.149306858644));
#42337=CARTESIAN_POINT('Ctrl Pts',(149.915454634947,2.86712545234502,340.060043528167));
#42338=CARTESIAN_POINT('Ctrl Pts',(149.637216600673,5.80666465201795,335.327252938012));
#42339=CARTESIAN_POINT('Ctrl Pts',(149.358978566399,3.41751340676379,330.294147156888));
#42340=CARTESIAN_POINT('Ctrl Pts',(149.080740532125,-2.10783944946231,329.579533071615));
#42341=CARTESIAN_POINT('Ctrl Pts',(148.876593092822,-4.74262473034225,332.704915984254));
#42342=CARTESIAN_POINT('Ctrl Pts',(148.765191664944,-4.92286447585139,334.666557075651));
#42343=CARTESIAN_POINT('Ctrl Pts',(148.74653624849,-4.91982192786215,334.995611025212));
#42344=CARTESIAN_POINT('',(152.246536248436,-4.91824906311658,335.003035729386));
#42345=CARTESIAN_POINT('Ctrl Pts',(152.246536248436,-4.91824906311658,335.003035729386));
#42346=CARTESIAN_POINT('Ctrl Pts',(152.237771470162,-4.91815313595883,335.158449336348));
#42347=CARTESIAN_POINT('Ctrl Pts',(152.229006691887,-4.91068658036438,335.313587684498));
#42348=CARTESIAN_POINT('Ctrl Pts',(152.220241913612,-4.89595254032275,335.467794597454));
#42349=CARTESIAN_POINT('Ctrl Pts',(152.211507220859,-4.8812690755803,335.621472187785));
#42350=CARTESIAN_POINT('Ctrl Pts',(152.202772528106,-4.85936810387403,335.774224550554));
#42351=CARTESIAN_POINT('Ctrl Pts',(152.194037835353,-4.83040182517022,335.925419510218));
#42352=CARTESIAN_POINT('Ctrl Pts',(152.185256280418,-4.80128014053808,336.07742564046));
#42353=CARTESIAN_POINT('Ctrl Pts',(152.176474725482,-4.7650172323429,336.227857418963));
#42354=CARTESIAN_POINT('Ctrl Pts',(152.167693170547,-4.72181658489604,336.376092729833));
#42355=CARTESIAN_POINT('Ctrl Pts',(152.158915083411,-4.678632997204,336.5242695032));
#42356=CARTESIAN_POINT('Ctrl Pts',(152.150136996275,-4.62851729139738,336.67025138024));
#42357=CARTESIAN_POINT('Ctrl Pts',(152.141358909139,-4.57171947922819,336.813439843432));
#42358=CARTESIAN_POINT('Ctrl Pts',(152.13358383036,-4.52141154115342,336.940267199348));
#42359=CARTESIAN_POINT('Ctrl Pts',(152.125808751582,-4.46574249469378,337.06519993769));
#42360=CARTESIAN_POINT('Ctrl Pts',(152.118033672803,-4.4048752241667,337.187751659129));
#42361=CARTESIAN_POINT('Ctrl Pts',(152.110268161754,-4.344082854691,337.310152572873));
#42362=CARTESIAN_POINT('Ctrl Pts',(152.102502650705,-4.27810516104536,337.430177952832));
#42363=CARTESIAN_POINT('Ctrl Pts',(152.094737139656,-4.20715380138612,337.54735940809));
#42364=CARTESIAN_POINT('Ctrl Pts',(152.086979328134,-4.1362727902066,337.664424677593));
#42365=CARTESIAN_POINT('Ctrl Pts',(152.079221516612,-4.06042812793231,337.778651301669));
#42366=CARTESIAN_POINT('Ctrl Pts',(152.07146370509,-3.97987811948626,337.889593953575));
#42367=CARTESIAN_POINT('Ctrl Pts',(152.063711731567,-3.89938872747609,338.000453117616));
#42368=CARTESIAN_POINT('Ctrl Pts',(152.055959758044,-3.8142012660504,338.10803291345));
#42369=CARTESIAN_POINT('Ctrl Pts',(152.048207784521,-3.72461802884623,338.21191587712));
#42370=CARTESIAN_POINT('Ctrl Pts',(152.040459093963,-3.63507273019601,338.315754846293));
#42371=CARTESIAN_POINT('Ctrl Pts',(152.032710403405,-3.54113561311906,338.415899801796));
#42372=CARTESIAN_POINT('Ctrl Pts',(152.024961712848,-3.44314989659545,338.511965525468));
#42373=CARTESIAN_POINT('Ctrl Pts',(152.01721463447,-3.34518456681849,338.608011261864));
#42374=CARTESIAN_POINT('Ctrl Pts',(152.009467556092,-3.24317259201413,338.69997918112));
#42375=CARTESIAN_POINT('Ctrl Pts',(152.001720477714,-3.13749449131678,338.787520479081));
#42376=CARTESIAN_POINT('Ctrl Pts',(151.993973334408,-3.03181550493526,338.875062510722));
#42377=CARTESIAN_POINT('Ctrl Pts',(151.986226191103,-2.92247063238652,338.958177597719));
#42378=CARTESIAN_POINT('Ctrl Pts',(151.978479047797,-2.80987363613107,339.036557098751));
#42379=CARTESIAN_POINT('Ctrl Pts',(151.970730162769,-2.69725132568067,339.114954221158));
#42380=CARTESIAN_POINT('Ctrl Pts',(151.962981277741,-2.58137575736353,339.188613415776));
#42381=CARTESIAN_POINT('Ctrl Pts',(151.955232392713,-2.46268949637323,339.257269489585));
#42382=CARTESIAN_POINT('Ctrl Pts',(151.947475282938,-2.34387726055889,339.325998435661));
#42383=CARTESIAN_POINT('Ctrl Pts',(151.939718173163,-2.22224871153101,339.389713456949));
#42384=CARTESIAN_POINT('Ctrl Pts',(151.931961063388,-2.09827132087224,339.448195198786));
#42385=CARTESIAN_POINT('Ctrl Pts',(151.924199808462,-1.97422768065998,339.506708191396));
#42386=CARTESIAN_POINT('Ctrl Pts',(151.916438553536,-1.84783305783023,339.559982180544));
#42387=CARTESIAN_POINT('Ctrl Pts',(151.90867729861,-1.71957377460646,339.607846470553));
#42388=CARTESIAN_POINT('Ctrl Pts',(151.900903628205,-1.59110931832913,339.655787327826));
#42389=CARTESIAN_POINT('Ctrl Pts',(151.893129957801,-1.46077461284239,339.698301071917));
#42390=CARTESIAN_POINT('Ctrl Pts',(151.885356287396,-1.32907082524571,339.735267025626));
#42391=CARTESIAN_POINT('Ctrl Pts',(151.877944483219,-1.20349788064487,339.770512205297));
#42392=CARTESIAN_POINT('Ctrl Pts',(151.870532679042,-1.07668072700208,339.800714403701));
#42393=CARTESIAN_POINT('Ctrl Pts',(151.863120874864,-0.949059483035493,
339.825812797878));
#42394=CARTESIAN_POINT('Ctrl Pts',(151.855345796086,-0.815183141740809,
339.852141339117));
#42395=CARTESIAN_POINT('Ctrl Pts',(151.847570717307,-0.679998821417218,
339.872936323657));
#42396=CARTESIAN_POINT('Ctrl Pts',(151.839795638529,-0.544003691687033,
339.888071505812));
#42397=CARTESIAN_POINT('Ctrl Pts',(151.83203012748,-0.408175912621808,339.903188063161));
#42398=CARTESIAN_POINT('Ctrl Pts',(151.824264616431,-0.271539694153764,
339.912658633153));
#42399=CARTESIAN_POINT('Ctrl Pts',(151.816499105382,-0.13460345657086,339.916407730445));
#42400=CARTESIAN_POINT('Ctrl Pts',(151.80874129386,0.00219700833375552,
339.920153110496));
#42401=CARTESIAN_POINT('Ctrl Pts',(151.800983482338,0.139296512160548,339.918188296525));
#42402=CARTESIAN_POINT('Ctrl Pts',(151.793225670815,0.276180786534392,339.910489510797));
#42403=CARTESIAN_POINT('Ctrl Pts',(151.785473697292,0.41296205115092,339.90279651865));
#42404=CARTESIAN_POINT('Ctrl Pts',(151.777721723769,0.54952802001571,339.889378165396));
#42405=CARTESIAN_POINT('Ctrl Pts',(151.769969750246,0.685364050348281,339.870262742501));
#42406=CARTESIAN_POINT('Ctrl Pts',(151.762221059689,0.821142554041314,339.851155414999));
#42407=CARTESIAN_POINT('Ctrl Pts',(151.754472369131,0.95619134778373,339.826355870927));
#42408=CARTESIAN_POINT('Ctrl Pts',(151.746723678574,1.09000075792248,339.795944266798));
#42409=CARTESIAN_POINT('Ctrl Pts',(151.738976600196,1.22378232789584,339.765538990056));
#42410=CARTESIAN_POINT('Ctrl Pts',(151.731229521818,1.35632464626067,339.729524062341));
#42411=CARTESIAN_POINT('Ctrl Pts',(151.72348244344,1.48712847542296,339.688030712366));
#42412=CARTESIAN_POINT('Ctrl Pts',(151.715735300134,1.61793340084729,339.646537014637));
#42413=CARTESIAN_POINT('Ctrl Pts',(151.707988156829,1.74699943542992,339.599564921257));
#42414=CARTESIAN_POINT('Ctrl Pts',(151.700241013523,1.87384312548903,339.547295350377));
#42415=CARTESIAN_POINT('Ctrl Pts',(151.692492128495,2.00071533270255,339.495014028187));
#42416=CARTESIAN_POINT('Ctrl Pts',(151.684743243467,2.12536383986188,339.437433007463));
#42417=CARTESIAN_POINT('Ctrl Pts',(151.676994358438,2.24732614308001,339.374780939559));
#42418=CARTESIAN_POINT('Ctrl Pts',(151.669237248664,2.369417898347,339.312062372102));
#42419=CARTESIAN_POINT('Ctrl Pts',(151.661480138889,2.48881740597233,339.244262184379));
#42420=CARTESIAN_POINT('Ctrl Pts',(151.653723029114,2.60508723024303,339.171654777822));
#42421=CARTESIAN_POINT('Ctrl Pts',(151.645961774188,2.72141918539019,339.099008572188));
#42422=CARTESIAN_POINT('Ctrl Pts',(151.638200519262,2.83461780235072,339.021550249728));
#42423=CARTESIAN_POINT('Ctrl Pts',(151.630439264336,2.94427636262732,338.939596395949));
#42424=CARTESIAN_POINT('Ctrl Pts',(151.622665593931,3.05411034086269,338.857511442713));
#42425=CARTESIAN_POINT('Ctrl Pts',(151.614891923527,3.1603926430021,338.770916834665));
#42426=CARTESIAN_POINT('Ctrl Pts',(151.607118253122,3.26275057874034,338.680168708555));
#42427=CARTESIAN_POINT('Ctrl Pts',(151.599706448945,3.36034372794295,338.59364492955));
#42428=CARTESIAN_POINT('Ctrl Pts',(151.592294644768,3.45436943951627,338.503345822087));
#42429=CARTESIAN_POINT('Ctrl Pts',(151.584882840591,3.54453839264294,338.409608576594));
#42430=CARTESIAN_POINT('Ctrl Pts',(151.577107761812,3.63912679476281,338.311276989468));
#42431=CARTESIAN_POINT('Ctrl Pts',(151.569332683034,3.72976973350651,338.208850969828));
#42432=CARTESIAN_POINT('Ctrl Pts',(151.561557604256,3.81609199917105,338.10268027943));
#42433=CARTESIAN_POINT('Ctrl Pts',(151.553792093207,3.90230803979211,337.996640238825));
#42434=CARTESIAN_POINT('Ctrl Pts',(151.546026582158,3.98421374214145,337.886864996553));
#42435=CARTESIAN_POINT('Ctrl Pts',(151.538261071109,4.06147049359346,337.773741244631));
#42436=CARTESIAN_POINT('Ctrl Pts',(151.530503259587,4.13865064475154,337.660729655239));
#42437=CARTESIAN_POINT('Ctrl Pts',(151.522745448064,4.21119079905411,337.544376484));
#42438=CARTESIAN_POINT('Ctrl Pts',(151.514987636542,4.27879266117119,337.425101322668));
#42439=CARTESIAN_POINT('Ctrl Pts',(151.507235663019,4.34634365074317,337.305915919678));
#42440=CARTESIAN_POINT('Ctrl Pts',(151.499483689496,4.40896355312974,337.183813242061));
#42441=CARTESIAN_POINT('Ctrl Pts',(151.491731715973,4.46639765649051,337.059241374049));
#42442=CARTESIAN_POINT('Ctrl Pts',(151.483983025416,4.52380743647445,336.934722262297));
#42443=CARTESIAN_POINT('Ctrl Pts',(151.476234334858,4.57603562218161,336.807736394205));
#42444=CARTESIAN_POINT('Ctrl Pts',(151.4684856443,4.62287380527458,336.678755742509));
#42445=CARTESIAN_POINT('Ctrl Pts',(151.460738565922,4.66970224329234,336.549801926315));
#42446=CARTESIAN_POINT('Ctrl Pts',(151.452991487545,4.71114277597546,336.418854519213));
#42447=CARTESIAN_POINT('Ctrl Pts',(151.445244409167,4.74703559024165,336.286404356133));
#42448=CARTESIAN_POINT('Ctrl Pts',(151.437497265861,4.78292870532418,336.153953082994));
#42449=CARTESIAN_POINT('Ctrl Pts',(151.429750122555,4.81327390701554,336.019999406025));
#42450=CARTESIAN_POINT('Ctrl Pts',(151.422002979249,4.83796170872064,335.885047776932));
#42451=CARTESIAN_POINT('Ctrl Pts',(151.414254094221,4.86265506076768,335.750065807849));
#42452=CARTESIAN_POINT('Ctrl Pts',(151.406505209193,4.88168841155758,335.614085824607));
#42453=CARTESIAN_POINT('Ctrl Pts',(151.398756324165,4.89500375150042,335.477620492961));
#42454=CARTESIAN_POINT('Ctrl Pts',(151.39099921439,4.90833322448267,335.341010315603));
#42455=CARTESIAN_POINT('Ctrl Pts',(151.383242104616,4.9159325248913,335.203914150413));
#42456=CARTESIAN_POINT('Ctrl Pts',(151.375484994841,4.91779568118029,335.066848340776));
#42457=CARTESIAN_POINT('Ctrl Pts',(151.367723739915,4.91965983308043,334.929709287552));
#42458=CARTESIAN_POINT('Ctrl Pts',(151.359962484989,4.9157817441957,334.792601012723));
#42459=CARTESIAN_POINT('Ctrl Pts',(151.352201230063,4.90620753931681,334.656036857133));
#42460=CARTESIAN_POINT('Ctrl Pts',(151.344427559658,4.89661801883033,334.5192542434));
#42461=CARTESIAN_POINT('Ctrl Pts',(151.336653889253,4.88131421767315,334.383017876885));
#42462=CARTESIAN_POINT('Ctrl Pts',(151.328880218849,4.8603939347265,334.247833886848));
#42463=CARTESIAN_POINT('Ctrl Pts',(151.321468414671,4.84044749598381,334.118942744068));
#42464=CARTESIAN_POINT('Ctrl Pts',(151.314056610494,4.81539575779751,333.991008488843));
#42465=CARTESIAN_POINT('Ctrl Pts',(151.306644806317,4.78536570269473,333.864456890306));
#42466=CARTESIAN_POINT('Ctrl Pts',(151.298869727538,4.7538637851369,333.73170262095));
#42467=CARTESIAN_POINT('Ctrl Pts',(151.29109464876,4.71678365530317,333.600050443547));
#42468=CARTESIAN_POINT('Ctrl Pts',(151.283319569982,4.67421638781622,333.470005156097));
#42469=CARTESIAN_POINT('Ctrl Pts',(151.275554058933,4.63170150206187,333.340119897652));
#42470=CARTESIAN_POINT('Ctrl Pts',(151.267788547884,4.5837130341727,333.21183796267));
#42471=CARTESIAN_POINT('Ctrl Pts',(151.260023036835,4.53039291899408,333.085653358969));
#42472=CARTESIAN_POINT('Ctrl Pts',(151.252265225312,4.47712567086492,332.959593867669));
#42473=CARTESIAN_POINT('Ctrl Pts',(151.24450741379,4.41853744673061,332.835627927039));
#42474=CARTESIAN_POINT('Ctrl Pts',(151.236749602268,4.35481966552782,332.714233445158));
#42475=CARTESIAN_POINT('Ctrl Pts',(151.228997628745,4.29114983397599,332.592930316475));
#42476=CARTESIAN_POINT('Ctrl Pts',(151.221245655222,4.22235830973238,332.474195139512));
#42477=CARTESIAN_POINT('Ctrl Pts',(151.213493681699,4.14868405719308,332.35848459098));
#42478=CARTESIAN_POINT('Ctrl Pts',(151.205744991141,4.07504100574346,332.242823045933));
#42479=CARTESIAN_POINT('Ctrl Pts',(151.197996300584,3.99651954827849,332.13018391066));
#42480=CARTESIAN_POINT('Ctrl Pts',(151.190247610026,3.91340379503152,332.020997851707));
#42481=CARTESIAN_POINT('Ctrl Pts',(151.182500531648,3.83030533471121,331.911834509826));
#42482=CARTESIAN_POINT('Ctrl Pts',(151.17475345327,3.74261471653039,331.806123126054));
#42483=CARTESIAN_POINT('Ctrl Pts',(151.167006374892,3.65065821002524,331.704263709567));
#42484=CARTESIAN_POINT('Ctrl Pts',(151.159259231587,3.55870093283603,331.6024034394));
#42485=CARTESIAN_POINT('Ctrl Pts',(151.151512088281,3.46247795793816,331.504395491043));
#42486=CARTESIAN_POINT('Ctrl Pts',(151.143764944975,3.36235424005557,331.410604921873));
#42487=CARTESIAN_POINT('Ctrl Pts',(151.136016059947,3.26220801223553,331.316793266592));
#42488=CARTESIAN_POINT('Ctrl Pts',(151.128267174919,3.15815958156755,331.227201144393));
#42489=CARTESIAN_POINT('Ctrl Pts',(151.120518289891,3.0506086673033,331.142154769632));
#42490=CARTESIAN_POINT('Ctrl Pts',(151.112761180116,2.94294359738744,331.05701812577));
#42491=CARTESIAN_POINT('Ctrl Pts',(151.105004070341,2.83176892475961,330.976437110372));
#42492=CARTESIAN_POINT('Ctrl Pts',(151.097246960566,2.71751562204035,330.900696168071));
#42493=CARTESIAN_POINT('Ctrl Pts',(151.08948570564,2.60320126600928,330.824914752232));
#42494=CARTESIAN_POINT('Ctrl Pts',(151.081724450714,2.48580533620802,330.75397876513));
#42495=CARTESIAN_POINT('Ctrl Pts',(151.073963195788,2.36578447267566,330.68812721763));
#42496=CARTESIAN_POINT('Ctrl Pts',(151.066189525383,2.24557161487636,330.622170329115));
#42497=CARTESIAN_POINT('Ctrl Pts',(151.058415854978,2.12272578286044,330.561314306838));
#42498=CARTESIAN_POINT('Ctrl Pts',(151.050642184574,1.99772551610582,330.505750805218));
#42499=CARTESIAN_POINT('Ctrl Pts',(151.043230380397,1.87854404184419,330.452773797967));
#42500=CARTESIAN_POINT('Ctrl Pts',(151.03581857622,1.75740446427026,330.404607772696));
#42501=CARTESIAN_POINT('Ctrl Pts',(151.028406772043,1.63473353926475,330.361376355199));
#42502=CARTESIAN_POINT('Ctrl Pts',(151.020631693264,1.50605014680464,330.31602603715));
#42503=CARTESIAN_POINT('Ctrl Pts',(151.012856614486,1.37527483624023,330.275962962004));
#42504=CARTESIAN_POINT('Ctrl Pts',(151.005081535708,1.24288138868291,330.241383718331));
#42505=CARTESIAN_POINT('Ctrl Pts',(150.997316024659,1.11065085969133,330.206847026618));
#42506=CARTESIAN_POINT('Ctrl Pts',(150.98955051361,0.976806530237054,330.17778083722));
#42507=CARTESIAN_POINT('Ctrl Pts',(150.98178500256,0.841840631123751,330.154333130075));
#42508=CARTESIAN_POINT('Ctrl Pts',(150.974027191038,0.707008551092452,330.1309086714));
#42509=CARTESIAN_POINT('Ctrl Pts',(150.966269379516,0.571057497048823,330.11309167536));
#42510=CARTESIAN_POINT('Ctrl Pts',(150.958511567994,0.434492939863328,330.100979797173));
#42511=CARTESIAN_POINT('Ctrl Pts',(150.950759594471,0.298031151837965,330.088877033558));
#42512=CARTESIAN_POINT('Ctrl Pts',(150.943007620948,0.160957167401659,330.08247087662));
#42513=CARTESIAN_POINT('Ctrl Pts',(150.935255647425,0.0237843330877862,
330.08180751007));
#42514=CARTESIAN_POINT('Ctrl Pts',(150.927506956867,-0.113330408449408,
330.081144424457));
#42515=CARTESIAN_POINT('Ctrl Pts',(150.91975826631,-0.250543526545395,330.086219293893));
#42516=CARTESIAN_POINT('Ctrl Pts',(150.912009575752,-0.387339116163727,
330.097026262401));
#42517=CARTESIAN_POINT('Ctrl Pts',(150.904262497374,-0.524106244317147,
330.107830982429));
#42518=CARTESIAN_POINT('Ctrl Pts',(150.896515418996,-0.660455627368479,
330.124365398577));
#42519=CARTESIAN_POINT('Ctrl Pts',(150.888768340618,-0.795874325900693,
330.14657161175));
#42520=CARTESIAN_POINT('Ctrl Pts',(150.881021197313,-0.931294159371987,
330.168778011032));
#42521=CARTESIAN_POINT('Ctrl Pts',(150.873274054007,-1.06578290704377,330.1966562389));
#42522=CARTESIAN_POINT('Ctrl Pts',(150.865526910701,-1.19883608643651,330.230096950633));
#42523=CARTESIAN_POINT('Ctrl Pts',(150.857778025673,-1.3319191790086,330.263545180549));
#42524=CARTESIAN_POINT('Ctrl Pts',(150.850029140645,-1.46356568206226,330.302558287556));
#42525=CARTESIAN_POINT('Ctrl Pts',(150.842280255617,-1.59328496396169,330.346976672516));
#42526=CARTESIAN_POINT('Ctrl Pts',(150.834523145842,-1.72314193124734,330.391442203608));
#42527=CARTESIAN_POINT('Ctrl Pts',(150.826766036067,-1.85106722077621,330.441324346459));
#42528=CARTESIAN_POINT('Ctrl Pts',(150.819008926292,-1.97658841297388,330.496414616309));
#42529=CARTESIAN_POINT('Ctrl Pts',(150.811247671366,-2.10217667968327,330.551534324638));
#42530=CARTESIAN_POINT('Ctrl Pts',(150.80348641644,-2.22535793838321,330.611867533612));
#42531=CARTESIAN_POINT('Ctrl Pts',(150.795725161514,-2.34568408561011,330.677159587376));
#42532=CARTESIAN_POINT('Ctrl Pts',(150.787951491109,-2.46620271545834,330.742556087147));
#42533=CARTESIAN_POINT('Ctrl Pts',(150.780177820705,-2.58385677149312,330.812927082518));
#42534=CARTESIAN_POINT('Ctrl Pts',(150.7724041503,-2.69822612225555,330.887973874636));
#42535=CARTESIAN_POINT('Ctrl Pts',(150.764992346123,-2.80727155222481,330.959527220526));
#42536=CARTESIAN_POINT('Ctrl Pts',(150.757580541946,-2.91333096686714,331.035330675669));
#42537=CARTESIAN_POINT('Ctrl Pts',(150.750168737769,-3.01606946452102,331.115092272951));
#42538=CARTESIAN_POINT('Ctrl Pts',(150.742483981885,-3.12259147393376,331.197791220381));
#42539=CARTESIAN_POINT('Ctrl Pts',(150.734799226001,-3.22589699379611,331.285020276609));
#42540=CARTESIAN_POINT('Ctrl Pts',(150.727114470118,-3.3255695308752,331.376497501337));
#42541=CARTESIAN_POINT('Ctrl Pts',(150.719439211367,-3.42511888859246,331.467861674803));
#42542=CARTESIAN_POINT('Ctrl Pts',(150.711763952616,-3.52104390063296,331.563463307134));
#42543=CARTESIAN_POINT('Ctrl Pts',(150.704088693865,-3.61295851277673,331.662978296826));
#42544=CARTESIAN_POINT('Ctrl Pts',(150.696420980401,-3.7047827667819,331.762395456706));
#42545=CARTESIAN_POINT('Ctrl Pts',(150.688753266937,-3.79260419319596,331.865718028775));
#42546=CARTESIAN_POINT('Ctrl Pts',(150.681085553473,-3.87607157639534,331.972583246865));
#42547=CARTESIAN_POINT('Ctrl Pts',(150.673396002333,-3.95977667500354,332.079752817483));
#42548=CARTESIAN_POINT('Ctrl Pts',(150.665706451194,-4.03910259183008,332.190484969602));
#42549=CARTESIAN_POINT('Ctrl Pts',(150.658016900054,-4.11373364393594,332.30437788827));
#42550=CARTESIAN_POINT('Ctrl Pts',(150.650357840518,-4.1880687593316,332.417819183991));
#42551=CARTESIAN_POINT('Ctrl Pts',(150.642698780982,-4.25774595314952,332.534395888207));
#42552=CARTESIAN_POINT('Ctrl Pts',(150.635039721446,-4.32249528753078,332.653679998002));
#42553=CARTESIAN_POINT('Ctrl Pts',(150.627381925982,-4.38723393550335,332.772944420819));
#42554=CARTESIAN_POINT('Ctrl Pts',(150.619724130518,-4.44704615044988,332.894915008386));
#42555=CARTESIAN_POINT('Ctrl Pts',(150.612066335054,-4.50170736277977,333.019138096082));
#42556=CARTESIAN_POINT('Ctrl Pts',(150.604408053322,-4.55637204609036,333.143369071929));
#42557=CARTESIAN_POINT('Ctrl Pts',(150.596749771589,-4.60588491556441,333.269852465188));
#42558=CARTESIAN_POINT('Ctrl Pts',(150.589091489856,-4.65006928660642,333.398114020206));
#42559=CARTESIAN_POINT('Ctrl Pts',(150.581378559544,-4.69456895201306,333.527290834275));
#42560=CARTESIAN_POINT('Ctrl Pts',(150.573665629233,-4.73366362839711,333.658270901046));
#42561=CARTESIAN_POINT('Ctrl Pts',(150.565952698921,-4.7672240071005,333.79055453673));
#42562=CARTESIAN_POINT('Ctrl Pts',(150.558284606373,-4.80058928844805,333.922069164776));
#42563=CARTESIAN_POINT('Ctrl Pts',(150.550616513825,-4.82848441999502,334.054871839774));
#42564=CARTESIAN_POINT('Ctrl Pts',(150.542948421276,-4.85083394677773,334.188462518864));
#42565=CARTESIAN_POINT('Ctrl Pts',(150.535213072083,-4.8733795006912,334.323224918401));
#42566=CARTESIAN_POINT('Ctrl Pts',(150.52747772289,-4.89028165472963,334.458788797211));
#42567=CARTESIAN_POINT('Ctrl Pts',(150.519742373697,-4.90151655350136,334.594637769085));
#42568=CARTESIAN_POINT('Ctrl Pts',(150.512007024504,-4.91275145227308,334.73048674096));
#42569=CARTESIAN_POINT('Ctrl Pts',(150.504271675311,-4.91831913794538,334.866620391478));
#42570=CARTESIAN_POINT('Ctrl Pts',(150.496536326118,-4.91824935158945,335.002525488068));
#42571=CARTESIAN_POINT('',(153.996536248542,-4.91824850103284,334.996160131745));
#42572=CARTESIAN_POINT('Ctrl Pts',(153.99653624849,-4.91824850103355,334.99616013266));
#42573=CARTESIAN_POINT('Ctrl Pts',(153.988795046099,-4.91835554475088,335.133265807329));
#42574=CARTESIAN_POINT('Ctrl Pts',(153.981053843708,-4.91272516499156,335.270440402459));
#42575=CARTESIAN_POINT('Ctrl Pts',(153.973312641316,-4.90136686420779,335.407168177718));
#42576=CARTESIAN_POINT('Ctrl Pts',(153.965572721839,-4.89001044578267,335.543873293714));
#42577=CARTESIAN_POINT('Ctrl Pts',(153.957832802361,-4.87292802653742,335.680131347521));
#42578=CARTESIAN_POINT('Ctrl Pts',(153.950092882884,-4.85018113288858,335.81542997288));
#42579=CARTESIAN_POINT('Ctrl Pts',(153.942352568803,-4.82743307953775,335.950735496152));
#42580=CARTESIAN_POINT('Ctrl Pts',(153.934612254722,-4.79902004156157,336.085081107864));
#42581=CARTESIAN_POINT('Ctrl Pts',(153.926871940641,-4.76505492617729,336.217963305282));
#42582=CARTESIAN_POINT('Ctrl Pts',(153.91912955453,-4.73108071856075,336.350881074368));
#42583=CARTESIAN_POINT('Ctrl Pts',(153.91138716842,-4.69155157263227,336.482334270744));
#42584=CARTESIAN_POINT('Ctrl Pts',(153.903644782309,-4.6466305397093,336.611833642142));
#42585=CARTESIAN_POINT('Ctrl Pts',(153.895893585931,-4.60165838994896,336.741480374317));
#42586=CARTESIAN_POINT('Ctrl Pts',(153.888142389554,-4.55128222528017,336.869168470188));
#42587=CARTESIAN_POINT('Ctrl Pts',(153.880391193176,-4.49571385557278,336.994427233897));
#42588=CARTESIAN_POINT('Ctrl Pts',(153.872635568759,-4.44011374122829,337.119757554393));
#42589=CARTESIAN_POINT('Ctrl Pts',(153.864879944342,-4.37931568542567,337.242655427412));
#42590=CARTESIAN_POINT('Ctrl Pts',(153.857124319926,-4.3135774697723,337.362674855915));
#42591=CARTESIAN_POINT('Ctrl Pts',(153.849355638484,-4.24772858018298,337.48289634379));
#42592=CARTESIAN_POINT('Ctrl Pts',(153.841586957043,-4.17692311280368,337.600229368254));
#42593=CARTESIAN_POINT('Ctrl Pts',(153.833818275602,-4.10146269925848,337.714256212868));
#42594=CARTESIAN_POINT('Ctrl Pts',(153.826141221996,-4.02689230473695,337.826938166085));
#42595=CARTESIAN_POINT('Ctrl Pts',(153.818464168389,-3.94777646187569,337.936391269431));
#42596=CARTESIAN_POINT('Ctrl Pts',(153.810787114782,-3.86444337650643,338.042245955257));
#42597=CARTESIAN_POINT('Ctrl Pts',(153.803012036004,-3.78004624490054,338.149452256465));
#42598=CARTESIAN_POINT('Ctrl Pts',(153.795236957225,-3.69105123874667,338.253313320985));
#42599=CARTESIAN_POINT('Ctrl Pts',(153.787461878447,-3.59775322759171,338.353409425622));
#42600=CARTESIAN_POINT('Ctrl Pts',(153.779696367398,-3.50457002557909,338.453382355631));
#42601=CARTESIAN_POINT('Ctrl Pts',(153.771930856349,-3.40709461830108,338.54959926095));
#42602=CARTESIAN_POINT('Ctrl Pts',(153.7641653453,-3.30566348531353,338.641671592053));
#42603=CARTESIAN_POINT('Ctrl Pts',(153.756407533778,-3.20433292158963,338.733652633171));
#42604=CARTESIAN_POINT('Ctrl Pts',(153.748649722255,-3.09905472493873,338.821497016904));
#42605=CARTESIAN_POINT('Ctrl Pts',(153.740891910733,-2.99020350399843,338.904851606294));
#42606=CARTESIAN_POINT('Ctrl Pts',(153.73313993721,-2.88143419705372,338.988143468712));
#42607=CARTESIAN_POINT('Ctrl Pts',(153.725387963687,-2.76909752685823,339.066952025261));
#42608=CARTESIAN_POINT('Ctrl Pts',(153.717635990164,-2.6536023146422,339.140963392524));
#42609=CARTESIAN_POINT('Ctrl Pts',(153.709887299606,-2.53815601471722,339.214943415929));
#42610=CARTESIAN_POINT('Ctrl Pts',(153.702138609049,-2.41955416166732,339.284130080327));
#42611=CARTESIAN_POINT('Ctrl Pts',(153.694389918491,-2.29823560290742,339.348252082852));
#42612=CARTESIAN_POINT('Ctrl Pts',(153.686642840113,-2.17694228548709,339.412360744259));
#42613=CARTESIAN_POINT('Ctrl Pts',(153.678895761736,-2.05293373200298,339.47140665723));
#42614=CARTESIAN_POINT('Ctrl Pts',(153.671148683358,-1.92667415244975,339.525164060317));
#42615=CARTESIAN_POINT('Ctrl Pts',(153.663401540052,-1.80041351471949,339.578921913942));
#42616=CARTESIAN_POINT('Ctrl Pts',(153.655654396746,-1.671902172925,339.627391016158));
#42617=CARTESIAN_POINT('Ctrl Pts',(153.64790725344,-1.54162474196582,339.670393582714));
#42618=CARTESIAN_POINT('Ctrl Pts',(153.640158368412,-1.41131802187474,339.713405817161));
#42619=CARTESIAN_POINT('Ctrl Pts',(153.632409483384,-1.27924479362876,339.750948947894));
#42620=CARTESIAN_POINT('Ctrl Pts',(153.624660598356,-1.14590488371914,339.782895050068));
#42621=CARTESIAN_POINT('Ctrl Pts',(153.616903488581,-1.01242344545098,339.814875060166));
#42622=CARTESIAN_POINT('Ctrl Pts',(153.609146378807,-0.877673020533642,
339.841246083298));
#42623=CARTESIAN_POINT('Ctrl Pts',(153.601389269032,-0.742164230805109,
339.861931233267));
#42624=CARTESIAN_POINT('Ctrl Pts',(153.593628014106,-0.606583029512098,
339.882627436718));
#42625=CARTESIAN_POINT('Ctrl Pts',(153.58586675918,-0.470243044250462,339.897631670086));
#42626=CARTESIAN_POINT('Ctrl Pts',(153.578105504253,-0.333659083452315,
339.906919061746));
#42627=CARTESIAN_POINT('Ctrl Pts',(153.570331833849,-0.196856632829616,
339.916221310207));
#42628=CARTESIAN_POINT('Ctrl Pts',(153.562558163444,-0.0598098177201696,
339.9197884322));
#42629=CARTESIAN_POINT('Ctrl Pts',(153.554784493039,0.0769665939859852,
339.91764773097));
#42630=CARTESIAN_POINT('Ctrl Pts',(153.547372688862,0.207376030821223,339.915606679897));
#42631=CARTESIAN_POINT('Ctrl Pts',(153.539960884685,0.337539384918909,339.908377261115));
#42632=CARTESIAN_POINT('Ctrl Pts',(153.532549080508,0.467017474504463,339.896026730014));
#42633=CARTESIAN_POINT('Ctrl Pts',(153.52477400173,0.602841670955703,339.883070862593));
#42634=CARTESIAN_POINT('Ctrl Pts',(153.516998922951,0.738340960250965,339.864438244851));
#42635=CARTESIAN_POINT('Ctrl Pts',(153.509223844173,0.873002817372639,339.840149702577));
#42636=CARTESIAN_POINT('Ctrl Pts',(153.501458333124,1.00749896450609,339.815891048902));
#42637=CARTESIAN_POINT('Ctrl Pts',(153.493692822075,1.14115934890247,339.785990387768));
#42638=CARTESIAN_POINT('Ctrl Pts',(153.485927311026,1.27347514258071,339.750520405569));
#42639=CARTESIAN_POINT('Ctrl Pts',(153.478169499503,1.40565974476388,339.715085591961));
#42640=CARTESIAN_POINT('Ctrl Pts',(153.470411687981,1.5365020341918,339.674092546933));
#42641=CARTESIAN_POINT('Ctrl Pts',(153.462653876459,1.66550232823403,339.62766518421));
#42642=CARTESIAN_POINT('Ctrl Pts',(153.454901902936,1.79440554546437,339.581272759549));
#42643=CARTESIAN_POINT('Ctrl Pts',(153.447149929413,1.9214691600932,339.529454288967));
#42644=CARTESIAN_POINT('Ctrl Pts',(153.43939795589,2.04620798423178,339.472383698629));
#42645=CARTESIAN_POINT('Ctrl Pts',(153.431649265332,2.17089398140445,339.415337277721));
#42646=CARTESIAN_POINT('Ctrl Pts',(153.423900574775,2.29325679158807,339.353043323267));
#42647=CARTESIAN_POINT('Ctrl Pts',(153.416151884217,2.41283078489675,339.285724053874));
#42648=CARTESIAN_POINT('Ctrl Pts',(153.408404805839,2.53237989983724,339.218418790817));
#42649=CARTESIAN_POINT('Ctrl Pts',(153.400657727461,2.64914101164359,339.146090484148));
#42650=CARTESIAN_POINT('Ctrl Pts',(153.392910649084,2.7626730620327,339.069007325481));
#42651=CARTESIAN_POINT('Ctrl Pts',(153.385163505778,2.87620606392955,338.991923520783));
#42652=CARTESIAN_POINT('Ctrl Pts',(153.377416362472,2.98650962704934,338.910085004164));
#42653=CARTESIAN_POINT('Ctrl Pts',(153.369669219166,3.09317199589559,338.823803089374));
#42654=CARTESIAN_POINT('Ctrl Pts',(153.361920334138,3.19985834470723,338.737501776578));
#42655=CARTESIAN_POINT('Ctrl Pts',(153.35417144911,3.30290156645283,338.64675532355));
#42656=CARTESIAN_POINT('Ctrl Pts',(153.346422564082,3.40192360160668,338.551914817578));
#42657=CARTESIAN_POINT('Ctrl Pts',(153.338665454307,3.50105073977157,338.456973646913));
#42658=CARTESIAN_POINT('Ctrl Pts',(153.330908344532,3.59614788262497,338.357930013612));
#42659=CARTESIAN_POINT('Ctrl Pts',(153.323151234758,3.6868740481465,338.255171702937));
#42660=CARTESIAN_POINT('Ctrl Pts',(153.315389979832,3.77764869483008,338.152358481507));
#42661=CARTESIAN_POINT('Ctrl Pts',(153.307628724905,3.86404746398213,338.045826930833));
#42662=CARTESIAN_POINT('Ctrl Pts',(153.299867469979,3.94577084814139,337.935996504844));
#42663=CARTESIAN_POINT('Ctrl Pts',(153.292093799574,4.02762496308171,337.825990385968));
#42664=CARTESIAN_POINT('Ctrl Pts',(153.28432012917,4.10478852746684,337.712675169768));
#42665=CARTESIAN_POINT('Ctrl Pts',(153.276546458765,4.1770059307357,337.596498510899));
#42666=CARTESIAN_POINT('Ctrl Pts',(153.269134654588,4.24586159650712,337.485729903451));
#42667=CARTESIAN_POINT('Ctrl Pts',(153.261722850411,4.31022108369358,337.372360508752));
#42668=CARTESIAN_POINT('Ctrl Pts',(153.254311046234,4.36990328232864,337.256796039875));
#42669=CARTESIAN_POINT('Ctrl Pts',(153.246535967456,4.43251068330356,337.135567412128));
#42670=CARTESIAN_POINT('Ctrl Pts',(153.238760888677,4.49016855791999,337.011539990409));
#42671=CARTESIAN_POINT('Ctrl Pts',(153.230985809899,4.54261706233336,336.885156037971));
#42672=CARTESIAN_POINT('Ctrl Pts',(153.22322029885,4.5950010255231,336.758927609032));
#42673=CARTESIAN_POINT('Ctrl Pts',(153.215454787801,4.64218822510127,336.630348776834));
#42674=CARTESIAN_POINT('Ctrl Pts',(153.207689276752,4.68396442858952,336.499886760462));
#42675=CARTESIAN_POINT('Ctrl Pts',(153.19993146523,4.72569921085014,336.369554097559));
#42676=CARTESIAN_POINT('Ctrl Pts',(153.192173653707,4.76203355527629,336.237342336136));
#42677=CARTESIAN_POINT('Ctrl Pts',(153.184415842185,4.79280125661933,336.103738726805));
#42678=CARTESIAN_POINT('Ctrl Pts',(153.176663868662,4.82354580429143,335.970235658426));
#42679=CARTESIAN_POINT('Ctrl Pts',(153.168911895139,4.84873195966467,335.835343206326));
#42680=CARTESIAN_POINT('Ctrl Pts',(153.161159921616,4.86824341795597,335.699563496781));
#42681=CARTESIAN_POINT('Ctrl Pts',(153.153411231059,4.88774661313315,335.563841290023));
#42682=CARTESIAN_POINT('Ctrl Pts',(153.145662540501,4.90157983561699,335.427232959263));
#42683=CARTESIAN_POINT('Ctrl Pts',(153.137913849943,4.90967797472423,335.290250317843));
#42684=CARTESIAN_POINT('Ctrl Pts',(153.130166771566,4.91777442894599,335.153296176805));
#42685=CARTESIAN_POINT('Ctrl Pts',(153.122419693188,4.92013815016103,335.015968269962));
#42686=CARTESIAN_POINT('Ctrl Pts',(153.11467261481,4.9167559844742,334.878782626505));
#42687=CARTESIAN_POINT('Ctrl Pts',(153.106925471504,4.91337379044156,334.741595833299));
#42688=CARTESIAN_POINT('Ctrl Pts',(153.099178328198,4.9042456230898,334.604551696612));
#42689=CARTESIAN_POINT('Ctrl Pts',(153.091431184892,4.88941044826714,334.468164940159));
#42690=CARTESIAN_POINT('Ctrl Pts',(153.083682299864,4.87457193818225,334.331747521068));
#42691=CARTESIAN_POINT('Ctrl Pts',(153.075933414836,4.85402390974645,334.195988164808));
#42692=CARTESIAN_POINT('Ctrl Pts',(153.068184529808,4.82785701004614,334.061394783176));
#42693=CARTESIAN_POINT('Ctrl Pts',(153.060427420033,4.80166233652811,333.926658542739));
#42694=CARTESIAN_POINT('Ctrl Pts',(153.052670310259,4.76983695295263,333.793091133403));
#42695=CARTESIAN_POINT('Ctrl Pts',(153.044913200484,4.73252243128416,333.661189147082));
#42696=CARTESIAN_POINT('Ctrl Pts',(153.037151945558,4.69518796992836,333.529216676556));
#42697=CARTESIAN_POINT('Ctrl Pts',(153.029390690632,4.65235864776371,333.39891177349));
#42698=CARTESIAN_POINT('Ctrl Pts',(153.021629435705,4.60422511187629,333.270753290688));
#42699=CARTESIAN_POINT('Ctrl Pts',(153.013855765301,4.55601457801818,333.14238979608));
#42700=CARTESIAN_POINT('Ctrl Pts',(153.006082094896,4.50248302757505,333.016179943064));
#42701=CARTESIAN_POINT('Ctrl Pts',(152.998308424491,4.44386857735386,332.892580931635));
#42702=CARTESIAN_POINT('Ctrl Pts',(152.990896620314,4.38798264389175,332.774735483923));
#42703=CARTESIAN_POINT('Ctrl Pts',(152.983484816137,4.32747651272099,332.65926353349));
#42704=CARTESIAN_POINT('Ctrl Pts',(152.97607301196,4.26259334762634,332.546536934194));
#42705=CARTESIAN_POINT('Ctrl Pts',(152.968297933181,4.19453006533398,332.428285268473));
#42706=CARTESIAN_POINT('Ctrl Pts',(152.960522854403,4.12143474476487,332.312681177048));
#42707=CARTESIAN_POINT('Ctrl Pts',(152.952747775625,4.04353867810841,332.200182502172));
#42708=CARTESIAN_POINT('Ctrl Pts',(152.944982264576,3.96573846752111,332.087822264079));
#42709=CARTESIAN_POINT('Ctrl Pts',(152.937216753527,3.88314948570998,331.978560157305));
#42710=CARTESIAN_POINT('Ctrl Pts',(152.929451242478,3.7960486936827,331.872829173568));
#42711=CARTESIAN_POINT('Ctrl Pts',(152.921693430955,3.70903426234456,331.767203022409));
#42712=CARTESIAN_POINT('Ctrl Pts',(152.913935619433,3.61751717018306,331.665101326606));
#42713=CARTESIAN_POINT('Ctrl Pts',(152.906177807911,3.52181721343487,331.566927530964));
#42714=CARTESIAN_POINT('Ctrl Pts',(152.898425834388,3.42618927393833,331.468827614215));
#42715=CARTESIAN_POINT('Ctrl Pts',(152.890673860865,3.32638500701644,331.37464999288));
#42716=CARTESIAN_POINT('Ctrl Pts',(152.882921887342,3.22276372217456,331.284764199471));
#42717=CARTESIAN_POINT('Ctrl Pts',(152.875173196784,3.11918632100873,331.194916472748));
#42718=CARTESIAN_POINT('Ctrl Pts',(152.867424506227,3.01179541169728,331.109357214484));
#42719=CARTESIAN_POINT('Ctrl Pts',(152.859675815669,2.90098615387256,331.028418149208));
#42720=CARTESIAN_POINT('Ctrl Pts',(152.851928737291,2.79019995083955,330.947495923981));
#42721=CARTESIAN_POINT('Ctrl Pts',(152.844181658913,2.67599712939249,330.871192210117));
#42722=CARTESIAN_POINT('Ctrl Pts',(152.836434580535,2.55880451115963,330.799797322013));
#42723=CARTESIAN_POINT('Ctrl Pts',(152.82868743723,2.44161091073966,330.728401835551));
#42724=CARTESIAN_POINT('Ctrl Pts',(152.820940293924,2.32142779736306,330.661915460266));
#42725=CARTESIAN_POINT('Ctrl Pts',(152.813193150618,2.19870909983899,330.600583975482));
#42726=CARTESIAN_POINT('Ctrl Pts',(152.80544426559,2.07596281254593,330.539238702078));
#42727=CARTESIAN_POINT('Ctrl Pts',(152.797695380562,1.95068015633531,330.48305080002));
#42728=CARTESIAN_POINT('Ctrl Pts',(152.789946495534,1.82333729941243,330.432218902457));
#42729=CARTESIAN_POINT('Ctrl Pts',(152.782189385759,1.695859279466,330.381333051393));
#42730=CARTESIAN_POINT('Ctrl Pts',(152.774432275984,1.56631705422675,330.335814706118));
#42731=CARTESIAN_POINT('Ctrl Pts',(152.766675166209,1.43520483114177,330.295813550127));
#42732=CARTESIAN_POINT('Ctrl Pts',(152.758913911283,1.304022545877,330.255791018797));
#42733=CARTESIAN_POINT('Ctrl Pts',(152.751152656357,1.17126896918634,330.221291649586));
#42734=CARTESIAN_POINT('Ctrl Pts',(152.743391401431,1.03744994868626,330.192414258022));
#42735=CARTESIAN_POINT('Ctrl Pts',(152.735617731026,0.903416861364845,330.163490672042));
#42736=CARTESIAN_POINT('Ctrl Pts',(152.727844060621,0.76831530981056,330.140207101469));
#42737=CARTESIAN_POINT('Ctrl Pts',(152.720070390217,0.632658621919278,330.122610725951));
#42738=CARTESIAN_POINT('Ctrl Pts',(152.71265858604,0.503316785489045,330.105833465946));
#42739=CARTESIAN_POINT('Ctrl Pts',(152.705246781863,0.373470619469935,330.094225864332));
#42740=CARTESIAN_POINT('Ctrl Pts',(152.697834977686,0.243564413581649,330.087784670952));
#42741=CARTESIAN_POINT('Ctrl Pts',(152.690059898908,0.107291117569584,330.081027775497));
#42742=CARTESIAN_POINT('Ctrl Pts',(152.682284820129,-0.0294789013836393,
330.079935182752));
#42743=CARTESIAN_POINT('Ctrl Pts',(152.674509741351,-0.16623546848306,330.084560158895));
#42744=CARTESIAN_POINT('Ctrl Pts',(152.666744230302,-0.3028237479202,330.089179443711));
#42745=CARTESIAN_POINT('Ctrl Pts',(152.658978719253,-0.439398221523491,
330.099502285041));
#42746=CARTESIAN_POINT('Ctrl Pts',(152.651213208204,-0.575444897828011,
330.115530097128));
#42747=CARTESIAN_POINT('Ctrl Pts',(152.643455396681,-0.71135668345707,330.131542017592));
#42748=CARTESIAN_POINT('Ctrl Pts',(152.635697585159,-0.846741327519914,
330.15324760663));
#42749=CARTESIAN_POINT('Ctrl Pts',(152.627939773637,-0.981086504580793,
330.180596267895));
#42750=CARTESIAN_POINT('Ctrl Pts',(152.620187800114,-1.11533058263551,330.207924348425));
#42751=CARTESIAN_POINT('Ctrl Pts',(152.612435826591,-1.24853636920625,330.240886970895));
#42752=CARTESIAN_POINT('Ctrl Pts',(152.604683853068,-1.38019867352889,330.279381959522));
#42753=CARTESIAN_POINT('Ctrl Pts',(152.59693516251,-1.51180521878738,330.317860645498));
#42754=CARTESIAN_POINT('Ctrl Pts',(152.589186471953,-1.64186920750584,330.361866928186));
#42755=CARTESIAN_POINT('Ctrl Pts',(152.581437781395,-1.76989784189834,330.411248024599));
#42756=CARTESIAN_POINT('Ctrl Pts',(152.573690703017,-1.89789983886424,330.460618846863));
#42757=CARTESIAN_POINT('Ctrl Pts',(152.565943624639,-2.02386695936215,330.51536211795));
#42758=CARTESIAN_POINT('Ctrl Pts',(152.558196546262,-2.14732409414879,330.575276020226));
#42759=CARTESIAN_POINT('Ctrl Pts',(152.550449402956,-2.27078226362516,330.635190424638));
#42760=CARTESIAN_POINT('Ctrl Pts',(152.54270225965,-2.39173005378051,330.700275376016));
#42761=CARTESIAN_POINT('Ctrl Pts',(152.534955116344,-2.50971513661294,330.770282161236));
#42762=CARTESIAN_POINT('Ctrl Pts',(152.527206231316,-2.62772674499622,330.840304685467));
#42763=CARTESIAN_POINT('Ctrl Pts',(152.519457346288,-2.74277398454481,330.915251045998));
#42764=CARTESIAN_POINT('Ctrl Pts',(152.51170846126,-2.85443213846829,330.994828314619));
#42765=CARTESIAN_POINT('Ctrl Pts',(152.503951351485,-2.96620880751044,331.074490047375));
#42766=CARTESIAN_POINT('Ctrl Pts',(152.496194241711,-3.07458888635121,331.158792279771));
#42767=CARTESIAN_POINT('Ctrl Pts',(152.488437131936,-3.17917905894054,331.247400424546));
#42768=CARTESIAN_POINT('Ctrl Pts',(152.48067587701,-3.28382512117416,331.336055918682));
#42769=CARTESIAN_POINT('Ctrl Pts',(152.472914622083,-3.38467695450139,331.429021645241));
#42770=CARTESIAN_POINT('Ctrl Pts',(152.465153367157,-3.48137771966674,331.525925700923));
#42771=CARTESIAN_POINT('Ctrl Pts',(152.457379696753,-3.57823317454143,331.622984771513));
#42772=CARTESIAN_POINT('Ctrl Pts',(152.449606026348,-3.67092402744085,331.723994472432));
#42773=CARTESIAN_POINT('Ctrl Pts',(152.441832355943,-3.75913281281358,331.828548666915));
#42774=CARTESIAN_POINT('Ctrl Pts',(152.434420551766,-3.84323545800619,331.928235838491));
#42775=CARTESIAN_POINT('Ctrl Pts',(152.427008747589,-3.92326374884816,332.031144710368));
#42776=CARTESIAN_POINT('Ctrl Pts',(152.419596943412,-3.99897998780284,332.136899910996));
#42777=CARTESIAN_POINT('Ctrl Pts',(152.411752387183,-4.07911706101047,332.248829826849));
#42778=CARTESIAN_POINT('Ctrl Pts',(152.403907830954,-4.15467548780588,332.364300171864));
#42779=CARTESIAN_POINT('Ctrl Pts',(152.396063274724,-4.22532975812652,332.482904154071));
#42780=CARTESIAN_POINT('Ctrl Pts',(152.388228710807,-4.29589402979664,332.6013570598));
#42781=CARTESIAN_POINT('Ctrl Pts',(152.380394146889,-4.36156638223422,332.722935335455));
#42782=CARTESIAN_POINT('Ctrl Pts',(152.372559582971,-4.4220627456671,332.847200860302));
#42783=CARTESIAN_POINT('Ctrl Pts',(152.364733405835,-4.48249434866032,332.971333360789));
#42784=CARTESIAN_POINT('Ctrl Pts',(152.356907228699,-4.53776082443947,333.098147044492));
#42785=CARTESIAN_POINT('Ctrl Pts',(152.349081051563,-4.58762262067717,333.227176897502));
#42786=CARTESIAN_POINT('Ctrl Pts',(152.341261661756,-4.63744117378289,333.356094848106));
#42787=CARTESIAN_POINT('Ctrl Pts',(152.333442271949,-4.6818642413228,333.487224787547));
#42788=CARTESIAN_POINT('Ctrl Pts',(152.325622882142,-4.72069937701304,333.620079547811));
#42789=CARTESIAN_POINT('Ctrl Pts',(152.31780913696,-4.7595064785793,333.75283840351));
#42790=CARTESIAN_POINT('Ctrl Pts',(152.309995391777,-4.79273357672973,333.887319234516));
#42791=CARTESIAN_POINT('Ctrl Pts',(152.302181646594,-4.8202374249548,334.023017794653));
#42792=CARTESIAN_POINT('Ctrl Pts',(152.294371178942,-4.84772973649703,334.158659435073));
#42793=CARTESIAN_POINT('Ctrl Pts',(152.286560711289,-4.86950350289265,334.295517414046));
#42794=CARTESIAN_POINT('Ctrl Pts',(152.278750243637,-4.8854661601859,334.43307543696));
#42795=CARTESIAN_POINT('Ctrl Pts',(152.27094092684,-4.9014264654151,334.570613190987));
#42796=CARTESIAN_POINT('Ctrl Pts',(152.263131610044,-4.91157732054033,334.708850404923));
#42797=CARTESIAN_POINT('Ctrl Pts',(152.255322293248,-4.91587782163216,334.847263935873));
#42798=CARTESIAN_POINT('Ctrl Pts',(152.252393611662,-4.91749061295388,334.899172338349));
#42799=CARTESIAN_POINT('Ctrl Pts',(152.249464930076,-4.91828111641089,334.951105496473));
#42800=CARTESIAN_POINT('Ctrl Pts',(152.24653624849,-4.91824906311716,335.003035728436));
#42801=CARTESIAN_POINT('',(155.746536248441,-4.91824983112492,334.998711147934));
#42802=CARTESIAN_POINT('Ctrl Pts',(155.746536248441,-4.91824983112492,334.998711147934));
#42803=CARTESIAN_POINT('Ctrl Pts',(155.73881437765,-4.91828535226794,335.134259563696));
#42804=CARTESIAN_POINT('Ctrl Pts',(155.731092506859,-4.91271300065732,335.270034172756));
#42805=CARTESIAN_POINT('Ctrl Pts',(155.723370636069,-4.90150278861575,335.405528637327));
#42806=CARTESIAN_POINT('Ctrl Pts',(155.715658110667,-4.89030614372606,335.540859119809));
#42807=CARTESIAN_POINT('Ctrl Pts',(155.707945585266,-4.87348524360162,335.675909740718));
#42808=CARTESIAN_POINT('Ctrl Pts',(155.700233059864,-4.85106207896362,335.810172678224));
#42809=CARTESIAN_POINT('Ctrl Pts',(155.692527960626,-4.8286605049299,335.944306337906));
#42810=CARTESIAN_POINT('Ctrl Pts',(155.684822861388,-4.80066746362549,336.07765343435));
#42811=CARTESIAN_POINT('Ctrl Pts',(155.67711776215,-4.76715682936312,336.209710224292));
#42812=CARTESIAN_POINT('Ctrl Pts',(155.669418176934,-4.73367017641276,336.341672510052));
#42813=CARTESIAN_POINT('Ctrl Pts',(155.661718591718,-4.69467388546408,336.472345943801));
#42814=CARTESIAN_POINT('Ctrl Pts',(155.654019006503,-4.65029301382672,336.601236381068));
#42815=CARTESIAN_POINT('Ctrl Pts',(155.646322237362,-4.60592837421368,336.730079677468));
#42816=CARTESIAN_POINT('Ctrl Pts',(155.638625468221,-4.55618319763893,336.857140899253));
#42817=CARTESIAN_POINT('Ctrl Pts',(155.63092869908,-4.50123248290631,336.981940765343));
#42818=CARTESIAN_POINT('Ctrl Pts',(155.623233156016,-4.44629052169457,337.106720751105));
#42819=CARTESIAN_POINT('Ctrl Pts',(155.615537612953,-4.38614483115809,337.229239734583));
#42820=CARTESIAN_POINT('Ctrl Pts',(155.607842069889,-4.32101847795669,337.349038606677));
#42821=CARTESIAN_POINT('Ctrl Pts',(155.600146030071,-4.25588792078289,337.46884521191));
#42822=CARTESIAN_POINT('Ctrl Pts',(155.592449990252,-4.1857762509565,337.585931007953));
#42823=CARTESIAN_POINT('Ctrl Pts',(155.584753950433,-4.1109521632586,337.699862102756));
#42824=CARTESIAN_POINT('Ctrl Pts',(155.577055690991,-4.03610649546407,337.813826056551));
#42825=CARTESIAN_POINT('Ctrl Pts',(155.56935743155,-3.9565459240256,337.924633167845));
#42826=CARTESIAN_POINT('Ctrl Pts',(155.561659172108,-3.87258179019653,338.031879506303));
#42827=CARTESIAN_POINT('Ctrl Pts',(155.553952605069,-3.78852704625478,338.139241579925));
#42828=CARTESIAN_POINT('Ctrl Pts',(155.546246038031,-3.70005949677172,338.243034896075));
#42829=CARTESIAN_POINT('Ctrl Pts',(155.538539470992,-3.60753024948391,338.342889253559));
#42830=CARTESIAN_POINT('Ctrl Pts',(155.530828242175,-3.51494503033456,338.442804013936));
#42831=CARTESIAN_POINT('Ctrl Pts',(155.523117013357,-3.41829350140623,338.538774791744));
#42832=CARTESIAN_POINT('Ctrl Pts',(155.51540578454,-3.31796190590271,338.630469921853));
#42833=CARTESIAN_POINT('Ctrl Pts',(155.507683202205,-3.2174825886095,338.722300057975));
#42834=CARTESIAN_POINT('Ctrl Pts',(155.49996061987,-3.11331268921402,338.809841722717));
#42835=CARTESIAN_POINT('Ctrl Pts',(155.492238037535,-3.00587000081113,338.892804721627));
#42836=CARTESIAN_POINT('Ctrl Pts',(155.488230465165,-2.95011347654464,338.935857706718));
#42837=CARTESIAN_POINT('Ctrl Pts',(155.484222892795,-2.8934760464137,338.977678378518));
#42838=CARTESIAN_POINT('Ctrl Pts',(155.480215320426,-2.83601879579477,339.018231010333));
#42839=CARTESIAN_POINT('Ctrl Pts',(155.472440241647,-2.72454616130369,339.096907046086));
#42840=CARTESIAN_POINT('Ctrl Pts',(155.464665162869,-2.60962098522146,339.171065226659));
#42841=CARTESIAN_POINT('Ctrl Pts',(155.45689008409,-2.49164561765528,339.240387385431));
#42842=CARTESIAN_POINT('Ctrl Pts',(155.449124573041,-2.37381542628964,339.309624238873));
#42843=CARTESIAN_POINT('Ctrl Pts',(155.441359061992,-2.25294284551895,339.374036715234));
#42844=CARTESIAN_POINT('Ctrl Pts',(155.433593550943,-2.12946121369527,339.433348396175));
#42845=CARTESIAN_POINT('Ctrl Pts',(155.425835739421,-2.0061020142688,339.492601269411));
#42846=CARTESIAN_POINT('Ctrl Pts',(155.418077927899,-1.88013926189763,339.546763243698));
#42847=CARTESIAN_POINT('Ctrl Pts',(155.410320116377,-1.75203273767333,339.595602718754));
#42848=CARTESIAN_POINT('Ctrl Pts',(155.402568142854,-1.62402261767111,339.644405440557));
#42849=CARTESIAN_POINT('Ctrl Pts',(155.394816169331,-1.4938723006851,339.6878934969));
#42850=CARTESIAN_POINT('Ctrl Pts',(155.387064195808,-1.36206316109458,339.725882669691));
#42851=CARTESIAN_POINT('Ctrl Pts',(155.37931550525,-1.23030984275312,339.763855754046));
#42852=CARTESIAN_POINT('Ctrl Pts',(155.371566814692,-1.09689947385912,339.796334478605));
#42853=CARTESIAN_POINT('Ctrl Pts',(155.363818124135,-0.962330060539396,
339.823184001993));
#42854=CARTESIAN_POINT('Ctrl Pts',(155.356071045757,-0.827788645510108,
339.850027939114));
#42855=CARTESIAN_POINT('Ctrl Pts',(155.348323967379,-0.6920890487956,339.871244928235));
#42856=CARTESIAN_POINT('Ctrl Pts',(155.340576889001,-0.555740593810602,
339.886751012165));
#42857=CARTESIAN_POINT('Ctrl Pts',(155.332829745696,-0.419390996094409,
339.90225722605));
#42858=CARTESIAN_POINT('Ctrl Pts',(155.32508260239,-0.282392917632038,339.912052395111));
#42859=CARTESIAN_POINT('Ctrl Pts',(155.317335459084,-0.145261552604407,
339.916104366654));
#42860=CARTESIAN_POINT('Ctrl Pts',(155.309586574056,-0.00809935753444271,
339.920157249166));
#42861=CARTESIAN_POINT('Ctrl Pts',(155.301837689028,0.129195793101662,339.918464353288));
#42862=CARTESIAN_POINT('Ctrl Pts',(155.294088804,0.266108348808019,339.911045653341));
#42863=CARTESIAN_POINT('Ctrl Pts',(155.286331694225,0.40316622491569,339.903619079108));
#42864=CARTESIAN_POINT('Ctrl Pts',(155.27857458445,0.539840303972119,339.890454581757));
#42865=CARTESIAN_POINT('Ctrl Pts',(155.270817474676,0.675619248307293,339.87162413306));
#42866=CARTESIAN_POINT('Ctrl Pts',(155.263056219749,0.811470748569065,339.852783621974));
#42867=CARTESIAN_POINT('Ctrl Pts',(155.255294964823,0.946425776604411,339.828271196388));
#42868=CARTESIAN_POINT('Ctrl Pts',(155.247533709897,1.07998382011621,339.79820987565));
#42869=CARTESIAN_POINT('Ctrl Pts',(155.239760039492,1.21375551297109,339.768100466596));
#42870=CARTESIAN_POINT('Ctrl Pts',(155.231986369088,1.34612537806441,339.732424526438));
#42871=CARTESIAN_POINT('Ctrl Pts',(155.224212698683,1.47660782568998,339.691355069872));
#42872=CARTESIAN_POINT('Ctrl Pts',(155.216800894506,1.60101628398516,339.65219740639));
#42873=CARTESIAN_POINT('Ctrl Pts',(155.209389090329,1.72370881808154,339.60813715988));
#42874=CARTESIAN_POINT('Ctrl Pts',(155.201977286152,1.84428368065753,339.55936407493));
#42875=CARTESIAN_POINT('Ctrl Pts',(155.194202207374,1.97076827642355,339.508200475798));
#42876=CARTESIAN_POINT('Ctrl Pts',(155.186427128595,2.09532207974599,339.451688690113));
#42877=CARTESIAN_POINT('Ctrl Pts',(155.178652049817,2.21745980279598,339.389994884449));
#42878=CARTESIAN_POINT('Ctrl Pts',(155.170886538768,2.3394472276023,339.32837699694));
#42879=CARTESIAN_POINT('Ctrl Pts',(155.163121027719,2.45902414227711,339.261589952012));
#42880=CARTESIAN_POINT('Ctrl Pts',(155.15535551667,2.57572359649386,339.189848567307));
#42881=CARTESIAN_POINT('Ctrl Pts',(155.147597705147,2.69230734286179,339.118178314394));
#42882=CARTESIAN_POINT('Ctrl Pts',(155.139839893625,2.8060189755836,339.041563700727));
#42883=CARTESIAN_POINT('Ctrl Pts',(155.132082082103,2.91641492311124,338.960266033836));
#42884=CARTESIAN_POINT('Ctrl Pts',(155.12433010858,3.02672779418749,338.879029546017));
#42885=CARTESIAN_POINT('Ctrl Pts',(155.116578135057,3.13372963308817,338.79311725046));
#42886=CARTESIAN_POINT('Ctrl Pts',(155.108826161534,3.23700502759131,338.702834254169));
#42887=CARTESIAN_POINT('Ctrl Pts',(155.101077470976,3.3402366849036,338.612589492781));
#42888=CARTESIAN_POINT('Ctrl Pts',(155.093328780419,3.43974474298275,338.517977968881));
#42889=CARTESIAN_POINT('Ctrl Pts',(155.085580089861,3.53514631114801,338.419345496038));
#42890=CARTESIAN_POINT('Ctrl Pts',(155.077833011483,3.6305280302202,338.320733544505));
#42891=CARTESIAN_POINT('Ctrl Pts',(155.070085933105,3.72180468724035,338.218102588848));
#42892=CARTESIAN_POINT('Ctrl Pts',(155.062338854728,3.8086300566899,338.111835495938));
#42893=CARTESIAN_POINT('Ctrl Pts',(155.054591711422,3.89545615381955,338.005567512407));
#42894=CARTESIAN_POINT('Ctrl Pts',(155.046844568116,3.97783064165802,337.895663633528));
#42895=CARTESIAN_POINT('Ctrl Pts',(155.03909742481,4.05544768118593,337.78253969741));
#42896=CARTESIAN_POINT('Ctrl Pts',(155.031348539782,4.13308217067191,337.669390328631));
#42897=CARTESIAN_POINT('Ctrl Pts',(155.023599654754,4.20595686241477,337.5530197843));
#42898=CARTESIAN_POINT('Ctrl Pts',(155.015850769726,4.27380955929132,337.433872411079));
#42899=CARTESIAN_POINT('Ctrl Pts',(155.008093659951,4.34173427572167,337.314598573604));
#42900=CARTESIAN_POINT('Ctrl Pts',(155.000336550176,4.40462615558138,337.192542359817));
#42901=CARTESIAN_POINT('Ctrl Pts',(154.992579440402,4.46226900731624,337.068172712528));
#42902=CARTESIAN_POINT('Ctrl Pts',(154.984818185476,4.51994266154805,336.943736606076));
#42903=CARTESIAN_POINT('Ctrl Pts',(154.977056930549,4.57236154931104,336.816984963854));
#42904=CARTESIAN_POINT('Ctrl Pts',(154.969295675623,4.61935826427569,336.68840525016));
#42905=CARTESIAN_POINT('Ctrl Pts',(154.961522005219,4.66643015866804,336.559619850828));
#42906=CARTESIAN_POINT('Ctrl Pts',(154.953748334814,4.70806242885946,336.429000908979));
#42907=CARTESIAN_POINT('Ctrl Pts',(154.945974664409,4.74413778614593,336.297050395537));
#42908=CARTESIAN_POINT('Ctrl Pts',(154.938562860232,4.77853382687156,336.171242210241));
#42909=CARTESIAN_POINT('Ctrl Pts',(154.931151056055,4.80787859589356,336.044223913224));
#42910=CARTESIAN_POINT('Ctrl Pts',(154.923739251878,4.83211424495484,335.916436024065));
#42911=CARTESIAN_POINT('Ctrl Pts',(154.915964173099,4.85753775537083,335.782384869798));
#42912=CARTESIAN_POINT('Ctrl Pts',(154.908189094321,4.87741899903553,335.647063149466));
#42913=CARTESIAN_POINT('Ctrl Pts',(154.900414015543,4.89163509187614,335.510968874224));
#42914=CARTESIAN_POINT('Ctrl Pts',(154.892648504494,4.90583369090947,335.375042071653));
#42915=CARTESIAN_POINT('Ctrl Pts',(154.884882993445,4.91438096984336,335.238344990791));
#42916=CARTESIAN_POINT('Ctrl Pts',(154.877117482396,4.91720487979926,335.101386550283));
#42917=CARTESIAN_POINT('Ctrl Pts',(154.869359670873,4.92002598984022,334.964563904468));
#42918=CARTESIAN_POINT('Ctrl Pts',(154.861601859351,4.91713501594497,334.82748080298));
#42919=CARTESIAN_POINT('Ctrl Pts',(154.853844047829,4.90851165517153,334.690651663096));
#42920=CARTESIAN_POINT('Ctrl Pts',(154.846092074306,4.89989478375052,334.553925491478));
#42921=CARTESIAN_POINT('Ctrl Pts',(154.838340100783,4.88555413635134,334.41745328959));
#42922=CARTESIAN_POINT('Ctrl Pts',(154.83058812726,4.86552148057395,334.281749497339));
#42923=CARTESIAN_POINT('Ctrl Pts',(154.822839436702,4.84549730863821,334.146103175724));
#42924=CARTESIAN_POINT('Ctrl Pts',(154.815090746145,4.81978597973966,334.011225002383));
#42925=CARTESIAN_POINT('Ctrl Pts',(154.807342055587,4.7884710917699,333.877624097825));
#42926=CARTESIAN_POINT('Ctrl Pts',(154.799594977209,4.75716271912418,333.74405099005));
#42927=CARTESIAN_POINT('Ctrl Pts',(154.791847898831,4.72025319554371,333.611755002791));
#42928=CARTESIAN_POINT('Ctrl Pts',(154.784100820454,4.67787711945422,333.481234475705));
#42929=CARTESIAN_POINT('Ctrl Pts',(154.776353677148,4.63550068821224,333.350712854731));
#42930=CARTESIAN_POINT('Ctrl Pts',(154.768606533842,4.58765773378256,333.22196709538));
#42931=CARTESIAN_POINT('Ctrl Pts',(154.760859390536,4.53453243626125,333.09547941807));
#42932=CARTESIAN_POINT('Ctrl Pts',(154.753110505508,4.48139519504535,332.968963303646));
#42933=CARTESIAN_POINT('Ctrl Pts',(154.74536162048,4.4229733989114,332.844706641768));
#42934=CARTESIAN_POINT('Ctrl Pts',(154.737612735452,4.35949881853884,332.723170381065));
#42935=CARTESIAN_POINT('Ctrl Pts',(154.729855625677,4.29595686559076,332.60150512052));
#42936=CARTESIAN_POINT('Ctrl Pts',(154.722098515902,4.227351596389,332.482566376142));
#42937=CARTESIAN_POINT('Ctrl Pts',(154.714341406128,4.15396036129341,332.366789719885));
#42938=CARTESIAN_POINT('Ctrl Pts',(154.706580151201,4.08052990826851,332.250951196285));
#42939=CARTESIAN_POINT('Ctrl Pts',(154.698818896275,4.00230861616061,332.138278448644));
#42940=CARTESIAN_POINT('Ctrl Pts',(154.691057641349,3.9196158109255,332.029176047417));
#42941=CARTESIAN_POINT('Ctrl Pts',(154.683283970944,3.83679072415144,331.919899117904));
#42942=CARTESIAN_POINT('Ctrl Pts',(154.67551030054,3.74948007957757,331.814204249367));
#42943=CARTESIAN_POINT('Ctrl Pts',(154.667736630135,3.65804252361451,331.712461717648));
#42944=CARTESIAN_POINT('Ctrl Pts',(154.660324825958,3.57086140788074,331.61545532526));
#42945=CARTESIAN_POINT('Ctrl Pts',(154.652913021781,3.47992915042439,331.522041794123));
#42946=CARTESIAN_POINT('Ctrl Pts',(154.645501217604,3.38558488854456,331.432508160492));
#42947=CARTESIAN_POINT('Ctrl Pts',(154.637726138826,3.28661653335231,331.338586216769));
#42948=CARTESIAN_POINT('Ctrl Pts',(154.629951060047,3.18358049349499,331.248637307193));
#42949=CARTESIAN_POINT('Ctrl Pts',(154.622175981269,3.07682905755571,331.163034270015));
#42950=CARTESIAN_POINT('Ctrl Pts',(154.61441047022,2.97020898605451,331.077536572824));
#42951=CARTESIAN_POINT('Ctrl Pts',(154.606644959171,2.85988291752784,330.996374349489));
#42952=CARTESIAN_POINT('Ctrl Pts',(154.598879448122,2.74623982273755,330.919883592529));
#42953=CARTESIAN_POINT('Ctrl Pts',(154.591121636599,2.63270940540648,330.843468676378));
#42954=CARTESIAN_POINT('Ctrl Pts',(154.583363825077,2.51586882896713,330.771716225961));
#42955=CARTESIAN_POINT('Ctrl Pts',(154.575606013555,2.39613969079377,330.704921695161));
#42956=CARTESIAN_POINT('Ctrl Pts',(154.567854040032,2.27650065259376,330.638177429363));
#42957=CARTESIAN_POINT('Ctrl Pts',(154.560102066509,2.15397771934535,330.57638384649));
#42958=CARTESIAN_POINT('Ctrl Pts',(154.552350092986,2.02902068581284,330.519792625442));
#42959=CARTESIAN_POINT('Ctrl Pts',(154.544601402428,1.90411657165833,330.46322537081));
#42960=CARTESIAN_POINT('Ctrl Pts',(154.536852711871,1.77678076281382,330.411856256905));
#42961=CARTESIAN_POINT('Ctrl Pts',(154.529104021313,1.64748662919201,330.365890498798));
#42962=CARTESIAN_POINT('Ctrl Pts',(154.521356942935,1.51821939629449,330.31993430425));
#42963=CARTESIAN_POINT('Ctrl Pts',(154.513609864557,1.38699501711946,330.279379360211));
#42964=CARTESIAN_POINT('Ctrl Pts',(154.50586278618,1.2543053950483,330.244382160176));
#42965=CARTESIAN_POINT('Ctrl Pts',(154.498115642874,1.12161466091073,330.209384666831));
#42966=CARTESIAN_POINT('Ctrl Pts',(154.490368499568,0.987459037332595,330.17994511008));
#42967=CARTESIAN_POINT('Ctrl Pts',(154.482621356262,0.852343704169711,330.156169566091));
#42968=CARTESIAN_POINT('Ctrl Pts',(154.474872471234,0.717197994211744,330.132388676855));
#42969=CARTESIAN_POINT('Ctrl Pts',(154.467123586206,0.581092530209212,330.11427440201));
#42970=CARTESIAN_POINT('Ctrl Pts',(154.459374701178,0.444540358112609,330.101881286401));
#42971=CARTESIAN_POINT('Ctrl Pts',(154.451617591403,0.307843248129065,330.089475016611));
#42972=CARTESIAN_POINT('Ctrl Pts',(154.443860481629,0.17069887280036,330.082802071825));
#42973=CARTESIAN_POINT('Ctrl Pts',(154.436103371854,0.0336236040688946,
330.081864935186));
#42974=CARTESIAN_POINT('Ctrl Pts',(154.428342116928,-0.103524913303038,
330.080927297772));
#42975=CARTESIAN_POINT('Ctrl Pts',(154.420580862002,-0.240603860058357,
330.085731562174));
#42976=CARTESIAN_POINT('Ctrl Pts',(154.412819607075,-0.377100218672374,
330.096228136671));
#42977=CARTESIAN_POINT('Ctrl Pts',(154.405045936671,-0.513814926976299,
330.106741502267));
#42978=CARTESIAN_POINT('Ctrl Pts',(154.397272266266,-0.649944796492763,
330.122965327844));
#42979=CARTESIAN_POINT('Ctrl Pts',(154.389498595861,-0.784984370213917,
330.14479839749));
#42980=CARTESIAN_POINT('Ctrl Pts',(154.382086791684,-0.913737819290731,
330.165615132491));
#42981=CARTESIAN_POINT('Ctrl Pts',(154.374674987507,-1.04149991271711,330.191530585975));
#42982=CARTESIAN_POINT('Ctrl Pts',(154.36726318333,-1.16784574893145,330.22241490194));
#42983=CARTESIAN_POINT('Ctrl Pts',(154.359488104552,-1.30038417094281,330.25481295023));
#42984=CARTESIAN_POINT('Ctrl Pts',(154.351713025773,-1.4317828413548,330.292781638085));
#42985=CARTESIAN_POINT('Ctrl Pts',(154.343937946995,-1.56153758896135,330.33622648269));
#42986=CARTESIAN_POINT('Ctrl Pts',(154.336172435946,-1.69113266509016,330.379617865648));
#42987=CARTESIAN_POINT('Ctrl Pts',(154.328406924897,-1.81908747640063,330.428471874242));
#42988=CARTESIAN_POINT('Ctrl Pts',(154.320641413848,-1.94490898521745,330.482643239491));
#42989=CARTESIAN_POINT('Ctrl Pts',(154.312883602326,-2.0706057416418,330.536760893673));
#42990=CARTESIAN_POINT('Ctrl Pts',(154.305125790803,-2.19417304819069,330.596185259009));
#42991=CARTESIAN_POINT('Ctrl Pts',(154.297367979281,-2.3151343008612,330.660721692323));
#42992=CARTESIAN_POINT('Ctrl Pts',(154.289616005758,-2.4360045263529,330.725209559924));
#42993=CARTESIAN_POINT('Ctrl Pts',(154.281864032235,-2.55427225804356,330.794801654997));
#42994=CARTESIAN_POINT('Ctrl Pts',(154.274112058712,-2.66948244402078,330.869255933423));
#42995=CARTESIAN_POINT('Ctrl Pts',(154.266363368155,-2.78464383841632,330.943678680418));
#42996=CARTESIAN_POINT('Ctrl Pts',(154.258614677597,-2.89674993490381,331.022959303572));
#42997=CARTESIAN_POINT('Ctrl Pts',(154.250865987039,-3.00537199613136,331.106810789678));
#42998=CARTESIAN_POINT('Ctrl Pts',(154.243118908662,-3.1139714576321,331.190644829781));
#42999=CARTESIAN_POINT('Ctrl Pts',(154.235371830284,-3.21908801650164,331.279047602517));
#43000=CARTESIAN_POINT('Ctrl Pts',(154.227624751906,-3.32032387687554,331.371690143448));
#43001=CARTESIAN_POINT('Ctrl Pts',(154.2198776086,-3.42156058570353,331.464333460813));
#43002=CARTESIAN_POINT('Ctrl Pts',(154.212130465294,-3.51891624280707,331.561216353366));
#43003=CARTESIAN_POINT('Ctrl Pts',(154.204383321988,-3.61202826466784,331.66197140849));
#43004=CARTESIAN_POINT('Ctrl Pts',(154.19663443696,-3.70516122008752,331.762749115488));
#43005=CARTESIAN_POINT('Ctrl Pts',(154.188885551932,-3.79404837655751,331.867400430336));
#43006=CARTESIAN_POINT('Ctrl Pts',(154.181136666904,-3.87836622755252,331.975523439092));
#43007=CARTESIAN_POINT('Ctrl Pts',(154.173379557129,-3.96277357438588,332.083761210728));
#43008=CARTESIAN_POINT('Ctrl Pts',(154.165622447355,-4.04260168685022,332.195477728472));
#43009=CARTESIAN_POINT('Ctrl Pts',(154.15786533758,-4.11756903833055,332.310240107913));
#43010=CARTESIAN_POINT('Ctrl Pts',(154.150104082654,-4.19257644996644,332.4250638127));
#43011=CARTESIAN_POINT('Ctrl Pts',(154.142342827728,-4.26271772521411,332.542936286614));
#43012=CARTESIAN_POINT('Ctrl Pts',(154.134581572801,-4.32775694359023,332.663399285349));
#43013=CARTESIAN_POINT('Ctrl Pts',(154.126807902397,-4.39290020351956,332.784054985623));
#43014=CARTESIAN_POINT('Ctrl Pts',(154.119034231992,-4.45292492599718,332.907309140046));
#43015=CARTESIAN_POINT('Ctrl Pts',(154.111260561587,-4.5076426938536,333.032681925298));
#43016=CARTESIAN_POINT('Ctrl Pts',(154.10384875741,-4.55981333645127,333.152218577232));
#43017=CARTESIAN_POINT('Ctrl Pts',(154.096436953233,-4.60715987847357,333.273680786186));
#43018=CARTESIAN_POINT('Ctrl Pts',(154.089025149056,-4.64956157998799,333.396640970837));
#43019=CARTESIAN_POINT('Ctrl Pts',(154.079880925922,-4.70187416281465,333.548341601099));
#43020=CARTESIAN_POINT('Ctrl Pts',(154.070736702789,-4.74679633555163,333.702713734351));
#43021=CARTESIAN_POINT('Ctrl Pts',(154.061592479655,-4.78408881765321,333.859089290389));
#43022=CARTESIAN_POINT('Ctrl Pts',(154.052490952621,-4.82120717413257,334.014734699505));
#43023=CARTESIAN_POINT('Ctrl Pts',(154.043389425587,-4.85076683947267,334.172364783848));
#43024=CARTESIAN_POINT('Ctrl Pts',(154.034287898553,-4.87257861659285,334.331299254059));
#43025=CARTESIAN_POINT('Ctrl Pts',(154.025265126919,-4.89420165667757,334.488858466281));
#43026=CARTESIAN_POINT('Ctrl Pts',(154.016242355285,-4.90821023847201,334.647699488882));
#43027=CARTESIAN_POINT('Ctrl Pts',(154.007219583651,-4.91446721116948,334.807139706419));
#43028=CARTESIAN_POINT('Ctrl Pts',(154.003658471948,-4.91693671606248,334.870067645598));
#43029=CARTESIAN_POINT('Ctrl Pts',(154.000097360245,-4.91819925871801,334.933088712353));
#43030=CARTESIAN_POINT('Ctrl Pts',(153.996536248542,-4.91824850103284,334.996160131745));
#43031=CARTESIAN_POINT('',(157.496536248451,-4.91824791444093,335.004529304303));
#43032=CARTESIAN_POINT('Ctrl Pts',(157.496536248451,-4.91824791444093,335.004529304303));
#43033=CARTESIAN_POINT('Ctrl Pts',(157.486533103091,-4.91808521296232,335.181202398966));
#43034=CARTESIAN_POINT('Ctrl Pts',(157.476529957731,-4.90839940609836,335.357450971929));
#43035=CARTESIAN_POINT('Ctrl Pts',(157.466526812371,-4.88934810921038,335.532407860067));
#43036=CARTESIAN_POINT('Ctrl Pts',(157.456290198198,-4.86985216381327,335.711448161524));
#43037=CARTESIAN_POINT('Ctrl Pts',(157.446053584026,-4.84054843538798,335.889136075352));
#43038=CARTESIAN_POINT('Ctrl Pts',(157.435816969853,-4.80165374290327,336.064567703701));
#43039=CARTESIAN_POINT('Ctrl Pts',(157.43317183335,-4.79160337183968,336.109899157649));
#43040=CARTESIAN_POINT('Ctrl Pts',(157.430526696846,-4.78091285455322,336.155080074558));
#43041=CARTESIAN_POINT('Ctrl Pts',(157.427881560343,-4.76958644365158,336.200095087497));
#43042=CARTESIAN_POINT('Ctrl Pts',(157.420106481565,-4.73629374328191,336.332411613088));
#43043=CARTESIAN_POINT('Ctrl Pts',(157.412331402786,-4.69743823030342,336.463550779452));
#43044=CARTESIAN_POINT('Ctrl Pts',(157.404556324008,-4.6531177914097,336.593009065187));
#43045=CARTESIAN_POINT('Ctrl Pts',(157.396790812959,-4.60885189163762,336.722308044259));
#43046=CARTESIAN_POINT('Ctrl Pts',(157.38902530191,-4.55913457204411,336.849929892019));
#43047=CARTESIAN_POINT('Ctrl Pts',(157.381259790861,-4.5041144291156,336.975382563437));
#43048=CARTESIAN_POINT('Ctrl Pts',(157.373501979338,-4.44914883881894,337.100710848167));
#43049=CARTESIAN_POINT('Ctrl Pts',(157.365744167816,-4.38889104441723,337.223873881003));
#43050=CARTESIAN_POINT('Ctrl Pts',(157.357986356294,-4.32353890444586,337.344396383772));
#43051=CARTESIAN_POINT('Ctrl Pts',(157.350234382771,-4.25823594403232,337.464828189536));
#43052=CARTESIAN_POINT('Ctrl Pts',(157.342482409248,-4.18784645432413,337.582623078197));
#43053=CARTESIAN_POINT('Ctrl Pts',(157.334730435725,-4.1126155481167,337.697327643407));
#43054=CARTESIAN_POINT('Ctrl Pts',(157.326981745167,-4.0374165022427,337.811983631166));
#43055=CARTESIAN_POINT('Ctrl Pts',(157.31923305461,-3.95738033177873,337.923551572327));
#43056=CARTESIAN_POINT('Ctrl Pts',(157.311484364052,-3.87279693981029,338.031604678301));
#43057=CARTESIAN_POINT('Ctrl Pts',(157.303737285674,-3.78823114612297,338.139635302923));
#43058=CARTESIAN_POINT('Ctrl Pts',(157.295990207296,-3.69912025354925,338.244152239353));
#43059=CARTESIAN_POINT('Ctrl Pts',(157.288243128919,-3.60579590641386,338.344759923192));
#43060=CARTESIAN_POINT('Ctrl Pts',(157.280495985613,-3.5124707771306,338.44536845022));
#43061=CARTESIAN_POINT('Ctrl Pts',(157.272748842307,-3.41493238867397,338.542067372741));
#43062=CARTESIAN_POINT('Ctrl Pts',(157.265001699001,-3.31355059478758,338.634496597644));
#43063=CARTESIAN_POINT('Ctrl Pts',(157.257252813973,-3.21214600812157,338.726946602599));
#43064=CARTESIAN_POINT('Ctrl Pts',(157.249503928945,-3.10689658539734,338.815124736515));
#43065=CARTESIAN_POINT('Ctrl Pts',(157.241755043917,-2.99820641690037,338.898710215463));
#43066=CARTESIAN_POINT('Ctrl Pts',(157.233997934142,-2.88940088353549,338.982384412903));
#43067=CARTESIAN_POINT('Ctrl Pts',(157.226240824367,-2.77714761943565,339.061455979065));
#43068=CARTESIAN_POINT('Ctrl Pts',(157.218483714593,-2.66188140104686,339.135646318202));
#43069=CARTESIAN_POINT('Ctrl Pts',(157.210722459666,-2.54655358807648,339.209876302284));
#43070=CARTESIAN_POINT('Ctrl Pts',(157.20296120474,-2.42820994976775,339.279219664418));
#43071=CARTESIAN_POINT('Ctrl Pts',(157.195199949814,-2.30731031378142,339.343443585269));
#43072=CARTESIAN_POINT('Ctrl Pts',(157.187426279409,-2.18621727777866,339.407770243464));
#43073=CARTESIAN_POINT('Ctrl Pts',(157.179652609005,-2.06256042628889,339.466960926604));
#43074=CARTESIAN_POINT('Ctrl Pts',(157.1718789386,-1.93682084457429,339.520830463369));
#43075=CARTESIAN_POINT('Ctrl Pts',(157.164467134423,-1.81693447064047,339.572192360236));
#43076=CARTESIAN_POINT('Ctrl Pts',(157.157055330246,-1.69515517386244,339.618717258106));
#43077=CARTESIAN_POINT('Ctrl Pts',(157.149643526069,-1.57191134148936,339.660287308417));
#43078=CARTESIAN_POINT('Ctrl Pts',(157.141868447291,-1.44262696176637,339.703894830726));
#43079=CARTESIAN_POINT('Ctrl Pts',(157.134093368512,-1.31132229143814,339.742187328599));
#43080=CARTESIAN_POINT('Ctrl Pts',(157.126318289734,-1.17847372450055,339.774974632724));
#43081=CARTESIAN_POINT('Ctrl Pts',(157.118552778685,-1.04578863618212,339.807721589985));
#43082=CARTESIAN_POINT('Ctrl Pts',(157.110787267636,-0.91156380729692,339.834976740029));
#43083=CARTESIAN_POINT('Ctrl Pts',(157.103021756587,-0.776293423092196,
339.856598767014));
#43084=CARTESIAN_POINT('Ctrl Pts',(157.095263945064,-0.641157159867239,
339.878199355697));
#43085=CARTESIAN_POINT('Ctrl Pts',(157.087506133542,-0.504977787845208,
339.894177875002));
#43086=CARTESIAN_POINT('Ctrl Pts',(157.07974832202,-0.368262051188472,339.904443508101));
#43087=CARTESIAN_POINT('Ctrl Pts',(157.071996348497,-0.23164919745919,339.914701415986));
#43088=CARTESIAN_POINT('Ctrl Pts',(157.064244374974,-0.0945011707113606,
339.91925496572));
#43089=CARTESIAN_POINT('Ctrl Pts',(157.056492401451,0.0426681053860614,
339.918064913691));
#43090=CARTESIAN_POINT('Ctrl Pts',(157.048743710893,0.179779290213689,339.91687536565));
#43091=CARTESIAN_POINT('Ctrl Pts',(157.040995020336,0.316911316446174,339.90994705714));
#43092=CARTESIAN_POINT('Ctrl Pts',(157.033246329778,0.453548405259294,339.897292814054));
#43093=CARTESIAN_POINT('Ctrl Pts',(157.0254992514,0.590157065584847,339.88464120379));
#43094=CARTESIAN_POINT('Ctrl Pts',(157.017752173023,0.726270604352937,339.866266064609));
#43095=CARTESIAN_POINT('Ctrl Pts',(157.010005094645,0.861376911248659,339.842232220709));
#43096=CARTESIAN_POINT('Ctrl Pts',(157.002257951339,0.996484350465272,339.818198175381));
#43097=CARTESIAN_POINT('Ctrl Pts',(156.994510808033,1.13058415613934,339.788505399197));
#43098=CARTESIAN_POINT('Ctrl Pts',(156.986763664727,1.26317336920926,339.753270043015));
#43099=CARTESIAN_POINT('Ctrl Pts',(156.979014779699,1.39579239114918,339.718026765177));
#43100=CARTESIAN_POINT('Ctrl Pts',(156.971265894671,1.52689976700366,339.677238528132));
#43101=CARTESIAN_POINT('Ctrl Pts',(156.963517009643,1.65600706628379,339.631071545433));
#43102=CARTESIAN_POINT('Ctrl Pts',(156.955759899868,1.78525140138543,339.584855560621));
#43103=CARTESIAN_POINT('Ctrl Pts',(156.948002790094,1.91249105058461,339.533249557597));
#43104=CARTESIAN_POINT('Ctrl Pts',(156.940245680319,2.03725645429074,339.476468385005));
#43105=CARTESIAN_POINT('Ctrl Pts',(156.932484425393,2.16208852863936,339.41965687037));
#43106=CARTESIAN_POINT('Ctrl Pts',(156.924723170467,2.28444337447842,339.357664852337));
#43107=CARTESIAN_POINT('Ctrl Pts',(156.91696191554,2.40387636993161,339.290753017896));
#43108=CARTESIAN_POINT('Ctrl Pts',(156.909188245136,2.5235004192544,339.223734146327));
#43109=CARTESIAN_POINT('Ctrl Pts',(156.901414574731,2.64019294525471,339.151779936814));
#43110=CARTESIAN_POINT('Ctrl Pts',(156.893640904326,2.75353789057768,339.07519473739));
#43111=CARTESIAN_POINT('Ctrl Pts',(156.886229100149,2.86160660142614,339.002174597426));
#43112=CARTESIAN_POINT('Ctrl Pts',(156.878817295972,2.96663214579147,338.924945080553));
#43113=CARTESIAN_POINT('Ctrl Pts',(156.871405491795,3.0682835973832,338.843802652131));
#43114=CARTESIAN_POINT('Ctrl Pts',(156.863630413017,3.1749172894221,338.758683191581));
#43115=CARTESIAN_POINT('Ctrl Pts',(156.855855334238,3.27817475919368,338.668988560862));
#43116=CARTESIAN_POINT('Ctrl Pts',(156.84808025546,3.37763828513822,338.575016458321));
#43117=CARTESIAN_POINT('Ctrl Pts',(156.840314744411,3.47697941488193,338.481159994436));
#43118=CARTESIAN_POINT('Ctrl Pts',(156.832549233362,3.57253560874617,338.383036797854));
#43119=CARTESIAN_POINT('Ctrl Pts',(156.824783722313,3.66392059923009,338.280985965383));
#43120=CARTESIAN_POINT('Ctrl Pts',(156.817025910791,3.75521498122989,338.179036316609));
#43121=CARTESIAN_POINT('Ctrl Pts',(156.809268099269,3.84234613117196,338.073167071059));
#43122=CARTESIAN_POINT('Ctrl Pts',(156.801510287746,3.92496345090526,337.963755214514));
#43123=CARTESIAN_POINT('Ctrl Pts',(156.793758314223,4.00751859848546,337.854425693861));
#43124=CARTESIAN_POINT('Ctrl Pts',(156.7860063407,4.08556644242812,337.741559179287));
#43125=CARTESIAN_POINT('Ctrl Pts',(156.778254367177,4.15879586835624,337.625566603201));
#43126=CARTESIAN_POINT('Ctrl Pts',(156.77050567662,4.23199428157903,337.509623150039));
#43127=CARTESIAN_POINT('Ctrl Pts',(156.762756986062,4.30037812717194,337.390556598315));
#43128=CARTESIAN_POINT('Ctrl Pts',(156.755008295505,4.36367907318612,337.268807618274));
#43129=CARTESIAN_POINT('Ctrl Pts',(156.747261217127,4.42696684890979,337.147083969125));
#43130=CARTESIAN_POINT('Ctrl Pts',(156.739514138749,4.48517364837742,337.022679348344));
#43131=CARTESIAN_POINT('Ctrl Pts',(156.731767060371,4.53807685136121,336.896059480512));
#43132=CARTESIAN_POINT('Ctrl Pts',(156.724019917065,4.59098049772476,336.769438551484));
#43133=CARTESIAN_POINT('Ctrl Pts',(156.71627277376,4.6385803082592,336.640602699034));
#43134=CARTESIAN_POINT('Ctrl Pts',(156.708525630454,4.68070177669209,336.510037728062));
#43135=CARTESIAN_POINT('Ctrl Pts',(156.700776745426,4.72283271492532,336.379443403313));
#43136=CARTESIAN_POINT('Ctrl Pts',(156.693027860398,4.75948274023017,336.247119558411));
#43137=CARTESIAN_POINT('Ctrl Pts',(156.685278975369,4.79052730736479,336.113566872663));
#43138=CARTESIAN_POINT('Ctrl Pts',(156.677521865595,4.82160482552374,335.979872432715));
#43139=CARTESIAN_POINT('Ctrl Pts',(156.66976475582,4.84706491180638,335.844946927776));
#43140=CARTESIAN_POINT('Ctrl Pts',(156.662007646045,4.86683413138314,335.709301487454));
#43141=CARTESIAN_POINT('Ctrl Pts',(156.654246391119,4.88661391499873,335.573583562545));
#43142=CARTESIAN_POINT('Ctrl Pts',(156.646485136193,4.90069673229623,335.437145324294));
#43143=CARTESIAN_POINT('Ctrl Pts',(156.638723881267,4.90906119011706,335.30050173741));
#43144=CARTESIAN_POINT('Ctrl Pts',(156.630950210862,4.91743902834443,335.163639565319));
#43145=CARTESIAN_POINT('Ctrl Pts',(156.623176540458,4.92008022012367,335.02657177918));
#43146=CARTESIAN_POINT('Ctrl Pts',(156.615402870053,4.91701554570077,334.889812950684));
#43147=CARTESIAN_POINT('Ctrl Pts',(156.607991065876,4.91409353260957,334.759420278556));
#43148=CARTESIAN_POINT('Ctrl Pts',(156.600579261699,4.90598493267237,334.629308734669));
#43149=CARTESIAN_POINT('Ctrl Pts',(156.593167457522,4.89275996672966,334.499917036415));
#43150=CARTESIAN_POINT('Ctrl Pts',(156.585392378743,4.87888680581097,334.364183465593));
#43151=CARTESIAN_POINT('Ctrl Pts',(156.577617299965,4.85933921909417,334.228813145002));
#43152=CARTESIAN_POINT('Ctrl Pts',(156.569842221186,4.83414149436549,334.094318447271));
#43153=CARTESIAN_POINT('Ctrl Pts',(156.562076710137,4.80897477704125,333.959989253828));
#43154=CARTESIAN_POINT('Ctrl Pts',(156.554311199088,4.77817182718233,333.826533919828));
#43155=CARTESIAN_POINT('Ctrl Pts',(156.546545688039,4.74180876701852,333.694460770591));
#43156=CARTESIAN_POINT('Ctrl Pts',(156.538787876517,4.70548176093474,333.562518572266));
#43157=CARTESIAN_POINT('Ctrl Pts',(156.531030064995,4.66360571854861,333.431956205875));
#43158=CARTESIAN_POINT('Ctrl Pts',(156.523272253473,4.61630792646881,333.303272505521));
#43159=CARTESIAN_POINT('Ctrl Pts',(156.51552027995,4.56904572747745,333.174685643732));
#43160=CARTESIAN_POINT('Ctrl Pts',(156.507768306427,4.51637003421296,333.047974999368));
#43161=CARTESIAN_POINT('Ctrl Pts',(156.500016332904,4.458458046662,332.923624574251));
#43162=CARTESIAN_POINT('Ctrl Pts',(156.492267642346,4.40057058487215,332.799326811613));
#43163=CARTESIAN_POINT('Ctrl Pts',(156.484518951788,4.33745140406873,332.677387633773));
#43164=CARTESIAN_POINT('Ctrl Pts',(156.476770261231,4.26932586344716,332.558271158748));
#43165=CARTESIAN_POINT('Ctrl Pts',(156.469023182853,4.20121449691332,332.439179466901));
#43166=CARTESIAN_POINT('Ctrl Pts',(156.461276104475,4.12809903633994,332.322909648801));
#43167=CARTESIAN_POINT('Ctrl Pts',(156.453529026097,4.05025064688352,332.209900940841));
#43168=CARTESIAN_POINT('Ctrl Pts',(156.445781882791,3.97240160498266,332.09689128576));
#43169=CARTESIAN_POINT('Ctrl Pts',(156.438034739485,3.88981977682201,331.987143117224));
#43170=CARTESIAN_POINT('Ctrl Pts',(156.43028759618,3.80281925074881,331.881066078187));
#43171=CARTESIAN_POINT('Ctrl Pts',(156.422538711152,3.71579916511037,331.77496519078));
#43172=CARTESIAN_POINT('Ctrl Pts',(156.414789826123,3.62435865259686,331.67253737739));
#43173=CARTESIAN_POINT('Ctrl Pts',(156.407040941095,3.52885134654363,331.57415831707));
#43174=CARTESIAN_POINT('Ctrl Pts',(156.399283831321,3.43324266804885,331.4756748362));
#43175=CARTESIAN_POINT('Ctrl Pts',(156.391526721546,3.33355884602364,331.381248973731));
#43176=CARTESIAN_POINT('Ctrl Pts',(156.383769611771,3.23018996045864,331.291219084139));
#43177=CARTESIAN_POINT('Ctrl Pts',(156.376008356845,3.12676583786634,331.201141085453));
#43178=CARTESIAN_POINT('Ctrl Pts',(156.368247101919,3.01965303305044,331.115463984402));
#43179=CARTESIAN_POINT('Ctrl Pts',(156.360485846993,2.90927301375598,331.034484447902));
#43180=CARTESIAN_POINT('Ctrl Pts',(156.352712176588,2.79871642240342,330.953375370535));
#43181=CARTESIAN_POINT('Ctrl Pts',(156.344938506183,2.68488249724977,330.876979091993));
#43182=CARTESIAN_POINT('Ctrl Pts',(156.337164835779,2.56822060956445,330.805548192778));
#43183=CARTESIAN_POINT('Ctrl Pts',(156.329753031601,2.4569893608182,330.737442419107));
#43184=CARTESIAN_POINT('Ctrl Pts',(156.322341227424,2.34318775905778,330.673850291587));
#43185=CARTESIAN_POINT('Ctrl Pts',(156.314929423247,2.2272227316258,330.614950175171));
#43186=CARTESIAN_POINT('Ctrl Pts',(156.307154344469,2.10557391275734,330.553163188596));
#43187=CARTESIAN_POINT('Ctrl Pts',(156.29937926569,1.98115980136051,330.496344523276));
#43188=CARTESIAN_POINT('Ctrl Pts',(156.291604186912,1.85442440602456,330.444751029324));
#43189=CARTESIAN_POINT('Ctrl Pts',(156.283838675863,1.72784496666089,330.393221024451));
#43190=CARTESIAN_POINT('Ctrl Pts',(156.276073164814,1.59895028551374,330.346903543247));
#43191=CARTESIAN_POINT('Ctrl Pts',(156.268307653765,1.46820901829683,330.306009656903));
#43192=CARTESIAN_POINT('Ctrl Pts',(156.260549842243,1.337597381427,330.265156316966));
#43193=CARTESIAN_POINT('Ctrl Pts',(156.252792030721,1.20514317272121,330.229715986273));
#43194=CARTESIAN_POINT('Ctrl Pts',(156.245034219198,1.07133475450583,330.199851574556));
#43195=CARTESIAN_POINT('Ctrl Pts',(156.237282245675,0.937627031368573,330.170009636757));
#43196=CARTESIAN_POINT('Ctrl Pts',(156.229530272153,0.802567507113986,330.145735350689));
#43197=CARTESIAN_POINT('Ctrl Pts',(156.22177829863,0.666659082280117,330.127141626262));
#43198=CARTESIAN_POINT('Ctrl Pts',(156.214029608072,0.530808214744785,330.108555776288));
#43199=CARTESIAN_POINT('Ctrl Pts',(156.206280917514,0.394109548130885,330.095645756016));
#43200=CARTESIAN_POINT('Ctrl Pts',(156.198532226957,0.257075323970763,330.088473216982));
#43201=CARTESIAN_POINT('Ctrl Pts',(156.190785148579,0.120069610925533,330.081302170254));
#43202=CARTESIAN_POINT('Ctrl Pts',(156.183038070201,-0.0172711307029542,
330.079866250765));
#43203=CARTESIAN_POINT('Ctrl Pts',(156.175290991823,-0.154430794635645,
330.084175125966));
#43204=CARTESIAN_POINT('Ctrl Pts',(156.167543848517,-0.291591608098359,
330.08848403728));
#43205=CARTESIAN_POINT('Ctrl Pts',(156.159796705212,-0.428570950156742,
330.098537827043));
#43206=CARTESIAN_POINT('Ctrl Pts',(156.152049561906,-0.564854372084219,
330.114294052971));
#43207=CARTESIAN_POINT('Ctrl Pts',(156.144300676878,-0.701168433418233,
330.130053821233));
#43208=CARTESIAN_POINT('Ctrl Pts',(156.13655179185,-0.836785875076158,330.151518531871));
#43209=CARTESIAN_POINT('Ctrl Pts',(156.128802906822,-0.971199409237683,
330.178594108562));
#43210=CARTESIAN_POINT('Ctrl Pts',(156.121045797047,-1.10575561131321,330.205698423549));
#43211=CARTESIAN_POINT('Ctrl Pts',(156.113288687272,-1.23910496950445,330.238425423815));
#43212=CARTESIAN_POINT('Ctrl Pts',(156.105531577498,-1.37075185965037,330.276630185793));
#43213=CARTESIAN_POINT('Ctrl Pts',(156.097770322571,-1.50246909768508,330.314855363174));
#43214=CARTESIAN_POINT('Ctrl Pts',(156.090009067645,-1.63248168461715,330.358564010365));
#43215=CARTESIAN_POINT('Ctrl Pts',(156.082247812719,-1.76031206652673,330.407562249639));
#43216=CARTESIAN_POINT('Ctrl Pts',(156.074474142314,-1.88834693538757,330.456638870128));
#43217=CARTESIAN_POINT('Ctrl Pts',(156.06670047191,-2.01419226454658,330.511021836393));
#43218=CARTESIAN_POINT('Ctrl Pts',(156.058926801505,-2.13739247309216,330.57046994835));
#43219=CARTESIAN_POINT('Ctrl Pts',(156.051514997328,-2.25485768229059,330.627150736394));
#43220=CARTESIAN_POINT('Ctrl Pts',(156.044103193151,-2.36991823564859,330.688435582049));
#43221=CARTESIAN_POINT('Ctrl Pts',(156.036691388974,-2.48220393053748,330.754078814942));
#43222=CARTESIAN_POINT('Ctrl Pts',(156.028916310195,-2.59999308181405,330.82293941822));
#43223=CARTESIAN_POINT('Ctrl Pts',(156.021141231417,-2.7151007242116,330.896814058694));
#43224=CARTESIAN_POINT('Ctrl Pts',(156.013366152639,-2.82707058846668,330.975468356401));
#43225=CARTESIAN_POINT('Ctrl Pts',(156.00560064159,-2.93890266667534,331.054025864988));
#43226=CARTESIAN_POINT('Ctrl Pts',(155.99783513054,-3.04760433270449,331.137351105436));
#43227=CARTESIAN_POINT('Ctrl Pts',(155.990069619491,-3.15274447578762,331.22516419789));
#43228=CARTESIAN_POINT('Ctrl Pts',(155.982311807969,-3.25778037211277,331.312890223407));
#43229=CARTESIAN_POINT('Ctrl Pts',(155.974553996447,-3.35926147482994,331.405094996791));
#43230=CARTESIAN_POINT('Ctrl Pts',(155.966796184925,-3.45678650879377,331.501456003546));
#43231=CARTESIAN_POINT('Ctrl Pts',(155.959044211402,-3.55423815207675,331.597744495588));
#43232=CARTESIAN_POINT('Ctrl Pts',(155.951292237879,-3.64773937538844,331.698182721853));
#43233=CARTESIAN_POINT('Ctrl Pts',(155.943540264356,-3.73692308204036,331.80240888458));
#43234=CARTESIAN_POINT('Ctrl Pts',(155.935791573798,-3.82606901933971,331.906590907465));
#43235=CARTESIAN_POINT('Ctrl Pts',(155.928042883241,-3.9109008230817,332.014557379813));
#43236=CARTESIAN_POINT('Ctrl Pts',(155.920294192683,-3.99108944589062,332.125910909975));
#43237=CARTESIAN_POINT('Ctrl Pts',(155.912547114305,-4.07126138478685,332.237241272105));
#43238=CARTESIAN_POINT('Ctrl Pts',(155.904800035927,-4.14679183602421,332.351956973348));
#43239=CARTESIAN_POINT('Ctrl Pts',(155.897052957549,-4.21739337531564,332.469629240537));
#43240=CARTESIAN_POINT('Ctrl Pts',(155.889305814244,-4.28799550631593,332.587302493933));
#43241=CARTESIAN_POINT('Ctrl Pts',(155.881558670938,-4.35366844187699,332.707932027524));
#43242=CARTESIAN_POINT('Ctrl Pts',(155.873811527632,-4.41416947489604,332.831062262444));
#43243=CARTESIAN_POINT('Ctrl Pts',(155.866062642604,-4.47468410983167,332.954220179654));
#43244=CARTESIAN_POINT('Ctrl Pts',(155.858313757576,-4.53002435613471,333.079879566187));
#43245=CARTESIAN_POINT('Ctrl Pts',(155.850564872548,-4.57999480204501,333.207562922795));
#43246=CARTESIAN_POINT('Ctrl Pts',(155.842807762773,-4.63001828710295,333.335381803836));
#43247=CARTESIAN_POINT('Ctrl Pts',(155.835050652998,-4.67466044368149,333.465228581742));
#43248=CARTESIAN_POINT('Ctrl Pts',(155.827293543223,-4.71377493042639,333.596608049124));
#43249=CARTESIAN_POINT('Ctrl Pts',(155.819532288297,-4.75291031870232,333.728057721493));
#43250=CARTESIAN_POINT('Ctrl Pts',(155.811771033371,-4.78651205570566,333.861041336538));
#43251=CARTESIAN_POINT('Ctrl Pts',(155.804009778445,-4.81448474552528,333.995052390617));
#43252=CARTESIAN_POINT('Ctrl Pts',(155.79623610804,-4.84250218253236,334.129277818709));
#43253=CARTESIAN_POINT('Ctrl Pts',(155.788462437635,-4.86487251460147,334.264533584332));
#43254=CARTESIAN_POINT('Ctrl Pts',(155.78068876723,-4.88155203105705,334.400306052571));
#43255=CARTESIAN_POINT('Ctrl Pts',(155.773276963053,-4.89745511200852,334.529758279747));
#43256=CARTESIAN_POINT('Ctrl Pts',(155.765865158876,-4.90818524543721,334.65967990028));
#43257=CARTESIAN_POINT('Ctrl Pts',(155.758453354699,-4.91374868291656,334.789626656546));
#43258=CARTESIAN_POINT('Ctrl Pts',(155.754480985963,-4.91673041645718,334.859271836005));
#43259=CARTESIAN_POINT('Ctrl Pts',(155.750508617226,-4.91823155793977,334.928980857133));
#43260=CARTESIAN_POINT('Ctrl Pts',(155.74653624849,-4.9182498311247,334.998711147067));
#43261=CARTESIAN_POINT('',(159.246536248535,-4.91824990229953,334.999019678274));
#43262=CARTESIAN_POINT('Ctrl Pts',(159.24653624849,-4.91824990229969,334.999019679075));
#43263=CARTESIAN_POINT('Ctrl Pts',(159.238532934143,-4.91827822418977,335.14111001863));
#43264=CARTESIAN_POINT('Ctrl Pts',(159.230529619796,-4.91214462811284,335.283122174808));
#43265=CARTESIAN_POINT('Ctrl Pts',(159.222526305449,-4.89989552381521,335.424507854104));
#43266=CARTESIAN_POINT('Ctrl Pts',(159.214516214359,-4.88763604768447,335.566013250615));
#43267=CARTESIAN_POINT('Ctrl Pts',(159.206506123268,-4.86925076832775,335.7068907614));
#43268=CARTESIAN_POINT('Ctrl Pts',(159.198496032178,-4.84483770014801,335.846599504916));
#43269=CARTESIAN_POINT('Ctrl Pts',(159.190063843328,-4.8191381670273,335.993670305474));
#43270=CARTESIAN_POINT('Ctrl Pts',(159.181631654479,-4.7867584610174,336.139445373955));
#43271=CARTESIAN_POINT('Ctrl Pts',(159.17319946563,-4.74787291413732,336.283310505568));
#43272=CARTESIAN_POINT('Ctrl Pts',(159.165166204723,-4.71082704749778,336.42036935924));
#43273=CARTESIAN_POINT('Ctrl Pts',(159.157132943816,-4.66787693508807,336.555694534693));
#43274=CARTESIAN_POINT('Ctrl Pts',(159.149099682909,-4.61922322496871,336.688774662413));
#43275=CARTESIAN_POINT('Ctrl Pts',(159.141057776062,-4.57051715042545,336.821998019996));
#43276=CARTESIAN_POINT('Ctrl Pts',(159.133015869215,-4.51609536852315,336.952971185732));
#43277=CARTESIAN_POINT('Ctrl Pts',(159.124973962368,-4.45620553497504,337.081205249983));
#43278=CARTESIAN_POINT('Ctrl Pts',(159.116917656263,-4.39620846701454,337.209668920892));
#43279=CARTESIAN_POINT('Ctrl Pts',(159.108861350158,-4.33072395016572,337.335383380747));
#43280=CARTESIAN_POINT('Ctrl Pts',(159.100805044053,-4.26004465514347,337.457885798544));
#43281=CARTESIAN_POINT('Ctrl Pts',(159.099639951364,-4.24982310586148,337.475601941585));
#43282=CARTESIAN_POINT('Ctrl Pts',(159.098474858675,-4.23949298126891,337.493250959373));
#43283=CARTESIAN_POINT('Ctrl Pts',(159.097309765986,-4.22905523794468,337.510831507073));
#43284=CARTESIAN_POINT('Ctrl Pts',(159.089534687208,-4.15940045649074,337.628152767989));
#43285=CARTESIAN_POINT('Ctrl Pts',(159.08175960843,-4.08474986776342,337.742758707826));
#43286=CARTESIAN_POINT('Ctrl Pts',(159.073984529651,-4.00534092879957,337.854194651138));
#43287=CARTESIAN_POINT('Ctrl Pts',(159.066219018602,-3.92602970759045,337.965493465427));
#43288=CARTESIAN_POINT('Ctrl Pts',(159.058453507553,-3.84197201148367,338.073629729549));
#43289=CARTESIAN_POINT('Ctrl Pts',(159.050687996504,-3.75345062640725,338.178174233365));
#43290=CARTESIAN_POINT('Ctrl Pts',(159.042930184982,-3.66501701054178,338.282615081));
#43291=CARTESIAN_POINT('Ctrl Pts',(159.03517237346,-3.57212876417649,338.383470959018));
#43292=CARTESIAN_POINT('Ctrl Pts',(159.027414561938,-3.47511110534665,338.480342780244));
#43293=CARTESIAN_POINT('Ctrl Pts',(159.019662588415,-3.37816645538184,338.577141702353));
#43294=CARTESIAN_POINT('Ctrl Pts',(159.011910614892,-3.27709885379081,338.66996226023));
#43295=CARTESIAN_POINT('Ctrl Pts',(159.004158641369,-3.1722725700779,338.758439809766));
#43296=CARTESIAN_POINT('Ctrl Pts',(158.996409950811,-3.06749068035845,338.846879889007));
#43297=CARTESIAN_POINT('Ctrl Pts',(158.988661260253,-2.95895357258093,338.930980366488));
#43298=CARTESIAN_POINT('Ctrl Pts',(158.980912569696,-2.84706085227632,339.010414887008));
#43299=CARTESIAN_POINT('Ctrl Pts',(158.973165491318,-2.73519141218658,339.089832880512));
#43300=CARTESIAN_POINT('Ctrl Pts',(158.96541841294,-2.61996806679041,339.164586621901));
#43301=CARTESIAN_POINT('Ctrl Pts',(158.957671334562,-2.50182152122744,339.234391590113));
#43302=CARTESIAN_POINT('Ctrl Pts',(158.949924191257,-2.38367398548289,339.304197143359));
#43303=CARTESIAN_POINT('Ctrl Pts',(158.942177047951,-2.26260353723115,339.369053641872));
#43304=CARTESIAN_POINT('Ctrl Pts',(158.934429904645,-2.13906738459991,339.428721461849));
#43305=CARTESIAN_POINT('Ctrl Pts',(158.926681019617,-2.01550345841856,339.488402696418));
#43306=CARTESIAN_POINT('Ctrl Pts',(158.918932134589,-1.88947307667827,339.542892761229));
#43307=CARTESIAN_POINT('Ctrl Pts',(158.911183249561,-1.76145504787547,339.591999474827));
#43308=CARTESIAN_POINT('Ctrl Pts',(158.903426139786,-1.6333011394143,339.641158310799));
#43309=CARTESIAN_POINT('Ctrl Pts',(158.895669030011,-1.50315573507092,339.684922241206));
#43310=CARTESIAN_POINT('Ctrl Pts',(158.887911920237,-1.3715150195725,339.723148273513));
#43311=CARTESIAN_POINT('Ctrl Pts',(158.88015066531,-1.23980395948498,339.761394732589));
#43312=CARTESIAN_POINT('Ctrl Pts',(158.872389410384,-1.10659637548001,339.794097303796));
#43313=CARTESIAN_POINT('Ctrl Pts',(158.864628155458,-0.972399404108642,
339.821164015193));
#43314=CARTESIAN_POINT('Ctrl Pts',(158.856854485054,-0.837987761317682,
339.848274024507));
#43315=CARTESIAN_POINT('Ctrl Pts',(158.849080814649,-0.702583954722853,
339.869730097086));
#43316=CARTESIAN_POINT('Ctrl Pts',(158.841307144244,-0.566701902813514,
339.885491993223));
#43317=CARTESIAN_POINT('Ctrl Pts',(158.833895340067,-0.437145193110627,
339.900520169303));
#43318=CARTESIAN_POINT('Ctrl Pts',(158.82648353589,-0.307154047705987,339.910372344821));
#43319=CARTESIAN_POINT('Ctrl Pts',(158.819071731713,-0.177172671851662,
339.915057772483));
#43320=CARTESIAN_POINT('Ctrl Pts',(158.811296652934,-0.0408205215732932,
339.919972846913));
#43321=CARTESIAN_POINT('Ctrl Pts',(158.803521574156,0.0959517752568021,
339.919217424385));
#43322=CARTESIAN_POINT('Ctrl Pts',(158.795746495378,0.23263337072655,339.912745136614));
#43323=CARTESIAN_POINT('Ctrl Pts',(158.787980984329,0.369146770791589,339.906280813405));
#43324=CARTESIAN_POINT('Ctrl Pts',(158.78021547328,0.505569304871357,339.894113640831));
#43325=CARTESIAN_POINT('Ctrl Pts',(158.772449962231,0.641387009309717,339.876249149376));
#43326=CARTESIAN_POINT('Ctrl Pts',(158.764692150708,0.777070050098496,339.858402370616));
#43327=CARTESIAN_POINT('Ctrl Pts',(158.756934339186,0.912149069623679,339.834869565268));
#43328=CARTESIAN_POINT('Ctrl Pts',(158.749176527664,1.04611247282728,339.805708247147));
#43329=CARTESIAN_POINT('Ctrl Pts',(158.741424554141,1.17997506432178,339.776568873842));
#43330=CARTESIAN_POINT('Ctrl Pts',(158.733672580618,1.3127233301591,339.741809501391));
#43331=CARTESIAN_POINT('Ctrl Pts',(158.725920607095,1.44385350619738,339.701539121941));
#43332=CARTESIAN_POINT('Ctrl Pts',(158.718171916537,1.57492814852837,339.66128579702));
#43333=CARTESIAN_POINT('Ctrl Pts',(158.71042322598,1.70438569112442,339.615526221602));
#43334=CARTESIAN_POINT('Ctrl Pts',(158.702674535422,1.83173544545043,339.564419822976));
#43335=CARTESIAN_POINT('Ctrl Pts',(158.694927457044,1.95905870359635,339.513324057464));
#43336=CARTESIAN_POINT('Ctrl Pts',(158.687180378667,2.08427468323903,339.456883826972));
#43337=CARTESIAN_POINT('Ctrl Pts',(158.679433300289,2.20691104528425,339.39530734997));
#43338=CARTESIAN_POINT('Ctrl Pts',(158.671686156983,2.32954843514021,339.333730356898));
#43339=CARTESIAN_POINT('Ctrl Pts',(158.663939013677,2.44960581496282,339.267017206849));
#43340=CARTESIAN_POINT('Ctrl Pts',(158.656191870371,2.56663425843017,339.195422701702));
#43341=CARTESIAN_POINT('Ctrl Pts',(158.648442985343,2.6836890123765,339.123812100589));
#43342=CARTESIAN_POINT('Ctrl Pts',(158.640694100315,2.79771314155195,339.047318164551));
#43343=CARTESIAN_POINT('Ctrl Pts',(158.632945215287,2.90828592572085,338.966239533457));
#43344=CARTESIAN_POINT('Ctrl Pts',(158.625188105512,3.01897607298517,338.885074844665));
#43345=CARTESIAN_POINT('Ctrl Pts',(158.617430995737,3.12620724175919,338.799315971539));
#43346=CARTESIAN_POINT('Ctrl Pts',(158.609673885963,3.22959067254162,338.709302784936));
#43347=CARTESIAN_POINT('Ctrl Pts',(158.601912631037,3.33302934812382,338.619241498163));
#43348=CARTESIAN_POINT('Ctrl Pts',(158.59415137611,3.43261590508547,338.524921636667));
#43349=CARTESIAN_POINT('Ctrl Pts',(158.586390121184,3.52799856157159,338.426719891098));
#43350=CARTESIAN_POINT('Ctrl Pts',(158.57861645078,3.62353379922298,338.32836105474));
#43351=CARTESIAN_POINT('Ctrl Pts',(158.570842780375,3.7148514376178,338.226108217083));
#43352=CARTESIAN_POINT('Ctrl Pts',(158.56306910997,3.80163952754342,338.120371767133));
#43353=CARTESIAN_POINT('Ctrl Pts',(158.555657305793,3.88438761100264,338.019557374367));
#43354=CARTESIAN_POINT('Ctrl Pts',(158.548245501616,3.96301818325018,337.915576624448));
#43355=CARTESIAN_POINT('Ctrl Pts',(158.540833697439,4.03729864013467,337.808808066221));
#43356=CARTESIAN_POINT('Ctrl Pts',(158.533058618661,4.11521980348147,337.696806462907));
#43357=CARTESIAN_POINT('Ctrl Pts',(158.525283539882,4.18859989036917,337.581382918117));
#43358=CARTESIAN_POINT('Ctrl Pts',(158.517508461104,4.25712345959927,337.46294192222));
#43359=CARTESIAN_POINT('Ctrl Pts',(158.509742950055,4.32556270621511,337.344646675508));
#43360=CARTESIAN_POINT('Ctrl Pts',(158.501977439006,4.38915713233624,337.223341700921));
#43361=CARTESIAN_POINT('Ctrl Pts',(158.494211927957,4.44763325343954,337.099462194325));
#43362=CARTESIAN_POINT('Ctrl Pts',(158.486454116435,4.5060513952982,336.97570551462));
#43363=CARTESIAN_POINT('Ctrl Pts',(158.478696304912,4.55936116552816,336.849379734031));
#43364=CARTESIAN_POINT('Ctrl Pts',(158.47093849339,4.6073340752823,336.720946187782));
#43365=CARTESIAN_POINT('Ctrl Pts',(158.463186519867,4.65527088390076,336.592609291849));
#43366=CARTESIAN_POINT('Ctrl Pts',(158.455434546344,4.6978786897868,336.462168152121));
#43367=CARTESIAN_POINT('Ctrl Pts',(158.447682572821,4.73497653107848,336.330105376516));
#43368=CARTESIAN_POINT('Ctrl Pts',(158.439933882264,4.77205866141234,336.198098529575));
#43369=CARTESIAN_POINT('Ctrl Pts',(158.432185191706,4.80363536277662,336.064471788207));
#43370=CARTESIAN_POINT('Ctrl Pts',(158.424436501148,4.82957516125823,335.929724058126));
#43371=CARTESIAN_POINT('Ctrl Pts',(158.41668942277,4.85550956274804,335.795004363435));
#43372=CARTESIAN_POINT('Ctrl Pts',(158.408942344393,4.875809320304,335.659164527529));
#43373=CARTESIAN_POINT('Ctrl Pts',(158.401195266015,4.89039391949234,335.52271442939));
#43374=CARTESIAN_POINT('Ctrl Pts',(158.393448122709,4.9049786409137,335.386263187667));
#43375=CARTESIAN_POINT('Ctrl Pts',(158.385700979403,4.91384806688786,335.249202062171));
#43376=CARTESIAN_POINT('Ctrl Pts',(158.377953836097,4.91697352595815,335.112046452539));
#43377=CARTESIAN_POINT('Ctrl Pts',(158.370204951069,4.92009968769801,334.974860007415));
#43378=CARTESIAN_POINT('Ctrl Pts',(158.362456066041,4.91747930395742,334.837579426582));
#43379=CARTESIAN_POINT('Ctrl Pts',(158.354707181013,4.90913583151195,334.700720113831));
#43380=CARTESIAN_POINT('Ctrl Pts',(158.346950071238,4.90078350321865,334.563715537192));
#43381=CARTESIAN_POINT('Ctrl Pts',(158.339192961463,4.88669597556864,334.427133512602));
#43382=CARTESIAN_POINT('Ctrl Pts',(158.331435851689,4.86694867314278,334.291484879841));
#43383=CARTESIAN_POINT('Ctrl Pts',(158.323674596763,4.84719081838988,334.155763760788));
#43384=CARTESIAN_POINT('Ctrl Pts',(158.315913341836,4.82176723487931,334.020977411325));
#43385=CARTESIAN_POINT('Ctrl Pts',(158.30815208691,4.7908043204682,333.887625501244));
#43386=CARTESIAN_POINT('Ctrl Pts',(158.300378416506,4.75979187548484,333.754060271566));
#43387=CARTESIAN_POINT('Ctrl Pts',(158.292604746101,4.72322249677057,333.62193444354));
#43388=CARTESIAN_POINT('Ctrl Pts',(158.284831075696,4.68127247557753,333.491732426955));
#43389=CARTESIAN_POINT('Ctrl Pts',(158.277419271519,4.6412752379636,333.367591345566));
#43390=CARTESIAN_POINT('Ctrl Pts',(158.270007467342,4.59638712148911,333.245199269658));
#43391=CARTESIAN_POINT('Ctrl Pts',(158.262595663165,4.54680058049984,333.124956655523));
#43392=CARTESIAN_POINT('Ctrl Pts',(158.254820584386,4.49478365542606,332.998820592686));
#43393=CARTESIAN_POINT('Ctrl Pts',(158.247045505608,4.43743170972269,332.87465140904));
#43394=CARTESIAN_POINT('Ctrl Pts',(158.23927042683,4.37491418463676,332.752933258765));
#43395=CARTESIAN_POINT('Ctrl Pts',(158.231504915781,4.3124735913456,332.631364890423));
#43396=CARTESIAN_POINT('Ctrl Pts',(158.223739404732,4.24488024330886,332.512241898544));
#43397=CARTESIAN_POINT('Ctrl Pts',(158.215973893683,4.17235210784672,332.396029771551));
#43398=CARTESIAN_POINT('Ctrl Pts',(158.20821608216,4.09989588424172,332.27993286922));
#43399=CARTESIAN_POINT('Ctrl Pts',(158.200458270638,4.02251481588706,332.166741417671));
#43400=CARTESIAN_POINT('Ctrl Pts',(158.192700459116,3.940473200989,332.05689721301));
#43401=CARTESIAN_POINT('Ctrl Pts',(158.184948485593,3.85849332500805,331.947135669597));
#43402=CARTESIAN_POINT('Ctrl Pts',(158.17719651207,3.77186011637104,331.840716671212));
#43403=CARTESIAN_POINT('Ctrl Pts',(158.169444538547,3.68088148152566,331.738053559382));
#43404=CARTESIAN_POINT('Ctrl Pts',(158.161695847989,3.58994137618627,331.635433925441));
#43405=CARTESIAN_POINT('Ctrl Pts',(158.153947157432,3.49465976354808,331.53656730635));
#43406=CARTESIAN_POINT('Ctrl Pts',(158.146198466874,3.39538503598947,331.441834247835));
#43407=CARTESIAN_POINT('Ctrl Pts',(158.138451388496,3.29613096336722,331.347120899325));
#43408=CARTESIAN_POINT('Ctrl Pts',(158.130704310118,3.19288571095138,331.256539670423));
#43409=CARTESIAN_POINT('Ctrl Pts',(158.122957231741,3.08603447587614,331.170434192209));
#43410=CARTESIAN_POINT('Ctrl Pts',(158.115210088435,2.97918234528422,331.084327992347));
#43411=CARTESIAN_POINT('Ctrl Pts',(158.107462945129,2.86872447610553,331.002697863253));
#43412=CARTESIAN_POINT('Ctrl Pts',(158.099715801823,2.75507876312124,330.925846827683));
#43413=CARTESIAN_POINT('Ctrl Pts',(158.091966916795,2.64140750016842,330.848978514369));
#43414=CARTESIAN_POINT('Ctrl Pts',(158.084218031767,2.52454729099416,330.776891651514));
#43415=CARTESIAN_POINT('Ctrl Pts',(158.076469146739,2.40494424344854,330.709845428379));
#43416=CARTESIAN_POINT('Ctrl Pts',(158.068712036964,2.28521424799237,330.642728041689));
#43417=CARTESIAN_POINT('Ctrl Pts',(158.060954927189,2.16273594011134,330.580662173654));
#43418=CARTESIAN_POINT('Ctrl Pts',(158.053197817415,2.03797971244386,330.52386084285));
#43419=CARTESIAN_POINT('Ctrl Pts',(158.045436562489,1.91315681903709,330.467029159232));
#43420=CARTESIAN_POINT('Ctrl Pts',(158.037675307562,1.78605394239045,330.415467765261));
#43421=CARTESIAN_POINT('Ctrl Pts',(158.029914052636,1.6571596666253,330.369340770278));
#43422=CARTESIAN_POINT('Ctrl Pts',(158.022140382232,1.52805920202558,330.323139987136));
#43423=CARTESIAN_POINT('Ctrl Pts',(158.014366711827,1.39716198528526,330.282391090947));
#43424=CARTESIAN_POINT('Ctrl Pts',(158.006593041422,1.26497076824122,330.247207976568));
#43425=CARTESIAN_POINT('Ctrl Pts',(157.999181237245,1.13893308415445,330.213662644629));
#43426=CARTESIAN_POINT('Ctrl Pts',(157.991769433068,1.01171944089938,330.185176644288));
#43427=CARTESIAN_POINT('Ctrl Pts',(157.984357628891,0.883770738806445,330.161804846461));
#43428=CARTESIAN_POINT('Ctrl Pts',(157.976582550113,0.749550889683846,330.137287527201));
#43429=CARTESIAN_POINT('Ctrl Pts',(157.968807471334,0.614097945448172,330.118320931796));
#43430=CARTESIAN_POINT('Ctrl Pts',(157.961032392556,0.477910736060523,330.105024577094));
#43431=CARTESIAN_POINT('Ctrl Pts',(157.953266881507,0.341891113704359,330.091744584403));
#43432=CARTESIAN_POINT('Ctrl Pts',(157.945501370458,0.205139409327207,330.084120986626));
#43433=CARTESIAN_POINT('Ctrl Pts',(157.937735859409,0.0681650167000006,
330.082222392889));
#43434=CARTESIAN_POINT('Ctrl Pts',(157.929978047886,-0.0686735654189404,
330.080325681614));
#43435=CARTESIAN_POINT('Ctrl Pts',(157.922220236364,-0.205734008072243,
330.084142683489));
#43436=CARTESIAN_POINT('Ctrl Pts',(157.914462424842,-0.342501768563146,
330.093690225737));
#43437=CARTESIAN_POINT('Ctrl Pts',(157.906710451319,-0.479166606975382,
330.103230583156));
#43438=CARTESIAN_POINT('Ctrl Pts',(157.898958477796,-0.615538813271953,
330.11849287019));
#43439=CARTESIAN_POINT('Ctrl Pts',(157.891206504273,-0.751104173897883,
330.139441844556));
#43440=CARTESIAN_POINT('Ctrl Pts',(157.883457813716,-0.886612122514278,
330.160381947019));
#43441=CARTESIAN_POINT('Ctrl Pts',(157.875709123158,-1.02131351959116,330.187003887275));
#43442=CARTESIAN_POINT('Ctrl Pts',(157.8679604326,-1.15469982100203,330.219220629868));
#43443=CARTESIAN_POINT('Ctrl Pts',(157.860213354223,-1.28805837027858,330.251430669499));
#43444=CARTESIAN_POINT('Ctrl Pts',(157.852466275845,-1.4201019884216,330.289233104388));
#43445=CARTESIAN_POINT('Ctrl Pts',(157.844719197467,-1.55033325645351,330.332489972541));
#43446=CARTESIAN_POINT('Ctrl Pts',(157.836972054161,-1.68056561594917,330.375747203228));
#43447=CARTESIAN_POINT('Ctrl Pts',(157.829224910855,-1.8089852240907,330.424458835146));
#43448=CARTESIAN_POINT('Ctrl Pts',(157.821477767549,-1.93511111573167,330.478437434661));
#43449=CARTESIAN_POINT('Ctrl Pts',(157.813728882521,-2.06126536314975,330.532428169711));
#43450=CARTESIAN_POINT('Ctrl Pts',(157.805979997493,-2.18512450865172,330.591688074874));
#43451=CARTESIAN_POINT('Ctrl Pts',(157.798231112465,-2.30622917990243,330.655982270724));
#43452=CARTESIAN_POINT('Ctrl Pts',(157.790474002691,-2.42746239290329,330.720344709098));
#43453=CARTESIAN_POINT('Ctrl Pts',(157.782716892916,-2.54593494564991,330.789751928622));
#43454=CARTESIAN_POINT('Ctrl Pts',(157.774959783141,-2.66121314982761,330.863923642668));
#43455=CARTESIAN_POINT('Ctrl Pts',(157.767198528215,-2.77655295499194,330.938134991706));
#43456=CARTESIAN_POINT('Ctrl Pts',(157.759437273289,-2.88869469091162,331.017115683429));
#43457=CARTESIAN_POINT('Ctrl Pts',(157.751676018363,-2.99723595363773,331.100543666007));
#43458=CARTESIAN_POINT('Ctrl Pts',(157.743902347958,-3.10595084701051,331.184105106167));
#43459=CARTESIAN_POINT('Ctrl Pts',(157.736128677553,-3.21105345801417,331.272127802395));
#43460=CARTESIAN_POINT('Ctrl Pts',(157.728355007149,-3.3121759421672,331.364250614986));
#43461=CARTESIAN_POINT('Ctrl Pts',(157.720943202972,-3.40859115035515,331.452085088489));
#43462=CARTESIAN_POINT('Ctrl Pts',(157.713531398794,-3.50138823764749,331.543646345776));
#43463=CARTESIAN_POINT('Ctrl Pts',(157.706119594617,-3.59028246545467,331.638593318156));
#43464=CARTESIAN_POINT('Ctrl Pts',(157.69843538853,-3.68244377330101,331.737029823724));
#43465=CARTESIAN_POINT('Ctrl Pts',(157.690751182442,-3.77071663201147,331.839433621995));
#43466=CARTESIAN_POINT('Ctrl Pts',(157.683066976355,-3.85473394334092,331.945460871333));
#43467=CARTESIAN_POINT('Ctrl Pts',(157.675294862694,-3.9397124155088,332.052701075934));
#43468=CARTESIAN_POINT('Ctrl Pts',(157.667522749033,-4.02033702629779,332.163647915457));
#43469=CARTESIAN_POINT('Ctrl Pts',(157.659750635372,-4.09626487565926,332.277905745397));
#43470=CARTESIAN_POINT('Ctrl Pts',(157.652085329165,-4.1711492945344,332.390593399124));
#43471=CARTESIAN_POINT('Ctrl Pts',(157.644420022959,-4.24146497036335,332.506501287287));
#43472=CARTESIAN_POINT('Ctrl Pts',(157.636754716753,-4.30692271572899,332.625215844916));
#43473=CARTESIAN_POINT('Ctrl Pts',(157.62909448777,-4.37233710423443,332.743851770285));
#43474=CARTESIAN_POINT('Ctrl Pts',(157.621434258788,-4.43289976821759,332.865290318654));
#43475=CARTESIAN_POINT('Ctrl Pts',(157.613774029805,-4.48836528415092,332.989089723899));
#43476=CARTESIAN_POINT('Ctrl Pts',(157.606117122602,-4.54380674803161,333.112835444801));
#43477=CARTESIAN_POINT('Ctrl Pts',(157.598460215399,-4.59415529729811,333.238939620846));
#43478=CARTESIAN_POINT('Ctrl Pts',(157.590803308196,-4.63921210000655,333.36693718625));
#43479=CARTESIAN_POINT('Ctrl Pts',(157.582947719888,-4.68543803473639,333.498256027098));
#43480=CARTESIAN_POINT('Ctrl Pts',(157.575092131579,-4.72609365772853,333.631567466467));
#43481=CARTESIAN_POINT('Ctrl Pts',(157.56723654327,-4.76101761804595,333.766349197238));
#43482=CARTESIAN_POINT('Ctrl Pts',(157.559579005358,-4.79506109635081,333.897732891575));
#43483=CARTESIAN_POINT('Ctrl Pts',(157.551921467446,-4.82365839707103,334.030513215732));
#43484=CARTESIAN_POINT('Ctrl Pts',(157.544263929534,-4.84671133777158,334.164193640359));
#43485=CARTESIAN_POINT('Ctrl Pts',(157.536309316027,-4.87065862155782,334.303060221711));
#43486=CARTESIAN_POINT('Ctrl Pts',(157.528354702519,-4.88862259265559,334.442897688675));
#43487=CARTESIAN_POINT('Ctrl Pts',(157.520400089012,-4.9005522594639,334.583141972893));
#43488=CARTESIAN_POINT('Ctrl Pts',(157.512445475505,-4.91248192627221,334.723386257111));
#43489=CARTESIAN_POINT('Ctrl Pts',(157.504490861997,-4.91837729646438,334.864036875012));
#43490=CARTESIAN_POINT('Ctrl Pts',(157.49653624849,-4.91824791444157,335.004529303609));
#43491=CARTESIAN_POINT('',(160.996536248442,-4.91824826623638,334.995870331392));
#43492=CARTESIAN_POINT('Ctrl Pts',(160.996536248442,-4.91824826623638,334.995870331392));
#43493=CARTESIAN_POINT('Ctrl Pts',(160.988888496737,-4.91836138603388,335.130590886655));
#43494=CARTESIAN_POINT('Ctrl Pts',(160.981240745031,-4.91293495396237,335.265506930197));
#43495=CARTESIAN_POINT('Ctrl Pts',(160.973592993325,-4.90194747536038,335.400117496878));
#43496=CARTESIAN_POINT('Ctrl Pts',(160.965952299152,-4.89097013627331,335.534603841624));
#43497=CARTESIAN_POINT('Ctrl Pts',(160.958311604979,-4.87444199050219,335.668784870466));
#43498=CARTESIAN_POINT('Ctrl Pts',(160.950670910806,-4.85239359350145,335.802159258655));
#43499=CARTESIAN_POINT('Ctrl Pts',(160.943007038341,-4.8302783119756,335.935938242363));
#43500=CARTESIAN_POINT('Ctrl Pts',(160.935343165875,-4.80260923420165,336.068905274069));
#43501=CARTESIAN_POINT('Ctrl Pts',(160.927679293409,-4.76946974119217,336.200558807536));
#43502=CARTESIAN_POINT('Ctrl Pts',(160.920045957973,-4.73646229391907,336.331687761832));
#43503=CARTESIAN_POINT('Ctrl Pts',(160.912412622537,-4.69802804746684,336.461513272552));
#43504=CARTESIAN_POINT('Ctrl Pts',(160.904779287102,-4.65430054956791,336.589550079989));
#43505=CARTESIAN_POINT('Ctrl Pts',(160.897146710172,-4.61057739676862,336.717574164706));
#43506=CARTESIAN_POINT('Ctrl Pts',(160.889514133243,-4.5615621687742,336.843809517671));
#43507=CARTESIAN_POINT('Ctrl Pts',(160.881881556314,-4.50743792766208,336.967787181271));
#43508=CARTESIAN_POINT('Ctrl Pts',(160.874247971392,-4.45330653865675,337.091781217924));
#43509=CARTESIAN_POINT('Ctrl Pts',(160.86661438647,-4.39406495682902,337.213516602669));
#43510=CARTESIAN_POINT('Ctrl Pts',(160.858980801548,-4.32994368055142,337.332545987918));
#43511=CARTESIAN_POINT('Ctrl Pts',(160.851293899055,-4.26537454252244,337.452406746341));
#43512=CARTESIAN_POINT('Ctrl Pts',(160.843606996562,-4.1958574744717,337.569523191195));
#43513=CARTESIAN_POINT('Ctrl Pts',(160.835920094069,-4.12167339589594,337.683466318042));
#43514=CARTESIAN_POINT('Ctrl Pts',(160.828275344467,-4.04789612271273,337.796784611644));
#43515=CARTESIAN_POINT('Ctrl Pts',(160.820630594865,-3.96950318168107,337.906964009669));
#43516=CARTESIAN_POINT('Ctrl Pts',(160.812985845263,-3.88681216102772,338.013614820674));
#43517=CARTESIAN_POINT('Ctrl Pts',(160.805277866324,-3.8034372071318,338.121147735134));
#43518=CARTESIAN_POINT('Ctrl Pts',(160.797569887385,-3.71569303168184,338.225093115699));
#43519=CARTESIAN_POINT('Ctrl Pts',(160.789861908447,-3.62394324269666,338.325089237331));
#43520=CARTESIAN_POINT('Ctrl Pts',(160.782153929508,-3.53219345371147,338.425085358962));
#43521=CARTESIAN_POINT('Ctrl Pts',(160.774445950569,-3.43643838960118,338.521131976034));
#43522=CARTESIAN_POINT('Ctrl Pts',(160.766737971631,-3.33707505998658,338.612909230318));
#43523=CARTESIAN_POINT('Ctrl Pts',(160.758962892852,-3.23684674831298,338.705485428021));
#43524=CARTESIAN_POINT('Ctrl Pts',(160.751187814074,-3.13260480339346,338.794033995275));
#43525=CARTESIAN_POINT('Ctrl Pts',(160.743412735296,-3.02470651911524,338.878186887673));
#43526=CARTESIAN_POINT('Ctrl Pts',(160.735647224247,-2.91694101054498,338.96223622458));
#43527=CARTESIAN_POINT('Ctrl Pts',(160.727881713198,-2.80552842031864,339.041900411215));
#43528=CARTESIAN_POINT('Ctrl Pts',(160.720116202149,-2.69086222332686,339.116848741158));
#43529=CARTESIAN_POINT('Ctrl Pts',(160.712358390626,-2.5763097182034,339.191722759613));
#43530=CARTESIAN_POINT('Ctrl Pts',(160.704600579104,-2.45851035123436,339.261890013978));
#43531=CARTESIAN_POINT('Ctrl Pts',(160.696842767582,-2.33788967322245,339.32706077359));
#43532=CARTESIAN_POINT('Ctrl Pts',(160.689090794059,-2.21735976609566,339.392182490138));
#43533=CARTESIAN_POINT('Ctrl Pts',(160.681338820536,-2.09401311640985,339.452315011018));
#43534=CARTESIAN_POINT('Ctrl Pts',(160.673586847013,-1.96830287833509,339.50721275753));
#43535=CARTESIAN_POINT('Ctrl Pts',(160.665838156455,-1.84264587862081,339.562087254813));
#43536=CARTESIAN_POINT('Ctrl Pts',(160.658089465898,-1.71462763886035,339.611731230944));
#43537=CARTESIAN_POINT('Ctrl Pts',(160.65034077534,-1.58472425844211,339.655945885339));
#43538=CARTESIAN_POINT('Ctrl Pts',(160.642593696962,-1.45484790550707,339.700151340506));
#43539=CARTESIAN_POINT('Ctrl Pts',(160.634846618585,-1.32308756186165,339.738929594957));
#43540=CARTESIAN_POINT('Ctrl Pts',(160.627099540207,-1.18993720038836,339.772130815645));
#43541=CARTESIAN_POINT('Ctrl Pts',(160.619352396901,-1.05678572298708,339.805332314592));
#43542=CARTESIAN_POINT('Ctrl Pts',(160.611605253595,-0.922244583783325,
339.832956591977));
#43543=CARTESIAN_POINT('Ctrl Pts',(160.603858110289,-0.786820349727822,
339.854904406861));
#43544=CARTESIAN_POINT('Ctrl Pts',(160.596109225261,-0.651365669429618,
339.876857156079));
#43545=CARTESIAN_POINT('Ctrl Pts',(160.588360340233,-0.515027884974828,
339.893130840803));
#43546=CARTESIAN_POINT('Ctrl Pts',(160.580611455205,-0.378320732445168,
339.90367785299));
#43547=CARTESIAN_POINT('Ctrl Pts',(160.57285434543,-0.241468477530827,339.914236059884));
#43548=CARTESIAN_POINT('Ctrl Pts',(160.565097235656,-0.104246461714505,
339.919055422054));
#43549=CARTESIAN_POINT('Ctrl Pts',(160.557340125881,0.0328289566454363,
339.918140433345));
#43550=CARTESIAN_POINT('Ctrl Pts',(160.549578870955,0.169977623725964,339.917224955695));
#43551=CARTESIAN_POINT('Ctrl Pts',(160.541817616029,0.306979147040823,339.910569040322));
#43552=CARTESIAN_POINT('Ctrl Pts',(160.534056361103,0.443321225932666,339.89822920586));
#43553=CARTESIAN_POINT('Ctrl Pts',(160.526282690698,0.579881407717048,339.885869631683));
#43554=CARTESIAN_POINT('Ctrl Pts',(160.518509020293,0.715779649412491,339.867808020597));
#43555=CARTESIAN_POINT('Ctrl Pts',(160.510735349889,0.850511907688802,339.844152408562));
#43556=CARTESIAN_POINT('Ctrl Pts',(160.503323545711,0.978972346929401,339.821597970959));
#43557=CARTESIAN_POINT('Ctrl Pts',(160.495911741534,1.10637263163476,339.7939586746));
#43558=CARTESIAN_POINT('Ctrl Pts',(160.488499937357,1.23228965352745,339.76137010453));
#43559=CARTESIAN_POINT('Ctrl Pts',(160.480724858579,1.3643782437488,339.727184271565));
#43560=CARTESIAN_POINT('Ctrl Pts',(160.4729497798,1.49525192085116,339.687443706834));
#43561=CARTESIAN_POINT('Ctrl Pts',(160.465174701022,1.6244078362171,339.642249696444));
#43562=CARTESIAN_POINT('Ctrl Pts',(160.457409189973,1.75340481700674,339.597111300161));
#43563=CARTESIAN_POINT('Ctrl Pts',(160.449643678924,1.88068787653359,339.546532938675));
#43564=CARTESIAN_POINT('Ctrl Pts',(160.441878167875,2.00576598487248,339.490666529195));
#43565=CARTESIAN_POINT('Ctrl Pts',(160.434120356352,2.13072007790309,339.434855511422));
#43566=CARTESIAN_POINT('Ctrl Pts',(160.42636254483,2.25347321584484,339.373767038131));
#43567=CARTESIAN_POINT('Ctrl Pts',(160.418604733308,2.37355146804535,339.307602174185));
#43568=CARTESIAN_POINT('Ctrl Pts',(160.410852759785,2.49353935755304,339.241487101396));
#43569=CARTESIAN_POINT('Ctrl Pts',(160.403100786262,2.61085602700582,339.170303429641));
#43570=CARTESIAN_POINT('Ctrl Pts',(160.395348812739,2.7250497363142,339.094299329203));
#43571=CARTESIAN_POINT('Ctrl Pts',(160.387600122181,2.83919508451884,339.018327416547));
#43572=CARTESIAN_POINT('Ctrl Pts',(160.379851431624,2.95021977837428,338.937539351638));
#43573=CARTESIAN_POINT('Ctrl Pts',(160.372102741066,3.05769899753217,338.852227914206));
#43574=CARTESIAN_POINT('Ctrl Pts',(160.364355662688,3.16515585474074,338.766934226532));
#43575=CARTESIAN_POINT('Ctrl Pts',(160.35660858431,3.26906839856009,338.677119281156));
#43576=CARTESIAN_POINT('Ctrl Pts',(160.348861505933,3.36904331411287,338.583117387155));
#43577=CARTESIAN_POINT('Ctrl Pts',(160.341114362627,3.46901906755175,338.489114705327));
#43578=CARTESIAN_POINT('Ctrl Pts',(160.333367219321,3.56505684213524,338.390925272635));
#43579=CARTESIAN_POINT('Ctrl Pts',(160.325620076015,3.65679905159574,338.288921367067));
#43580=CARTESIAN_POINT('Ctrl Pts',(160.317871190987,3.74856188665252,338.186894528855));
#43581=CARTESIAN_POINT('Ctrl Pts',(160.310122305959,3.83602697354957,338.081051801856));
#43582=CARTESIAN_POINT('Ctrl Pts',(160.302373420931,3.91887626559672,337.971799434256));
#43583=CARTESIAN_POINT('Ctrl Pts',(160.294616311156,4.00181349473862,337.862431105064));
#43584=CARTESIAN_POINT('Ctrl Pts',(160.286859201381,4.08012490575982,337.749646217865));
#43585=CARTESIAN_POINT('Ctrl Pts',(160.279102091607,4.1535348464942,337.633881421298));
#43586=CARTESIAN_POINT('Ctrl Pts',(160.27134083668,4.22698401515371,337.518054763725));
#43587=CARTESIAN_POINT('Ctrl Pts',(160.263579581754,4.29552629933025,337.399245362245));
#43588=CARTESIAN_POINT('Ctrl Pts',(160.255818326828,4.35893199146693,337.277914606886));
#43589=CARTESIAN_POINT('Ctrl Pts',(160.248044656423,4.4224391120471,337.156389761861));
#43590=CARTESIAN_POINT('Ctrl Pts',(160.240270986019,4.48079305437756,337.032335857023));
#43591=CARTESIAN_POINT('Ctrl Pts',(160.232497315614,4.53381190143574,336.906235217621));
#43592=CARTESIAN_POINT('Ctrl Pts',(160.225085511437,4.58436270840709,336.786004593323));
#43593=CARTESIAN_POINT('Ctrl Pts',(160.21767370726,4.63006383871998,336.663913766749));
#43594=CARTESIAN_POINT('Ctrl Pts',(160.210261903083,4.67080034056367,336.540391911525));
#43595=CARTESIAN_POINT('Ctrl Pts',(160.202486824305,4.71353345971103,336.410815882221));
#43596=CARTESIAN_POINT('Ctrl Pts',(160.194711745526,4.75093802721173,336.279255515189));
#43597=CARTESIAN_POINT('Ctrl Pts',(160.186936666748,4.78282709647227,336.146188478284));
#43598=CARTESIAN_POINT('Ctrl Pts',(160.179171155699,4.814676924203,336.013285188838));
#43599=CARTESIAN_POINT('Ctrl Pts',(160.17140564465,4.84102466799748,335.878879295031));
#43600=CARTESIAN_POINT('Ctrl Pts',(160.163640133601,4.86173235381075,335.74346592552));
#43601=CARTESIAN_POINT('Ctrl Pts',(160.155882322079,4.88241950789321,335.60818681876));
#43602=CARTESIAN_POINT('Ctrl Pts',(160.148124510556,4.89747767395135,335.471902608088));
#43603=CARTESIAN_POINT('Ctrl Pts',(160.140366699034,4.90681946064763,335.335120639635));
#43604=CARTESIAN_POINT('Ctrl Pts',(160.132614725511,4.91615421735313,335.198441603952));
#43605=CARTESIAN_POINT('Ctrl Pts',(160.124862751988,4.9197811306071,335.061265944464));
#43606=CARTESIAN_POINT('Ctrl Pts',(160.117110778465,4.91766442961309,334.92410783823));
#43607=CARTESIAN_POINT('Ctrl Pts',(160.109362087908,4.9155486250432,334.787007818535));
#43608=CARTESIAN_POINT('Ctrl Pts',(160.10161339735,4.90769405016423,334.649925727324));
#43609=CARTESIAN_POINT('Ctrl Pts',(160.093864706792,4.8941170150312,334.513377245002));
#43610=CARTESIAN_POINT('Ctrl Pts',(160.086117628415,4.88054280471372,334.376857172732));
#43611=CARTESIAN_POINT('Ctrl Pts',(160.078370550037,4.86124854099071,334.240870877234));
#43612=CARTESIAN_POINT('Ctrl Pts',(160.070623471659,4.83630250624762,334.105930019203));
#43613=CARTESIAN_POINT('Ctrl Pts',(160.062876328353,4.81135626243274,333.970988030237));
#43614=CARTESIAN_POINT('Ctrl Pts',(160.055129185047,4.78075822417572,333.837091880575));
#43615=CARTESIAN_POINT('Ctrl Pts',(160.047382041741,4.7446279375319,333.70474373312));
#43616=CARTESIAN_POINT('Ctrl Pts',(160.039633156713,4.70848952803252,333.572365830991));
#43617=CARTESIAN_POINT('Ctrl Pts',(160.031884271685,4.66681649810859,333.441537000599));
#43618=CARTESIAN_POINT('Ctrl Pts',(160.024135386657,4.61977835721469,333.312744538397));
#43619=CARTESIAN_POINT('Ctrl Pts',(160.016378276882,4.57269028955213,333.183815374544));
#43620=CARTESIAN_POINT('Ctrl Pts',(160.008621167108,4.52022586975861,333.056927264257));
#43621=CARTESIAN_POINT('Ctrl Pts',(160.000864057333,4.46260311378447,332.932548304956));
#43622=CARTESIAN_POINT('Ctrl Pts',(159.993102802407,4.40494956605198,332.808102881516));
#43623=CARTESIAN_POINT('Ctrl Pts',(159.985341547481,4.34213236858375,332.686169628044));
#43624=CARTESIAN_POINT('Ctrl Pts',(159.977580292554,4.27441520615785,332.567191395143));
#43625=CARTESIAN_POINT('Ctrl Pts',(159.96980662215,4.20658971834105,332.448022835845));
#43626=CARTESIAN_POINT('Ctrl Pts',(159.962032951745,4.13384880973275,332.331819074693));
#43627=CARTESIAN_POINT('Ctrl Pts',(159.95425928134,4.05649963218452,332.218994103461));
#43628=CARTESIAN_POINT('Ctrl Pts',(159.946847477163,3.98275107745958,332.111421161782));
#43629=CARTESIAN_POINT('Ctrl Pts',(159.939435672986,3.90481380064109,332.00691975448));
#43630=CARTESIAN_POINT('Ctrl Pts',(159.932023868809,3.82298649596497,331.905818797457));
#43631=CARTESIAN_POINT('Ctrl Pts',(159.924248790031,3.73714859133651,331.799762581368));
#43632=CARTESIAN_POINT('Ctrl Pts',(159.916473711252,3.64675842973054,331.697113419032));
#43633=CARTESIAN_POINT('Ctrl Pts',(159.908698632474,3.55211652470703,331.598287011313));
#43634=CARTESIAN_POINT('Ctrl Pts',(159.900933121425,3.45759108257287,331.49958221578));
#43635=CARTESIAN_POINT('Ctrl Pts',(159.893167610376,3.35882457504668,331.404691094571));
#43636=CARTESIAN_POINT('Ctrl Pts',(159.885402099327,3.25615870070829,331.313997615532));
#43637=CARTESIAN_POINT('Ctrl Pts',(159.877644287804,3.15359461988362,331.223394059342));
#43638=CARTESIAN_POINT('Ctrl Pts',(159.869886476282,3.04713915732539,331.136980119872));
#43639=CARTESIAN_POINT('Ctrl Pts',(159.86212866476,2.93717165875148,331.055103840463));
#43640=CARTESIAN_POINT('Ctrl Pts',(159.854376691237,2.827286914207,330.973289175551));
#43641=CARTESIAN_POINT('Ctrl Pts',(159.846624717714,2.71389570650215,330.896005606332));
#43642=CARTESIAN_POINT('Ctrl Pts',(159.838872744191,2.59741106046541,330.823561463942));
#43643=CARTESIAN_POINT('Ctrl Pts',(159.831124053633,2.48097574574546,330.751148001689));
#43644=CARTESIAN_POINT('Ctrl Pts',(159.823375363076,2.36144992956506,330.683570095951));
#43645=CARTESIAN_POINT('Ctrl Pts',(159.815626672518,2.23927608488586,330.621093095514));
#43646=CARTESIAN_POINT('Ctrl Pts',(159.80787959414,2.11712765949555,330.558629093938));
#43647=CARTESIAN_POINT('Ctrl Pts',(159.800132515762,1.99233264926582,330.501264064542));
#43648=CARTESIAN_POINT('Ctrl Pts',(159.792385437385,1.86535827210762,330.449217476172));
#43649=CARTESIAN_POINT('Ctrl Pts',(159.784638294079,1.73838283078182,330.397170451602));
#43650=CARTESIAN_POINT('Ctrl Pts',(159.776891150773,1.60922834776634,330.350442105211));
#43651=CARTESIAN_POINT('Ctrl Pts',(159.769144007467,1.47838179578895,330.309203657333));
#43652=CARTESIAN_POINT('Ctrl Pts',(159.761395122439,1.34750582672902,330.267955938176));
#43653=CARTESIAN_POINT('Ctrl Pts',(159.753646237411,1.21493740445249,330.232200691013));
#43654=CARTESIAN_POINT('Ctrl Pts',(159.745897352383,1.0811780382342,330.202059075797));
#43655=CARTESIAN_POINT('Ctrl Pts',(159.738140242608,0.947276698442352,330.17188546796));
#43656=CARTESIAN_POINT('Ctrl Pts',(159.730383132833,0.812182271505018,330.147337480529));
#43657=CARTESIAN_POINT('Ctrl Pts',(159.722626023059,0.676406371469306,330.128485093615));
#43658=CARTESIAN_POINT('Ctrl Pts',(159.714864768133,0.54055791713391,330.109622632587));
#43659=CARTESIAN_POINT('Ctrl Pts',(159.707103513206,0.404027652957149,330.096461874102));
#43660=CARTESIAN_POINT('Ctrl Pts',(159.69934225828,0.267330676423168,330.089020731876));
#43661=CARTESIAN_POINT('Ctrl Pts',(159.691568587876,0.130415029276243,330.081567686248));
#43662=CARTESIAN_POINT('Ctrl Pts',(159.683794917471,-0.00666747209512181,
330.079852545226));
#43663=CARTESIAN_POINT('Ctrl Pts',(159.676021247066,-0.143402475685821,
330.08384105297));
#43664=CARTESIAN_POINT('Ctrl Pts',(159.668609442889,-0.273772431963202,
330.087643894718));
#43665=CARTESIAN_POINT('Ctrl Pts',(159.661197638712,-0.403826227329201,
330.096631305733));
#43666=CARTESIAN_POINT('Ctrl Pts',(159.653785834535,-0.533125628792797,
330.110730102927));
#43667=CARTESIAN_POINT('Ctrl Pts',(159.646010755756,-0.668762379084622,
330.12551992417));
#43668=CARTESIAN_POINT('Ctrl Pts',(159.638235676978,-0.803997552647739,
330.145981587706));
#43669=CARTESIAN_POINT('Ctrl Pts',(159.6304605982,-0.938318952627116,330.172087344862));
#43670=CARTESIAN_POINT('Ctrl Pts',(159.622695087151,-1.07247506157325,330.198160977222));
#43671=CARTESIAN_POINT('Ctrl Pts',(159.614929576102,-1.20571925425497,330.229864809954));
#43672=CARTESIAN_POINT('Ctrl Pts',(159.607164065053,-1.33754373121088,330.267119288467));
#43673=CARTESIAN_POINT('Ctrl Pts',(159.59940625353,-1.46923750381394,330.304336829056));
#43674=CARTESIAN_POINT('Ctrl Pts',(159.591648442008,-1.59951398827963,330.347093957571));
#43675=CARTESIAN_POINT('Ctrl Pts',(159.583890630486,-1.72787522180085,330.395260020328));
#43676=CARTESIAN_POINT('Ctrl Pts',(159.576138656963,-1.85613985942228,330.443389836595));
#43677=CARTESIAN_POINT('Ctrl Pts',(159.56838668344,-1.98249175042594,330.496920348415));
#43678=CARTESIAN_POINT('Ctrl Pts',(159.560634709917,-2.10644810114723,330.555671090066));
#43679=CARTESIAN_POINT('Ctrl Pts',(159.552886019359,-2.23035195628102,330.614396950744));
#43680=CARTESIAN_POINT('Ctrl Pts',(159.545137328802,-2.35186193645208,330.678338477128));
#43681=CARTESIAN_POINT('Ctrl Pts',(159.537388638244,-2.47051545669817,330.747267179717));
#43682=CARTESIAN_POINT('Ctrl Pts',(159.529641559866,-2.58914429008816,330.816181541113));
#43683=CARTESIAN_POINT('Ctrl Pts',(159.521894481488,-2.70491750790789,330.890080818589));
#43684=CARTESIAN_POINT('Ctrl Pts',(159.514147403111,-2.81739771570163,330.968690885821));
#43685=CARTESIAN_POINT('Ctrl Pts',(159.506400259805,-2.92987886618784,331.047301611882));
#43686=CARTESIAN_POINT('Ctrl Pts',(159.498653116499,-3.03906663121529,331.130622982536));
#43687=CARTESIAN_POINT('Ctrl Pts',(159.490905973193,-3.1445534990683,331.218338149173));
#43688=CARTESIAN_POINT('Ctrl Pts',(159.483157088165,-3.2500640826087,331.306073036043));
#43689=CARTESIAN_POINT('Ctrl Pts',(159.475408203137,-3.35187181282146,331.398203434683));
#43690=CARTESIAN_POINT('Ctrl Pts',(159.467659318109,-3.44960340827078,331.494373181848));
#43691=CARTESIAN_POINT('Ctrl Pts',(159.459902208334,-3.54743873704552,331.590645004577));
#43692=CARTESIAN_POINT('Ctrl Pts',(159.452145098559,-3.64118900951678,331.69096446574));
#43693=CARTESIAN_POINT('Ctrl Pts',(159.444387988785,-3.73051851420033,331.794939208422));
#43694=CARTESIAN_POINT('Ctrl Pts',(159.436626733858,-3.81989575371496,331.898969511883));
#43695=CARTESIAN_POINT('Ctrl Pts',(159.428865478932,-3.90484727634865,332.006658682194));
#43696=CARTESIAN_POINT('Ctrl Pts',(159.421104224006,-3.98507926926955,332.117583257033));
#43697=CARTESIAN_POINT('Ctrl Pts',(159.413330553601,-4.06543960723152,332.228685275041));
#43698=CARTESIAN_POINT('Ctrl Pts',(159.405556883197,-4.14106511319184,332.343032713749));
#43699=CARTESIAN_POINT('Ctrl Pts',(159.397783212792,-4.21170624823518,332.460174505783));
#43700=CARTESIAN_POINT('Ctrl Pts',(159.390371408615,-4.27905902144712,332.571863319214));
#43701=CARTESIAN_POINT('Ctrl Pts',(159.382959604438,-4.34188088694468,332.686091934111));
#43702=CARTESIAN_POINT('Ctrl Pts',(159.375547800261,-4.39999623292924,332.802452227434));
#43703=CARTESIAN_POINT('Ctrl Pts',(159.367226760812,-4.46524081777695,332.933086897193));
#43704=CARTESIAN_POINT('Ctrl Pts',(159.358905721363,-4.52473714990775,333.066776016648));
#43705=CARTESIAN_POINT('Ctrl Pts',(159.350584681915,-4.57820922808688,333.203007143487));
#43706=CARTESIAN_POINT('Ctrl Pts',(159.341913979133,-4.63392828817218,333.344962919292));
#43707=CARTESIAN_POINT('Ctrl Pts',(159.333243276352,-4.68310559610706,333.489678738939));
#43708=CARTESIAN_POINT('Ctrl Pts',(159.32457257357,-4.72548118704292,333.636544605275));
#43709=CARTESIAN_POINT('Ctrl Pts',(159.316291958506,-4.76595033533406,333.776803098252));
#43710=CARTESIAN_POINT('Ctrl Pts',(159.308011343441,-4.80021621604412,333.919022072236));
#43711=CARTESIAN_POINT('Ctrl Pts',(159.299730728377,-4.82810048408559,334.06264799671));
#43712=CARTESIAN_POINT('Ctrl Pts',(159.291464605672,-4.85593595033821,334.206022553565));
#43713=CARTESIAN_POINT('Ctrl Pts',(159.283198482967,-4.87741200318246,334.350798854617));
#43714=CARTESIAN_POINT('Ctrl Pts',(159.274932360262,-4.89240012795802,334.496408845931));
#43715=CARTESIAN_POINT('Ctrl Pts',(159.266685408795,-4.90735349146548,334.641681130693));
#43716=CARTESIAN_POINT('Ctrl Pts',(159.258438457328,-4.91584889819635,334.78778294644));
#43717=CARTESIAN_POINT('Ctrl Pts',(159.250191505861,-4.91780897882096,334.934137185545));
#43718=CARTESIAN_POINT('Ctrl Pts',(159.248973086752,-4.91809856457844,334.955759818134));
#43719=CARTESIAN_POINT('Ctrl Pts',(159.247754667644,-4.91824559059081,334.97738794205));
#43720=CARTESIAN_POINT('Ctrl Pts',(159.246536248535,-4.91824990229953,334.999019678274));
#43721=CARTESIAN_POINT('',(162.746536248527,-4.91824899084518,335.003150642852));
#43722=CARTESIAN_POINT('Ctrl Pts',(162.74653624849,-4.91824899084476,335.003150643507));
#43723=CARTESIAN_POINT('Ctrl Pts',(162.735825569509,-4.91812835470727,335.191467271566));
#43724=CARTESIAN_POINT('Ctrl Pts',(162.725114890528,-4.90719245495907,335.379437381484));
#43725=CARTESIAN_POINT('Ctrl Pts',(162.714404211548,-4.88555668033054,335.566143962061));
#43726=CARTESIAN_POINT('Ctrl Pts',(162.706629132769,-4.86985087377294,335.701677701338));
#43727=CARTESIAN_POINT('Ctrl Pts',(162.698854053991,-4.84847606729068,335.836771555718));
#43728=CARTESIAN_POINT('Ctrl Pts',(162.691078975213,-4.82146346917885,335.970913527496));
#43729=CARTESIAN_POINT('Ctrl Pts',(162.683313464164,-4.79448411178871,336.104890429037));
#43730=CARTESIAN_POINT('Ctrl Pts',(162.675547953115,-4.76188084315117,336.237917399112));
#43731=CARTESIAN_POINT('Ctrl Pts',(162.667782442066,-4.72373664658983,336.369487187295));
#43732=CARTESIAN_POINT('Ctrl Pts',(162.660024630544,-4.68563027011051,336.500926523649));
#43733=CARTESIAN_POINT('Ctrl Pts',(162.652266819021,-4.6419940069098,336.630911180349));
#43734=CARTESIAN_POINT('Ctrl Pts',(162.644509007499,-4.59296187178296,336.758944088608));
#43735=CARTESIAN_POINT('Ctrl Pts',(162.636757033976,-4.54396663489257,336.886880648044));
#43736=CARTESIAN_POINT('Ctrl Pts',(162.629005060453,-4.48958374765954,337.012868018967));
#43737=CARTESIAN_POINT('Ctrl Pts',(162.62125308693,-4.42999693330044,337.136424637905));
#43738=CARTESIAN_POINT('Ctrl Pts',(162.613504396373,-4.3704353539926,337.259928930542));
#43739=CARTESIAN_POINT('Ctrl Pts',(162.605755705815,-4.30567440033075,337.381004167309));
#43740=CARTESIAN_POINT('Ctrl Pts',(162.598007015257,-4.23594568169184,337.49918931741));
#43741=CARTESIAN_POINT('Ctrl Pts',(162.59025993688,-4.16623147069527,337.617349878103));
#43742=CARTESIAN_POINT('Ctrl Pts',(162.582512858502,-4.09155174909183,337.732621211734));
#43743=CARTESIAN_POINT('Ctrl Pts',(162.574765780124,-4.01218359185996,337.844567785747));
#43744=CARTESIAN_POINT('Ctrl Pts',(162.567018636818,-3.93281476944641,337.95651529798));
#43745=CARTESIAN_POINT('Ctrl Pts',(162.559271493512,-3.84875765910029,338.065137676152));
#43746=CARTESIAN_POINT('Ctrl Pts',(162.551524350206,-3.76033185523241,338.170029558383));
#43747=CARTESIAN_POINT('Ctrl Pts',(162.543775465178,-3.67188617136659,338.274945022537));
#43748=CARTESIAN_POINT('Ctrl Pts',(162.53602658015,-3.57907009144691,338.376128023051));
#43749=CARTESIAN_POINT('Ctrl Pts',(162.528277695122,-3.48224229237244,338.473207693144));
#43750=CARTESIAN_POINT('Ctrl Pts',(162.520520585347,-3.38531171927157,338.570390404601));
#43751=CARTESIAN_POINT('Ctrl Pts',(162.512763475573,-3.28436119756791,338.663460808298));
#43752=CARTESIAN_POINT('Ctrl Pts',(162.505006365798,-3.17978534319233,338.752085851059));
#43753=CARTESIAN_POINT('Ctrl Pts',(162.497245110872,-3.07515360682391,338.84075825221));
#43754=CARTESIAN_POINT('Ctrl Pts',(162.489483855946,-2.96689298596905,338.924980319224));
#43755=CARTESIAN_POINT('Ctrl Pts',(162.481722601019,-2.85542891820251,339.004461106765));
#43756=CARTESIAN_POINT('Ctrl Pts',(162.473948930615,-2.74378654425357,339.084069037663));
#43757=CARTESIAN_POINT('Ctrl Pts',(162.46617526021,-2.62893081082613,339.158920319481));
#43758=CARTESIAN_POINT('Ctrl Pts',(162.458401589805,-2.51131446081569,339.228768466279));
#43759=CARTESIAN_POINT('Ctrl Pts',(162.450989785628,-2.39917318019426,339.29536516504));
#43760=CARTESIAN_POINT('Ctrl Pts',(162.443577981451,-2.28452276557371,339.357413901315));
#43761=CARTESIAN_POINT('Ctrl Pts',(162.436166177274,-2.16777251706213,339.414741824475));
#43762=CARTESIAN_POINT('Ctrl Pts',(162.428391098496,-2.04529999109075,339.47487955992));
#43763=CARTESIAN_POINT('Ctrl Pts',(162.420616019717,-1.92012955256796,339.530012065426));
#43764=CARTESIAN_POINT('Ctrl Pts',(162.412840940939,-1.79270863988575,339.579888513379));
#43765=CARTESIAN_POINT('Ctrl Pts',(162.40507542989,-1.66544452674867,339.629703585187));
#43766=CARTESIAN_POINT('Ctrl Pts',(162.397309918841,-1.53593581017178,339.674275327623));
#43767=CARTESIAN_POINT('Ctrl Pts',(162.389544407792,-1.40465395489751,339.713399020823));
#43768=CARTESIAN_POINT('Ctrl Pts',(162.381786596269,-1.27350226596498,339.752483922766));
#43769=CARTESIAN_POINT('Ctrl Pts',(162.374028784747,-1.14058130917899,339.78613141436));
#43770=CARTESIAN_POINT('Ctrl Pts',(162.366270973225,-1.00638160338075,339.814185199063));
#43771=CARTESIAN_POINT('Ctrl Pts',(162.358518999702,-0.872282887116861,
339.842217872403));
#43772=CARTESIAN_POINT('Ctrl Pts',(162.350767026179,-0.73690771831346,339.864665137881));
#43773=CARTESIAN_POINT('Ctrl Pts',(162.343015052656,-0.600760477143031,
339.881420890643));
#43774=CARTESIAN_POINT('Ctrl Pts',(162.335266362098,-0.464670894410022,
339.898169547333));
#43775=CARTESIAN_POINT('Ctrl Pts',(162.327517671541,-0.327810276776393,
339.909231437694));
#43776=CARTESIAN_POINT('Ctrl Pts',(162.319768980983,-0.190691651998446,
339.914551836776));
#43777=CARTESIAN_POINT('Ctrl Pts',(162.312021902605,-0.0536015558956443,
339.919871128904));
#43778=CARTESIAN_POINT('Ctrl Pts',(162.304274824228,0.0837460502419204,
339.919451290681));
#43779=CARTESIAN_POINT('Ctrl Pts',(162.29652774585,0.220834976626965,339.913289628711));
#43780=CARTESIAN_POINT('Ctrl Pts',(162.288780602544,0.357925051949207,339.9071279151));
#43781=CARTESIAN_POINT('Ctrl Pts',(162.281033459238,0.494756052714651,339.895224299309));
#43782=CARTESIAN_POINT('Ctrl Pts',(162.273286315932,0.630814150597845,339.877628170526));
#43783=CARTESIAN_POINT('Ctrl Pts',(162.265537430904,0.766902837229969,339.860028085759));
#43784=CARTESIAN_POINT('Ctrl Pts',(162.257788545876,0.902217887636804,339.836732991467));
#43785=CARTESIAN_POINT('Ctrl Pts',(162.250039660848,1.036253331379,339.807843809412));
#43786=CARTESIAN_POINT('Ctrl Pts',(162.242282551073,1.17043104172609,339.778923964081));
#43787=CARTESIAN_POINT('Ctrl Pts',(162.234525441299,1.30332604959777,339.744398252514));
#43788=CARTESIAN_POINT('Ctrl Pts',(162.226768331524,1.43444473415226,339.704418281484));
#43789=CARTESIAN_POINT('Ctrl Pts',(162.219007076598,1.56563348433942,339.664416946436));
#43790=CARTESIAN_POINT('Ctrl Pts',(162.211245821671,1.69504365122858,339.618955673842));
#43791=CARTESIAN_POINT('Ctrl Pts',(162.203484566745,1.82220034399506,339.568234776021));
#43792=CARTESIAN_POINT('Ctrl Pts',(162.195710896341,1.94956044602968,339.517432741292));
#43793=CARTESIAN_POINT('Ctrl Pts',(162.187937225936,2.07465951357069,339.461354428271));
#43794=CARTESIAN_POINT('Ctrl Pts',(162.180163555531,2.19704526617383,339.400247170431));
#43795=CARTESIAN_POINT('Ctrl Pts',(162.172751751354,2.31373393254928,339.341984470144));
#43796=CARTESIAN_POINT('Ctrl Pts',(162.165339947177,2.42795595662479,339.279150622085));
#43797=CARTESIAN_POINT('Ctrl Pts',(162.157928143,2.53934448884438,339.211996276052));
#43798=CARTESIAN_POINT('Ctrl Pts',(162.150153064222,2.65619250483726,339.141550495477));
#43799=CARTESIAN_POINT('Ctrl Pts',(162.142377985443,2.77029151148098,339.066127365561));
#43800=CARTESIAN_POINT('Ctrl Pts',(162.134602906665,2.8811884478948,338.985967409578));
#43801=CARTESIAN_POINT('Ctrl Pts',(162.126837395616,2.99194891856831,338.905906095524));
#43802=CARTESIAN_POINT('Ctrl Pts',(162.119071884567,3.0995148454276,338.821119780165));
#43803=CARTESIAN_POINT('Ctrl Pts',(162.111306373518,3.20345893854672,338.731894142596));
#43804=CARTESIAN_POINT('Ctrl Pts',(162.103548561995,3.30729997079486,338.642756972507));
#43805=CARTESIAN_POINT('Ctrl Pts',(162.095790750473,3.40752602103372,338.549189492596));
#43806=CARTESIAN_POINT('Ctrl Pts',(162.088032938951,3.50374020827666,338.451519609593));
#43807=CARTESIAN_POINT('Ctrl Pts',(162.080280965428,3.59988199129257,338.353923226275));
#43808=CARTESIAN_POINT('Ctrl Pts',(162.072528991905,3.69201764738974,338.252230862099));
#43809=CARTESIAN_POINT('Ctrl Pts',(162.064777018382,3.77978500167942,338.146809241689));
#43810=CARTESIAN_POINT('Ctrl Pts',(162.057028327824,3.86751518644246,338.041432267397));
#43811=CARTESIAN_POINT('Ctrl Pts',(162.049279637267,3.95088049930486,337.932329477842));
#43812=CARTESIAN_POINT('Ctrl Pts',(162.041530946709,4.02955729213068,337.819902674196));
#43813=CARTESIAN_POINT('Ctrl Pts',(162.033783868331,4.10821771559263,337.707499261885));
#43814=CARTESIAN_POINT('Ctrl Pts',(162.026036789953,4.18219133535917,337.591773531149));
#43815=CARTESIAN_POINT('Ctrl Pts',(162.018289711576,4.25119654658299,337.473158099439));
#43816=CARTESIAN_POINT('Ctrl Pts',(162.01054256827,4.32020233613688,337.354541673618));
#43817=CARTESIAN_POINT('Ctrl Pts',(162.002795424964,4.38423943754145,337.233035836379));
#43818=CARTESIAN_POINT('Ctrl Pts',(161.995048281658,4.44307132122676,337.109099404246));
#43819=CARTESIAN_POINT('Ctrl Pts',(161.98729939663,4.50191643156854,336.985135108572));
#43820=CARTESIAN_POINT('Ctrl Pts',(161.979550511602,4.55555382795097,336.858739483672));
#43821=CARTESIAN_POINT('Ctrl Pts',(161.971801626574,4.60379456799849,336.730392625437));
#43822=CARTESIAN_POINT('Ctrl Pts',(161.964044516799,4.65208651126594,336.601909538521));
#43823=CARTESIAN_POINT('Ctrl Pts',(161.956287407024,4.6949702181088,336.471471447597));
#43824=CARTESIAN_POINT('Ctrl Pts',(161.94853029725,4.73230605133504,336.339575492086));
#43825=CARTESIAN_POINT('Ctrl Pts',(161.940769042323,4.76966183563678,336.207609055593));
#43826=CARTESIAN_POINT('Ctrl Pts',(161.933007787397,4.8014637484968,336.074183582244));
#43827=CARTESIAN_POINT('Ctrl Pts',(161.925246532471,4.82762324614092,335.939806818351));
#43828=CARTESIAN_POINT('Ctrl Pts',(161.917472862066,4.8538245904559,335.80521509543));
#43829=CARTESIAN_POINT('Ctrl Pts',(161.909699191662,4.87436542428713,335.669669427714));
#43830=CARTESIAN_POINT('Ctrl Pts',(161.901925521257,4.88920898072962,335.533683993814));
#43831=CARTESIAN_POINT('Ctrl Pts',(161.89451371708,4.90336156604838,335.404028714579));
#43832=CARTESIAN_POINT('Ctrl Pts',(161.887101912903,4.91233533399939,335.273973977125));
#43833=CARTESIAN_POINT('Ctrl Pts',(161.879690108726,4.91614253800159,335.143963914059));
#43834=CARTESIAN_POINT('Ctrl Pts',(161.871915029948,4.92013634441305,335.007581670521));
#43835=CARTESIAN_POINT('Ctrl Pts',(161.864139951169,4.91845694487922,334.870817598263));
#43836=CARTESIAN_POINT('Ctrl Pts',(161.856364872391,4.91106142331369,334.734182846791));
#43837=CARTESIAN_POINT('Ctrl Pts',(161.848599361342,4.90367500240827,334.597716233079));
#43838=CARTESIAN_POINT('Ctrl Pts',(161.840833850293,4.89058647614153,334.461379010087));
#43839=CARTESIAN_POINT('Ctrl Pts',(161.833068339244,4.87180484706228,334.325685092379));
#43840=CARTESIAN_POINT('Ctrl Pts',(161.825310527722,4.85304184002295,334.190125715585));
#43841=CARTESIAN_POINT('Ctrl Pts',(161.817552716199,4.82859701674449,334.055208759429));
#43842=CARTESIAN_POINT('Ctrl Pts',(161.809794904677,4.79853134591831,333.921445418748));
#43843=CARTESIAN_POINT('Ctrl Pts',(161.802042931154,4.76848830046288,333.787782739223));
#43844=CARTESIAN_POINT('Ctrl Pts',(161.794290957631,4.73283291217347,333.655272327021));
#43845=CARTESIAN_POINT('Ctrl Pts',(161.786538984108,4.69167757399479,333.524417198469));
#43846=CARTESIAN_POINT('Ctrl Pts',(161.778790293551,4.65053966512626,333.393617487142));
#43847=CARTESIAN_POINT('Ctrl Pts',(161.771041602993,4.60390655607368,333.26447203729));
#43848=CARTESIAN_POINT('Ctrl Pts',(161.763292912435,4.55194098543875,333.137470449205));
#43849=CARTESIAN_POINT('Ctrl Pts',(161.755545834057,4.49998622667481,333.010495284862));
#43850=CARTESIAN_POINT('Ctrl Pts',(161.74779875568,4.44270136105948,332.8856634566));
#43851=CARTESIAN_POINT('Ctrl Pts',(161.740051677302,4.38029779329731,332.763445886071));
#43852=CARTESIAN_POINT('Ctrl Pts',(161.732304533996,4.31789370253317,332.64122729124));
#43853=CARTESIAN_POINT('Ctrl Pts',(161.72455739069,4.25037100180412,332.521623345964));
#43854=CARTESIAN_POINT('Ctrl Pts',(161.716810247384,4.1779875199909,332.405081244952));
#43855=CARTESIAN_POINT('Ctrl Pts',(161.709061362356,4.10558776483425,332.288512942801));
#43856=CARTESIAN_POINT('Ctrl Pts',(161.701312477328,4.02832526021898,332.175008186667));
#43857=CARTESIAN_POINT('Ctrl Pts',(161.6935635923,3.94650148146258,332.064985669658));
#43858=CARTESIAN_POINT('Ctrl Pts',(161.685806482525,3.86459085410195,331.954846373613));
#43859=CARTESIAN_POINT('Ctrl Pts',(161.678049372751,3.77810951510899,331.84819701411));
#43860=CARTESIAN_POINT('Ctrl Pts',(161.670292262976,3.68739995393148,331.745424045709));
#43861=CARTESIAN_POINT('Ctrl Pts',(161.66253100805,3.59664192046482,331.642596158721));
#43862=CARTESIAN_POINT('Ctrl Pts',(161.654769753124,3.5016514332598,331.543649072151));
#43863=CARTESIAN_POINT('Ctrl Pts',(161.647008498198,3.40280755090739,331.448932015015));
#43864=CARTESIAN_POINT('Ctrl Pts',(161.639234827793,3.30380555055638,331.354063441455));
#43865=CARTESIAN_POINT('Ctrl Pts',(161.631461157388,3.20093813065343,331.263438677657));
#43866=CARTESIAN_POINT('Ctrl Pts',(161.623687486984,3.09461777827886,331.177366893245));
#43867=CARTESIAN_POINT('Ctrl Pts',(161.616275682806,2.99324666388503,331.095301771104));
#43868=CARTESIAN_POINT('Ctrl Pts',(161.608863878629,2.88873708131458,331.017375457209));
#43869=CARTESIAN_POINT('Ctrl Pts',(161.601452074452,2.78146914217968,330.943817993038));
#43870=CARTESIAN_POINT('Ctrl Pts',(161.593676995674,2.6689436818145,330.866655258432));
#43871=CARTESIAN_POINT('Ctrl Pts',(161.585901916895,2.55302703626747,330.794056614309));
#43872=CARTESIAN_POINT('Ctrl Pts',(161.578126838117,2.43412581770559,330.726334762048));
#43873=CARTESIAN_POINT('Ctrl Pts',(161.570361327068,2.31537091466275,330.658696245838));
#43874=CARTESIAN_POINT('Ctrl Pts',(161.562595816019,2.19363908263863,330.595922772417));
#43875=CARTESIAN_POINT('Ctrl Pts',(161.55483030497,2.0693673551506,330.538284880011));
#43876=CARTESIAN_POINT('Ctrl Pts',(161.547072493447,1.94521884344229,330.480704135743));
#43877=CARTESIAN_POINT('Ctrl Pts',(161.539314681925,1.81853580016415,330.428249002637));
#43878=CARTESIAN_POINT('Ctrl Pts',(161.531556870403,1.68978109361745,330.381144847676));
#43879=CARTESIAN_POINT('Ctrl Pts',(161.52380489688,1.56112327907038,330.334076140085));
#43880=CARTESIAN_POINT('Ctrl Pts',(161.516052923357,1.43039726995477,330.292350529284));
#43881=CARTESIAN_POINT('Ctrl Pts',(161.508300949834,1.29808688570233,330.256145712644));
#43882=CARTESIAN_POINT('Ctrl Pts',(161.500552259276,1.16583253497618,330.219956228765));
#43883=CARTESIAN_POINT('Ctrl Pts',(161.492803568719,1.03199551988241,330.189282991762));
#43884=CARTESIAN_POINT('Ctrl Pts',(161.485054878161,0.897075622947639,330.164254102084));
#43885=CARTESIAN_POINT('Ctrl Pts',(161.477307799783,0.762183797224345,330.139230419875));
#43886=CARTESIAN_POINT('Ctrl Pts',(161.469560721405,0.626209921878928,330.119848820369));
#43887=CARTESIAN_POINT('Ctrl Pts',(161.461813643028,0.489664408190774,330.106186371566));
#43888=CARTESIAN_POINT('Ctrl Pts',(161.454066499722,0.353117750119721,330.092523808258));
#43889=CARTESIAN_POINT('Ctrl Pts',(161.446319356416,0.215999833082388,330.084580530173));
#43890=CARTESIAN_POINT('Ctrl Pts',(161.43857221311,0.078826238651887,330.082381726222));
#43891=CARTESIAN_POINT('Ctrl Pts',(161.430823328082,-0.0583781953148501,
330.080182427932));
#43892=CARTESIAN_POINT('Ctrl Pts',(161.423074443054,-0.19563794083539,330.083730179941));
#43893=CARTESIAN_POINT('Ctrl Pts',(161.415325558026,-0.332437764348275,
330.092998044087));
#43894=CARTESIAN_POINT('Ctrl Pts',(161.407568448251,-0.46938278860729,330.10227574524));
#43895=CARTESIAN_POINT('Ctrl Pts',(161.399811338476,-0.605866525105003,
330.117285660232));
#43896=CARTESIAN_POINT('Ctrl Pts',(161.392054228702,-0.7413786552649,330.137948915116));
#43897=CARTESIAN_POINT('Ctrl Pts',(161.384292973775,-0.876963198774339,
330.158623211784));
#43898=CARTESIAN_POINT('Ctrl Pts',(161.376531718849,-1.01157471799402,330.184956792883));
#43899=CARTESIAN_POINT('Ctrl Pts',(161.368770463923,-1.14471440844185,330.216819887815));
#43900=CARTESIAN_POINT('Ctrl Pts',(161.360996793518,-1.27806707900423,330.248733953314));
#43901=CARTESIAN_POINT('Ctrl Pts',(161.353223123114,-1.40994283971743,330.286195101552));
#43902=CARTESIAN_POINT('Ctrl Pts',(161.345449452709,-1.53985848282114,330.329023772766));
#43903=CARTESIAN_POINT('Ctrl Pts',(161.338037648532,-1.66372652148162,330.369858759031));
#43904=CARTESIAN_POINT('Ctrl Pts',(161.330625844355,-1.78581255320543,330.415572696768));
#43905=CARTESIAN_POINT('Ctrl Pts',(161.323214040178,-1.90571743100325,330.465970430658));
#43906=CARTESIAN_POINT('Ctrl Pts',(161.3154389614,-2.03149920404092,330.518838307612));
#43907=CARTESIAN_POINT('Ctrl Pts',(161.307663882621,-2.15527810090941,330.577027795782));
#43908=CARTESIAN_POINT('Ctrl Pts',(161.299888803843,-2.27657112317238,330.640366186979));
#43909=CARTESIAN_POINT('Ctrl Pts',(161.292123292794,-2.3977148866496,330.703626636253));
#43910=CARTESIAN_POINT('Ctrl Pts',(161.284357781745,-2.51637851894135,330.772023202428));
#43911=CARTESIAN_POINT('Ctrl Pts',(161.276592270696,-2.63209801476996,330.845334778452));
#43912=CARTESIAN_POINT('Ctrl Pts',(161.268834459174,-2.74770277438154,330.918573665834));
#43913=CARTESIAN_POINT('Ctrl Pts',(161.261076647651,-2.86036887868161,330.996717657191));
#43914=CARTESIAN_POINT('Ctrl Pts',(161.253318836129,-2.96965632716724,331.079499475703));
#43915=CARTESIAN_POINT('Ctrl Pts',(161.245566862606,-3.07886153338226,331.16221899827));
#43916=CARTESIAN_POINT('Ctrl Pts',(161.237814889083,-3.18469283427131,331.249569166033));
#43917=CARTESIAN_POINT('Ctrl Pts',(161.23006291556,-3.28673897786701,331.341239287153));
#43918=CARTESIAN_POINT('Ctrl Pts',(161.222314225003,-3.38874190486018,331.432870585923));
#43919=CARTESIAN_POINT('Ctrl Pts',(161.214565534445,-3.48696257267444,331.52881793863));
#43920=CARTESIAN_POINT('Ctrl Pts',(161.206816843887,-3.58102279790618,331.62873038999));
#43921=CARTESIAN_POINT('Ctrl Pts',(161.19906976551,-3.6750634531224,331.72862205373));
#43922=CARTESIAN_POINT('Ctrl Pts',(161.191322687132,-3.76494511976427,331.832476890774));
#43923=CARTESIAN_POINT('Ctrl Pts',(161.183575608754,-3.85032677687502,331.939907391307));
#43924=CARTESIAN_POINT('Ctrl Pts',(161.175828465448,-3.93570914956624,332.04733879221));
#43925=CARTESIAN_POINT('Ctrl Pts',(161.168081322142,-4.01659119430352,332.158345610372));
#43926=CARTESIAN_POINT('Ctrl Pts',(161.160334178837,-4.09267271842105,332.272507913414));
#43927=CARTESIAN_POINT('Ctrl Pts',(161.152585293808,-4.16877134728048,332.386695882564));
#43928=CARTESIAN_POINT('Ctrl Pts',(161.14483640878,-4.24006709119236,332.504040423062));
#43929=CARTESIAN_POINT('Ctrl Pts',(161.137087523752,-4.30630378058577,332.62409368623));
#43930=CARTESIAN_POINT('Ctrl Pts',(161.129330413978,-4.37261077428567,332.744274375171));
#43931=CARTESIAN_POINT('Ctrl Pts',(161.121573304203,-4.43384779780058,332.867169187216));
#43932=CARTESIAN_POINT('Ctrl Pts',(161.113816194428,-4.48980501525064,332.992306301367));
#43933=CARTESIAN_POINT('Ctrl Pts',(161.106054939502,-4.54579213444854,333.117510284791));
#43934=CARTESIAN_POINT('Ctrl Pts',(161.098293684576,-4.59649368135744,333.244958594867));
#43935=CARTESIAN_POINT('Ctrl Pts',(161.09053242965,-4.64174885111503,333.374161549947));
#43936=CARTESIAN_POINT('Ctrl Pts',(161.082758759245,-4.6870764143956,333.503571187647));
#43937=CARTESIAN_POINT('Ctrl Pts',(161.07498508884,-4.72694007679532,333.634740705109));
#43938=CARTESIAN_POINT('Ctrl Pts',(161.067211418436,-4.76122934250337,333.767166592526));
#43939=CARTESIAN_POINT('Ctrl Pts',(161.059799614259,-4.79392243464328,333.893428023024));
#43940=CARTESIAN_POINT('Ctrl Pts',(161.052387810082,-4.82154836619667,334.020831206468));
#43941=CARTESIAN_POINT('Ctrl Pts',(161.044976005905,-4.84405524609774,334.148934881896));
#43942=CARTESIAN_POINT('Ctrl Pts',(161.032948588466,-4.88057801887158,334.356813603857));
#43943=CARTESIAN_POINT('Ctrl Pts',(161.020921171028,-4.90372683021974,334.567106545968));
#43944=CARTESIAN_POINT('Ctrl Pts',(161.00889375359,-4.91325675924559,334.778434930037));
#43945=CARTESIAN_POINT('Ctrl Pts',(161.004774585223,-4.91652058395112,334.850810999055));
#43946=CARTESIAN_POINT('Ctrl Pts',(161.000655416857,-4.91818733857957,334.923308266447));
#43947=CARTESIAN_POINT('Ctrl Pts',(160.99653624849,-4.91824826623568,334.995870330555));
#43948=CARTESIAN_POINT('',(164.496536248442,-4.91824939077852,335.002447980137));
#43949=CARTESIAN_POINT('Ctrl Pts',(164.496536248442,-4.91824939077852,335.002447980137));
#43950=CARTESIAN_POINT('Ctrl Pts',(164.48801435836,-4.91817413949945,335.15363570911));
#43951=CARTESIAN_POINT('Ctrl Pts',(164.479492468279,-4.91112349237319,335.304585905361));
#43952=CARTESIAN_POINT('Ctrl Pts',(164.470970578197,-4.89718756698481,335.454683402237));
#43953=CARTESIAN_POINT('Ctrl Pts',(164.462404819792,-4.88317990332284,335.60555355934));
#43954=CARTESIAN_POINT('Ctrl Pts',(164.453839061386,-4.86221597859101,335.755561974361));
#43955=CARTESIAN_POINT('Ctrl Pts',(164.445273302981,-4.83443761129456,335.904099576928));
#43956=CARTESIAN_POINT('Ctrl Pts',(164.436684914085,-4.80658585433951,336.053029611628));
#43957=CARTESIAN_POINT('Ctrl Pts',(164.428096525189,-4.77188371897625,336.200480825931));
#43958=CARTESIAN_POINT('Ctrl Pts',(164.419508136293,-4.73052300940142,336.345858506688));
#43959=CARTESIAN_POINT('Ctrl Pts',(164.410889304865,-4.68901569203211,336.491751495363));
#43960=CARTESIAN_POINT('Ctrl Pts',(164.402270473436,-4.64080263496645,336.635556003889));
#43961=CARTESIAN_POINT('Ctrl Pts',(164.393651642007,-4.5861250243414,336.776693649341));
#43962=CARTESIAN_POINT('Ctrl Pts',(164.390378567069,-4.56536073413448,336.830291877131));
#43963=CARTESIAN_POINT('Ctrl Pts',(164.38710549213,-4.54366462411572,336.883505748913));
#43964=CARTESIAN_POINT('Ctrl Pts',(164.383832417192,-4.52105162432562,336.936304540273));
#43965=CARTESIAN_POINT('Ctrl Pts',(164.376057338413,-4.46733520838884,337.061726282811));
#43966=CARTESIAN_POINT('Ctrl Pts',(164.368282259635,-4.40831083353155,337.185109243612));
#43967=CARTESIAN_POINT('Ctrl Pts',(164.360507180857,-4.34415446699743,337.305971602029));
#43968=CARTESIAN_POINT('Ctrl Pts',(164.352741669808,-4.2800770489568,337.42668523162));
#43969=CARTESIAN_POINT('Ctrl Pts',(164.344976158758,-4.21088038627454,337.544884088496));
#43970=CARTESIAN_POINT('Ctrl Pts',(164.337210647709,-4.13678871564286,337.660105671704));
#43971=CARTESIAN_POINT('Ctrl Pts',(164.329452836187,-4.06277050711833,337.775213012376));
#43972=CARTESIAN_POINT('Ctrl Pts',(164.321695024665,-3.98386715926199,337.887348627327));
#43973=CARTESIAN_POINT('Ctrl Pts',(164.313937213143,-3.90034891531345,337.99607433174));
#43974=CARTESIAN_POINT('Ctrl Pts',(164.30618523962,-3.81689352149178,338.104718216614));
#43975=CARTESIAN_POINT('Ctrl Pts',(164.298433266097,-3.72883038127933,338.209956989849));
#43976=CARTESIAN_POINT('Ctrl Pts',(164.290681292574,-3.63647295772348,338.311381507807));
#43977=CARTESIAN_POINT('Ctrl Pts',(164.282932602016,-3.54415464759149,338.412763072422));
#43978=CARTESIAN_POINT('Ctrl Pts',(164.275183911459,-3.44754593386803,338.510333306152));
#43979=CARTESIAN_POINT('Ctrl Pts',(164.267435220901,-3.34700031872777,338.603716405176));
#43980=CARTESIAN_POINT('Ctrl Pts',(164.259688142523,-3.24647562294249,338.697080075067));
#43981=CARTESIAN_POINT('Ctrl Pts',(164.251941064145,-3.14201594122153,338.786258077235));
#43982=CARTESIAN_POINT('Ctrl Pts',(164.244193985768,-3.03401107837778,338.870912016409));
#43983=CARTESIAN_POINT('Ctrl Pts',(164.236446842462,-2.92600531034933,338.955566665065));
#43984=CARTESIAN_POINT('Ctrl Pts',(164.228699699156,-2.8144546095731,339.035696933976));
#43985=CARTESIAN_POINT('Ctrl Pts',(164.22095255585,-2.69978092686067,339.111005474268));
#43986=CARTESIAN_POINT('Ctrl Pts',(164.213203670822,-2.5850814630697,339.186330945519));
#43987=CARTESIAN_POINT('Ctrl Pts',(164.205454785794,-2.46725794687209,339.256832316537));
#43988=CARTESIAN_POINT('Ctrl Pts',(164.197705900766,-2.34675994733358,339.322256449135));
#43989=CARTESIAN_POINT('Ctrl Pts',(164.189948790991,-2.22613404997346,339.387750023583));
#43990=CARTESIAN_POINT('Ctrl Pts',(164.182191681216,-2.10282834270516,339.44815540771));
#43991=CARTESIAN_POINT('Ctrl Pts',(164.174434571442,-1.9773160533486,339.50326595791));
#43992=CARTESIAN_POINT('Ctrl Pts',(164.166673316516,-1.85173669423774,339.558405957426));
#43993=CARTESIAN_POINT('Ctrl Pts',(164.158912061589,-1.72394876749512,339.608245343245));
#43994=CARTESIAN_POINT('Ctrl Pts',(164.151150806663,-1.59444302994478,339.652626622324));
#43995=CARTESIAN_POINT('Ctrl Pts',(164.143377136259,-1.46473012542015,339.697078896986));
#43996=CARTESIAN_POINT('Ctrl Pts',(164.135603465854,-1.33329429383625,339.736055506212));
#43997=CARTESIAN_POINT('Ctrl Pts',(164.127829795449,-1.2006397799857,339.769449358282));
#43998=CARTESIAN_POINT('Ctrl Pts',(164.120417991272,-1.07416036566921,339.801288718504));
#43999=CARTESIAN_POINT('Ctrl Pts',(164.113006187095,-0.946573456739391,
339.828053320418));
#44000=CARTESIAN_POINT('Ctrl Pts',(164.105594382918,-0.818320654648899,
339.849694255175));
#44001=CARTESIAN_POINT('Ctrl Pts',(164.09781930414,-0.683781800682978,339.872395876609));
#44002=CARTESIAN_POINT('Ctrl Pts',(164.090044225361,-0.548084960631892,
339.889530620364));
#44003=CARTESIAN_POINT('Ctrl Pts',(164.082269146583,-0.411730533729872,
339.90098572025));
#44004=CARTESIAN_POINT('Ctrl Pts',(164.074503635534,-0.275543899630949,
339.912426723906));
#44005=CARTESIAN_POINT('Ctrl Pts',(164.066738124485,-0.13870167454075,339.918201957715));
#44006=CARTESIAN_POINT('Ctrl Pts',(164.058972613436,-0.00171413271892654,
339.918249701291));
#44007=CARTESIAN_POINT('Ctrl Pts',(164.051214801913,0.135137585556445,339.918297397529));
#44008=CARTESIAN_POINT('Ctrl Pts',(164.043456990391,0.272133945475837,339.912628904578));
#44009=CARTESIAN_POINT('Ctrl Pts',(164.035699178869,0.408760223954992,339.901234348795));
#44010=CARTESIAN_POINT('Ctrl Pts',(164.027947205346,0.545283686826738,339.889848367778));
#44011=CARTESIAN_POINT('Ctrl Pts',(164.020195231823,0.681437234641364,339.872744933225));
#44012=CARTESIAN_POINT('Ctrl Pts',(164.0124432583,0.81670717694351,339.849966231803));
#44013=CARTESIAN_POINT('Ctrl Pts',(164.004694567742,0.951919832344895,339.827197177174));
#44014=CARTESIAN_POINT('Ctrl Pts',(163.996945877185,1.08624924186076,339.798757700798));
#44015=CARTESIAN_POINT('Ctrl Pts',(163.989197186627,1.21918808373027,339.764741701183));
#44016=CARTESIAN_POINT('Ctrl Pts',(163.981450108249,1.3520992665634,339.730732778881));
#44017=CARTESIAN_POINT('Ctrl Pts',(163.973703029872,1.48362007878995,339.691149737978));
#44018=CARTESIAN_POINT('Ctrl Pts',(163.965955951494,1.61325501085684,339.646137248559));
#44019=CARTESIAN_POINT('Ctrl Pts',(163.958208808188,1.74289102938928,339.601124381892));
#44020=CARTESIAN_POINT('Ctrl Pts',(163.950461664882,1.87064076698849,339.550682104161));
#44021=CARTESIAN_POINT('Ctrl Pts',(163.942714521576,1.99602583484769,339.495004330267));
#44022=CARTESIAN_POINT('Ctrl Pts',(163.934965636548,2.12143909193207,339.439314038828));
#44023=CARTESIAN_POINT('Ctrl Pts',(163.92721675152,2.24448626422885,339.378386067629));
#44024=CARTESIAN_POINT('Ctrl Pts',(163.919467866492,2.36471119481717,339.31246148129));
#44025=CARTESIAN_POINT('Ctrl Pts',(163.911710756717,2.48506373338902,339.246466921913));
#44026=CARTESIAN_POINT('Ctrl Pts',(163.903953646942,2.60258770307625,339.17546534147));
#44027=CARTESIAN_POINT('Ctrl Pts',(163.896196537168,2.71685324213598,339.099742860619));
#44028=CARTESIAN_POINT('Ctrl Pts',(163.888435282242,2.83117984104629,339.023979916095));
#44029=CARTESIAN_POINT('Ctrl Pts',(163.880674027315,2.94224422348891,338.943491273711));
#44030=CARTESIAN_POINT('Ctrl Pts',(163.872912772389,3.04964837352559,338.858604392828));
#44031=CARTESIAN_POINT('Ctrl Pts',(163.865139101985,3.15722433519939,338.7735817206));
#44032=CARTESIAN_POINT('Ctrl Pts',(163.85736543158,3.26112806768403,338.684147005491));
#44033=CARTESIAN_POINT('Ctrl Pts',(163.849591761175,3.36099663947487,338.590666324227));
#44034=CARTESIAN_POINT('Ctrl Pts',(163.842179956998,3.45621630522143,338.501537191167));
#44035=CARTESIAN_POINT('Ctrl Pts',(163.834768152821,3.54776782732529,338.40873049935));
#44036=CARTESIAN_POINT('Ctrl Pts',(163.827356348644,3.63537110140622,338.312591133472));
#44037=CARTESIAN_POINT('Ctrl Pts',(163.819581269866,3.72726807290682,338.211739690889));
#44038=CARTESIAN_POINT('Ctrl Pts',(163.811806191087,3.81511039091875,338.106901916162));
#44039=CARTESIAN_POINT('Ctrl Pts',(163.804031112309,3.89853243320858,337.998437581428));
#44040=CARTESIAN_POINT('Ctrl Pts',(163.79626560126,3.98185181936449,337.890106718963));
#44041=CARTESIAN_POINT('Ctrl Pts',(163.788500090211,4.06076151668513,337.778158482881));
#44042=CARTESIAN_POINT('Ctrl Pts',(163.780734579162,4.13493348449984,337.66298857325));
#44043=CARTESIAN_POINT('Ctrl Pts',(163.77297676764,4.20903191059251,337.547932854921));
#44044=CARTESIAN_POINT('Ctrl Pts',(163.765218956117,4.27840174513961,337.429662146381));
#44045=CARTESIAN_POINT('Ctrl Pts',(163.757461144595,4.34275613898933,337.308603946061));
#44046=CARTESIAN_POINT('Ctrl Pts',(163.749709171072,4.40706210411684,337.187636845876));
#44047=CARTESIAN_POINT('Ctrl Pts',(163.741957197549,4.46635995832735,337.063886772979));
#44048=CARTESIAN_POINT('Ctrl Pts',(163.734205224026,4.52040718990632,336.937808530259));
#44049=CARTESIAN_POINT('Ctrl Pts',(163.726456533469,4.57443153245066,336.811783681749));
#44050=CARTESIAN_POINT('Ctrl Pts',(163.718707842911,4.62320952134495,336.68343298297));
#44051=CARTESIAN_POINT('Ctrl Pts',(163.710959152353,4.66654557693405,336.553233865488));
#44052=CARTESIAN_POINT('Ctrl Pts',(163.703212073975,4.70987261609483,336.423061837018));
#44053=CARTESIAN_POINT('Ctrl Pts',(163.695464995598,4.74775985069061,336.291042525437));
#44054=CARTESIAN_POINT('Ctrl Pts',(163.68771791722,4.78006078823127,336.157670904581));
#44055=CARTESIAN_POINT('Ctrl Pts',(163.679970773914,4.81236199648488,336.024298165943));
#44056=CARTESIAN_POINT('Ctrl Pts',(163.672223630608,4.83907672229522,335.889573475317));
#44057=CARTESIAN_POINT('Ctrl Pts',(163.664476487302,4.86010914920729,335.754004058538));
#44058=CARTESIAN_POINT('Ctrl Pts',(163.656727602274,4.88114630465544,335.618404162875));
#44059=CARTESIAN_POINT('Ctrl Pts',(163.648978717246,4.89649855920798,335.481959549333));
#44060=CARTESIAN_POINT('Ctrl Pts',(163.641229832218,4.90612177656237,335.345184263895));
#44061=CARTESIAN_POINT('Ctrl Pts',(163.633472722443,4.91575520809909,335.208263803755));
#44062=CARTESIAN_POINT('Ctrl Pts',(163.625715612669,4.91964742787418,335.071012361134));
#44063=CARTESIAN_POINT('Ctrl Pts',(163.617958502894,4.91780641799855,334.933946252247));
#44064=CARTESIAN_POINT('Ctrl Pts',(163.610197247968,4.91596442434611,334.796806899614));
#44065=CARTESIAN_POINT('Ctrl Pts',(163.602435993042,4.90838311802871,334.659853468132));
#44066=CARTESIAN_POINT('Ctrl Pts',(163.594674738115,4.89512247734571,334.523597864945));
#44067=CARTESIAN_POINT('Ctrl Pts',(163.586901067711,4.88184062395925,334.387124297199));
#44068=CARTESIAN_POINT('Ctrl Pts',(163.579127397306,4.86286133566008,334.251351175755));
#44069=CARTESIAN_POINT('Ctrl Pts',(163.571353726902,4.8382960511165,334.116781802582));
#44070=CARTESIAN_POINT('Ctrl Pts',(163.563941922724,4.81487428647819,333.988476666104));
#44071=CARTESIAN_POINT('Ctrl Pts',(163.556530118547,4.7863749412202,333.861266011809));
#44072=CARTESIAN_POINT('Ctrl Pts',(163.54911831437,4.75293645569013,333.735572022347));
#44073=CARTESIAN_POINT('Ctrl Pts',(163.541343235592,4.71785905037651,333.603717396039));
#44074=CARTESIAN_POINT('Ctrl Pts',(163.533568156813,4.67723524766031,333.473115181295));
#44075=CARTESIAN_POINT('Ctrl Pts',(163.525793078035,4.63116972843598,333.344267530995));
#44076=CARTESIAN_POINT('Ctrl Pts',(163.518027566986,4.58516089576573,333.215578435931));
#44077=CARTESIAN_POINT('Ctrl Pts',(163.510262055937,4.53372380079088,333.088639973857));
#44078=CARTESIAN_POINT('Ctrl Pts',(163.502496544888,4.47701367451134,332.963942137183));
#44079=CARTESIAN_POINT('Ctrl Pts',(163.494738733365,4.42035977648714,332.839367938777));
#44080=CARTESIAN_POINT('Ctrl Pts',(163.486980921843,4.35844341239523,332.717030298203));
#44081=CARTESIAN_POINT('Ctrl Pts',(163.479223110321,4.291468844249,332.597401776963));
#44082=CARTESIAN_POINT('Ctrl Pts',(163.471471136798,4.22454467658916,332.477863279979));
#44083=CARTESIAN_POINT('Ctrl Pts',(163.463719163275,4.15257007162135,332.361030184086));
#44084=CARTESIAN_POINT('Ctrl Pts',(163.455967189752,4.07579624579284,332.2473525425));
#44085=CARTESIAN_POINT('Ctrl Pts',(163.448218499194,3.99905493372514,332.133723043462));
#44086=CARTESIAN_POINT('Ctrl Pts',(163.440469808637,3.91751866155143,332.023246664098));
#44087=CARTESIAN_POINT('Ctrl Pts',(163.432721118079,3.83148307228506,331.916346237125));
#44088=CARTESIAN_POINT('Ctrl Pts',(163.424974039701,3.74546538344163,331.809468051679));
#44089=CARTESIAN_POINT('Ctrl Pts',(163.417226961323,3.65495048443267,331.706164643055));
#44090=CARTESIAN_POINT('Ctrl Pts',(163.409479882946,3.56027533382699,331.60682705866));
#44091=CARTESIAN_POINT('Ctrl Pts',(163.40173273964,3.4655993897524,331.50748864172));
#44092=CARTESIAN_POINT('Ctrl Pts',(163.393985596334,3.36676339420635,331.412116398254));
#44093=CARTESIAN_POINT('Ctrl Pts',(163.386238453028,3.26414203243208,331.321065391365));
#44094=CARTESIAN_POINT('Ctrl Pts',(163.378489568,3.16149759919699,331.229993914278));
#44095=CARTESIAN_POINT('Ctrl Pts',(163.370740682972,3.05506639860117,331.14324586632));
#44096=CARTESIAN_POINT('Ctrl Pts',(163.362991797944,2.94525681819376,331.06113654243));
#44097=CARTESIAN_POINT('Ctrl Pts',(163.355234688169,2.83533068476313,330.978940066854));
#44098=CARTESIAN_POINT('Ctrl Pts',(163.347477578394,2.72201932198736,330.90139238512));
#44099=CARTESIAN_POINT('Ctrl Pts',(163.33972046862,2.60576123076575,330.82876619323));
#44100=CARTESIAN_POINT('Ctrl Pts',(163.331959213693,2.48944101493743,330.756101192226));
#44101=CARTESIAN_POINT('Ctrl Pts',(163.324197958767,2.37017127276737,330.688363114287));
#44102=CARTESIAN_POINT('Ctrl Pts',(163.316436703841,2.24841493559251,330.625778544712));
#44103=CARTESIAN_POINT('Ctrl Pts',(163.308663033436,2.12646382795849,330.563093860221));
#44104=CARTESIAN_POINT('Ctrl Pts',(163.300889363032,2.00201853161359,330.505579321984));
#44105=CARTESIAN_POINT('Ctrl Pts',(163.293115692627,1.87556258977798,330.453413584421));
#44106=CARTESIAN_POINT('Ctrl Pts',(163.28570388845,1.75499320245967,330.403676174493));
#44107=CARTESIAN_POINT('Ctrl Pts',(163.278292084273,1.63259641833461,330.358800897544));
#44108=CARTESIAN_POINT('Ctrl Pts',(163.270880280096,1.50880217781459,330.318899803388));
#44109=CARTESIAN_POINT('Ctrl Pts',(163.263105201318,1.37894041280134,330.277043037748));
#44110=CARTESIAN_POINT('Ctrl Pts',(163.255330122539,1.24713035350329,330.240528107771));
#44111=CARTESIAN_POINT('Ctrl Pts',(163.247555043761,1.11385091983099,330.209538728797));
#44112=CARTESIAN_POINT('Ctrl Pts',(163.239789532712,0.98073549498679,330.178587484228));
#44113=CARTESIAN_POINT('Ctrl Pts',(163.232024021663,0.84615467056458,330.153148349199));
#44114=CARTESIAN_POINT('Ctrl Pts',(163.224258510614,0.710604496037439,330.13335594966));
#44115=CARTESIAN_POINT('Ctrl Pts',(163.216500699092,0.575188719903009,330.113583174343));
#44116=CARTESIAN_POINT('Ctrl Pts',(163.208742887569,0.438805890615215,330.099446048789));
#44117=CARTESIAN_POINT('Ctrl Pts',(163.200985076047,0.301963933117836,330.091028534856));
#44118=CARTESIAN_POINT('Ctrl Pts',(163.193233102524,0.165224953533006,330.08261735537));
#44119=CARTESIAN_POINT('Ctrl Pts',(163.185481129001,0.0280279220224473,
330.079917244129));
#44120=CARTESIAN_POINT('Ctrl Pts',(163.177729155478,-0.109112754430488,
330.082960497482));
#44121=CARTESIAN_POINT('Ctrl Pts',(163.169980464921,-0.246195351725502,
330.086002462015));
#44122=CARTESIAN_POINT('Ctrl Pts',(163.162231774363,-0.383221251466671,
330.094782944779));
#44123=CARTESIAN_POINT('Ctrl Pts',(163.154483083805,-0.519674895201839,
330.109282152301));
#44124=CARTESIAN_POINT('Ctrl Pts',(163.146736005428,-0.656100148616698,
330.123778343143));
#44125=CARTESIAN_POINT('Ctrl Pts',(163.13898892705,-0.791952994407409,330.143990850815));
#44126=CARTESIAN_POINT('Ctrl Pts',(163.131241848672,-0.926722244851329,
330.16984793786));
#44127=CARTESIAN_POINT('Ctrl Pts',(163.123494705366,-1.06149262479126,330.195705241611));
#44128=CARTESIAN_POINT('Ctrl Pts',(163.11574756206,-1.19517900739775,330.227207145442));
#44129=CARTESIAN_POINT('Ctrl Pts',(163.108000418755,-1.32728004884665,330.264230713555));
#44130=CARTESIAN_POINT('Ctrl Pts',(163.100251533726,-1.45941078941435,330.301262605353));
#44131=CARTESIAN_POINT('Ctrl Pts',(163.092502648698,-1.58995510329353,330.343818526192));
#44132=CARTESIAN_POINT('Ctrl Pts',(163.08475376367,-1.71842685030941,330.391725678452));
#44133=CARTESIAN_POINT('Ctrl Pts',(163.076996653896,-1.84703495856495,330.439683679859));
#44134=CARTESIAN_POINT('Ctrl Pts',(163.069239544121,-1.97356573874499,330.493004121937));
#44135=CARTESIAN_POINT('Ctrl Pts',(163.061482434346,-2.09755257696487,330.551465831381));
#44136=CARTESIAN_POINT('Ctrl Pts',(163.05372117942,-2.22160566978676,330.609958780894));
#44137=CARTESIAN_POINT('Ctrl Pts',(163.045959924494,-2.34311176583828,330.67359829081));
#44138=CARTESIAN_POINT('Ctrl Pts',(163.038198669568,-2.46162980599996,330.742117690599));
#44139=CARTESIAN_POINT('Ctrl Pts',(163.030424999163,-2.58033743640092,330.810746699097));
#44140=CARTESIAN_POINT('Ctrl Pts',(163.022651328758,-2.69604712914511,330.884270986893));
#44141=CARTESIAN_POINT('Ctrl Pts',(163.014877658354,-2.80834697693655,330.962380612337));
#44142=CARTESIAN_POINT('Ctrl Pts',(163.007465854177,-2.91541923979571,331.036854215925));
#44143=CARTESIAN_POINT('Ctrl Pts',(163.000054049999,-3.01939174057162,331.115495695617));
#44144=CARTESIAN_POINT('Ctrl Pts',(162.992642245822,-3.11993758875825,331.198004141934));
#44145=CARTESIAN_POINT('Ctrl Pts',(162.984971950382,-3.22399003570806,331.283390121446));
#44146=CARTESIAN_POINT('Ctrl Pts',(162.977301654941,-3.32472052302233,331.373203600424));
#44147=CARTESIAN_POINT('Ctrl Pts',(162.9696313595,-3.42172113219513,331.467153052284));
#44148=CARTESIAN_POINT('Ctrl Pts',(162.961970553342,-3.51860173735074,331.560986274856));
#44149=CARTESIAN_POINT('Ctrl Pts',(162.954309747185,-3.61176135496804,331.658945017541));
#44150=CARTESIAN_POINT('Ctrl Pts',(162.946648941027,-3.70082357338688,331.760696380213));
#44151=CARTESIAN_POINT('Ctrl Pts',(162.938995661286,-3.78979829196516,331.862347776501));
#44152=CARTESIAN_POINT('Ctrl Pts',(162.931342381545,-3.87468335526745,331.967784080454));
#44153=CARTESIAN_POINT('Ctrl Pts',(162.923689101803,-3.95513818248469,332.076634641385));
#44154=CARTESIAN_POINT('Ctrl Pts',(162.9160414755,-4.03553357814199,332.185404794976));
#44155=CARTESIAN_POINT('Ctrl Pts',(162.908393849196,-4.11150501114932,332.297583864859));
#44156=CARTESIAN_POINT('Ctrl Pts',(162.900746222892,-4.18275163918189,332.412767542832));
#44157=CARTESIAN_POINT('Ctrl Pts',(162.89310159564,-4.25397032752569,332.527906051004));
#44158=CARTESIAN_POINT('Ctrl Pts',(162.885456968388,-4.32046768349657,332.646046483016));
#44159=CARTESIAN_POINT('Ctrl Pts',(162.877812341136,-4.38198595454,332.766755240303));
#44160=CARTESIAN_POINT('Ctrl Pts',(162.870168952057,-4.44349426168674,332.887444446819));
#44161=CARTESIAN_POINT('Ctrl Pts',(162.862525562978,-4.50002490540647,333.010700792823));
#44162=CARTESIAN_POINT('Ctrl Pts',(162.854882173899,-4.55136617113473,333.136066246148));
#44163=CARTESIAN_POINT('Ctrl Pts',(162.847238263366,-4.60271093950638,333.261440252251));
#44164=CARTESIAN_POINT('Ctrl Pts',(162.839594352834,-4.64886547449734,333.388923279055));
#44165=CARTESIAN_POINT('Ctrl Pts',(162.831950442302,-4.68966648554024,333.518038017728));
#44166=CARTESIAN_POINT('Ctrl Pts',(162.824300353631,-4.73050047372324,333.647257112511));
#44167=CARTESIAN_POINT('Ctrl Pts',(162.81665026496,-4.76597217494867,333.7781101689));
#44168=CARTESIAN_POINT('Ctrl Pts',(162.809000176289,-4.79596835592378,333.910105238347));
#44169=CARTESIAN_POINT('Ctrl Pts',(162.801346840274,-4.82597726981325,334.042156337658));
#44170=CARTESIAN_POINT('Ctrl Pts',(162.793693504259,-4.85050596118483,334.175350020076));
#44171=CARTESIAN_POINT('Ctrl Pts',(162.786040168244,-4.86949271350167,334.309186149781));
#44172=CARTESIAN_POINT('Ctrl Pts',(162.778376692472,-4.88850462099753,334.443199596372));
#44173=CARTESIAN_POINT('Ctrl Pts',(162.770713216701,-4.90195988485668,334.577856790165));
#44174=CARTESIAN_POINT('Ctrl Pts',(162.76304974093,-4.90984881383883,334.712654062591));
#44175=CARTESIAN_POINT('Ctrl Pts',(162.757545243462,-4.91551524913529,334.809475826872));
#44176=CARTESIAN_POINT('Ctrl Pts',(162.752040745995,-4.91831098889184,334.906369812791));
#44177=CARTESIAN_POINT('Ctrl Pts',(162.746536248527,-4.91824899084518,335.003150642852));
#44178=CARTESIAN_POINT('',(166.246536248533,-4.9182482206735,334.995816419961));
#44179=CARTESIAN_POINT('Ctrl Pts',(166.24653624849,-4.91824822067415,334.995816420722));
#44180=CARTESIAN_POINT('Ctrl Pts',(166.238483097421,-4.9183694473876,335.138331484532));
#44181=CARTESIAN_POINT('Ctrl Pts',(166.230429946352,-4.91229114364639,335.280950775894));
#44182=CARTESIAN_POINT('Ctrl Pts',(166.222376795283,-4.90001804275799,335.423091294103));
#44183=CARTESIAN_POINT('Ctrl Pts',(166.214669495024,-4.88827202274059,335.559127442372));
#44184=CARTESIAN_POINT('Ctrl Pts',(166.206962194764,-4.87085227486632,335.694724653029));
#44185=CARTESIAN_POINT('Ctrl Pts',(166.199254894505,-4.84781615683562,335.829374205063));
#44186=CARTESIAN_POINT('Ctrl Pts',(166.191548140149,-4.82478167043767,335.964014219959));
#44187=CARTESIAN_POINT('Ctrl Pts',(166.183841385792,-4.79613167145662,336.097706320243));
#44188=CARTESIAN_POINT('Ctrl Pts',(166.176134631436,-4.76197497548818,336.229950159691));
#44189=CARTESIAN_POINT('Ctrl Pts',(166.168426712617,-4.72781311856482,336.362213980711));
#44190=CARTESIAN_POINT('Ctrl Pts',(166.160718793797,-4.68814300815376,336.493028722961));
#44191=CARTESIAN_POINT('Ctrl Pts',(166.153010874978,-4.64312372530918,336.621907868521));
#44192=CARTESIAN_POINT('Ctrl Pts',(166.145300080857,-4.5980876488272,336.750835090139));
#44193=CARTESIAN_POINT('Ctrl Pts',(166.137589286737,-4.5476985602563,336.877824905842));
#44194=CARTESIAN_POINT('Ctrl Pts',(166.129878492616,-4.49216402145174,337.002409914796));
#44195=CARTESIAN_POINT('Ctrl Pts',(166.12215883249,-4.43656562806739,337.127138173764));
#44196=CARTESIAN_POINT('Ctrl Pts',(166.114439172364,-4.37581013511344,337.249455745313));
#44197=CARTESIAN_POINT('Ctrl Pts',(166.106719512238,-4.31015166500581,337.368918674659));
#44198=CARTESIAN_POINT('Ctrl Pts',(166.09899463244,-4.24444879971705,337.48846237924));
#44199=CARTESIAN_POINT('Ctrl Pts',(166.091269752641,-4.17383655953049,337.605147261037));
#44200=CARTESIAN_POINT('Ctrl Pts',(166.083544872843,-4.098612262968,337.718558548266));
#44201=CARTESIAN_POINT('Ctrl Pts',(166.075808780588,-4.02327878034587,337.832134448952));
#44202=CARTESIAN_POINT('Ctrl Pts',(166.068072688332,-3.94332011063052,337.942426952751));
#44203=CARTESIAN_POINT('Ctrl Pts',(166.060336596077,-3.85907388987416,338.049054242711));
#44204=CARTESIAN_POINT('Ctrl Pts',(166.05797793833,-3.83338805331583,338.081563845135));
#44205=CARTESIAN_POINT('Ctrl Pts',(166.055619280582,-3.80730391285455,338.113732997247));
#44206=CARTESIAN_POINT('Ctrl Pts',(166.053260622835,-3.78083169644808,338.145551580508));
#44207=CARTESIAN_POINT('Ctrl Pts',(166.045485544057,-3.69356868924297,338.250438350005));
#44208=CARTESIAN_POINT('Ctrl Pts',(166.037710465278,-3.60179987368437,338.351856870673));
#44209=CARTESIAN_POINT('Ctrl Pts',(166.0299353865,-3.50583135248403,338.449395539865));
#44210=CARTESIAN_POINT('Ctrl Pts',(166.022169875451,-3.40998092665856,338.546814181515));
#44211=CARTESIAN_POINT('Ctrl Pts',(166.014404364402,-3.30994134955729,338.640362195426));
#44212=CARTESIAN_POINT('Ctrl Pts',(166.006638853353,-3.206059476404,338.729660265528));
#44213=CARTESIAN_POINT('Ctrl Pts',(165.998881041831,-3.10228060243011,338.818869796335));
#44214=CARTESIAN_POINT('Ctrl Pts',(165.991123230308,-2.99466730832114,338.903837515938));
#44215=CARTESIAN_POINT('Ctrl Pts',(165.983365418786,-2.88360360762239,338.984220538149));
#44216=CARTESIAN_POINT('Ctrl Pts',(165.975613445263,-2.77262348588069,339.064543069586));
#44217=CARTESIAN_POINT('Ctrl Pts',(165.96786147174,-2.65819844120394,339.140287542697));
#44218=CARTESIAN_POINT('Ctrl Pts',(165.960109498217,-2.54074562661766,339.211151234915));
#44219=CARTESIAN_POINT('Ctrl Pts',(165.952360807659,-2.42334255336819,339.281984916317));
#44220=CARTESIAN_POINT('Ctrl Pts',(165.944612117102,-2.30291459452029,339.347941726467));
#44221=CARTESIAN_POINT('Ctrl Pts',(165.936863426544,-2.17990776780511,339.408762319105));
#44222=CARTESIAN_POINT('Ctrl Pts',(165.929116348166,-2.05692653368781,339.469570257511));
#44223=CARTESIAN_POINT('Ctrl Pts',(165.921369269788,-1.93136784911224,339.525243930854));
#44224=CARTESIAN_POINT('Ctrl Pts',(165.913622191411,-1.80370185461097,339.575570202955));
#44225=CARTESIAN_POINT('Ctrl Pts',(165.905875048105,-1.67603479014578,339.625896896839));
#44226=CARTESIAN_POINT('Ctrl Pts',(165.898127904799,-1.5462607441682,339.670875956744));
#44227=CARTESIAN_POINT('Ctrl Pts',(165.890380761493,-1.41486895833322,339.710342757512));
#44228=CARTESIAN_POINT('Ctrl Pts',(165.882631876465,-1.28344763283514,339.749818431254));
#44229=CARTESIAN_POINT('Ctrl Pts',(165.874882991437,-1.15040821803063,339.783779267421));
#44230=CARTESIAN_POINT('Ctrl Pts',(165.867134106409,-1.01625381442326,339.812110893067));
#44231=CARTESIAN_POINT('Ctrl Pts',(165.859376996634,-0.881957017945779,
339.840472590192));
#44232=CARTESIAN_POINT('Ctrl Pts',(165.851619886859,-0.746543251634799,
339.863193060476));
#44233=CARTESIAN_POINT('Ctrl Pts',(165.843862777085,-0.610525028347018,
339.880209242672));
#44234=CARTESIAN_POINT('Ctrl Pts',(165.836101522159,-0.474434121269662,
339.897234517772));
#44235=CARTESIAN_POINT('Ctrl Pts',(165.828340267232,-0.337738502948436,
339.908549398765));
#44236=CARTESIAN_POINT('Ctrl Pts',(165.820579012306,-0.200953465884062,
339.914142933111));
#44237=CARTESIAN_POINT('Ctrl Pts',(165.812805341902,-0.0639496173386181,
339.91974541529));
#44238=CARTESIAN_POINT('Ctrl Pts',(165.805031671497,0.0731435447082648,
339.919608262227));
#44239=CARTESIAN_POINT('Ctrl Pts',(165.797258001092,0.20981217803582,339.913772676106));
#44240=CARTESIAN_POINT('Ctrl Pts',(165.789846196915,0.340118853600547,339.908208737924));
#44241=CARTESIAN_POINT('Ctrl Pts',(165.782434392738,0.470039347797948,339.897464975405));
#44242=CARTESIAN_POINT('Ctrl Pts',(165.775022588561,0.599136456423764,339.881620485974));
#44243=CARTESIAN_POINT('Ctrl Pts',(165.767247509783,0.734560998904761,339.864999410918));
#44244=CARTESIAN_POINT('Ctrl Pts',(165.759472431004,0.869507368395578,339.842712437039));
#44245=CARTESIAN_POINT('Ctrl Pts',(165.751697352226,1.0034637897097,339.814794230831));
#44246=CARTESIAN_POINT('Ctrl Pts',(165.743931841177,1.13725536911931,339.786910379752));
#44247=CARTESIAN_POINT('Ctrl Pts',(165.736166330128,1.27005904521528,339.753409163228));
#44248=CARTESIAN_POINT('Ctrl Pts',(165.728400819079,1.4013681397591,339.714376989526));
#44249=CARTESIAN_POINT('Ctrl Pts',(165.720643007557,1.53254704095354,339.675383516337));
#44250=CARTESIAN_POINT('Ctrl Pts',(165.712885196034,1.66223393736663,339.630870110016));
#44251=CARTESIAN_POINT('Ctrl Pts',(165.705127384512,1.78993267692197,339.580974140353));
#44252=CARTESIAN_POINT('Ctrl Pts',(165.697375410989,1.91753531912598,339.53111571899));
#44253=CARTESIAN_POINT('Ctrl Pts',(165.689623437466,2.04315241988421,339.475882938388));
#44254=CARTESIAN_POINT('Ctrl Pts',(165.681871463943,2.16630366789437,339.415462770873));
#44255=CARTESIAN_POINT('Ctrl Pts',(165.674122773386,2.28940276127794,339.355068191335));
#44256=CARTESIAN_POINT('Ctrl Pts',(165.666374082828,2.41003772874752,339.289490766096));
#44257=CARTESIAN_POINT('Ctrl Pts',(165.65862539227,2.52774911471334,339.218965213837));
#44258=CARTESIAN_POINT('Ctrl Pts',(165.650878313893,2.645436009842,339.148454335008));
#44259=CARTESIAN_POINT('Ctrl Pts',(165.643131235515,2.76020019828136,339.072997577672));
#44260=CARTESIAN_POINT('Ctrl Pts',(165.635384157137,2.87160802925319,338.992874952816));
#44261=CARTESIAN_POINT('Ctrl Pts',(165.627637013831,2.98301679393007,338.912751656456));
#44262=CARTESIAN_POINT('Ctrl Pts',(165.619889870525,3.09106882770222,338.827962642798));
#44263=CARTESIAN_POINT('Ctrl Pts',(165.61214272722,3.19536093702955,338.738830237468));
#44264=CARTESIAN_POINT('Ctrl Pts',(165.604393842192,3.29967649343707,338.649677793282));
#44265=CARTESIAN_POINT('Ctrl Pts',(165.596644957164,3.40023014624294,338.556180268223));
#44266=CARTESIAN_POINT('Ctrl Pts',(165.588896072135,3.49665346024702,338.458698836476));
#44267=CARTESIAN_POINT('Ctrl Pts',(165.581138962361,3.59317911895288,338.361113936931));
#44268=CARTESIAN_POINT('Ctrl Pts',(165.573381852586,3.68556540612536,338.259536962084));
#44269=CARTESIAN_POINT('Ctrl Pts',(165.565624742811,3.77348194210339,338.154364768875));
#44270=CARTESIAN_POINT('Ctrl Pts',(165.557863487885,3.86144545786724,338.049136375008));
#44271=CARTESIAN_POINT('Ctrl Pts',(165.550102232959,3.94493422535332,337.940309244642));
#44272=CARTESIAN_POINT('Ctrl Pts',(165.542340978033,4.02366017999723,337.828310771186));
#44273=CARTESIAN_POINT('Ctrl Pts',(165.534567307628,4.10251207051185,337.716133136672));
#44274=CARTESIAN_POINT('Ctrl Pts',(165.526793637224,4.17658571196255,337.60077435056));
#44275=CARTESIAN_POINT('Ctrl Pts',(165.519019966819,4.2456376826352,337.482688810602));
#44276=CARTESIAN_POINT('Ctrl Pts',(165.511608162642,4.31147526745983,337.370100180939));
#44277=CARTESIAN_POINT('Ctrl Pts',(165.504196358465,4.37274804259686,337.25503319926));
#44278=CARTESIAN_POINT('Ctrl Pts',(165.496784554288,4.429285926475,337.137898324063));
#44279=CARTESIAN_POINT('Ctrl Pts',(165.489009475509,4.48859490045991,337.015022319705));
#44280=CARTESIAN_POINT('Ctrl Pts',(165.481234396731,4.54288053240625,336.889482278253));
#44281=CARTESIAN_POINT('Ctrl Pts',(165.473459317953,4.59189502318759,336.76172732241));
#44282=CARTESIAN_POINT('Ctrl Pts',(165.465693806904,4.64084919851758,336.634129577173));
#44283=CARTESIAN_POINT('Ctrl Pts',(165.457928295855,4.68454500023399,336.504322702141));
#44284=CARTESIAN_POINT('Ctrl Pts',(165.450162784806,4.72278089822452,336.372779534326));
#44285=CARTESIAN_POINT('Ctrl Pts',(165.442404973283,4.76097888521093,336.241366791946));
#44286=CARTESIAN_POINT('Ctrl Pts',(165.434647161761,4.79372763326548,336.108221555664));
#44287=CARTESIAN_POINT('Ctrl Pts',(165.426889350239,4.82087416321797,335.973835389025));
#44288=CARTESIAN_POINT('Ctrl Pts',(165.419137376716,4.84800026454584,335.839550352237));
#44289=CARTESIAN_POINT('Ctrl Pts',(165.411385403193,4.86953246212534,335.704026625446));
#44290=CARTESIAN_POINT('Ctrl Pts',(165.40363342967,4.88536806097013,335.567769294127));
#44291=CARTESIAN_POINT('Ctrl Pts',(165.395884739112,4.90119695342938,335.431569667868));
#44292=CARTESIAN_POINT('Ctrl Pts',(165.388136048555,4.91133400044307,335.29463744246));
#44293=CARTESIAN_POINT('Ctrl Pts',(165.380387357997,4.91572794417595,335.157486003656));
#44294=CARTESIAN_POINT('Ctrl Pts',(165.372640279619,4.92012097371215,335.020363100355));
#44295=CARTESIAN_POINT('Ctrl Pts',(165.364893201241,4.91877326420113,334.883021464807));
#44296=CARTESIAN_POINT('Ctrl Pts',(165.357146122864,4.91168560953754,334.745977293216));
#44297=CARTESIAN_POINT('Ctrl Pts',(165.349398979558,4.90459789547258,334.608931973063));
#44298=CARTESIAN_POINT('Ctrl Pts',(165.341651836252,4.89177016049177,334.472184512192));
#44299=CARTESIAN_POINT('Ctrl Pts',(165.333904692946,4.87325526393051,334.336248393543));
#44300=CARTESIAN_POINT('Ctrl Pts',(165.326155807918,4.85473620482745,334.20028171357));
#44301=CARTESIAN_POINT('Ctrl Pts',(165.31840692289,4.83052749262428,334.065127126011));
#44302=CARTESIAN_POINT('Ctrl Pts',(165.310658037862,4.80073346496936,333.931289907962));
#44303=CARTESIAN_POINT('Ctrl Pts',(165.302900928087,4.77090781362567,333.797310633707));
#44304=CARTESIAN_POINT('Ctrl Pts',(165.295143818312,4.73548508954091,333.664651904274));
#44305=CARTESIAN_POINT('Ctrl Pts',(165.287386708538,4.69462023078815,333.533806305028));
#44306=CARTESIAN_POINT('Ctrl Pts',(165.279625453611,4.65373353516151,333.402890786078));
#44307=CARTESIAN_POINT('Ctrl Pts',(165.271864198685,4.60739904218282,333.273790695604));
#44308=CARTESIAN_POINT('Ctrl Pts',(165.264102943759,4.5558202678229,333.146979560341));
#44309=CARTESIAN_POINT('Ctrl Pts',(165.256329273354,4.50415898423348,333.019965568589));
#44310=CARTESIAN_POINT('Ctrl Pts',(165.24855560295,4.44723681765391,332.895248204751));
#44311=CARTESIAN_POINT('Ctrl Pts',(165.240781932545,4.38530415139085,332.773278068035));
#44312=CARTESIAN_POINT('Ctrl Pts',(165.233370128368,4.32625446564266,332.656985670528));
#44313=CARTESIAN_POINT('Ctrl Pts',(165.225958324191,4.26265040036041,332.543190740389));
#44314=CARTESIAN_POINT('Ctrl Pts',(165.218546520014,4.19474507795339,332.432258425486));
#44315=CARTESIAN_POINT('Ctrl Pts',(165.210771441235,4.12351151341542,332.315888987379));
#44316=CARTESIAN_POINT('Ctrl Pts',(165.202996362457,4.04731928463488,332.202302121427));
#44317=CARTESIAN_POINT('Ctrl Pts',(165.195221283678,3.96641197014625,332.091949253266));
#44318=CARTESIAN_POINT('Ctrl Pts',(165.187455772629,3.88560421725891,331.981732181335));
#44319=CARTESIAN_POINT('Ctrl Pts',(165.17969026158,3.80009315230977,331.874741501066));
#44320=CARTESIAN_POINT('Ctrl Pts',(165.171924750531,3.7101673345222,331.771402562668));
#44321=CARTESIAN_POINT('Ctrl Pts',(165.164166939009,3.62033067844447,331.668166085129));
#44322=CARTESIAN_POINT('Ctrl Pts',(165.156409127487,3.52608823542148,331.568574437002));
#44323=CARTESIAN_POINT('Ctrl Pts',(165.148651315965,3.42777058591576,331.473022274974));
#44324=CARTESIAN_POINT('Ctrl Pts',(165.140899342442,3.32952692355933,331.377542018978));
#44325=CARTESIAN_POINT('Ctrl Pts',(165.133147368919,3.22721443805593,331.286095469747));
#44326=CARTESIAN_POINT('Ctrl Pts',(165.125395395396,3.12120229240839,331.19904231642));
#44327=CARTESIAN_POINT('Ctrl Pts',(165.117646704838,3.01523504296749,331.112026030155));
#44328=CARTESIAN_POINT('Ctrl Pts',(165.10989801428,2.90557155110333,331.029399686719));
#44329=CARTESIAN_POINT('Ctrl Pts',(165.102149323723,2.79261579529406,330.951484212409));
#44330=CARTESIAN_POINT('Ctrl Pts',(165.094402245345,2.6796835408733,330.873584949064));
#44331=CARTESIAN_POINT('Ctrl Pts',(165.086655166967,2.56346070653789,330.800394827088));
#44332=CARTESIAN_POINT('Ctrl Pts',(165.078908088589,2.44438180230996,330.732192522262));
#44333=CARTESIAN_POINT('Ctrl Pts',(165.071160945283,2.32530190008611,330.663989645835));
#44334=CARTESIAN_POINT('Ctrl Pts',(165.063413801977,2.20336621940721,330.600774864204));
#44335=CARTESIAN_POINT('Ctrl Pts',(165.055666658672,2.07903516425226,330.542781601907));
#44336=CARTESIAN_POINT('Ctrl Pts',(165.047917773643,1.95467615683688,330.484775301493));
#44337=CARTESIAN_POINT('Ctrl Pts',(165.040168888615,1.82792105749378,330.431993021559));
#44338=CARTESIAN_POINT('Ctrl Pts',(165.032420003587,1.69925122759994,330.384620456777));
#44339=CARTESIAN_POINT('Ctrl Pts',(165.024662893813,1.57044482621895,330.337197610266));
#44340=CARTESIAN_POINT('Ctrl Pts',(165.016905784038,1.43972000193101,330.295196084207));
#44341=CARTESIAN_POINT('Ctrl Pts',(165.009148674263,1.30757482616058,330.258752154075));
#44342=CARTESIAN_POINT('Ctrl Pts',(165.001387419337,1.17535903623344,330.222288749472));
#44343=CARTESIAN_POINT('Ctrl Pts',(164.993626164411,1.04172176310057,330.191388946403));
#44344=CARTESIAN_POINT('Ctrl Pts',(164.985864909485,0.907171339665501,330.166137856435));
#44345=CARTESIAN_POINT('Ctrl Pts',(164.97809123908,0.772405679402744,330.140846372952));
#44346=CARTESIAN_POINT('Ctrl Pts',(164.970317568675,0.636724336893146,330.121221715357));
#44347=CARTESIAN_POINT('Ctrl Pts',(164.962543898271,0.500641727399296,330.107297176071));
#44348=CARTESIAN_POINT('Ctrl Pts',(164.955132094093,0.370893796117201,330.094020827439));
#44349=CARTESIAN_POINT('Ctrl Pts',(164.947720289916,0.240781402330473,330.085925876618));
#44350=CARTESIAN_POINT('Ctrl Pts',(164.940308485739,0.11074858573003,330.082997070038));
#44351=CARTESIAN_POINT('Ctrl Pts',(164.932533406961,-0.0256575265601337,
330.079924713922));
#44352=CARTESIAN_POINT('Ctrl Pts',(164.924758328182,-0.162407132311235,
330.082528013814));
#44353=CARTESIAN_POINT('Ctrl Pts',(164.916983249404,-0.298988803753761,
330.090846431641));
#44354=CARTESIAN_POINT('Ctrl Pts',(164.909217738355,-0.43540240275471,330.099154613126));
#44355=CARTESIAN_POINT('Ctrl Pts',(164.901452227306,-0.571648092207341,
330.113163895723));
#44356=CARTESIAN_POINT('Ctrl Pts',(164.893686716257,-0.707212030092754,
330.13286180523));
#44357=CARTESIAN_POINT('Ctrl Pts',(164.885928904735,-0.842641555938794,
330.152540184202));
#44358=CARTESIAN_POINT('Ctrl Pts',(164.878171093213,-0.977390291093121,
330.177895909745));
#44359=CARTESIAN_POINT('Ctrl Pts',(164.87041328169,-1.11094746427157,330.208864561074));
#44360=CARTESIAN_POINT('Ctrl Pts',(164.862661308167,-1.24440413144189,330.239809907511));
#44361=CARTESIAN_POINT('Ctrl Pts',(164.854909334644,-1.37667064221152,330.276359684322));
#44362=CARTESIAN_POINT('Ctrl Pts',(164.847157361121,-1.50724475102736,330.318398102893));
#44363=CARTESIAN_POINT('Ctrl Pts',(164.839408670564,-1.63776356163028,330.360418718168));
#44364=CARTESIAN_POINT('Ctrl Pts',(164.831659980006,-1.76659102451878,330.407923232513));
#44365=CARTESIAN_POINT('Ctrl Pts',(164.823911289449,-1.893238649988,330.46074560344));
#44366=CARTESIAN_POINT('Ctrl Pts',(164.816164211071,-2.01985992536101,330.513556984231));
#44367=CARTESIAN_POINT('Ctrl Pts',(164.808417132693,-2.14430190489733,330.57168387048));
#44368=CARTESIAN_POINT('Ctrl Pts',(164.800670054315,-2.2660951058813,330.634911680893));
#44369=CARTESIAN_POINT('Ctrl Pts',(164.792922911009,-2.38788932760944,330.698140021217));
#44370=CARTESIAN_POINT('Ctrl Pts',(164.785175767704,-2.50703437959486,330.766469190879));
#44371=CARTESIAN_POINT('Ctrl Pts',(164.777428624398,-2.62308481915098,330.839638345764));
#44372=CARTESIAN_POINT('Ctrl Pts',(164.76967973937,-2.73916134930914,330.912823950628));
#44373=CARTESIAN_POINT('Ctrl Pts',(164.761930854342,-2.85214155202689,330.990851497547));
#44374=CARTESIAN_POINT('Ctrl Pts',(164.754181969314,-2.96160878042939,331.073416689514));
#44375=CARTESIAN_POINT('Ctrl Pts',(164.746424859539,-3.07119219847979,331.15606951703));
#44376=CARTESIAN_POINT('Ctrl Pts',(164.738667749764,-3.17725488121721,331.243269374868));
#44377=CARTESIAN_POINT('Ctrl Pts',(164.730910639989,-3.27941269666047,331.33467117062));
#44378=CARTESIAN_POINT('Ctrl Pts',(164.723149385063,-3.38162510197416,331.42612180857));
#44379=CARTESIAN_POINT('Ctrl Pts',(164.715388130137,-3.47992820219039,331.521778586103));
#44380=CARTESIAN_POINT('Ctrl Pts',(164.707626875211,-3.57397533707553,331.621260093988));
#44381=CARTESIAN_POINT('Ctrl Pts',(164.699853204806,-3.66817291672646,331.720900739865));
#44382=CARTESIAN_POINT('Ctrl Pts',(164.692079534402,-3.75810066979844,331.824378047128));
#44383=CARTESIAN_POINT('Ctrl Pts',(164.684305863997,-3.84345222036665,331.931277449449));
#44384=CARTESIAN_POINT('Ctrl Pts',(164.67689405982,-3.92483063572159,332.033200658874));
#44385=CARTESIAN_POINT('Ctrl Pts',(164.669482255643,-4.00204913469065,332.138234304259));
#44386=CARTESIAN_POINT('Ctrl Pts',(164.662070451466,-4.07488024897162,332.245996728571));
#44387=CARTESIAN_POINT('Ctrl Pts',(164.654169951851,-4.15251346438675,332.360864441127));
#44388=CARTESIAN_POINT('Ctrl Pts',(164.646269452237,-4.22540144646196,332.479187903196));
#44389=CARTESIAN_POINT('Ctrl Pts',(164.638368952622,-4.29322723335163,332.600545273336));
#44390=CARTESIAN_POINT('Ctrl Pts',(164.630478996904,-4.360962500893,332.721740681625));
#44391=CARTESIAN_POINT('Ctrl Pts',(164.622589041186,-4.42364883999927,332.845961615013));
#44392=CARTESIAN_POINT('Ctrl Pts',(164.614699085468,-4.4810116748555,332.972756198108));
#44393=CARTESIAN_POINT('Ctrl Pts',(164.606818151548,-4.53830891797762,333.099405797494));
#44394=CARTESIAN_POINT('Ctrl Pts',(164.598937217627,-4.59029462212641,333.228622849245));
#44395=CARTESIAN_POINT('Ctrl Pts',(164.591056283707,-4.63673949099087,333.35992989321));
#44396=CARTESIAN_POINT('Ctrl Pts',(164.583179614105,-4.68315922885682,333.491165887838));
#44397=CARTESIAN_POINT('Ctrl Pts',(164.575302944504,-4.72404395697051,333.624489278899));
#44398=CARTESIAN_POINT('Ctrl Pts',(164.567426274903,-4.75921185762725,333.759401129809));
#44399=CARTESIAN_POINT('Ctrl Pts',(164.559559820631,-4.79433414868988,333.89413801222));
#44400=CARTESIAN_POINT('Ctrl Pts',(164.551693366359,-4.82375430849274,334.030458883297));
#44401=CARTESIAN_POINT('Ctrl Pts',(164.543826912088,-4.8473404005135,334.167849710659));
#44402=CARTESIAN_POINT('Ctrl Pts',(164.535945134821,-4.87097243566829,334.305508160364));
#44403=CARTESIAN_POINT('Ctrl Pts',(164.528063357555,-4.88874754373616,334.444240376606));
#44404=CARTESIAN_POINT('Ctrl Pts',(164.520181580289,-4.90058419455674,334.583517569926));
#44405=CARTESIAN_POINT('Ctrl Pts',(164.512299803023,-4.91242084537732,334.722794763246));
#44406=CARTESIAN_POINT('Ctrl Pts',(164.504418025756,-4.91831898961313,334.862616557649));
#44407=CARTESIAN_POINT('Ctrl Pts',(164.49653624849,-4.91824939077894,335.002447979287));
#44408=CARTESIAN_POINT('',(167.996536248449,-4.91824997640728,334.999518263764));
#44409=CARTESIAN_POINT('Ctrl Pts',(167.996536248449,-4.91824997640728,334.999518263764));
#44410=CARTESIAN_POINT('Ctrl Pts',(167.988782474437,-4.91826330456105,335.135591050191));
#44411=CARTESIAN_POINT('Ctrl Pts',(167.981028700426,-4.91262528295511,335.271884721958));
#44412=CARTESIAN_POINT('Ctrl Pts',(167.973274926414,-4.90130688742149,335.407889516677));
#44413=CARTESIAN_POINT('Ctrl Pts',(167.965530681001,-4.89000240104323,335.543727175354));
#44414=CARTESIAN_POINT('Ctrl Pts',(167.957786435588,-4.87303146095585,335.679276275156));
#44415=CARTESIAN_POINT('Ctrl Pts',(167.950042190175,-4.8504170187412,335.814025679451));
#44416=CARTESIAN_POINT('Ctrl Pts',(167.942305583009,-4.82782488143851,335.948642178695));
#44417=CARTESIAN_POINT('Ctrl Pts',(167.934568975844,-4.79960038272873,336.082460166602));
#44418=CARTESIAN_POINT('Ctrl Pts',(167.926832368679,-4.76581834802965,336.214972648286));
#44419=CARTESIAN_POINT('Ctrl Pts',(167.919101516249,-4.7320614414861,336.347386562958));
#44420=CARTESIAN_POINT('Ctrl Pts',(167.911370663819,-4.69275532322838,336.478496524548));
#44421=CARTESIAN_POINT('Ctrl Pts',(167.903639811389,-4.64802599510974,336.607805153395));
#44422=CARTESIAN_POINT('Ctrl Pts',(167.895912112537,-4.60331491303071,336.737061034516));
#44423=CARTESIAN_POINT('Ctrl Pts',(167.888184413685,-4.55318514861906,336.864516673185));
#44424=CARTESIAN_POINT('Ctrl Pts',(167.880456714834,-4.49781264724263,336.989689536788));
#44425=CARTESIAN_POINT('Ctrl Pts',(167.872730512087,-4.44245086614406,337.114838166559));
#44426=CARTESIAN_POINT('Ctrl Pts',(167.86500430934,-4.38184852582045,337.237704540794));
#44427=CARTESIAN_POINT('Ctrl Pts',(167.857278106594,-4.31622967029951,337.357826222546));
#44428=CARTESIAN_POINT('Ctrl Pts',(167.849551703081,-4.25060910966695,337.47795102567));
#44429=CARTESIAN_POINT('Ctrl Pts',(167.841825299568,-4.17997196292442,337.595330649212));
#44430=CARTESIAN_POINT('Ctrl Pts',(167.834098896056,-4.10458796687714,337.709527760453));
#44431=CARTESIAN_POINT('Ctrl Pts',(167.826370595115,-4.02918545824734,337.823752915889));
#44432=CARTESIAN_POINT('Ctrl Pts',(167.818642294175,-3.9490339976311,337.934793675944));
#44433=CARTESIAN_POINT('Ctrl Pts',(167.810913993234,-3.86444607508734,338.042242527354));
#44434=CARTESIAN_POINT('Ctrl Pts',(167.803177450501,-3.77976794434275,338.149805966843));
#44435=CARTESIAN_POINT('Ctrl Pts',(167.795440907768,-3.69064414589996,338.253769537759));
#44436=CARTESIAN_POINT('Ctrl Pts',(167.787704365035,-3.5974271314745,338.3537592484));
#44437=CARTESIAN_POINT('Ctrl Pts',(167.779963499509,-3.50415803204282,338.453804828292));
#44438=CARTESIAN_POINT('Ctrl Pts',(167.772222633983,-3.40679144008804,338.549871848678));
#44439=CARTESIAN_POINT('Ctrl Pts',(167.764481768456,-3.30571516406244,338.641624680907));
#44440=CARTESIAN_POINT('Ctrl Pts',(167.756728880654,-3.20448190729009,338.733520013716));
#44441=CARTESIAN_POINT('Ctrl Pts',(167.748975992852,-3.0995277583632,338.821087521177));
#44442=CARTESIAN_POINT('Ctrl Pts',(167.74122310505,-2.99127252594288,338.904032753198));
#44443=CARTESIAN_POINT('Ctrl Pts',(167.73504501286,-2.90500650183863,338.97012983899));
#44444=CARTESIAN_POINT('Ctrl Pts',(167.728866920669,-2.81664490383749,339.033292524293));
#44445=CARTESIAN_POINT('Ctrl Pts',(167.722688828479,-2.72641170751432,339.093392512773));
#44446=CARTESIAN_POINT('Ctrl Pts',(167.7149137497,-2.6128539637631,339.169027859512));
#44447=CARTESIAN_POINT('Ctrl Pts',(167.707138670922,-2.49596701032929,339.240053713681));
#44448=CARTESIAN_POINT('Ctrl Pts',(167.699363592144,-2.37616164720912,339.306162896226));
#44449=CARTESIAN_POINT('Ctrl Pts',(167.691598081095,-2.25650371221542,339.372190727213));
#44450=CARTESIAN_POINT('Ctrl Pts',(167.683832570046,-2.1339348521281,339.433313737856));
#44451=CARTESIAN_POINT('Ctrl Pts',(167.676067058997,-2.00889571584567,339.489267319436));
#44452=CARTESIAN_POINT('Ctrl Pts',(167.668309247474,-1.88398055623153,339.545165422876));
#44453=CARTESIAN_POINT('Ctrl Pts',(167.660551435952,-1.75660034912292,339.595904138669));
#44454=CARTESIAN_POINT('Ctrl Pts',(167.65279362443,-1.62722096553022,339.641264374267));
#44455=CARTESIAN_POINT('Ctrl Pts',(167.645041650907,-1.49793894402527,339.68659047485));
#44456=CARTESIAN_POINT('Ctrl Pts',(167.637289677384,-1.36666110793366,339.726546022741));
#44457=CARTESIAN_POINT('Ctrl Pts',(167.629537703861,-1.23387363341416,339.76095987373));
#44458=CARTESIAN_POINT('Ctrl Pts',(167.621789013303,-1.10114239446967,339.795359150432));
#44459=CARTESIAN_POINT('Ctrl Pts',(167.614040322746,-0.966903166271453,
339.824221300216));
#44460=CARTESIAN_POINT('Ctrl Pts',(167.606291632188,-0.83165741650632,339.847424986946));
#44461=CARTESIAN_POINT('Ctrl Pts',(167.59854455381,-0.696439805749181,339.870623845955));
#44462=CARTESIAN_POINT('Ctrl Pts',(167.590797475432,-0.560216474970463,
339.88816651757));
#44463=CARTESIAN_POINT('Ctrl Pts',(167.583050397055,-0.423498830134245,
339.899982837049));
#44464=CARTESIAN_POINT('Ctrl Pts',(167.575303253749,-0.286780039472225,
339.911799255561));
#44465=CARTESIAN_POINT('Ctrl Pts',(167.567556110443,-0.149567315912039,
339.917889192556));
#44466=CARTESIAN_POINT('Ctrl Pts',(167.559808967137,-0.0123765342951703,
339.918234427505));
#44467=CARTESIAN_POINT('Ctrl Pts',(167.552060082109,0.124845090721558,339.918579740071));
#44468=CARTESIAN_POINT('Ctrl Pts',(167.544311197081,0.26204437318215,339.913177779605));
#44469=CARTESIAN_POINT('Ctrl Pts',(167.536562312053,0.398706490519899,339.902062443188));
#44470=CARTESIAN_POINT('Ctrl Pts',(167.528805202278,0.535513662441278,339.890935308839));
#44471=CARTESIAN_POINT('Ctrl Pts',(167.521048092503,0.671782140103341,339.874082716395));
#44472=CARTESIAN_POINT('Ctrl Pts',(167.513290982729,0.807002717186098,339.851590427577));
#44473=CARTESIAN_POINT('Ctrl Pts',(167.505529727803,0.942295551821779,339.829086119598));
#44474=CARTESIAN_POINT('Ctrl Pts',(167.497768472876,1.0765389877383,339.800936190408));
#44475=CARTESIAN_POINT('Ctrl Pts',(167.49000721795,1.20923601932964,339.767277138163));
#44476=CARTESIAN_POINT('Ctrl Pts',(167.482233547546,1.34214532292559,339.733564242405));
#44477=CARTESIAN_POINT('Ctrl Pts',(167.474459877141,1.47350290420733,339.694324724941));
#44478=CARTESIAN_POINT('Ctrl Pts',(167.466686206736,1.60282802557411,339.649744657821));
#44479=CARTESIAN_POINT('Ctrl Pts',(167.459274402559,1.72613303142783,339.60723980355));
#44480=CARTESIAN_POINT('Ctrl Pts',(167.451862598382,1.84759027292765,339.559880520056));
#44481=CARTESIAN_POINT('Ctrl Pts',(167.444450794205,1.96680327628418,339.507867337766));
#44482=CARTESIAN_POINT('Ctrl Pts',(167.436675715427,2.09185926405209,339.453304834473));
#44483=CARTESIAN_POINT('Ctrl Pts',(167.428900636648,2.21484065756744,339.39344826681));
#44484=CARTESIAN_POINT('Ctrl Pts',(167.42112555787,2.3352668359619,339.328476853046));
#44485=CARTESIAN_POINT('Ctrl Pts',(167.413360046821,2.45554482227723,339.263585390743));
#44486=CARTESIAN_POINT('Ctrl Pts',(167.405594535772,2.57327350912233,339.1935917897));
#44487=CARTESIAN_POINT('Ctrl Pts',(167.397829024723,2.68799192097653,339.118723406016));
#44488=CARTESIAN_POINT('Ctrl Pts',(167.3900712132,2.80259658919157,339.043929254552));
#44489=CARTESIAN_POINT('Ctrl Pts',(167.382313401678,2.91419659690643,338.964270151358));
#44490=CARTESIAN_POINT('Ctrl Pts',(167.374555590156,3.02235559498915,338.880019293758));
#44491=CARTESIAN_POINT('Ctrl Pts',(167.366803616633,3.13043319999614,338.7958318376));
#44492=CARTESIAN_POINT('Ctrl Pts',(167.35905164311,3.23507464246211,338.707059744154));
#44493=CARTESIAN_POINT('Ctrl Pts',(167.351299669587,3.33587290575179,338.61401923337));
#44494=CARTESIAN_POINT('Ctrl Pts',(167.343550979029,3.43662848091667,338.521018125299));
#44495=CARTESIAN_POINT('Ctrl Pts',(167.335802288472,3.53354382744071,338.423752459797));
#44496=CARTESIAN_POINT('Ctrl Pts',(167.328053597914,3.62624553823805,338.322578269794));
#44497=CARTESIAN_POINT('Ctrl Pts',(167.320306519536,3.71892796167028,338.221425129927));
#44498=CARTESIAN_POINT('Ctrl Pts',(167.312559441158,3.80739822926484,338.116365371086));
#44499=CARTESIAN_POINT('Ctrl Pts',(167.30481236278,3.89132058688308,338.007791075291));
#44500=CARTESIAN_POINT('Ctrl Pts',(167.297065219475,3.97524364785143,337.899215869538));
#44501=CARTESIAN_POINT('Ctrl Pts',(167.289318076169,4.05461848377652,337.78712637734));
#44502=CARTESIAN_POINT('Ctrl Pts',(167.281570932863,4.12915060314886,337.671946548682));
#44503=CARTESIAN_POINT('Ctrl Pts',(167.273822047835,4.20369947892386,337.556740825154));
#44504=CARTESIAN_POINT('Ctrl Pts',(167.266073162807,4.27340325935474,337.438443710742));
#44505=CARTESIAN_POINT('Ctrl Pts',(167.258324277779,4.33801184918885,337.317506474381));
#44506=CARTESIAN_POINT('Ctrl Pts',(167.250567168004,4.40268901524788,337.196440873988));
#44507=CARTESIAN_POINT('Ctrl Pts',(167.242810058229,4.46226000307407,337.072729899188));
#44508=CARTESIAN_POINT('Ctrl Pts',(167.235052948455,4.51652137076929,336.946848163028));
#44509=CARTESIAN_POINT('Ctrl Pts',(167.227291693528,4.57081173400451,336.820899159692));
#44510=CARTESIAN_POINT('Ctrl Pts',(167.219530438602,4.61978668405707,336.692777448544));
#44511=CARTESIAN_POINT('Ctrl Pts',(167.211769183676,4.66329204688818,336.562974839186));
#44512=CARTESIAN_POINT('Ctrl Pts',(167.203995513271,4.70686700412138,336.432964587956));
#44513=CARTESIAN_POINT('Ctrl Pts',(167.196221842867,4.74495478127576,336.301268441003));
#44514=CARTESIAN_POINT('Ctrl Pts',(167.188448172462,4.77745169560569,336.168391355092));
#44515=CARTESIAN_POINT('Ctrl Pts',(167.181036368285,4.80843587075487,336.041699729501));
#44516=CARTESIAN_POINT('Ctrl Pts',(167.173624564108,4.83433792148842,335.913934918175));
#44517=CARTESIAN_POINT('Ctrl Pts',(167.166212759931,4.85511192340498,335.785538842904));
#44518=CARTESIAN_POINT('Ctrl Pts',(167.158437681153,4.87690412103831,335.65084969351));
#44519=CARTESIAN_POINT('Ctrl Pts',(167.150662602374,4.89312174500852,335.515040192678));
#44520=CARTESIAN_POINT('Ctrl Pts',(167.142887523596,4.90365541225215,335.37861149004));
#44521=CARTESIAN_POINT('Ctrl Pts',(167.135122012547,4.91417611714764,335.242350671605));
#44522=CARTESIAN_POINT('Ctrl Pts',(167.127356501498,4.91902675250529,335.10547255345));
#44523=CARTESIAN_POINT('Ctrl Pts',(167.119590990449,4.91814904661359,334.968487815153));
#44524=CARTESIAN_POINT('Ctrl Pts',(167.111833178926,4.91727221096984,334.831638897623));
#44525=CARTESIAN_POINT('Ctrl Pts',(167.104075367404,4.91067833942356,334.694683958678));
#44526=CARTESIAN_POINT('Ctrl Pts',(167.096317555882,4.8983610358791,334.558137776359));
#44527=CARTESIAN_POINT('Ctrl Pts',(167.088565582359,4.88605300149619,334.421694349372));
#44528=CARTESIAN_POINT('Ctrl Pts',(167.080813608836,4.86803014309089,334.285659454471));
#44529=CARTESIAN_POINT('Ctrl Pts',(167.073061635313,4.84433811671005,334.150546485386));
#44530=CARTESIAN_POINT('Ctrl Pts',(167.065312944755,4.82065612391641,334.015490736724));
#44531=CARTESIAN_POINT('Ctrl Pts',(167.057564254198,4.7913098057294,333.881356521528));
#44532=CARTESIAN_POINT('Ctrl Pts',(167.04981556364,4.75639648583532,333.74865051563));
#44533=CARTESIAN_POINT('Ctrl Pts',(167.042068485262,4.72149042994909,333.615972120325));
#44534=CARTESIAN_POINT('Ctrl Pts',(167.034321406885,4.68101977560688,333.484721721038));
#44535=CARTESIAN_POINT('Ctrl Pts',(167.026574328507,4.63513253711278,333.355393838666));
#44536=CARTESIAN_POINT('Ctrl Pts',(167.018827185201,4.58924491403937,333.226064872401));
#44537=CARTESIAN_POINT('Ctrl Pts',(167.011080041895,4.53794074697179,333.098658823561));
#44538=CARTESIAN_POINT('Ctrl Pts',(167.003332898589,4.48141717824412,332.973652760004));
#44539=CARTESIAN_POINT('Ctrl Pts',(166.995584013561,4.42488090181821,332.84861859243));
#44540=CARTESIAN_POINT('Ctrl Pts',(166.987835128533,4.36312304974399,332.725985839905));
#44541=CARTESIAN_POINT('Ctrl Pts',(166.980086243505,4.29638776280485,332.606209020378));
#44542=CARTESIAN_POINT('Ctrl Pts',(166.97232913373,4.22958164234264,332.486305068497));
#44543=CARTESIAN_POINT('Ctrl Pts',(166.964572023956,4.15778772407131,332.369263446944));
#44544=CARTESIAN_POINT('Ctrl Pts',(166.956814914181,4.08129502614167,332.255512074705));
#44545=CARTESIAN_POINT('Ctrl Pts',(166.949053659255,4.00476145295993,332.141699917369));
#44546=CARTESIAN_POINT('Ctrl Pts',(166.941292404328,3.92352432835442,332.031181827511));
#44547=CARTESIAN_POINT('Ctrl Pts',(166.933531149402,3.83791379309335,331.924353599764));
#44548=CARTESIAN_POINT('Ctrl Pts',(166.925757478998,3.7521663088763,331.817354481668));
#44549=CARTESIAN_POINT('Ctrl Pts',(166.917983808593,3.66203169098352,331.714057315452));
#44550=CARTESIAN_POINT('Ctrl Pts',(166.910210138188,3.56787845964979,331.614822551229));
#44551=CARTESIAN_POINT('Ctrl Pts',(166.902798334011,3.47810808388649,331.520207189155));
#44552=CARTESIAN_POINT('Ctrl Pts',(166.895386529834,3.38468501420987,331.429284731544));
#44553=CARTESIAN_POINT('Ctrl Pts',(166.887974725657,3.28795601975188,331.342332946443));
#44554=CARTESIAN_POINT('Ctrl Pts',(166.880199646879,3.18648604913493,331.251119395338));
#44555=CARTESIAN_POINT('Ctrl Pts',(166.8724245681,3.08105722941441,331.163987335706));
#44556=CARTESIAN_POINT('Ctrl Pts',(166.864649489322,2.9720317945545,331.08129995092));
#44557=CARTESIAN_POINT('Ctrl Pts',(166.856883978273,2.86314052243333,330.998714318226));
#44558=CARTESIAN_POINT('Ctrl Pts',(166.849118467224,2.75066174983152,330.920562711671));
#44559=CARTESIAN_POINT('Ctrl Pts',(166.841352956175,2.63499338393629,330.847170491206));
#44560=CARTESIAN_POINT('Ctrl Pts',(166.833595144653,2.51943970356208,330.77385103934));
#44561=CARTESIAN_POINT('Ctrl Pts',(166.82583733313,2.40070305134741,330.705281790662));
#44562=CARTESIAN_POINT('Ctrl Pts',(166.818079521608,2.2792128538355,330.641746699719));
#44563=CARTESIAN_POINT('Ctrl Pts',(166.810327548085,2.15781408154979,330.578259420947));
#44564=CARTESIAN_POINT('Ctrl Pts',(166.802575574562,2.03366623341493,330.519798939769));
#44565=CARTESIAN_POINT('Ctrl Pts',(166.794823601039,1.90722574027958,330.466604689847));
#44566=CARTESIAN_POINT('Ctrl Pts',(166.787074910481,1.7808387947685,330.413432967722));
#44567=CARTESIAN_POINT('Ctrl Pts',(166.779326219924,1.6521614949197,330.3655231923));
#44568=CARTESIAN_POINT('Ctrl Pts',(166.771577529366,1.52167258268121,330.323067713381));
#44569=CARTESIAN_POINT('Ctrl Pts',(166.763830450988,1.39121081975087,330.28062106768));
#44570=CARTESIAN_POINT('Ctrl Pts',(166.756083372611,1.25893856561594,330.243626582119));
#44571=CARTESIAN_POINT('Ctrl Pts',(166.748336294233,1.12535177248105,330.212227401946));
#44572=CARTESIAN_POINT('Ctrl Pts',(166.740589150927,0.991763859760445,330.180827958618));
#44573=CARTESIAN_POINT('Ctrl Pts',(166.732842007621,0.856861766570149,330.155024003647));
#44574=CARTESIAN_POINT('Ctrl Pts',(166.725094864315,0.721153354477636,330.13490792463));
#44575=CARTESIAN_POINT('Ctrl Pts',(166.717345979287,0.585414432252612,330.114787323092));
#44576=CARTESIAN_POINT('Ctrl Pts',(166.709597094259,0.448869216977219,330.10035719939));
#44577=CARTESIAN_POINT('Ctrl Pts',(166.701848209231,0.312032041077469,330.091658216073));
#44578=CARTESIAN_POINT('Ctrl Pts',(166.694091099456,0.175049624785287,330.082949999566));
#44579=CARTESIAN_POINT('Ctrl Pts',(166.686333989682,0.037775019537325,330.079985099827));
#44580=CARTESIAN_POINT('Ctrl Pts',(166.678576879907,-0.0992755241577299,
330.082752046845));
#44581=CARTESIAN_POINT('Ctrl Pts',(166.670815624981,-0.236399303281239,
330.085520472432));
#44582=CARTESIAN_POINT('Ctrl Pts',(166.663054370055,-0.373298392352362,
330.094026823681));
#44583=CARTESIAN_POINT('Ctrl Pts',(166.655293115128,-0.509461301106,330.108207665367));
#44584=CARTESIAN_POINT('Ctrl Pts',(166.647519444724,-0.645842026138325,
330.122411191778));
#44585=CARTESIAN_POINT('Ctrl Pts',(166.639745774319,-0.781483830623061,
330.142307291072));
#44586=CARTESIAN_POINT('Ctrl Pts',(166.631972103914,-0.915884176925122,
330.167781126961));
#44587=CARTESIAN_POINT('Ctrl Pts',(166.624560299737,-1.04402815477236,330.19206914966));
#44588=CARTESIAN_POINT('Ctrl Pts',(166.61714849556,-1.17104337273989,330.221427243102));
#44589=CARTESIAN_POINT('Ctrl Pts',(166.609736691383,-1.29650859307653,330.255714117954));
#44590=CARTESIAN_POINT('Ctrl Pts',(166.601961612605,-1.42812323760285,330.291681494678));
#44591=CARTESIAN_POINT('Ctrl Pts',(166.594186533826,-1.55844802928339,330.333186681303));
#44592=CARTESIAN_POINT('Ctrl Pts',(166.586411455048,-1.68698153388864,330.380121606923));
#44593=CARTESIAN_POINT('Ctrl Pts',(166.578645943999,-1.81535686983368,330.42699877613));
#44594=CARTESIAN_POINT('Ctrl Pts',(166.57088043295,-1.94194494096252,330.479292256995));
#44595=CARTESIAN_POINT('Ctrl Pts',(166.563114921901,-2.06625681474186,330.536843511814));
#44596=CARTESIAN_POINT('Ctrl Pts',(166.555357110379,-2.19044543293661,330.594337704397));
#44597=CARTESIAN_POINT('Ctrl Pts',(166.547599298856,-2.31236199263233,330.657079133417));
#44598=CARTESIAN_POINT('Ctrl Pts',(166.539841487334,-2.43153532304733,330.724860349033));
#44599=CARTESIAN_POINT('Ctrl Pts',(166.532089513811,-2.55061897175201,330.792590557134));
#44600=CARTESIAN_POINT('Ctrl Pts',(166.524337540288,-2.66696316180209,330.865352810382));
#44601=CARTESIAN_POINT('Ctrl Pts',(166.516585566765,-2.7801195474,330.942892857631));
#44602=CARTESIAN_POINT('Ctrl Pts',(166.508836876208,-2.89322801120153,331.020400066624));
#44603=CARTESIAN_POINT('Ctrl Pts',(166.50108818565,-3.00315103391497,331.102680824733));
#44604=CARTESIAN_POINT('Ctrl Pts',(166.493339495092,-3.10946778975002,331.189436639156));
#44605=CARTESIAN_POINT('Ctrl Pts',(166.485592416715,-3.21576242549584,331.276174403307));
#44606=CARTESIAN_POINT('Ctrl Pts',(166.477845338337,-3.31845198413921,331.367385124834));
#44607=CARTESIAN_POINT('Ctrl Pts',(166.470098259959,-3.41714770359287,331.462729211054));
#44608=CARTESIAN_POINT('Ctrl Pts',(166.462351116653,-3.51584425021167,331.55807409635));
#44609=CARTESIAN_POINT('Ctrl Pts',(166.454603973347,-3.61054660975593,331.657552143858));
#44610=CARTESIAN_POINT('Ctrl Pts',(166.446856830042,-3.70090225848921,331.760786278183));
#44611=CARTESIAN_POINT('Ctrl Pts',(166.439107945013,-3.79127822109058,331.864043621732));
#44612=CARTESIAN_POINT('Ctrl Pts',(166.431359059985,-3.87730527091292,331.971058438386));
#44613=CARTESIAN_POINT('Ctrl Pts',(166.423610174957,-3.9586708791634,332.081420219873));
#44614=CARTESIAN_POINT('Ctrl Pts',(166.415853065183,-4.04012284971122,332.191899140496));
#44615=CARTESIAN_POINT('Ctrl Pts',(166.408095955408,-4.11690326286945,332.305731807299));
#44616=CARTESIAN_POINT('Ctrl Pts',(166.400338845633,-4.18874239124351,332.422477887137));
#44617=CARTESIAN_POINT('Ctrl Pts',(166.392577590707,-4.26061990815084,332.539286352346));
#44618=CARTESIAN_POINT('Ctrl Pts',(166.384816335781,-4.32755068827428,332.659010991716));
#44619=CARTESIAN_POINT('Ctrl Pts',(166.377055080855,-4.38931127891853,332.781187353728));
#44620=CARTESIAN_POINT('Ctrl Pts',(166.36928141045,-4.45117066638002,332.903559158101));
#44621=CARTESIAN_POINT('Ctrl Pts',(166.361507740045,-4.50784317555067,333.028390166249));
#44622=CARTESIAN_POINT('Ctrl Pts',(166.353734069641,-4.55915342276538,333.155195639048));
#44623=CARTESIAN_POINT('Ctrl Pts',(166.346322265464,-4.60807516562759,333.27609828658));
#44624=CARTESIAN_POINT('Ctrl Pts',(166.338910461287,-4.65212254109825,333.398795442048));
#44625=CARTESIAN_POINT('Ctrl Pts',(166.331498657109,-4.69118640647375,333.522856417874));
#44626=CARTESIAN_POINT('Ctrl Pts',(166.322082044832,-4.74081659981526,333.680474466093));
#44627=CARTESIAN_POINT('Ctrl Pts',(166.312665432554,-4.78253107194937,333.840696708659));
#44628=CARTESIAN_POINT('Ctrl Pts',(166.303248820276,-4.81609572084062,334.002801388789));
#44629=CARTESIAN_POINT('Ctrl Pts',(166.293796724985,-4.84978684566856,334.165516900313));
#44630=CARTESIAN_POINT('Ctrl Pts',(166.284344629695,-4.87526646562748,334.330129101346));
#44631=CARTESIAN_POINT('Ctrl Pts',(166.274892534404,-4.89234628133885,334.495885999034));
#44632=CARTESIAN_POINT('Ctrl Pts',(166.265440439114,-4.90942609705022,334.661642896723));
#44633=CARTESIAN_POINT('Ctrl Pts',(166.255988343823,-4.91810593516986,334.828544509634));
#44634=CARTESIAN_POINT('Ctrl Pts',(166.246536248533,-4.9182482206735,334.995816419961));
#44635=CARTESIAN_POINT('',(169.746536248436,-4.91824799493152,335.004441041773));
#44636=CARTESIAN_POINT('Ctrl Pts',(169.746536248436,-4.91824799493153,335.004441041773));
#44637=CARTESIAN_POINT('Ctrl Pts',(169.736906562874,-4.91809427474665,335.174679024157));
#44638=CARTESIAN_POINT('Ctrl Pts',(169.727276877313,-4.90909813996316,335.344523781032));
#44639=CARTESIAN_POINT('Ctrl Pts',(169.717647191752,-4.89140358538227,335.513180306919));
#44640=CARTESIAN_POINT('Ctrl Pts',(169.707853191742,-4.87340710287746,335.68471467381));
#44641=CARTESIAN_POINT('Ctrl Pts',(169.698059191733,-4.84641285341689,335.855020025711));
#44642=CARTESIAN_POINT('Ctrl Pts',(169.688265191723,-4.81062090901127,336.023283700781));
#44643=CARTESIAN_POINT('Ctrl Pts',(169.682295150614,-4.78880353314214,336.125850686315));
#44644=CARTESIAN_POINT('Ctrl Pts',(169.676325109505,-4.76371818085054,336.227659510964));
#44645=CARTESIAN_POINT('Ctrl Pts',(169.670355068397,-4.73541877841011,336.328530035634));
#44646=CARTESIAN_POINT('Ctrl Pts',(169.662579989618,-4.69856307183378,336.459898691465));
#44647=CARTESIAN_POINT('Ctrl Pts',(169.65480491084,-4.65617839560353,336.589940112037));
#44648=CARTESIAN_POINT('Ctrl Pts',(169.647029832061,-4.60837620570426,336.718153604658));
#44649=CARTESIAN_POINT('Ctrl Pts',(169.639264321012,-4.56063283944293,336.846209322414));
#44650=CARTESIAN_POINT('Ctrl Pts',(169.631498809963,-4.50748535936967,336.972441225097));
#44651=CARTESIAN_POINT('Ctrl Pts',(169.623733298914,-4.44909560265916,337.096361462367));
#44652=CARTESIAN_POINT('Ctrl Pts',(169.615975487392,-4.39076373956246,337.220158832362));
#44653=CARTESIAN_POINT('Ctrl Pts',(169.60821767587,-4.32720010914372,337.341648746887));
#44654=CARTESIAN_POINT('Ctrl Pts',(169.600459864348,-4.25861533960452,337.460361447386));
#44655=CARTESIAN_POINT('Ctrl Pts',(169.592707890825,-4.1900821822793,337.578984812814));
#44656=CARTESIAN_POINT('Ctrl Pts',(169.584955917302,-4.11653560163343,337.694834787053));
#44657=CARTESIAN_POINT('Ctrl Pts',(169.577203943779,-4.03823287190434,337.807464752187));
#44658=CARTESIAN_POINT('Ctrl Pts',(169.569455253221,-3.95996330342776,337.920047018463));
#44659=CARTESIAN_POINT('Ctrl Pts',(169.561706562663,-3.87694181469024,338.02941166762));
#44660=CARTESIAN_POINT('Ctrl Pts',(169.553957872106,-3.78946973466079,338.135139900003));
#44661=CARTESIAN_POINT('Ctrl Pts',(169.546210793728,-3.70201585392821,338.240846134744));
#44662=CARTESIAN_POINT('Ctrl Pts',(169.53846371535,-3.61011347275525,338.342917156638));
#44663=CARTESIAN_POINT('Ctrl Pts',(169.530716636972,-3.51410480244014,338.440966506662));
#44664=CARTESIAN_POINT('Ctrl Pts',(169.522969493666,-3.4180953274799,338.539016678433));
#44665=CARTESIAN_POINT('Ctrl Pts',(169.51522235036,-3.31797976820315,338.633044831824));
#44666=CARTESIAN_POINT('Ctrl Pts',(169.507475207055,-3.21413757295082,338.722700998555));
#44667=CARTESIAN_POINT('Ctrl Pts',(169.499726322027,-3.11027203176837,338.812377321897));
#44668=CARTESIAN_POINT('Ctrl Pts',(169.491977436998,-3.00267848322954,338.897679447295));
#44669=CARTESIAN_POINT('Ctrl Pts',(169.48422855197,-2.89176953759251,338.978297626366));
#44670=CARTESIAN_POINT('Ctrl Pts',(169.476471442196,-2.78074287205469,339.059001374405));
#44671=CARTESIAN_POINT('Ctrl Pts',(169.468714332421,-2.66639409656422,339.135011014717));
#44672=CARTESIAN_POINT('Ctrl Pts',(169.460957222646,-2.54916535642159,339.206059800825));
#44673=CARTESIAN_POINT('Ctrl Pts',(169.45319596772,-2.43187397298848,339.277146553134));
#44674=CARTESIAN_POINT('Ctrl Pts',(169.445434712794,-2.31169990067159,339.34326698071));
#44675=CARTESIAN_POINT('Ctrl Pts',(169.437673457867,-2.18910908997195,339.404200773659));
#44676=CARTESIAN_POINT('Ctrl Pts',(169.429899787463,-2.06632217392745,339.465232040819));
#44677=CARTESIAN_POINT('Ctrl Pts',(169.422126117058,-1.94111115128372,339.521059934381));
#44678=CARTESIAN_POINT('Ctrl Pts',(169.414352446653,-1.813961934944,339.571512349439));
#44679=CARTESIAN_POINT('Ctrl Pts',(169.406940642476,-1.69273154521676,339.619616192438));
#44680=CARTESIAN_POINT('Ctrl Pts',(169.399528838299,-1.56973961832718,339.6628336561));
#44681=CARTESIAN_POINT('Ctrl Pts',(169.392117034122,-1.4454175693604,339.701058509813));
#44682=CARTESIAN_POINT('Ctrl Pts',(169.384341955344,-1.31500212643597,339.741156877473));
#44683=CARTESIAN_POINT('Ctrl Pts',(169.376566876566,-1.18271074122502,339.77588757344));
#44684=CARTESIAN_POINT('Ctrl Pts',(169.368791797787,-1.04902477212184,339.805073369885));
#44685=CARTESIAN_POINT('Ctrl Pts',(169.361026286738,-0.915503312114484,
339.834223251349));
#44686=CARTESIAN_POINT('Ctrl Pts',(169.353260775689,-0.780591061039154,
339.85784172723));
#44687=CARTESIAN_POINT('Ctrl Pts',(169.34549526464,-0.644785842036669,339.87580088605));
#44688=CARTESIAN_POINT('Ctrl Pts',(169.337737453118,-0.509115274304072,
339.893742238312));
#44689=CARTESIAN_POINT('Ctrl Pts',(169.329979641596,-0.37255388560567,339.906035389262));
#44690=CARTESIAN_POINT('Ctrl Pts',(169.322221830073,-0.235610688940603,
339.912603247338));
#44691=CARTESIAN_POINT('Ctrl Pts',(169.31446985655,-0.0987705463739764,
339.919166162893));
#44692=CARTESIAN_POINT('Ctrl Pts',(169.306717883027,0.0384504434042439,
339.920012342711));
#44693=CARTESIAN_POINT('Ctrl Pts',(169.298965909504,0.175537484005724,339.915116443606));
#44694=CARTESIAN_POINT('Ctrl Pts',(169.291217218947,0.312566468164167,339.910222617917));
#44695=CARTESIAN_POINT('Ctrl Pts',(169.283468528389,0.449461226160686,339.899591563854));
#44696=CARTESIAN_POINT('Ctrl Pts',(169.275719837832,0.585706514034807,339.883250038849));
#44697=CARTESIAN_POINT('Ctrl Pts',(169.267972759454,0.721923454938865,339.866911913835));
#44698=CARTESIAN_POINT('Ctrl Pts',(169.260225681076,0.85749080665001,339.844865727636));
#44699=CARTESIAN_POINT('Ctrl Pts',(169.252478602698,0.99189839735956,339.817190117882));
#44700=CARTESIAN_POINT('Ctrl Pts',(169.244731459392,1.12630711453411,339.789514276178));
#44701=CARTESIAN_POINT('Ctrl Pts',(169.236984316087,1.25955566847734,339.756208995645));
#44702=CARTESIAN_POINT('Ctrl Pts',(169.229237172781,1.39114442212714,339.71740397457));
#44703=CARTESIAN_POINT('Ctrl Pts',(169.221488287753,1.52276275972243,339.678590229302));
#44704=CARTESIAN_POINT('Ctrl Pts',(169.213739402725,1.65272017964195,339.634274393616));
#44705=CARTESIAN_POINT('Ctrl Pts',(169.205990517697,1.78053292077407,339.584635817657));
#44706=CARTESIAN_POINT('Ctrl Pts',(169.198233407922,1.90848132367025,339.5349445548));
#44707=CARTESIAN_POINT('Ctrl Pts',(169.190476298147,2.03428013555196,339.479919407771));
#44708=CARTESIAN_POINT('Ctrl Pts',(169.182719188372,2.15746577342481,339.419787834161));
#44709=CARTESIAN_POINT('Ctrl Pts',(169.174957933446,2.28071723776381,339.359624128162));
#44710=CARTESIAN_POINT('Ctrl Pts',(169.16719667852,2.40135240204773,339.2943487443));
#44711=CARTESIAN_POINT('Ctrl Pts',(169.159435423594,2.51893385043307,339.224234287968));
#44712=CARTESIAN_POINT('Ctrl Pts',(169.151661753189,2.63670339081611,339.154007671356));
#44713=CARTESIAN_POINT('Ctrl Pts',(169.143888082785,2.7514091265073,339.078926727765));
#44714=CARTESIAN_POINT('Ctrl Pts',(169.13611441238,2.86264337546678,338.999306935882));
#44715=CARTESIAN_POINT('Ctrl Pts',(169.128702608203,2.96869964337571,338.923393464467));
#44716=CARTESIAN_POINT('Ctrl Pts',(169.121290804026,3.07160011948947,338.843354378633));
#44717=CARTESIAN_POINT('Ctrl Pts',(169.113878999849,3.17102200876316,338.759494977047));
#44718=CARTESIAN_POINT('Ctrl Pts',(169.10610392107,3.27531686099277,338.671525376385));
#44719=CARTESIAN_POINT('Ctrl Pts',(169.098328842292,3.37611310359405,338.579073500683));
#44720=CARTESIAN_POINT('Ctrl Pts',(169.090553763514,3.47300121125691,338.482448226336));
#44721=CARTESIAN_POINT('Ctrl Pts',(169.082788252465,3.56977009193509,338.38594185554));
#44722=CARTESIAN_POINT('Ctrl Pts',(169.075022741416,3.66264013250227,338.285272577912));
#44723=CARTESIAN_POINT('Ctrl Pts',(169.067257230367,3.75123436879995,338.180789803309));
#44724=CARTESIAN_POINT('Ctrl Pts',(169.059499418844,3.83974076365441,338.076410623682));
#44725=CARTESIAN_POINT('Ctrl Pts',(169.051741607322,3.92397953986661,337.968225767876));
#44726=CARTESIAN_POINT('Ctrl Pts',(169.0439837958,4.00361041335615,337.856621557114));
#44727=CARTESIAN_POINT('Ctrl Pts',(169.036231822277,4.08318136208807,337.74510133206));
#44728=CARTESIAN_POINT('Ctrl Pts',(169.028479848754,4.15815108405777,337.630167190727));
#44729=CARTESIAN_POINT('Ctrl Pts',(169.020727875231,4.22821968177318,337.512238321729));
#44730=CARTESIAN_POINT('Ctrl Pts',(169.012979184673,4.29825860539588,337.394359395678));
#44731=CARTESIAN_POINT('Ctrl Pts',(169.005230494116,4.36340033380143,337.273488599793));
#44732=CARTESIAN_POINT('Ctrl Pts',(168.997481803558,4.42338853981542,337.150073693697));
#44733=CARTESIAN_POINT('Ctrl Pts',(168.98973472518,4.48336426478213,337.026684465104));
#44734=CARTESIAN_POINT('Ctrl Pts',(168.981987646802,4.53818842933706,336.900752530485));
#44735=CARTESIAN_POINT('Ctrl Pts',(168.974240568425,4.58765107829978,336.772749459533));
#44736=CARTESIAN_POINT('Ctrl Pts',(168.966493425119,4.63711414180711,336.644745315792));
#44737=CARTESIAN_POINT('Ctrl Pts',(168.958746281813,4.68121545920871,336.514670365694));
#44738=CARTESIAN_POINT('Ctrl Pts',(168.950999138507,4.71979371427856,336.383014951892));
#44739=CARTESIAN_POINT('Ctrl Pts',(168.943250253479,4.75838064255917,336.251329939157));
#44740=CARTESIAN_POINT('Ctrl Pts',(168.935501368451,4.79144192776782,336.118064130695));
#44741=CARTESIAN_POINT('Ctrl Pts',(168.927752483423,4.81886659837128,335.9837213882));
#44742=CARTESIAN_POINT('Ctrl Pts',(168.919995373648,4.84632037780348,335.849236052929));
#44743=CARTESIAN_POINT('Ctrl Pts',(168.912238263874,4.86812551320016,335.713671883818));
#44744=CARTESIAN_POINT('Ctrl Pts',(168.904481154099,4.88422240714451,335.577541808052));
#44745=CARTESIAN_POINT('Ctrl Pts',(168.896719899173,4.90032790275431,335.441338988725));
#44746=CARTESIAN_POINT('Ctrl Pts',(168.888958644246,4.9107190493142,335.304570049732));
#44747=CARTESIAN_POINT('Ctrl Pts',(168.88119738932,4.91538837570153,335.167750345807));
#44748=CARTESIAN_POINT('Ctrl Pts',(168.873423718916,4.92006517148935,335.030711774945));
#44749=CARTESIAN_POINT('Ctrl Pts',(168.865650048511,4.9190018596383,334.893622667941));
#44750=CARTESIAN_POINT('Ctrl Pts',(168.857876378106,4.91224311276248,334.756996576943));
#44751=CARTESIAN_POINT('Ctrl Pts',(168.850464573929,4.90579898717977,334.62673046335));
#44752=CARTESIAN_POINT('Ctrl Pts',(168.843052769752,4.89417776439534,334.496885515713));
#44753=CARTESIAN_POINT('Ctrl Pts',(168.835640965575,4.8774614936528,334.3678983939));
#44754=CARTESIAN_POINT('Ctrl Pts',(168.827865886797,4.85992590868598,334.232589229014));
#44755=CARTESIAN_POINT('Ctrl Pts',(168.820090808018,4.83672778459249,334.097796503387));
#44756=CARTESIAN_POINT('Ctrl Pts',(168.81231572924,4.80790524447894,333.96403174633));
#44757=CARTESIAN_POINT('Ctrl Pts',(168.804550218191,4.77911817233594,333.830431595322));
#44758=CARTESIAN_POINT('Ctrl Pts',(168.796784707142,4.74472053692603,333.697857274387));
#44759=CARTESIAN_POINT('Ctrl Pts',(168.789019196093,4.70480216751732,333.566814866452));
#44760=CARTESIAN_POINT('Ctrl Pts',(168.78126138457,4.6649233772881,333.435902387445));
#44761=CARTESIAN_POINT('Ctrl Pts',(168.773503573048,4.61953485944662,333.30651917025));
#44762=CARTESIAN_POINT('Ctrl Pts',(168.765745761526,4.56877733250919,333.179160427591));
#44763=CARTESIAN_POINT('Ctrl Pts',(168.757993788003,4.51805800222039,333.051897526425));
#44764=CARTESIAN_POINT('Ctrl Pts',(168.75024181448,4.46197784908123,332.926656429017));
#44765=CARTESIAN_POINT('Ctrl Pts',(168.742489840957,4.40072708599791,332.803916172578));
#44766=CARTESIAN_POINT('Ctrl Pts',(168.734741150399,4.33950226264913,332.681227896711));
#44767=CARTESIAN_POINT('Ctrl Pts',(168.726992459842,4.27311135879626,332.561038704339));
#44768=CARTESIAN_POINT('Ctrl Pts',(168.719243769284,4.20179219171555,332.443806454875));
#44769=CARTESIAN_POINT('Ctrl Pts',(168.711496690906,4.1304878631832,332.32659859656));
#44770=CARTESIAN_POINT('Ctrl Pts',(168.703749612528,4.0542575139732,332.212346791169));
#44771=CARTESIAN_POINT('Ctrl Pts',(168.696002534151,3.97338407830348,332.10148278791));
#44772=CARTESIAN_POINT('Ctrl Pts',(168.688255390845,3.89250996483651,331.990617855503));
#44773=CARTESIAN_POINT('Ctrl Pts',(168.680508247539,3.80699291765138,331.883141097643));
#44774=CARTESIAN_POINT('Ctrl Pts',(168.672761104233,3.71715797887775,331.779453521129));
#44775=CARTESIAN_POINT('Ctrl Pts',(168.665012219205,3.62730284330266,331.675742633447));
#44776=CARTESIAN_POINT('Ctrl Pts',(168.657263334177,3.53312814034821,331.575822917634));
#44777=CARTESIAN_POINT('Ctrl Pts',(168.649514449149,3.43499752499764,331.480060360495));
#44778=CARTESIAN_POINT('Ctrl Pts',(168.641757339374,3.33676275279803,331.384196159988));
#44779=CARTESIAN_POINT('Ctrl Pts',(168.634000229599,3.23456396079939,331.292498205864));
#44780=CARTESIAN_POINT('Ctrl Pts',(168.626243119825,3.12880022883224,331.205294189195));
#44781=CARTESIAN_POINT('Ctrl Pts',(168.618481864899,3.02297998010843,331.118043573487));
#44782=CARTESIAN_POINT('Ctrl Pts',(168.610720609972,2.91359130711932,331.03529191597));
#44783=CARTESIAN_POINT('Ctrl Pts',(168.602959355046,2.80106353960211,330.957324387289));
#44784=CARTESIAN_POINT('Ctrl Pts',(168.595185684642,2.68835576432956,330.87923213597));
#44785=CARTESIAN_POINT('Ctrl Pts',(168.587412014237,2.57249919052745,330.80593951562));
#44786=CARTESIAN_POINT('Ctrl Pts',(168.579638343832,2.45394985006524,330.737686872617));
#44787=CARTESIAN_POINT('Ctrl Pts',(168.572226539655,2.34091900992311,330.672611406566));
#44788=CARTESIAN_POINT('Ctrl Pts',(168.564814735478,2.22544071286094,330.612117389065));
#44789=CARTESIAN_POINT('Ctrl Pts',(168.557402931301,2.107926557031,330.556372124867));
#44790=CARTESIAN_POINT('Ctrl Pts',(168.549627852523,1.984652682367,330.497894619213));
#44791=CARTESIAN_POINT('Ctrl Pts',(168.541852773744,1.8587487676556,330.444458338431));
#44792=CARTESIAN_POINT('Ctrl Pts',(168.534077694966,1.73066559940786,330.396308041851));
#44793=CARTESIAN_POINT('Ctrl Pts',(168.526312183917,1.60274004565279,330.348216997276));
#44794=CARTESIAN_POINT('Ctrl Pts',(168.518546672868,1.47264093657317,330.305399130563));
#44795=CARTESIAN_POINT('Ctrl Pts',(168.510781161819,1.34084245987025,330.268052772874));
#44796=CARTESIAN_POINT('Ctrl Pts',(168.503023350296,1.20917466174083,330.230743444207));
#44797=CARTESIAN_POINT('Ctrl Pts',(168.495265538774,1.07581122273547,330.19889493435));
#44798=CARTESIAN_POINT('Ctrl Pts',(168.487507727252,0.941244728661796,330.17265689812));
#44799=CARTESIAN_POINT('Ctrl Pts',(168.479755753729,0.806779500142261,330.146438606845));
#44800=CARTESIAN_POINT('Ctrl Pts',(168.472003780206,0.6711134006884,330.125822459897));
#44801=CARTESIAN_POINT('Ctrl Pts',(168.464251806683,0.534752198028195,330.110907737708));
#44802=CARTESIAN_POINT('Ctrl Pts',(168.456503116125,0.398448744418182,330.095999331913));
#44803=CARTESIAN_POINT('Ctrl Pts',(168.448754425568,0.261451160844527,330.086787590903));
#44804=CARTESIAN_POINT('Ctrl Pts',(168.44100573501,0.124273167629879,330.083320303059));
#44805=CARTESIAN_POINT('Ctrl Pts',(168.433258656632,-0.012876284557547,
330.079853736614));
#44806=CARTESIAN_POINT('Ctrl Pts',(168.425511578255,-0.150205681220574,
330.082129255903));
#44807=CARTESIAN_POINT('Ctrl Pts',(168.417764499877,-0.287198843298569,
330.090142579778));
#44808=CARTESIAN_POINT('Ctrl Pts',(168.410017356571,-0.42419315351114,330.098155970813));
#44809=CARTESIAN_POINT('Ctrl Pts',(168.402270213265,-0.560850833310727,
330.111907239524));
#44810=CARTESIAN_POINT('Ctrl Pts',(168.394523069959,-0.696658768576774,
330.131340058839));
#44811=CARTESIAN_POINT('Ctrl Pts',(168.386774184931,-0.832497236349791,
330.150777247065));
#44812=CARTESIAN_POINT('Ctrl Pts',(168.379025299903,-0.967485192582247,
330.17589847229));
#44813=CARTESIAN_POINT('Ctrl Pts',(168.371276414875,-1.10111807658499,330.206595985741));
#44814=CARTESIAN_POINT('Ctrl Pts',(168.3635193051,-1.23489279991167,330.237326081849));
#44815=CARTESIAN_POINT('Ctrl Pts',(168.355762195326,-1.36730919634014,330.273644201753));
#44816=CARTESIAN_POINT('Ctrl Pts',(168.348005085551,-1.49787573846262,330.315392083149));
#44817=CARTESIAN_POINT('Ctrl Pts',(168.340243830625,-1.62851205117045,330.357162273278));
#44818=CARTESIAN_POINT('Ctrl Pts',(168.332482575698,-1.75729617308055,330.404367871928));
#44819=CARTESIAN_POINT('Ctrl Pts',(168.324721320772,-1.88375596315883,330.456802168762));
#44820=CARTESIAN_POINT('Ctrl Pts',(168.316947650368,-2.01041804768812,330.509320343383));
#44821=CARTESIAN_POINT('Ctrl Pts',(168.309173979963,-2.13474801570329,330.567083765584));
#44822=CARTESIAN_POINT('Ctrl Pts',(168.301400309558,-2.25629696979506,330.629839013653));
#44823=CARTESIAN_POINT('Ctrl Pts',(168.293988505381,-2.37218779083118,330.689672989826));
#44824=CARTESIAN_POINT('Ctrl Pts',(168.286576701204,-2.48555043341456,330.754044369432));
#44825=CARTESIAN_POINT('Ctrl Pts',(168.279164897027,-2.59602146803341,330.822697569003));
#44826=CARTESIAN_POINT('Ctrl Pts',(168.271389818249,-2.71190701713495,330.894715666393));
#44827=CARTESIAN_POINT('Ctrl Pts',(168.26361473947,-2.82497655827244,330.971673516613));
#44828=CARTESIAN_POINT('Ctrl Pts',(168.255839660692,-2.93478032165797,331.053324496984));
#44829=CARTESIAN_POINT('Ctrl Pts',(168.248074149643,-3.04444896452226,331.134875000625));
#44830=CARTESIAN_POINT('Ctrl Pts',(168.240308638594,-3.15085951512902,331.221106912426));
#44831=CARTESIAN_POINT('Ctrl Pts',(168.232543127545,-3.25358858239829,331.311728806204));
#44832=CARTESIAN_POINT('Ctrl Pts',(168.224785316022,-3.35621579349819,331.40226084811));
#44833=CARTESIAN_POINT('Ctrl Pts',(168.2170275045,-3.45516849413348,331.497173953003));
#44834=CARTESIAN_POINT('Ctrl Pts',(168.209269692978,-3.55005426993032,331.596134881778));
#44835=CARTESIAN_POINT('Ctrl Pts',(168.201517719455,-3.64486864117196,331.695021339316));
#44836=CARTESIAN_POINT('Ctrl Pts',(168.193765745932,-3.73562190990028,331.797949276588));
#44837=CARTESIAN_POINT('Ctrl Pts',(168.186013772409,-3.82195688914436,331.904547109061));
#44838=CARTESIAN_POINT('Ctrl Pts',(168.178265081851,-3.90825530547336,332.011099797289));
#44839=CARTESIAN_POINT('Ctrl Pts',(168.170516391294,-3.99013890840325,332.121318986401));
#44840=CARTESIAN_POINT('Ctrl Pts',(168.162767700736,-4.06728950812258,332.234798539054));
#44841=CARTESIAN_POINT('Ctrl Pts',(168.155020622358,-4.14442405601523,332.348254481339));
#44842=CARTESIAN_POINT('Ctrl Pts',(168.14727354398,-4.21682733979214,332.464969114844));
#44843=CARTESIAN_POINT('Ctrl Pts',(168.139526465603,-4.28422362545514,332.584506056809));
#44844=CARTESIAN_POINT('Ctrl Pts',(168.131779322297,-4.3516204759639,332.704044000609));
#44845=CARTESIAN_POINT('Ctrl Pts',(168.124032178991,-4.41401005268988,332.826403959564));
#44846=CARTESIAN_POINT('Ctrl Pts',(168.116285035685,-4.4711620467765,332.951123963251));
#44847=CARTESIAN_POINT('Ctrl Pts',(168.108536150657,-4.52832688984473,333.075872006642));
#44848=CARTESIAN_POINT('Ctrl Pts',(168.100787265629,-4.58025164433972,333.202980795305));
#44849=CARTESIAN_POINT('Ctrl Pts',(168.093038380601,-4.62675387176355,333.331967724347));
#44850=CARTESIAN_POINT('Ctrl Pts',(168.085281270826,-4.67330545713206,333.461091561448));
#44851=CARTESIAN_POINT('Ctrl Pts',(168.077524161051,-4.71442288545073,333.592097152797));
#44852=CARTESIAN_POINT('Ctrl Pts',(168.069767051276,-4.74997324918173,333.7244855177));
#44853=CARTESIAN_POINT('Ctrl Pts',(168.06200579635,-4.78554260989044,333.856944626711));
#44854=CARTESIAN_POINT('Ctrl Pts',(168.054244541424,-4.81553889289518,333.990787600401));
#44855=CARTESIAN_POINT('Ctrl Pts',(168.046483286498,-4.83988042272313,334.125505542475));
#44856=CARTESIAN_POINT('Ctrl Pts',(168.038709616093,-4.86426089106589,334.260438989353));
#44857=CARTESIAN_POINT('Ctrl Pts',(168.030935945688,-4.88296847675385,334.396249814137));
#44858=CARTESIAN_POINT('Ctrl Pts',(168.023162275284,-4.89597336336474,334.532423388392));
#44859=CARTESIAN_POINT('Ctrl Pts',(168.015750471107,-4.90837286937501,334.662258050002));
#44860=CARTESIAN_POINT('Ctrl Pts',(168.00833866693,-4.91558863361006,334.792422161769));
#44861=CARTESIAN_POINT('Ctrl Pts',(168.000926862752,-4.91763890909733,334.922471797183));
#44862=CARTESIAN_POINT('Ctrl Pts',(167.999463324665,-4.91804375738991,334.948151454953));
#44863=CARTESIAN_POINT('Ctrl Pts',(167.997999786577,-4.91824746069164,334.973834292198));
#44864=CARTESIAN_POINT('Ctrl Pts',(167.99653624849,-4.91824997640721,334.999518263041));
#44865=CARTESIAN_POINT('',(171.496536248527,-4.91824971188752,334.998316545704));
#44866=CARTESIAN_POINT('Ctrl Pts',(171.49653624849,-4.91824971188774,334.998316546354));
#44867=CARTESIAN_POINT('Ctrl Pts',(171.488603707819,-4.91829790514505,335.139114289432));
#44868=CARTESIAN_POINT('Ctrl Pts',(171.480671167148,-4.91229569124257,335.279865940706));
#44869=CARTESIAN_POINT('Ctrl Pts',(171.472738626477,-4.90028124430733,335.420031890682));
#44870=CARTESIAN_POINT('Ctrl Pts',(171.464801568283,-4.88825995523447,335.560277664117));
#44871=CARTESIAN_POINT('Ctrl Pts',(171.456864510089,-4.87021964015133,335.699936708887));
#44872=CARTESIAN_POINT('Ctrl Pts',(171.448927451896,-4.84625020104069,335.838476029123));
#44873=CARTESIAN_POINT('Ctrl Pts',(171.440984525747,-4.8222630410576,335.977117773016));
#44874=CARTESIAN_POINT('Ctrl Pts',(171.433041599598,-4.7923380824285,336.114637784287));
#44875=CARTESIAN_POINT('Ctrl Pts',(171.425098673449,-4.75661600854616,336.250514777898));
#44876=CARTESIAN_POINT('Ctrl Pts',(171.417142776465,-4.72083560035479,336.386613659258));
#44877=CARTESIAN_POINT('Ctrl Pts',(171.409186879482,-4.67923925564794,336.521063810024));
#44878=CARTESIAN_POINT('Ctrl Pts',(171.401230982498,-4.63201741025085,336.65335954155));
#44879=CARTESIAN_POINT('Ctrl Pts',(171.393267950449,-4.58475321500933,336.785773919511));
#44880=CARTESIAN_POINT('Ctrl Pts',(171.385304918399,-4.53185359555243,336.916029689037));
#44881=CARTESIAN_POINT('Ctrl Pts',(171.377341886349,-4.47355635531153,337.04364297233));
#44882=CARTESIAN_POINT('Ctrl Pts',(171.369364296103,-4.41515253473246,337.171489561124));
#44883=CARTESIAN_POINT('Ctrl Pts',(171.361386705857,-4.35133153930368,337.296683686043));
#44884=CARTESIAN_POINT('Ctrl Pts',(171.353409115612,-4.28237670327676,337.418766800196));
#44885=CARTESIAN_POINT('Ctrl Pts',(171.348867168421,-4.2431180782887,337.488273385551));
#44886=CARTESIAN_POINT('Ctrl Pts',(171.34432522123,-4.20219613096733,337.556772086059));
#44887=CARTESIAN_POINT('Ctrl Pts',(171.33978327404,-4.15966913126676,337.624182878705));
#44888=CARTESIAN_POINT('Ctrl Pts',(171.332008195261,-4.08686978794295,337.739579249765));
#44889=CARTESIAN_POINT('Ctrl Pts',(171.324233116483,-4.00914982865405,337.852126305575));
#44890=CARTESIAN_POINT('Ctrl Pts',(171.316458037705,-3.92675890896485,337.961375952723));
#44891=CARTESIAN_POINT('Ctrl Pts',(171.308692526655,-3.84446937654756,338.070491161225));
#44892=CARTESIAN_POINT('Ctrl Pts',(171.300927015606,-3.75752055353427,338.176316725574));
#44893=CARTESIAN_POINT('Ctrl Pts',(171.293161504557,-3.66620671976475,338.278431233144));
#44894=CARTESIAN_POINT('Ctrl Pts',(171.285403693035,-3.57498342392752,338.380444493881));
#44895=CARTESIAN_POINT('Ctrl Pts',(171.277645881513,-3.47940398901383,338.478753730808));
#44896=CARTESIAN_POINT('Ctrl Pts',(171.269888069991,-3.3798042975632,338.57296878977));
#44897=CARTESIAN_POINT('Ctrl Pts',(171.262136096468,-3.2802795580389,338.667112948914));
#44898=CARTESIAN_POINT('Ctrl Pts',(171.254384122945,-3.17674086664551,338.757168795145));
#44899=CARTESIAN_POINT('Ctrl Pts',(171.246632149422,-3.06956221249043,338.842781659963));
#44900=CARTESIAN_POINT('Ctrl Pts',(171.238883458864,-2.9624289485588,338.928358267683));
#44901=CARTESIAN_POINT('Ctrl Pts',(171.231134768307,-2.85165909261949,339.009495392925));
#44902=CARTESIAN_POINT('Ctrl Pts',(171.223386077749,-2.7376609223481,339.085877596888));
#44903=CARTESIAN_POINT('Ctrl Pts',(171.215638999371,-2.62368647034811,339.162243908895));
#44904=CARTESIAN_POINT('Ctrl Pts',(171.207891920993,-2.50648536454885,339.233857049974));
#44905=CARTESIAN_POINT('Ctrl Pts',(171.200144842615,-2.38649584053138,339.300444240497));
#44906=CARTESIAN_POINT('Ctrl Pts',(171.19239769931,-2.26650531088626,339.367031989085));
#44907=CARTESIAN_POINT('Ctrl Pts',(171.184650556004,-2.1437266581851,339.428593513435));
#44908=CARTESIAN_POINT('Ctrl Pts',(171.176903412698,-2.01862339820749,339.484901630884));
#44909=CARTESIAN_POINT('Ctrl Pts',(171.16915452767,-1.89349201236096,339.541222407595));
#44910=CARTESIAN_POINT('Ctrl Pts',(171.161405642642,-1.76603533564503,339.592287266795));
#44911=CARTESIAN_POINT('Ctrl Pts',(171.153656757614,-1.63673719444059,339.637917034492));
#44912=CARTESIAN_POINT('Ctrl Pts',(171.145899647839,-1.50730181485311,339.683595234096));
#44913=CARTESIAN_POINT('Ctrl Pts',(171.138142538064,-1.37602143555847,339.723826688068));
#44914=CARTESIAN_POINT('Ctrl Pts',(171.13038542829,-1.24339592375126,339.758481862874));
#44915=CARTESIAN_POINT('Ctrl Pts',(171.122624173363,-1.1106995411112,339.793155556297));
#44916=CARTESIAN_POINT('Ctrl Pts',(171.114862918437,-0.976656975481078,
339.822246950202));
#44917=CARTESIAN_POINT('Ctrl Pts',(171.107101663511,-0.841777663316359,
339.845677808939));
#44918=CARTESIAN_POINT('Ctrl Pts',(171.099327993106,-0.706682588209115,
339.869146149413));
#44919=CARTESIAN_POINT('Ctrl Pts',(171.091554322702,-0.570748479577714,
339.886935809376));
#44920=CARTESIAN_POINT('Ctrl Pts',(171.083780652297,-0.434490155547044,
339.899020449767));
#44921=CARTESIAN_POINT('Ctrl Pts',(171.07636884812,-0.304574689282362,339.91054254724));
#44922=CARTESIAN_POINT('Ctrl Pts',(171.068957043943,-0.174364800245908,
339.916878795561));
#44923=CARTESIAN_POINT('Ctrl Pts',(171.061545239766,-0.0443042815042223,
339.91805044638));
#44924=CARTESIAN_POINT('Ctrl Pts',(171.053770160987,0.092130890691618,339.919279523296));
#44925=CARTESIAN_POINT('Ctrl Pts',(171.045995082209,0.228832840549928,339.914828821295));
#44926=CARTESIAN_POINT('Ctrl Pts',(171.038220003431,0.365289653809286,339.904665792011));
#44927=CARTESIAN_POINT('Ctrl Pts',(171.030454492382,0.501578548272557,339.894515268981));
#44928=CARTESIAN_POINT('Ctrl Pts',(171.022688981333,0.637622520277791,339.878666433876));
#44929=CARTESIAN_POINT('Ctrl Pts',(171.014923470284,0.772907943249615,339.857138702339));
#44930=CARTESIAN_POINT('Ctrl Pts',(171.007165658761,0.908059230331103,339.835632315611));
#44931=CARTESIAN_POINT('Ctrl Pts',(170.999407847239,1.04245308157693,339.808458298778));
#44932=CARTESIAN_POINT('Ctrl Pts',(170.991650035717,1.17557964272247,339.775687967834));
#44933=CARTESIAN_POINT('Ctrl Pts',(170.983898062194,1.30860602190894,339.742942297604));
#44934=CARTESIAN_POINT('Ctrl Pts',(170.976146088671,1.44036663122452,339.704608788909));
#44935=CARTESIAN_POINT('Ctrl Pts',(170.968394115148,1.57036083539402,339.660810005692));
#44936=CARTESIAN_POINT('Ctrl Pts',(170.96064542459,1.7002999869407,339.617029771286));
#44937=CARTESIAN_POINT('Ctrl Pts',(170.952896734033,1.82847385156352,339.567788990371));
#44938=CARTESIAN_POINT('Ctrl Pts',(170.945148043475,1.95439622756584,339.51326029032));
#44939=CARTESIAN_POINT('Ctrl Pts',(170.937400965097,2.08029240436603,339.45874293542));
#44940=CARTESIAN_POINT('Ctrl Pts',(170.929653886719,2.2039376658452,339.398940004977));
#44941=CARTESIAN_POINT('Ctrl Pts',(170.921906808342,2.32486547137441,339.33407240393));
#44942=CARTESIAN_POINT('Ctrl Pts',(170.914159665036,2.44579429039497,339.269204259231));
#44943=CARTESIAN_POINT('Ctrl Pts',(170.90641252173,2.56400526359214,339.199271544032));
#44944=CARTESIAN_POINT('Ctrl Pts',(170.898665378424,2.67905651323399,339.124541097067));
#44945=CARTESIAN_POINT('Ctrl Pts',(170.890916493396,2.79413362883978,339.049793849111));
#44946=CARTESIAN_POINT('Ctrl Pts',(170.883167608368,2.90604927959664,338.970246935906));
#44947=CARTESIAN_POINT('Ctrl Pts',(170.87541872334,3.01439096805303,338.886210256049));
#44948=CARTESIAN_POINT('Ctrl Pts',(170.867661613565,3.1228476514967,338.802084378791));
#44949=CARTESIAN_POINT('Ctrl Pts',(170.85990450379,3.22772248554509,338.713459455323));
#44950=CARTESIAN_POINT('Ctrl Pts',(170.852147394016,3.32863603586379,338.620685736604));
#44951=CARTESIAN_POINT('Ctrl Pts',(170.84438613909,3.42960351115714,338.527862442576));
#44952=CARTESIAN_POINT('Ctrl Pts',(170.836624884163,3.52660520855334,338.430886211971));
#44953=CARTESIAN_POINT('Ctrl Pts',(170.828863629237,3.61929965272588,338.330143102973));
#44954=CARTESIAN_POINT('Ctrl Pts',(170.821089958833,3.71214237780011,338.229238837832));
#44955=CARTESIAN_POINT('Ctrl Pts',(170.813316288428,3.80066382846647,338.124555951633));
#44956=CARTESIAN_POINT('Ctrl Pts',(170.805542618023,3.88456325801952,338.016513112344));
#44957=CARTESIAN_POINT('Ctrl Pts',(170.798130813846,3.96455714894188,337.913499693218));
#44958=CARTESIAN_POINT('Ctrl Pts',(170.790719009669,4.04034947773265,337.807432327161));
#44959=CARTESIAN_POINT('Ctrl Pts',(170.783307205492,4.11171795346504,337.698695709719));
#44960=CARTESIAN_POINT('Ctrl Pts',(170.775532126714,4.18658441078877,337.584629586746));
#44961=CARTESIAN_POINT('Ctrl Pts',(170.767757047935,4.25681898954915,337.467265470468));
#44962=CARTESIAN_POINT('Ctrl Pts',(170.759981969157,4.32211729294997,337.347016226719));
#44963=CARTESIAN_POINT('Ctrl Pts',(170.752216458108,4.38733524263126,337.22691495732));
#44964=CARTESIAN_POINT('Ctrl Pts',(170.744450947059,4.44762881852518,337.103935964809));
#44965=CARTESIAN_POINT('Ctrl Pts',(170.73668543601,4.50273639484788,336.978521675649));
#44966=CARTESIAN_POINT('Ctrl Pts',(170.728927624487,4.55778933184837,336.853231735121));
#44967=CARTESIAN_POINT('Ctrl Pts',(170.721169812965,4.6076663457877,336.725511658688));
#44968=CARTESIAN_POINT('Ctrl Pts',(170.713412001443,4.65215149640935,336.595828786855));
#44969=CARTESIAN_POINT('Ctrl Pts',(170.70566002792,4.69660317054424,336.466243505497));
#44970=CARTESIAN_POINT('Ctrl Pts',(170.697908054397,4.73567093139604,336.334698737004));
#44971=CARTESIAN_POINT('Ctrl Pts',(170.690156080874,4.76918692312449,336.201681802641));
#44972=CARTESIAN_POINT('Ctrl Pts',(170.682407390316,4.80268872081063,336.068721201028));
#44973=CARTESIAN_POINT('Ctrl Pts',(170.674658699759,4.83064333039579,335.934290051809));
#44974=CARTESIAN_POINT('Ctrl Pts',(170.666910009201,4.85293280628301,335.798890630939));
#44975=CARTESIAN_POINT('Ctrl Pts',(170.659162930823,4.87521764465859,335.663519381049));
#44976=CARTESIAN_POINT('Ctrl Pts',(170.651415852446,4.89183963035951,335.527180645661));
#44977=CARTESIAN_POINT('Ctrl Pts',(170.643668774068,4.90273205515801,335.390386293082));
#44978=CARTESIAN_POINT('Ctrl Pts',(170.635921630762,4.91362457124555,335.253590794034));
#44979=CARTESIAN_POINT('Ctrl Pts',(170.628174487456,4.91878739962699,335.116340059819));
#44980=CARTESIAN_POINT('Ctrl Pts',(170.62042734415,4.9182058052906,334.979150076599));
#44981=CARTESIAN_POINT('Ctrl Pts',(170.612678459122,4.91762408019946,334.841929250158));
#44982=CARTESIAN_POINT('Ctrl Pts',(170.604929574094,4.91129536416978,334.704769592685));
#44983=CARTESIAN_POINT('Ctrl Pts',(170.597180689066,4.8992570315022,334.568185685999));
#44984=CARTESIAN_POINT('Ctrl Pts',(170.589423579291,4.88720592122396,334.431456807743));
#44985=CARTESIAN_POINT('Ctrl Pts',(170.581666469517,4.86943312277005,334.295305291));
#44986=CARTESIAN_POINT('Ctrl Pts',(170.573909359742,4.84602783595446,334.160239751087));
#44987=CARTESIAN_POINT('Ctrl Pts',(170.566148104816,4.82261004210197,334.025102036468));
#44988=CARTESIAN_POINT('Ctrl Pts',(170.55838684989,4.79355384530654,333.891051836812));
#44989=CARTESIAN_POINT('Ctrl Pts',(170.550625594963,4.7589990982376,333.758585224241));
#44990=CARTESIAN_POINT('Ctrl Pts',(170.542851924559,4.7243890748347,333.62590670826));
#44991=CARTESIAN_POINT('Ctrl Pts',(170.535078254154,4.68426303883409,333.494817215447));
#44992=CARTESIAN_POINT('Ctrl Pts',(170.527304583749,4.63881030576238,333.365796215384));
#44993=CARTESIAN_POINT('Ctrl Pts',(170.519892779572,4.5954734083504,333.242781173914));
#44994=CARTESIAN_POINT('Ctrl Pts',(170.512480975395,4.54729467545668,333.121646649758));
#44995=CARTESIAN_POINT('Ctrl Pts',(170.505069171218,4.49447731139666,333.002787752931));
#44996=CARTESIAN_POINT('Ctrl Pts',(170.49729409244,4.43907121098931,332.878103227509));
#44997=CARTESIAN_POINT('Ctrl Pts',(170.489519013661,4.37838518238395,332.755529014171));
#44998=CARTESIAN_POINT('Ctrl Pts',(170.481743934883,4.3126016866966,332.63554451207));
#44999=CARTESIAN_POINT('Ctrl Pts',(170.473978423834,4.2468991417886,332.515707658538));
#45000=CARTESIAN_POINT('Ctrl Pts',(170.466212912785,4.17611179690491,332.398454514881));
#45001=CARTESIAN_POINT('Ctrl Pts',(170.458447401736,4.10047011717344,332.284244510147));
#45002=CARTESIAN_POINT('Ctrl Pts',(170.450689590214,4.02490343638772,332.170147744965));
#45003=CARTESIAN_POINT('Ctrl Pts',(170.442931778692,3.94449221351208,332.05908843793));
#45004=CARTESIAN_POINT('Ctrl Pts',(170.435173967169,3.85951258748423,331.951501082573));
#45005=CARTESIAN_POINT('Ctrl Pts',(170.427421993646,3.77459691131963,331.843994690113));
#45006=CARTESIAN_POINT('Ctrl Pts',(170.419670020123,3.68511991621315,331.739955354269));
#45007=CARTESIAN_POINT('Ctrl Pts',(170.4119180466,3.59140056458649,331.639787946098));
#45008=CARTESIAN_POINT('Ctrl Pts',(170.404169356043,3.49772090316113,331.539662958884));
#45009=CARTESIAN_POINT('Ctrl Pts',(170.396420665485,3.39980272510159,331.443406922798));
#45010=CARTESIAN_POINT('Ctrl Pts',(170.388671974927,3.29800457784401,331.35139083115));
#45011=CARTESIAN_POINT('Ctrl Pts',(170.38092489655,3.19622761054127,331.259393884217));
#45012=CARTESIAN_POINT('Ctrl Pts',(170.373177818172,3.09057256952619,331.171635388993));
#45013=CARTESIAN_POINT('Ctrl Pts',(170.365430739794,2.9814337961282,331.088448443162));
#45014=CARTESIAN_POINT('Ctrl Pts',(170.357683596488,2.87229410804189,331.005260800143));
#45015=CARTESIAN_POINT('Ctrl Pts',(170.349936453182,2.75967094020464,330.926645019884));
#45016=CARTESIAN_POINT('Ctrl Pts',(170.342189309877,2.64399022242767,330.852892723089));
#45017=CARTESIAN_POINT('Ctrl Pts',(170.334440424849,2.52828349716938,330.779123845212));
#45018=CARTESIAN_POINT('Ctrl Pts',(170.32669153982,2.40951818364181,330.710220836661));
#45019=CARTESIAN_POINT('Ctrl Pts',(170.318942654792,2.28814723005367,330.646430738337));
#45020=CARTESIAN_POINT('Ctrl Pts',(170.311185545018,2.16664745208172,330.582572932544));
#45021=CARTESIAN_POINT('Ctrl Pts',(170.303428435243,2.04253685594054,330.523839059847));
#45022=CARTESIAN_POINT('Ctrl Pts',(170.295671325468,1.91629141823982,330.470429351155));
#45023=CARTESIAN_POINT('Ctrl Pts',(170.287910070542,1.78997851901345,330.416991102021));
#45024=CARTESIAN_POINT('Ctrl Pts',(170.280148815616,1.66152887095638,330.368882822961));
#45025=CARTESIAN_POINT('Ctrl Pts',(170.27238756069,1.53143531400347,330.326255361969));
#45026=CARTESIAN_POINT('Ctrl Pts',(170.264613890285,1.40113364975705,330.283559710932));
#45027=CARTESIAN_POINT('Ctrl Pts',(170.25684021988,1.26918319806779,330.246362504182));
#45028=CARTESIAN_POINT('Ctrl Pts',(170.249066549476,1.13608960462986,330.214764010756));
#45029=CARTESIAN_POINT('Ctrl Pts',(170.241654745299,1.00919154998876,330.184636434802));
#45030=CARTESIAN_POINT('Ctrl Pts',(170.234242941122,0.881254667472015,330.159598117423));
#45031=CARTESIAN_POINT('Ctrl Pts',(170.226831136945,0.752721179036315,330.139691996475));
#45032=CARTESIAN_POINT('Ctrl Pts',(170.219056058166,0.617887881449027,330.118810217242));
#45033=CARTESIAN_POINT('Ctrl Pts',(170.211280979388,0.481971918204775,330.103510453232));
#45034=CARTESIAN_POINT('Ctrl Pts',(170.203505900609,0.345475166458746,330.093898699389));
#45035=CARTESIAN_POINT('Ctrl Pts',(170.19574038956,0.209146382655525,330.084298773421));
#45036=CARTESIAN_POINT('Ctrl Pts',(170.187974878511,0.0722386185744949,
330.080372957898));
#45037=CARTESIAN_POINT('Ctrl Pts',(170.180209367462,-0.0647370641909145,
330.082176073199));
#45038=CARTESIAN_POINT('Ctrl Pts',(170.17245155594,-0.201576935167323,330.083977400705));
#45039=CARTESIAN_POINT('Ctrl Pts',(170.164693744418,-0.338484202491844,
330.091496349901));
#45040=CARTESIAN_POINT('Ctrl Pts',(170.156935932896,-0.47494405665984,330.104735839044));
#45041=CARTESIAN_POINT('Ctrl Pts',(170.149183959373,-0.611301220462109,
330.117965365051));
#45042=CARTESIAN_POINT('Ctrl Pts',(170.14143198585,-0.747211253796988,330.136906824743));
#45043=CARTESIAN_POINT('Ctrl Pts',(170.133680012327,-0.882161083087291,
330.161511094775));
#45044=CARTESIAN_POINT('Ctrl Pts',(170.125931321769,-1.01705376104355,330.186104944883));
#45045=CARTESIAN_POINT('Ctrl Pts',(170.118182631211,-1.15098666001239,330.21635676551));
#45046=CARTESIAN_POINT('Ctrl Pts',(170.110433940654,-1.28345377321459,330.252165812234));
#45047=CARTESIAN_POINT('Ctrl Pts',(170.102686862276,-1.41589332552739,330.287967408586));
#45048=CARTESIAN_POINT('Ctrl Pts',(170.094939783898,-1.54686732158466,330.32932382928));
#45049=CARTESIAN_POINT('Ctrl Pts',(170.08719270552,-1.67588225171733,330.376083722549));
#45050=CARTESIAN_POINT('Ctrl Pts',(170.079445562214,-1.80489826311936,330.42284400771));
#45051=CARTESIAN_POINT('Ctrl Pts',(170.071698418909,-1.9319548083658,330.475007722583));
#45052=CARTESIAN_POINT('Ctrl Pts',(170.063951275603,-2.05657616232355,330.5323745064));
#45053=CARTESIAN_POINT('Ctrl Pts',(170.056202390575,-2.18122553380696,330.589754187488));
#45054=CARTESIAN_POINT('Ctrl Pts',(170.048453505547,-2.30343826958043,330.652339101798));
#45055=CARTESIAN_POINT('Ctrl Pts',(170.040704620519,-2.42276151141272,330.719882043528));
#45056=CARTESIAN_POINT('Ctrl Pts',(170.032947510744,-2.54221140416723,330.787496676033));
#45057=CARTESIAN_POINT('Ctrl Pts',(170.025190400969,-2.65876533578624,330.860079655447));
#45058=CARTESIAN_POINT('Ctrl Pts',(170.017433291194,-2.77199734957368,330.937339079316));
#45059=CARTESIAN_POINT('Ctrl Pts',(170.009672036268,-2.88528987092869,331.01463978815));
#45060=CARTESIAN_POINT('Ctrl Pts',(170.001910781342,-2.99525662413858,331.096621687301));
#45061=CARTESIAN_POINT('Ctrl Pts',(169.994149526416,-3.10150405393699,331.182951969661));
#45062=CARTESIAN_POINT('Ctrl Pts',(169.986375856011,-3.20792144499722,331.269420352338));
#45063=CARTESIAN_POINT('Ctrl Pts',(169.978602185607,-3.3106073304452,331.360250759255));
#45064=CARTESIAN_POINT('Ctrl Pts',(169.970828515202,-3.40920375800942,331.45507224349));
#45065=CARTESIAN_POINT('Ctrl Pts',(169.963416711025,-3.50321049815017,331.545479764822));
#45066=CARTESIAN_POINT('Ctrl Pts',(169.956004906848,-3.59349974155205,331.639514948513));
#45067=CARTESIAN_POINT('Ctrl Pts',(169.948593102671,-3.67979606917959,331.736829156825));
#45068=CARTESIAN_POINT('Ctrl Pts',(169.940888249857,-3.76950438942144,331.837990983791));
#45069=CARTESIAN_POINT('Ctrl Pts',(169.933183397044,-3.85519379095433,331.943030722558));
#45070=CARTESIAN_POINT('Ctrl Pts',(169.925478544231,-3.93650558769228,332.051592494147));
#45071=CARTESIAN_POINT('Ctrl Pts',(169.917785908505,-4.01768845356278,332.159982126344));
#45072=CARTESIAN_POINT('Ctrl Pts',(169.91009327278,-4.0945072985029,332.271882355992));
#45073=CARTESIAN_POINT('Ctrl Pts',(169.902400637055,-4.16664149157643,332.386901887955));
#45074=CARTESIAN_POINT('Ctrl Pts',(169.894715036249,-4.23870971788721,332.501816234487));
#45075=CARTESIAN_POINT('Ctrl Pts',(169.887029435444,-4.30610160079548,332.619843875871));
#45076=CARTESIAN_POINT('Ctrl Pts',(169.879343834638,-4.3685377832728,332.740561862184));
#45077=CARTESIAN_POINT('Ctrl Pts',(169.871663523159,-4.43093099638733,332.861196768867));
#45078=CARTESIAN_POINT('Ctrl Pts',(169.863983211681,-4.48837511010907,332.984517985316));
#45079=CARTESIAN_POINT('Ctrl Pts',(169.856302900202,-4.5406352564568,333.110075522588));
#45080=CARTESIAN_POINT('Ctrl Pts',(169.848626136853,-4.59287125979836,333.235575055116));
#45081=CARTESIAN_POINT('Ctrl Pts',(169.840949373505,-4.63992790790951,333.363308485592));
#45082=CARTESIAN_POINT('Ctrl Pts',(169.833272610157,-4.68161750597623,333.492803732012));
#45083=CARTESIAN_POINT('Ctrl Pts',(169.8255959283,-4.72330666149022,333.622297603785));
#45084=CARTESIAN_POINT('Ctrl Pts',(169.817919246444,-4.75962874628732,333.753552878788));
#45085=CARTESIAN_POINT('Ctrl Pts',(169.810242564587,-4.79044526993776,333.886080264009));
#45086=CARTESIAN_POINT('Ctrl Pts',(169.802566164899,-4.8212606608792,334.018602777981));
#45087=CARTESIAN_POINT('Ctrl Pts',(169.794889765211,-4.84657080862806,334.152396919398));
#45088=CARTESIAN_POINT('Ctrl Pts',(169.787213365523,-4.86628809491317,334.286961964685));
#45089=CARTESIAN_POINT('Ctrl Pts',(169.77953231574,-4.8860173252431,334.421608524786));
#45090=CARTESIAN_POINT('Ctrl Pts',(169.771851265956,-4.90014687278142,334.557026526107));
#45091=CARTESIAN_POINT('Ctrl Pts',(169.764170216173,-4.90864086521297,334.692708739367));
#45092=CARTESIAN_POINT('Ctrl Pts',(169.758292226945,-4.91514096577472,334.79654071682));
#45093=CARTESIAN_POINT('Ctrl Pts',(169.752414237718,-4.91834182617851,334.900527260846));
#45094=CARTESIAN_POINT('Ctrl Pts',(169.74653624849,-4.91824799493239,335.004441040815));
#45095=CARTESIAN_POINT('',(173.246536248458,-4.9182485732376,334.996253755704));
#45096=CARTESIAN_POINT('Ctrl Pts',(173.246536248458,-4.9182485732376,334.996253755704));
#45097=CARTESIAN_POINT('Ctrl Pts',(173.238884065945,-4.91835115497214,335.130927959976));
#45098=CARTESIAN_POINT('Ctrl Pts',(173.231231883431,-4.91291799432863,335.265810654158));
#45099=CARTESIAN_POINT('Ctrl Pts',(173.223579700918,-4.90192431480923,335.400401141834));
#45100=CARTESIAN_POINT('Ctrl Pts',(173.215935198301,-4.89094166878634,335.534856551561));
#45101=CARTESIAN_POINT('Ctrl Pts',(173.208290695685,-4.87440963568348,335.669019938917));
#45102=CARTESIAN_POINT('Ctrl Pts',(173.200646193069,-4.85235547248282,335.802389824939));
#45103=CARTESIAN_POINT('Ctrl Pts',(173.192669746678,-4.82934366134187,335.941550971119));
#45104=CARTESIAN_POINT('Ctrl Pts',(173.184693300287,-4.80031934116843,336.079847708487));
#45105=CARTESIAN_POINT('Ctrl Pts',(173.176716853896,-4.76537387231715,336.216714806163));
#45106=CARTESIAN_POINT('Ctrl Pts',(173.169081214905,-4.73192150876764,336.347734021528));
#45107=CARTESIAN_POINT('Ctrl Pts',(173.161445575915,-4.69304363311525,336.477442806396));
#45108=CARTESIAN_POINT('Ctrl Pts',(173.153809936924,-4.64887264541713,336.605355471287));
#45109=CARTESIAN_POINT('Ctrl Pts',(173.146175547409,-4.60470888574302,336.733247204888));
#45110=CARTESIAN_POINT('Ctrl Pts',(173.138541157894,-4.55525386766006,336.85934302168));
#45111=CARTESIAN_POINT('Ctrl Pts',(173.13090676838,-4.50068956887602,336.983173332594));
#45112=CARTESIAN_POINT('Ctrl Pts',(173.123271862838,-4.44612158196254,337.107012013489));
#45113=CARTESIAN_POINT('Ctrl Pts',(173.115636957297,-4.38644379067124,337.228584515003));
#45114=CARTESIAN_POINT('Ctrl Pts',(173.108002051756,-4.3218856996806,337.347442664134));
#45115=CARTESIAN_POINT('Ctrl Pts',(173.100364864461,-4.2573083149754,337.466336334997));
#45116=CARTESIAN_POINT('Ctrl Pts',(173.092727677166,-4.18784792324968,337.582513686413));
#45117=CARTESIAN_POINT('Ctrl Pts',(173.08509048987,-4.11377892183343,337.695553012793));
#45118=CARTESIAN_POINT('Ctrl Pts',(173.077445162384,-4.03963097304869,337.808712823548));
#45119=CARTESIAN_POINT('Ctrl Pts',(173.069799834897,-3.96086483198049,337.918727596373));
#45120=CARTESIAN_POINT('Ctrl Pts',(173.062154507411,-3.87779712334483,338.025206196721));
#45121=CARTESIAN_POINT('Ctrl Pts',(173.054504380427,-3.79467726740023,338.131751641003));
#45122=CARTESIAN_POINT('Ctrl Pts',(173.046854253443,-3.70725072930545,338.234756187929));
#45123=CARTESIAN_POINT('Ctrl Pts',(173.039204126459,-3.61587208542439,338.333864443007));
#45124=CARTESIAN_POINT('Ctrl Pts',(173.03154326898,-3.52436526876287,338.43311171285));
#45125=CARTESIAN_POINT('Ctrl Pts',(173.023882411502,-3.42889556893902,338.528451502177));
#45126=CARTESIAN_POINT('Ctrl Pts',(173.016221554023,-3.32985196175119,338.619567512193));
#45127=CARTESIAN_POINT('Ctrl Pts',(173.013884862577,-3.29964198194271,338.647359440425));
#45128=CARTESIAN_POINT('Ctrl Pts',(173.01154817113,-3.26909971494764,338.674758707052));
#45129=CARTESIAN_POINT('Ctrl Pts',(173.009211479684,-3.23823673494268,338.701757138302));
#45130=CARTESIAN_POINT('Ctrl Pts',(173.001436400905,-3.13554362959582,338.791591390992));
#45131=CARTESIAN_POINT('Ctrl Pts',(172.993661322127,-3.02894718200958,338.877291036297));
#45132=CARTESIAN_POINT('Ctrl Pts',(172.985886243349,-2.91881450009625,338.958497818179));
#45133=CARTESIAN_POINT('Ctrl Pts',(172.9781207323,-2.80881734345941,339.039604669947));
#45134=CARTESIAN_POINT('Ctrl Pts',(172.970355221251,-2.69529292244631,339.116229429175));
#45135=CARTESIAN_POINT('Ctrl Pts',(172.962589710202,-2.5786435038994,339.188052141783));
#45136=CARTESIAN_POINT('Ctrl Pts',(172.954831898679,-2.46210974359035,339.259803641964));
#45137=CARTESIAN_POINT('Ctrl Pts',(172.947074087157,-2.34245748252479,339.326762367052));
#45138=CARTESIAN_POINT('Ctrl Pts',(172.939316275635,-2.22011994459096,339.388650190449));
#45139=CARTESIAN_POINT('Ctrl Pts',(172.931564302112,-2.09787446953426,339.450491441297));
#45140=CARTESIAN_POINT('Ctrl Pts',(172.923812328589,-1.97294808720568,339.507269210311));
#45141=CARTESIAN_POINT('Ctrl Pts',(172.916060355066,-1.84580042180711,339.558750252575));
#45142=CARTESIAN_POINT('Ctrl Pts',(172.908311664508,-1.71870660352015,339.610209492588));
#45143=CARTESIAN_POINT('Ctrl Pts',(172.900562973951,-1.58939373472774,339.656376320962));
#45144=CARTESIAN_POINT('Ctrl Pts',(172.892814283393,-1.45834311253914,339.697064873792));
#45145=CARTESIAN_POINT('Ctrl Pts',(172.885067205015,-1.32731975652699,339.737744961029));
#45146=CARTESIAN_POINT('Ctrl Pts',(172.877320126637,-1.19455973933672,339.772948924038));
#45147=CARTESIAN_POINT('Ctrl Pts',(172.86957304826,-1.0605609019548,339.802540331506));
#45148=CARTESIAN_POINT('Ctrl Pts',(172.861825904954,-0.926560941533609,
339.83213198698));
#45149=CARTESIAN_POINT('Ctrl Pts',(172.854078761648,-0.791322521890436,
339.856110908803));
#45150=CARTESIAN_POINT('Ctrl Pts',(172.846331618342,-0.655354706495,339.87439157959));
#45151=CARTESIAN_POINT('Ctrl Pts',(172.838582733314,-0.519356322648134,
339.892676360259));
#45152=CARTESIAN_POINT('Ctrl Pts',(172.830833848286,-0.382628604052833,
339.905260288596));
#45153=CARTESIAN_POINT('Ctrl Pts',(172.823084963258,-0.245686385583616,
339.912109654969));
#45154=CARTESIAN_POINT('Ctrl Pts',(172.815327853483,-0.108598815228768,
339.91896629133));
#45155=CARTESIAN_POINT('Ctrl Pts',(172.807570743708,0.0287033187940506,
339.920076187369));
#45156=CARTESIAN_POINT('Ctrl Pts',(172.799813633934,0.165703968071794,339.915457787172));
#45157=CARTESIAN_POINT('Ctrl Pts',(172.792052379007,0.302777826116149,339.910836919049));
#45158=CARTESIAN_POINT('Ctrl Pts',(172.784291124081,0.439549488840512,339.90048168483));
#45159=CARTESIAN_POINT('Ctrl Pts',(172.776529869155,0.575508369748936,339.884462424756));
#45160=CARTESIAN_POINT('Ctrl Pts',(172.76875619875,0.711684740557825,339.868417539086));
#45161=CARTESIAN_POINT('Ctrl Pts',(172.760982528346,0.847045345256766,339.846690583788));
#45162=CARTESIAN_POINT('Ctrl Pts',(172.753208857941,0.981089243648321,339.819403174512));
#45163=CARTESIAN_POINT('Ctrl Pts',(172.745797053764,1.1088933663199,339.793386000703));
#45164=CARTESIAN_POINT('Ctrl Pts',(172.738385249587,1.23550032983211,339.76231446975));
#45165=CARTESIAN_POINT('Ctrl Pts',(172.73097344541,1.36049084386056,339.726335549479));
#45166=CARTESIAN_POINT('Ctrl Pts',(172.723198366632,1.49160751530998,339.688593195151));
#45167=CARTESIAN_POINT('Ctrl Pts',(172.715423287853,1.62135962966051,339.645330963759));
#45168=CARTESIAN_POINT('Ctrl Pts',(172.707648209075,1.74924725861172,339.596663691281));
#45169=CARTESIAN_POINT('Ctrl Pts',(172.699882698026,1.87697751369374,339.54805630698));
#45170=CARTESIAN_POINT('Ctrl Pts',(172.692117186977,2.00284748668668,339.494057253359));
#45171=CARTESIAN_POINT('Ctrl Pts',(172.684351675928,2.12637043170788,339.434831659675));
#45172=CARTESIAN_POINT('Ctrl Pts',(172.676593864405,2.24977090336935,339.37566478834));
#45173=CARTESIAN_POINT('Ctrl Pts',(172.668836052883,2.37082862790541,339.311281857578));
#45174=CARTESIAN_POINT('Ctrl Pts',(172.661078241361,2.48907528042128,339.241896664335));
#45175=CARTESIAN_POINT('Ctrl Pts',(172.653326267838,2.60723294858118,339.172563685651));
#45176=CARTESIAN_POINT('Ctrl Pts',(172.645574294315,2.72258341959847,339.098236134285));
#45177=CARTESIAN_POINT('Ctrl Pts',(172.637822320792,2.83468182381689,339.019174295825));
#45178=CARTESIAN_POINT('Ctrl Pts',(172.630073630234,2.94673275429471,338.940145940101));
#45179=CARTESIAN_POINT('Ctrl Pts',(172.622324939677,3.05553403847513,338.85638750985));
#45180=CARTESIAN_POINT('Ctrl Pts',(172.614576249119,3.16066892195133,338.768203156454));
#45181=CARTESIAN_POINT('Ctrl Pts',(172.606829170741,3.26578193123692,338.68003715055));
#45182=CARTESIAN_POINT('Ctrl Pts',(172.599082092363,3.36722975784459,338.587447304171));
#45183=CARTESIAN_POINT('Ctrl Pts',(172.591335013986,3.46462826344901,338.490778431612));
#45184=CARTESIAN_POINT('Ctrl Pts',(172.58358787068,3.56202758534641,338.394108748876));
#45185=CARTESIAN_POINT('Ctrl Pts',(172.575840727374,3.65537724112323,338.293360247122));
#45186=CARTESIAN_POINT('Ctrl Pts',(172.568093584068,3.74432983393046,338.188914730318));
#45187=CARTESIAN_POINT('Ctrl Pts',(172.56034469904,3.8333024251691,338.084445731944));
#45188=CARTESIAN_POINT('Ctrl Pts',(172.552595814012,3.91787573294078,337.976278362108));
#45189=CARTESIAN_POINT('Ctrl Pts',(172.544846928984,3.9977428034048,337.864827314224));
#45190=CARTESIAN_POINT('Ctrl Pts',(172.537089819209,4.07769464560279,337.753257971046));
#45191=CARTESIAN_POINT('Ctrl Pts',(172.529332709434,4.15293004397512,337.638398305767));
#45192=CARTESIAN_POINT('Ctrl Pts',(172.52157559966,4.22318524513987,337.520692255658));
#45193=CARTESIAN_POINT('Ctrl Pts',(172.513814344734,4.29347798843775,337.402923307199));
#45194=CARTESIAN_POINT('Ctrl Pts',(172.506053089807,4.35878504572007,337.2823052867));
#45195=CARTESIAN_POINT('Ctrl Pts',(172.498291834881,4.41888925994629,337.159305622378));
#45196=CARTESIAN_POINT('Ctrl Pts',(172.490518164477,4.47908962132733,337.036109198678));
#45197=CARTESIAN_POINT('Ctrl Pts',(172.482744494072,4.53407035128552,336.910523876191));
#45198=CARTESIAN_POINT('Ctrl Pts',(172.474970823667,4.58366263153101,336.783036719422));
#45199=CARTESIAN_POINT('Ctrl Pts',(172.46755901949,4.63094637919994,336.661484120472));
#45200=CARTESIAN_POINT('Ctrl Pts',(172.460147215313,4.67333195860183,336.538203035529));
#45201=CARTESIAN_POINT('Ctrl Pts',(172.452735411136,4.71071605606521,336.413625587498));
#45202=CARTESIAN_POINT('Ctrl Pts',(172.444960332358,4.74993245950672,336.282942227642));
#45203=CARTESIAN_POINT('Ctrl Pts',(172.437185253579,4.78376864041988,336.150419230752));
#45204=CARTESIAN_POINT('Ctrl Pts',(172.429410174801,4.81205062693849,336.016539141539));
#45205=CARTESIAN_POINT('Ctrl Pts',(172.421644663752,4.84029781067216,335.882823800299));
#45206=CARTESIAN_POINT('Ctrl Pts',(172.413879152703,4.86300431926685,335.747755068312));
#45207=CARTESIAN_POINT('Ctrl Pts',(172.406113641654,4.88004560731185,335.611831621491));
#45208=CARTESIAN_POINT('Ctrl Pts',(172.398355830131,4.89706999887007,335.476042943164));
#45209=CARTESIAN_POINT('Ctrl Pts',(172.390598018609,4.90844029987912,335.339401621821));
#45210=CARTESIAN_POINT('Ctrl Pts',(172.382840207087,4.91408285928114,335.202417179654));
#45211=CARTESIAN_POINT('Ctrl Pts',(172.375088233564,4.9197211724783,335.065535822624));
#45212=CARTESIAN_POINT('Ctrl Pts',(172.367336260041,4.91964030750197,334.928312247693));
#45213=CARTESIAN_POINT('Ctrl Pts',(172.359584286518,4.91381839955879,334.791261410713));
#45214=CARTESIAN_POINT('Ctrl Pts',(172.35183559596,4.90799895719709,334.654268614844));
#45215=CARTESIAN_POINT('Ctrl Pts',(172.344086905403,4.89644332417758,334.517448801137));
#45216=CARTESIAN_POINT('Ctrl Pts',(172.336338214845,4.87918173816371,334.381317021028));
#45217=CARTESIAN_POINT('Ctrl Pts',(172.328591136467,4.86192374356699,334.245213564273));
#45218=CARTESIAN_POINT('Ctrl Pts',(172.32084405809,4.83896220648185,334.109798243904));
#45219=CARTESIAN_POINT('Ctrl Pts',(172.313096979712,4.81037920931537,333.975580688836));
#45220=CARTESIAN_POINT('Ctrl Pts',(172.305349836406,4.78179597259581,333.841362008894));
#45221=CARTESIAN_POINT('Ctrl Pts',(172.2976026931,4.74759126323896,333.708341496577));
#45222=CARTESIAN_POINT('Ctrl Pts',(172.289855549794,4.70789815197728,333.577017901339));
#45223=CARTESIAN_POINT('Ctrl Pts',(172.282106664766,4.66819611686151,333.445664781769));
#45224=CARTESIAN_POINT('Ctrl Pts',(172.274357779738,4.62300333756766,333.316009712511));
#45225=CARTESIAN_POINT('Ctrl Pts',(172.26660889471,4.57250242829785,333.188535231999));
#45226=CARTESIAN_POINT('Ctrl Pts',(172.258851784935,4.52194791684115,333.060925448756));
#45227=CARTESIAN_POINT('Ctrl Pts',(172.251094675161,4.46607416494939,332.935501241658));
#45228=CARTESIAN_POINT('Ctrl Pts',(172.243337565386,4.40511175685733,332.812724646484));
#45229=CARTESIAN_POINT('Ctrl Pts',(172.23557631046,4.34411677240365,332.689882443424));
#45230=CARTESIAN_POINT('Ctrl Pts',(172.227815055533,4.27802790170672,332.569691013737));
#45231=CARTESIAN_POINT('Ctrl Pts',(172.220053800607,4.20712069899228,332.452585921643));
#45232=CARTESIAN_POINT('Ctrl Pts',(172.212280130203,4.13610006786209,332.335293499566));
#45233=CARTESIAN_POINT('Ctrl Pts',(172.204506459798,4.06024591871126,332.2210976067));
#45234=CARTESIAN_POINT('Ctrl Pts',(172.196732789393,3.97987647721037,332.110403784497));
#45235=CARTESIAN_POINT('Ctrl Pts',(172.189320985216,3.9032482525467,332.004862786349));
#45236=CARTESIAN_POINT('Ctrl Pts',(172.181909181039,3.82251582723015,331.902505379444));
#45237=CARTESIAN_POINT('Ctrl Pts',(172.174497376862,3.73798667367353,331.803652288949));
#45238=CARTESIAN_POINT('Ctrl Pts',(172.166722298084,3.64931449450228,331.699954114022));
#45239=CARTESIAN_POINT('Ctrl Pts',(172.158947219305,3.55618377817555,331.599784749845));
#45240=CARTESIAN_POINT('Ctrl Pts',(172.151172140527,3.45890616067516,331.5035516257));
#45241=CARTESIAN_POINT('Ctrl Pts',(172.143406629478,3.36174824947598,331.407436922542));
#45242=CARTESIAN_POINT('Ctrl Pts',(172.135641118429,3.26045386588272,331.315249093922));
#45243=CARTESIAN_POINT('Ctrl Pts',(172.12787560738,3.15537495844174,331.227362734884));
#45244=CARTESIAN_POINT('Ctrl Pts',(172.120117795857,3.05040023704328,331.139563515428));
#45245=CARTESIAN_POINT('Ctrl Pts',(172.112359984335,2.94164875711457,331.056057527278));
#45246=CARTESIAN_POINT('Ctrl Pts',(172.104602172813,2.82950912992339,330.977182436876));
#45247=CARTESIAN_POINT('Ctrl Pts',(172.09685019929,2.71745389135814,330.898366702481));
#45248=CARTESIAN_POINT('Ctrl Pts',(172.089098225767,2.60201589898342,330.824175153282));
#45249=CARTESIAN_POINT('Ctrl Pts',(172.081346252244,2.48361635786692,330.754904848012));
#45250=CARTESIAN_POINT('Ctrl Pts',(172.073597561686,2.36526695902625,330.685663878756));
#45251=CARTESIAN_POINT('Ctrl Pts',(172.065848871129,2.24395884266799,330.621340205175));
#45252=CARTESIAN_POINT('Ctrl Pts',(172.058100180571,2.12014148986842,330.562187123657));
#45253=CARTESIAN_POINT('Ctrl Pts',(172.050353102193,1.99634989830326,330.503046349431));
#45254=CARTESIAN_POINT('Ctrl Pts',(172.042606023816,1.87005046119664,330.449074195848));
#45255=CARTESIAN_POINT('Ctrl Pts',(172.034858945438,1.74171615587461,330.400477427508));
#45256=CARTESIAN_POINT('Ctrl Pts',(172.027111802132,1.61338077498778,330.35188025188));
#45257=CARTESIAN_POINT('Ctrl Pts',(172.019364658826,1.48301085741342,330.308658689773));
#45258=CARTESIAN_POINT('Ctrl Pts',(172.01161751552,1.35109782441841,330.270970741119));
#45259=CARTESIAN_POINT('Ctrl Pts',(172.003868630492,1.2191551345729,330.233274319414));
#45260=CARTESIAN_POINT('Ctrl Pts',(171.996119745464,1.0856690147272,330.201114094086));
#45261=CARTESIAN_POINT('Ctrl Pts',(171.988370860436,0.951144064768316,330.174597630191));
#45262=CARTESIAN_POINT('Ctrl Pts',(171.980613750661,0.816476328637388,330.148053021448));
#45263=CARTESIAN_POINT('Ctrl Pts',(171.972856640887,0.680767943897373,330.127164216128));
#45264=CARTESIAN_POINT('Ctrl Pts',(171.965099531112,0.544532228650927,330.1119873451));
#45265=CARTESIAN_POINT('Ctrl Pts',(171.957338276186,0.408223713394111,330.096802364038));
#45266=CARTESIAN_POINT('Ctrl Pts',(171.94957702126,0.271387695886138,330.087335426165));
#45267=CARTESIAN_POINT('Ctrl Pts',(171.941815766333,0.134539569573238,330.083590520846));
#45268=CARTESIAN_POINT('Ctrl Pts',(171.934042095929,-0.00252746914292362,
330.079839624898));
#45269=CARTESIAN_POINT('Ctrl Pts',(171.926268425524,-0.139606264332587,
330.081829047007));
#45270=CARTESIAN_POINT('Ctrl Pts',(171.918494755119,-0.276183577365626,
330.089510646168));
#45271=CARTESIAN_POINT('Ctrl Pts',(171.911082950942,-0.406403183618759,
330.09683466504));
#45272=CARTESIAN_POINT('Ctrl Pts',(171.903671146765,-0.536166658549343,
330.109332817696));
#45273=CARTESIAN_POINT('Ctrl Pts',(171.896259342588,-0.66503790655522,330.126920106817));
#45274=CARTESIAN_POINT('Ctrl Pts',(171.88848426381,-0.800225518313382,330.145369401367));
#45275=CARTESIAN_POINT('Ctrl Pts',(171.880709185031,-0.934858448114493,
330.16947761691));
#45276=CARTESIAN_POINT('Ctrl Pts',(171.872934106253,-1.06842543586947,330.199203175463));
#45277=CARTESIAN_POINT('Ctrl Pts',(171.865168595204,-1.20182806094268,330.228892154824));
#45278=CARTESIAN_POINT('Ctrl Pts',(171.857403084155,-1.33416697600323,330.264184639206));
#45279=CARTESIAN_POINT('Ctrl Pts',(171.849637573106,-1.46493671653396,330.30498738244));
#45280=CARTESIAN_POINT('Ctrl Pts',(171.841879761584,-1.59557679848631,330.345749669635));
#45281=CARTESIAN_POINT('Ctrl Pts',(171.834121950061,-1.72465043139156,330.392011227458));
#45282=CARTESIAN_POINT('Ctrl Pts',(171.826364138539,-1.85166336448089,330.443627995089));
#45283=CARTESIAN_POINT('Ctrl Pts',(171.818612165016,-1.9785807163094,330.495205919465));
#45284=CARTESIAN_POINT('Ctrl Pts',(171.810860191493,-2.10344009434181,330.552130885633));
#45285=CARTESIAN_POINT('Ctrl Pts',(171.80310821797,-2.22576375732302,330.614209448789));
#45286=CARTESIAN_POINT('Ctrl Pts',(171.795359527413,-2.34803561616103,330.676261721638));
#45287=CARTESIAN_POINT('Ctrl Pts',(171.787610836855,-2.4677735479811,330.743463074013));
#45288=CARTESIAN_POINT('Ctrl Pts',(171.779862146297,-2.5845213104435,330.815572600897));
#45289=CARTESIAN_POINT('Ctrl Pts',(171.77211506792,-2.70124478255856,330.887667124792));
#45290=CARTESIAN_POINT('Ctrl Pts',(171.764367989542,-2.81497899043046,330.96466758671));
#45291=CARTESIAN_POINT('Ctrl Pts',(171.756620911164,-2.92529410612515,331.046288142116));
#45292=CARTESIAN_POINT('Ctrl Pts',(171.748873767858,-3.03561014636689,331.127909381582));
#45293=CARTESIAN_POINT('Ctrl Pts',(171.741126624552,-3.14250672305798,331.214150559282));
#45294=CARTESIAN_POINT('Ctrl Pts',(171.733379481247,-3.24558503444035,331.304683931418));
#45295=CARTESIAN_POINT('Ctrl Pts',(171.725630596219,-3.34868652001539,331.395237657379));
#45296=CARTESIAN_POINT('Ctrl Pts',(171.71788171119,-3.44796773848256,331.49008524008));
#45297=CARTESIAN_POINT('Ctrl Pts',(171.710132826162,-3.54306516813837,331.588860560337));
#45298=CARTESIAN_POINT('Ctrl Pts',(171.702375716388,-3.63826353518874,331.687740721739));
#45299=CARTESIAN_POINT('Ctrl Pts',(171.694618606613,-3.72926897115358,331.790556666521));
#45300=CARTESIAN_POINT('Ctrl Pts',(171.686861496838,-3.81575648850863,331.896907110171));
#45301=CARTESIAN_POINT('Ctrl Pts',(171.679100241912,-3.90229022202734,332.003314384098));
#45302=CARTESIAN_POINT('Ctrl Pts',(171.671338986986,-3.98430099277517,332.113259607193));
#45303=CARTESIAN_POINT('Ctrl Pts',(171.66357773206,-4.06150653704379,332.226311532985));
#45304=CARTESIAN_POINT('Ctrl Pts',(171.655804061655,-4.13883558502221,332.339544305015));
#45305=CARTESIAN_POINT('Ctrl Pts',(171.64803039125,-4.21134383918479,332.455893378795));
#45306=CARTESIAN_POINT('Ctrl Pts',(171.640256720846,-4.2787940394573,332.574901109149));
#45307=CARTESIAN_POINT('Ctrl Pts',(171.632844916669,-4.34310441667927,332.688369001024));
#45308=CARTESIAN_POINT('Ctrl Pts',(171.625433112491,-4.40281691558553,332.804253343021));
#45309=CARTESIAN_POINT('Ctrl Pts',(171.618021308314,-4.45776701588196,332.922141416117));
#45310=CARTESIAN_POINT('Ctrl Pts',(171.609572694798,-4.52040387851417,333.056520407251));
#45311=CARTESIAN_POINT('Ctrl Pts',(171.601124081281,-4.57702589321632,333.193873629242));
#45312=CARTESIAN_POINT('Ctrl Pts',(171.592675467765,-4.62736511960204,333.333664165785));
#45313=CARTESIAN_POINT('Ctrl Pts',(171.584255967307,-4.6775308821615,333.472972998434));
#45314=CARTESIAN_POINT('Ctrl Pts',(171.575836466848,-4.72145694007028,333.614702130559));
#45315=CARTESIAN_POINT('Ctrl Pts',(171.56741696639,-4.75892347987298,333.758295375215));
#45316=CARTESIAN_POINT('Ctrl Pts',(171.559015379067,-4.79631030672791,333.901583114188));
#45317=CARTESIAN_POINT('Ctrl Pts',(171.550613791744,-4.82726493948641,334.04672678951));
#45318=CARTESIAN_POINT('Ctrl Pts',(171.542212204421,-4.85161628364152,334.193152741342));
#45319=CARTESIAN_POINT('Ctrl Pts',(171.533839254757,-4.87588462378235,334.339079585538));
#45320=CARTESIAN_POINT('Ctrl Pts',(171.525466305092,-4.89359451160953,334.486279713807));
#45321=CARTESIAN_POINT('Ctrl Pts',(171.517093355428,-4.90462539132199,334.634168299215));
#45322=CARTESIAN_POINT('Ctrl Pts',(171.510240986461,-4.91365299340367,334.755199380713));
#45323=CARTESIAN_POINT('Ctrl Pts',(171.503388617494,-4.91820808107563,334.876691189428));
#45324=CARTESIAN_POINT('Ctrl Pts',(171.496536248527,-4.91824971188751,334.998316545704));
#45325=CARTESIAN_POINT('',(174.996536248523,-4.91824863027879,335.003670594061));
#45326=CARTESIAN_POINT('Ctrl Pts',(174.99653624849,-4.91824863027836,335.003670594644));
#45327=CARTESIAN_POINT('Ctrl Pts',(174.98331673886,-4.91807501968798,335.236292317054));
#45328=CARTESIAN_POINT('Ctrl Pts',(174.970097229231,-4.90139623116265,335.468309461225));
#45329=CARTESIAN_POINT('Ctrl Pts',(174.956877719601,-4.86847588454197,335.697943854571));
#45330=CARTESIAN_POINT('Ctrl Pts',(174.949102640823,-4.84911372243734,335.833003743216));
#45331=CARTESIAN_POINT('Ctrl Pts',(174.941327562044,-4.82409651574911,335.967470732522));
#45332=CARTESIAN_POINT('Ctrl Pts',(174.933552483266,-4.79346929543573,336.100833854955));
#45333=CARTESIAN_POINT('Ctrl Pts',(174.925786972217,-4.76287976386681,336.234032865575));
#45334=CARTESIAN_POINT('Ctrl Pts',(174.918021461168,-4.72669404126795,336.366130334791));
#45335=CARTESIAN_POINT('Ctrl Pts',(174.910255950119,-4.68500878645265,336.496621439564));
#45336=CARTESIAN_POINT('Ctrl Pts',(174.902498138597,-4.6433648626888,336.626983162026));
#45337=CARTESIAN_POINT('Ctrl Pts',(174.894740327074,-4.59623237626986,336.7557413197));
#45338=CARTESIAN_POINT('Ctrl Pts',(174.886982515552,-4.54375872374385,336.882402646328));
#45339=CARTESIAN_POINT('Ctrl Pts',(174.879230542029,-4.49132455930545,337.008968656291));
#45340=CARTESIAN_POINT('Ctrl Pts',(174.871478568506,-4.43355737817314,337.133440616346));
#45341=CARTESIAN_POINT('Ctrl Pts',(174.863726594983,-4.37065384821781,337.255342102999));
#45342=CARTESIAN_POINT('Ctrl Pts',(174.855977904425,-4.30777695794471,337.377191964299));
#45343=CARTESIAN_POINT('Ctrl Pts',(174.848229213868,-4.23976822412976,337.496473170708));
#45344=CARTESIAN_POINT('Ctrl Pts',(174.84048052331,-4.16687162853289,337.612731117782));
#45345=CARTESIAN_POINT('Ctrl Pts',(174.832733444932,-4.09399019968162,337.728964876419));
#45346=CARTESIAN_POINT('Ctrl Pts',(174.824986366554,-4.01622313936925,337.842176295924));
#45347=CARTESIAN_POINT('Ctrl Pts',(174.817239288177,-3.93385918940115,337.951937489254));
#45348=CARTESIAN_POINT('Ctrl Pts',(174.809492144871,-3.85149454914383,338.061699602489));
#45349=CARTESIAN_POINT('Ctrl Pts',(174.801745001565,-3.76453317699013,338.168011119234));
#45350=CARTESIAN_POINT('Ctrl Pts',(174.793997858259,-3.67330550344933,338.270475460973));
#45351=CARTESIAN_POINT('Ctrl Pts',(174.786248973231,-3.58205731999085,338.372962838872));
#45352=CARTESIAN_POINT('Ctrl Pts',(174.778500088203,-3.48654118640158,338.471601028783));
#45353=CARTESIAN_POINT('Ctrl Pts',(174.770751203175,-3.38712566936063,338.566028990692));
#45354=CARTESIAN_POINT('Ctrl Pts',(174.7629940934,-3.28760463166257,338.660557179417));
#45355=CARTESIAN_POINT('Ctrl Pts',(174.755236983625,-3.18417622663505,338.75086594372));
#45356=CARTESIAN_POINT('Ctrl Pts',(174.747479873851,-3.07724392515281,338.836633014456));
#45357=CARTESIAN_POINT('Ctrl Pts',(174.739718618925,-2.97025448246778,338.922445916372));
#45358=CARTESIAN_POINT('Ctrl Pts',(174.731957363998,-2.85975772718503,339.003712057366));
#45359=CARTESIAN_POINT('Ctrl Pts',(174.724196109072,-2.74618680282642,339.080152093548));
#45360=CARTESIAN_POINT('Ctrl Pts',(174.716422438668,-2.63243420200145,339.156714408876));
#45361=CARTESIAN_POINT('Ctrl Pts',(174.708648768263,-2.51559793843602,339.228434987562));
#45362=CARTESIAN_POINT('Ctrl Pts',(174.700875097858,-2.39613724972105,339.295079666665));
#45363=CARTESIAN_POINT('Ctrl Pts',(174.693463293681,-2.28223748480732,339.358622019922));
#45364=CARTESIAN_POINT('Ctrl Pts',(174.686051489504,-2.16595238685683,339.417550274945));
#45365=CARTESIAN_POINT('Ctrl Pts',(174.678639685327,-2.04769577692535,339.471702703408));
#45366=CARTESIAN_POINT('Ctrl Pts',(174.670864606549,-1.92364305827191,339.528509303701));
#45367=CARTESIAN_POINT('Ctrl Pts',(174.66308952777,-1.79702865221146,339.580239604505));
#45368=CARTESIAN_POINT('Ctrl Pts',(174.655314448992,-1.66830661107918,339.626654959464));
#45369=CARTESIAN_POINT('Ctrl Pts',(174.647548937943,-1.53974297061342,339.673013197373));
#45370=CARTESIAN_POINT('Ctrl Pts',(174.639783426894,-1.40907721973958,339.714069371594));
#45371=CARTESIAN_POINT('Ctrl Pts',(174.632017915845,-1.27678618255062,339.749631575875));
#45372=CARTESIAN_POINT('Ctrl Pts',(174.624260104323,-1.14462631231009,339.785158520126));
#45373=CARTESIAN_POINT('Ctrl Pts',(174.616502292801,-1.0108447377249,339.815202234028));
#45374=CARTESIAN_POINT('Ctrl Pts',(174.608744481278,-0.875936021643368,
339.839619731806));
#45375=CARTESIAN_POINT('Ctrl Pts',(174.600992507755,-0.741128828649,339.864018854643));
#45376=CARTESIAN_POINT('Ctrl Pts',(174.593240534232,-0.60519656555478,339.882800119406));
#45377=CARTESIAN_POINT('Ctrl Pts',(174.585488560709,-0.46864629531195,339.895871088212));
#45378=CARTESIAN_POINT('Ctrl Pts',(174.577739870152,-0.332153854189639,
339.908936521455));
#45379=CARTESIAN_POINT('Ctrl Pts',(174.569991179594,-0.195044314760044,
339.91629643143));
#45380=CARTESIAN_POINT('Ctrl Pts',(174.562242489037,-0.0578319961281068,
339.917909975053));
#45381=CARTESIAN_POINT('Ctrl Pts',(174.554495410659,0.0793517743349073,
339.919523182965));
#45382=CARTESIAN_POINT('Ctrl Pts',(174.546748332281,0.216637890863955,339.915392398025));
#45383=CARTESIAN_POINT('Ctrl Pts',(174.539001253903,0.353510279357964,339.905528875146));
#45384=CARTESIAN_POINT('Ctrl Pts',(174.531254110597,0.490383814974363,339.895665269601));
#45385=CARTESIAN_POINT('Ctrl Pts',(174.523506967292,0.626843225776368,339.880068858382));
#45386=CARTESIAN_POINT('Ctrl Pts',(174.515759823986,0.762376205521692,339.858802896162));
#45387=CARTESIAN_POINT('Ctrl Pts',(174.508010938958,0.897939655958299,339.837532152903));
#45388=CARTESIAN_POINT('Ctrl Pts',(174.50026205393,1.03257587480725,339.810589382839));
#45389=CARTESIAN_POINT('Ctrl Pts',(174.492513168902,1.16578180324149,339.778089142087));
#45390=CARTESIAN_POINT('Ctrl Pts',(174.484756059127,1.29912911782448,339.745554405244));
#45391=CARTESIAN_POINT('Ctrl Pts',(174.476998949352,1.4310427290607,339.707450507188));
#45392=CARTESIAN_POINT('Ctrl Pts',(174.469241839577,1.56103329270892,339.66394233686));
#45393=CARTESIAN_POINT('Ctrl Pts',(174.461480584651,1.69109331915798,339.620410917157));
#45394=CARTESIAN_POINT('Ctrl Pts',(174.453719329725,1.81922788544291,339.571469610237));
#45395=CARTESIAN_POINT('Ctrl Pts',(174.445958074799,1.94496768651358,339.517331486721));
#45396=CARTESIAN_POINT('Ctrl Pts',(174.438184404394,2.07090863028747,339.463106759851));
#45397=CARTESIAN_POINT('Ctrl Pts',(174.43041073399,2.19444680127458,339.403668773679));
#45398=CARTESIAN_POINT('Ctrl Pts',(174.422637063585,2.31513676705072,339.33927699189));
#45399=CARTESIAN_POINT('Ctrl Pts',(174.415225259408,2.43020858588388,339.277882663036));
#45400=CARTESIAN_POINT('Ctrl Pts',(174.407813455231,2.54269115165218,339.211985503431));
#45401=CARTESIAN_POINT('Ctrl Pts',(174.400401651054,2.65222452123518,339.141845983551));
#45402=CARTESIAN_POINT('Ctrl Pts',(174.392626572275,2.76712644754428,339.068268716868));
#45403=CARTESIAN_POINT('Ctrl Pts',(174.384851493497,2.87914588136086,338.989790195661));
#45404=CARTESIAN_POINT('Ctrl Pts',(174.377076414718,2.98783642609918,338.906663096989));
#45405=CARTESIAN_POINT('Ctrl Pts',(174.369310903669,3.09639322020262,338.823638291504));
#45406=CARTESIAN_POINT('Ctrl Pts',(174.36154539262,3.20162896839791,338.735976525637));
#45407=CARTESIAN_POINT('Ctrl Pts',(174.353779881571,3.30312425574478,338.643974919454));
#45408=CARTESIAN_POINT('Ctrl Pts',(174.346022070049,3.40451891021875,338.552064533132));
#45409=CARTESIAN_POINT('Ctrl Pts',(174.338264258527,3.50218019658619,338.455823130458));
#45410=CARTESIAN_POINT('Ctrl Pts',(174.330506447005,3.59572023872465,338.355589222078));
#45411=CARTESIAN_POINT('Ctrl Pts',(174.322754473482,3.689189889015,338.255430742892));
#45412=CARTESIAN_POINT('Ctrl Pts',(174.315002499959,3.77854420258656,338.151286022901));
#45413=CARTESIAN_POINT('Ctrl Pts',(174.307250526436,3.8634310455938,338.043531438714));
#45414=CARTESIAN_POINT('Ctrl Pts',(174.299501835878,3.94828193897268,337.935822488658));
#45415=CARTESIAN_POINT('Ctrl Pts',(174.29175314532,4.02866888341605,337.824507021447));
#45416=CARTESIAN_POINT('Ctrl Pts',(174.284004454763,4.10427920552521,337.709995436453));
#45417=CARTESIAN_POINT('Ctrl Pts',(174.276257376385,4.17987379627534,337.59550767655));
#45418=CARTESIAN_POINT('Ctrl Pts',(174.268510298007,4.25069352622226,337.477825447534));
#45419=CARTESIAN_POINT('Ctrl Pts',(174.260763219629,4.31646858255452,337.357388817807));
#45420=CARTESIAN_POINT('Ctrl Pts',(174.253016076323,4.38224419014507,337.236951178704));
#45421=CARTESIAN_POINT('Ctrl Pts',(174.245268933018,4.44297485244015,337.113759435894));
#45422=CARTESIAN_POINT('Ctrl Pts',(174.237521789712,4.4984365233414,336.98827862936));
#45423=CARTESIAN_POINT('Ctrl Pts',(174.229772904684,4.55391066320374,336.862769612076));
#45424=CARTESIAN_POINT('Ctrl Pts',(174.222024019656,4.60411329650204,336.73497086445));
#45425=CARTESIAN_POINT('Ctrl Pts',(174.214275134627,4.64886852192176,336.605367412272));
#45426=CARTESIAN_POINT('Ctrl Pts',(174.206518024853,4.69367125100018,336.47562639765));
#45427=CARTESIAN_POINT('Ctrl Pts',(174.198760915078,4.7330148944555,336.344077222069));
#45428=CARTESIAN_POINT('Ctrl Pts',(174.191003805303,4.76677329866749,336.211220616408));
#45429=CARTESIAN_POINT('Ctrl Pts',(174.183242550377,4.8005497422913,336.078293016424));
#45430=CARTESIAN_POINT('Ctrl Pts',(174.175481295451,4.82873491936202,335.944056976578));
#45431=CARTESIAN_POINT('Ctrl Pts',(174.167720040525,4.85125403761879,335.809022450237));
#45432=CARTESIAN_POINT('Ctrl Pts',(174.15994637012,4.87380917912581,335.673771912662));
#45433=CARTESIAN_POINT('Ctrl Pts',(174.152172699715,4.89068010144037,335.537720724239));
#45434=CARTESIAN_POINT('Ctrl Pts',(174.144399029311,4.90184394406614,335.401383869285));
#45435=CARTESIAN_POINT('Ctrl Pts',(174.136987225134,4.91248810713189,335.271393527729));
#45436=CARTESIAN_POINT('Ctrl Pts',(174.129575420956,4.91794455035138,335.141143804223));
#45437=CARTESIAN_POINT('Ctrl Pts',(174.122163616779,4.91823752302836,335.011078338136));
#45438=CARTESIAN_POINT('Ctrl Pts',(174.114388538001,4.91854485516896,334.874637976112));
#45439=CARTESIAN_POINT('Ctrl Pts',(174.106613459222,4.91317073573236,334.737969213465));
#45440=CARTESIAN_POINT('Ctrl Pts',(174.098838380444,4.9020860754402,334.60158417266));
#45441=CARTESIAN_POINT('Ctrl Pts',(174.091072869395,4.89101505552821,334.46536696233));
#45442=CARTESIAN_POINT('Ctrl Pts',(174.083307358346,4.87424750820317,334.329433165025));
#45443=CARTESIAN_POINT('Ctrl Pts',(174.075541847297,4.85180631857765,334.194296264431));
#45444=CARTESIAN_POINT('Ctrl Pts',(174.067784035775,4.82938737945698,334.059293352468));
#45445=CARTESIAN_POINT('Ctrl Pts',(174.060026224253,4.80130605658553,333.925086147932));
#45446=CARTESIAN_POINT('Ctrl Pts',(174.05226841273,4.76763710875924,333.792184011663));
#45447=CARTESIAN_POINT('Ctrl Pts',(174.044516439207,4.7339934978839,333.659381888467));
#45448=CARTESIAN_POINT('Ctrl Pts',(174.036764465684,4.69477072723567,333.527883256083));
#45449=CARTESIAN_POINT('Ctrl Pts',(174.029012492161,4.6500947401073,333.398187910357));
#45450=CARTESIAN_POINT('Ctrl Pts',(174.021263801604,4.605437673286,333.268547490687));
#45451=CARTESIAN_POINT('Ctrl Pts',(174.013515111046,4.55533211033673,333.140709207536));
#45452=CARTESIAN_POINT('Ctrl Pts',(174.005766420489,4.49995395932998,333.015158085285));
#45453=CARTESIAN_POINT('Ctrl Pts',(173.998019342111,4.44458733021006,332.889633084993));
#45454=CARTESIAN_POINT('Ctrl Pts',(173.990272263733,4.38395045269997,332.766394656483));
#45455=CARTESIAN_POINT('Ctrl Pts',(173.982525185355,4.3182673785125,332.645907837366));
#45456=CARTESIAN_POINT('Ctrl Pts',(173.974778042049,4.25258375383766,332.525420008453));
#45457=CARTESIAN_POINT('Ctrl Pts',(173.967030898744,4.18185403522065,332.407684178123));
#45458=CARTESIAN_POINT('Ctrl Pts',(173.959283755438,4.10634804050459,332.293140411336));
#45459=CARTESIAN_POINT('Ctrl Pts',(173.95153487041,4.03082507043788,332.178570892678));
#45460=CARTESIAN_POINT('Ctrl Pts',(173.943785985382,3.95052390259725,332.067195191881));
#45461=CARTESIAN_POINT('Ctrl Pts',(173.936037100353,3.86575721522074,331.959423703396));
#45462=CARTESIAN_POINT('Ctrl Pts',(173.928279990579,3.78090055560641,331.85153782514));
#45463=CARTESIAN_POINT('Ctrl Pts',(173.920522880804,3.69156915039299,331.747264108802));
#45464=CARTESIAN_POINT('Ctrl Pts',(173.912765771029,3.59811580589651,331.646979613862));
#45465=CARTESIAN_POINT('Ctrl Pts',(173.905004516103,3.5046125229208,331.546641530095));
#45466=CARTESIAN_POINT('Ctrl Pts',(173.897243261177,3.40698318979185,331.450297189768));
#45467=CARTESIAN_POINT('Ctrl Pts',(173.889482006251,3.30561616279193,331.358285452319));
#45468=CARTESIAN_POINT('Ctrl Pts',(173.881708335846,3.20408698158427,331.266126526077));
#45469=CARTESIAN_POINT('Ctrl Pts',(173.873934665441,3.09880845883244,331.178314302906));
#45470=CARTESIAN_POINT('Ctrl Pts',(173.866160995037,2.99020128470804,331.09514669425));
#45471=CARTESIAN_POINT('Ctrl Pts',(173.85874919086,2.88664980066902,331.015850557785));
#45472=CARTESIAN_POINT('Ctrl Pts',(173.851337386683,2.78007282393473,330.940776519158));
#45473=CARTESIAN_POINT('Ctrl Pts',(173.843925582506,2.67085654300497,330.87014426533));
#45474=CARTESIAN_POINT('Ctrl Pts',(173.836150503727,2.55628724680781,330.796050114339));
#45475=CARTESIAN_POINT('Ctrl Pts',(173.828375424949,2.4384513242031,330.726610016504));
#45476=CARTESIAN_POINT('Ctrl Pts',(173.82060034617,2.31776368802125,330.662125572473));
#45477=CARTESIAN_POINT('Ctrl Pts',(173.812834835121,2.19722456565895,330.597720480656));
#45478=CARTESIAN_POINT('Ctrl Pts',(173.805069324072,2.07384105350507,330.53825909132));
#45479=CARTESIAN_POINT('Ctrl Pts',(173.797303813023,1.94805733539498,330.484000035373));
#45480=CARTESIAN_POINT('Ctrl Pts',(173.789546001501,1.82239833220769,330.429794777438));
#45481=CARTESIAN_POINT('Ctrl Pts',(173.781788189979,1.69434421561682,330.380781741747));
#45482=CARTESIAN_POINT('Ctrl Pts',(173.774030378457,1.5643637742931,330.337173706412));
#45483=CARTESIAN_POINT('Ctrl Pts',(173.766278404934,1.43448114737362,330.293598487506));
#45484=CARTESIAN_POINT('Ctrl Pts',(173.758526431411,1.3026754502025,330.255420296752));
#45485=CARTESIAN_POINT('Ctrl Pts',(173.750774457888,1.16943512690991,330.222803693959));
#45486=CARTESIAN_POINT('Ctrl Pts',(173.74302576733,1.03625123097314,330.190200904317));
#45487=CARTESIAN_POINT('Ctrl Pts',(173.735277076772,0.901634296192913,330.163155110784));
#45488=CARTESIAN_POINT('Ctrl Pts',(173.727528386215,0.766087383869004,330.141780863035));
#45489=CARTESIAN_POINT('Ctrl Pts',(173.719781307837,0.630568673212303,330.120411062376));
#45490=CARTESIAN_POINT('Ctrl Pts',(173.712034229459,0.494120755737382,330.104710521219));
#45491=CARTESIAN_POINT('Ctrl Pts',(173.704287151081,0.357255938731466,330.094742488234));
#45492=CARTESIAN_POINT('Ctrl Pts',(173.696540007775,0.220389974666582,330.084774371707));
#45493=CARTESIAN_POINT('Ctrl Pts',(173.688792864469,0.0831074939433382,
330.080538887571));
#45494=CARTESIAN_POINT('Ctrl Pts',(173.681045721164,-0.0540754295057921,
330.082047284649));
#45495=CARTESIAN_POINT('Ctrl Pts',(173.673296836136,-0.191289194588415,
330.083556020847));
#45496=CARTESIAN_POINT('Ctrl Pts',(173.665547951107,-0.32840296708379,330.090811203597));
#45497=CARTESIAN_POINT('Ctrl Pts',(173.657799066079,-0.464902429405222,
330.103771983084));
#45498=CARTESIAN_POINT('Ctrl Pts',(173.650041956305,-0.601546773666418,
330.116746519276));
#45499=CARTESIAN_POINT('Ctrl Pts',(173.64228484653,-0.737575115513532,330.135438712587));
#45500=CARTESIAN_POINT('Ctrl Pts',(173.634527736755,-0.87247945384309,330.159755929179));
#45501=CARTESIAN_POINT('Ctrl Pts',(173.626766481829,-1.00745588073751,330.184086140113));
#45502=CARTESIAN_POINT('Ctrl Pts',(173.619005226903,-1.1413067260601,330.214047278384));
#45503=CARTESIAN_POINT('Ctrl Pts',(173.611243971977,-1.27353687381356,330.249496143193));
#45504=CARTESIAN_POINT('Ctrl Pts',(173.603470301572,-1.40597854670977,330.285001714633));
#45505=CARTESIAN_POINT('Ctrl Pts',(173.595696631167,-1.53679396810694,330.326012437812));
#45506=CARTESIAN_POINT('Ctrl Pts',(173.587922960763,-1.66550495832667,330.372335762365));
#45507=CARTESIAN_POINT('Ctrl Pts',(173.580511156585,-1.78822442098549,330.416502725015));
#45508=CARTESIAN_POINT('Ctrl Pts',(173.573099352408,-1.90903069919843,330.465498708422));
#45509=CARTESIAN_POINT('Ctrl Pts',(173.565687548231,-2.02753006475578,330.519117843659));
#45510=CARTESIAN_POINT('Ctrl Pts',(173.557912469453,-2.15183743721038,330.575365012438));
#45511=CARTESIAN_POINT('Ctrl Pts',(173.550137390674,-2.273998876064,330.636877732265));
#45512=CARTESIAN_POINT('Ctrl Pts',(173.542362311896,-2.39353622575786,330.703470307506));
#45513=CARTESIAN_POINT('Ctrl Pts',(173.534596800847,-2.51292647713295,330.769980936344));
#45514=CARTESIAN_POINT('Ctrl Pts',(173.526831289798,-2.62969872614955,330.841558794322));
#45515=CARTESIAN_POINT('Ctrl Pts',(173.519065778749,-2.74339511119906,330.917970317802));
#45516=CARTESIAN_POINT('Ctrl Pts',(173.511307967227,-2.8569787659517,330.994306079033));
#45517=CARTESIAN_POINT('Ctrl Pts',(173.503550155705,-2.96749230354208,331.075465751609));
#45518=CARTESIAN_POINT('Ctrl Pts',(173.495792344182,-3.07450310586851,331.161170267581));
#45519=CARTESIAN_POINT('Ctrl Pts',(173.488040370659,-3.18143337917254,331.246810288186));
#45520=CARTESIAN_POINT('Ctrl Pts',(173.480288397136,-3.28486586002153,331.336988101208));
#45521=CARTESIAN_POINT('Ctrl Pts',(173.472536423613,-3.38439784141672,331.43138201631));
#45522=CARTESIAN_POINT('Ctrl Pts',(173.464787733056,-3.4838876709588,331.525735955534));
#45523=CARTESIAN_POINT('Ctrl Pts',(173.457039042498,-3.57948000346481,331.624302177149));
#45524=CARTESIAN_POINT('Ctrl Pts',(173.449290351941,-3.67080627633533,331.726719635577));
#45525=CARTESIAN_POINT('Ctrl Pts',(173.441543273563,-3.76211354801196,331.829115785198));
#45526=CARTESIAN_POINT('Ctrl Pts',(173.433796195185,-3.84915626555285,331.935361286274));
#45527=CARTESIAN_POINT('Ctrl Pts',(173.426049116807,-3.93160400293221,332.045059556162));
#45528=CARTESIAN_POINT('Ctrl Pts',(173.418301973501,-4.01405243130296,332.154758745428));
#45529=CARTESIAN_POINT('Ctrl Pts',(173.410554830196,-4.09190556785868,332.267910448764));
#45530=CARTESIAN_POINT('Ctrl Pts',(173.40280768689,-4.16487467600814,332.384086775972));
#45531=CARTESIAN_POINT('Ctrl Pts',(173.395058801862,-4.2378601891622,332.500289222084));
#45532=CARTESIAN_POINT('Ctrl Pts',(173.387309916834,-4.30595928108932,332.619517314258));
#45533=CARTESIAN_POINT('Ctrl Pts',(173.379561031806,-4.36892797651213,332.741316445681));
#45534=CARTESIAN_POINT('Ctrl Pts',(173.371803922031,-4.43196350755898,332.863244855962));
#45535=CARTESIAN_POINT('Ctrl Pts',(173.364046812256,-4.48985758450184,332.987749409016));
#45536=CARTESIAN_POINT('Ctrl Pts',(173.356289702482,-4.54241319656434,333.114352786395));
#45537=CARTESIAN_POINT('Ctrl Pts',(173.348528447556,-4.59499689266553,333.24102381657));
#45538=CARTESIAN_POINT('Ctrl Pts',(173.340767192629,-4.64223630506473,333.369795539072));
#45539=CARTESIAN_POINT('Ctrl Pts',(173.333005937703,-4.68398391869246,333.500174106128));
#45540=CARTESIAN_POINT('Ctrl Pts',(173.325232267299,-4.72579831489646,333.6307612364));
#45541=CARTESIAN_POINT('Ctrl Pts',(173.317458596894,-4.76210325355548,333.762959970584));
#45542=CARTESIAN_POINT('Ctrl Pts',(173.309684926489,-4.79280188391725,333.896263997136));
#45543=CARTESIAN_POINT('Ctrl Pts',(173.302273122312,-4.82207148565075,334.023362689183));
#45544=CARTESIAN_POINT('Ctrl Pts',(173.294861318135,-4.84624492692439,334.151465803835));
#45545=CARTESIAN_POINT('Ctrl Pts',(173.287449513958,-4.86528225838518,334.28013083915));
#45546=CARTESIAN_POINT('Ctrl Pts',(173.273811758802,-4.90031103937786,334.516875119869));
#45547=CARTESIAN_POINT('Ctrl Pts',(173.260174003646,-4.91806575156673,334.756236763849));
#45548=CARTESIAN_POINT('Ctrl Pts',(173.24653624849,-4.91824857323717,334.996253755141));
#45549=CARTESIAN_POINT('',(176.746536248452,-4.91824967172903,335.001796952215));
#45550=CARTESIAN_POINT('Ctrl Pts',(176.746536248452,-4.91824967172903,335.001796952215));
#45551=CARTESIAN_POINT('Ctrl Pts',(176.738150524747,-4.91819529342756,335.150630104864));
#45552=CARTESIAN_POINT('Ctrl Pts',(176.729764801042,-4.91138089118401,335.299258443303));
#45553=CARTESIAN_POINT('Ctrl Pts',(176.721379077337,-4.89788709035797,335.447085129035));
#45554=CARTESIAN_POINT('Ctrl Pts',(176.712958450813,-4.88433712601955,335.595527094777));
#45555=CARTESIAN_POINT('Ctrl Pts',(176.704537824288,-4.86405212912126,335.743160447532));
#45556=CARTESIAN_POINT('Ctrl Pts',(176.696117197763,-4.8371644110477,335.889395032027));
#45557=CARTESIAN_POINT('Ctrl Pts',(176.687678931725,-4.81022036862904,336.035935948474));
#45558=CARTESIAN_POINT('Ctrl Pts',(176.679240665686,-4.77664603317014,336.181071971229));
#45559=CARTESIAN_POINT('Ctrl Pts',(176.670802399648,-4.73662377549646,336.324227424539));
#45560=CARTESIAN_POINT('Ctrl Pts',(176.66233646536,-4.69647028875198,336.467852270588));
#45561=CARTESIAN_POINT('Ctrl Pts',(176.653870531072,-4.64982665521896,336.60948328444));
#45562=CARTESIAN_POINT('Ctrl Pts',(176.645404596783,-4.59692468450908,336.748561267857));
#45563=CARTESIAN_POINT('Ctrl Pts',(176.639038372937,-4.55714339446076,336.853145303639));
#45564=CARTESIAN_POINT('Ctrl Pts',(176.632672149091,-4.51382416144281,336.95628609718));
#45565=CARTESIAN_POINT('Ctrl Pts',(176.626305925245,-4.46708249308073,337.05775534564));
#45566=CARTESIAN_POINT('Ctrl Pts',(176.618530846466,-4.40999682306017,337.181679891722));
#45567=CARTESIAN_POINT('Ctrl Pts',(176.610755767688,-4.34766021946007,337.303422980626));
#45568=CARTESIAN_POINT('Ctrl Pts',(176.602980688909,-4.28026160395896,337.422507722212));
#45569=CARTESIAN_POINT('Ctrl Pts',(176.59521517786,-4.21294592674504,337.541445922442));
#45570=CARTESIAN_POINT('Ctrl Pts',(176.587449666811,-4.14058082249508,337.657731947315));
#45571=CARTESIAN_POINT('Ctrl Pts',(176.579684155762,-4.06340294269931,337.770909523561));
#45572=CARTESIAN_POINT('Ctrl Pts',(176.571926344239,-3.98630158499605,337.883974883911));
#45573=CARTESIAN_POINT('Ctrl Pts',(176.564168532717,-3.90439716685733,337.993937608203));
#45574=CARTESIAN_POINT('Ctrl Pts',(176.556410721194,-3.81797167250749,338.10036697351));
#45575=CARTESIAN_POINT('Ctrl Pts',(176.548658747671,-3.73161121608271,338.206716247345));
#45576=CARTESIAN_POINT('Ctrl Pts',(176.540906774148,-3.64073670087276,338.309537152526));
#45577=CARTESIAN_POINT('Ctrl Pts',(176.533154800625,-3.54567253044435,338.408429164491));
#45578=CARTESIAN_POINT('Ctrl Pts',(176.525406110067,-3.45064861974863,338.50727929563));
#45579=CARTESIAN_POINT('Ctrl Pts',(176.517657419509,-3.35143885315349,338.602203561708));
#45580=CARTESIAN_POINT('Ctrl Pts',(176.509908728951,-3.24840675790063,338.692835847655));
#45581=CARTESIAN_POINT('Ctrl Pts',(176.502161650573,-3.1453960993357,338.783449276798));
#45582=CARTESIAN_POINT('Ctrl Pts',(176.494414572195,-3.03856498725729,338.869772244013));
#45583=CARTESIAN_POINT('Ctrl Pts',(176.486667493817,-2.92831222752099,338.951477010012));
#45584=CARTESIAN_POINT('Ctrl Pts',(176.478920350511,-2.81805854376046,339.033182460775));
#45585=CARTESIAN_POINT('Ctrl Pts',(176.471173207205,-2.70438346918492,339.110269400398));
#45586=CARTESIAN_POINT('Ctrl Pts',(176.463426063899,-2.58771683484811,339.18245198958));
#45587=CARTESIAN_POINT('Ctrl Pts',(176.455677178871,-2.47102397137492,339.254650806941));
#45588=CARTESIAN_POINT('Ctrl Pts',(176.447928293843,-2.35133854214129,339.32194287419));
#45589=CARTESIAN_POINT('Ctrl Pts',(176.440179408815,-2.2291167918094,339.384087292809));
#45590=CARTESIAN_POINT('Ctrl Pts',(176.43242229904,-2.1067653140489,339.446297672157));
#45591=CARTESIAN_POINT('Ctrl Pts',(176.424665189265,-1.98187248648536,339.50334931105));
#45592=CARTESIAN_POINT('Ctrl Pts',(176.41690807949,-1.85491694762461,339.555048427834));
#45593=CARTESIAN_POINT('Ctrl Pts',(176.409146824564,-1.72789356778323,339.606775170973));
#45594=CARTESIAN_POINT('Ctrl Pts',(176.401385569637,-1.59880564799407,339.653143560695));
#45595=CARTESIAN_POINT('Ctrl Pts',(176.393624314711,-1.46814802133065,339.694009421589));
#45596=CARTESIAN_POINT('Ctrl Pts',(176.385850644306,-1.33728138504572,339.734940654542));
#45597=CARTESIAN_POINT('Ctrl Pts',(176.378076973901,-1.2048404019347,339.770351668144));
#45598=CARTESIAN_POINT('Ctrl Pts',(176.370303303496,-1.07133202628335,339.800149034349));
#45599=CARTESIAN_POINT('Ctrl Pts',(176.362891499321,-0.944038497675528,
339.828559325979));
#45600=CARTESIAN_POINT('Ctrl Pts',(176.355479695146,-0.815774997577205,
339.851866787858));
#45601=CARTESIAN_POINT('Ctrl Pts',(176.348067890971,-0.686984287717369,
339.870034460959));
#45602=CARTESIAN_POINT('Ctrl Pts',(176.340292812193,-0.551881161484992,
339.889092585842));
#45603=CARTESIAN_POINT('Ctrl Pts',(176.332517733414,-0.415770887673747,
339.902554577005));
#45604=CARTESIAN_POINT('Ctrl Pts',(176.324742654636,-0.279156729737768,
339.910321230097));
#45605=CARTESIAN_POINT('Ctrl Pts',(176.316977143587,-0.142710684220461,
339.918078325828));
#45606=CARTESIAN_POINT('Ctrl Pts',(176.309211632538,-0.00576237483657899,
339.920154006373));
#45607=CARTESIAN_POINT('Ctrl Pts',(176.301446121489,0.131176442785312,339.916500361371));
#45608=CARTESIAN_POINT('Ctrl Pts',(176.293688309967,0.267979485170984,339.912850338968));
#45609=CARTESIAN_POINT('Ctrl Pts',(176.285930498445,0.404772666305083,339.903482306176));
#45610=CARTESIAN_POINT('Ctrl Pts',(176.278172686923,0.541041184245535,339.888400300656));
#45611=CARTESIAN_POINT('Ctrl Pts',(176.2704207134,0.677207155804843,339.873329644822));
#45612=CARTESIAN_POINT('Ctrl Pts',(176.262668739877,0.812848863114032,339.852553617917));
#45613=CARTESIAN_POINT('Ctrl Pts',(176.254916766354,0.94745394314014,339.826128270998));
#45614=CARTESIAN_POINT('Ctrl Pts',(176.247168075796,1.08200201783484,339.799714115229));
#45615=CARTESIAN_POINT('Ctrl Pts',(176.239419385239,1.21551395565618,339.767655473082));
#45616=CARTESIAN_POINT('Ctrl Pts',(176.231670694681,1.3474851571824,339.730059916499));
#45617=CARTESIAN_POINT('Ctrl Pts',(176.223923616303,1.47942890099786,339.692472181986));
#45618=CARTESIAN_POINT('Ctrl Pts',(176.216176537926,1.60983217045877,339.649349931471));
#45619=CARTESIAN_POINT('Ctrl Pts',(176.208429459548,1.7382035458745,339.600851170774));
#45620=CARTESIAN_POINT('Ctrl Pts',(176.200682316242,1.86657599716592,339.55235200361));
#45621=CARTESIAN_POINT('Ctrl Pts',(176.192935172936,1.99291615479683,339.498476374529));
#45622=CARTESIAN_POINT('Ctrl Pts',(176.185188029631,2.11675104415547,339.439431053589));
#45623=CARTESIAN_POINT('Ctrl Pts',(176.177439144603,2.24061377422634,339.380372458006));
#45624=CARTESIAN_POINT('Ctrl Pts',(176.169690259575,2.36196976249369,339.316142025998));
#45625=CARTESIAN_POINT('Ctrl Pts',(176.161941374547,2.48036953208909,339.246993059423));
#45626=CARTESIAN_POINT('Ctrl Pts',(176.154184264772,2.59889497242325,339.17777069742));
#45627=CARTESIAN_POINT('Ctrl Pts',(176.146427154997,2.71445758805366,339.103619569682));
#45628=CARTESIAN_POINT('Ctrl Pts',(176.138670045223,2.82663540509307,339.024837307168));
#45629=CARTESIAN_POINT('Ctrl Pts',(176.130908790297,2.93887316637111,338.946012945932));
#45630=CARTESIAN_POINT('Ctrl Pts',(176.12314753537,3.04772221497418,338.862552756513));
#45631=CARTESIAN_POINT('Ctrl Pts',(176.115386280444,3.15279352815466,338.774794833011));
#45632=CARTESIAN_POINT('Ctrl Pts',(176.10761261004,3.25803292119363,338.686896525432));
#45633=CARTESIAN_POINT('Ctrl Pts',(176.099838939635,3.35948221341567,338.594687008579));
#45634=CARTESIAN_POINT('Ctrl Pts',(176.092065269231,3.45678849712969,338.498542031849));
#45635=CARTESIAN_POINT('Ctrl Pts',(176.084653465053,3.54956514993692,338.406872626906));
#45636=CARTESIAN_POINT('Ctrl Pts',(176.077241660875,3.63857563156937,338.311626118262));
#45637=CARTESIAN_POINT('Ctrl Pts',(176.069829856697,3.72354925861636,338.213154833051));
#45638=CARTESIAN_POINT('Ctrl Pts',(176.062054777919,3.81268769623886,338.109857176832));
#45639=CARTESIAN_POINT('Ctrl Pts',(176.05427969914,3.89766525097212,338.002684199664));
#45640=CARTESIAN_POINT('Ctrl Pts',(176.046504620362,3.97812615503005,337.892005421358));
#45641=CARTESIAN_POINT('Ctrl Pts',(176.038739109313,4.05848804682317,337.781462840335));
#45642=CARTESIAN_POINT('Ctrl Pts',(176.030973598264,4.1343441191766,337.667423355154));
#45643=CARTESIAN_POINT('Ctrl Pts',(176.023208087215,4.20537714291025,337.550291384997));
#45644=CARTESIAN_POINT('Ctrl Pts',(176.015450275693,4.27633973719405,337.433275551528));
#45645=CARTESIAN_POINT('Ctrl Pts',(176.00769246417,4.34248859806439,337.313173667076));
#45646=CARTESIAN_POINT('Ctrl Pts',(175.999934652648,4.4035485320052,337.190420824585));
#45647=CARTESIAN_POINT('Ctrl Pts',(175.992182679125,4.46456251640938,337.067760357501));
#45648=CARTESIAN_POINT('Ctrl Pts',(175.984430705602,4.52049502309245,336.942453251748));
#45649=CARTESIAN_POINT('Ctrl Pts',(175.976678732079,4.57111591754807,336.814960696775));
#45650=CARTESIAN_POINT('Ctrl Pts',(175.968930041521,4.62171537402483,336.687522134975));
#45651=CARTESIAN_POINT('Ctrl Pts',(175.961181350964,4.66700754837085,336.557900327318));
#45652=CARTESIAN_POINT('Ctrl Pts',(175.953432660406,4.70680983242573,336.426577815571));
#45653=CARTESIAN_POINT('Ctrl Pts',(175.945685582028,4.74660383528297,336.29528262657));
#45654=CARTESIAN_POINT('Ctrl Pts',(175.937938503651,4.78091010649549,336.16228781114));
#45655=CARTESIAN_POINT('Ctrl Pts',(175.930191425273,4.8095955811343,336.028092120597));
#45656=CARTESIAN_POINT('Ctrl Pts',(175.922444281967,4.83828129618499,335.893895305365));
#45657=CARTESIAN_POINT('Ctrl Pts',(175.914697138661,4.86134603899531,335.758497977184));
#45658=CARTESIAN_POINT('Ctrl Pts',(175.906949995355,4.87870773321556,335.622409765639));
#45659=CARTESIAN_POINT('Ctrl Pts',(175.899201110327,4.89607333071325,335.486290958575));
#45660=CARTESIAN_POINT('Ctrl Pts',(175.891452225299,4.90773327879709,335.349481346722));
#45661=CARTESIAN_POINT('Ctrl Pts',(175.883703340271,4.91365734668025,335.212495980939));
#45662=CARTESIAN_POINT('Ctrl Pts',(175.875946230496,4.91958770243027,335.075365217474));
#45663=CARTESIAN_POINT('Ctrl Pts',(175.868189120722,4.91976999946911,334.938058718559));
#45664=CARTESIAN_POINT('Ctrl Pts',(175.860432010947,4.91422616773608,334.801092396229));
#45665=CARTESIAN_POINT('Ctrl Pts',(175.852670756021,4.90867937355664,334.664052883476));
#45666=CARTESIAN_POINT('Ctrl Pts',(175.844909501095,4.89740038568387,334.527354298872));
#45667=CARTESIAN_POINT('Ctrl Pts',(175.837148246168,4.8804629921296,334.391506742064));
#45668=CARTESIAN_POINT('Ctrl Pts',(175.829374575764,4.86349850426553,334.255441873438));
#45669=CARTESIAN_POINT('Ctrl Pts',(175.821600905359,4.8408575875193,334.120231138731));
#45670=CARTESIAN_POINT('Ctrl Pts',(175.813827234954,4.81266523897367,333.986374645111));
#45671=CARTESIAN_POINT('Ctrl Pts',(175.806415430777,4.78578525103527,333.858749203471));
#45672=CARTESIAN_POINT('Ctrl Pts',(175.7990036266,4.75385910895547,333.732355039452));
#45673=CARTESIAN_POINT('Ctrl Pts',(175.791591822423,4.71703660981305,333.607610440939));
#45674=CARTESIAN_POINT('Ctrl Pts',(175.783816743645,4.67840933029932,333.476751738058));
#45675=CARTESIAN_POINT('Ctrl Pts',(175.776041664866,4.63427151824114,333.347294851836));
#45676=CARTESIAN_POINT('Ctrl Pts',(175.768266586088,4.58474138436665,333.219738923367));
#45677=CARTESIAN_POINT('Ctrl Pts',(175.760501075039,4.53527220047513,333.092339960588));
#45678=CARTESIAN_POINT('Ctrl Pts',(175.75273556399,4.48042403783168,332.966837662012));
#45679=CARTESIAN_POINT('Ctrl Pts',(175.744970052941,4.42036531024096,332.843717646847));
#45680=CARTESIAN_POINT('Ctrl Pts',(175.737212241418,4.36036613105347,332.720719705536));
#45681=CARTESIAN_POINT('Ctrl Pts',(175.729454429896,4.29516683839358,332.600099696084));
#45682=CARTESIAN_POINT('Ctrl Pts',(175.721696618374,4.22498438819908,332.482324488348));
#45683=CARTESIAN_POINT('Ctrl Pts',(175.713944644851,4.15485475252395,332.36463791019));
#45684=CARTESIAN_POINT('Ctrl Pts',(175.706192671328,4.07974962275891,332.249792207009));
#45685=CARTESIAN_POINT('Ctrl Pts',(175.698440697805,3.99993228396393,332.138230479895));
#45686=CARTESIAN_POINT('Ctrl Pts',(175.690692007247,3.92014874785933,332.026715999238));
#45687=CARTESIAN_POINT('Ctrl Pts',(175.682943316689,3.83565719884264,331.918483045743));
#45688=CARTESIAN_POINT('Ctrl Pts',(175.675194626132,3.74676459682838,331.813946309546));
#45689=CARTESIAN_POINT('Ctrl Pts',(175.667447547754,3.65789048966241,331.709431323091));
#45690=CARTESIAN_POINT('Ctrl Pts',(175.659700469376,3.56461740389315,331.608611321866));
#45691=CARTESIAN_POINT('Ctrl Pts',(175.651953390998,3.46729274107458,331.511868105964));
#45692=CARTESIAN_POINT('Ctrl Pts',(175.644206247692,3.36996726258167,331.415124079261));
#45693=CARTESIAN_POINT('Ctrl Pts',(175.636459104387,3.26859041652813,331.322457181591));
#45694=CARTESIAN_POINT('Ctrl Pts',(175.628711961081,3.16354634508102,331.234212222519));
#45695=CARTESIAN_POINT('Ctrl Pts',(175.620963076053,3.0584786574965,331.145947424106));
#45696=CARTESIAN_POINT('Ctrl Pts',(175.613214191025,2.94974240313968,331.062106793901));
#45697=CARTESIAN_POINT('Ctrl Pts',(175.605465305996,2.83775433965222,330.98299447719));
#45698=CARTESIAN_POINT('Ctrl Pts',(175.597708196222,2.72564741087706,330.903798189849));
#45699=CARTESIAN_POINT('Ctrl Pts',(175.589951086447,2.61028209802139,330.829340467172));
#45700=CARTESIAN_POINT('Ctrl Pts',(175.582193976672,2.49210411006948,330.75988205741));
#45701=CARTESIAN_POINT('Ctrl Pts',(175.574432721746,2.37386297157946,330.690386531295));
#45702=CARTESIAN_POINT('Ctrl Pts',(175.56667146682,2.25280650792318,330.625895824932));
#45703=CARTESIAN_POINT('Ctrl Pts',(175.558910211894,2.12940360370253,330.566623932595));
#45704=CARTESIAN_POINT('Ctrl Pts',(175.551136541489,2.005803295052,330.507257224547));
#45705=CARTESIAN_POINT('Ctrl Pts',(175.543362871084,1.87984940445537,330.453126167522));
#45706=CARTESIAN_POINT('Ctrl Pts',(175.53558920068,1.75203012579135,330.40439628549));
#45707=CARTESIAN_POINT('Ctrl Pts',(175.528177396503,1.63016086530532,330.357934791191));
#45708=CARTESIAN_POINT('Ctrl Pts',(175.520765592326,1.50659624888517,330.316383030537));
#45709=CARTESIAN_POINT('Ctrl Pts',(175.513353788149,1.3817690875308,330.279841395541));
#45710=CARTESIAN_POINT('Ctrl Pts',(175.505578709371,1.25082377515307,330.241508746162));
#45711=CARTESIAN_POINT('Ctrl Pts',(175.497803630592,1.11807521495644,330.208568624591));
#45712=CARTESIAN_POINT('Ctrl Pts',(175.490028551814,0.984007115942841,330.181191738793));
#45713=CARTESIAN_POINT('Ctrl Pts',(175.482263040765,0.850103996260252,330.153848541996));
#45714=CARTESIAN_POINT('Ctrl Pts',(175.474497529716,0.714884947920567,330.132055037017));
#45715=CARTESIAN_POINT('Ctrl Pts',(175.466732018667,0.578849476850443,330.115932397514));
#45716=CARTESIAN_POINT('Ctrl Pts',(175.458974207145,0.442948885345953,330.099825743656));
#45717=CARTESIAN_POINT('Ctrl Pts',(175.451216395622,0.306233867690224,330.08937881153));
#45718=CARTESIAN_POINT('Ctrl Pts',(175.4434585841,0.169214432013063,330.084661808329));
#45719=CARTESIAN_POINT('Ctrl Pts',(175.435706610577,0.0322981078065591,
330.079948354823));
#45720=CARTESIAN_POINT('Ctrl Pts',(175.427954637054,-0.104921789370491,
330.080956260904));
#45721=CARTESIAN_POINT('Ctrl Pts',(175.420202663531,-0.241930167705256,
330.087703911972));
#45722=CARTESIAN_POINT('Ctrl Pts',(175.412453972974,-0.378880522910594,
330.094448705406));
#45723=CARTESIAN_POINT('Ctrl Pts',(175.404705282416,-0.515619147850069,
330.106928389981));
#45724=CARTESIAN_POINT('Ctrl Pts',(175.396956591859,-0.651631207117099,
330.125109249182));
#45725=CARTESIAN_POINT('Ctrl Pts',(175.389209513481,-0.787614967939216,
330.143286325704));
#45726=CARTESIAN_POINT('Ctrl Pts',(175.381462435103,-0.922872076587738,
330.167162165707));
#45727=CARTESIAN_POINT('Ctrl Pts',(175.373715356725,-1.05689347030419,330.196651245753));
#45728=CARTESIAN_POINT('Ctrl Pts',(175.365968213419,-1.19091598724888,330.226140572945));
#45729=CARTESIAN_POINT('Ctrl Pts',(175.358221070114,-1.32370238686213,330.261243150017));
#45730=CARTESIAN_POINT('Ctrl Pts',(175.350473926808,-1.45475483005692,330.301822539864));
#45731=CARTESIAN_POINT('Ctrl Pts',(175.34272504178,-1.58583673662319,330.34241105282));
#45732=CARTESIAN_POINT('Ctrl Pts',(175.334976156752,-1.7151835377412,330.388478713116));
#45733=CARTESIAN_POINT('Ctrl Pts',(175.327227271723,-1.84231393967725,330.439839650827));
#45734=CARTESIAN_POINT('Ctrl Pts',(175.319470161949,-1.96957927913551,330.491255103567));
#45735=CARTESIAN_POINT('Ctrl Pts',(175.311713052174,-2.0946231570666,330.547974910234));
#45736=CARTESIAN_POINT('Ctrl Pts',(175.303955942399,-2.21698510599749,330.609765370474));
#45737=CARTESIAN_POINT('Ctrl Pts',(175.296194687473,-2.3394124412415,330.671588849561));
#45738=CARTESIAN_POINT('Ctrl Pts',(175.288433432547,-2.45915465077377,330.738488190786));
#45739=CARTESIAN_POINT('Ctrl Pts',(175.280672177621,-2.57577804188075,330.810184903666));
#45740=CARTESIAN_POINT('Ctrl Pts',(175.272898507216,-2.69258799240602,330.881996307921));
#45741=CARTESIAN_POINT('Ctrl Pts',(175.265124836812,-2.80626883052823,330.958620200636));
#45742=CARTESIAN_POINT('Ctrl Pts',(175.257351166407,-2.91641717388945,331.039735623681));
#45743=CARTESIAN_POINT('Ctrl Pts',(175.24993936223,-3.0214380853683,331.117075104269));
#45744=CARTESIAN_POINT('Ctrl Pts',(175.242527558053,-3.12324775145683,331.198497184425));
#45745=CARTESIAN_POINT('Ctrl Pts',(175.235115753875,-3.22152753150027,331.283692232028));
#45746=CARTESIAN_POINT('Ctrl Pts',(175.227453993813,-3.32312170152013,331.371760399735));
#45747=CARTESIAN_POINT('Ctrl Pts',(175.21979223375,-3.42128496967472,331.464156638968));
#45748=CARTESIAN_POINT('Ctrl Pts',(175.212130473687,-3.51561789539192,331.560579427273));
#45749=CARTESIAN_POINT('Ctrl Pts',(175.204478209541,-3.60983390571463,331.656882710026));
#45750=CARTESIAN_POINT('Ctrl Pts',(175.196825945396,-3.70022873512071,331.757202332378));
#45751=CARTESIAN_POINT('Ctrl Pts',(175.189173681251,-3.78643552622414,331.861196236104));
#45752=CARTESIAN_POINT('Ctrl Pts',(175.181147121554,-3.87685895410756,331.970276798476));
#45753=CARTESIAN_POINT('Ctrl Pts',(175.173120561857,-3.96267393582545,332.083399904661));
#45754=CARTESIAN_POINT('Ctrl Pts',(175.16509400216,-4.04349958118173,332.200126038643));
#45755=CARTESIAN_POINT('Ctrl Pts',(175.157455179504,-4.1204208020118,332.311213512045));
#45756=CARTESIAN_POINT('Ctrl Pts',(175.149816356847,-4.19282314218833,332.425563705027));
#45757=CARTESIAN_POINT('Ctrl Pts',(175.142177534191,-4.26041931293051,332.542763678335));
#45758=CARTESIAN_POINT('Ctrl Pts',(175.134541627137,-4.32798968342031,332.659918918504));
#45759=CARTESIAN_POINT('Ctrl Pts',(175.126905720083,-4.39075733081347,332.779921427516));
#45760=CARTESIAN_POINT('Ctrl Pts',(175.119269813029,-4.44847898427495,332.902330390895));
#45761=CARTESIAN_POINT('Ctrl Pts',(175.111635055533,-4.50619194795037,333.024720926047));
#45762=CARTESIAN_POINT('Ctrl Pts',(175.104000298038,-4.55886025722331,333.149516830151));
#45763=CARTESIAN_POINT('Ctrl Pts',(175.096365540542,-4.60628745153904,333.27625437599));
#45764=CARTESIAN_POINT('Ctrl Pts',(175.08873016777,-4.65371846795447,333.403002135453));
#45765=CARTESIAN_POINT('Ctrl Pts',(175.081094794998,-4.69590738979103,333.531691469616));
#45766=CARTESIAN_POINT('Ctrl Pts',(175.073459422227,-4.73270678457583,333.661840983392));
#45767=CARTESIAN_POINT('Ctrl Pts',(175.065818297401,-4.76953390192671,333.792088544391));
#45768=CARTESIAN_POINT('Ctrl Pts',(175.058177172575,-4.80096327696741,333.923798092651));
#45769=CARTESIAN_POINT('Ctrl Pts',(175.050536047748,-4.8268980031814,334.056475368958));
#45770=CARTESIAN_POINT('Ctrl Pts',(175.042891561909,-4.85284413700427,334.189211004488));
#45771=CARTESIAN_POINT('Ctrl Pts',(175.035247076069,-4.87329074815301,334.322914817622));
#45772=CARTESIAN_POINT('Ctrl Pts',(175.02760259023,-4.88819266699765,334.457086090793));
#45773=CARTESIAN_POINT('Ctrl Pts',(175.019949266185,-4.90311181476041,334.591412486664));
#45774=CARTESIAN_POINT('Ctrl Pts',(175.01229594214,-4.91247344731158,334.726207020056));
#45775=CARTESIAN_POINT('Ctrl Pts',(175.004642618094,-4.91628447297953,334.860967474164));
#45776=CARTESIAN_POINT('Ctrl Pts',(175.001940494904,-4.91763001392046,334.908546715035));
#45777=CARTESIAN_POINT('Ctrl Pts',(174.999238371714,-4.91828411700569,334.956121738744));
#45778=CARTESIAN_POINT('Ctrl Pts',(174.996536248523,-4.91824863027879,335.003670594061));
#45779=CARTESIAN_POINT('',(178.49653624852,-4.91824801907883,334.995585781249));
#45780=CARTESIAN_POINT('Ctrl Pts',(178.49653624849,-4.9182480190793,334.995585781775));
#45781=CARTESIAN_POINT('Ctrl Pts',(178.488851432236,-4.91836997075314,335.131462294372));
#45782=CARTESIAN_POINT('Ctrl Pts',(178.481166615983,-4.9128568937543,335.267459173279));
#45783=CARTESIAN_POINT('Ctrl Pts',(178.473481799729,-4.90170571785073,335.403068378925));
#45784=CARTESIAN_POINT('Ctrl Pts',(178.465800244587,-4.8905592740358,335.538620037746));
#45785=CARTESIAN_POINT('Ctrl Pts',(178.458118689445,-4.87377952071571,335.67378395427));
#45786=CARTESIAN_POINT('Ctrl Pts',(178.450437134304,-4.8514154582341,335.808053905446));
#45787=CARTESIAN_POINT('Ctrl Pts',(178.442757111446,-4.82905585684227,335.942297073014));
#45788=CARTESIAN_POINT('Ctrl Pts',(178.435077088589,-4.80111422662373,336.075646237142));
#45789=CARTESIAN_POINT('Ctrl Pts',(178.427397065732,-4.76769116346065,336.207602597032));
#45790=CARTESIAN_POINT('Ctrl Pts',(178.419716841635,-4.7342672245123,336.339562414578));
#45791=CARTESIAN_POINT('Ctrl Pts',(178.412036617538,-4.69536166472711,336.470128969166));
#45792=CARTESIAN_POINT('Ctrl Pts',(178.404356393441,-4.65112558195678,336.598816400769));
#45793=CARTESIAN_POINT('Ctrl Pts',(178.396674234723,-4.60687835627982,336.727536248262));
#45794=CARTESIAN_POINT('Ctrl Pts',(178.388992076006,-4.55729806644526,336.854375654774));
#45795=CARTESIAN_POINT('Ctrl Pts',(178.381309917289,-4.50258461379164,336.978867064294));
#45796=CARTESIAN_POINT('Ctrl Pts',(178.373619516441,-4.4478124594802,337.103492039724));
#45797=CARTESIAN_POINT('Ctrl Pts',(178.365929115592,-4.38789630542493,337.225763622743));
#45798=CARTESIAN_POINT('Ctrl Pts',(178.358238714744,-4.32308302785332,337.345236916984));
#45799=CARTESIAN_POINT('Ctrl Pts',(178.350543892233,-4.25823248533059,337.464778903424));
#45800=CARTESIAN_POINT('Ctrl Pts',(178.342849069723,-4.18847941623002,337.581519055833));
#45801=CARTESIAN_POINT('Ctrl Pts',(178.335154247212,-4.11411436898883,337.69504100551));
#45802=CARTESIAN_POINT('Ctrl Pts',(178.32744756894,-4.03963474415269,337.808737863594));
#45803=CARTESIAN_POINT('Ctrl Pts',(178.319740890669,-3.96052918114889,337.919206292991));
#45804=CARTESIAN_POINT('Ctrl Pts',(178.312034212397,-3.8771292477966,338.026062104184));
#45805=CARTESIAN_POINT('Ctrl Pts',(178.306600851894,-3.81833064639821,338.101397563062));
#45806=CARTESIAN_POINT('Ctrl Pts',(178.301167491391,-3.75739835439175,338.174938069751));
#45807=CARTESIAN_POINT('Ctrl Pts',(178.295734130888,-3.69445924923038,338.246560321059));
#45808=CARTESIAN_POINT('Ctrl Pts',(178.287959052102,-3.60439408585605,338.349050970533));
#45809=CARTESIAN_POINT('Ctrl Pts',(178.280183973316,-3.50991847046176,338.447952891543));
#45810=CARTESIAN_POINT('Ctrl Pts',(178.27240889453,-3.41134951540899,338.542862902544));
#45811=CARTESIAN_POINT('Ctrl Pts',(178.264643383473,-3.31290185572934,338.637656120734));
#45812=CARTESIAN_POINT('Ctrl Pts',(178.256877872416,-3.21037115768049,338.72846693446));
#45813=CARTESIAN_POINT('Ctrl Pts',(178.24911236136,-3.10411439888144,338.814925538088));
#45814=CARTESIAN_POINT('Ctrl Pts',(178.24135454983,-2.9979629939665,338.90129841776));
#45815=CARTESIAN_POINT('Ctrl Pts',(178.2335967383,-2.88809318160164,338.983327429775));
#45816=CARTESIAN_POINT('Ctrl Pts',(178.225838926769,-2.77489809983399,339.060680189086));
#45817=CARTESIAN_POINT('Ctrl Pts',(178.218086953239,-2.66178820095424,339.137974737994));
#45818=CARTESIAN_POINT('Ctrl Pts',(178.210334979708,-2.54535833493829,339.210599819007));
#45819=CARTESIAN_POINT('Ctrl Pts',(178.202583006177,-2.42603368200257,339.278264091461));
#45820=CARTESIAN_POINT('Ctrl Pts',(178.194834315611,-2.3067595631265,339.345899708057));
#45821=CARTESIAN_POINT('Ctrl Pts',(178.187085625045,-2.18459343495103,339.40857850224));
#45822=CARTESIAN_POINT('Ctrl Pts',(178.17933693448,-2.05998815984202,339.466053273732));
#45823=CARTESIAN_POINT('Ctrl Pts',(178.171589856094,-1.93540880990023,339.523516087118));
#45824=CARTESIAN_POINT('Ctrl Pts',(178.163842777708,-1.80839167716165,339.575776867847));
#45825=CARTESIAN_POINT('Ctrl Pts',(178.156095699322,-1.67941248940075,339.622635260644));
#45826=CARTESIAN_POINT('Ctrl Pts',(178.148348556008,-1.55043222066922,339.669494046159));
#45827=CARTESIAN_POINT('Ctrl Pts',(178.140601412694,-1.41949023149725,339.710950219963));
#45828=CARTESIAN_POINT('Ctrl Pts',(178.13285426938,-1.28708003305147,339.746852436196));
#45829=CARTESIAN_POINT('Ctrl Pts',(178.125105384344,-1.15464006598175,339.78276272401));
#45830=CARTESIAN_POINT('Ctrl Pts',(178.117356499308,-1.02073160998556,339.813116467314));
#45831=CARTESIAN_POINT('Ctrl Pts',(178.109607614271,-0.885860672215242,
339.837812928579));
#45832=CARTESIAN_POINT('Ctrl Pts',(178.101850504489,-0.750846581037659,
339.862535602922));
#45833=CARTESIAN_POINT('Ctrl Pts',(178.094093394706,-0.614868352456746,
339.881588929765));
#45834=CARTESIAN_POINT('Ctrl Pts',(178.086336284923,-0.478440016111392,
339.894923718863));
#45835=CARTESIAN_POINT('Ctrl Pts',(178.078575029988,-0.341938776824875,
339.908265633645));
#45836=CARTESIAN_POINT('Ctrl Pts',(178.070813775054,-0.204987340582888,
339.915882900022));
#45837=CARTESIAN_POINT('Ctrl Pts',(178.06305252012,-0.0681011076885268,
339.917778492534));
#45838=CARTESIAN_POINT('Ctrl Pts',(178.055278849707,0.0690040985662645,
339.919677117377));
#45839=CARTESIAN_POINT('Ctrl Pts',(178.047505179294,0.206043502116605,339.915835789281));
#45840=CARTESIAN_POINT('Ctrl Pts',(178.039731508881,0.342504561618265,339.906309579284));
#45841=CARTESIAN_POINT('Ctrl Pts',(178.032319704792,0.472613324282115,339.897226816772));
#45842=CARTESIAN_POINT('Ctrl Pts',(178.024907900704,0.60219608894837,339.882976555734));
#45843=CARTESIAN_POINT('Ctrl Pts',(178.017496096615,0.73081794824608,339.863649677868));
#45844=CARTESIAN_POINT('Ctrl Pts',(178.009721017839,0.865743949582712,339.843375531909));
#45845=CARTESIAN_POINT('Ctrl Pts',(178.001945939062,1.0000388612588,339.817450475875));
#45846=CARTESIAN_POINT('Ctrl Pts',(177.994170860286,1.13319203161789,339.785922991647));
#45847=CARTESIAN_POINT('Ctrl Pts',(177.986405349239,1.26618134852352,339.754434303996));
#45848=CARTESIAN_POINT('Ctrl Pts',(177.978639838193,1.39803134290858,339.717356994719));
#45849=CARTESIAN_POINT('Ctrl Pts',(177.970874327146,1.5282378562543,339.674791130865));
#45850=CARTESIAN_POINT('Ctrl Pts',(177.963116515626,1.6583152694632,339.632267471188));
#45851=CARTESIAN_POINT('Ctrl Pts',(177.955358704106,1.7867520753299,339.58426620733));
#45852=CARTESIAN_POINT('Ctrl Pts',(177.947600892586,1.91305601462299,339.53093806484));
#45853=CARTESIAN_POINT('Ctrl Pts',(177.939848919065,2.03926490619641,339.477650053468));
#45854=CARTESIAN_POINT('Ctrl Pts',(177.932096945544,2.1633437673262,339.419043293903));
#45855=CARTESIAN_POINT('Ctrl Pts',(177.924344972023,2.28481751402039,339.355317668107));
#45856=CARTESIAN_POINT('Ctrl Pts',(177.916596281468,2.40623981651021,339.291619030152));
#45857=CARTESIAN_POINT('Ctrl Pts',(177.908847590913,2.52505885347051,339.222806018859));
#45858=CARTESIAN_POINT('Ctrl Pts',(177.901098900357,2.64082167910272,339.149125681596));
#45859=CARTESIAN_POINT('Ctrl Pts',(177.893351821982,2.75656041931198,339.075460674144));
#45860=CARTESIAN_POINT('Ctrl Pts',(177.885604743606,2.86924388344247,338.996930564775));
#45861=CARTESIAN_POINT('Ctrl Pts',(177.87785766523,2.97844614487324,338.913826979389));
#45862=CARTESIAN_POINT('Ctrl Pts',(177.870110521927,3.08764932152388,338.830722697514));
#45863=CARTESIAN_POINT('Ctrl Pts',(177.862363378623,3.19337092623292,338.743045099879));
#45864=CARTESIAN_POINT('Ctrl Pts',(177.85461623532,3.29521662182914,338.651127288622));
#45865=CARTESIAN_POINT('Ctrl Pts',(177.846867350294,3.3970852145003,338.559188812289));
#45866=CARTESIAN_POINT('Ctrl Pts',(177.839118465268,3.49507587398259,338.463008487228));
#45867=CARTESIAN_POINT('Ctrl Pts',(177.831369580242,3.5888300584333,338.362957310788));
#45868=CARTESIAN_POINT('Ctrl Pts',(177.82361247047,3.68268375454419,338.262799938996));
#45869=CARTESIAN_POINT('Ctrl Pts',(177.815855360697,3.7722917254758,338.158763794259));
#45870=CARTESIAN_POINT('Ctrl Pts',(177.808098250925,3.85733443517002,338.0512545154));
#45871=CARTESIAN_POINT('Ctrl Pts',(177.800336996001,3.94242258896909,337.943687787021));
#45872=CARTESIAN_POINT('Ctrl Pts',(177.792575741077,4.02294039121272,337.83264454269));
#45873=CARTESIAN_POINT('Ctrl Pts',(177.784814486153,4.09861143057847,337.71855980321));
#45874=CARTESIAN_POINT('Ctrl Pts',(177.77704081575,4.17440351894647,337.604292565327));
#45875=CARTESIAN_POINT('Ctrl Pts',(177.769267145348,4.24533314882702,337.486974444453));
#45876=CARTESIAN_POINT('Ctrl Pts',(177.761493474945,4.31116926509982,337.367066249634));
#45877=CARTESIAN_POINT('Ctrl Pts',(177.754081670744,4.37394069454455,337.252739809726));
#45878=CARTESIAN_POINT('Ctrl Pts',(177.746669866542,4.43208201639745,337.136059262717));
#45879=CARTESIAN_POINT('Ctrl Pts',(177.739258062341,4.48543430167461,337.017439512813));
#45880=CARTESIAN_POINT('Ctrl Pts',(177.731482983563,4.54140154119123,336.89300585604));
#45881=CARTESIAN_POINT('Ctrl Pts',(177.723707904786,4.59227529104021,336.766044864336));
#45882=CARTESIAN_POINT('Ctrl Pts',(177.715932826008,4.63781997775631,336.637012191899));
#45883=CARTESIAN_POINT('Ctrl Pts',(177.70816731496,4.68330861883573,336.50813830238));
#45884=CARTESIAN_POINT('Ctrl Pts',(177.700401803912,4.72348111597075,336.377198169639));
#45885=CARTESIAN_POINT('Ctrl Pts',(177.692636292864,4.75814878857253,336.24466990335));
#45886=CARTESIAN_POINT('Ctrl Pts',(177.684878481343,4.79278208807592,336.112273039224));
#45887=CARTESIAN_POINT('Ctrl Pts',(177.677120669822,4.8219213265913,335.978291550884));
#45888=CARTESIAN_POINT('Ctrl Pts',(177.6693628583,4.8454268627324,335.843220955866));
#45889=CARTESIAN_POINT('Ctrl Pts',(177.661610884778,4.86891471021218,335.708252005753));
#45890=CARTESIAN_POINT('Ctrl Pts',(177.653858911256,4.88677722716964,335.572195963845));
#45891=CARTESIAN_POINT('Ctrl Pts',(177.646106937734,4.89892540340302,335.435560506006));
#45892=CARTESIAN_POINT('Ctrl Pts',(177.638358247178,4.9110684348765,335.298982913366));
#45893=CARTESIAN_POINT('Ctrl Pts',(177.630609556621,4.91750190434473,335.161826781371));
#45894=CARTESIAN_POINT('Ctrl Pts',(177.622860866064,4.91818844424897,335.024606693316));
#45895=CARTESIAN_POINT('Ctrl Pts',(177.615113787687,4.91887484131284,334.887415155045));
#45896=CARTESIAN_POINT('Ctrl Pts',(177.607366709311,4.91381668518364,334.750160077805));
#45897=CARTESIAN_POINT('Ctrl Pts',(177.599619630934,4.90302871696604,334.613357447885));
#45898=CARTESIAN_POINT('Ctrl Pts',(177.591872487629,4.89224065833493,334.476553671427));
#45899=CARTESIAN_POINT('Ctrl Pts',(177.584125344324,4.87572272256143,334.340202739516));
#45900=CARTESIAN_POINT('Ctrl Pts',(177.576378201019,4.85354162387011,334.204816519374));
#45901=CARTESIAN_POINT('Ctrl Pts',(177.568629315992,4.83135553839694,334.069399861536));
#45902=CARTESIAN_POINT('Ctrl Pts',(177.560880430965,4.80350381966597,333.934948732704));
#45903=CARTESIAN_POINT('Ctrl Pts',(177.553131545938,4.77010441969993,333.801965406318));
#45904=CARTESIAN_POINT('Ctrl Pts',(177.545374436164,4.73666956926564,333.668840930055));
#45905=CARTESIAN_POINT('Ctrl Pts',(177.537617326391,4.69767537039572,333.53718774807));
#45906=CARTESIAN_POINT('Ctrl Pts',(177.529860216617,4.65329001413586,333.407494079495));
#45907=CARTESIAN_POINT('Ctrl Pts',(177.522098961692,4.60888093976079,333.27773110677));
#45908=CARTESIAN_POINT('Ctrl Pts',(177.514337706767,4.55907510947838,333.149930097909));
#45909=CARTESIAN_POINT('Ctrl Pts',(177.506576451842,4.50408875953656,333.024558907809));
#45910=CARTESIAN_POINT('Ctrl Pts',(177.498802781438,4.44901444935495,332.898987164663));
#45911=CARTESIAN_POINT('Ctrl Pts',(177.491029111034,4.38874323128088,332.77585335875));
#45912=CARTESIAN_POINT('Ctrl Pts',(177.483255440631,4.32353757229044,332.655601159467));
#45913=CARTESIAN_POINT('Ctrl Pts',(177.475843636443,4.26136725231417,332.540946728808));
#45914=CARTESIAN_POINT('Ctrl Pts',(177.468431832255,4.19471169657706,332.428911911962));
#45915=CARTESIAN_POINT('Ctrl Pts',(177.461020028067,4.12383380128391,332.319854884174));
#45916=CARTESIAN_POINT('Ctrl Pts',(177.453244949287,4.04948196930619,332.20545264674));
#45917=CARTESIAN_POINT('Ctrl Pts',(177.445469870508,3.97024846794033,332.093965947486));
#45918=CARTESIAN_POINT('Ctrl Pts',(177.437694791728,3.88638898420485,331.985839465796));
#45919=CARTESIAN_POINT('Ctrl Pts',(177.429929280678,3.80263269490266,331.877846040626));
#45920=CARTESIAN_POINT('Ctrl Pts',(177.422163769628,3.71426198706275,331.773204911548));
#45921=CARTESIAN_POINT('Ctrl Pts',(177.414398258578,3.62157680741814,331.672333476673));
#45922=CARTESIAN_POINT('Ctrl Pts',(177.406640447055,3.52898352539915,331.57156205612));
#45923=CARTESIAN_POINT('Ctrl Pts',(177.398882635531,3.43208454742217,331.474553177578));
#45924=CARTESIAN_POINT('Ctrl Pts',(177.391124824008,3.33122099678566,331.381692421439));
#45925=CARTESIAN_POINT('Ctrl Pts',(177.383372850484,3.23043334916917,331.288901545963));
#45926=CARTESIAN_POINT('Ctrl Pts',(177.37562087696,3.12568735374209,331.200252843189));
#45927=CARTESIAN_POINT('Ctrl Pts',(177.367868903435,3.01736175744166,331.116095896237));
#45928=CARTESIAN_POINT('Ctrl Pts',(177.360120212877,2.90908203709536,331.031974589801));
#45929=CARTESIAN_POINT('Ctrl Pts',(177.352371522318,2.79722603904751,330.952341495026));
#45930=CARTESIAN_POINT('Ctrl Pts',(177.344622831759,2.68220626563671,330.877506505635));
#45931=CARTESIAN_POINT('Ctrl Pts',(177.33687575338,2.56721042305009,330.802687086289));
#45932=CARTESIAN_POINT('Ctrl Pts',(177.329128675001,2.44905244183251,330.732663999698));
#45933=CARTESIAN_POINT('Ctrl Pts',(177.321381596622,2.3281742031205,330.667704079541));
#45934=CARTESIAN_POINT('Ctrl Pts',(177.313634453315,2.20729495133221,330.602743614958));
#45935=CARTESIAN_POINT('Ctrl Pts',(177.305887310008,2.08369574088242,330.542846586477));
#45936=CARTESIAN_POINT('Ctrl Pts',(177.298140166701,1.95784311473272,330.488233893408));
#45937=CARTESIAN_POINT('Ctrl Pts',(177.290391281671,1.83196219424135,330.433608922246));
#45938=CARTESIAN_POINT('Ctrl Pts',(177.282642396642,1.70382720844067,330.384270806113));
#45939=CARTESIAN_POINT('Ctrl Pts',(177.274893511613,1.57392436038893,330.340392165614));
#45940=CARTESIAN_POINT('Ctrl Pts',(177.267136401837,1.44388363211172,330.296466951872));
#45941=CARTESIAN_POINT('Ctrl Pts',(177.259379292061,1.31207166414775,330.258012914593));
#45942=CARTESIAN_POINT('Ctrl Pts',(177.251622182285,1.17899002820679,330.225152821724));
#45943=CARTESIAN_POINT('Ctrl Pts',(177.243860927358,1.04583727769469,330.192275169473));
#45944=CARTESIAN_POINT('Ctrl Pts',(177.23609967243,0.911413890165617,330.164997495625));
#45945=CARTESIAN_POINT('Ctrl Pts',(177.228338417503,0.776230312625155,330.143391145639));
#45946=CARTESIAN_POINT('Ctrl Pts',(177.220564747097,0.640830485416796,330.121750232533));
#45947=CARTESIAN_POINT('Ctrl Pts',(177.212791076691,0.504668426580055,330.105798817874));
#45948=CARTESIAN_POINT('Ctrl Pts',(177.205017406285,0.368259263117793,330.095556282551));
#45949=CARTESIAN_POINT('Ctrl Pts',(177.197605602121,0.238199979280686,330.085790539729));
#45950=CARTESIAN_POINT('Ctrl Pts',(177.190193797957,0.107916366155344,330.081214150661));
#45951=CARTESIAN_POINT('Ctrl Pts',(177.182781993793,-0.0221481108367294,
330.081799869496));
#45952=CARTESIAN_POINT('Ctrl Pts',(177.175006915015,-0.158587435520085,
330.082414296158));
#45953=CARTESIAN_POINT('Ctrl Pts',(177.167231836237,-0.295216773365073,
330.088711587753));
#45954=CARTESIAN_POINT('Ctrl Pts',(177.159456757459,-0.431523817072754,
330.100717373145));
#45955=CARTESIAN_POINT('Ctrl Pts',(177.15169124641,-0.567663126285112,330.112708384655));
#45956=CARTESIAN_POINT('Ctrl Pts',(177.143925735362,-0.703480544842646,
330.130393878924));
#45957=CARTESIAN_POINT('Ctrl Pts',(177.136160224313,-0.83846275538047,330.153747502416));
#45958=CARTESIAN_POINT('Ctrl Pts',(177.128402412791,-0.973311130663834,
330.177077970722));
#45959=CARTESIAN_POINT('Ctrl Pts',(177.120644601269,-1.10732556324428,330.206065317992));
#45960=CARTESIAN_POINT('Ctrl Pts',(177.112886789748,-1.23999720895503,330.240631346041));
#45961=CARTESIAN_POINT('Ctrl Pts',(177.105134816225,-1.37256901504501,330.275171362058));
#45962=CARTESIAN_POINT('Ctrl Pts',(177.097382842702,-1.50379966887132,330.315281604522));
#45963=CARTESIAN_POINT('Ctrl Pts',(177.08963086918,-1.63319023683207,330.360832756537));
#45964=CARTESIAN_POINT('Ctrl Pts',(177.081882178623,-1.76252600781031,330.406364617613));
#45965=CARTESIAN_POINT('Ctrl Pts',(177.074133488065,-1.89002287492386,330.457332675765));
#45966=CARTESIAN_POINT('Ctrl Pts',(177.066384797508,-2.01519701324465,330.513557750254));
#45967=CARTESIAN_POINT('Ctrl Pts',(177.058637719131,-2.14034510804055,330.569771126646));
#45968=CARTESIAN_POINT('Ctrl Pts',(177.050890640753,-2.26317107895541,330.631239183739));
#45969=CARTESIAN_POINT('Ctrl Pts',(177.043143562376,-2.38321141261797,330.697734733275));
#45970=CARTESIAN_POINT('Ctrl Pts',(177.03539641907,-2.50325275233455,330.764230840108));
#45971=CARTESIAN_POINT('Ctrl Pts',(177.027649275765,-2.62050806631345,330.83575433402));
#45972=CARTESIAN_POINT('Ctrl Pts',(177.01990213246,-2.7345391224461,330.912032430374));
#45973=CARTESIAN_POINT('Ctrl Pts',(177.012153247432,-2.84859581518041,330.988327675663));
#45974=CARTESIAN_POINT('Ctrl Pts',(177.004404362404,-2.95942648281034,331.069379433174));
#45975=CARTESIAN_POINT('Ctrl Pts',(176.996655477376,-3.06662285261261,331.154872259296));
#45976=CARTESIAN_POINT('Ctrl Pts',(176.988898367602,-3.17393300174964,331.240455828387));
#45977=CARTESIAN_POINT('Ctrl Pts',(176.981141257828,-3.27760084130692,331.330489638237));
#45978=CARTESIAN_POINT('Ctrl Pts',(176.973384148053,-3.37725170386577,331.424618343276));
#45979=CARTESIAN_POINT('Ctrl Pts',(176.965622893128,-3.47695581665924,331.518797347686));
#45980=CARTESIAN_POINT('Ctrl Pts',(176.957861638202,-3.57263840274313,331.617075327511));
#45981=CARTESIAN_POINT('Ctrl Pts',(176.950100383276,-3.66396323403733,331.719061646095));
#45982=CARTESIAN_POINT('Ctrl Pts',(176.942326712872,-3.75543415529907,331.821211109552));
#45983=CARTESIAN_POINT('Ctrl Pts',(176.934553042468,-3.84253314321025,331.927080463919));
#45984=CARTESIAN_POINT('Ctrl Pts',(176.926779372063,-3.92496513518874,332.03624701602));
#45985=CARTESIAN_POINT('Ctrl Pts',(176.919367567882,-4.00355989815917,332.140331838923));
#45986=CARTESIAN_POINT('Ctrl Pts',(176.9119557637,-4.07791222027853,332.247413562207));
#45987=CARTESIAN_POINT('Ctrl Pts',(176.904543959519,-4.14780502857619,332.357104522041));
#45988=CARTESIAN_POINT('Ctrl Pts',(176.896578469935,-4.22291905248635,332.474989746292));
#45989=CARTESIAN_POINT('Ctrl Pts',(176.88861298035,-4.29311033714613,332.596246708684));
#45990=CARTESIAN_POINT('Ctrl Pts',(176.880647490766,-4.35807046888413,332.720437574722));
#45991=CARTESIAN_POINT('Ctrl Pts',(176.872693252424,-4.42293884453604,332.844453021352));
#45992=CARTESIAN_POINT('Ctrl Pts',(176.864739014081,-4.48259061177193,332.97139379955));
#45993=CARTESIAN_POINT('Ctrl Pts',(176.856784775739,-4.53676066080434,333.100793384311));
#45994=CARTESIAN_POINT('Ctrl Pts',(176.848840386968,-4.59086363216895,333.230032736202));
#45995=CARTESIAN_POINT('Ctrl Pts',(176.840895998197,-4.63949826263529,333.361724496742));
#45996=CARTESIAN_POINT('Ctrl Pts',(176.832951609425,-4.68244544840857,333.495377892899));
#45997=CARTESIAN_POINT('Ctrl Pts',(176.825017922654,-4.72533477941262,333.62885124265));
#45998=CARTESIAN_POINT('Ctrl Pts',(176.817084235883,-4.76255182620758,333.764280614637));
#45999=CARTESIAN_POINT('Ctrl Pts',(176.809150549112,-4.79392586400262,333.901156119848));
#46000=CARTESIAN_POINT('Ctrl Pts',(176.801223146645,-4.82527505029799,334.037923205429));
#46001=CARTESIAN_POINT('Ctrl Pts',(176.793295744179,-4.85079036196863,334.176133788734));
#46002=CARTESIAN_POINT('Ctrl Pts',(176.785368341712,-4.8703509690766,334.315263188871));
#46003=CARTESIAN_POINT('Ctrl Pts',(176.777446779236,-4.88989716619812,334.454290094604));
#46004=CARTESIAN_POINT('Ctrl Pts',(176.769525216761,-4.90349734986709,334.594234107436));
#46005=CARTESIAN_POINT('Ctrl Pts',(176.761603654285,-4.91108187582924,334.734560983649));
#46006=CARTESIAN_POINT('Ctrl Pts',(176.756581185687,-4.91589065485409,334.823531730446));
#46007=CARTESIAN_POINT('Ctrl Pts',(176.751558717088,-4.91828224055931,334.912656185423));
#46008=CARTESIAN_POINT('Ctrl Pts',(176.74653624849,-4.91824967172928,335.001796951547));
#46009=CARTESIAN_POINT('',(180.24653624852,-4.91824998793836,335.000344447839));
#46010=CARTESIAN_POINT('Ctrl Pts',(180.24653624849,-4.91824998793832,335.000344448365));
#46011=CARTESIAN_POINT('Ctrl Pts',(180.245490955929,-4.9182487032425,335.018688141735));
#46012=CARTESIAN_POINT('Ctrl Pts',(180.244445663368,-4.91814479377736,335.037031417793));
#46013=CARTESIAN_POINT('Ctrl Pts',(180.243400370807,-4.91793827065545,335.055373536301));
#46014=CARTESIAN_POINT('Ctrl Pts',(180.235625292529,-4.91640211369949,335.191805586485));
#46015=CARTESIAN_POINT('Ctrl Pts',(180.227850214252,-4.90918193865282,335.328389254008));
#46016=CARTESIAN_POINT('Ctrl Pts',(180.220075135975,-4.89625557816743,335.464612070188));
#46017=CARTESIAN_POINT('Ctrl Pts',(180.212309625435,-4.88334512440573,335.60066725537));
#46018=CARTESIAN_POINT('Ctrl Pts',(180.204544114896,-4.86474249320673,335.736362087336));
#46019=CARTESIAN_POINT('Ctrl Pts',(180.196778604356,-4.84047750526045,335.871183438529));
#46020=CARTESIAN_POINT('Ctrl Pts',(180.18902079335,-4.81623657614479,336.005871113824));
#46021=CARTESIAN_POINT('Ctrl Pts',(180.181262982344,-4.78634453174525,336.139686649638));
#46022=CARTESIAN_POINT('Ctrl Pts',(180.173505171339,-4.75088300599652,336.27212174175));
#46023=CARTESIAN_POINT('Ctrl Pts',(180.165753198339,-4.71544816620316,336.404457172133));
#46024=CARTESIAN_POINT('Ctrl Pts',(180.158001225339,-4.67445228816595,336.5354138505));
#46025=CARTESIAN_POINT('Ctrl Pts',(180.15024925234,-4.62802805641185,336.664493728304));
#46026=CARTESIAN_POINT('Ctrl Pts',(180.142500562314,-4.58162348539915,336.79351894056));
#46027=CARTESIAN_POINT('Ctrl Pts',(180.134751872288,-4.52979526506278,336.920668566067));
#46028=CARTESIAN_POINT('Ctrl Pts',(180.127003182262,-4.47272584056937,337.045460001467));
#46029=CARTESIAN_POINT('Ctrl Pts',(180.119256104421,-4.41566828988442,337.170225472885));
#46030=CARTESIAN_POINT('Ctrl Pts',(180.11150902658,-4.35337186654326,337.292633374876));
#46031=CARTESIAN_POINT('Ctrl Pts',(180.103761948739,-4.28606688491897,337.412221739497));
#46032=CARTESIAN_POINT('Ctrl Pts',(180.096014805974,-4.21876133925372,337.531811106313));
#46033=CARTESIAN_POINT('Ctrl Pts',(180.08826766321,-4.14644734329543,337.648580547998));
#46034=CARTESIAN_POINT('Ctrl Pts',(180.080520520445,-4.06940063596396,337.762093685326));
#46035=CARTESIAN_POINT('Ctrl Pts',(180.072771635962,-3.99233660693642,337.875632342758));
#46036=CARTESIAN_POINT('Ctrl Pts',(180.06502275148,-3.91053796874405,337.985912915717));
#46037=CARTESIAN_POINT('Ctrl Pts',(180.057273866997,-3.82432291591003,338.092529271866));
#46038=CARTESIAN_POINT('Ctrl Pts',(180.049516757771,-3.73801635355931,338.199258791678));
#46039=CARTESIAN_POINT('Ctrl Pts',(180.041759648545,-3.64728425875788,338.30231602115));
#46040=CARTESIAN_POINT('Ctrl Pts',(180.034002539319,-3.5524845000535,338.401328702049));
#46041=CARTESIAN_POINT('Ctrl Pts',(180.026241284944,-3.45763408341873,338.500394292127));
#46042=CARTESIAN_POINT('Ctrl Pts',(180.01848003057,-3.35871195348679,338.595410756462));
#46043=CARTESIAN_POINT('Ctrl Pts',(180.010718776195,-3.25611100940342,338.686044513695));
#46044=CARTESIAN_POINT('Ctrl Pts',(180.002945106341,-3.15334593722364,338.776823255423));
#46045=CARTESIAN_POINT('Ctrl Pts',(179.995171436487,-3.04689059479092,338.863205033769));
#46046=CARTESIAN_POINT('Ctrl Pts',(179.987397766633,-2.93716965893771,338.944897648497));
#46047=CARTESIAN_POINT('Ctrl Pts',(179.979985956599,-2.83255616897477,339.022787519417));
#46048=CARTESIAN_POINT('Ctrl Pts',(179.972574146566,-2.72497450279379,339.096414793428));
#46049=CARTESIAN_POINT('Ctrl Pts',(179.965162336532,-2.6148137828259,339.165565020936));
#46050=CARTESIAN_POINT('Ctrl Pts',(179.95738725742,-2.49925384417118,339.238104452878));
#46051=CARTESIAN_POINT('Ctrl Pts',(179.949612178308,-2.38049045859568,339.305946120166));
#46052=CARTESIAN_POINT('Ctrl Pts',(179.941837099196,-2.25894257607548,339.368794055628));
#46053=CARTESIAN_POINT('Ctrl Pts',(179.934071587809,-2.1375442658974,339.431564652739));
#46054=CARTESIAN_POINT('Ctrl Pts',(179.926306076423,-2.01336862041317,339.489353567204));
#46055=CARTESIAN_POINT('Ctrl Pts',(179.918540565036,-1.88686327735886,339.541908193156));
#46056=CARTESIAN_POINT('Ctrl Pts',(179.910782753173,-1.76048336465994,339.594410711068));
#46057=CARTESIAN_POINT('Ctrl Pts',(179.90302494131,-1.63177870986369,339.641689119491));
#46058=CARTESIAN_POINT('Ctrl Pts',(179.895267129447,-1.50122093376931,339.68353699361));
#46059=CARTESIAN_POINT('Ctrl Pts',(179.88751515558,-1.37076140648656,339.725353375894));
#46060=CARTESIAN_POINT('Ctrl Pts',(179.879763181713,-1.23845190437485,339.761747239317));
#46061=CARTESIAN_POINT('Ctrl Pts',(179.872011207846,-1.10478305041207,339.792560638534));
#46062=CARTESIAN_POINT('Ctrl Pts',(179.864262516941,-0.971170805227721,
339.823360988272));
#46063=CARTESIAN_POINT('Ctrl Pts',(179.856513826036,-0.836200733283099,
339.848585486676));
#46064=CARTESIAN_POINT('Ctrl Pts',(179.848765135131,-0.700377397695667,
339.868126391467));
#46065=CARTESIAN_POINT('Ctrl Pts',(179.841018056404,-0.564582321251315,
339.887663230614));
#46066=CARTESIAN_POINT('Ctrl Pts',(179.833270977677,-0.427934720928508,
339.901518772632));
#46067=CARTESIAN_POINT('Ctrl Pts',(179.82552389895,-0.290947711851586,339.909636696485));
#46068=CARTESIAN_POINT('Ctrl Pts',(179.817776755293,-0.153959554662009,
339.917754688375));
#46069=CARTESIAN_POINT('Ctrl Pts',(179.810029611637,-0.0166323732341754,
339.920134943061));
#46070=CARTESIAN_POINT('Ctrl Pts',(179.80228246798,0.120517653584459,339.916773185502));
#46071=CARTESIAN_POINT('Ctrl Pts',(179.7945335826,0.257698514663268,339.913410672148));
#46072=CARTESIAN_POINT('Ctrl Pts',(179.786784697219,0.394701751198794,339.904303587325));
#46073=CARTESIAN_POINT('Ctrl Pts',(179.779035811839,0.531013644441538,339.889499726139));
#46074=CARTESIAN_POINT('Ctrl Pts',(179.771278701712,0.667470220532111,339.874680151983));
#46075=CARTESIAN_POINT('Ctrl Pts',(179.763521591584,0.803233598294663,339.854151765049));
#46076=CARTESIAN_POINT('Ctrl Pts',(179.755764481457,0.937797074547684,339.828014054399));
#46077=CARTESIAN_POINT('Ctrl Pts',(179.748003226178,1.07243245722768,339.80186237659));
#46078=CARTESIAN_POINT('Ctrl Pts',(179.740241970899,1.20586628071717,339.770095492868));
#46079=CARTESIAN_POINT('Ctrl Pts',(179.73248071562,1.3376054089815,339.732863280548));
#46080=CARTESIAN_POINT('Ctrl Pts',(179.724707044864,1.46955527686569,339.695571508838));
#46081=CARTESIAN_POINT('Ctrl Pts',(179.716933374109,1.59980466066831,339.652797059961));
#46082=CARTESIAN_POINT('Ctrl Pts',(179.709159703354,1.72787802589608,339.604738927467));
#46083=CARTESIAN_POINT('Ctrl Pts',(179.701747902989,1.84998947685191,339.558917938233));
#46084=CARTESIAN_POINT('Ctrl Pts',(179.694336102623,1.97012267446546,339.508294223313));
#46085=CARTESIAN_POINT('Ctrl Pts',(179.686924302258,2.0878867086058,339.4530789522));
#46086=CARTESIAN_POINT('Ctrl Pts',(179.67914922353,2.21142277158844,339.395157386761));
#46087=CARTESIAN_POINT('Ctrl Pts',(179.671374144803,2.3327419534251,339.331999744926));
#46088=CARTESIAN_POINT('Ctrl Pts',(179.663599066075,2.4513686511619,339.263798165791));
#46089=CARTESIAN_POINT('Ctrl Pts',(179.655833555076,2.56984937119489,339.19568051304));
#46090=CARTESIAN_POINT('Ctrl Pts',(179.648068044078,2.68564386396864,339.12253146587));
#46091=CARTESIAN_POINT('Ctrl Pts',(179.64030253308,2.79829746537685,339.044590752816));
#46092=CARTESIAN_POINT('Ctrl Pts',(179.632544721608,2.91083937041216,338.966727318205));
#46093=CARTESIAN_POINT('Ctrl Pts',(179.624786910136,3.02024626215157,338.884081893331));
#46094=CARTESIAN_POINT('Ctrl Pts',(179.617029098665,3.12608933250522,338.796939365818));
#46095=CARTESIAN_POINT('Ctrl Pts',(179.609277125192,3.23185275259354,338.709862415819));
#46096=CARTESIAN_POINT('Ctrl Pts',(179.601525151719,3.33405738892024,338.618295346733));
#46097=CARTESIAN_POINT('Ctrl Pts',(179.593773178247,3.43230491764391,338.522565260548));
#46098=CARTESIAN_POINT('Ctrl Pts',(179.586024487739,3.53051083848612,338.426875716106));
#46099=CARTESIAN_POINT('Ctrl Pts',(179.578275797231,3.62476270547678,338.327026933339));
#46100=CARTESIAN_POINT('Ctrl Pts',(179.570527106724,3.71469686779026,338.223384904558));
#46101=CARTESIAN_POINT('Ctrl Pts',(179.562780028395,3.80461231855318,338.119764439362));
#46102=CARTESIAN_POINT('Ctrl Pts',(179.555032950067,3.89021159547421,338.012352592995));
#46103=CARTESIAN_POINT('Ctrl Pts',(179.547285871739,3.97116966096564,337.901550376321));
#46104=CARTESIAN_POINT('Ctrl Pts',(179.539538728483,4.05212840496694,337.790747231012));
#46105=CARTESIAN_POINT('Ctrl Pts',(179.531791585226,4.12844562935505,337.676553974325));
#46106=CARTESIAN_POINT('Ctrl Pts',(179.52404444197,4.19983840517142,337.559402358549));
#46107=CARTESIAN_POINT('Ctrl Pts',(179.51629555699,4.27124723160302,337.442224404597));
#46108=CARTESIAN_POINT('Ctrl Pts',(179.508546672011,4.33772920304924,337.32208710179));
#46109=CARTESIAN_POINT('Ctrl Pts',(179.500797787032,4.39904650875091,337.199448311815));
#46110=CARTESIAN_POINT('Ctrl Pts',(179.493040677306,4.46042889728169,337.076679351747));
#46111=CARTESIAN_POINT('Ctrl Pts',(179.485283567579,4.5166354945222,336.951403950854));
#46112=CARTESIAN_POINT('Ctrl Pts',(179.477526457852,4.56747575678702,336.824102045847));
#46113=CARTESIAN_POINT('Ctrl Pts',(179.469765202974,4.61834318646519,336.696732114765));
#46114=CARTESIAN_POINT('Ctrl Pts',(179.462003948095,4.66383843763788,336.567333890356));
#46115=CARTESIAN_POINT('Ctrl Pts',(179.454242693217,4.70382068113828,336.436403168402));
#46116=CARTESIAN_POINT('Ctrl Pts',(179.446469022859,4.74386688320451,336.305262999943));
#46117=CARTESIAN_POINT('Ctrl Pts',(179.438695352501,4.77838235613106,336.172585813604));
#46118=CARTESIAN_POINT('Ctrl Pts',(179.430921682143,4.80727709884326,336.038879183273));
#46119=CARTESIAN_POINT('Ctrl Pts',(179.423509877423,4.83482678651144,335.911396618659));
#46120=CARTESIAN_POINT('Ctrl Pts',(179.416098072704,4.8572672072836,335.782978577792));
#46121=CARTESIAN_POINT('Ctrl Pts',(179.408686267984,4.87456439414474,335.654068062083));
#46122=CARTESIAN_POINT('Ctrl Pts',(179.40091118927,4.89270936618117,335.518839269012));
#46123=CARTESIAN_POINT('Ctrl Pts',(179.393136110556,4.9052515283151,335.382641157187));
#46124=CARTESIAN_POINT('Ctrl Pts',(179.385361031843,4.91209507835586,335.245977648765));
#46125=CARTESIAN_POINT('Ctrl Pts',(179.377595520859,4.91893020697159,335.109482313511));
#46126=CARTESIAN_POINT('Ctrl Pts',(179.369830009876,4.920080657008,334.972523107822));
#46127=CARTESIAN_POINT('Ctrl Pts',(179.362064498892,4.91550197646241,334.835612099307));
#46128=CARTESIAN_POINT('Ctrl Pts',(179.354306687437,4.91092783569256,334.698836838475));
#46129=CARTESIAN_POINT('Ctrl Pts',(179.346548875981,4.90063588173872,334.562110067858));
#46130=CARTESIAN_POINT('Ctrl Pts',(179.338791064526,4.88463363001364,334.425946550363));
#46131=CARTESIAN_POINT('Ctrl Pts',(179.33103909107,4.86864342049248,334.289885500251));
#46132=CARTESIAN_POINT('Ctrl Pts',(179.323287117615,4.84695151196733,334.154387246218));
#46133=CARTESIAN_POINT('Ctrl Pts',(179.31553514416,4.81961741558545,334.019963760933));
#46134=CARTESIAN_POINT('Ctrl Pts',(179.307786453671,4.79229489521391,333.885597204094));
#46135=CARTESIAN_POINT('Ctrl Pts',(179.300037763182,4.75933501720027,333.75230489295));
#46136=CARTESIAN_POINT('Ctrl Pts',(179.292289072693,4.72084875995142,333.620590688677));
#46137=CARTESIAN_POINT('Ctrl Pts',(179.284541994385,4.68237051009347,333.488903888656));
#46138=CARTESIAN_POINT('Ctrl Pts',(179.276794916077,4.6383682776122,333.358794917368));
#46139=CARTESIAN_POINT('Ctrl Pts',(179.269047837768,4.58900338460175,333.230754115841));
#46140=CARTESIAN_POINT('Ctrl Pts',(179.261300694533,4.53963807787014,333.10271224122));
#46141=CARTESIAN_POINT('Ctrl Pts',(179.253553551297,4.48491016157507,332.97673893564));
#46142=CARTESIAN_POINT('Ctrl Pts',(179.245806408061,4.42502959632726,332.853305766038));
#46143=CARTESIAN_POINT('Ctrl Pts',(179.238057523104,4.36513556866156,332.729844846047));
#46144=CARTESIAN_POINT('Ctrl Pts',(179.230308638147,4.30008675748139,332.608925550018));
#46145=CARTESIAN_POINT('Ctrl Pts',(179.222559753189,4.23013949539465,332.490995633323));
#46146=CARTESIAN_POINT('Ctrl Pts',(179.214802643486,4.16011799056537,332.372940544604));
#46147=CARTESIAN_POINT('Ctrl Pts',(179.207045533782,4.0851878485239,332.257881510219));
#46148=CARTESIAN_POINT('Ctrl Pts',(179.199288424079,4.00564954416337,332.146238483712));
#46149=CARTESIAN_POINT('Ctrl Pts',(179.191527169224,3.92606873707989,332.034535798748));
#46150=CARTESIAN_POINT('Ctrl Pts',(179.18376591437,3.84187510082044,331.926253067364));
#46151=CARTESIAN_POINT('Ctrl Pts',(179.176004659516,3.75340934988947,331.821777019361));
#46152=CARTESIAN_POINT('Ctrl Pts',(179.168230989183,3.66480208258636,331.717133843728));
#46153=CARTESIAN_POINT('Ctrl Pts',(179.16045731885,3.57190930926451,331.616309807623));
#46154=CARTESIAN_POINT('Ctrl Pts',(179.152683648517,3.47510915488219,331.519655272225));
#46155=CARTESIAN_POINT('Ctrl Pts',(179.145271843581,3.38281506068305,331.427500018427));
#46156=CARTESIAN_POINT('Ctrl Pts',(179.137860038646,3.28696938682149,331.339135016504));
#46157=CARTESIAN_POINT('Ctrl Pts',(179.130448233711,3.18792628116515,331.254828563556));
#46158=CARTESIAN_POINT('Ctrl Pts',(179.122673154881,3.08402878781031,331.166390008677));
#46159=CARTESIAN_POINT('Ctrl Pts',(179.114898076051,2.97628417163581,331.082138422369));
#46160=CARTESIAN_POINT('Ctrl Pts',(179.107122997222,2.8650643474924,331.002427067929));
#46161=CARTESIAN_POINT('Ctrl Pts',(179.099357486121,2.75398138641355,330.922813803378));
#46162=CARTESIAN_POINT('Ctrl Pts',(179.09159197502,2.63943204097068,330.847729879603));
#46163=CARTESIAN_POINT('Ctrl Pts',(179.083826463919,2.52182286423267,330.777489786403));
#46164=CARTESIAN_POINT('Ctrl Pts',(179.076068652345,2.40433029732672,330.707319336454));
#46165=CARTESIAN_POINT('Ctrl Pts',(179.06831084077,2.28378427004081,330.641983358621));
#46166=CARTESIAN_POINT('Ctrl Pts',(179.060553029195,2.1606217245274,330.581754100777));
#46167=CARTESIAN_POINT('Ctrl Pts',(179.05280105562,2.03755186272676,330.521570167355));
#46168=CARTESIAN_POINT('Ctrl Pts',(179.045049082044,1.91186975164524,330.466485475703));
#46169=CARTESIAN_POINT('Ctrl Pts',(179.037297108468,1.78403812493704,330.41672703941));
#46170=CARTESIAN_POINT('Ctrl Pts',(179.029548417857,1.65626063498904,330.366989675842));
#46171=CARTESIAN_POINT('Ctrl Pts',(179.021799727246,1.52633580347281,330.32257422275));
#46172=CARTESIAN_POINT('Ctrl Pts',(179.014051036635,1.39474739480084,330.283660024214));
#46173=CARTESIAN_POINT('Ctrl Pts',(179.006303958203,1.26318636419047,330.2447539221));
#46174=CARTESIAN_POINT('Ctrl Pts',(178.998556879771,1.1299628194759,330.211346908665));
#46175=CARTESIAN_POINT('Ctrl Pts',(178.99080980134,0.995576399546803,330.183568676378));
#46176=CARTESIAN_POINT('Ctrl Pts',(178.98306265798,0.861188853325156,330.155790211282));
#46177=CARTESIAN_POINT('Ctrl Pts',(178.97531551462,0.72563879523206,330.133640700551));
#46178=CARTESIAN_POINT('Ctrl Pts',(178.96756837126,0.589436397711769,330.117198775748));
#46179=CARTESIAN_POINT('Ctrl Pts',(178.959819486178,0.45320337899708,330.100753154452));
#46180=CARTESIAN_POINT('Ctrl Pts',(178.952070601095,0.316318116999823,330.090017719318));
#46181=CARTESIAN_POINT('Ctrl Pts',(178.944321716013,0.179295855061354,330.085019220907));
#46182=CARTESIAN_POINT('Ctrl Pts',(178.936564606184,0.0421281562781302,
330.080015417037));
#46183=CARTESIAN_POINT('Ctrl Pts',(178.928807496355,-0.0951764416912896,
330.080760727998));
#46184=CARTESIAN_POINT('Ctrl Pts',(178.921050386526,-0.232102186732936,
330.087229738995));
#46185=CARTESIAN_POINT('Ctrl Pts',(178.913289131545,-0.36910110051628,330.093702206825));
#46186=CARTESIAN_POINT('Ctrl Pts',(178.905527876564,-0.505720368851173,
330.105904434397));
#46187=CARTESIAN_POINT('Ctrl Pts',(178.897766621584,-0.64145040221728,330.123759189294));
#46188=CARTESIAN_POINT('Ctrl Pts',(178.889992951125,-0.777397559394959,
330.141642505979));
#46189=CARTESIAN_POINT('Ctrl Pts',(178.882219280666,-0.912452253790739,
330.165196351795));
#46190=CARTESIAN_POINT('Ctrl Pts',(178.874445610207,-1.04611523409038,330.194292353929));
#46191=CARTESIAN_POINT('Ctrl Pts',(178.867033806617,-1.17355615952385,330.222033927774));
#46192=CARTESIAN_POINT('Ctrl Pts',(178.859622003027,-1.29973174525168,330.254813221642));
#46193=CARTESIAN_POINT('Ctrl Pts',(178.852210199436,-1.42422472502374,330.292477616078));
#46194=CARTESIAN_POINT('Ctrl Pts',(178.844435120669,-1.55481948672895,330.331988057752));
#46195=CARTESIAN_POINT('Ctrl Pts',(178.836660041902,-1.68397523620287,330.376999435934));
#46196=CARTESIAN_POINT('Ctrl Pts',(178.828884963135,-1.81119364234137,330.427390170544));
#46197=CARTESIAN_POINT('Ctrl Pts',(178.821119452097,-1.93825549813117,330.477718896145));
#46198=CARTESIAN_POINT('Ctrl Pts',(178.813353941059,-2.06338439417958,330.533413664419));
#46199=CARTESIAN_POINT('Ctrl Pts',(178.805588430022,-2.18609586011521,330.594302784702));
#46200=CARTESIAN_POINT('Ctrl Pts',(178.797830618511,-2.30868565727432,330.655131533244));
#46201=CARTESIAN_POINT('Ctrl Pts',(178.790072807,-2.42886244638127,330.721144211956));
#46202=CARTESIAN_POINT('Ctrl Pts',(178.782314995489,-2.54616083392577,330.792120715814));
#46203=CARTESIAN_POINT('Ctrl Pts',(178.774563021977,-2.6633709507132,330.863043807602));
#46204=CARTESIAN_POINT('Ctrl Pts',(178.766811048466,-2.77770664435982,330.938923087794));
#46205=CARTESIAN_POINT('Ctrl Pts',(178.759059074954,-2.88872660256619,331.019492283876));
#46206=CARTESIAN_POINT('Ctrl Pts',(178.751310384408,-2.99969954375468,331.100027358855));
#46207=CARTESIAN_POINT('Ctrl Pts',(178.743561693862,-3.10735922669989,331.185248170248));
#46208=CARTESIAN_POINT('Ctrl Pts',(178.735813003315,-3.21129304446125,331.274844963616));
#46209=CARTESIAN_POINT('Ctrl Pts',(178.728065924949,-3.31520523792383,331.364423115624));
#46210=CARTESIAN_POINT('Ctrl Pts',(178.720318846582,-3.41539281225687,331.458375183585));
#46211=CARTESIAN_POINT('Ctrl Pts',(178.712571768216,-3.51147632302539,331.556351194542));
#46212=CARTESIAN_POINT('Ctrl Pts',(178.704824624921,-3.60756063906641,331.654328026633));
#46213=CARTESIAN_POINT('Ctrl Pts',(178.697077481627,-3.69954054925603,331.756328589914));
#46214=CARTESIAN_POINT('Ctrl Pts',(178.689330338332,-3.78707384705354,331.861966421553));
#46215=CARTESIAN_POINT('Ctrl Pts',(178.681581453316,-3.87462682419518,331.967628002819));
#46216=CARTESIAN_POINT('Ctrl Pts',(178.673832568299,-3.95773095032338,332.076928178727));
#46217=CARTESIAN_POINT('Ctrl Pts',(178.666083683282,-4.03608490258727,332.18944814643));
#46218=CARTESIAN_POINT('Ctrl Pts',(178.658326573518,-4.11452202054696,332.302087543991));
#46219=CARTESIAN_POINT('Ctrl Pts',(178.650569463755,-4.18819866928732,332.417953238892));
#46220=CARTESIAN_POINT('Ctrl Pts',(178.642812353991,-4.25685711759007,332.536597770781));
#46221=CARTESIAN_POINT('Ctrl Pts',(178.635051099076,-4.32555225477276,332.655305702515));
#46222=CARTESIAN_POINT('Ctrl Pts',(178.627289844161,-4.3892236669036,332.776795084044));
#46223=CARTESIAN_POINT('Ctrl Pts',(178.619528589246,-4.44766053224136,332.900595595784));
#46224=CARTESIAN_POINT('Ctrl Pts',(178.611754918852,-4.5061908775207,333.024594147999));
#46225=CARTESIAN_POINT('Ctrl Pts',(178.603981248459,-4.55946979114974,333.150910857898));
#46226=CARTESIAN_POINT('Ctrl Pts',(178.596207578065,-4.60733505103374,333.279056424511));
#46227=CARTESIAN_POINT('Ctrl Pts',(178.588795773764,-4.65297217238041,333.40123678638));
#46228=CARTESIAN_POINT('Ctrl Pts',(178.581383969463,-4.69368821862418,333.525079296806));
#46229=CARTESIAN_POINT('Ctrl Pts',(178.573972165163,-4.72938572398217,333.650150476426));
#46230=CARTESIAN_POINT('Ctrl Pts',(178.564222497849,-4.77634308915807,333.814672142449));
#46231=CARTESIAN_POINT('Ctrl Pts',(178.554472830535,-4.8147381632881,333.981738629569));
#46232=CARTESIAN_POINT('Ctrl Pts',(178.544723163222,-4.84434037783941,334.150559380454));
#46233=CARTESIAN_POINT('Ctrl Pts',(178.535124052667,-4.87348546771993,334.316773159823));
#46234=CARTESIAN_POINT('Ctrl Pts',(178.525524942111,-4.894107175471,334.48468753632));
#46235=CARTESIAN_POINT('Ctrl Pts',(178.515925831556,-4.90603092899386,334.653526932857));
#46236=CARTESIAN_POINT('Ctrl Pts',(178.509462637211,-4.91405933286542,334.767208489779));
#46237=CARTESIAN_POINT('Ctrl Pts',(178.502999442865,-4.91814545352143,334.881308968517));
#46238=CARTESIAN_POINT('Ctrl Pts',(178.49653624852,-4.91824801907883,334.995585781249));
#46239=CARTESIAN_POINT('',(181.996536248449,-4.91824818069158,335.004230321965));
#46240=CARTESIAN_POINT('Ctrl Pts',(181.996536248449,-4.91824818069158,335.004230321965));
#46241=CARTESIAN_POINT('Ctrl Pts',(181.987210597247,-4.91810625049596,335.169240912697));
#46242=CARTESIAN_POINT('Ctrl Pts',(181.977884946045,-4.90965625100552,335.333889388984));
#46243=CARTESIAN_POINT('Ctrl Pts',(181.968559294843,-4.8930298995958,335.497434884343));
#46244=CARTESIAN_POINT('Ctrl Pts',(181.959112154449,-4.87618694969273,335.663110955859));
#46245=CARTESIAN_POINT('Ctrl Pts',(181.949665014055,-4.85095328809792,335.827655110689));
#46246=CARTESIAN_POINT('Ctrl Pts',(181.940217873661,-4.81751501808247,335.990319197557));
#46247=CARTESIAN_POINT('Ctrl Pts',(181.931088107924,-4.78520009958176,336.147518619288));
#46248=CARTESIAN_POINT('Ctrl Pts',(181.921958342187,-4.74522291969737,336.302962321272));
#46249=CARTESIAN_POINT('Ctrl Pts',(181.91282857645,-4.69779351779615,336.45599420557));
#46250=CARTESIAN_POINT('Ctrl Pts',(181.905053524964,-4.65740189632902,336.586318554922));
#46251=CARTESIAN_POINT('Ctrl Pts',(181.897278473478,-4.61151922383854,336.715166790492));
#46252=CARTESIAN_POINT('Ctrl Pts',(181.889503421991,-4.56027043970645,336.842041416266));
#46253=CARTESIAN_POINT('Ctrl Pts',(181.881737938622,-4.50908472323853,336.968759907871));
#46254=CARTESIAN_POINT('Ctrl Pts',(181.873972455252,-4.45254617945793,337.093509263252));
#46255=CARTESIAN_POINT('Ctrl Pts',(181.866206971883,-4.39082976365685,337.21580618491));
#46256=CARTESIAN_POINT('Ctrl Pts',(181.858449188395,-4.32917454290447,337.337981842785));
#46257=CARTESIAN_POINT('Ctrl Pts',(181.850691404908,-4.26235184230619,337.457709559476));
#46258=CARTESIAN_POINT('Ctrl Pts',(181.84293362142,-4.19058490167554,337.57452544061));
#46259=CARTESIAN_POINT('Ctrl Pts',(181.835181676256,-4.11887197113864,337.691253408888));
#46260=CARTESIAN_POINT('Ctrl Pts',(181.827429731093,-4.04222241065873,337.805073571734));
#46261=CARTESIAN_POINT('Ctrl Pts',(181.819677785929,-3.96090546396482,337.915546427007));
#46262=CARTESIAN_POINT('Ctrl Pts',(181.811929124124,-3.87962295930347,338.025972491177));
#46263=CARTESIAN_POINT('Ctrl Pts',(181.804180462319,-3.79367723154422,338.133053753465));
#46264=CARTESIAN_POINT('Ctrl Pts',(181.796431800514,-3.70338081158259,338.236379709939));
#46265=CARTESIAN_POINT('Ctrl Pts',(181.788684751125,-3.61310318136283,338.33968416536));
#46266=CARTESIAN_POINT('Ctrl Pts',(181.780937701736,-3.51847691676246,338.439234575164));
#46267=CARTESIAN_POINT('Ctrl Pts',(181.773190652347,-3.41985454242128,338.534653868653));
#46268=CARTESIAN_POINT('Ctrl Pts',(181.765443538239,-3.32123134418514,338.630073959278));
#46269=CARTESIAN_POINT('Ctrl Pts',(181.757696424131,-3.2186122505378,338.721362592959));
#46270=CARTESIAN_POINT('Ctrl Pts',(181.749949310022,-3.11238602376485,338.808180182393));
#46271=CARTESIAN_POINT('Ctrl Pts',(181.742200454374,-3.00613591748659,338.895017288298));
#46272=CARTESIAN_POINT('Ctrl Pts',(181.734451598725,-2.89627736712124,338.977381102642));
#46273=CARTESIAN_POINT('Ctrl Pts',(181.726702743077,-2.78323119818521,339.054973139239));
#46274=CARTESIAN_POINT('Ctrl Pts',(181.718945662805,-2.67006504222195,339.132647531902));
#46275=CARTESIAN_POINT('Ctrl Pts',(181.711188582533,-2.55370483193987,339.205539807943));
#46276=CARTESIAN_POINT('Ctrl Pts',(181.703431502261,-2.43459975534441,339.273395265334));
#46277=CARTESIAN_POINT('Ctrl Pts',(181.695670276952,-2.31543103430932,339.341286981654));
#46278=CARTESIAN_POINT('Ctrl Pts',(181.687909051642,-2.19351487161421,339.404136337351));
#46279=CARTESIAN_POINT('Ctrl Pts',(181.680147826333,-2.06932299717013,339.46173569319));
#46280=CARTESIAN_POINT('Ctrl Pts',(181.672374185441,-1.94493245378691,339.519427190345));
#46281=CARTESIAN_POINT('Ctrl Pts',(181.66460054455,-1.81825928533402,339.571851755619));
#46282=CARTESIAN_POINT('Ctrl Pts',(181.656826903658,-1.68979387444757,339.618850476512));
#46283=CARTESIAN_POINT('Ctrl Pts',(181.649414783164,-1.56730286693722,339.663663478193));
#46284=CARTESIAN_POINT('Ctrl Pts',(181.64200266267,-1.44318284228606,339.703543866795));
#46285=CARTESIAN_POINT('Ctrl Pts',(181.634590542176,-1.31786798642013,339.738397095313));
#46286=CARTESIAN_POINT('Ctrl Pts',(181.626815450207,-1.1864164631764,339.774957086121));
#46287=CARTESIAN_POINT('Ctrl Pts',(181.619040358238,-1.05323471644738,339.806100655392));
#46288=CARTESIAN_POINT('Ctrl Pts',(181.611265266269,-0.918808719549712,
339.83166364717));
#46289=CARTESIAN_POINT('Ctrl Pts',(181.603499741899,-0.784548139855005,
339.857195182542));
#46290=CARTESIAN_POINT('Ctrl Pts',(181.595734217529,-0.649046736773575,
339.877159731758));
#46291=CARTESIAN_POINT('Ctrl Pts',(181.587968693158,-0.512805609667528,
339.891442882135));
#46292=CARTESIAN_POINT('Ctrl Pts',(181.580210868199,-0.376699563770435,
339.905711870965));
#46293=CARTESIAN_POINT('Ctrl Pts',(181.57245304324,-0.239855639646728,339.914310630511));
#46294=CARTESIAN_POINT('Ctrl Pts',(181.56469521828,-0.102784749130356,339.917175851833));
#46295=CARTESIAN_POINT('Ctrl Pts',(181.556943231219,0.0341829931588555,
339.920038917026));
#46296=CARTESIAN_POINT('Ctrl Pts',(181.549191244157,0.171376972665348,339.917177023835));
#46297=CARTESIAN_POINT('Ctrl Pts',(181.541439257096,0.308281894647593,339.908578749081));
#46298=CARTESIAN_POINT('Ctrl Pts',(181.533690552894,0.445128839282379,339.899984115578));
#46299=CARTESIAN_POINT('Ctrl Pts',(181.525941848693,0.581686580569214,339.885657956626));
#46300=CARTESIAN_POINT('Ctrl Pts',(181.518193144491,0.717440784221783,339.865640942737));
#46301=CARTESIAN_POINT('Ctrl Pts',(181.510446052407,0.853166744221293,339.845628093386));
#46302=CARTESIAN_POINT('Ctrl Pts',(181.502698960323,0.988089112662411,339.819926801105));
#46303=CARTESIAN_POINT('Ctrl Pts',(181.494951868238,1.12170002745138,339.788629460599));
#46304=CARTESIAN_POINT('Ctrl Pts',(181.487204711177,1.25531206287902,339.757331857592));
#46305=CARTESIAN_POINT('Ctrl Pts',(181.479457554115,1.38761224214373,339.720438201888));
#46306=CARTESIAN_POINT('Ctrl Pts',(181.471710397053,1.5181046137789,339.678091645546));
#46307=CARTESIAN_POINT('Ctrl Pts',(181.463961498233,1.64862632343256,339.635735568616));
#46308=CARTESIAN_POINT('Ctrl Pts',(181.456212599412,1.77733904496999,339.587924272167));
#46309=CARTESIAN_POINT('Ctrl Pts',(181.448463700592,1.90376403871786,339.534850113001));
#46310=CARTESIAN_POINT('Ctrl Pts',(181.440706577045,2.03032322069275,339.481719620612));
#46311=CARTESIAN_POINT('Ctrl Pts',(181.432949453498,2.15458946333378,339.423315258419));
#46312=CARTESIAN_POINT('Ctrl Pts',(181.425192329951,2.27610549761311,339.359876927877));
#46313=CARTESIAN_POINT('Ctrl Pts',(181.417431061242,2.39768646622964,339.296404697892));
#46314=CARTESIAN_POINT('Ctrl Pts',(181.409669792533,2.51651395967518,339.22789333464));
#46315=CARTESIAN_POINT('Ctrl Pts',(181.401908523823,2.63215808641805,339.15462716385));
#46316=CARTESIAN_POINT('Ctrl Pts',(181.394134839757,2.7479872039459,339.081243792414));
#46317=CARTESIAN_POINT('Ctrl Pts',(181.38636115569,2.86062245755833,339.003090637233));
#46318=CARTESIAN_POINT('Ctrl Pts',(181.378587471623,2.96966483711331,338.920494078265));
#46319=CARTESIAN_POINT('Ctrl Pts',(181.371175817049,3.07362898644098,338.841744136953));
#46320=CARTESIAN_POINT('Ctrl Pts',(181.363764162476,3.17432715178658,338.758955523226));
#46321=CARTESIAN_POINT('Ctrl Pts',(181.356352507902,3.27144492442103,338.672442126022));
#46322=CARTESIAN_POINT('Ctrl Pts',(181.348577429029,3.37332478601966,338.581686616557));
#46323=CARTESIAN_POINT('Ctrl Pts',(181.340802350156,3.47158620445461,338.486545000152));
#46324=CARTESIAN_POINT('Ctrl Pts',(181.333027271284,3.56582814977722,338.387337105863));
#46325=CARTESIAN_POINT('Ctrl Pts',(181.325261760107,3.65995412479419,338.288251292774));
#46326=CARTESIAN_POINT('Ctrl Pts',(181.31749624893,3.7500702015863,338.185109438602));
#46327=CARTESIAN_POINT('Ctrl Pts',(181.309730737753,3.83580899468906,338.07827101126));
#46328=CARTESIAN_POINT('Ctrl Pts',(181.30197292607,3.92146277789733,337.97153851407));
#46329=CARTESIAN_POINT('Ctrl Pts',(181.294215114387,4.00274767133497,337.861117040443));
#46330=CARTESIAN_POINT('Ctrl Pts',(181.286457302703,4.07933395357429,337.747401965078));
#46331=CARTESIAN_POINT('Ctrl Pts',(181.278705328986,4.15586260253463,337.633772463428));
#46332=CARTESIAN_POINT('Ctrl Pts',(181.270953355269,4.22769946073253,337.51685461632));
#46333=CARTESIAN_POINT('Ctrl Pts',(181.263201381552,4.29455606666506,337.397075562591));
#46334=CARTESIAN_POINT('Ctrl Pts',(181.25545269075,4.36138435921617,337.27734723459));
#46335=CARTESIAN_POINT('Ctrl Pts',(181.247703999949,4.42323640425902,337.154760450559));
#46336=CARTESIAN_POINT('Ctrl Pts',(181.239955309147,4.47986806669162,337.029769732639));
#46337=CARTESIAN_POINT('Ctrl Pts',(181.232208230495,4.53648794665621,336.904805019591));
#46338=CARTESIAN_POINT('Ctrl Pts',(181.224461151843,4.58788944317424,336.777437723296));
#46339=CARTESIAN_POINT('Ctrl Pts',(181.21671407319,4.6338754195587,336.648144914293));
#46340=CARTESIAN_POINT('Ctrl Pts',(181.20896692958,4.67986178152939,336.518851021187));
#46341=CARTESIAN_POINT('Ctrl Pts',(181.20121978597,4.72043240181103,336.387631951445));
#46342=CARTESIAN_POINT('Ctrl Pts',(181.193472642359,4.75543927216071,336.25498222748));
#46343=CARTESIAN_POINT('Ctrl Pts',(181.185723756996,4.79045401293386,336.122302680527));
#46344=CARTESIAN_POINT('Ctrl Pts',(181.177974871633,4.8199024149628,335.988192217169));
#46345=CARTESIAN_POINT('Ctrl Pts',(181.170225986271,4.84368716160249,335.853157513609));
#46346=CARTESIAN_POINT('Ctrl Pts',(181.162468876115,4.86749715375857,335.717979482021));
#46347=CARTESIAN_POINT('Ctrl Pts',(181.154711765959,4.88563141408742,335.581875636139));
#46348=CARTESIAN_POINT('Ctrl Pts',(181.146954655804,4.89804422625352,335.445360326213));
#46349=CARTESIAN_POINT('Ctrl Pts',(181.139193400471,4.91046367147038,335.308772066421));
#46350=CARTESIAN_POINT('Ctrl Pts',(181.131432145138,4.9171555573637,335.171772294676));
#46351=CARTESIAN_POINT('Ctrl Pts',(181.123670889806,4.91812634045303,335.034876379429));
#46352=CARTESIAN_POINT('Ctrl Pts',(181.115897218954,4.91909867648387,334.897761474634));
#46353=CARTESIAN_POINT('Ctrl Pts',(181.108123548102,4.91433163504473,334.760751149172));
#46354=CARTESIAN_POINT('Ctrl Pts',(181.100349877251,4.90388374864744,334.624357560636));
#46355=CARTESIAN_POINT('Ctrl Pts',(181.092938076043,4.89392221843911,334.494313186036));
#46356=CARTESIAN_POINT('Ctrl Pts',(181.085526274836,4.87879686579945,334.364829707653));
#46357=CARTESIAN_POINT('Ctrl Pts',(181.078114473628,4.85860150844942,334.236341408355));
#46358=CARTESIAN_POINT('Ctrl Pts',(181.070339398603,4.83741631821718,334.101555525835));
#46359=CARTESIAN_POINT('Ctrl Pts',(181.062564323579,4.81058461613832,333.967438891342));
#46360=CARTESIAN_POINT('Ctrl Pts',(181.054789248554,4.77815833222233,333.834501816941));
#46361=CARTESIAN_POINT('Ctrl Pts',(181.047023741314,4.7457719511656,333.701728331108));
#46362=CARTESIAN_POINT('Ctrl Pts',(181.039258234075,4.70780477825916,333.570131893342));
#46363=CARTESIAN_POINT('Ctrl Pts',(181.031492726836,4.66436028364287,333.440215974285));
#46364=CARTESIAN_POINT('Ctrl Pts',(181.023734919175,4.62095886467914,333.310428868166));
#46365=CARTESIAN_POINT('Ctrl Pts',(181.015977111514,4.57209105480738,333.182319333131));
#46366=CARTESIAN_POINT('Ctrl Pts',(181.008219303853,4.51791090113808,333.056378598626));
#46367=CARTESIAN_POINT('Ctrl Pts',(181.000467334238,4.46377152010305,332.930532639333));
#46368=CARTESIAN_POINT('Ctrl Pts',(180.992715364624,4.40432790642545,332.806852589557));
#46369=CARTESIAN_POINT('Ctrl Pts',(180.984963395009,4.33978314649324,332.68581217186));
#46370=CARTESIAN_POINT('Ctrl Pts',(180.977214708418,4.27526572180386,332.564823015786));
#46371=CARTESIAN_POINT('Ctrl Pts',(180.969466021827,4.20565163123511,332.446471612538));
#46372=CARTESIAN_POINT('Ctrl Pts',(180.961717335236,4.13119097596314,332.331209228392));
#46373=CARTESIAN_POINT('Ctrl Pts',(180.95397026086,4.05674581319582,332.215970826079));
#46374=CARTESIAN_POINT('Ctrl Pts',(180.946223186484,3.97745630345275,332.103820492588));
#46375=CARTESIAN_POINT('Ctrl Pts',(180.938476112108,3.89361694290864,331.995182174508));
#46376=CARTESIAN_POINT('Ctrl Pts',(180.930728972835,3.80977688004724,331.886542946372));
#46377=CARTESIAN_POINT('Ctrl Pts',(180.922981833562,3.72138712916976,331.78141610177));
#46378=CARTESIAN_POINT('Ctrl Pts',(180.915234694289,3.62878344835714,331.680193718388));
#46379=CARTESIAN_POINT('Ctrl Pts',(180.907485813321,3.53615894858904,331.578948578413));
#46380=CARTESIAN_POINT('Ctrl Pts',(180.899736932353,3.43931889752034,331.481609934707));
#46381=CARTESIAN_POINT('Ctrl Pts',(180.891988051386,3.33863670577549,331.388533814453));
#46382=CARTESIAN_POINT('Ctrl Pts',(180.884230945692,3.23784764912627,331.295358902442));
#46383=CARTESIAN_POINT('Ctrl Pts',(180.876473839998,3.13320859292652,331.206455817308));
#46384=CARTESIAN_POINT('Ctrl Pts',(180.868716734305,3.02512732498981,331.122141347328));
#46385=CARTESIAN_POINT('Ctrl Pts',(180.860955483478,2.91698830209655,331.037781822562));
#46386=CARTESIAN_POINT('Ctrl Pts',(180.85319423265,2.80540372011654,330.958016025974));
#46387=CARTESIAN_POINT('Ctrl Pts',(180.845432981823,2.69081045684819,330.883117423606));
#46388=CARTESIAN_POINT('Ctrl Pts',(180.837659315506,2.57603388144784,330.808099007715));
#46389=CARTESIAN_POINT('Ctrl Pts',(180.82988564919,2.45823934315503,330.737963544721));
#46390=CARTESIAN_POINT('Ctrl Pts',(180.822111982873,2.33788920102439,330.672938971284));
#46391=CARTESIAN_POINT('Ctrl Pts',(180.814700135033,2.22314065064444,330.610940909554));
#46392=CARTESIAN_POINT('Ctrl Pts',(180.807288287194,2.10606929737862,330.553588807962));
#46393=CARTESIAN_POINT('Ctrl Pts',(180.799876439354,1.98709111732864,330.501038791684));
#46394=CARTESIAN_POINT('Ctrl Pts',(180.79210135845,1.8622821633874,330.445913452243));
#46395=CARTESIAN_POINT('Ctrl Pts',(180.784326277547,1.73498034195015,330.395898563748));
#46396=CARTESIAN_POINT('Ctrl Pts',(180.776551196643,1.60564288863294,330.351226615904));
#46397=CARTESIAN_POINT('Ctrl Pts',(180.768785683446,1.47646459286564,330.30660963959));
#46398=CARTESIAN_POINT('Ctrl Pts',(180.76102017025,1.34525601531228,330.267322648326));
#46399=CARTESIAN_POINT('Ctrl Pts',(180.753254657053,1.21249652972999,330.233551088295));
#46400=CARTESIAN_POINT('Ctrl Pts',(180.745496843362,1.07986867518179,330.199813012767));
#46401=CARTESIAN_POINT('Ctrl Pts',(180.737739029672,0.945693349134705,330.171579581488));
#46402=CARTESIAN_POINT('Ctrl Pts',(180.729981215982,0.810467001486327,330.148987084948));
#46403=CARTESIAN_POINT('Ctrl Pts',(180.722229240273,0.675342415613457,330.126411589921));
#46404=CARTESIAN_POINT('Ctrl Pts',(180.714477264564,0.539168766413863,330.109468644382));
#46405=CARTESIAN_POINT('Ctrl Pts',(180.706725288855,0.402454319765606,330.098243826647));
#46406=CARTESIAN_POINT('Ctrl Pts',(180.698976596092,0.265797771408406,330.0870237626));
#46407=CARTESIAN_POINT('Ctrl Pts',(180.691227903329,0.128601269872828,330.081517041851));
#46408=CARTESIAN_POINT('Ctrl Pts',(180.683479210566,-0.00862036059448677,
330.081757554585));
#46409=CARTESIAN_POINT('Ctrl Pts',(180.675732129972,-0.145813441167131,
330.081998017278));
#46410=CARTESIAN_POINT('Ctrl Pts',(180.667985049377,-0.283031249644119,
330.087983334336));
#46411=CARTESIAN_POINT('Ctrl Pts',(180.660237968783,-0.419757910862382,
330.099695278988));
#46412=CARTESIAN_POINT('Ctrl Pts',(180.652490823251,-0.556485718147188,
330.111407321812));
#46413=CARTESIAN_POINT('Ctrl Pts',(180.644743677719,-0.692721980513987,
330.128846054614));
#46414=CARTESIAN_POINT('Ctrl Pts',(180.636996532187,-0.82795529290341,330.151941306517));
#46415=CARTESIAN_POINT('Ctrl Pts',(180.629247644925,-0.963219008731504,
330.175041750744));
#46416=CARTESIAN_POINT('Ctrl Pts',(180.621498757664,-1.09747894067125,330.203801178847));
#46417=CARTESIAN_POINT('Ctrl Pts',(180.613749870402,-1.23023362338467,330.238098248137));
#46418=CARTESIAN_POINT('Ctrl Pts',(180.605992758395,-1.36312921323199,330.272431720676));
#46419=CARTESIAN_POINT('Ctrl Pts',(180.598235646388,-1.49451598327833,330.312314477747));
#46420=CARTESIAN_POINT('Ctrl Pts',(180.59047853438,-1.6239068615804,330.357575033734));
#46421=CARTESIAN_POINT('Ctrl Pts',(180.582717277219,-1.75336688226033,330.402859775525));
#46422=CARTESIAN_POINT('Ctrl Pts',(180.574956020057,-1.88082852297318,330.453527898072));
#46423=CARTESIAN_POINT('Ctrl Pts',(180.567194762895,-2.00582540012955,330.509360009231));
#46424=CARTESIAN_POINT('Ctrl Pts',(180.559421090273,-2.13102223121361,330.56528143342));
#46425=CARTESIAN_POINT('Ctrl Pts',(180.55164741765,-2.25374606974708,330.626383179212));
#46426=CARTESIAN_POINT('Ctrl Pts',(180.543873745028,-2.37355502941302,330.692399788183));
#46427=CARTESIAN_POINT('Ctrl Pts',(180.536461965045,-2.48778644770066,330.755343084696));
#46428=CARTESIAN_POINT('Ctrl Pts',(180.529050185062,-2.59936802770936,330.822753787484));
#46429=CARTESIAN_POINT('Ctrl Pts',(180.52163840508,-2.70794338199464,330.894366589379));
#46430=CARTESIAN_POINT('Ctrl Pts',(180.513878670321,-2.82161593468427,330.969341338944));
#46431=CARTESIAN_POINT('Ctrl Pts',(180.506118935562,-2.93235554456295,331.049161358738));
#46432=CARTESIAN_POINT('Ctrl Pts',(180.498359200804,-3.03972028326498,331.133569648628));
#46433=CARTESIAN_POINT('Ctrl Pts',(180.490609025355,-3.14695275805946,331.217873954936));
#46434=CARTESIAN_POINT('Ctrl Pts',(180.482858849906,-3.25081832769985,331.306755045375));
#46435=CARTESIAN_POINT('Ctrl Pts',(180.475108674458,-3.35090255687002,331.399911790405));
#46436=CARTESIAN_POINT('Ctrl Pts',(180.467366173794,-3.4508876753905,331.492976284883));
#46437=CARTESIAN_POINT('Ctrl Pts',(180.45962367313,-3.54709861924634,331.590307742795));
#46438=CARTESIAN_POINT('Ctrl Pts',(180.451881172467,-3.63915298617011,331.691564024233));
#46439=CARTESIAN_POINT('Ctrl Pts',(180.444144468867,-3.73113842897115,331.792744491773));
#46440=CARTESIAN_POINT('Ctrl Pts',(180.436407765267,-3.81897322598363,331.897843644671));
#46441=CARTESIAN_POINT('Ctrl Pts',(180.428671061668,-3.90231118561838,332.006481923706));
#46442=CARTESIAN_POINT('Ctrl Pts',(180.420937575272,-3.98561449028321,332.115075026974));
#46443=CARTESIAN_POINT('Ctrl Pts',(180.413204088877,-4.06442443789406,332.227204018703));
#46444=CARTESIAN_POINT('Ctrl Pts',(180.405470602481,-4.13843473160768,332.342455826383));
#46445=CARTESIAN_POINT('Ctrl Pts',(180.397738661595,-4.21243023462844,332.457684601402));
#46446=CARTESIAN_POINT('Ctrl Pts',(180.39000672071,-4.281627779502,332.576034620936));
#46447=CARTESIAN_POINT('Ctrl Pts',(180.382274779824,-4.34576432241902,332.697063718535));
#46448=CARTESIAN_POINT('Ctrl Pts',(180.374542692827,-4.4099020773275,332.818095103226));
#46449=CARTESIAN_POINT('Ctrl Pts',(180.36681060583,-4.46897845602357,332.941805319855));
#46450=CARTESIAN_POINT('Ctrl Pts',(180.359078518834,-4.52277652114452,333.067727865366));
#46451=CARTESIAN_POINT('Ctrl Pts',(180.351344594356,-4.57658737102809,333.193680335556));
#46452=CARTESIAN_POINT('Ctrl Pts',(180.343610669879,-4.62511725738823,333.321845819719));
#46453=CARTESIAN_POINT('Ctrl Pts',(180.335876745402,-4.6681976659552,333.451738518831));
#46454=CARTESIAN_POINT('Ctrl Pts',(180.328134605733,-4.71132383574079,333.581769193613));
#46455=CARTESIAN_POINT('Ctrl Pts',(180.320392466064,-4.74898884220444,333.713530374675));
#46456=CARTESIAN_POINT('Ctrl Pts',(180.312650326396,-4.78107414634263,333.846521318067));
#46457=CARTESIAN_POINT('Ctrl Pts',(180.304903927326,-4.81317710246988,333.9795854275));
#46458=CARTESIAN_POINT('Ctrl Pts',(180.297157528257,-4.83969416457988,334.113880262331));
#46459=CARTESIAN_POINT('Ctrl Pts',(180.289411129187,-4.8605582812456,334.248896640192));
#46460=CARTESIAN_POINT('Ctrl Pts',(180.281652613415,-4.88145503298411,334.384124206928));
#46461=CARTESIAN_POINT('Ctrl Pts',(180.273894097643,-4.89668112984652,334.520075181497));
#46462=CARTESIAN_POINT('Ctrl Pts',(180.266135581871,-4.90622151443417,334.656236252925));
#46463=CARTESIAN_POINT('Ctrl Pts',(180.259602470754,-4.91425506033938,334.770891611707));
#46464=CARTESIAN_POINT('Ctrl Pts',(180.253069359637,-4.91825801731504,334.885695792017));
#46465=CARTESIAN_POINT('Ctrl Pts',(180.24653624852,-4.91824998793836,335.000344447839));
#46466=CARTESIAN_POINT('',(183.746536248537,-4.91824946343417,334.997702625515));
#46467=CARTESIAN_POINT('Ctrl Pts',(183.74653624849,-4.91824946343456,334.997702626357));
#46468=CARTESIAN_POINT('Ctrl Pts',(183.738662233524,-4.91831472035729,335.137405554579));
#46469=CARTESIAN_POINT('Ctrl Pts',(183.730788218558,-4.91242323172791,335.277092861909));
#46470=CARTESIAN_POINT('Ctrl Pts',(183.722914203592,-4.9006054591028,335.416232142814));
#46471=CARTESIAN_POINT('Ctrl Pts',(183.715037492967,-4.88878364067781,335.555419057881));
#46472=CARTESIAN_POINT('Ctrl Pts',(183.707160782342,-4.87103152767783,335.694057201196));
#46473=CARTESIAN_POINT('Ctrl Pts',(183.699284071717,-4.8474314120948,335.831619965812));
#46474=CARTESIAN_POINT('Ctrl Pts',(183.691403188189,-4.82381879370446,335.969255608067));
#46475=CARTESIAN_POINT('Ctrl Pts',(183.68352230466,-4.79435206354287,336.10581436943));
#46476=CARTESIAN_POINT('Ctrl Pts',(183.675641421132,-4.75916446642854,336.240780659095));
#46477=CARTESIAN_POINT('Ctrl Pts',(183.667749095471,-4.72392578098497,336.375942904233));
#46478=CARTESIAN_POINT('Ctrl Pts',(183.659856769809,-4.68294972730786,336.509507696768));
#46479=CARTESIAN_POINT('Ctrl Pts',(183.651964444148,-4.63641950913448,336.640974465925));
#46480=CARTESIAN_POINT('Ctrl Pts',(183.644066234623,-4.58985460188793,336.772539245805));
#46481=CARTESIAN_POINT('Ctrl Pts',(183.636168025098,-4.53772741418317,336.902002538605));
#46482=CARTESIAN_POINT('Ctrl Pts',(183.628269815572,-4.48026877631966,337.028885101339));
#46483=CARTESIAN_POINT('Ctrl Pts',(183.620356925575,-4.42270333957709,337.156003501815));
#46484=CARTESIAN_POINT('Ctrl Pts',(183.612444035578,-4.35978681345751,337.280531251256));
#46485=CARTESIAN_POINT('Ctrl Pts',(183.604531145581,-4.29179594580606,337.402013868));
#46486=CARTESIAN_POINT('Ctrl Pts',(183.597106357752,-4.22799905657679,337.51600289787));
#46487=CARTESIAN_POINT('Ctrl Pts',(183.589681569923,-4.15973509277527,337.627310935476));
#46488=CARTESIAN_POINT('Ctrl Pts',(183.582256782094,-4.08726574767666,337.735588011812));
#46489=CARTESIAN_POINT('Ctrl Pts',(183.574483044214,-4.01139048954663,337.848953892314));
#46490=CARTESIAN_POINT('Ctrl Pts',(183.566709306335,-3.93067481074444,337.959340381255));
#46491=CARTESIAN_POINT('Ctrl Pts',(183.558935568455,-3.84538014502149,338.066306345226));
#46492=CARTESIAN_POINT('Ctrl Pts',(183.55117141566,-3.76019064834008,338.173140419262));
#46493=CARTESIAN_POINT('Ctrl Pts',(183.543407262865,-3.67043363986846,338.27656205715));
#46494=CARTESIAN_POINT('Ctrl Pts',(183.535643110069,-3.5764144512764,338.376157984337));
#46495=CARTESIAN_POINT('Ctrl Pts',(183.527886672613,-3.48248869076345,338.475654941767));
#46496=CARTESIAN_POINT('Ctrl Pts',(183.520130235156,-3.38430944539702,338.571333471441));
#46497=CARTESIAN_POINT('Ctrl Pts',(183.5123737977,-3.28222280124049,338.662812654985));
#46498=CARTESIAN_POINT('Ctrl Pts',(183.504623212537,-3.18021318227063,338.754222816756));
#46499=CARTESIAN_POINT('Ctrl Pts',(183.496872627374,-3.0743023226734,338.841439679069));
#46500=CARTESIAN_POINT('Ctrl Pts',(183.489122042212,-2.96487345396073,338.924118813759));
#46501=CARTESIAN_POINT('Ctrl Pts',(183.481374756881,-2.8554911748783,339.006762747589));
#46502=CARTESIAN_POINT('Ctrl Pts',(183.473627471551,-2.7425941770438,339.084872561081));
#46503=CARTESIAN_POINT('Ctrl Pts',(183.46588018622,-2.62659891860498,339.158143958942));
#46504=CARTESIAN_POINT('Ctrl Pts',(183.458134523145,-2.51062794918574,339.231400014017));
#46505=CARTESIAN_POINT('Ctrl Pts',(183.45038886007,-2.39156033998065,339.299819459971));
#46506=CARTESIAN_POINT('Ctrl Pts',(183.442643196996,-2.26984135408545,339.363141447373));
#46507=CARTESIAN_POINT('Ctrl Pts',(183.43489747775,-2.14812148550022,339.426463893977));
#46508=CARTESIAN_POINT('Ctrl Pts',(183.427151758505,-2.02375054875627,339.484688627805));
#46509=CARTESIAN_POINT('Ctrl Pts',(183.419406039259,-1.89719785537914,339.537601057833));
#46510=CARTESIAN_POINT('Ctrl Pts',(183.411658585736,-1.77061682666147,339.590525335034));
#46511=CARTESIAN_POINT('Ctrl Pts',(183.403911132212,-1.64185342995883,339.638134790811));
#46512=CARTESIAN_POINT('Ctrl Pts',(183.396163678688,-1.51139599080171,339.680263370953));
#46513=CARTESIAN_POINT('Ctrl Pts',(183.388408004165,-1.38080012027327,339.722436654696));
#46514=CARTESIAN_POINT('Ctrl Pts',(183.380652329641,-1.24850698914037,339.759117324682));
#46515=CARTESIAN_POINT('Ctrl Pts',(183.372896655117,-1.11501962321825,339.790189380634));
#46516=CARTESIAN_POINT('Ctrl Pts',(183.365136839753,-0.981460986919521,
339.821278026299));
#46517=CARTESIAN_POINT('Ctrl Pts',(183.357377024389,-0.846707229366385,
339.846752018567));
#46518=CARTESIAN_POINT('Ctrl Pts',(183.349617209025,-0.711269560545343,
339.866546894333));
#46519=CARTESIAN_POINT('Ctrl Pts',(183.34184497105,-0.57561507091135,339.886373459518));
#46520=CARTESIAN_POINT('Ctrl Pts',(183.334072733075,-0.439274871295413,
339.900502700093));
#46521=CARTESIAN_POINT('Ctrl Pts',(183.326300495101,-0.302764153413162,
339.908922175988));
#46522=CARTESIAN_POINT('Ctrl Pts',(183.318873246007,-0.172312781626706,
339.91696793384));
#46523=CARTESIAN_POINT('Ctrl Pts',(183.311445996913,-0.0417059970710242,
339.919799946453));
#46524=CARTESIAN_POINT('Ctrl Pts',(183.304018747819,0.0886102589325586,
339.917451706373));
#46525=CARTESIAN_POINT('Ctrl Pts',(183.296243208508,0.225037509280272,339.914993348935));
#46526=CARTESIAN_POINT('Ctrl Pts',(183.288467669196,0.361577749274374,339.906849358024));
#46527=CARTESIAN_POINT('Ctrl Pts',(183.280692129884,0.497718315349884,339.893001077158));
#46528=CARTESIAN_POINT('Ctrl Pts',(183.272926154675,0.6336914252225,339.879169830013));
#46529=CARTESIAN_POINT('Ctrl Pts',(183.265160179465,0.769265454236493,339.859648292778));
#46530=CARTESIAN_POINT('Ctrl Pts',(183.257394204256,0.903927437011325,339.834469800414));
#46531=CARTESIAN_POINT('Ctrl Pts',(183.249635925466,1.03845596389929,339.809316261033));
#46532=CARTESIAN_POINT('Ctrl Pts',(183.241877646676,1.17207386162816,339.778516994751));
#46533=CARTESIAN_POINT('Ctrl Pts',(183.234119367886,1.30427334318214,339.742157115571));
#46534=CARTESIAN_POINT('Ctrl Pts',(183.226366924501,1.43637339062766,339.705824584549));
#46535=CARTESIAN_POINT('Ctrl Pts',(183.218614481116,1.56705677013313,339.66393986879));
#46536=CARTESIAN_POINT('Ctrl Pts',(183.210862037731,1.69582629933627,339.616639061588));
#46537=CARTESIAN_POINT('Ctrl Pts',(183.203112875046,1.82454133550684,339.569358271267));
#46538=CARTESIAN_POINT('Ctrl Pts',(183.195363712361,1.95134376613767,339.516666082607));
#46539=CARTESIAN_POINT('Ctrl Pts',(183.187614549676,2.07575219336666,339.458748242975));
#46540=CARTESIAN_POINT('Ctrl Pts',(183.179866997861,2.20013475898928,339.40084244311));
#46541=CARTESIAN_POINT('Ctrl Pts',(183.172119446045,2.32212395700371,339.337713317832));
#46542=CARTESIAN_POINT('Ctrl Pts',(183.16437189423,2.44125935066559,339.269594342006));
#46543=CARTESIAN_POINT('Ctrl Pts',(183.156624276629,2.5603957559335,339.201474787765));
#46544=CARTESIAN_POINT('Ctrl Pts',(183.148876659027,2.67667796924099,339.12836549246));
#46545=CARTESIAN_POINT('Ctrl Pts',(183.141129041426,2.78967145085819,339.050545180438));
#46546=CARTESIAN_POINT('Ctrl Pts',(183.133379681695,2.90269034018911,338.972707369741));
#46547=CARTESIAN_POINT('Ctrl Pts',(183.125630321964,3.01241870448798,338.890156656029));
#46548=CARTESIAN_POINT('Ctrl Pts',(183.117880962233,3.11845253832436,338.803214013005));
#46549=CARTESIAN_POINT('Ctrl Pts',(183.110123379805,3.22459888263836,338.716179116802));
#46550=CARTESIAN_POINT('Ctrl Pts',(183.102365797376,3.32704256283489,338.624743230307));
#46551=CARTESIAN_POINT('Ctrl Pts',(183.094608214948,3.42541371574121,338.529266770664));
#46552=CARTESIAN_POINT('Ctrl Pts',(183.086846487737,3.52383742716301,338.433739299105));
#46553=CARTESIAN_POINT('Ctrl Pts',(183.079084760526,3.61818400692725,338.334167236275));
#46554=CARTESIAN_POINT('Ctrl Pts',(183.071323033316,3.70812250454873,338.230945767691));
#46555=CARTESIAN_POINT('Ctrl Pts',(183.063548896042,3.79820480294702,338.127559260467));
#46556=CARTESIAN_POINT('Ctrl Pts',(183.055774758768,3.88386469091444,338.02051199282));
#46557=CARTESIAN_POINT('Ctrl Pts',(183.048000621495,3.96481281290701,337.910230647407));
#46558=CARTESIAN_POINT('Ctrl Pts',(183.040593985512,4.04193433160511,337.805162554005));
#46559=CARTESIAN_POINT('Ctrl Pts',(183.033187349529,4.11477920662459,337.697159390882));
#46560=CARTESIAN_POINT('Ctrl Pts',(183.025780713546,4.18313606116424,337.586610862942));
#46561=CARTESIAN_POINT('Ctrl Pts',(183.018005522485,4.25489436082336,337.470561427252));
#46562=CARTESIAN_POINT('Ctrl Pts',(183.010230331425,4.32193314534969,337.351340323045));
#46563=CARTESIAN_POINT('Ctrl Pts',(183.002455140365,4.38395929370328,337.229368514547));
#46564=CARTESIAN_POINT('Ctrl Pts',(182.994689514232,4.44590913838514,337.107546754006));
#46565=CARTESIAN_POINT('Ctrl Pts',(182.986923888099,4.50285844093783,336.982981367197));
#46566=CARTESIAN_POINT('Ctrl Pts',(182.979158261967,4.55455763588336,336.856121710426));
#46567=CARTESIAN_POINT('Ctrl Pts',(182.971400332695,4.6062055894306,336.72938778997));
#46568=CARTESIAN_POINT('Ctrl Pts',(182.963642403424,4.6526136443135,336.600364484482));
#46569=CARTESIAN_POINT('Ctrl Pts',(182.955884474153,4.69357857819171,336.469524818722));
#46570=CARTESIAN_POINT('Ctrl Pts',(182.948132380349,4.73451269849694,336.338783569759));
#46571=CARTESIAN_POINT('Ctrl Pts',(182.940380286544,4.77001173095744,336.206229051496));
#46572=CARTESIAN_POINT('Ctrl Pts',(182.93262819274,4.79992106078274,336.072352960902));
#46573=CARTESIAN_POINT('Ctrl Pts',(182.924879378459,4.82981773746841,335.938533506577));
#46574=CARTESIAN_POINT('Ctrl Pts',(182.917130564177,4.85412932973476,335.803393972577));
#46575=CARTESIAN_POINT('Ctrl Pts',(182.909381749896,4.87275151938588,335.667439654817));
#46576=CARTESIAN_POINT('Ctrl Pts',(182.901634545713,4.89136983959658,335.531513586535));
#46577=CARTESIAN_POINT('Ctrl Pts',(182.893887341531,4.90430105562567,335.394773458246));
#46578=CARTESIAN_POINT('Ctrl Pts',(182.886140137349,4.911492327446,335.257732768462));
#46579=CARTESIAN_POINT('Ctrl Pts',(182.878392866271,4.91868366136183,335.120690895353));
#46580=CARTESIAN_POINT('Ctrl Pts',(182.870645595193,4.92013493173456,334.983348845895));
#46581=CARTESIAN_POINT('Ctrl Pts',(182.862898324115,4.91584536414341,334.846222828971));
#46582=CARTESIAN_POINT('Ctrl Pts',(182.855149309458,4.9115548311543,334.709065950853));
#46583=CARTESIAN_POINT('Ctrl Pts',(182.847400294801,4.90152090144786,334.572125592609));
#46584=CARTESIAN_POINT('Ctrl Pts',(182.839651280144,4.88579485286582,334.435915149814));
#46585=CARTESIAN_POINT('Ctrl Pts',(182.831894038515,4.8700521082577,334.29956009516));
#46586=CARTESIAN_POINT('Ctrl Pts',(182.824136796887,4.84860521780202,334.163936892858));
#46587=CARTESIAN_POINT('Ctrl Pts',(182.816379555258,4.82155710453961,334.029551572641));
#46588=CARTESIAN_POINT('Ctrl Pts',(182.808618167059,4.79449453292637,333.895094417835));
#46589=CARTESIAN_POINT('Ctrl Pts',(182.80085677886,4.76182486556082,333.76187684303));
#46590=CARTESIAN_POINT('Ctrl Pts',(182.79309539066,4.7237013206043,333.630390969575));
#46591=CARTESIAN_POINT('Ctrl Pts',(182.785321585883,4.68551678604702,333.49869474656));
#46592=CARTESIAN_POINT('Ctrl Pts',(182.777547781106,4.64186106319591,333.368736131593));
#46593=CARTESIAN_POINT('Ctrl Pts',(182.769773976329,4.5929363660258,333.240989312102));
#46594=CARTESIAN_POINT('Ctrl Pts',(182.762363543976,4.5462985652168,333.119213786325));
#46595=CARTESIAN_POINT('Ctrl Pts',(182.754953111624,4.49487334525659,332.99944822182));
#46596=CARTESIAN_POINT('Ctrl Pts',(182.747542679272,4.43887438890023,332.882081866061));
#46597=CARTESIAN_POINT('Ctrl Pts',(182.739767793996,4.38012134446927,332.75894330843));
#46598=CARTESIAN_POINT('Ctrl Pts',(182.73199290872,4.31614755979411,332.638056719292));
#46599=CARTESIAN_POINT('Ctrl Pts',(182.724218023444,4.24714834915519,332.519896380639));
#46600=CARTESIAN_POINT('Ctrl Pts',(182.716452708519,4.17823407181412,332.401881489262));
#46601=CARTESIAN_POINT('Ctrl Pts',(182.708687393594,4.1043068720002,332.286586505573));
#46602=CARTESIAN_POINT('Ctrl Pts',(182.700922078669,4.02560951209295,332.174464454542));
#46603=CARTESIAN_POINT('Ctrl Pts',(182.693164465668,3.94699020711559,332.062453610276));
#46604=CARTESIAN_POINT('Ctrl Pts',(182.685406852667,3.86361038055084,331.953609753793));
#46605=CARTESIAN_POINT('Ctrl Pts',(182.677649239666,3.77575777952021,331.848359751987));
#46606=CARTESIAN_POINT('Ctrl Pts',(182.669897466842,3.68797131671046,331.743188985718));
#46607=CARTESIAN_POINT('Ctrl Pts',(182.662145694018,3.59571903124513,331.641606987716));
#46608=CARTESIAN_POINT('Ctrl Pts',(182.654393921194,3.49933067914566,331.544009858161));
#46609=CARTESIAN_POINT('Ctrl Pts',(182.646645433943,3.40298318104794,331.446454094945));
#46610=CARTESIAN_POINT('Ctrl Pts',(182.638896946692,3.3025033771423,331.35288011846));
#46611=CARTESIAN_POINT('Ctrl Pts',(182.63114845944,3.19825967999946,331.263649095469));
#46612=CARTESIAN_POINT('Ctrl Pts',(182.623401585928,3.09403769317387,331.17443665618));
#46613=CARTESIAN_POINT('Ctrl Pts',(182.615654712416,2.98605366909098,331.089565625335));
#46614=CARTESIAN_POINT('Ctrl Pts',(182.607907838903,2.87471077863055,331.009358322058));
#46615=CARTESIAN_POINT('Ctrl Pts',(182.600160901831,2.76336697465094,330.929150360716));
#46616=CARTESIAN_POINT('Ctrl Pts',(182.592413964759,2.64866456649613,330.853606431745));
#46617=CARTESIAN_POINT('Ctrl Pts',(182.584667027687,2.53103718259929,330.783006539868));
#46618=CARTESIAN_POINT('Ctrl Pts',(182.576918350071,2.41338337075461,330.71239078595));
#46619=CARTESIAN_POINT('Ctrl Pts',(182.569169672455,2.29280361057261,330.646721480619));
#46620=CARTESIAN_POINT('Ctrl Pts',(182.561420994839,2.16975733561803,330.586233335683));
#46621=CARTESIAN_POINT('Ctrl Pts',(182.553664093177,2.04658046570813,330.525680991758));
#46622=CARTESIAN_POINT('Ctrl Pts',(182.545907191515,1.92093220301761,330.470320965749));
#46623=CARTESIAN_POINT('Ctrl Pts',(182.538150289853,1.79329373726262,330.420340554758));
#46624=CARTESIAN_POINT('Ctrl Pts',(182.53038924375,1.66558707545349,330.370333439695));
#46625=CARTESIAN_POINT('Ctrl Pts',(182.522628197647,1.53588846121267,330.325711794006));
#46626=CARTESIAN_POINT('Ctrl Pts',(182.514867151544,1.40469460780011,330.28661309446));
#46627=CARTESIAN_POINT('Ctrl Pts',(182.507093689075,1.27329086632136,330.24745184358));
#46628=CARTESIAN_POINT('Ctrl Pts',(182.499320226606,1.14038748464425,330.21383129127));
#46629=CARTESIAN_POINT('Ctrl Pts',(182.491546764136,1.00649261114424,330.185838007897));
#46630=CARTESIAN_POINT('Ctrl Pts',(182.484132724423,0.878788655103757,330.159139054189));
#46631=CARTESIAN_POINT('Ctrl Pts',(182.476718684711,0.750183129836309,330.137558670627));
#46632=CARTESIAN_POINT('Ctrl Pts',(182.469304644998,0.62111967389052,330.12112785439));
#46633=CARTESIAN_POINT('Ctrl Pts',(182.461529486789,0.485769874346384,330.103896736041));
#46634=CARTESIAN_POINT('Ctrl Pts',(182.45375432858,0.349488651101491,330.092274978123));
#46635=CARTESIAN_POINT('Ctrl Pts',(182.445979170372,0.212780573065129,330.086354969045));
#46636=CARTESIAN_POINT('Ctrl Pts',(182.438213579175,0.0762407086890431,
330.080442244295));
#46637=CARTESIAN_POINT('Ctrl Pts',(182.430447987978,-0.0607245786593256,
330.080217325762));
#46638=CARTESIAN_POINT('Ctrl Pts',(182.422682396782,-0.197602922753006,
330.08572119763));
#46639=CARTESIAN_POINT('Ctrl Pts',(182.414924504484,-0.334345564028642,
330.091219612895));
#46640=CARTESIAN_POINT('Ctrl Pts',(182.407166612187,-0.471001045551423,
330.102435500246));
#46641=CARTESIAN_POINT('Ctrl Pts',(182.39940871989,-0.607054657868781,330.119357859373));
#46642=CARTESIAN_POINT('Ctrl Pts',(182.391656665053,-0.743005896038143,
330.136267485196));
#46643=CARTESIAN_POINT('Ctrl Pts',(182.383904610217,-0.878355780121441,
330.158874988023));
#46644=CARTESIAN_POINT('Ctrl Pts',(182.37615255538,-1.01259274292381,330.187117391887));
#46645=CARTESIAN_POINT('Ctrl Pts',(182.368403782979,-1.14677286605946,330.21534783713));
#46646=CARTESIAN_POINT('Ctrl Pts',(182.360655010579,-1.27984062348581,330.249208357569));
#46647=CARTESIAN_POINT('Ctrl Pts',(182.352906238178,-1.41129290768061,330.288584566053));
#46648=CARTESIAN_POINT('Ctrl Pts',(182.345159077646,-1.54271784768671,330.327952583653));
#46649=CARTESIAN_POINT('Ctrl Pts',(182.337411917115,-1.67252760868526,330.372833895044));
#46650=CARTESIAN_POINT('Ctrl Pts',(182.329664756583,-1.80023294365699,330.423063862028));
#46651=CARTESIAN_POINT('Ctrl Pts',(182.321917530891,-1.92793935274515,330.473294251491));
#46652=CARTESIAN_POINT('Ctrl Pts',(182.314170305199,-2.05354093676256,330.528873243206));
#46653=CARTESIAN_POINT('Ctrl Pts',(182.306423079507,-2.17656755136495,330.589587688566));
#46654=CARTESIAN_POINT('Ctrl Pts',(182.298674111938,-2.2996218271253,330.65031578489));
#46655=CARTESIAN_POINT('Ctrl Pts',(182.290925144369,-2.42009963098066,330.71618145954));
#46656=CARTESIAN_POINT('Ctrl Pts',(182.2831761768,-2.53755494317087,330.786925353986));
#46657=CARTESIAN_POINT('Ctrl Pts',(182.275418984706,-2.65513491894708,330.857744333904));
#46658=CARTESIAN_POINT('Ctrl Pts',(182.267661792613,-2.76968565945884,330.933451674372));
#46659=CARTESIAN_POINT('Ctrl Pts',(182.259904600519,-2.88078924456396,331.013744063547));
#46660=CARTESIAN_POINT('Ctrl Pts',(182.252143263265,-2.99195219937276,331.094079358047));
#46661=CARTESIAN_POINT('Ctrl Pts',(182.244381926011,-3.09966402157302,331.179004341388));
#46662=CARTESIAN_POINT('Ctrl Pts',(182.236620588757,-3.20354028590892,331.268175687541));
#46663=CARTESIAN_POINT('Ctrl Pts',(182.228846836842,-3.30758270571109,331.357489667882));
#46664=CARTESIAN_POINT('Ctrl Pts',(182.221073084927,-3.40777702194416,331.451063317094));
#46665=CARTESIAN_POINT('Ctrl Pts',(182.213299333012,-3.50377542993101,331.548516145321));
#46666=CARTESIAN_POINT('Ctrl Pts',(182.205888425583,-3.59529305523456,331.641420304936));
#46667=CARTESIAN_POINT('Ctrl Pts',(182.198477518153,-3.6829974302838,331.737849479016));
#46668=CARTESIAN_POINT('Ctrl Pts',(182.191066610724,-3.76662275388509,331.837447851432));
#46669=CARTESIAN_POINT('Ctrl Pts',(182.182961178964,-3.85808515039839,331.946380235041));
#46670=CARTESIAN_POINT('Ctrl Pts',(182.174855747204,-3.94498091133261,332.059477675757));
#46671=CARTESIAN_POINT('Ctrl Pts',(182.166750315444,-4.0269075543671,332.176314711041));
#46672=CARTESIAN_POINT('Ctrl Pts',(182.159031256342,-4.10492888850736,332.28758231621));
#46673=CARTESIAN_POINT('Ctrl Pts',(182.151312197239,-4.17844356562488,332.402240893272));
#46674=CARTESIAN_POINT('Ctrl Pts',(182.143593138136,-4.24714239787314,332.519886189166));
#46675=CARTESIAN_POINT('Ctrl Pts',(182.135881261439,-4.31577730744665,332.637422018833));
#46676=CARTESIAN_POINT('Ctrl Pts',(182.128169384742,-4.37960508622303,332.757938700952));
#46677=CARTESIAN_POINT('Ctrl Pts',(182.120457508046,-4.4383588660141,332.881001736911));
#46678=CARTESIAN_POINT('Ctrl Pts',(182.112751089534,-4.49707106202213,333.00397767334));
#46679=CARTESIAN_POINT('Ctrl Pts',(182.105044671022,-4.55071623349502,333.129496022812));
#46680=CARTESIAN_POINT('Ctrl Pts',(182.097338252511,-4.59907286804657,333.257096727613));
#46681=CARTESIAN_POINT('Ctrl Pts',(182.089635572285,-4.6474060454057,333.384635534924));
#46682=CARTESIAN_POINT('Ctrl Pts',(182.08193289206,-4.69045565138616,333.514254318132));
#46683=CARTESIAN_POINT('Ctrl Pts',(182.074230211834,-4.72804803173018,333.645472454266));
#46684=CARTESIAN_POINT('Ctrl Pts',(182.066528352036,-4.76563640803903,333.776676614109));
#46685=CARTESIAN_POINT('Ctrl Pts',(182.058826492237,-4.79776859951033,333.909479409798));
#46686=CARTESIAN_POINT('Ctrl Pts',(182.051124632439,-4.8243206934159,334.043384659553));
#46687=CARTESIAN_POINT('Ctrl Pts',(182.04342322529,-4.85087122681638,334.177282039502));
#46688=CARTESIAN_POINT('Ctrl Pts',(182.035721818141,-4.87184224376834,334.312281355446));
#46689=CARTESIAN_POINT('Ctrl Pts',(182.028020410992,-4.88716101142139,334.447876543749));
#46690=CARTESIAN_POINT('Ctrl Pts',(182.020315803866,-4.90248614410664,334.583528072599));
#46691=CARTESIAN_POINT('Ctrl Pts',(182.01261119674,-4.91215429899052,334.719775574408));
#46692=CARTESIAN_POINT('Ctrl Pts',(182.004906589614,-4.91614465092684,334.85610825714));
#46693=CARTESIAN_POINT('Ctrl Pts',(182.002116475906,-4.91758970003254,334.905479195944));
#46694=CARTESIAN_POINT('Ctrl Pts',(181.999326362198,-4.91829064435592,334.954861295829));
#46695=CARTESIAN_POINT('Ctrl Pts',(181.99653624849,-4.91824818069221,335.00423032124));
#46696=CARTESIAN_POINT('',(185.231450264354,-2.85698122534213,339.003353761603));
#46697=CARTESIAN_POINT('Ctrl Pts',(185.231450264354,-2.85698122534213,339.003353761603));
#46698=CARTESIAN_POINT('Ctrl Pts',(185.223817702065,-2.74793304536805,339.081175663288));
#46699=CARTESIAN_POINT('Ctrl Pts',(185.216185139776,-2.63549753799294,339.154684880481));
#46700=CARTESIAN_POINT('Ctrl Pts',(185.208552577486,-2.52005774144929,339.223563902945));
#46701=CARTESIAN_POINT('Ctrl Pts',(185.200929512,-2.40476158067637,339.292357222803));
#46702=CARTESIAN_POINT('Ctrl Pts',(185.193306446513,-2.28646890749794,339.356531596598));
#46703=CARTESIAN_POINT('Ctrl Pts',(185.185683381027,-2.16559473885085,339.415810513322));
#46704=CARTESIAN_POINT('Ctrl Pts',(185.178067826808,-2.04483967167305,339.475031020493));
#46705=CARTESIAN_POINT('Ctrl Pts',(185.17045227259,-1.92150852917018,339.529365485536));
#46706=CARTESIAN_POINT('Ctrl Pts',(185.162836718371,-1.79604366280304,339.578581682552));
#46707=CARTESIAN_POINT('Ctrl Pts',(185.154945478167,-1.66603692011077,339.629579524793));
#46708=CARTESIAN_POINT('Ctrl Pts',(185.147054237962,-1.53373942709063,339.675081300838));
#46709=CARTESIAN_POINT('Ctrl Pts',(185.139162997758,-1.39966974248112,339.714881512242));
#46710=CARTESIAN_POINT('Ctrl Pts',(185.13155580986,-1.27042601706156,339.753249079148));
#46711=CARTESIAN_POINT('Ctrl Pts',(185.123948621962,-1.13953589971074,339.786318319177));
#46712=CARTESIAN_POINT('Ctrl Pts',(185.116341434065,-1.00748186865543,339.813955062818));
#46713=CARTESIAN_POINT('Ctrl Pts',(185.108735312539,-0.875446348877749,
339.841587932352));
#46714=CARTESIAN_POINT('Ctrl Pts',(185.101129191014,-0.742247636966592,
339.8637897361));
#46715=CARTESIAN_POINT('Ctrl Pts',(185.093523069488,-0.608379719212441,
339.88047714673));
#46716=CARTESIAN_POINT('Ctrl Pts',(185.085916236046,-0.47449927169694,339.897166119266));
#46717=CARTESIAN_POINT('Ctrl Pts',(185.078309402603,-0.339949896725272,
339.908339622693));
#46718=CARTESIAN_POINT('Ctrl Pts',(185.07070256916,-0.205231435088321,339.913966129366));
#46719=CARTESIAN_POINT('Ctrl Pts',(185.063093244994,-0.0704688622632049,
339.919594478338));
#46720=CARTESIAN_POINT('Ctrl Pts',(185.055483920828,0.0644625019824259,
339.919672203098));
#46721=CARTESIAN_POINT('Ctrl Pts',(185.047874596661,0.199062687180237,339.914219888148));
#46722=CARTESIAN_POINT('Ctrl Pts',(185.040256878758,0.333811347922438,339.908761558828));
#46723=CARTESIAN_POINT('Ctrl Pts',(185.032639160855,0.468227695011502,339.897761033209));
#46724=CARTESIAN_POINT('Ctrl Pts',(185.025021442952,0.601816548656929,339.881290803083));
#46725=CARTESIAN_POINT('Ctrl Pts',(185.017398721146,0.735493153717287,339.864809754045));
#46726=CARTESIAN_POINT('Ctrl Pts',(185.009775999341,0.868340784862089,339.842851917027));
#46727=CARTESIAN_POINT('Ctrl Pts',(185.002153277536,0.999875724090086,339.815540634121));
#46728=CARTESIAN_POINT('Ctrl Pts',(184.994519720211,1.13159763714151,339.788190528869));
#46729=CARTESIAN_POINT('Ctrl Pts',(184.986886162886,1.26200274453607,339.755471894781));
#46730=CARTESIAN_POINT('Ctrl Pts',(184.979252605561,1.39062354056651,339.717557549296));
#46731=CARTESIAN_POINT('Ctrl Pts',(184.977317388195,1.42323077563327,339.707945713467));
#46732=CARTESIAN_POINT('Ctrl Pts',(184.975382170829,1.45572344117559,339.698000189718));
#46733=CARTESIAN_POINT('Ctrl Pts',(184.973446953463,1.48809415044879,339.687724273238));
#46734=CARTESIAN_POINT('Ctrl Pts',(184.96565848958,1.61837310746679,339.646367883108));
#46735=CARTESIAN_POINT('Ctrl Pts',(184.957870025698,1.74712778550745,339.599512591787));
#46736=CARTESIAN_POINT('Ctrl Pts',(184.950081561815,1.87386032935745,339.547288260993));
#46737=CARTESIAN_POINT('Ctrl Pts',(184.942302612285,2.00043805729286,339.49512772721));
#46738=CARTESIAN_POINT('Ctrl Pts',(184.934523662756,2.12499820984358,339.437611352051));
#46739=CARTESIAN_POINT('Ctrl Pts',(184.926744713226,2.24705760125291,339.374918879151));
#46740=CARTESIAN_POINT('Ctrl Pts',(184.918973425117,2.36899677741104,339.312288151532));
#46741=CARTESIAN_POINT('Ctrl Pts',(184.911202137008,2.48843975011919,339.244491648805));
#46742=CARTESIAN_POINT('Ctrl Pts',(184.903430848899,2.60492317208862,339.171757223283));
#46743=CARTESIAN_POINT('Ctrl Pts',(184.89566537582,2.72131943289969,339.099077222817));
#46744=CARTESIAN_POINT('Ctrl Pts',(184.88789990274,2.83476022230911,339.021466860022));
#46745=CARTESIAN_POINT('Ctrl Pts',(184.88013442966,2.94480698156192,338.939199779631));
#46746=CARTESIAN_POINT('Ctrl Pts',(184.872372254371,3.05480700686631,338.856967635894));
#46747=CARTESIAN_POINT('Ctrl Pts',(184.864610079082,3.1614155579396,338.770082940957));
#46748=CARTESIAN_POINT('Ctrl Pts',(184.856847903794,3.26422343308172,338.678862384137));
#46749=CARTESIAN_POINT('Ctrl Pts',(184.849087352215,3.367009802633,338.587660909046));
#46750=CARTESIAN_POINT('Ctrl Pts',(184.841326800636,3.46599678677146,338.492125634548));
#46751=CARTESIAN_POINT('Ctrl Pts',(184.833566249057,3.5608089294898,338.39261297972));
#46752=CARTESIAN_POINT('Ctrl Pts',(184.825805657541,3.65562156012198,338.293099812789));
#46753=CARTESIAN_POINT('Ctrl Pts',(184.818045066026,3.74625903790054,338.189609506535));
#46754=CARTESIAN_POINT('Ctrl Pts',(184.81028447451,3.83238365846775,338.082534437246));
#46755=CARTESIAN_POINT('Ctrl Pts',(184.802522179749,3.91852718112861,337.97543586779));
#46756=CARTESIAN_POINT('Ctrl Pts',(184.794759884987,4.00015563160498,337.864751272943));
#46757=CARTESIAN_POINT('Ctrl Pts',(184.786997590225,4.07697263100072,337.750904801801));
#46758=CARTESIAN_POINT('Ctrl Pts',(184.779227208787,4.15386965753146,337.636939726613));
#46759=CARTESIAN_POINT('Ctrl Pts',(184.771456827349,4.22594500175642,337.519806518169));
#46760=CARTESIAN_POINT('Ctrl Pts',(184.763686445911,4.29294626376753,337.399957382727));
#46761=CARTESIAN_POINT('Ctrl Pts',(184.755911974034,4.35998279619555,337.280045156996));
#46762=CARTESIAN_POINT('Ctrl Pts',(184.748137502157,4.42193974796744,337.157414502478));
#46763=CARTESIAN_POINT('Ctrl Pts',(184.740363030279,4.47861191896625,337.032539874589));
#46764=CARTESIAN_POINT('Ctrl Pts',(184.732576370516,4.53537293380594,336.907469483217));
#46765=CARTESIAN_POINT('Ctrl Pts',(184.724789710753,4.5868324660391,336.780148449852));
#46766=CARTESIAN_POINT('Ctrl Pts',(184.717003050991,4.63283415774104,336.651069571329));
#46767=CARTESIAN_POINT('Ctrl Pts',(184.70973834039,4.6757523007587,336.530643005173));
#46768=CARTESIAN_POINT('Ctrl Pts',(184.70247362979,4.71392020384367,336.40868675833));
#46769=CARTESIAN_POINT('Ctrl Pts',(184.69520891919,4.74725098005436,336.285609269908));
#46770=CARTESIAN_POINT('Ctrl Pts',(184.687424242118,4.78296738276084,336.153722598179));
#46771=CARTESIAN_POINT('Ctrl Pts',(184.679639565047,4.81323836545848,336.020144099434));
#46772=CARTESIAN_POINT('Ctrl Pts',(184.671854887975,4.8379041263559,335.885362483217));
#46773=CARTESIAN_POINT('Ctrl Pts',(184.664079600278,4.86254013700524,335.750743431883));
#46774=CARTESIAN_POINT('Ctrl Pts',(184.656304312581,4.88158430898547,335.61492453046));
#46775=CARTESIAN_POINT('Ctrl Pts',(184.648529024885,4.89492673991659,335.478409106675));
#46776=CARTESIAN_POINT('Ctrl Pts',(184.640761269935,4.9082562446166,335.342025939892));
#46777=CARTESIAN_POINT('Ctrl Pts',(184.632993514986,4.91589496413867,335.204947979227));
#46778=CARTESIAN_POINT('Ctrl Pts',(184.625225760037,4.91778419782772,335.067687857818));
#46779=CARTESIAN_POINT('Ctrl Pts',(184.617463687663,4.91967204942996,334.930528150351));
#46780=CARTESIAN_POINT('Ctrl Pts',(184.609701615289,4.91581878241357,334.793186935617));
#46781=CARTESIAN_POINT('Ctrl Pts',(184.601939542914,4.90621762379767,334.65618072998));
#46782=CARTESIAN_POINT('Ctrl Pts',(184.594180552715,4.89662027762425,334.519228926973));
#46783=CARTESIAN_POINT('Ctrl Pts',(184.586421562516,4.88127960618991,334.382612256533));
#46784=CARTESIAN_POINT('Ctrl Pts',(184.578662572317,4.86024092128453,334.246845799606));
#46785=CARTESIAN_POINT('Ctrl Pts',(184.570905073578,4.83920628050715,334.111105440172));
#46786=CARTESIAN_POINT('Ctrl Pts',(184.563147574839,4.81247586460318,333.976215354093));
#46787=CARTESIAN_POINT('Ctrl Pts',(184.555390076099,4.78014665025893,333.842683680009));
#46788=CARTESIAN_POINT('Ctrl Pts',(184.547632401474,4.74781670291267,333.709148978354));
#46789=CARTESIAN_POINT('Ctrl Pts',(184.539874726848,4.70988779598382,333.576973128845));
#46790=CARTESIAN_POINT('Ctrl Pts',(184.532117052223,4.66650755751355,333.446651913392));
#46791=CARTESIAN_POINT('Ctrl Pts',(184.524357534611,4.62311701322361,333.316299737599));
#46792=CARTESIAN_POINT('Ctrl Pts',(184.516598016999,4.57427268320736,333.187803442396));
#46793=CARTESIAN_POINT('Ctrl Pts',(184.508838499386,4.52017125212072,333.061641180276));
#46794=CARTESIAN_POINT('Ctrl Pts',(184.501070656481,4.46601177486198,332.935343556924));
#46795=CARTESIAN_POINT('Ctrl Pts',(184.493302813575,4.40658408313757,332.811385327803));
#46796=CARTESIAN_POINT('Ctrl Pts',(184.48553497067,4.34213222882723,332.690222787826));
#46797=CARTESIAN_POINT('Ctrl Pts',(184.47776291104,4.27764538723547,332.56899447553));
#46798=CARTESIAN_POINT('Ctrl Pts',(184.46999085141,4.2081291455521,332.450565212436));
#46799=CARTESIAN_POINT('Ctrl Pts',(184.46221879178,4.13387175970386,332.335363563857));
#46800=CARTESIAN_POINT('Ctrl Pts',(184.454434302843,4.05949561925503,332.219977681405));
#46801=CARTESIAN_POINT('Ctrl Pts',(184.446649813906,3.98036340801068,332.107830046665));
#46802=CARTESIAN_POINT('Ctrl Pts',(184.438865324969,3.89680519102534,331.999318016567));
#46803=CARTESIAN_POINT('Ctrl Pts',(184.431567178284,3.81846734133424,331.897585363452));
#46804=CARTESIAN_POINT('Ctrl Pts',(184.4242690316,3.73623980330836,331.799048106545));
#46805=CARTESIAN_POINT('Ctrl Pts',(184.416970884915,3.65042360366862,331.704003856756));
#46806=CARTESIAN_POINT('Ctrl Pts',(184.409204894486,3.55910620297908,331.602866846755));
#46807=CARTESIAN_POINT('Ctrl Pts',(184.401438904057,3.46343492066193,331.50536424042));
#46808=CARTESIAN_POINT('Ctrl Pts',(184.393672913627,3.3637306636303,331.411894777873));
#46809=CARTESIAN_POINT('Ctrl Pts',(184.385916602342,3.26415067302245,331.318541811013));
#46810=CARTESIAN_POINT('Ctrl Pts',(184.378160291057,3.16054799150972,331.229212252213));
#46811=CARTESIAN_POINT('Ctrl Pts',(184.370403979771,3.05328302497456,331.144271037547));
#46812=CARTESIAN_POINT('Ctrl Pts',(184.362655469153,2.94612593681738,331.059415249844));
#46813=CARTESIAN_POINT('Ctrl Pts',(184.354906958534,2.83531419825708,330.978939265473));
#46814=CARTESIAN_POINT('Ctrl Pts',(184.347158447916,2.72124395620983,330.90317020206));
#46815=CARTESIAN_POINT('Ctrl Pts',(184.339415866339,2.60726099896148,330.827459115971));
#46816=CARTESIAN_POINT('Ctrl Pts',(184.331673284762,2.49002482595842,330.756447998258));
#46817=CARTESIAN_POINT('Ctrl Pts',(184.323930703185,2.36996315621844,330.69042256124));
#46818=CARTESIAN_POINT('Ctrl Pts',(184.316191510396,2.2499540352959,330.62442602236));
#46819=CARTESIAN_POINT('Ctrl Pts',(184.308452317607,2.12712221996486,330.563411012492));
#46820=CARTESIAN_POINT('Ctrl Pts',(184.300713124817,2.00192259021132,330.507618782282));
#46821=CARTESIAN_POINT('Ctrl Pts',(184.292975607458,1.87675006448171,330.451838630335));
#46822=CARTESIAN_POINT('Ctrl Pts',(184.285238090099,1.74921110162522,330.40127916862));
#46823=CARTESIAN_POINT('Ctrl Pts',(184.277500572741,1.61978288774046,330.356134534778));
#46824=CARTESIAN_POINT('Ctrl Pts',(184.269763044928,1.49035449899087,330.310989839942));
#46825=CARTESIAN_POINT('Ctrl Pts',(184.262025517115,1.35903722411994,330.271260116828));
#46826=CARTESIAN_POINT('Ctrl Pts',(184.254287989302,1.2263254346455,330.237090281053));
#46827=CARTESIAN_POINT('Ctrl Pts',(184.246548765495,1.09358455597324,330.202912955565));
#46828=CARTESIAN_POINT('Ctrl Pts',(184.238809541688,0.959448933976456,330.174298039999));
#46829=CARTESIAN_POINT('Ctrl Pts',(184.23107031788,0.824424805284255,330.15133968988));
#46830=CARTESIAN_POINT('Ctrl Pts',(184.223322887694,0.689257502135376,330.128356995599));
#46831=CARTESIAN_POINT('Ctrl Pts',(184.215575457508,0.553200197285356,330.11104291412));
#46832=CARTESIAN_POINT('Ctrl Pts',(184.207828027322,0.416766496517759,330.099439955487));
#46833=CARTESIAN_POINT('Ctrl Pts',(184.200076477443,0.280260247199368,330.087830826986));
#46834=CARTESIAN_POINT('Ctrl Pts',(184.192324927565,0.143377594536541,330.081938889113));
#46835=CARTESIAN_POINT('Ctrl Pts',(184.184573377687,0.00663283769598015,
330.081754472582));
#46836=CARTESIAN_POINT('Ctrl Pts',(184.176809358013,-0.130331898273189,
330.081569759384));
#46837=CARTESIAN_POINT('Ctrl Pts',(184.169045338339,-0.267157903322725,
330.087110899134));
#46838=CARTESIAN_POINT('Ctrl Pts',(184.161281318665,-0.403334414585777,
330.098316165591));
#46839=CARTESIAN_POINT('Ctrl Pts',(184.153765162657,-0.535163537412979,
330.109163707757));
#46840=CARTESIAN_POINT('Ctrl Pts',(184.146249006649,-0.66638369400634,330.125319154275));
#46841=CARTESIAN_POINT('Ctrl Pts',(184.138732850642,-0.796541975815797,
330.146681141398));
#46842=CARTESIAN_POINT('Ctrl Pts',(184.1309552338,-0.931228009951312,330.168786237492));
#46843=CARTESIAN_POINT('Ctrl Pts',(184.123177616959,-1.06520495165966,330.196536910097));
#46844=CARTESIAN_POINT('Ctrl Pts',(184.115400000118,-1.19796258057449,330.229877494441));
#46845=CARTESIAN_POINT('Ctrl Pts',(184.107631935139,-1.33055716692858,330.26317713248));
#46846=CARTESIAN_POINT('Ctrl Pts',(184.09986387016,-1.46193504483815,330.30205292825));
#46847=CARTESIAN_POINT('Ctrl Pts',(184.092095805181,-1.59159321286036,330.346397727859));
#46848=CARTESIAN_POINT('Ctrl Pts',(184.084335426717,-1.72112308386848,330.3906986482));
#46849=CARTESIAN_POINT('Ctrl Pts',(184.076575048254,-1.84893626423228,330.440457677262));
#46850=CARTESIAN_POINT('Ctrl Pts',(184.06881466979,-1.97454236023251,330.495517173954));
#46851=CARTESIAN_POINT('Ctrl Pts',(184.061060119138,-2.10005412982255,330.550535322614));
#46852=CARTESIAN_POINT('Ctrl Pts',(184.053305568486,-2.22336175788803,330.610845859634));
#46853=CARTESIAN_POINT('Ctrl Pts',(184.045551017834,-2.3439927091478,330.67624223135));
#46854=CARTESIAN_POINT('Ctrl Pts',(184.037799743937,-2.46457268671841,330.741610969244));
#46855=CARTESIAN_POINT('Ctrl Pts',(184.03004847004,-2.58247789444863,330.812061081661));
#46856=CARTESIAN_POINT('Ctrl Pts',(184.022297196143,-2.69725858685646,330.887339160819));
#46857=CARTESIAN_POINT('Ctrl Pts',(184.014547531043,-2.81201545622994,330.962601615814));
#46858=CARTESIAN_POINT('Ctrl Pts',(184.006797865943,-2.92364877381903,331.042689830283));
#46859=CARTESIAN_POINT('Ctrl Pts',(183.999048200843,-3.03173642524737,331.127306194607));
#46860=CARTESIAN_POINT('Ctrl Pts',(183.991298469927,-3.1398249946362,331.211923277557));
#46861=CARTESIAN_POINT('Ctrl Pts',(183.983548739011,-3.24436753026002,331.301068346297));
#46862=CARTESIAN_POINT('Ctrl Pts',(183.975799008096,-3.34497407275734,331.394402751959));
#46863=CARTESIAN_POINT('Ctrl Pts',(183.968047537065,-3.44560320531852,331.487758114809));
#46864=CARTESIAN_POINT('Ctrl Pts',(183.960296066035,-3.54229429981986,331.585304420843));
#46865=CARTESIAN_POINT('Ctrl Pts',(183.952544595004,-3.63469370544349,331.686665617522));
#46866=CARTESIAN_POINT('Ctrl Pts',(183.944784916504,-3.72719094609492,331.78813413822));
#46867=CARTESIAN_POINT('Ctrl Pts',(183.937025238003,-3.81538715692437,331.893425329381));
#46868=CARTESIAN_POINT('Ctrl Pts',(183.929265559502,-3.89896816031605,332.002129030905));
#46869=CARTESIAN_POINT('Ctrl Pts',(183.921501741213,-3.98259375416966,332.110890725849));
#46870=CARTESIAN_POINT('Ctrl Pts',(183.913737922924,-4.0615990095167,332.223068239711));
#46871=CARTESIAN_POINT('Ctrl Pts',(183.905974104635,-4.13571326520763,332.338222614401));
#46872=CARTESIAN_POINT('Ctrl Pts',(183.898197906043,-4.2099457046265,332.453560616021));
#46873=CARTESIAN_POINT('Ctrl Pts',(183.89042170745,-4.27927136155874,332.571884627123));
#46874=CARTESIAN_POINT('Ctrl Pts',(183.882645508857,-4.34346527456366,332.692730516138));
#46875=CARTESIAN_POINT('Ctrl Pts',(183.875261944694,-4.40441791998991,332.807474676131));
#46876=CARTESIAN_POINT('Ctrl Pts',(183.867878380531,-4.46074422753017,332.924492031672));
#46877=CARTESIAN_POINT('Ctrl Pts',(183.860494816367,-4.51229256241462,333.043370527239));
#46878=CARTESIAN_POINT('Ctrl Pts',(183.851901462611,-4.57228704034016,333.181727145238));
#46879=CARTESIAN_POINT('Ctrl Pts',(183.843308108854,-4.62597157335744,333.322977368862));
#46880=CARTESIAN_POINT('Ctrl Pts',(183.834714755098,-4.67308623617143,333.466556785595));
#46881=CARTESIAN_POINT('Ctrl Pts',(183.826155630823,-4.72001322947433,333.609564289524));
#46882=CARTESIAN_POINT('Ctrl Pts',(183.817596506549,-4.76042246392151,333.754882245335));
#46883=CARTESIAN_POINT('Ctrl Pts',(183.809037382274,-4.79410300807903,333.901929232505));
#46884=CARTESIAN_POINT('Ctrl Pts',(183.800500556196,-4.82769580781691,334.048593133448));
#46885=CARTESIAN_POINT('Ctrl Pts',(183.791963730118,-4.85459480847109,334.196976842495));
#46886=CARTESIAN_POINT('Ctrl Pts',(183.78342690404,-4.87463832611427,334.346483166186));
#46887=CARTESIAN_POINT('Ctrl Pts',(183.77492515661,-4.89459948299498,334.495375153859));
#46888=CARTESIAN_POINT('Ctrl Pts',(183.766423409181,-4.90776128352893,334.645380310851));
#46889=CARTESIAN_POINT('Ctrl Pts',(183.757921661751,-4.9140129244875,334.795892086215));
#46890=CARTESIAN_POINT('Ctrl Pts',(183.754126524013,-4.91680362589586,334.863079793613));
#46891=CARTESIAN_POINT('Ctrl Pts',(183.750331386275,-4.91821801072524,334.930368253243));
#46892=CARTESIAN_POINT('Ctrl Pts',(183.746536248537,-4.91824946343417,334.997702625515));
#46893=CARTESIAN_POINT('',(185.231676812499,2.85706463458485,339.00329423554));
#46894=CARTESIAN_POINT('Origin',(185.231676812499,0.,335.));
#46895=CARTESIAN_POINT('',(184.091817376473,-4.91824940656917,334.997583953229));
#46896=CARTESIAN_POINT('Ctrl Pts',(185.231676812499,2.85706463458463,339.00329423554));
#46897=CARTESIAN_POINT('Ctrl Pts',(185.222579442691,2.9878247153018,338.909973590028));
#46898=CARTESIAN_POINT('Ctrl Pts',(185.213482072884,3.11390580132401,338.810317313122));
#46899=CARTESIAN_POINT('Ctrl Pts',(185.204384703076,3.23476879094588,338.704787973909));
#46900=CARTESIAN_POINT('Ctrl Pts',(185.1950657941,3.3585750363445,338.596688784007));
#46901=CARTESIAN_POINT('Ctrl Pts',(185.185746885124,3.476905728084,338.48242695956));
#46902=CARTESIAN_POINT('Ctrl Pts',(185.176427976148,3.58922166565946,338.362539352522));
#46903=CARTESIAN_POINT('Ctrl Pts',(185.167314876684,3.69905708878743,338.245299481396));
#46904=CARTESIAN_POINT('Ctrl Pts',(185.15820177722,3.80314056875857,338.122679795787));
#46905=CARTESIAN_POINT('Ctrl Pts',(185.149088677757,3.90100650166295,337.995218078285));
#46906=CARTESIAN_POINT('Ctrl Pts',(185.139666864024,4.00218772921781,337.863438482869));
#46907=CARTESIAN_POINT('Ctrl Pts',(185.130245050292,4.09672267977152,337.726483109028));
#46908=CARTESIAN_POINT('Ctrl Pts',(185.120823236559,4.18414116197834,337.584984680639));
#46909=CARTESIAN_POINT('Ctrl Pts',(185.111401422827,4.27155964418516,337.44348625225));
#46910=CARTESIAN_POINT('Ctrl Pts',(185.101979609095,4.35186152211415,337.297444838005));
#46911=CARTESIAN_POINT('Ctrl Pts',(185.092557795362,4.424623503881,337.147531120008));
#46912=CARTESIAN_POINT('Ctrl Pts',(185.084782311257,4.48467135122184,337.023812718805));
#46913=CARTESIAN_POINT('Ctrl Pts',(185.077006827152,4.53954842512907,336.897528290713));
#46914=CARTESIAN_POINT('Ctrl Pts',(185.069231343047,4.58904037605888,336.769149934121));
#46915=CARTESIAN_POINT('Ctrl Pts',(185.061456840608,4.63852607856139,336.640787785475));
#46916=CARTESIAN_POINT('Ctrl Pts',(185.053682338168,4.68262787275381,336.510332596953));
#46917=CARTESIAN_POINT('Ctrl Pts',(185.045907835729,4.72117985492044,336.378275676341));
#46918=CARTESIAN_POINT('Ctrl Pts',(185.038129436014,4.75975116278613,336.246152556998));
#46919=CARTESIAN_POINT('Ctrl Pts',(185.030351036299,4.79276698724958,336.112426473256));
#46920=CARTESIAN_POINT('Ctrl Pts',(185.022572636584,4.82011148302006,335.977603372416));
#46921=CARTESIAN_POINT('Ctrl Pts',(185.014792468078,4.84746219687077,335.842749613089));
#46922=CARTESIAN_POINT('Ctrl Pts',(185.007012299572,4.86913894489199,335.706798722194));
#46923=CARTESIAN_POINT('Ctrl Pts',(184.999232131065,4.88507734499522,335.570265197881));
#46924=CARTESIAN_POINT('Ctrl Pts',(184.991443525169,4.90103302987852,335.433583606515));
#46925=CARTESIAN_POINT('Ctrl Pts',(184.983654919272,4.91123789581269,335.296318506361));
#46926=CARTESIAN_POINT('Ctrl Pts',(184.975866313375,4.91567957915306,335.158988482594));
#46927=CARTESIAN_POINT('Ctrl Pts',(184.968390468325,4.91994290135146,335.027173111266));
#46928=CARTESIAN_POINT('Ctrl Pts',(184.960914623275,4.91889694997854,334.895298241123));
#46929=CARTESIAN_POINT('Ctrl Pts',(184.953438778225,4.9125758885357,334.76381955653));
#46930=CARTESIAN_POINT('Ctrl Pts',(184.945564587241,4.90591801311239,334.625335108822));
#46931=CARTESIAN_POINT('Ctrl Pts',(184.937690396256,4.89339311908122,334.486988322013));
#46932=CARTESIAN_POINT('Ctrl Pts',(184.929816205271,4.87501593909813,334.349306019669));
#46933=CARTESIAN_POINT('Ctrl Pts',(184.921949019059,4.85665510720187,334.21174619761));
#46934=CARTESIAN_POINT('Ctrl Pts',(184.914081832846,4.83245240543065,334.074850055284));
#46935=CARTESIAN_POINT('Ctrl Pts',(184.906214646633,4.8024745030993,333.939141051043));
#46936=CARTESIAN_POINT('Ctrl Pts',(184.898352758719,4.77251678992486,333.80352344247));
#46937=CARTESIAN_POINT('Ctrl Pts',(184.890490870804,4.73679170318165,333.66909174716));
#46938=CARTESIAN_POINT('Ctrl Pts',(184.882628982889,4.69541726479236,333.536360778064));
#46939=CARTESIAN_POINT('Ctrl Pts',(184.874770691361,4.6540617529575,333.403690526165));
#46940=CARTESIAN_POINT('Ctrl Pts',(184.866912399832,4.60706214927302,333.272719810437));
#46941=CARTESIAN_POINT('Ctrl Pts',(184.859054108303,4.55458669943747,333.143949607417));
#46942=CARTESIAN_POINT('Ctrl Pts',(184.851196167121,4.50211358911507,333.01518514536));
#46943=CARTESIAN_POINT('Ctrl Pts',(184.843338225938,4.44416525229962,332.888621353558));
#46944=CARTESIAN_POINT('Ctrl Pts',(184.835480284756,4.38095863009341,332.764740609256));
#46945=CARTESIAN_POINT('Ctrl Pts',(184.827622207873,4.31775091636225,332.640857725638));
#46946=CARTESIAN_POINT('Ctrl Pts',(184.819764130991,4.24928490721179,332.519658318505));
#46947=CARTESIAN_POINT('Ctrl Pts',(184.811906054108,4.17582400184014,332.401601076017));
#46948=CARTESIAN_POINT('Ctrl Pts',(184.804046302178,4.10234743734809,332.283518668136));
#46949=CARTESIAN_POINT('Ctrl Pts',(184.796186550247,4.02387405542442,332.168580079521));
#46950=CARTESIAN_POINT('Ctrl Pts',(184.788326798316,3.94071103870938,332.057215676966));
#46951=CARTESIAN_POINT('Ctrl Pts',(184.780463831184,3.85751400236523,331.945805718396));
#46952=CARTESIAN_POINT('Ctrl Pts',(184.772600864051,3.76962373634181,331.837973160097));
#46953=CARTESIAN_POINT('Ctrl Pts',(184.764737896919,3.67738806029112,331.734115722116));
#46954=CARTESIAN_POINT('Ctrl Pts',(184.756865106111,3.58503714868493,331.630128528817));
#46955=CARTESIAN_POINT('Ctrl Pts',(184.748992315303,3.48833023282654,331.530126659555));
#46956=CARTESIAN_POINT('Ctrl Pts',(184.741119524495,3.38765294139393,331.434471902906));
#46957=CARTESIAN_POINT('Ctrl Pts',(184.733241550299,3.28690936477144,331.338754167867));
#46958=CARTESIAN_POINT('Ctrl Pts',(184.725363576103,3.18219048574338,331.247389498811));
#46959=CARTESIAN_POINT('Ctrl Pts',(184.717485601907,3.07391490856393,331.160699256712));
#46960=CARTESIAN_POINT('Ctrl Pts',(184.70959467446,2.96546130074035,331.073866475363));
#46961=CARTESIAN_POINT('Ctrl Pts',(184.701703747012,2.85343961281812,330.991723703143));
#46962=CARTESIAN_POINT('Ctrl Pts',(184.693812819564,2.7382981212166,330.914549417525));
#46963=CARTESIAN_POINT('Ctrl Pts',(184.68760879436,2.64777128255249,330.85387325287));
#46964=CARTESIAN_POINT('Ctrl Pts',(184.681404769155,2.5553165529785,330.796267481384));
#46965=CARTESIAN_POINT('Ctrl Pts',(184.675200743951,2.4611617124476,330.741847103769));
#46966=CARTESIAN_POINT('Ctrl Pts',(184.667489928554,2.34413920364659,330.674209485963));
#46967=CARTESIAN_POINT('Ctrl Pts',(184.659779113157,2.22411053131831,330.611274870948));
#46968=CARTESIAN_POINT('Ctrl Pts',(184.65206829776,2.10149395557967,330.553326387381));
#46969=CARTESIAN_POINT('Ctrl Pts',(184.644367804453,1.97904152063397,330.495455476605));
#46970=CARTESIAN_POINT('Ctrl Pts',(184.636667311146,1.85400842801085,330.442557590228));
#46971=CARTESIAN_POINT('Ctrl Pts',(184.628966817839,1.7268408492561,330.394872016562));
#46972=CARTESIAN_POINT('Ctrl Pts',(184.621274712016,1.59981178319868,330.347238382687));
#46973=CARTESIAN_POINT('Ctrl Pts',(184.613582606194,1.47065322559616,330.304805906676));
#46974=CARTESIAN_POINT('Ctrl Pts',(184.605890500372,1.3398344216355,330.267767251592));
#46975=CARTESIAN_POINT('Ctrl Pts',(184.598204855771,1.20912550296542,330.23075970827));
#46976=CARTESIAN_POINT('Ctrl Pts',(184.59051921117,1.0767594938103,330.199137079345));
#46977=CARTESIAN_POINT('Ctrl Pts',(184.582833566569,0.943223598027069,330.173043162962));
#46978=CARTESIAN_POINT('Ctrl Pts',(184.575088947532,0.808663038133427,330.146749019522));
#46979=CARTESIAN_POINT('Ctrl Pts',(184.567344328495,0.672914944454686,330.126068941496));
#46980=CARTESIAN_POINT('Ctrl Pts',(184.559599709458,0.536491694095676,330.111098311004));
#46981=CARTESIAN_POINT('Ctrl Pts',(184.55192014685,0.401214427747725,330.096253436958));
#46982=CARTESIAN_POINT('Ctrl Pts',(184.544240584243,0.265273708744855,330.087022482791));
#46983=CARTESIAN_POINT('Ctrl Pts',(184.536561021635,0.129176771301089,330.083446692625));
#46984=CARTESIAN_POINT('Ctrl Pts',(184.528881768299,-0.00691468524943978,
330.079871046464));
#46985=CARTESIAN_POINT('Ctrl Pts',(184.521202514962,-0.143161949681559,
330.081950121998));
#46986=CARTESIAN_POINT('Ctrl Pts',(184.513523261626,-0.279056173881734,
330.089673054234));
#46987=CARTESIAN_POINT('Ctrl Pts',(184.50584258536,-0.414975578638653,330.097397417492));
#46988=CARTESIAN_POINT('Ctrl Pts',(184.498161909095,-0.550541415532521,
330.110767694871));
#46989=CARTESIAN_POINT('Ctrl Pts',(184.490481232829,-0.685248845503751,
330.129721046774));
#46990=CARTESIAN_POINT('Ctrl Pts',(184.482688022566,-0.821929951359796,
330.148952095116));
#46991=CARTESIAN_POINT('Ctrl Pts',(184.474894812304,-0.957726877239136,
330.17393105805));
#46992=CARTESIAN_POINT('Ctrl Pts',(184.467101602041,-1.09212301522409,330.204538564213));
#46993=CARTESIAN_POINT('Ctrl Pts',(184.459408829424,-1.22478707731167,330.23475160574));
#46994=CARTESIAN_POINT('Ctrl Pts',(184.451716056807,-1.35608587604265,330.270448800903));
#46995=CARTESIAN_POINT('Ctrl Pts',(184.444023284189,-1.48553870176006,330.311465279208));
#46996=CARTESIAN_POINT('Ctrl Pts',(184.436179855104,-1.61752675196568,330.353285030671));
#46997=CARTESIAN_POINT('Ctrl Pts',(184.428336426019,-1.74759536268877,330.400634423609));
#46998=CARTESIAN_POINT('Ctrl Pts',(184.420492996933,-1.87525817414061,330.453288018489));
#46999=CARTESIAN_POINT('Ctrl Pts',(184.412649567848,-2.00292098559246,330.505941613368));
#47000=CARTESIAN_POINT('Ctrl Pts',(184.404806138762,-2.12817763568885,330.563899166777));
#47001=CARTESIAN_POINT('Ctrl Pts',(184.396962709677,-2.25057076624572,330.626887345538));
#47002=CARTESIAN_POINT('Ctrl Pts',(184.389174245794,-2.37210618990496,330.689434115576));
#47003=CARTESIAN_POINT('Ctrl Pts',(184.381385781912,-2.49121980444608,330.757147720362));
#47004=CARTESIAN_POINT('Ctrl Pts',(184.373597318029,-2.60744245830814,330.82981692379));
#47005=CARTESIAN_POINT('Ctrl Pts',(184.365818368499,-2.72352313509079,330.90239735484));
#47006=CARTESIAN_POINT('Ctrl Pts',(184.358039418969,-2.83671955153112,330.979921133902));
#47007=CARTESIAN_POINT('Ctrl Pts',(184.35026046944,-2.94658535540073,331.06213029598));
#47008=CARTESIAN_POINT('Ctrl Pts',(184.342489181331,-3.05634295337928,331.144258490957));
#47009=CARTESIAN_POINT('Ctrl Pts',(184.334717893222,-3.16277615748277,331.23106265316));
#47010=CARTESIAN_POINT('Ctrl Pts',(184.326946605113,-3.26546621479366,331.322240700842));
#47011=CARTESIAN_POINT('Ctrl Pts',(184.319181132033,-3.36807943212012,331.413350522643));
#47012=CARTESIAN_POINT('Ctrl Pts',(184.311415658953,-3.4669547881139,331.508827457513));
#47013=CARTESIAN_POINT('Ctrl Pts',(184.303650185873,-3.56170562253267,331.608328417886));
#47014=CARTESIAN_POINT('Ctrl Pts',(184.295888010585,-3.65641621877765,331.707787122832));
#47015=CARTESIAN_POINT('Ctrl Pts',(184.288125835296,-3.74700550970919,331.811266172619));
#47016=CARTESIAN_POINT('Ctrl Pts',(184.280363660007,-3.83312297281925,331.918384946534));
#47017=CARTESIAN_POINT('Ctrl Pts',(184.272603108428,-3.91922242167776,332.025481313096));
#47018=CARTESIAN_POINT('Ctrl Pts',(184.264842556849,-4.00085165976164,332.136215585984));
#47019=CARTESIAN_POINT('Ctrl Pts',(184.25708200527,-4.07770007525033,332.250173612971));
#47020=CARTESIAN_POINT('Ctrl Pts',(184.249321413755,-4.15454888620958,332.364132226398));
#47021=CARTESIAN_POINT('Ctrl Pts',(184.241560822239,-4.2266166077965,332.481314304259));
#47022=CARTESIAN_POINT('Ctrl Pts',(184.233800230724,-4.29363585803693,332.601276551772));
#47023=CARTESIAN_POINT('Ctrl Pts',(184.226037935962,-4.36066981724358,332.721265127849));
#47024=CARTESIAN_POINT('Ctrl Pts',(184.2182756412,-4.42265291031737,332.844034748019));
#47025=CARTESIAN_POINT('Ctrl Pts',(184.210513346439,-4.4793638093941,332.96911769775));
#47026=CARTESIAN_POINT('Ctrl Pts',(184.202742965001,-4.53613378928388,333.094330957572));
#47027=CARTESIAN_POINT('Ctrl Pts',(184.194972583563,-4.58762044218239,333.221862006101));
#47028=CARTESIAN_POINT('Ctrl Pts',(184.187202202125,-4.6336504895927,333.351222815903));
#47029=CARTESIAN_POINT('Ctrl Pts',(184.179427730247,-4.67970476787436,333.480651723075));
#47030=CARTESIAN_POINT('Ctrl Pts',(184.17165325837,-4.72029660145657,333.611911939237));
#47031=CARTESIAN_POINT('Ctrl Pts',(184.163878786493,-4.75530296609509,333.744501388632));
#47032=CARTESIAN_POINT('Ctrl Pts',(184.15609212673,-4.79036420951869,333.877298695883));
#47033=CARTESIAN_POINT('Ctrl Pts',(184.148305466967,-4.81982240259727,334.011429020029));
#47034=CARTESIAN_POINT('Ctrl Pts',(184.140518807204,-4.84360574158947,334.146380364248));
#47035=CARTESIAN_POINT('Ctrl Pts',(184.133254096604,-4.86579485478363,334.272285757665));
#47036=CARTESIAN_POINT('Ctrl Pts',(184.125989386003,-4.88304489384078,334.398905468304));
#47037=CARTESIAN_POINT('Ctrl Pts',(184.118724675403,-4.89533845131523,334.525822280601));
#47038=CARTESIAN_POINT('Ctrl Pts',(184.109755575772,-4.91051622616177,334.682515313133));
#47039=CARTESIAN_POINT('Ctrl Pts',(184.10078647614,-4.91817196805098,334.839945510906));
#47040=CARTESIAN_POINT('Ctrl Pts',(184.091817376508,-4.91824940656887,334.997583952616));
#47041=CARTESIAN_POINT('',(182.34181737656,-4.91824916970108,334.997142162596));
#47042=CARTESIAN_POINT('Ctrl Pts',(184.091817376473,-4.91824940656917,334.997583953229));
#47043=CARTESIAN_POINT('Ctrl Pts',(184.084130311134,-4.91831577608455,335.132689710906));
#47044=CARTESIAN_POINT('Ctrl Pts',(184.076443245795,-4.91281085209014,335.26801291328));
#47045=CARTESIAN_POINT('Ctrl Pts',(184.068756180455,-4.90170722235522,335.403050082261));
#47046=CARTESIAN_POINT('Ctrl Pts',(184.061077607281,-4.89061585918133,335.537938071045));
#47047=CARTESIAN_POINT('Ctrl Pts',(184.053399034107,-4.87393812510857,335.67254025952));
#47048=CARTESIAN_POINT('Ctrl Pts',(184.045720460933,-4.85169861664758,335.80635202965));
#47049=CARTESIAN_POINT('Ctrl Pts',(184.038048437324,-4.82947807774062,335.940049662832));
#47050=CARTESIAN_POINT('Ctrl Pts',(184.030376413715,-4.80170526764821,336.072957826291));
#47051=CARTESIAN_POINT('Ctrl Pts',(184.022704390106,-4.76845665061498,336.204576371056));
#47052=CARTESIAN_POINT('Ctrl Pts',(184.015036522363,-4.73522604406092,336.336123619229));
#47053=CARTESIAN_POINT('Ctrl Pts',(184.007368654621,-4.69652562755459,336.466382251169));
#47054=CARTESIAN_POINT('Ctrl Pts',(183.999700786879,-4.65248300065029,336.59486206023));
#47055=CARTESIAN_POINT('Ctrl Pts',(183.992035032746,-4.60845251387658,336.723306454471));
#47056=CARTESIAN_POINT('Ctrl Pts',(183.984369278613,-4.55908287407189,336.849972622525));
#47057=CARTESIAN_POINT('Ctrl Pts',(183.97670352448,-4.50455148146989,336.974385730623));
#47058=CARTESIAN_POINT('Ctrl Pts',(183.969038137298,-4.45002269922133,337.098792883213));
#47059=CARTESIAN_POINT('Ctrl Pts',(183.961372750116,-4.39033281619444,337.220946823846));
#47060=CARTESIAN_POINT('Ctrl Pts',(183.953707362934,-4.32570708748705,337.34039339765));
#47061=CARTESIAN_POINT('Ctrl Pts',(183.946040596582,-4.26106973121236,337.459861462478));
#47062=CARTESIAN_POINT('Ctrl Pts',(183.938373830231,-4.19149495373998,337.576620839945));
#47063=CARTESIAN_POINT('Ctrl Pts',(183.93070706388,-4.11725334028815,337.690243110647));
#47064=CARTESIAN_POINT('Ctrl Pts',(183.92303249413,-4.04293616213615,337.803981028524));
#47065=CARTESIAN_POINT('Ctrl Pts',(183.91535792438,-3.96394288019147,337.914575126835));
#47066=CARTESIAN_POINT('Ctrl Pts',(183.90768335463,-3.88058692300308,338.021626746558));
#47067=CARTESIAN_POINT('Ctrl Pts',(183.900004834352,-3.79718805785987,338.128733471715));
#47068=CARTESIAN_POINT('Ctrl Pts',(183.892326314074,-3.70942230367937,338.232293781788));
#47069=CARTESIAN_POINT('Ctrl Pts',(183.884647793795,-3.61764173005681,338.331944083482));
#47070=CARTESIAN_POINT('Ctrl Pts',(183.876957150543,-3.52571625176181,338.431751714704));
#47071=CARTESIAN_POINT('Ctrl Pts',(183.869266507291,-3.42976357394534,338.527636722327));
#47072=CARTESIAN_POINT('Ctrl Pts',(183.861575864039,-3.33017130772584,338.619273701131));
#47073=CARTESIAN_POINT('Ctrl Pts',(183.854546123069,-3.23913759166378,338.703035774492));
#47074=CARTESIAN_POINT('Ctrl Pts',(183.847516382099,-3.14506353565459,338.783248907216));
#47075=CARTESIAN_POINT('Ctrl Pts',(183.84048664113,-3.04826641418166,338.85969622259));
#47076=CARTESIAN_POINT('Ctrl Pts',(183.8327206507,-2.94133139023732,338.944150133776));
#47077=CARTESIAN_POINT('Ctrl Pts',(183.824954660271,-2.83071108871737,339.024293139672));
#47078=CARTESIAN_POINT('Ctrl Pts',(183.817188669842,-2.7167885402977,339.099785737061));
#47079=CARTESIAN_POINT('Ctrl Pts',(183.809432358556,-2.60300797927253,339.175184244233));
#47080=CARTESIAN_POINT('Ctrl Pts',(183.801676047271,-2.48593368351757,339.245943660324));
#47081=CARTESIAN_POINT('Ctrl Pts',(183.793919735985,-2.36598197792825,339.311764411771));
#47082=CARTESIAN_POINT('Ctrl Pts',(183.786171225367,-2.24615091000722,339.377518966061));
#47083=CARTESIAN_POINT('Ctrl Pts',(183.778422714749,-2.12344853218142,339.438344552282));
#47084=CARTESIAN_POINT('Ctrl Pts',(183.77067420413,-1.99832008759991,339.493984856449));
#47085=CARTESIAN_POINT('Ctrl Pts',(183.762931622553,-1.87328738938408,339.54958258551));
#47086=CARTESIAN_POINT('Ctrl Pts',(183.755189040976,-1.74583267588013,339.600002771));
#47087=CARTESIAN_POINT('Ctrl Pts',(183.747446459399,-1.61642539875726,339.645035198225));
#47088=CARTESIAN_POINT('Ctrl Pts',(183.73970726661,-1.48707476085487,339.690047915574));
#47089=CARTESIAN_POINT('Ctrl Pts',(183.731968073821,-1.35577362843123,339.729677436273));
#47090=CARTESIAN_POINT('Ctrl Pts',(183.724228881032,-1.22301080180226,339.763761921127));
#47091=CARTESIAN_POINT('Ctrl Pts',(183.716491363673,-1.09027671652678,339.79783902715));
#47092=CARTESIAN_POINT('Ctrl Pts',(183.708753846314,-0.956081945791869,
339.826373387539));
#47093=CARTESIAN_POINT('Ctrl Pts',(183.701016328955,-0.82092940889344,339.8492533413));
#47094=CARTESIAN_POINT('Ctrl Pts',(183.693278801142,-0.685776689396465,
339.872133325974));
#47095=CARTESIAN_POINT('Ctrl Pts',(183.685541273329,-0.549666587551065,
339.889358823176));
#47096=CARTESIAN_POINT('Ctrl Pts',(183.677803745517,-0.413110740497895,
339.900869573717));
#47097=CARTESIAN_POINT('Ctrl Pts',(183.670064521709,-0.276524961665025,
339.912382847308));
#47098=CARTESIAN_POINT('Ctrl Pts',(183.662325297902,-0.139493633689289,
339.918178848906));
#47099=CARTESIAN_POINT('Ctrl Pts',(183.654586074095,-0.00253160902896628,
339.918249348443));
#47100=CARTESIAN_POINT('Ctrl Pts',(183.646838643908,0.134575644959302,339.918319922734));
#47101=CARTESIAN_POINT('Ctrl Pts',(183.639091213722,0.271613056281813,339.91265286719));
#47102=CARTESIAN_POINT('Ctrl Pts',(183.631343783536,0.408067137857272,339.901292102446));
#47103=CARTESIAN_POINT('Ctrl Pts',(183.623592233658,0.544593778820921,339.889925296621));
#47104=CARTESIAN_POINT('Ctrl Pts',(183.615840683779,0.680536083323476,339.872858797906));
#47105=CARTESIAN_POINT('Ctrl Pts',(183.608089133901,0.815388600765422,339.850188088337));
#47106=CARTESIAN_POINT('Ctrl Pts',(183.600325114227,0.950458053320495,339.827480908755));
#47107=CARTESIAN_POINT('Ctrl Pts',(183.592561094553,1.08443383191718,339.799151584073));
#47108=CARTESIAN_POINT('Ctrl Pts',(183.584797074879,1.21682267218757,339.765346330221));
#47109=CARTESIAN_POINT('Ctrl Pts',(183.577280918871,1.34498504412012,339.732620297509));
#47110=CARTESIAN_POINT('Ctrl Pts',(183.569764762863,1.47165996656069,339.694762775491));
#47111=CARTESIAN_POINT('Ctrl Pts',(183.562248606856,1.5964178399923,339.65194939167));
#47112=CARTESIAN_POINT('Ctrl Pts',(183.554470990015,1.72551560439166,339.607646679658));
#47113=CARTESIAN_POINT('Ctrl Pts',(183.546693373173,1.8529707700418,339.557896287814));
#47114=CARTESIAN_POINT('Ctrl Pts',(183.538915756332,1.97828959446425,339.50283836518));
#47115=CARTESIAN_POINT('Ctrl Pts',(183.531147691353,2.10345451208518,339.44784806039));
#47116=CARTESIAN_POINT('Ctrl Pts',(183.523379626374,2.22648795474663,339.387563350159));
#47117=CARTESIAN_POINT('Ctrl Pts',(183.515611561395,2.34691190214015,339.322173942138));
#47118=CARTESIAN_POINT('Ctrl Pts',(183.507851182931,2.46721668979935,339.256849237065));
#47119=CARTESIAN_POINT('Ctrl Pts',(183.500090804468,2.58491677974573,339.186430071531));
#47120=CARTESIAN_POINT('Ctrl Pts',(183.492330426004,2.69955501941842,339.111153823397));
#47121=CARTESIAN_POINT('Ctrl Pts',(183.484575875352,2.81410716921139,339.035934105468));
#47122=CARTESIAN_POINT('Ctrl Pts',(183.4768213247,2.92560172037708,338.955864778789));
#47123=CARTESIAN_POINT('Ctrl Pts',(183.469066774049,3.03360730182606,338.871228461459));
#47124=CARTESIAN_POINT('Ctrl Pts',(183.461315500151,3.14156724454938,338.786627907962));
#47125=CARTESIAN_POINT('Ctrl Pts',(183.453564226254,3.24604084307936,338.697464442576));
#47126=CARTESIAN_POINT('Ctrl Pts',(183.445812952357,3.3466270258048,338.604063070016));
#47127=CARTESIAN_POINT('Ctrl Pts',(183.438063287257,3.44719233160352,338.510681083157));
#47128=CARTESIAN_POINT('Ctrl Pts',(183.430313622157,3.5438715404598,338.413063204326));
#47129=CARTESIAN_POINT('Ctrl Pts',(183.422563957057,3.63629821021753,338.311573400797));
#47130=CARTESIAN_POINT('Ctrl Pts',(183.414814226142,3.72872566493115,338.210082735342));
#47131=CARTESIAN_POINT('Ctrl Pts',(183.407064495226,3.81690024553004,338.104720368382));
#47132=CARTESIAN_POINT('Ctrl Pts',(183.39931476431,3.90049407107727,337.995885355615));
#47133=CARTESIAN_POINT('Ctrl Pts',(183.39156329328,3.98410666667491,337.887025905175));
#47134=CARTESIAN_POINT('Ctrl Pts',(183.383811822249,4.06313622261014,337.774692567));
#47135=CARTESIAN_POINT('Ctrl Pts',(183.376060351219,4.13729690671077,337.659315206632));
#47136=CARTESIAN_POINT('Ctrl Pts',(183.368300672718,4.21153611418,337.543815681546));
#47137=CARTESIAN_POINT('Ctrl Pts',(183.360540994217,4.28089594008427,337.425266024898));
#47138=CARTESIAN_POINT('Ctrl Pts',(183.352781315717,4.34513517033009,337.304123133442));
#47139=CARTESIAN_POINT('Ctrl Pts',(183.345017497428,4.40940867220259,337.182915612258));
#47140=CARTESIAN_POINT('Ctrl Pts',(183.337253679139,4.46855596658702,337.059112451734));
#47141=CARTESIAN_POINT('Ctrl Pts',(183.32948986085,4.52238355654552,336.933191669232));
#47142=CARTESIAN_POINT('Ctrl Pts',(183.321713662257,4.57629698080395,336.80707009152));
#47143=CARTESIAN_POINT('Ctrl Pts',(183.313937463665,4.62487361085573,336.678824509432));
#47144=CARTESIAN_POINT('Ctrl Pts',(183.306161265072,4.66796921373637,336.548950122538));
#47145=CARTESIAN_POINT('Ctrl Pts',(183.298777700908,4.7088888411416,336.425633329966));
#47146=CARTESIAN_POINT('Ctrl Pts',(183.291394136745,4.74486729916818,336.300848455172));
#47147=CARTESIAN_POINT('Ctrl Pts',(183.284010572581,4.77582394746742,336.175027099814));
#47148=CARTESIAN_POINT('Ctrl Pts',(183.276234394037,4.8084266876837,336.042515307105));
#47149=CARTESIAN_POINT('Ctrl Pts',(183.268458215494,4.83556150200425,335.90843692987));
#47150=CARTESIAN_POINT('Ctrl Pts',(183.26068203695,4.85707903122376,335.773282837613));
#47151=CARTESIAN_POINT('Ctrl Pts',(183.252915403468,4.87857014822109,335.638294643581));
#47152=CARTESIAN_POINT('Ctrl Pts',(183.245148769986,4.8944576385936,335.502233744006));
#47153=CARTESIAN_POINT('Ctrl Pts',(183.237382136505,4.90464232427141,335.365604613573));
#47154=CARTESIAN_POINT('Ctrl Pts',(183.229623181197,4.91481694126381,335.229110556108));
#47155=CARTESIAN_POINT('Ctrl Pts',(183.22186422589,4.91929994442945,335.092049772895));
#47156=CARTESIAN_POINT('Ctrl Pts',(183.214105270582,4.91804353454062,334.954934992919));
#47157=CARTESIAN_POINT('Ctrl Pts',(183.206352133207,4.91678806675131,334.81792302634));
#47158=CARTESIAN_POINT('Ctrl Pts',(183.198598995832,4.90980175566383,334.680857532755));
#47159=CARTESIAN_POINT('Ctrl Pts',(183.190845858457,4.89708879725493,334.544254046315));
#47160=CARTESIAN_POINT('Ctrl Pts',(183.183095977539,4.88438117851743,334.407707935799));
#47161=CARTESIAN_POINT('Ctrl Pts',(183.175346096622,4.86595173250282,334.271623834738));
#47162=CARTESIAN_POINT('Ctrl Pts',(183.167596215704,4.84185669610816,334.136514738486));
#47163=CARTESIAN_POINT('Ctrl Pts',(183.159847930984,4.81776662242882,334.001433469873));
#47164=CARTESIAN_POINT('Ctrl Pts',(183.152099646265,4.78801334800257,333.867327191067));
#47165=CARTESIAN_POINT('Ctrl Pts',(183.144351361545,4.7527046142189,333.734700860475));
#47166=CARTESIAN_POINT('Ctrl Pts',(183.136602997014,4.71739551673801,333.602073163767));
#47167=CARTESIAN_POINT('Ctrl Pts',(183.128854632484,4.67653094633414,333.470925823261));
#47168=CARTESIAN_POINT('Ctrl Pts',(183.121106267953,4.63026901798813,333.341750355477));
#47169=CARTESIAN_POINT('Ctrl Pts',(183.113356147906,4.58399660826075,333.212545620921));
#47170=CARTESIAN_POINT('Ctrl Pts',(183.105606027859,4.5323245389347,333.085314015891));
#47171=CARTESIAN_POINT('Ctrl Pts',(183.097855907812,4.47545958671199,332.960528364942));
#47172=CARTESIAN_POINT('Ctrl Pts',(183.090097548043,4.41853417717562,332.835610045188));
#47173=CARTESIAN_POINT('Ctrl Pts',(183.082339188273,4.35640501844851,332.713143230329));
#47174=CARTESIAN_POINT('Ctrl Pts',(183.074580828504,4.28932576175322,332.593577848327));
#47175=CARTESIAN_POINT('Ctrl Pts',(183.066818313455,4.22221057826133,332.473948428628));
#47176=CARTESIAN_POINT('Ctrl Pts',(183.059055798407,4.15014021918361,332.357223870529));
#47177=CARTESIAN_POINT('Ctrl Pts',(183.051293283358,4.07341191337439,332.243825396228));
#47178=CARTESIAN_POINT('Ctrl Pts',(183.043518348122,3.99656084065466,332.130245481971));
#47179=CARTESIAN_POINT('Ctrl Pts',(183.035743412885,3.91503716072815,332.020002600387));
#47180=CARTESIAN_POINT('Ctrl Pts',(183.027968477649,3.82917920583801,331.913485838024));
#47181=CARTESIAN_POINT('Ctrl Pts',(183.020569831202,3.74747657635232,331.812124239317));
#47182=CARTESIAN_POINT('Ctrl Pts',(183.013171184755,3.66184956223402,331.714136757172));
#47183=CARTESIAN_POINT('Ctrl Pts',(183.005772538308,3.57261956977787,331.619826561826));
#47184=CARTESIAN_POINT('Ctrl Pts',(182.997998800428,3.47886585721643,331.52073509378));
#47185=CARTESIAN_POINT('Ctrl Pts',(182.990225062549,3.38083770587482,331.425390039951));
#47186=CARTESIAN_POINT('Ctrl Pts',(182.982451324669,3.27886659433371,331.334182639702));
#47187=CARTESIAN_POINT('Ctrl Pts',(182.974687171874,3.17702121403236,331.243087698946));
#47188=CARTESIAN_POINT('Ctrl Pts',(182.966923019079,3.07124283549676,331.156120519001));
#47189=CARTESIAN_POINT('Ctrl Pts',(182.959158866284,2.96190156216339,331.07363753602));
#47190=CARTESIAN_POINT('Ctrl Pts',(182.951402428827,2.85266894266215,330.991236517441));
#47191=CARTESIAN_POINT('Ctrl Pts',(182.94364599137,2.73988078423507,330.913311062166));
#47192=CARTESIAN_POINT('Ctrl Pts',(182.935889553914,2.62394196427249,330.840178894396));
#47193=CARTESIAN_POINT('Ctrl Pts',(182.928138968751,2.50809062107366,330.767101905429));
#47194=CARTESIAN_POINT('Ctrl Pts',(182.920388383589,2.38909367739034,330.698811213191));
#47195=CARTESIAN_POINT('Ctrl Pts',(182.912637798426,2.26738653550387,330.635582357162));
#47196=CARTESIAN_POINT('Ctrl Pts',(182.904890513095,2.145731210755,330.572380420986));
#47197=CARTESIAN_POINT('Ctrl Pts',(182.897143227765,2.02136832905076,330.514236214586));
#47198=CARTESIAN_POINT('Ctrl Pts',(182.889395942434,1.89475934510586,330.461380156189));
#47199=CARTESIAN_POINT('Ctrl Pts',(182.881650279359,1.76817687265904,330.408535165675));
#47200=CARTESIAN_POINT('Ctrl Pts',(182.873904616285,1.63934959409558,330.360976271191));
#47201=CARTESIAN_POINT('Ctrl Pts',(182.86615895321,1.50876010339829,330.318886242261));
#47202=CARTESIAN_POINT('Ctrl Pts',(182.858413233964,1.37816966568314,330.2767959081));
#47203=CARTESIAN_POINT('Ctrl Pts',(182.850667514719,1.24581736251209,330.24017463858));
#47204=CARTESIAN_POINT('Ctrl Pts',(182.842921795473,1.11220176748111,330.209155576424));
#47205=CARTESIAN_POINT('Ctrl Pts',(182.83517434195,0.978556255715918,330.178129569052));
#47206=CARTESIAN_POINT('Ctrl Pts',(182.827426888426,0.843647270077547,330.152708353432));
#47207=CARTESIAN_POINT('Ctrl Pts',(182.819679434902,0.707984019387355,330.132974040465));
#47208=CARTESIAN_POINT('Ctrl Pts',(182.811923760379,0.572176813319829,330.113218786966));
#47209=CARTESIAN_POINT('Ctrl Pts',(182.804168085855,0.435614130961163,330.099162546979));
#47210=CARTESIAN_POINT('Ctrl Pts',(182.796412411331,0.298811309764709,330.090835624706));
#47211=CARTESIAN_POINT('Ctrl Pts',(182.788652595967,0.161935448033445,330.082504256597));
#47212=CARTESIAN_POINT('Ctrl Pts',(182.780892780603,0.0248195827529,330.079908308776));
#47213=CARTESIAN_POINT('Ctrl Pts',(182.773132965239,-0.112021492345339,
330.08302590532));
#47214=CARTESIAN_POINT('Ctrl Pts',(182.765360727264,-0.249081634955755,
330.086148492794));
#47215=CARTESIAN_POINT('Ctrl Pts',(182.75758848929,-0.385865717896615,330.095002877277));
#47216=CARTESIAN_POINT('Ctrl Pts',(182.749816251315,-0.521863715696806,
330.109515225999));
#47217=CARTESIAN_POINT('Ctrl Pts',(182.742389002221,-0.651825125676095,
330.123383410329));
#47218=CARTESIAN_POINT('Ctrl Pts',(182.734961753127,-0.781068451306207,
330.142417990637));
#47219=CARTESIAN_POINT('Ctrl Pts',(182.727534504033,-0.909159619807499,
330.166511420494));
#47220=CARTESIAN_POINT('Ctrl Pts',(182.719758964722,-1.04325744035854,330.191734677267));
#47221=CARTESIAN_POINT('Ctrl Pts',(182.71198342541,-1.17651648894425,330.222582492355));
#47222=CARTESIAN_POINT('Ctrl Pts',(182.704207886098,-1.30842819381469,330.258987584478));
#47223=CARTESIAN_POINT('Ctrl Pts',(182.696441910889,-1.44017764408495,330.295347897455));
#47224=CARTESIAN_POINT('Ctrl Pts',(182.688675935679,-1.5705826749916,330.337251783594));
#47225=CARTESIAN_POINT('Ctrl Pts',(182.68090996047,-1.69914310592826,330.384580650897));
#47226=CARTESIAN_POINT('Ctrl Pts',(182.67315168168,-1.82757612788094,330.431862613232));
#47227=CARTESIAN_POINT('Ctrl Pts',(182.665393402889,-1.95416782345623,330.484558723225));
#47228=CARTESIAN_POINT('Ctrl Pts',(182.657635124099,-2.07843177080675,330.54250020341));
#47229=CARTESIAN_POINT('Ctrl Pts',(182.649882680715,-2.20260225277733,330.600398102793));
#47230=CARTESIAN_POINT('Ctrl Pts',(182.64213023733,-2.32444811867142,330.663533354894));
#47231=CARTESIAN_POINT('Ctrl Pts',(182.634377793945,-2.4435019217258,330.731688692115));
#47232=CARTESIAN_POINT('Ctrl Pts',(182.62662863126,-2.56250534327389,330.799815187178));
#47233=CARTESIAN_POINT('Ctrl Pts',(182.618879468574,-2.6787187135427,330.872957348278));
#47234=CARTESIAN_POINT('Ctrl Pts',(182.611130305889,-2.79169844638803,330.95085158991));
#47235=CARTESIAN_POINT('Ctrl Pts',(182.603382754074,-2.90465469338577,331.028729639148));
#47236=CARTESIAN_POINT('Ctrl Pts',(182.595635202259,-3.01437831845557,331.111357582315));
#47237=CARTESIAN_POINT('Ctrl Pts',(182.587887650443,-3.12045437792336,331.198428280593));
#47238=CARTESIAN_POINT('Ctrl Pts',(182.580140032842,-3.22653133810722,331.285499718207));
#47239=CARTESIAN_POINT('Ctrl Pts',(182.572392415241,-3.32896036882893,331.37701373821));
#47240=CARTESIAN_POINT('Ctrl Pts',(182.564644797639,-3.42735962124693,331.472622916508));
#47241=CARTESIAN_POINT('Ctrl Pts',(182.556895437908,-3.52578099972094,331.568253593485));
#47242=CARTESIAN_POINT('Ctrl Pts',(182.549146078177,-3.62017051653461,331.667980988829));
#47243=CARTESIAN_POINT('Ctrl Pts',(182.541396718447,-3.71018348837263,331.771421126082));
#47244=CARTESIAN_POINT('Ctrl Pts',(182.533639136018,-3.80029197125682,331.874971021691));
#47245=CARTESIAN_POINT('Ctrl Pts',(182.52588155359,-3.88601437564062,331.982241233484));
#47246=CARTESIAN_POINT('Ctrl Pts',(182.518123971161,-3.96704627203496,332.092814602053));
#47247=CARTESIAN_POINT('Ctrl Pts',(182.51036224395,-4.04812146279008,332.203447048635));
#47248=CARTESIAN_POINT('Ctrl Pts',(182.50260051674,-4.12450093443874,332.317385844135));
#47249=CARTESIAN_POINT('Ctrl Pts',(182.494838789529,-4.19592443337213,332.434186052745));
#47250=CARTESIAN_POINT('Ctrl Pts',(182.487064652255,-4.26746212983944,332.551173010757));
#47251=CARTESIAN_POINT('Ctrl Pts',(182.479290514981,-4.33402782923239,332.671030182347));
#47252=CARTESIAN_POINT('Ctrl Pts',(182.471516377708,-4.39540755167253,332.793288528783));
#47253=CARTESIAN_POINT('Ctrl Pts',(182.464109741725,-4.45388571392279,332.909767442912));
#47254=CARTESIAN_POINT('Ctrl Pts',(182.456703105742,-4.50765687201246,333.028425445668));
#47255=CARTESIAN_POINT('Ctrl Pts',(182.449296469759,-4.55657774852652,333.148842987715));
#47256=CARTESIAN_POINT('Ctrl Pts',(182.440339878659,-4.61573608818309,333.294459795111));
#47257=CARTESIAN_POINT('Ctrl Pts',(182.431383287559,-4.6679636105574,333.44304691552));
#47258=CARTESIAN_POINT('Ctrl Pts',(182.42242669646,-4.7129878843127,333.59396718928));
#47259=CARTESIAN_POINT('Ctrl Pts',(182.413727250667,-4.75671950324406,333.740554515417));
#47260=CARTESIAN_POINT('Ctrl Pts',(182.405027804873,-4.79365563198517,333.889342650309));
#47261=CARTESIAN_POINT('Ctrl Pts',(182.39632835908,-4.82359349480214,334.0397245919));
#47262=CARTESIAN_POINT('Ctrl Pts',(182.387243195327,-4.8548587492319,334.196774201427));
#47263=CARTESIAN_POINT('Ctrl Pts',(182.378158031574,-4.87849083595186,334.355562030965));
#47264=CARTESIAN_POINT('Ctrl Pts',(182.36907286782,-4.89431507868469,334.515373367364));
#47265=CARTESIAN_POINT('Ctrl Pts',(182.360444744031,-4.90934326407371,334.667145204489));
#47266=CARTESIAN_POINT('Ctrl Pts',(182.351816620241,-4.91732970925359,334.819839802589));
#47267=CARTESIAN_POINT('Ctrl Pts',(182.343188496452,-4.91817494046866,334.972828002537));
#47268=CARTESIAN_POINT('Ctrl Pts',(182.342731456488,-4.91821971317398,334.980931933712));
#47269=CARTESIAN_POINT('Ctrl Pts',(182.342274416524,-4.91824445986726,334.989036685278));
#47270=CARTESIAN_POINT('Ctrl Pts',(182.34181737656,-4.91824916970108,334.997142162596));
#47271=CARTESIAN_POINT('',(180.591817376458,-4.9182484086652,335.003956407744));
#47272=CARTESIAN_POINT('Ctrl Pts',(182.341817376508,-4.91824916970162,334.997142163525));
#47273=CARTESIAN_POINT('Ctrl Pts',(182.33399174791,-4.91832981341144,335.135927521746));
#47274=CARTESIAN_POINT('Ctrl Pts',(182.326166119313,-4.91253165524224,335.274724294722));
#47275=CARTESIAN_POINT('Ctrl Pts',(182.318340490715,-4.9008783981803,335.413006039604));
#47276=CARTESIAN_POINT('Ctrl Pts',(182.310513578694,-4.88922322995347,335.551310463057));
#47277=CARTESIAN_POINT('Ctrl Pts',(182.302686666673,-4.87171108188477,335.689099311701));
#47278=CARTESIAN_POINT('Ctrl Pts',(182.294859754651,-4.84841756392563,335.825851190177));
#47279=CARTESIAN_POINT('Ctrl Pts',(182.287029996697,-4.82511557624064,335.962652792827));
#47280=CARTESIAN_POINT('Ctrl Pts',(182.279200238742,-4.79602809592471,336.098416300174));
#47281=CARTESIAN_POINT('Ctrl Pts',(182.271370480788,-4.76128183031932,336.232630680606));
#47282=CARTESIAN_POINT('Ctrl Pts',(182.263536312831,-4.72651599436453,336.366920655415));
#47283=CARTESIAN_POINT('Ctrl Pts',(182.255702144874,-4.68608512077128,336.499659398574));
#47284=CARTESIAN_POINT('Ctrl Pts',(182.247867976918,-4.64016564754835,336.630351442423));
#47285=CARTESIAN_POINT('Ctrl Pts',(182.240023128865,-4.59418357362901,336.761221654975));
#47286=CARTESIAN_POINT('Ctrl Pts',(182.232178280813,-4.54269808447251,336.890039238294));
#47287=CARTESIAN_POINT('Ctrl Pts',(182.224333432761,-4.48593385809718,337.016328466118));
#47288=CARTESIAN_POINT('Ctrl Pts',(182.216482296267,-4.42912412943677,337.142718927568));
#47289=CARTESIAN_POINT('Ctrl Pts',(182.208631159773,-4.36702740073226,337.26657665641));
#47290=CARTESIAN_POINT('Ctrl Pts',(182.20078002328,-4.29991371734091,337.387451588184));
#47291=CARTESIAN_POINT('Ctrl Pts',(182.192916621086,-4.23269518335661,337.508515360857));
#47292=CARTESIAN_POINT('Ctrl Pts',(182.185053218892,-4.16044424171952,337.626586709176));
#47293=CARTESIAN_POINT('Ctrl Pts',(182.177189816698,-4.08347386544473,337.741245018733));
#47294=CARTESIAN_POINT('Ctrl Pts',(182.175146022961,-4.06346832978651,337.771046106001));
#47295=CARTESIAN_POINT('Ctrl Pts',(182.173102229223,-4.04314418357207,337.800616806267));
#47296=CARTESIAN_POINT('Ctrl Pts',(182.171058435486,-4.02250734998357,337.829950120025));
#47297=CARTESIAN_POINT('Ctrl Pts',(182.16328355021,-3.94400186741796,337.941538263717));
#47298=CARTESIAN_POINT('Ctrl Pts',(182.155508664934,-3.86072540937495,338.050033628111));
#47299=CARTESIAN_POINT('Ctrl Pts',(182.147733779658,-3.77294980454117,338.155001241666));
#47300=CARTESIAN_POINT('Ctrl Pts',(182.139968464733,-3.68528224545914,338.259839647285));
#47301=CARTESIAN_POINT('Ctrl Pts',(182.132203149808,-3.59312680724248,338.361158645223));
#47302=CARTESIAN_POINT('Ctrl Pts',(182.124437834883,-3.49679854697354,338.458552151462));
#47303=CARTESIAN_POINT('Ctrl Pts',(182.116680221882,-3.4005658286088,338.555849059247));
#47304=CARTESIAN_POINT('Ctrl Pts',(182.108922608881,-3.3001687976538,338.649227947372));
#47305=CARTESIAN_POINT('Ctrl Pts',(182.10116499588,-3.19596249181755,338.738316039796));
#47306=CARTESIAN_POINT('Ctrl Pts',(182.093413223056,-3.09183463578897,338.827337063882));
#47307=CARTESIAN_POINT('Ctrl Pts',(182.085661450232,-2.98390350889375,338.91207346892));
#47308=CARTESIAN_POINT('Ctrl Pts',(182.077909677408,-2.87256042528724,338.992189833359));
#47309=CARTESIAN_POINT('Ctrl Pts',(182.070161190157,-2.76126453421413,339.072272240644));
#47310=CARTESIAN_POINT('Ctrl Pts',(182.062412702906,-2.64655987935621,339.147738274209));
#47311=CARTESIAN_POINT('Ctrl Pts',(182.054664215654,-2.52887004977796,339.218293414858));
#47312=CARTESIAN_POINT('Ctrl Pts',(182.046917342142,-2.41120473087652,339.288833861338));
#47313=CARTESIAN_POINT('Ctrl Pts',(182.03917046863,-2.29055580892797,339.354465248391));
#47314=CARTESIAN_POINT('Ctrl Pts',(182.031423595117,-2.16737465034927,339.414937166883));
#47315=CARTESIAN_POINT('Ctrl Pts',(182.023676658045,-2.0441924811235,339.475409581521));
#47316=CARTESIAN_POINT('Ctrl Pts',(182.015929720973,-1.91847838472056,339.530722270901));
#47317=CARTESIAN_POINT('Ctrl Pts',(182.008182783901,-1.79070668527723,339.58067163523));
#47318=CARTESIAN_POINT('Ctrl Pts',(182.000434106285,-1.66290627871049,339.63063222194));
#47319=CARTESIAN_POINT('Ctrl Pts',(181.992685428669,-1.53304771319022,339.67522694348));
#47320=CARTESIAN_POINT('Ctrl Pts',(181.984936751053,-1.40162318581535,339.714301168517));
#47321=CARTESIAN_POINT('Ctrl Pts',(181.977179849391,-1.27005917124119,339.753416864917));
#47322=CARTESIAN_POINT('Ctrl Pts',(181.969422947729,-1.136926250029,339.787000248999));
#47323=CARTESIAN_POINT('Ctrl Pts',(181.961666046067,-1.0027301456108,339.814947073186));
#47324=CARTESIAN_POINT('Ctrl Pts',(181.953904999964,-0.868462341452754,
339.842908829103));
#47325=CARTESIAN_POINT('Ctrl Pts',(181.946143953861,-0.73313060769247,339.865227960748));
#47326=CARTESIAN_POINT('Ctrl Pts',(181.938382907758,-0.597247647113583,
339.881851934514));
#47327=CARTESIAN_POINT('Ctrl Pts',(181.930609445289,-0.461147296686841,
339.898502503838));
#47328=CARTESIAN_POINT('Ctrl Pts',(181.92283598282,-0.324494347060001,339.909439677019));
#47329=CARTESIAN_POINT('Ctrl Pts',(181.91506252035,-0.187804267934973,339.914663021962));
#47330=CARTESIAN_POINT('Ctrl Pts',(181.907648480638,-0.0574343486144119,
339.919644854318));
#47331=CARTESIAN_POINT('Ctrl Pts',(181.900234440925,0.0729690550090576,
339.919429431031));
#47332=CARTESIAN_POINT('Ctrl Pts',(181.892820401212,0.202963363140059,339.9140603309));
#47333=CARTESIAN_POINT('Ctrl Pts',(181.885045243003,0.339289354247273,339.908429715935));
#47334=CARTESIAN_POINT('Ctrl Pts',(181.877270084795,0.475596244312727,339.897112967862));
#47335=CARTESIAN_POINT('Ctrl Pts',(181.869494926586,0.611371120462187,339.880103320173));
#47336=CARTESIAN_POINT('Ctrl Pts',(181.861729335389,0.746978931217701,339.863114602155));
#47337=CARTESIAN_POINT('Ctrl Pts',(181.853963744193,0.882055646439472,339.84044697035));
#47338=CARTESIAN_POINT('Ctrl Pts',(181.846198152996,1.01608925616967,339.812145642642));
#47339=CARTESIAN_POINT('Ctrl Pts',(181.838440260699,1.1499899833858,339.783872373206));
#47340=CARTESIAN_POINT('Ctrl Pts',(181.830682368401,1.2828492831529,339.749976603193));
#47341=CARTESIAN_POINT('Ctrl Pts',(181.822924476104,1.41416152279385,339.71055519551));
#47342=CARTESIAN_POINT('Ctrl Pts',(181.815172421267,1.54537495595415,339.671163450642));
#47343=CARTESIAN_POINT('Ctrl Pts',(181.807420366431,1.67504327320611,339.626254455923));
#47344=CARTESIAN_POINT('Ctrl Pts',(181.799668311594,1.80267262601678,339.575975793851));
#47345=CARTESIAN_POINT('Ctrl Pts',(181.791919539193,1.93024793700624,339.525718421164));
#47346=CARTESIAN_POINT('Ctrl Pts',(181.784170766793,2.05578563779871,339.470096046254));
#47347=CARTESIAN_POINT('Ctrl Pts',(181.776421994392,2.17880881230689,339.409305526034));
#47348=CARTESIAN_POINT('Ctrl Pts',(181.768674833861,2.30180639601633,339.34852765122));
#47349=CARTESIAN_POINT('Ctrl Pts',(181.760927673329,2.42229014365104,339.282583942509));
#47350=CARTESIAN_POINT('Ctrl Pts',(181.753180512798,2.53980520256777,339.211718484836));
#47351=CARTESIAN_POINT('Ctrl Pts',(181.745433287105,2.65732124989162,339.140852431121));
#47352=CARTESIAN_POINT('Ctrl Pts',(181.737686061413,2.7718682239794,339.065064747722));
#47353=CARTESIAN_POINT('Ctrl Pts',(181.729938835721,2.8830182131899,338.984644155369));
#47354=CARTESIAN_POINT('Ctrl Pts',(181.722189868152,2.99419319323221,338.904205481345));
#47355=CARTESIAN_POINT('Ctrl Pts',(181.714440900583,3.10196935196417,338.819132054661));
#47356=CARTESIAN_POINT('Ctrl Pts',(181.706691933014,3.20595028557887,338.729754124456));
#47357=CARTESIAN_POINT('Ctrl Pts',(181.698934740921,3.31004158147358,338.640281331166));
#47358=CARTESIAN_POINT('Ctrl Pts',(181.691177548827,3.41032930878365,338.546495163191));
#47359=CARTESIAN_POINT('Ctrl Pts',(181.683420356734,3.50645211354861,338.448764508906));
#47360=CARTESIAN_POINT('Ctrl Pts',(181.675659019479,3.60262628283465,338.350981630924));
#47361=CARTESIAN_POINT('Ctrl Pts',(181.667897682225,3.69463083285505,338.249250356418));
#47362=CARTESIAN_POINT('Ctrl Pts',(181.660136344971,3.78214412059007,338.143973427621));
#47363=CARTESIAN_POINT('Ctrl Pts',(181.652362593056,3.86979739036253,338.038528102922));
#47364=CARTESIAN_POINT('Ctrl Pts',(181.644588841141,3.95294480489276,337.929526101614));
#47365=CARTESIAN_POINT('Ctrl Pts',(181.636815089226,4.03130703749056,337.817400687155));
#47366=CARTESIAN_POINT('Ctrl Pts',(181.629404181797,4.10601166636027,337.710508792981));
#47367=CARTESIAN_POINT('Ctrl Pts',(181.621993274367,4.17636757725118,337.600778720445));
#47368=CARTESIAN_POINT('Ctrl Pts',(181.614582366938,4.24217217030331,337.488605701995));
#47369=CARTESIAN_POINT('Ctrl Pts',(181.606807279412,4.31121047303492,337.370920378725));
#47370=CARTESIAN_POINT('Ctrl Pts',(181.599032191885,4.37545695737443,337.250174054834));
#47371=CARTESIAN_POINT('Ctrl Pts',(181.591257104359,4.43462836544519,337.1267943772));
#47372=CARTESIAN_POINT('Ctrl Pts',(181.583491584237,4.49372696188098,337.003566520797));
#47373=CARTESIAN_POINT('Ctrl Pts',(181.575726064116,4.54776274037067,336.877712107178));
#47374=CARTESIAN_POINT('Ctrl Pts',(181.567960543995,4.59649664601165,336.749686156345));
#47375=CARTESIAN_POINT('Ctrl Pts',(181.560202723087,4.64518223386508,336.621787138303));
#47376=CARTESIAN_POINT('Ctrl Pts',(181.552444902179,4.68857627164759,336.491721230579));
#47377=CARTESIAN_POINT('Ctrl Pts',(181.544687081272,4.72648658466573,336.359966039089));
#47378=CARTESIAN_POINT('Ctrl Pts',(181.536935098061,4.76436837048295,336.228309992304));
#47379=CARTESIAN_POINT('Ctrl Pts',(181.52918311485,4.79677453740265,336.094967566079));
#47380=CARTESIAN_POINT('Ctrl Pts',(181.521431131639,4.82356193879182,335.960433904618));
#47381=CARTESIAN_POINT('Ctrl Pts',(181.513682430966,4.85033799719381,335.825957210742));
#47382=CARTESIAN_POINT('Ctrl Pts',(181.505933730292,4.87149994602879,335.690290667441));
#47383=CARTESIAN_POINT('Ctrl Pts',(181.498185029619,4.88695523757201,335.553941845745));
#47384=CARTESIAN_POINT('Ctrl Pts',(181.490437940866,4.90240731403442,335.417621387958));
#47385=CARTESIAN_POINT('Ctrl Pts',(181.482690852113,4.91215505048446,335.280619322229));
#47386=CARTESIAN_POINT('Ctrl Pts',(181.47494376336,4.91615755399456,335.143450224128));
#47387=CARTESIAN_POINT('Ctrl Pts',(181.467196609428,4.92016009117888,335.006279971982));
#47388=CARTESIAN_POINT('Ctrl Pts',(181.459449455496,4.91841728761306,334.868943075368));
#47389=CARTESIAN_POINT('Ctrl Pts',(181.451702301565,4.9109403648797,334.731955609842));
#47390=CARTESIAN_POINT('Ctrl Pts',(181.443953405669,4.90346176094433,334.594937342392));
#47391=CARTESIAN_POINT('Ctrl Pts',(181.436204509773,4.89024649351901,334.458269052591));
#47392=CARTESIAN_POINT('Ctrl Pts',(181.428455613878,4.87135775702261,334.32246279394));
#47393=CARTESIAN_POINT('Ctrl Pts',(181.420698492911,4.85244897106461,334.186512383647));
#47394=CARTESIAN_POINT('Ctrl Pts',(181.412941371945,4.82785474024287,334.051426220067));
#47395=CARTESIAN_POINT('Ctrl Pts',(181.405184250979,4.79768971904116,333.91770779255));
#47396=CARTESIAN_POINT('Ctrl Pts',(181.397422984667,4.76750857788533,333.783917906939));
#47397=CARTESIAN_POINT('Ctrl Pts',(181.389661718355,4.73175081628115,333.651497590957));
#47398=CARTESIAN_POINT('Ctrl Pts',(181.381900452044,4.69058104699797,333.520935260361));
#47399=CARTESIAN_POINT('Ctrl Pts',(181.374126770034,4.64934541843374,333.390164069202));
#47400=CARTESIAN_POINT('Ctrl Pts',(181.366353088024,4.60268061488252,333.261257170529));
#47401=CARTESIAN_POINT('Ctrl Pts',(181.358579406015,4.55079981485308,333.134683912139));
#47402=CARTESIAN_POINT('Ctrl Pts',(181.351167714898,4.50133490694478,333.014004690416));
#47403=CARTESIAN_POINT('Ctrl Pts',(181.343756023781,4.44712896206334,332.895446927018));
#47404=CARTESIAN_POINT('Ctrl Pts',(181.336344332664,4.3884047778019,332.779394999405));
#47405=CARTESIAN_POINT('Ctrl Pts',(181.328569281178,4.32680162287936,332.657653591403));
#47406=CARTESIAN_POINT('Ctrl Pts',(181.320794229692,4.26003132370039,332.538285192771));
#47407=CARTESIAN_POINT('Ctrl Pts',(181.313019178206,4.18830020322877,332.421759423534));
#47408=CARTESIAN_POINT('Ctrl Pts',(181.305253694836,4.11665735634828,332.30537705298));
#47409=CARTESIAN_POINT('Ctrl Pts',(181.297488211466,4.0400660380698,332.191830681109));
#47410=CARTESIAN_POINT('Ctrl Pts',(181.289722728097,3.95877951105733,332.081567570538));
#47411=CARTESIAN_POINT('Ctrl Pts',(181.281964944609,3.8775735838805,331.971413791599));
#47412=CARTESIAN_POINT('Ctrl Pts',(181.274207161122,3.79168194321293,331.864537107879));
#47413=CARTESIAN_POINT('Ctrl Pts',(181.266449377634,3.70140221459444,331.761357582521));
#47414=CARTESIAN_POINT('Ctrl Pts',(181.25869743247,3.61119042835433,331.658255707621));
#47415=CARTESIAN_POINT('Ctrl Pts',(181.250945487307,3.51659738372394,331.55884574585));
#47416=CARTESIAN_POINT('Ctrl Pts',(181.243193542143,3.41796198681423,331.463516023054));
#47417=CARTESIAN_POINT('Ctrl Pts',(181.235444880338,3.31936836721765,331.368226677444));
#47418=CARTESIAN_POINT('Ctrl Pts',(181.227696218533,3.21673608116487,331.277014404625));
#47419=CARTESIAN_POINT('Ctrl Pts',(181.219947556729,3.11044186705358,331.190231705972));
#47420=CARTESIAN_POINT('Ctrl Pts',(181.212200507339,3.00416977165798,331.103467065893));
#47421=CARTESIAN_POINT('Ctrl Pts',(181.20445345795,2.89423756648427,331.021130413605));
#47422=CARTESIAN_POINT('Ctrl Pts',(181.196706408561,2.78105583393632,330.943534603743));
#47423=CARTESIAN_POINT('Ctrl Pts',(181.188959294453,2.66787315586401,330.865938145643));
#47424=CARTESIAN_POINT('Ctrl Pts',(181.181212180345,2.5514412186582,330.79308282999));
#47425=CARTESIAN_POINT('Ctrl Pts',(181.173465066236,2.432200068598,330.725238499189));
#47426=CARTESIAN_POINT('Ctrl Pts',(181.165716210588,2.31293211329592,330.657378917079));
#47427=CARTESIAN_POINT('Ctrl Pts',(181.157967354939,2.19085402818108,330.594532754615));
#47428=CARTESIAN_POINT('Ctrl Pts',(181.150218499291,2.06643060311088,330.536923972749));
#47429=CARTESIAN_POINT('Ctrl Pts',(181.142461419019,1.94187511521186,330.479254045011));
#47430=CARTESIAN_POINT('Ctrl Pts',(181.134704338747,1.81496966992982,330.426832766878));
#47431=CARTESIAN_POINT('Ctrl Pts',(181.126947258475,1.68619970361795,330.379836190997));
#47432=CARTESIAN_POINT('Ctrl Pts',(181.119186033166,1.55736092838004,330.332814502243));
#47433=CARTESIAN_POINT('Ctrl Pts',(181.111424807856,1.42665601914718,330.291223410162));
#47434=CARTESIAN_POINT('Ctrl Pts',(181.103663582547,1.29458477212117,330.2551887993));
#47435=CARTESIAN_POINT('Ctrl Pts',(181.095889941655,1.16230225157505,330.219096544103));
#47436=CARTESIAN_POINT('Ctrl Pts',(181.088116300764,1.02864940678656,330.188578619371));
#47437=CARTESIAN_POINT('Ctrl Pts',(181.080342659872,0.894136281243819,330.163709750949));
#47438=CARTESIAN_POINT('Ctrl Pts',(181.072930539378,0.765878813670063,330.139997432376));
#47439=CARTESIAN_POINT('Ctrl Pts',(181.065518418884,0.636839567267541,330.121420597274));
#47440=CARTESIAN_POINT('Ctrl Pts',(181.05810629839,0.507462422473141,330.10799990267));
#47441=CARTESIAN_POINT('Ctrl Pts',(181.050331206421,0.371749680048379,330.09392199677));
#47442=CARTESIAN_POINT('Ctrl Pts',(181.042556114452,0.23523622890904,330.08547349236));
#47443=CARTESIAN_POINT('Ctrl Pts',(181.034781022483,0.0984286415098769,
330.082735021882));
#47444=CARTESIAN_POINT('Ctrl Pts',(181.027015498113,-0.0382105980329883,
330.079999921214));
#47445=CARTESIAN_POINT('Ctrl Pts',(181.019249973743,-0.175142866604414,
330.0829608816));
#47446=CARTESIAN_POINT('Ctrl Pts',(181.011484449372,-0.311854991428378,
330.091646963917));
#47447=CARTESIAN_POINT('Ctrl Pts',(181.003726624413,-0.448431568055069,
330.100324434103));
#47448=CARTESIAN_POINT('Ctrl Pts',(180.995968799453,-0.584788047729505,
330.114715705278));
#47449=CARTESIAN_POINT('Ctrl Pts',(180.988210974494,-0.720410123561506,
330.134797813413));
#47450=CARTESIAN_POINT('Ctrl Pts',(180.980458987433,-0.855930141424833,
330.154864809412));
#47451=CARTESIAN_POINT('Ctrl Pts',(180.972707000371,-0.990716470371876,
330.180614061333));
#47452=CARTESIAN_POINT('Ctrl Pts',(180.96495501331,-1.1242591532953,330.211970716596));
#47453=CARTESIAN_POINT('Ctrl Pts',(180.957206309108,-1.25774528273297,330.243314092749));
#47454=CARTESIAN_POINT('Ctrl Pts',(180.949457604907,-1.3899884339188,330.280260060053));
#47455=CARTESIAN_POINT('Ctrl Pts',(180.941708900705,-1.52048830249585,330.322682565351));
#47456=CARTESIAN_POINT('Ctrl Pts',(180.933961808621,-1.65096102058404,330.365096244649));
#47457=CARTESIAN_POINT('Ctrl Pts',(180.926214716537,-1.77969080598771,330.412984074842));
#47458=CARTESIAN_POINT('Ctrl Pts',(180.918467624452,-1.90619237957513,330.466170087603));
#47459=CARTESIAN_POINT('Ctrl Pts',(180.910720467391,-2.03269501417282,330.519356546452));
#47460=CARTESIAN_POINT('Ctrl Pts',(180.902973310329,-2.15696903935685,330.577841125011));
#47461=CARTESIAN_POINT('Ctrl Pts',(180.895226153267,-2.2785494015976,330.641399801888));
#47462=CARTESIAN_POINT('Ctrl Pts',(180.887477254447,-2.40015709820899,330.70497276838));
#47463=CARTESIAN_POINT('Ctrl Pts',(180.879728355626,-2.51906958046477,330.773621922178));
#47464=CARTESIAN_POINT('Ctrl Pts',(180.871979456806,-2.6348469875833,330.847077605526));
#47465=CARTESIAN_POINT('Ctrl Pts',(180.864222333259,-2.75074728151859,330.920611255166));
#47466=CARTESIAN_POINT('Ctrl Pts',(180.856465209712,-2.86350552257877,330.998961415703));
#47467=CARTESIAN_POINT('Ctrl Pts',(180.848708086165,-2.97271096425876,331.081815141488));
#47468=CARTESIAN_POINT('Ctrl Pts',(180.840946817456,-3.08197476188359,331.16471314169));
#47469=CARTESIAN_POINT('Ctrl Pts',(180.833185548747,-3.18768167610874,331.25211925348));
#47470=CARTESIAN_POINT('Ctrl Pts',(180.825424280037,-3.28945537701512,331.343681306953));
#47471=CARTESIAN_POINT('Ctrl Pts',(180.817650595971,-3.39139188080084,331.435389828185));
#47472=CARTESIAN_POINT('Ctrl Pts',(180.809876911904,-3.48938231888239,331.53126730242));
#47473=CARTESIAN_POINT('Ctrl Pts',(180.802103227837,-3.58308783646672,331.63092525778));
#47474=CARTESIAN_POINT('Ctrl Pts',(180.794691573263,-3.67242937929438,331.725942026445));
#47475=CARTESIAN_POINT('Ctrl Pts',(180.78727991869,-3.75787593256742,331.824394865921));
#47476=CARTESIAN_POINT('Ctrl Pts',(180.779868264116,-3.83916996566935,331.92592175812));
#47477=CARTESIAN_POINT('Ctrl Pts',(180.772032810466,-3.92511239891202,332.033253967166));
#47478=CARTESIAN_POINT('Ctrl Pts',(180.764197356815,-4.00669427622042,332.144372848535));
#47479=CARTESIAN_POINT('Ctrl Pts',(180.756361903165,-4.0835628426182,332.258887530055));
#47480=CARTESIAN_POINT('Ctrl Pts',(180.748614019154,-4.15957231994044,332.37212238659));
#47481=CARTESIAN_POINT('Ctrl Pts',(180.740866135143,-4.23097303984883,332.488677217721));
#47482=CARTESIAN_POINT('Ctrl Pts',(180.733118251132,-4.29746242262358,332.608138844197));
#47483=CARTESIAN_POINT('Ctrl Pts',(180.725377872357,-4.363887398328,332.727484750343));
#47484=CARTESIAN_POINT('Ctrl Pts',(180.717637493582,-4.42541031130816,332.849731510328));
#47485=CARTESIAN_POINT('Ctrl Pts',(180.709897114807,-4.48177151165708,332.974436577197));
#47486=CARTESIAN_POINT('Ctrl Pts',(180.702162542361,-4.53809043349586,333.099048098427));
#47487=CARTESIAN_POINT('Ctrl Pts',(180.694427969915,-4.58925518601485,333.226113901423));
#47488=CARTESIAN_POINT('Ctrl Pts',(180.68669339747,-4.6350519673576,333.355166779763));
#47489=CARTESIAN_POINT('Ctrl Pts',(180.678787062389,-4.68186576364981,333.487085551791));
#47490=CARTESIAN_POINT('Ctrl Pts',(180.670880727309,-4.72307016559635,333.621080326329));
#47491=CARTESIAN_POINT('Ctrl Pts',(180.662974392229,-4.75848864658392,333.756630037828));
#47492=CARTESIAN_POINT('Ctrl Pts',(180.655245615586,-4.79311170844795,333.889135608818));
#47493=CARTESIAN_POINT('Ctrl Pts',(180.647516838943,-4.82220588273384,334.023126615179));
#47494=CARTESIAN_POINT('Ctrl Pts',(180.639788062299,-4.84565678919855,334.158101345889));
#47495=CARTESIAN_POINT('Ctrl Pts',(180.631792948001,-4.86991582607383,334.297727375887));
#47496=CARTESIAN_POINT('Ctrl Pts',(180.623797833702,-4.88813555629895,334.438405718679));
#47497=CARTESIAN_POINT('Ctrl Pts',(180.615802719404,-4.9002471782909,334.579570869049));
#47498=CARTESIAN_POINT('Ctrl Pts',(180.607807605105,-4.91235880028286,334.720736019419));
#47499=CARTESIAN_POINT('Ctrl Pts',(180.599812490807,-4.91836229151515,334.862387513434));
#47500=CARTESIAN_POINT('Ctrl Pts',(180.591817376508,-4.9182484086659,335.003956406867));
#47501=CARTESIAN_POINT('',(178.84181737655,-4.91824988879026,335.001045903734));
#47502=CARTESIAN_POINT('Ctrl Pts',(180.591817376458,-4.9182484086652,335.003956407744));
#47503=CARTESIAN_POINT('Ctrl Pts',(180.582712087458,-4.91811871239747,335.165183081947));
#47504=CARTESIAN_POINT('Ctrl Pts',(180.573606798457,-4.9100573358069,335.326074667974));
#47505=CARTESIAN_POINT('Ctrl Pts',(180.564501509456,-4.894186142654,335.485927014637));
#47506=CARTESIAN_POINT('Ctrl Pts',(180.555336394497,-4.87821066842477,335.646829665117));
#47507=CARTESIAN_POINT('Ctrl Pts',(180.546171279538,-4.85432251810979,335.806679301925));
#47508=CARTESIAN_POINT('Ctrl Pts',(180.537006164579,-4.82269491367838,335.96477812583));
#47509=CARTESIAN_POINT('Ctrl Pts',(180.527773926185,-4.79083567511414,336.12403483332));
#47510=CARTESIAN_POINT('Ctrl Pts',(180.51854168779,-4.75112327297293,336.281514919373));
#47511=CARTESIAN_POINT('Ctrl Pts',(180.509309449396,-4.70378293552858,336.436526768957));
#47512=CARTESIAN_POINT('Ctrl Pts',(180.506749709545,-4.69065730519238,336.479505512777));
#47513=CARTESIAN_POINT('Ctrl Pts',(180.504189969693,-4.67694556728002,336.522294644668));
#47514=CARTESIAN_POINT('Ctrl Pts',(180.501630229842,-4.6626531617174,336.564879725738));
#47515=CARTESIAN_POINT('Ctrl Pts',(180.493855154817,-4.61924073233722,336.69422966732));
#47516=CARTESIAN_POINT('Ctrl Pts',(180.486080079792,-4.57037304221952,336.821976137904));
#47517=CARTESIAN_POINT('Ctrl Pts',(180.478305004767,-4.51618657349027,336.947624680457));
#47518=CARTESIAN_POINT('Ctrl Pts',(180.470539497528,-4.46206678508254,337.073118603501));
#47519=CARTESIAN_POINT('Ctrl Pts',(180.462773990289,-4.40264139431559,337.196519379768));
#47520=CARTESIAN_POINT('Ctrl Pts',(180.455008483049,-4.33809655530464,337.317347910728));
#47521=CARTESIAN_POINT('Ctrl Pts',(180.447250675388,-4.27361571314945,337.438056638986));
#47522=CARTESIAN_POINT('Ctrl Pts',(180.439492867727,-4.20402570722914,337.556197854845));
#47523=CARTESIAN_POINT('Ctrl Pts',(180.431735060066,-4.12956051163327,337.67131298115));
#47524=CARTESIAN_POINT('Ctrl Pts',(180.423983090452,-4.05515135394033,337.786341478926));
#47525=CARTESIAN_POINT('Ctrl Pts',(180.416231120837,-3.9758745205178,337.898348093026));
#47526=CARTESIAN_POINT('Ctrl Pts',(180.408479151223,-3.89200940936859,338.006899702332));
#47527=CARTESIAN_POINT('Ctrl Pts',(180.400730464632,-3.80817981579158,338.115405339129));
#47528=CARTESIAN_POINT('Ctrl Pts',(180.392981778041,-3.71976604779773,338.220458572709));
#47529=CARTESIAN_POINT('Ctrl Pts',(180.38523309145,-3.62709010415005,338.32165627946));
#47530=CARTESIAN_POINT('Ctrl Pts',(180.377486017074,-3.53443344293386,338.422832930717));
#47531=CARTESIAN_POINT('Ctrl Pts',(180.369738942698,-3.43751663379423,338.520155362682));
#47532=CARTESIAN_POINT('Ctrl Pts',(180.361991868321,-3.33670088054444,338.613254806442));
#47533=CARTESIAN_POINT('Ctrl Pts',(180.354244729049,-3.2358842827672,338.70635503009));
#47534=CARTESIAN_POINT('Ctrl Pts',(180.346497589776,-3.13116896289556,338.79523192979));
#47535=CARTESIAN_POINT('Ctrl Pts',(180.338750450503,-3.02295148050503,338.879555052968));
#47536=CARTESIAN_POINT('Ctrl Pts',(180.331001569535,-2.91470966889854,338.963897133486));
#47537=CARTESIAN_POINT('Ctrl Pts',(180.323252688567,-2.80296443630261,339.043683160093));
#47538=CARTESIAN_POINT('Ctrl Pts',(180.315503807599,-2.68814344063036,339.118624516158));
#47539=CARTESIAN_POINT('Ctrl Pts',(180.307746701906,-2.57320057301128,339.193645415593));
#47540=CARTESIAN_POINT('Ctrl Pts',(180.299989596212,-2.45517574873292,339.263811158537));
#47541=CARTESIAN_POINT('Ctrl Pts',(180.292232490519,-2.33452396191265,339.328877560495));
#47542=CARTESIAN_POINT('Ctrl Pts',(180.284471239691,-2.21380770287781,339.393978731727));
#47543=CARTESIAN_POINT('Ctrl Pts',(180.276709988864,-2.09046203550478,339.453974961451));
#47544=CARTESIAN_POINT('Ctrl Pts',(180.268948738037,-1.96496339486667,339.508669639631));
#47545=CARTESIAN_POINT('Ctrl Pts',(180.26117507172,-1.8392639970223,339.563451811594));
#47546=CARTESIAN_POINT('Ctrl Pts',(180.253401405404,-1.71140510839831,339.612915343827));
#47547=CARTESIAN_POINT('Ctrl Pts',(180.245627739087,-1.58188067819185,339.656912773766));
#47548=CARTESIAN_POINT('Ctrl Pts',(180.238215891247,-1.45838484892414,339.698862381939));
#47549=CARTESIAN_POINT('Ctrl Pts',(180.230804043408,-1.33337530696609,339.735843184145));
#47550=CARTESIAN_POINT('Ctrl Pts',(180.223392195568,-1.20728826984767,339.767770767978));
#47551=CARTESIAN_POINT('Ctrl Pts',(180.215617114664,-1.07502207446831,339.801263029656));
#47552=CARTESIAN_POINT('Ctrl Pts',(180.207842033761,-0.941152118279231,
339.829300105866));
#47553=CARTESIAN_POINT('Ctrl Pts',(180.200066952857,-0.806168059987069,
339.851729188811));
#47554=CARTESIAN_POINT('Ctrl Pts',(180.19230143966,-0.671350107733285,339.874130671414));
#47555=CARTESIAN_POINT('Ctrl Pts',(180.184535926463,-0.535421163114858,
339.890937828256));
#47556=CARTESIAN_POINT('Ctrl Pts',(180.176770413267,-0.398884849820955,
339.902047933169));
#47557=CARTESIAN_POINT('Ctrl Pts',(180.169012599576,-0.262483912286073,
339.913147022412));
#47558=CARTESIAN_POINT('Ctrl Pts',(180.161254785886,-0.125477191576643,
339.918560269316));
#47559=CARTESIAN_POINT('Ctrl Pts',(180.153496972196,0.0116230674311581,
339.918236265858));
#47560=CARTESIAN_POINT('Ctrl Pts',(180.145744996487,0.148620154490342,339.917912506223));
#47561=CARTESIAN_POINT('Ctrl Pts',(180.137993020778,0.285710250440326,339.911860090816));
#47562=CARTESIAN_POINT('Ctrl Pts',(180.130241045069,0.422377935519294,339.900079585281));
#47563=CARTESIAN_POINT('Ctrl Pts',(180.122492352306,0.558987742110832,339.888304068766));
#47564=CARTESIAN_POINT('Ctrl Pts',(180.114743659543,0.695175105011753,339.870805320436));
#47565=CARTESIAN_POINT('Ctrl Pts',(180.10699496678,0.830426776348472,339.847635963191));
#47566=CARTESIAN_POINT('Ctrl Pts',(180.099247886186,0.96565030765392,339.824471426489));
#47567=CARTESIAN_POINT('Ctrl Pts',(180.091500805591,1.09993814960133,339.795638693551));
#47568=CARTESIAN_POINT('Ctrl Pts',(180.083753724997,1.23278472786932,339.761241946933));
#47569=CARTESIAN_POINT('Ctrl Pts',(180.076006579465,1.36563241968038,339.726844911995));
#47570=CARTESIAN_POINT('Ctrl Pts',(180.068259433933,1.49703844531977,339.686883868326));
#47571=CARTESIAN_POINT('Ctrl Pts',(180.060512288401,1.62651031850972,339.641513465054));
#47572=CARTESIAN_POINT('Ctrl Pts',(180.052763401139,1.75601129983935,339.596132861513));
#47573=CARTESIAN_POINT('Ctrl Pts',(180.045014513878,1.88357689462751,339.545340607619));
#47574=CARTESIAN_POINT('Ctrl Pts',(180.037265626616,2.0087329682738,339.48934014357));
#47575=CARTESIAN_POINT('Ctrl Pts',(180.029508514609,2.13402188381516,339.433280240075));
#47576=CARTESIAN_POINT('Ctrl Pts',(180.021751402602,2.25689581203898,339.372001243529));
#47577=CARTESIAN_POINT('Ctrl Pts',(180.013994290594,2.37690318911734,339.305753626494));
#47578=CARTESIAN_POINT('Ctrl Pts',(180.006233033433,2.49697469432843,339.239470608835));
#47579=CARTESIAN_POINT('Ctrl Pts',(179.998471776271,2.61417626233654,339.168213883172));
#47580=CARTESIAN_POINT('Ctrl Pts',(179.990710519109,2.72808473277588,339.09227769748));
#47581=CARTESIAN_POINT('Ctrl Pts',(179.982936846487,2.84217541933596,339.016220038845));
#47582=CARTESIAN_POINT('Ctrl Pts',(179.975163173864,2.95296216551882,338.935468192095));
#47583=CARTESIAN_POINT('Ctrl Pts',(179.967389501242,3.06005366223507,338.850357729711));
#47584=CARTESIAN_POINT('Ctrl Pts',(179.959977721259,3.16215966157294,338.769209467875));
#47585=CARTESIAN_POINT('Ctrl Pts',(179.952565941277,3.26090650290947,338.684099461569));
#47586=CARTESIAN_POINT('Ctrl Pts',(179.945154161294,3.35598714836865,338.595348845729));
#47587=CARTESIAN_POINT('Ctrl Pts',(179.937379082681,3.45572830296004,338.502247995899));
#47588=CARTESIAN_POINT('Ctrl Pts',(179.929604004068,3.55174996597638,338.404846397423));
#47589=CARTESIAN_POINT('Ctrl Pts',(179.921828925455,3.64365865570261,338.303473121311));
#47590=CARTESIAN_POINT('Ctrl Pts',(179.914063414568,3.73545424596446,338.202224591436));
#47591=CARTESIAN_POINT('Ctrl Pts',(179.906297903682,3.82314667338922,338.097014395261));
#47592=CARTESIAN_POINT('Ctrl Pts',(179.898532392796,3.90637701369591,337.98821044931));
#47593=CARTESIAN_POINT('Ctrl Pts',(179.890774581433,3.98952483090685,337.879514382751));
#47594=CARTESIAN_POINT('Ctrl Pts',(179.883016770071,4.06821912939376,337.767231965866));
#47595=CARTESIAN_POINT('Ctrl Pts',(179.875258958708,4.1421394739621,337.651766136134));
#47596=CARTESIAN_POINT('Ctrl Pts',(179.867506985342,4.21600419115477,337.536387198056));
#47597=CARTESIAN_POINT('Ctrl Pts',(179.859755011976,4.28510189532527,337.417829943359));
#47598=CARTESIAN_POINT('Ctrl Pts',(179.852003038609,4.34915413891717,337.296528105301));
#47599=CARTESIAN_POINT('Ctrl Pts',(179.844254348203,4.41317925638844,337.175277638563));
#47600=CARTESIAN_POINT('Ctrl Pts',(179.836505657797,4.47216298099564,337.051285245185));
#47601=CARTESIAN_POINT('Ctrl Pts',(179.828756967391,4.52587181656437,336.925011003223));
#47602=CARTESIAN_POINT('Ctrl Pts',(179.821009889162,4.57956947758329,336.798763033619));
#47603=CARTESIAN_POINT('Ctrl Pts',(179.813262810932,4.62799427964139,336.670234519221));
#47604=CARTESIAN_POINT('Ctrl Pts',(179.805515732702,4.67096023676915,336.539906987133));
#47605=CARTESIAN_POINT('Ctrl Pts',(179.797768589542,4.71392655401164,336.409578362718));
#47606=CARTESIAN_POINT('Ctrl Pts',(179.790021446381,4.75143381268354,336.277451061759));
#47607=CARTESIAN_POINT('Ctrl Pts',(179.78227430322,4.78334554792102,336.144022915716));
#47608=CARTESIAN_POINT('Ctrl Pts',(179.774525418333,4.81526445760872,336.010564772132));
#47609=CARTESIAN_POINT('Ctrl Pts',(179.766776533446,4.84158524968982,335.875805581584));
#47610=CARTESIAN_POINT('Ctrl Pts',(179.75902764856,4.86222241989627,335.74025414687));
#47611=CARTESIAN_POINT('Ctrl Pts',(179.75127053892,4.88288149462591,335.604558836348));
#47612=CARTESIAN_POINT('Ctrl Pts',(179.74351342928,4.89784483775294,335.468069988922));
#47613=CARTESIAN_POINT('Ctrl Pts',(179.735756319641,4.90707870986626,335.331302879066));
#47614=CARTESIAN_POINT('Ctrl Pts',(179.727995064846,4.91631751626959,335.19446268518));
#47615=CARTESIAN_POINT('Ctrl Pts',(179.720233810052,4.91982074107055,335.057344323124));
#47616=CARTESIAN_POINT('Ctrl Pts',(179.712472555257,4.91760682728085,334.920462871684));
#47617=CARTESIAN_POINT('Ctrl Pts',(179.704698884977,4.91538937194855,334.783362454404));
#47618=CARTESIAN_POINT('Ctrl Pts',(179.696925214697,4.90743652516739,334.646500095476));
#47619=CARTESIAN_POINT('Ctrl Pts',(179.689151544417,4.89381871716129,334.51038645233));
#47620=CARTESIAN_POINT('Ctrl Pts',(179.681739738618,4.88083481834485,334.380608901541));
#47621=CARTESIAN_POINT('Ctrl Pts',(179.67432793282,4.86270153481921,334.251512215092));
#47622=CARTESIAN_POINT('Ctrl Pts',(179.666916127021,4.83952276121924,334.123528376876));
#47623=CARTESIAN_POINT('Ctrl Pts',(179.659141048744,4.81520793376719,333.989271707539));
#47624=CARTESIAN_POINT('Ctrl Pts',(179.651365970466,4.78526368527593,333.85581545574));
#47625=CARTESIAN_POINT('Ctrl Pts',(179.643590892189,4.74975380296486,333.723668587819));
#47626=CARTESIAN_POINT('Ctrl Pts',(179.63582538165,4.71428761786355,333.591684335176));
#47627=CARTESIAN_POINT('Ctrl Pts',(179.62805987111,4.67326952670137,333.461006634296));
#47628=CARTESIAN_POINT('Ctrl Pts',(179.62029436057,4.62681468373114,333.332136412979));
#47629=CARTESIAN_POINT('Ctrl Pts',(179.612536549564,4.58040590091978,333.203393966992));
#47630=CARTESIAN_POINT('Ctrl Pts',(179.604778738559,4.52857122551935,333.076455799486));
#47631=CARTESIAN_POINT('Ctrl Pts',(179.597020927553,4.47147609030416,332.951809423823));
#47632=CARTESIAN_POINT('Ctrl Pts',(179.589268954553,4.41442392104135,332.827256848626));
#47633=CARTESIAN_POINT('Ctrl Pts',(179.581516981553,4.35211933362127,332.704992986379));
#47634=CARTESIAN_POINT('Ctrl Pts',(179.573765008554,4.28477637956999,332.585486707517));
#47635=CARTESIAN_POINT('Ctrl Pts',(179.566016318528,4.21746194537485,332.466031039767));
#47636=CARTESIAN_POINT('Ctrl Pts',(179.558267628502,4.14511357993295,332.349330972468));
#47637=CARTESIAN_POINT('Ctrl Pts',(179.550518938476,4.06799181444826,332.235831832163));
#47638=CARTESIAN_POINT('Ctrl Pts',(179.542771860635,3.99088609484248,332.122356306378));
#47639=CARTESIAN_POINT('Ctrl Pts',(179.535024782794,3.90900917017971,332.012080706));
#47640=CARTESIAN_POINT('Ctrl Pts',(179.527277704953,3.82266531912732,331.905422012545));
#47641=CARTESIAN_POINT('Ctrl Pts',(179.519530562188,3.73632074448113,331.79876242525));
#47642=CARTESIAN_POINT('Ctrl Pts',(179.511783419424,3.6455094147187,331.695720109138));
#47643=CARTESIAN_POINT('Ctrl Pts',(179.504036276659,3.5505761179036,331.596679225599));
#47644=CARTESIAN_POINT('Ctrl Pts',(179.496287392176,3.45562147811633,331.497616075616));
#47645=CARTESIAN_POINT('Ctrl Pts',(179.488538507694,3.35654329766334,331.402556430443));
#47646=CARTESIAN_POINT('Ctrl Pts',(179.480789623211,3.25372316834826,331.311847534842));
#47647=CARTESIAN_POINT('Ctrl Pts',(179.473032513985,3.15079390472287,331.221042359914));
#47648=CARTESIAN_POINT('Ctrl Pts',(179.465275404759,3.04411505188468,331.134597418299));
#47649=CARTESIAN_POINT('Ctrl Pts',(179.457518295533,2.93410165674349,331.052819926784));
#47650=CARTESIAN_POINT('Ctrl Pts',(179.449757041159,2.82402947399585,330.970998736017));
#47651=CARTESIAN_POINT('Ctrl Pts',(179.441995786784,2.71061952142621,330.893850184876));
#47652=CARTESIAN_POINT('Ctrl Pts',(179.434234532409,2.5943149202941,330.82163750294));
#47653=CARTESIAN_POINT('Ctrl Pts',(179.426460862555,2.47782426967704,330.74930930423));
#47654=CARTESIAN_POINT('Ctrl Pts',(179.418687192701,2.35843005798795,330.681932945038));
#47655=CARTESIAN_POINT('Ctrl Pts',(179.410913522847,2.23659982174236,330.619725545142));
#47656=CARTESIAN_POINT('Ctrl Pts',(179.403501712813,2.12044071229309,330.56041386361));
#47657=CARTESIAN_POINT('Ctrl Pts',(179.39608990278,2.00206752582918,330.505800869709));
#47658=CARTESIAN_POINT('Ctrl Pts',(179.388678092746,1.88189975092606,330.456032967773));
#47659=CARTESIAN_POINT('Ctrl Pts',(179.380903013634,1.75584228960839,330.403825831724));
#47660=CARTESIAN_POINT('Ctrl Pts',(179.373127934522,1.62741151364918,330.356785749238));
#47661=CARTESIAN_POINT('Ctrl Pts',(179.36535285541,1.49706994276828,330.315134511114));
#47662=CARTESIAN_POINT('Ctrl Pts',(179.357587344023,1.36688876541817,330.273534527467));
#47663=CARTESIAN_POINT('Ctrl Pts',(179.349821832637,1.23480184043307,330.23731031161));
#47664=CARTESIAN_POINT('Ctrl Pts',(179.34205632125,1.10129272539183,330.206636108587));
#47665=CARTESIAN_POINT('Ctrl Pts',(179.334298509387,0.967915984962775,330.175992319111));
#47666=CARTESIAN_POINT('Ctrl Pts',(179.326540697524,0.833120239161106,330.150887678444));
#47667=CARTESIAN_POINT('Ctrl Pts',(179.318782885661,0.697404973659279,330.131446892021));
#47668=CARTESIAN_POINT('Ctrl Pts',(179.311030911794,0.561791838141364,330.112020735398));
#47669=CARTESIAN_POINT('Ctrl Pts',(179.303278937927,0.425260945617152,330.098250004465));
#47670=CARTESIAN_POINT('Ctrl Pts',(179.29552696406,0.288322414907676,330.090208431353));
#47671=CARTESIAN_POINT('Ctrl Pts',(179.287778273155,0.151441877685195,330.082170263847));
#47672=CARTESIAN_POINT('Ctrl Pts',(179.280029582251,0.0141544350259075,
330.079856451289));
#47673=CARTESIAN_POINT('Ctrl Pts',(179.272280891346,-0.123024439995396,
330.083288899105));
#47674=CARTESIAN_POINT('Ctrl Pts',(179.264533812619,-0.260174773842745,
330.086720632772));
#47675=CARTESIAN_POINT('Ctrl Pts',(179.256786733891,-0.397216194475365,
330.095896238996));
#47676=CARTESIAN_POINT('Ctrl Pts',(179.249039655164,-0.533633390503498,
330.110785495906));
#47677=CARTESIAN_POINT('Ctrl Pts',(179.241292511508,-0.670051729868452,
330.125674877606));
#47678=CARTESIAN_POINT('Ctrl Pts',(179.233545367851,-0.805845445627147,
330.146277963096));
#47679=CARTESIAN_POINT('Ctrl Pts',(179.225798224194,-0.940504903583203,
330.172512704436));
#47680=CARTESIAN_POINT('Ctrl Pts',(179.218049338814,-1.07519463586621,330.198753343907));
#47681=CARTESIAN_POINT('Ctrl Pts',(179.210300453433,-1.20874921932831,330.230628083928));
#47682=CARTESIAN_POINT('Ctrl Pts',(179.202551568053,-1.34067014714226,330.268003949805));
#47683=CARTESIAN_POINT('Ctrl Pts',(179.194794457926,-1.47273109718822,330.305419486811));
#47684=CARTESIAN_POINT('Ctrl Pts',(179.187037347799,-1.60315455113459,330.34834770681));
#47685=CARTESIAN_POINT('Ctrl Pts',(179.179280237672,-1.73145755805979,330.396605840563));
#47686=CARTESIAN_POINT('Ctrl Pts',(179.171518982392,-1.85982912601693,330.444889761922));
#47687=CARTESIAN_POINT('Ctrl Pts',(179.163757727113,-1.98607762956232,330.49850911948));
#47688=CARTESIAN_POINT('Ctrl Pts',(179.155996471834,-2.10974191491704,330.557233731678));
#47689=CARTESIAN_POINT('Ctrl Pts',(179.148222801079,-2.23360402277776,330.616052284093));
#47690=CARTESIAN_POINT('Ctrl Pts',(179.140449130323,-2.35487330574006,330.679992228318));
#47691=CARTESIAN_POINT('Ctrl Pts',(179.132675459568,-2.47311417224835,330.748777898824));
#47692=CARTESIAN_POINT('Ctrl Pts',(179.125263659203,-2.58585083491068,330.814361543133));
#47693=CARTESIAN_POINT('Ctrl Pts',(179.117851858838,-2.69583444196028,330.884349769728));
#47694=CARTESIAN_POINT('Ctrl Pts',(179.110440058472,-2.80271487094277,330.958469050632));
#47695=CARTESIAN_POINT('Ctrl Pts',(179.102708382103,-2.91420800976325,331.035787146694));
#47696=CARTESIAN_POINT('Ctrl Pts',(179.094976705735,-3.02268519373827,331.117851338745));
#47697=CARTESIAN_POINT('Ctrl Pts',(179.087245029366,-3.12771237425401,331.204397496255));
#47698=CARTESIAN_POINT('Ctrl Pts',(179.079522891834,-3.23260997910968,331.29083687878));
#47699=CARTESIAN_POINT('Ctrl Pts',(179.071800754301,-3.33406574526876,331.381746977801));
#47700=CARTESIAN_POINT('Ctrl Pts',(179.064078616769,-3.43167398503973,331.47682008366));
#47701=CARTESIAN_POINT('Ctrl Pts',(179.056364106087,-3.5291858209934,331.571799289554));
#47702=CARTESIAN_POINT('Ctrl Pts',(179.048649595406,-3.62285740967042,331.670933047297));
#47703=CARTESIAN_POINT('Ctrl Pts',(179.040935084725,-3.712315934423,331.773873302933));
#47704=CARTESIAN_POINT('Ctrl Pts',(179.033226296048,-3.80170810603049,331.876737205759));
#47705=CARTESIAN_POINT('Ctrl Pts',(179.025517507371,-3.88689317395647,331.983401690286));
#47706=CARTESIAN_POINT('Ctrl Pts',(179.017808718694,-3.96753532506472,332.093482064933));
#47707=CARTESIAN_POINT('Ctrl Pts',(179.010103047342,-4.0481448656259,332.203517924632));
#47708=CARTESIAN_POINT('Ctrl Pts',(179.00239737599,-4.12421490884533,332.316966609159));
#47709=CARTESIAN_POINT('Ctrl Pts',(178.994691704638,-4.19545027138025,332.433410807536));
#47710=CARTESIAN_POINT('Ctrl Pts',(178.986987464531,-4.26667240272455,332.549833377674));
#47711=CARTESIAN_POINT('Ctrl Pts',(178.979283224423,-4.33306143284986,332.66925001773));
#47712=CARTESIAN_POINT('Ctrl Pts',(178.971578984316,-4.39436609070922,332.791215328891));
#47713=CARTESIAN_POINT('Ctrl Pts',(178.963874459602,-4.45567301325495,332.913185145635));
#47714=CARTESIAN_POINT('Ctrl Pts',(178.956169934889,-4.51189501222608,333.037703467143));
#47715=CARTESIAN_POINT('Ctrl Pts',(178.948465410175,-4.56282748927638,333.164301668137));
#47716=CARTESIAN_POINT('Ctrl Pts',(178.940758885133,-4.61377318993814,333.290932737853));
#47717=CARTESIAN_POINT('Ctrl Pts',(178.933052360092,-4.65942648923579,333.419644394199));
#47718=CARTESIAN_POINT('Ctrl Pts',(178.925345835051,-4.69963166973435,333.549949921096));
#47719=CARTESIAN_POINT('Ctrl Pts',(178.917631200045,-4.73987916017159,333.680392575069));
#47720=CARTESIAN_POINT('Ctrl Pts',(178.909916565038,-4.7746669667763,333.812432070305));
#47721=CARTESIAN_POINT('Ctrl Pts',(178.902201930032,-4.80388971657654,333.945568089695));
#47722=CARTESIAN_POINT('Ctrl Pts',(178.894482839354,-4.83312934429419,334.078781003242));
#47723=CARTESIAN_POINT('Ctrl Pts',(178.886763748677,-4.85679744504241,334.213091313241));
#47724=CARTESIAN_POINT('Ctrl Pts',(178.879044657999,-4.8748403203292,334.347991630581));
#47725=CARTESIAN_POINT('Ctrl Pts',(178.871314161668,-4.89290985559224,334.483091275311));
#47726=CARTESIAN_POINT('Ctrl Pts',(178.863583665338,-4.90533753073623,334.618782275072));
#47727=CARTESIAN_POINT('Ctrl Pts',(178.855853169007,-4.91212170826543,334.754554719566));
#47728=CARTESIAN_POINT('Ctrl Pts',(178.851174571521,-4.91622758123578,334.836725978729));
#47729=CARTESIAN_POINT('Ctrl Pts',(178.846495974035,-4.91826735198843,334.918927091343));
#47730=CARTESIAN_POINT('Ctrl Pts',(178.84181737655,-4.91824988879026,335.001045903734));
#47731=CARTESIAN_POINT('',(177.091817376539,-4.91824792695348,334.995484303182));
#47732=CARTESIAN_POINT('Ctrl Pts',(178.841817376508,-4.9182498887901,335.001045904463));
#47733=CARTESIAN_POINT('Ctrl Pts',(178.838612259072,-4.91823792545276,335.057302173198));
#47734=CARTESIAN_POINT('Ctrl Pts',(178.835407141635,-4.91726078409659,335.113547047247));
#47735=CARTESIAN_POINT('Ctrl Pts',(178.832202024199,-4.91531943401054,335.169758428769));
#47736=CARTESIAN_POINT('Ctrl Pts',(178.824426945485,-4.91061004347224,335.306117836682));
#47737=CARTESIAN_POINT('Ctrl Pts',(178.816651866771,-4.90021464528335,335.442496600396));
#47738=CARTESIAN_POINT('Ctrl Pts',(178.808876788057,-4.88412299907667,335.578381874189));
#47739=CARTESIAN_POINT('Ctrl Pts',(178.801111277073,-4.86805115466751,335.714099932481));
#47740=CARTESIAN_POINT('Ctrl Pts',(178.79334576609,-4.84629705485512,335.849325324696));
#47741=CARTESIAN_POINT('Ctrl Pts',(178.785580255107,-4.81890244856952,335.983545755759));
#47742=CARTESIAN_POINT('Ctrl Pts',(178.777822443651,-4.79153500411964,336.117633106854));
#47743=CARTESIAN_POINT('Ctrl Pts',(178.770064632195,-4.75853826040876,336.250717099221));
#47744=CARTESIAN_POINT('Ctrl Pts',(178.76230682074,-4.72000565339145,336.382291465087));
#47745=CARTESIAN_POINT('Ctrl Pts',(178.754554847284,-4.68150204338778,336.513766817054));
#47746=CARTESIAN_POINT('Ctrl Pts',(178.746802873829,-4.6374709715389,336.643734430148));
#47747=CARTESIAN_POINT('Ctrl Pts',(178.739050900373,-4.58805667201154,336.771699477031));
#47748=CARTESIAN_POINT('Ctrl Pts',(178.731302209885,-4.53866329947717,336.899610330619));
#47749=CARTESIAN_POINT('Ctrl Pts',(178.723553519396,-4.4838913741393,337.02551994091));
#47750=CARTESIAN_POINT('Ctrl Pts',(178.715804828907,-4.42393451805586,337.148950079098));
#47751=CARTESIAN_POINT('Ctrl Pts',(178.708057750598,-4.36399013650276,337.272354536603));
#47752=CARTESIAN_POINT('Ctrl Pts',(178.70031067229,-4.29886314063021,337.393280196748));
#47753=CARTESIAN_POINT('Ctrl Pts',(178.692563593982,-4.22879452873173,337.511270574086));
#47754=CARTESIAN_POINT('Ctrl Pts',(178.684816450746,-4.15872532959671,337.629261940286));
#47755=CARTESIAN_POINT('Ctrl Pts',(178.67706930751,-4.08371463141165,337.74431763853));
#47756=CARTESIAN_POINT('Ctrl Pts',(178.669322164275,-4.00404824948484,337.85600782182));
#47757=CARTESIAN_POINT('Ctrl Pts',(178.661573279317,-3.92436395686988,337.967723115426));
#47758=CARTESIAN_POINT('Ctrl Pts',(178.65382439436,-3.84002212463943,338.076071070295));
#47759=CARTESIAN_POINT('Ctrl Pts',(178.646075509403,-3.7513503086192,338.180653065728));
#47760=CARTESIAN_POINT('Ctrl Pts',(178.638318399699,-3.66258437542264,338.285346065565));
#47761=CARTESIAN_POINT('Ctrl Pts',(178.630561289996,-3.56947953089565,338.386264822521));
#47762=CARTESIAN_POINT('Ctrl Pts',(178.622804180292,-3.47240220618024,338.483045503724));
#47763=CARTESIAN_POINT('Ctrl Pts',(178.615042925438,-3.37527300645101,338.579877901425));
#47764=CARTESIAN_POINT('Ctrl Pts',(178.607281670583,-3.27416738470544,338.672567553242));
#47765=CARTESIAN_POINT('Ctrl Pts',(178.599520415729,-3.16948589351096,338.760790107588));
#47766=CARTESIAN_POINT('Ctrl Pts',(178.591746745396,-3.06463694604437,338.849153789272));
#47767=CARTESIAN_POINT('Ctrl Pts',(178.583973075063,-2.95620100775418,338.933035854573));
#47768=CARTESIAN_POINT('Ctrl Pts',(178.57619940473,-2.84460943769667,339.012154061033));
#47769=CARTESIAN_POINT('Ctrl Pts',(178.568787599795,-2.73821247020903,339.08758930436));
#47770=CARTESIAN_POINT('Ctrl Pts',(178.561375794859,-2.62894728930402,339.15869406513));
#47771=CARTESIAN_POINT('Ctrl Pts',(178.553963989924,-2.51720789974148,339.225263003883));
#47772=CARTESIAN_POINT('Ctrl Pts',(178.546188911095,-2.39999184105947,339.295094677939));
#47773=CARTESIAN_POINT('Ctrl Pts',(178.538413832265,-2.27968248062893,339.360155341192));
#47774=CARTESIAN_POINT('Ctrl Pts',(178.530638753435,-2.1567055397287,339.420158852055));
#47775=CARTESIAN_POINT('Ctrl Pts',(178.522873242334,-2.03387992977276,339.480088524784));
#47776=CARTESIAN_POINT('Ctrl Pts',(178.515107731234,-1.90839361876503,339.534973257639));
#47777=CARTESIAN_POINT('Ctrl Pts',(178.507342220133,-1.78069999932524,339.584570925932));
#47778=CARTESIAN_POINT('Ctrl Pts',(178.499584408558,-1.65313298847095,339.634119417997));
#47779=CARTESIAN_POINT('Ctrl Pts',(178.491826596984,-1.52336338653626,339.678391137045));
#47780=CARTESIAN_POINT('Ctrl Pts',(178.484068785409,-1.39186748846544,339.717190684831));
#47781=CARTESIAN_POINT('Ctrl Pts',(178.476316811833,-1.26047054521905,339.755961034729));
#47782=CARTESIAN_POINT('Ctrl Pts',(178.468564838257,-1.12735026500233,339.789267299835));
#47783=CARTESIAN_POINT('Ctrl Pts',(178.460812864682,-0.993000812081995,
339.816962990278));
#47784=CARTESIAN_POINT('Ctrl Pts',(178.453064174071,-0.858708256224505,
339.844646951581));
#47785=CARTESIAN_POINT('Ctrl Pts',(178.44531548346,-0.72318794503902,339.866724985326));
#47786=CARTESIAN_POINT('Ctrl Pts',(178.437566792849,-0.586946811351083,
339.883101115392));
#47787=CARTESIAN_POINT('Ctrl Pts',(178.429819714417,-0.450734023762842,
339.899473838269));
#47788=CARTESIAN_POINT('Ctrl Pts',(178.422072635985,-0.313801099816476,
339.91014697054));
#47789=CARTESIAN_POINT('Ctrl Pts',(178.414325557554,-0.176662325884397,
339.915076142351));
#47790=CARTESIAN_POINT('Ctrl Pts',(178.406578414194,-0.0395224025923842,
339.920005355474));
#47791=CARTESIAN_POINT('Ctrl Pts',(178.398831270834,0.0978229835043959,
339.919190498078));
#47792=CARTESIAN_POINT('Ctrl Pts',(178.391084127474,0.234857693818518,339.912639303486));
#47793=CARTESIAN_POINT('Ctrl Pts',(178.383335242392,0.371923212448787,339.906086636046));
#47794=CARTESIAN_POINT('Ctrl Pts',(178.37558635731,0.508677525957545,339.893795083812));
#47795=CARTESIAN_POINT('Ctrl Pts',(178.367837472227,0.644608166431105,339.87582437894));
#47796=CARTESIAN_POINT('Ctrl Pts',(178.360080362398,0.780683085091036,339.857834599778));
#47797=CARTESIAN_POINT('Ctrl Pts',(178.352323252569,0.915932196194659,339.83415367797));
#47798=CARTESIAN_POINT('Ctrl Pts',(178.34456614274,1.0498512479887,339.804892862447));
#47799=CARTESIAN_POINT('Ctrl Pts',(178.336804887759,1.18384186184367,339.77561641088));
#47800=CARTESIAN_POINT('Ctrl Pts',(178.329043632779,1.31650062232678,339.740754223554));
#47801=CARTESIAN_POINT('Ctrl Pts',(178.321282377798,1.44733801327893,339.700467608421));
#47802=CARTESIAN_POINT('Ctrl Pts',(178.313508707339,1.5783847014096,339.660116547836));
#47803=CARTESIAN_POINT('Ctrl Pts',(178.305735036881,1.70760382916077,339.614323850227));
#47804=CARTESIAN_POINT('Ctrl Pts',(178.297961366422,1.834524619681,339.563299517047));
#47805=CARTESIAN_POINT('Ctrl Pts',(178.290549562831,1.95553720644523,339.514650383042));
#47806=CARTESIAN_POINT('Ctrl Pts',(178.283137759241,2.07446035361744,339.461245836355));
#47807=CARTESIAN_POINT('Ctrl Pts',(178.275725955651,2.19090816849813,339.4033060829));
#47808=CARTESIAN_POINT('Ctrl Pts',(178.267950876883,2.31306344715932,339.342526524813));
#47809=CARTESIAN_POINT('Ctrl Pts',(178.260175798116,2.43288064419288,339.276563875661));
#47810=CARTESIAN_POINT('Ctrl Pts',(178.252400719349,2.54988875482794,339.20562128591));
#47811=CARTESIAN_POINT('Ctrl Pts',(178.244635208311,2.66675287953293,339.134765995533));
#47812=CARTESIAN_POINT('Ctrl Pts',(178.236869697274,2.78081446475652,339.058943158501));
#47813=CARTESIAN_POINT('Ctrl Pts',(178.229104186236,2.89162454592362,338.978403014768));
#47814=CARTESIAN_POINT('Ctrl Pts',(178.221346374725,3.002324758572,338.897942726822));
#47815=CARTESIAN_POINT('Ctrl Pts',(178.213588563214,3.10977956871502,338.812774668443));
#47816=CARTESIAN_POINT('Ctrl Pts',(178.205830751703,3.21356691127736,338.723193625));
#47817=CARTESIAN_POINT('Ctrl Pts',(178.198078778192,3.3172761505726,338.633679994134));
#47818=CARTESIAN_POINT('Ctrl Pts',(178.19032680468,3.41732312099803,338.539760242682));
#47819=CARTESIAN_POINT('Ctrl Pts',(178.182574831168,3.5133172154582,338.441770649835));
#47820=CARTESIAN_POINT('Ctrl Pts',(178.174826140622,3.60927065636261,338.343822555639));
#47821=CARTESIAN_POINT('Ctrl Pts',(178.167077450076,3.7011743621283,338.241808326765));
#47822=CARTESIAN_POINT('Ctrl Pts',(178.159328759529,3.7886732939505,338.136102315647));
#47823=CARTESIAN_POINT('Ctrl Pts',(178.151581681163,3.87615402088921,338.030418297548));
#47824=CARTESIAN_POINT('Ctrl Pts',(178.143834602796,3.95923154768538,337.921044325935));
#47825=CARTESIAN_POINT('Ctrl Pts',(178.13608752443,4.03759025291669,337.808388864109));
#47826=CARTESIAN_POINT('Ctrl Pts',(178.128340381135,4.11594961486958,337.695732458122));
#47827=CARTESIAN_POINT('Ctrl Pts',(178.120593237841,4.18958985318097,337.57979482795));
#47828=CARTESIAN_POINT('Ctrl Pts',(178.112846094546,4.25823815876292,337.461014190482));
#47829=CARTESIAN_POINT('Ctrl Pts',(178.105097209529,4.3269018979417,337.342206848605));
#47830=CARTESIAN_POINT('Ctrl Pts',(178.097348324513,4.39057127560532,337.220555565911));
#47831=CARTESIAN_POINT('Ctrl Pts',(178.089599439496,4.44901919600697,337.096523612093));
#47832=CARTESIAN_POINT('Ctrl Pts',(178.081842329732,4.5075291536362,336.972360009475));
#47833=CARTESIAN_POINT('Ctrl Pts',(178.074085219969,4.56080641623842,336.845811042217));
#47834=CARTESIAN_POINT('Ctrl Pts',(178.066328110205,4.60867165585424,336.717360949546));
#47835=CARTESIAN_POINT('Ctrl Pts',(178.05856685529,4.65656247312396,336.588842217252));
#47836=CARTESIAN_POINT('Ctrl Pts',(178.050805600375,4.69903538383889,336.458420706747));
#47837=CARTESIAN_POINT('Ctrl Pts',(178.04304434546,4.73596113001569,336.326595355593));
#47838=CARTESIAN_POINT('Ctrl Pts',(178.035270675066,4.77294594535329,336.194559126835));
#47839=CARTESIAN_POINT('Ctrl Pts',(178.027497004672,4.80436577433105,336.061114950551));
#47840=CARTESIAN_POINT('Ctrl Pts',(178.019723334279,4.83014244728336,335.926772356866));
#47841=CARTESIAN_POINT('Ctrl Pts',(178.012311529978,4.85471921035278,335.798683440922));
#47842=CARTESIAN_POINT('Ctrl Pts',(178.004899725677,4.8741663288044,335.669778152457));
#47843=CARTESIAN_POINT('Ctrl Pts',(177.997487921376,4.88846014980437,335.540500163066));
#47844=CARTESIAN_POINT('Ctrl Pts',(177.989712842606,4.90345455328522,335.404885876716));
#47845=CARTESIAN_POINT('Ctrl Pts',(177.981937763835,4.91282511478255,335.268432865106));
#47846=CARTESIAN_POINT('Ctrl Pts',(177.974162685065,4.91648778014887,335.13164714257));
#47847=CARTESIAN_POINT('Ctrl Pts',(177.966397174024,4.9201459383722,334.995029743576));
#47848=CARTESIAN_POINT('Ctrl Pts',(177.958631662983,4.91811016570806,334.858080835288));
#47849=CARTESIAN_POINT('Ctrl Pts',(177.950866151942,4.91034793377973,334.721313380793));
#47850=CARTESIAN_POINT('Ctrl Pts',(177.943108340428,4.9025933981271,334.58468153163));
#47851=CARTESIAN_POINT('Ctrl Pts',(177.935350528914,4.88912372436133,334.448231165957));
#47852=CARTESIAN_POINT('Ctrl Pts',(177.9275927174,4.86995840015661,334.31247673258));
#47853=CARTESIAN_POINT('Ctrl Pts',(177.919840743885,4.85080749846647,334.176824458721));
#47854=CARTESIAN_POINT('Ctrl Pts',(177.912088770371,4.82596953214509,334.041867460213));
#47855=CARTESIAN_POINT('Ctrl Pts',(177.904336796856,4.79551590562572,333.908116186863));
#47856=CARTESIAN_POINT('Ctrl Pts',(177.896588106307,4.76507517623592,333.774421557259));
#47857=CARTESIAN_POINT('Ctrl Pts',(177.888839415758,4.72902360338711,333.641932017542));
#47858=CARTESIAN_POINT('Ctrl Pts',(177.881090725209,4.68748385615793,333.511148710999));
#47859=CARTESIAN_POINT('Ctrl Pts',(177.873343646839,4.64595275162066,333.380392615018));
#47860=CARTESIAN_POINT('Ctrl Pts',(177.86559656847,4.59893586219554,333.251342418399));
#47861=CARTESIAN_POINT('Ctrl Pts',(177.857849490101,4.54660587252341,333.12448457686));
#47862=CARTESIAN_POINT('Ctrl Pts',(177.850102346804,4.4942754442762,332.997625672132));
#47863=CARTESIAN_POINT('Ctrl Pts',(177.842355203507,4.43663197602107,332.87295952047));
#47864=CARTESIAN_POINT('Ctrl Pts',(177.83460806021,4.37389634103569,332.75095267716));
#47865=CARTESIAN_POINT('Ctrl Pts',(177.82685917519,4.31114660174834,332.628918404122));
#47866=CARTESIAN_POINT('Ctrl Pts',(177.819110290171,4.24330259635909,332.509544976673));
#47867=CARTESIAN_POINT('Ctrl Pts',(177.811361405152,4.170631003696,332.393274066284));
#47868=CARTESIAN_POINT('Ctrl Pts',(177.803604295386,4.09788227665428,332.27687974475));
#47869=CARTESIAN_POINT('Ctrl Pts',(177.79584718562,4.02029593406106,332.163594850421));
#47870=CARTESIAN_POINT('Ctrl Pts',(177.788090075854,3.93818213836565,332.053832233637));
#47871=CARTESIAN_POINT('Ctrl Pts',(177.780328820937,3.8560244636839,331.944010963221));
#47872=CARTESIAN_POINT('Ctrl Pts',(177.77256756602,3.76933476208939,331.837716023543));
#47873=CARTESIAN_POINT('Ctrl Pts',(177.764806311102,3.67846265191155,331.735326114144));
#47874=CARTESIAN_POINT('Ctrl Pts',(177.757032640707,3.58744517597258,331.632772414259));
#47875=CARTESIAN_POINT('Ctrl Pts',(177.749258970311,3.49223219347847,331.534136508935));
#47876=CARTESIAN_POINT('Ctrl Pts',(177.741485299915,3.39320987709146,331.439759868701));
#47877=CARTESIAN_POINT('Ctrl Pts',(177.734073495644,3.29879707205368,331.349776482535));
#47878=CARTESIAN_POINT('Ctrl Pts',(177.726661691373,3.20092181693157,331.263664937921));
#47879=CARTESIAN_POINT('Ctrl Pts',(177.719249887103,3.09994440472266,331.181685221183));
#47880=CARTESIAN_POINT('Ctrl Pts',(177.711474808317,2.99401778997952,331.095687435326));
#47881=CARTESIAN_POINT('Ctrl Pts',(177.70369972953,2.88434248966918,331.013964975834));
#47882=CARTESIAN_POINT('Ctrl Pts',(177.695924650744,2.77129853552137,330.936862359024));
#47883=CARTESIAN_POINT('Ctrl Pts',(177.688159139687,2.65839368915438,330.859854621891));
#47884=CARTESIAN_POINT('Ctrl Pts',(177.680393628631,2.54212875682175,330.787455634041));
#47885=CARTESIAN_POINT('Ctrl Pts',(177.672628117574,2.42291749715954,330.71997034304));
#47886=CARTESIAN_POINT('Ctrl Pts',(177.664870306044,2.3038244358069,330.6525519639));
#47887=CARTESIAN_POINT('Ctrl Pts',(177.657112494514,2.18179119862214,330.590037777483));
#47888=CARTESIAN_POINT('Ctrl Pts',(177.649354682984,2.05726094248102,330.532689793954));
#47889=CARTESIAN_POINT('Ctrl Pts',(177.641602709453,1.93282439930542,330.4753849666));
#47890=CARTESIAN_POINT('Ctrl Pts',(177.633850735922,1.80589493100876,330.423238766636));
#47891=CARTESIAN_POINT('Ctrl Pts',(177.626098762391,1.67694042676136,330.376467382229));
#47892=CARTESIAN_POINT('Ctrl Pts',(177.618350071825,1.54804053482146,330.32971580553));
#47893=CARTESIAN_POINT('Ctrl Pts',(177.610601381259,1.41711767933166,330.288334650108));
#47894=CARTESIAN_POINT('Ctrl Pts',(177.602852690694,1.28465966565384,330.252491958307));
#47895=CARTESIAN_POINT('Ctrl Pts',(177.595105612308,1.15222921097109,330.216656723876));
#47896=CARTESIAN_POINT('Ctrl Pts',(177.587358533922,1.01826461048224,330.186357763046));
#47897=CARTESIAN_POINT('Ctrl Pts',(177.579611455536,0.883268384747759,330.161713110717));
#47898=CARTESIAN_POINT('Ctrl Pts',(177.571864312222,0.748271027614099,330.137068251843));
#47899=CARTESIAN_POINT('Ctrl Pts',(177.564117168908,0.612242412508957,330.118077866188));
#47900=CARTESIAN_POINT('Ctrl Pts',(177.556370025594,0.475694402931241,330.104808696535));
#47901=CARTESIAN_POINT('Ctrl Pts',(177.548621140558,0.339115694461391,330.091536543691));
#47902=CARTESIAN_POINT('Ctrl Pts',(177.540872255521,0.202017748123602,330.083988204144));
#47903=CARTESIAN_POINT('Ctrl Pts',(177.533123370485,0.0649162900988813,
330.082178435752));
#47904=CARTESIAN_POINT('Ctrl Pts',(177.525366260702,-0.0723306888300711,
330.080366746454));
#47905=CARTESIAN_POINT('Ctrl Pts',(177.517609150919,-0.209580795434104,
330.08430580078));
#47906=CARTESIAN_POINT('Ctrl Pts',(177.509852041136,-0.34631900835463,330.093958193518));
#47907=CARTESIAN_POINT('Ctrl Pts',(177.502090786202,-0.483130289804384,
330.103615744185));
#47908=CARTESIAN_POINT('Ctrl Pts',(177.494329531267,-0.619428744305054,
330.118992672895));
#47909=CARTESIAN_POINT('Ctrl Pts',(177.486568276333,-0.75470671679276,330.139999914184));
#47910=CARTESIAN_POINT('Ctrl Pts',(177.47879460592,-0.890201089948413,330.161040760214));
#47911=CARTESIAN_POINT('Ctrl Pts',(177.471020935507,-1.02467133539786,330.187729840673));
#47912=CARTESIAN_POINT('Ctrl Pts',(177.463247265095,-1.15762132310105,330.219927204027));
#47913=CARTESIAN_POINT('Ctrl Pts',(177.455835461006,-1.28438245524558,330.250625771972));
#47914=CARTESIAN_POINT('Ctrl Pts',(177.448423656917,-1.4097614037054,330.28633126344));
#47915=CARTESIAN_POINT('Ctrl Pts',(177.441011852828,-1.53334456524882,330.326881393895));
#47916=CARTESIAN_POINT('Ctrl Pts',(177.433236774052,-1.66298490718434,330.369419007532));
#47917=CARTESIAN_POINT('Ctrl Pts',(177.425461695276,-1.79105866483917,330.417422595237));
#47918=CARTESIAN_POINT('Ctrl Pts',(177.4176866165,-1.9170704701182,330.470759017771));
#47919=CARTESIAN_POINT('Ctrl Pts',(177.409921105453,-2.04292720984825,330.524029806442));
#47920=CARTESIAN_POINT('Ctrl Pts',(177.402155594406,-2.16672668931163,330.582620221759));
#47921=CARTESIAN_POINT('Ctrl Pts',(177.394390083359,-2.28798856305544,330.646347349888));
#47922=CARTESIAN_POINT('Ctrl Pts',(177.386632271839,-2.40913020529838,330.710011292383));
#47923=CARTESIAN_POINT('Ctrl Pts',(177.378874460319,-2.52773890511602,330.778801631536));
#47924=CARTESIAN_POINT('Ctrl Pts',(177.371116648799,-2.64335451495748,330.85248749601));
#47925=CARTESIAN_POINT('Ctrl Pts',(177.363364675279,-2.7588831203857,330.926117909534));
#47926=CARTESIAN_POINT('Ctrl Pts',(177.355612701758,-2.87142279082685,331.00463630625));
#47927=CARTESIAN_POINT('Ctrl Pts',(177.347860728237,-2.98053852736156,331.087766219995));
#47928=CARTESIAN_POINT('Ctrl Pts',(177.340112037682,-3.08960805331701,331.170860928172));
#47929=CARTESIAN_POINT('Ctrl Pts',(177.332363347126,-3.1952562191147,331.258563032656));
#47930=CARTESIAN_POINT('Ctrl Pts',(177.324614656571,-3.29707773489245,331.350553264867));
#47931=CARTESIAN_POINT('Ctrl Pts',(177.316867578195,-3.3988780658534,331.442524357741));
#47932=CARTESIAN_POINT('Ctrl Pts',(177.30912049982,-3.49685304057089,331.538781541862));
#47933=CARTESIAN_POINT('Ctrl Pts',(177.301373421444,-3.59063145826818,331.63896611243));
#47934=CARTESIAN_POINT('Ctrl Pts',(177.293626278141,-3.68441066191886,331.739151522641));
#47935=CARTESIAN_POINT('Ctrl Pts',(177.285879134837,-3.77399297128208,331.843264099588));
#47936=CARTESIAN_POINT('Ctrl Pts',(177.278131991534,-3.85904526221765,331.950909524685));
#47937=CARTESIAN_POINT('Ctrl Pts',(177.270383106508,-3.94411667471395,332.05857915076));
#47938=CARTESIAN_POINT('Ctrl Pts',(177.262634221482,-4.02465579991533,332.169782898837));
#47939=CARTESIAN_POINT('Ctrl Pts',(177.254885336456,-4.10037113859408,332.284095070095));
#47940=CARTESIAN_POINT('Ctrl Pts',(177.247128226684,-4.17616684231572,332.398528573472));
#47941=CARTESIAN_POINT('Ctrl Pts',(177.239371116911,-4.24712831561527,332.516076764328));
#47942=CARTESIAN_POINT('Ctrl Pts',(177.231614007139,-4.31300830572589,332.636286308108));
#47943=CARTESIAN_POINT('Ctrl Pts',(177.223852752215,-4.37892349999687,332.756560088024));
#47944=CARTESIAN_POINT('Ctrl Pts',(177.216091497291,-4.43975162718117,332.879497704452));
#47945=CARTESIAN_POINT('Ctrl Pts',(177.208330242367,-4.4952928630415,333.004624060988));
#47946=CARTESIAN_POINT('Ctrl Pts',(177.200556571964,-4.55092294677859,333.129950578916));
#47947=CARTESIAN_POINT('Ctrl Pts',(177.192782901562,-4.60124909543224,333.257472469751));
#47948=CARTESIAN_POINT('Ctrl Pts',(177.185009231159,-4.64612051280132,333.386696791354));
#47949=CARTESIAN_POINT('Ctrl Pts',(177.177597426958,-4.68890315504944,333.509905690138));
#47950=CARTESIAN_POINT('Ctrl Pts',(177.170185622756,-4.72672738943699,333.634661814839));
#47951=CARTESIAN_POINT('Ctrl Pts',(177.162773818555,-4.75950586004737,333.760529536183));
#47952=CARTESIAN_POINT('Ctrl Pts',(177.152670117745,-4.80418915861181,333.932111213659));
#47953=CARTESIAN_POINT('Ctrl Pts',(177.142566416936,-4.8396124932973,334.106196656317));
#47954=CARTESIAN_POINT('Ctrl Pts',(177.132462716126,-4.86554630448217,334.281917677811));
#47955=CARTESIAN_POINT('Ctrl Pts',(177.122563772259,-4.89095455300756,334.454077618108));
#47956=CARTESIAN_POINT('Ctrl Pts',(177.112664828391,-4.90725404236607,334.627807747289));
#47957=CARTESIAN_POINT('Ctrl Pts',(177.102765884524,-4.91427367871666,334.802269695867));
#47958=CARTESIAN_POINT('Ctrl Pts',(177.099116381862,-4.91686164990708,334.866589622739));
#47959=CARTESIAN_POINT('Ctrl Pts',(177.0954668792,-4.91818872865841,334.931008785057));
#47960=CARTESIAN_POINT('Ctrl Pts',(177.091817376539,-4.91824792695348,334.995484303182));
#47961=CARTESIAN_POINT('',(175.341817376454,-4.91824985388346,335.001198864178));
#47962=CARTESIAN_POINT('Ctrl Pts',(177.091817376508,-4.91824792695398,334.995484303725));
#47963=CARTESIAN_POINT('Ctrl Pts',(177.084148538999,-4.91837232254791,335.13096914033));
#47964=CARTESIAN_POINT('Ctrl Pts',(177.076479701491,-4.91289412939069,335.266594157412));
#47965=CARTESIAN_POINT('Ctrl Pts',(177.068810863982,-4.90180544779519,335.401853722722));
#47966=CARTESIAN_POINT('Ctrl Pts',(177.061132735662,-4.89070333223931,335.537277155271));
#47967=CARTESIAN_POINT('Ctrl Pts',(177.053454607341,-4.87397710942963,335.672333847374));
#47968=CARTESIAN_POINT('Ctrl Pts',(177.04577647902,-4.85167123739451,335.806516749199));
#47969=CARTESIAN_POINT('Ctrl Pts',(177.038114233037,-4.82941150543142,335.940422091431));
#47970=CARTESIAN_POINT('Ctrl Pts',(177.030451987054,-4.80159524579017,336.073456857911));
#47971=CARTESIAN_POINT('Ctrl Pts',(177.022789741071,-4.76831839161924,336.20512355327));
#47972=CARTESIAN_POINT('Ctrl Pts',(177.015127988233,-4.73504367916306,336.336781774496));
#47973=CARTESIAN_POINT('Ctrl Pts',(177.007466235396,-4.6963091691295,336.467071711546));
#47974=CARTESIAN_POINT('Ctrl Pts',(176.999804482559,-4.65226142676251,336.59550828251));
#47975=CARTESIAN_POINT('Ctrl Pts',(176.992141475785,-4.60820647545964,336.723965873643));
#47976=CARTESIAN_POINT('Ctrl Pts',(176.984478469011,-4.55883669257436,336.850569116841));
#47977=CARTESIAN_POINT('Ctrl Pts',(176.976815462237,-4.50434762908291,336.97485075357));
#47978=CARTESIAN_POINT('Ctrl Pts',(176.969125489074,-4.44966681667031,337.099569741727));
#47979=CARTESIAN_POINT('Ctrl Pts',(176.961435515911,-4.38983079202168,337.221950383105));
#47980=CARTESIAN_POINT('Ctrl Pts',(176.953745542748,-4.32508420336451,337.341544297319));
#47981=CARTESIAN_POINT('Ctrl Pts',(176.946070909403,-4.26046677002372,337.46089964777));
#47982=CARTESIAN_POINT('Ctrl Pts',(176.938396276059,-4.19095858995303,337.577479057295));
#47983=CARTESIAN_POINT('Ctrl Pts',(176.930721642714,-4.11684648137234,337.690865680652));
#47984=CARTESIAN_POINT('Ctrl Pts',(176.923023999642,-4.04251217332467,337.804592254495));
#47985=CARTESIAN_POINT('Ctrl Pts',(176.91532635657,-3.9635465404106,337.915106551997));
#47986=CARTESIAN_POINT('Ctrl Pts',(176.907628713498,-3.88027923995974,338.022021853402));
#47987=CARTESIAN_POINT('Ctrl Pts',(176.899931070425,-3.79701193950888,338.128937154806));
#47988=CARTESIAN_POINT('Ctrl Pts',(176.892233427353,-3.70944327822093,338.232253196925));
#47989=CARTESIAN_POINT('Ctrl Pts',(176.884535784281,-3.61793887719243,338.331621428584));
#47990=CARTESIAN_POINT('Ctrl Pts',(176.876760705501,-3.52551397258233,338.431989271323));
#47991=CARTESIAN_POINT('Ctrl Pts',(176.868985626722,-3.42876328950201,338.528666761841));
#47992=CARTESIAN_POINT('Ctrl Pts',(176.861210547942,-3.32801323321346,338.621258204279));
#47993=CARTESIAN_POINT('Ctrl Pts',(176.853445036892,-3.22738715628303,338.713735707053));
#47994=CARTESIAN_POINT('Ctrl Pts',(176.845679525842,-3.12277178353067,338.802136904345));
#47995=CARTESIAN_POINT('Ctrl Pts',(176.837914014792,-3.01453259830653,338.886100394515));
#47996=CARTESIAN_POINT('Ctrl Pts',(176.830156203268,-2.90640073254962,338.969980634639));
#47997=CARTESIAN_POINT('Ctrl Pts',(176.822398391745,-2.79465251149058,339.049431685854));
#47998=CARTESIAN_POINT('Ctrl Pts',(176.814640580222,-2.67968869865466,339.124130398133));
#47999=CARTESIAN_POINT('Ctrl Pts',(176.806888606698,-2.56481139973323,339.198772897262));
#48000=CARTESIAN_POINT('Ctrl Pts',(176.799136633173,-2.44672365204024,339.268669963769));
#48001=CARTESIAN_POINT('Ctrl Pts',(176.791384659649,-2.32585729783566,339.333540226259));
#48002=CARTESIAN_POINT('Ctrl Pts',(176.78363596909,-2.20504213060369,339.398383016155));
#48003=CARTESIAN_POINT('Ctrl Pts',(176.775887278532,-2.08145104100421,339.458203051714));
#48004=CARTESIAN_POINT('Ctrl Pts',(176.768138587973,-1.95554251917341,339.512763733922));
#48005=CARTESIAN_POINT('Ctrl Pts',(176.760391509594,-1.82966019366203,339.567313064325));
#48006=CARTESIAN_POINT('Ctrl Pts',(176.752644431215,-1.70146175339532,339.616605062603));
#48007=CARTESIAN_POINT('Ctrl Pts',(176.744897352836,-1.57142745803403,339.660450493958));
#48008=CARTESIAN_POINT('Ctrl Pts',(176.737150209529,-1.44139207285996,339.70429629278));
#48009=CARTESIAN_POINT('Ctrl Pts',(176.729403066222,-1.30952117228818,339.742695308744));
#48010=CARTESIAN_POINT('Ctrl Pts',(176.721655922915,-1.1763116545147,339.775507716877));
#48011=CARTESIAN_POINT('Ctrl Pts',(176.713907037885,-1.04307218841358,339.808327501936));
#48012=CARTESIAN_POINT('Ctrl Pts',(176.706158152856,-0.908493885710526,
339.835558086421));
#48013=CARTESIAN_POINT('Ctrl Pts',(176.698409267827,-0.773084959967538,
339.857110530673));
#48014=CARTESIAN_POINT('Ctrl Pts',(176.690652158051,-0.637532309791568,
339.878685850912));
#48015=CARTESIAN_POINT('Ctrl Pts',(176.682895048275,-0.501147662058251,
339.894570930208));
#48016=CARTESIAN_POINT('Ctrl Pts',(176.675137938499,-0.364446051565146,
339.90472854886));
#48017=CARTESIAN_POINT('Ctrl Pts',(176.667376683572,-0.227671392102332,
339.914891595417));
#48018=CARTESIAN_POINT('Ctrl Pts',(176.659615428644,-0.0905798228575022,
339.919321070248));
#48019=CARTESIAN_POINT('Ctrl Pts',(176.651854173717,0.0463134645227931,
339.918031936202));
#48020=CARTESIAN_POINT('Ctrl Pts',(176.644080503311,0.183425736549433,339.916740739962));
#48021=CARTESIAN_POINT('Ctrl Pts',(176.636306832905,0.320338702313612,339.909712674659));
#48022=CARTESIAN_POINT('Ctrl Pts',(176.628533162499,0.456541240209833,339.897014719039));
#48023=CARTESIAN_POINT('Ctrl Pts',(176.621121358335,0.586403516950871,339.884907856332));
#48024=CARTESIAN_POINT('Ctrl Pts',(176.613709554171,0.715619732940218,339.867647128908));
#48025=CARTESIAN_POINT('Ctrl Pts',(176.606297750007,0.843757212542922,339.845333510583));
#48026=CARTESIAN_POINT('Ctrl Pts',(176.598522671229,0.978175091951562,339.821926235316));
#48027=CARTESIAN_POINT('Ctrl Pts',(176.590747592451,1.11183060239176,339.792884259309));
#48028=CARTESIAN_POINT('Ctrl Pts',(176.582972513673,1.2442143581582,339.758267929978));
#48029=CARTESIAN_POINT('Ctrl Pts',(176.575207002624,1.37643520728524,339.723694198243));
#48030=CARTESIAN_POINT('Ctrl Pts',(176.567441491576,1.50738704104545,339.683559859752));
#48031=CARTESIAN_POINT('Ctrl Pts',(176.559675980527,1.63656816507568,339.637976682085));
#48032=CARTESIAN_POINT('Ctrl Pts',(176.551918169005,1.76562120564498,339.592438700271));
#48033=CARTESIAN_POINT('Ctrl Pts',(176.544160357483,1.89290666412929,339.541462759868));
#48034=CARTESIAN_POINT('Ctrl Pts',(176.536402545962,2.01793592063853,339.485210996452));
#48035=CARTESIAN_POINT('Ctrl Pts',(176.528650572439,2.14287108866756,339.429001564273));
#48036=CARTESIAN_POINT('Ctrl Pts',(176.520898598916,2.26555307921234,339.367524371346));
#48037=CARTESIAN_POINT('Ctrl Pts',(176.513146625394,2.38551158643912,339.300990296835));
#48038=CARTESIAN_POINT('Ctrl Pts',(176.505397934837,2.50541929116682,339.234484399543));
#48039=CARTESIAN_POINT('Ctrl Pts',(176.497649244279,2.62260546549487,339.162926069337));
#48040=CARTESIAN_POINT('Ctrl Pts',(176.489900553722,2.73662303294255,339.086572823047));
#48041=CARTESIAN_POINT('Ctrl Pts',(176.482153475345,2.85061687808291,339.010235462689));
#48042=CARTESIAN_POINT('Ctrl Pts',(176.474406396967,2.96144310307452,338.929105387943));
#48043=CARTESIAN_POINT('Ctrl Pts',(176.46665931859,3.0686826802779,338.843484053598));
#48044=CARTESIAN_POINT('Ctrl Pts',(176.458912175284,3.17592315625227,338.757862001663));
#48045=CARTESIAN_POINT('Ctrl Pts',(176.451165031979,3.27957661902429,338.667748858932));
#48046=CARTESIAN_POINT('Ctrl Pts',(176.443417888674,3.37925658666645,338.573486810382));
#48047=CARTESIAN_POINT('Ctrl Pts',(176.435669003646,3.47895896448144,338.479203569722));
#48048=CARTESIAN_POINT('Ctrl Pts',(176.427920118618,3.57468578560278,338.380769835663));
#48049=CARTESIAN_POINT('Ctrl Pts',(176.420171233591,3.66608723525464,338.278564845478));
#48050=CARTESIAN_POINT('Ctrl Pts',(176.412414123816,3.75758569934959,338.17625137386));
#48051=CARTESIAN_POINT('Ctrl Pts',(176.404657014042,3.84474936006083,338.070158941868));
#48052=CARTESIAN_POINT('Ctrl Pts',(176.396899904268,3.92726820366388,337.960700511533));
#48053=CARTESIAN_POINT('Ctrl Pts',(176.389138649342,4.00983114269864,337.851183590112));
#48054=CARTESIAN_POINT('Ctrl Pts',(176.381377394416,4.0877440970172,337.738297407841));
#48055=CARTESIAN_POINT('Ctrl Pts',(176.37361613949,4.16074084943798,337.622483297624));
#48056=CARTESIAN_POINT('Ctrl Pts',(176.365842469086,4.233854372873,337.506483922575));
#48057=CARTESIAN_POINT('Ctrl Pts',(176.358068798682,4.30203578467009,337.387547599383));
#48058=CARTESIAN_POINT('Ctrl Pts',(176.350295128277,4.36506481145655,337.266140387153));
#48059=CARTESIAN_POINT('Ctrl Pts',(176.342883324096,4.42515982192092,337.150384709786));
#48060=CARTESIAN_POINT('Ctrl Pts',(176.335471519915,4.48057121702699,337.032383266751));
#48061=CARTESIAN_POINT('Ctrl Pts',(176.328059715733,4.53114976219593,336.912554546948));
#48062=CARTESIAN_POINT('Ctrl Pts',(176.320284636955,4.58420731249719,336.786852664712));
#48063=CARTESIAN_POINT('Ctrl Pts',(176.312509558176,4.63211396114196,336.658742614917));
#48064=CARTESIAN_POINT('Ctrl Pts',(176.304734479398,4.67464479772458,336.528685408319));
#48065=CARTESIAN_POINT('Ctrl Pts',(176.296968968349,4.71712329740518,336.398788245393));
#48066=CARTESIAN_POINT('Ctrl Pts',(176.2892034573,4.75423902720225,336.266949061178));
#48067=CARTESIAN_POINT('Ctrl Pts',(176.281437946251,4.78581447925148,336.13365022502));
#48068=CARTESIAN_POINT('Ctrl Pts',(176.273680134729,4.81735862414818,336.000483555045));
#48069=CARTESIAN_POINT('Ctrl Pts',(176.265922323207,4.84337333356298,335.865860491132));
#48070=CARTESIAN_POINT('Ctrl Pts',(176.258164511685,4.86373053050184,335.730279665035));
#48071=CARTESIAN_POINT('Ctrl Pts',(176.250412538162,4.88407240800433,335.594800867811));
#48072=CARTESIAN_POINT('Ctrl Pts',(176.242660564639,4.89876518948732,335.458366127998));
#48073=CARTESIAN_POINT('Ctrl Pts',(176.234908591116,4.90773169826503,335.321485054621));
#48074=CARTESIAN_POINT('Ctrl Pts',(176.227159900559,4.91669440972094,335.18466195046));
#48075=CARTESIAN_POINT('Ctrl Pts',(176.219411210001,4.91993564628801,335.047393277914));
#48076=CARTESIAN_POINT('Ctrl Pts',(176.211662519444,4.9174300206283,334.910194350269));
#48077=CARTESIAN_POINT('Ctrl Pts',(176.203915441066,4.91492491628493,334.773023968007));
#48078=CARTESIAN_POINT('Ctrl Pts',(176.196168362688,4.90667533514496,334.635923692346));
#48079=CARTESIAN_POINT('Ctrl Pts',(176.18842128431,4.89270801706991,334.499409027049));
#48080=CARTESIAN_POINT('Ctrl Pts',(176.180674141005,4.87874058193527,334.362893217628));
#48081=CARTESIAN_POINT('Ctrl Pts',(176.172926997699,4.8590553540693,334.226963417206));
#48082=CARTESIAN_POINT('Ctrl Pts',(176.165179854393,4.83373093657324,334.092129802607));
#48083=CARTESIAN_POINT('Ctrl Pts',(176.157430969365,4.80840082561055,333.957265874549));
#48084=CARTESIAN_POINT('Ctrl Pts',(176.149682084337,4.77742907435664,333.823499006796));
#48085=CARTESIAN_POINT('Ctrl Pts',(176.141933199309,4.74094528667819,333.691328593105));
#48086=CARTESIAN_POINT('Ctrl Pts',(176.134176089535,4.70442277473052,333.559017892372));
#48087=CARTESIAN_POINT('Ctrl Pts',(176.12641897976,4.66237664354093,333.428307407988));
#48088=CARTESIAN_POINT('Ctrl Pts',(176.118661869985,4.61498639547701,333.299681314558));
#48089=CARTESIAN_POINT('Ctrl Pts',(176.110900615059,4.56757082357981,333.170986487457));
#48090=CARTESIAN_POINT('Ctrl Pts',(176.103139360133,4.51480559480765,333.044378631334));
#48091=CARTESIAN_POINT('Ctrl Pts',(176.095378105207,4.45691777002193,332.920320444452));
#48092=CARTESIAN_POINT('Ctrl Pts',(176.087604434803,4.39893734358217,332.796063804903));
#48093=CARTESIAN_POINT('Ctrl Pts',(176.079830764398,4.33581812618019,332.674365332089));
#48094=CARTESIAN_POINT('Ctrl Pts',(176.072057093994,4.26783283429882,332.555662469915));
#48095=CARTESIAN_POINT('Ctrl Pts',(176.064645289815,4.20301227409989,332.442485254514));
#48096=CARTESIAN_POINT('Ctrl Pts',(176.057233485637,4.13376862862668,332.332031278521));
#48097=CARTESIAN_POINT('Ctrl Pts',(176.049821681459,4.06037305472955,332.224652504834));
#48098=CARTESIAN_POINT('Ctrl Pts',(176.04204660268,3.98338014513169,332.112010777597));
#48099=CARTESIAN_POINT('Ctrl Pts',(176.034271523902,3.90157470761217,332.002397355807));
#48100=CARTESIAN_POINT('Ctrl Pts',(176.026496445123,3.81522270402468,331.896250850794));
#48101=CARTESIAN_POINT('Ctrl Pts',(176.018730934074,3.72897696207507,331.790234965814));
#48102=CARTESIAN_POINT('Ctrl Pts',(176.010965423025,3.63819603049299,331.687677809286));
#48103=CARTESIAN_POINT('Ctrl Pts',(176.003199911976,3.54318948426011,331.588989689091));
#48104=CARTESIAN_POINT('Ctrl Pts',(175.995442100453,3.44827713729456,331.490399418455));
#48105=CARTESIAN_POINT('Ctrl Pts',(175.987684288931,3.34914778277772,331.395670829754));
#48106=CARTESIAN_POINT('Ctrl Pts',(175.979926477409,3.24615142097872,331.305181463918));
#48107=CARTESIAN_POINT('Ctrl Pts',(175.972174503885,3.14323256720816,331.214760194199));
#48108=CARTESIAN_POINT('Ctrl Pts',(175.964422530362,3.03645279091959,331.128572054455));
#48109=CARTESIAN_POINT('Ctrl Pts',(175.956670556839,2.92619886848063,331.046957722892));
#48110=CARTESIAN_POINT('Ctrl Pts',(175.948921866281,2.815991638643,330.965377955047));
#48111=CARTESIAN_POINT('Ctrl Pts',(175.941173175723,2.70231350248418,330.888368374878));
#48112=CARTESIAN_POINT('Ctrl Pts',(175.933424485166,2.58558405939438,330.816229196729));
#48113=CARTESIAN_POINT('Ctrl Pts',(175.925677406788,2.46887890284024,330.744105027737));
#48114=CARTESIAN_POINT('Ctrl Pts',(175.91793032841,2.34912403440981,330.676849450542));
#48115=CARTESIAN_POINT('Ctrl Pts',(175.910183250032,2.22676742268942,330.61471894769));
#48116=CARTESIAN_POINT('Ctrl Pts',(175.902436106726,2.10440978550293,330.552587924124));
#48117=CARTESIAN_POINT('Ctrl Pts',(175.89468896342,1.97945071005153,330.495582237544));
#48118=CARTESIAN_POINT('Ctrl Pts',(175.886941820114,1.85236175155943,330.44391187488));
#48119=CARTESIAN_POINT('Ctrl Pts',(175.879192935085,1.72524422077117,330.392229895621));
#48120=CARTESIAN_POINT('Ctrl Pts',(175.871444050057,1.59599621611924,330.345885774323));
#48121=CARTESIAN_POINT('Ctrl Pts',(175.863695165029,1.46510782455742,330.305040774946));
#48122=CARTESIAN_POINT('Ctrl Pts',(175.855938055254,1.33408050670447,330.264152422265));
#48123=CARTESIAN_POINT('Ctrl Pts',(175.848180945479,1.20140969760162,330.228774967733));
#48124=CARTESIAN_POINT('Ctrl Pts',(175.840423835704,1.0675996890353,330.199019478641));
#48125=CARTESIAN_POINT('Ctrl Pts',(175.832662580778,0.933718176678549,330.169248089166));
#48126=CARTESIAN_POINT('Ctrl Pts',(175.824901325852,0.798696636441872,330.145104720035));
#48127=CARTESIAN_POINT('Ctrl Pts',(175.817140070925,0.663047036828604,330.126648823504));
#48128=CARTESIAN_POINT('Ctrl Pts',(175.80936640052,0.527180442064314,330.108163403554));
#48129=CARTESIAN_POINT('Ctrl Pts',(175.801592730116,0.390684169631619,330.095383673364));
#48130=CARTESIAN_POINT('Ctrl Pts',(175.793819059711,0.254073657977923,330.088317025823));
#48131=CARTESIAN_POINT('Ctrl Pts',(175.786407255535,0.123822398544541,330.081579332426));
#48132=CARTESIAN_POINT('Ctrl Pts',(175.77899545136,-0.0065324160113929,
330.080034806898));
#48133=CARTESIAN_POINT('Ctrl Pts',(175.771583647185,-0.136548074050385,
330.083645894977));
#48134=CARTESIAN_POINT('Ctrl Pts',(175.763808568407,-0.272936186820303,
330.087433973241));
#48135=CARTESIAN_POINT('Ctrl Pts',(175.756033489628,-0.409382067935774,
330.096907798746));
#48136=CARTESIAN_POINT('Ctrl Pts',(175.74825841085,-0.545372952551393,330.112081076253));
#48137=CARTESIAN_POINT('Ctrl Pts',(175.740492899801,-0.681196491726141,
330.127235682076));
#48138=CARTESIAN_POINT('Ctrl Pts',(175.732727388752,-0.816565763695584,
330.148075742043));
#48139=CARTESIAN_POINT('Ctrl Pts',(175.724961877703,-0.950968203023476,
330.174562969084));
#48140=CARTESIAN_POINT('Ctrl Pts',(175.717204066181,-1.08523738194049,330.201023933962));
#48141=CARTESIAN_POINT('Ctrl Pts',(175.709446254659,-1.2185412548911,330.233120848133));
#48142=CARTESIAN_POINT('Ctrl Pts',(175.701688443137,-1.35037293442409,330.270763697966));
#48143=CARTESIAN_POINT('Ctrl Pts',(175.693936469614,-1.48210540643809,330.308378220361));
#48144=CARTESIAN_POINT('Ctrl Pts',(175.686184496091,-1.61236751586079,330.351530264396));
#48145=CARTESIAN_POINT('Ctrl Pts',(175.678432522568,-1.74066347223494,330.400078942098));
#48146=CARTESIAN_POINT('Ctrl Pts',(175.670683832011,-1.86890509519553,330.448607059407));
#48147=CARTESIAN_POINT('Ctrl Pts',(175.662935141453,-1.99518185640903,330.502527126678));
#48148=CARTESIAN_POINT('Ctrl Pts',(175.655186450896,-2.11901422992423,330.561648757041));
#48149=CARTESIAN_POINT('Ctrl Pts',(175.647439372518,-2.24282083908013,330.620758086654));
#48150=CARTESIAN_POINT('Ctrl Pts',(175.63969229414,-2.36418371961667,330.685066658427));
#48151=CARTESIAN_POINT('Ctrl Pts',(175.631945215762,-2.48264476838242,330.754336563442));
#48152=CARTESIAN_POINT('Ctrl Pts',(175.624198072457,-2.60110680996515,330.823607049005));
#48153=CARTESIAN_POINT('Ctrl Pts',(175.616450929151,-2.71666663384779,330.897838753439));
#48154=CARTESIAN_POINT('Ctrl Pts',(175.608703785845,-2.8288924719523,330.976748771872));
#48155=CARTESIAN_POINT('Ctrl Pts',(175.600954900817,-2.94114354080819,331.055676530953));
#48156=CARTESIAN_POINT('Ctrl Pts',(175.593206015789,-3.05005881268118,331.139284472186));
#48157=CARTESIAN_POINT('Ctrl Pts',(175.585457130761,-3.15523746309426,331.227247740179));
#48158=CARTESIAN_POINT('Ctrl Pts',(175.577700020986,-3.26052775121363,331.315304373293));
#48159=CARTESIAN_POINT('Ctrl Pts',(175.569942911212,-3.3620731949287,331.407725316465));
#48160=CARTESIAN_POINT('Ctrl Pts',(175.562185801437,-3.45950749416334,331.504146604858));
#48161=CARTESIAN_POINT('Ctrl Pts',(175.554424546511,-3.55699385917205,331.600619417704));
#48162=CARTESIAN_POINT('Ctrl Pts',(175.546663291585,-3.65036443630706,331.701096549058));
#48163=CARTESIAN_POINT('Ctrl Pts',(175.538902036659,-3.73929217536197,331.805179646713));
#48164=CARTESIAN_POINT('Ctrl Pts',(175.531128366254,-3.828362169818,331.909429243404));
#48165=CARTESIAN_POINT('Ctrl Pts',(175.52335469585,-3.91297488274637,332.017296025601));
#48166=CARTESIAN_POINT('Ctrl Pts',(175.515581025445,-3.99284516399051,332.128350550834));
#48167=CARTESIAN_POINT('Ctrl Pts',(175.508169221267,-4.06899746443525,332.23423546121));
#48168=CARTESIAN_POINT('Ctrl Pts',(175.500757417089,-4.14083875884401,332.343017774418));
#48169=CARTESIAN_POINT('Ctrl Pts',(175.493345612912,-4.20816105072475,332.454304882029));
#48170=CARTESIAN_POINT('Ctrl Pts',(175.485316210545,-4.28109305982305,332.574865132104));
#48171=CARTESIAN_POINT('Ctrl Pts',(175.477286808179,-4.34893939756361,332.698725310259));
#48172=CARTESIAN_POINT('Ctrl Pts',(175.469257405813,-4.41139899220035,332.825432918001));
#48173=CARTESIAN_POINT('Ctrl Pts',(175.461240024851,-4.47376507401649,332.951950822529));
#48174=CARTESIAN_POINT('Ctrl Pts',(175.453222643889,-4.53076031911879,333.081307349566));
#48175=CARTESIAN_POINT('Ctrl Pts',(175.445205262928,-4.58212772700723,333.213022508286));
#48176=CARTESIAN_POINT('Ctrl Pts',(175.437198648785,-4.63342615182149,333.34456078215));
#48177=CARTESIAN_POINT('Ctrl Pts',(175.429192034643,-4.67911166530576,333.478451048872));
#48178=CARTESIAN_POINT('Ctrl Pts',(175.4211854205,-4.71897386982171,333.6141902445));
#48179=CARTESIAN_POINT('Ctrl Pts',(175.413191135583,-4.75877469132224,333.749720418041));
#48180=CARTESIAN_POINT('Ctrl Pts',(175.405196850666,-4.79276998154569,333.887093504415));
#48181=CARTESIAN_POINT('Ctrl Pts',(175.397202565749,-4.82079818617205,334.025788569816));
#48182=CARTESIAN_POINT('Ctrl Pts',(175.389215601938,-4.84880072277973,334.164356619322));
#48183=CARTESIAN_POINT('Ctrl Pts',(175.381228638128,-4.87084698663245,334.304243889378));
#48184=CARTESIAN_POINT('Ctrl Pts',(175.373241674317,-4.88682560210799,334.444915684709));
#48185=CARTESIAN_POINT('Ctrl Pts',(175.365262388803,-4.90278885648177,334.585452244684));
#48186=CARTESIAN_POINT('Ctrl Pts',(175.35728310329,-4.91269604999984,334.726771473829));
#48187=CARTESIAN_POINT('Ctrl Pts',(175.349303817776,-4.91648717332359,334.868330196914));
#48188=CARTESIAN_POINT('Ctrl Pts',(175.346808337353,-4.91767282760537,334.91260195803));
#48189=CARTESIAN_POINT('Ctrl Pts',(175.344312856931,-4.91826065279927,334.956897091092));
#48190=CARTESIAN_POINT('Ctrl Pts',(175.341817376508,-4.9182498538837,335.001198863214));
#48191=CARTESIAN_POINT('',(173.591817376561,-4.918248352634,335.004025458105));
#48192=CARTESIAN_POINT('Ctrl Pts',(175.341817376454,-4.91824985388346,335.001198864178));
#48193=CARTESIAN_POINT('Ctrl Pts',(175.333534918477,-4.91821401243364,335.1482357083));
#48194=CARTESIAN_POINT('Ctrl Pts',(175.325252460499,-4.91158018368582,335.295096105342));
#48195=CARTESIAN_POINT('Ctrl Pts',(175.316970002522,-4.89842102387199,335.441196708271));
#48196=CARTESIAN_POINT('Ctrl Pts',(175.308481467198,-4.88493444860438,335.59093246693));
#48197=CARTESIAN_POINT('Ctrl Pts',(175.299992931875,-4.86459368168669,335.739869785143));
#48198=CARTESIAN_POINT('Ctrl Pts',(175.291504396551,-4.83753179226554,335.887394625474));
#48199=CARTESIAN_POINT('Ctrl Pts',(175.283178484465,-4.81098835413402,336.032093187028));
#48200=CARTESIAN_POINT('Ctrl Pts',(175.27485257238,-4.77797915311206,336.175432643527));
#48201=CARTESIAN_POINT('Ctrl Pts',(175.266526660294,-4.7386797945413,336.316851118125));
#48202=CARTESIAN_POINT('Ctrl Pts',(175.257956813351,-4.69822903257857,336.462412909999));
#48203=CARTESIAN_POINT('Ctrl Pts',(175.249386966408,-4.65111405515187,336.605939105334));
#48204=CARTESIAN_POINT('Ctrl Pts',(175.240817119466,-4.59757875988788,336.746840750935));
#48205=CARTESIAN_POINT('Ctrl Pts',(175.232247272523,-4.54404346462389,336.887742396536));
#48206=CARTESIAN_POINT('Ctrl Pts',(175.22367742558,-4.48408805384567,337.026019210004));
#48207=CARTESIAN_POINT('Ctrl Pts',(175.215107578637,-4.41800674350231,337.161110704445));
#48208=CARTESIAN_POINT('Ctrl Pts',(175.207332499859,-4.35805381818948,337.283673804882));
#48209=CARTESIAN_POINT('Ctrl Pts',(175.19955742108,-4.29290212467153,337.403933892506));
#48210=CARTESIAN_POINT('Ctrl Pts',(175.191782342302,-4.22275162680702,337.521418600867));
#48211=CARTESIAN_POINT('Ctrl Pts',(175.184016831253,-4.15268745359612,337.638758736815));
#48212=CARTESIAN_POINT('Ctrl Pts',(175.176251320204,-4.07763691392763,337.753329956538));
#48213=CARTESIAN_POINT('Ctrl Pts',(175.168485809155,-3.99784720897207,337.864681615156));
#48214=CARTESIAN_POINT('Ctrl Pts',(175.160727997633,-3.91813661574133,337.975922868281));
#48215=CARTESIAN_POINT('Ctrl Pts',(175.15297018611,-3.83369643449449,338.083950597289));
#48216=CARTESIAN_POINT('Ctrl Pts',(175.145212374588,-3.74481859252371,338.18834075525));
#48217=CARTESIAN_POINT('Ctrl Pts',(175.137460401065,-3.65600763394762,338.292652356307));
#48218=CARTESIAN_POINT('Ctrl Pts',(175.129708427542,-3.56276591409088,338.393331538536));
#48219=CARTESIAN_POINT('Ctrl Pts',(175.121956454019,-3.46542706564282,338.489985431948));
#48220=CARTESIAN_POINT('Ctrl Pts',(175.114207763461,-3.36812944025466,338.58659839238));
#48221=CARTESIAN_POINT('Ctrl Pts',(175.106459072904,-3.26673841412597,338.679189179708));
#48222=CARTESIAN_POINT('Ctrl Pts',(175.098710382346,-3.16162593260944,338.767400234213));
#48223=CARTESIAN_POINT('Ctrl Pts',(175.090963303968,-3.05653532062261,338.855592935672));
#48224=CARTESIAN_POINT('Ctrl Pts',(175.08321622559,-2.94772509256875,338.939407465718));
#48225=CARTESIAN_POINT('Ctrl Pts',(175.075469147212,-2.83560157018039,339.018525450671));
#48226=CARTESIAN_POINT('Ctrl Pts',(175.067722003907,-2.72347710808881,339.097644098709));
#48227=CARTESIAN_POINT('Ctrl Pts',(175.059974860601,-2.60803961564551,339.172065897786));
#48228=CARTESIAN_POINT('Ctrl Pts',(175.052227717295,-2.48972545671888,339.241515084574));
#48229=CARTESIAN_POINT('Ctrl Pts',(175.044478832267,-2.37138469825763,339.310979885013));
#48230=CARTESIAN_POINT('Ctrl Pts',(175.036729947239,-2.25016632340666,339.375469650738));
#48231=CARTESIAN_POINT('Ctrl Pts',(175.028981062211,-2.12653205709415,339.434754161467));
#48232=CARTESIAN_POINT('Ctrl Pts',(175.021223952436,-2.00276656409396,339.494101597389));
#48233=CARTESIAN_POINT('Ctrl Pts',(175.013466842661,-1.87658041030347,339.548232572515));
#48234=CARTESIAN_POINT('Ctrl Pts',(175.005709732886,-1.74845661241411,339.596964491597));
#48235=CARTESIAN_POINT('Ctrl Pts',(174.99794847796,-1.62026434926375,339.645722451459));
#48236=CARTESIAN_POINT('Ctrl Pts',(174.990187223034,-1.49013274950522,339.689075483008));
#48237=CARTESIAN_POINT('Ctrl Pts',(174.982425968108,-1.35855986608731,339.726890960532));
#48238=CARTESIAN_POINT('Ctrl Pts',(174.974652297703,-1.22677650893543,339.764766930496));
#48239=CARTESIAN_POINT('Ctrl Pts',(174.966878627298,-1.09354764094046,339.797087552765));
#48240=CARTESIAN_POINT('Ctrl Pts',(174.959104956894,-0.959382252510918,
339.823771217219));
#48241=CARTESIAN_POINT('Ctrl Pts',(174.951693152717,-0.831462295196669,
339.849212750671));
#48242=CARTESIAN_POINT('Ctrl Pts',(174.94428134854,-0.702691329622126,339.869530271913));
#48243=CARTESIAN_POINT('Ctrl Pts',(174.936869544363,-0.573512857440891,
339.884697131333));
#48244=CARTESIAN_POINT('Ctrl Pts',(174.929094465585,-0.438002963530012,
339.900607363713));
#48245=CARTESIAN_POINT('Ctrl Pts',(174.921319386806,-0.301616370445505,
339.910899548619));
#48246=CARTESIAN_POINT('Ctrl Pts',(174.913544308028,-0.164858513129928,
339.915486215335));
#48247=CARTESIAN_POINT('Ctrl Pts',(174.905778796979,-0.0282689450642106,
339.920067237865));
#48248=CARTESIAN_POINT('Ctrl Pts',(174.89801328593,0.108690591283536,339.918956699013));
#48249=CARTESIAN_POINT('Ctrl Pts',(174.890247774881,0.245507364282319,339.912118605712));
#48250=CARTESIAN_POINT('Ctrl Pts',(174.882489963359,0.382188483052412,339.905287292401));
#48251=CARTESIAN_POINT('Ctrl Pts',(174.874732151837,0.518726732294366,339.892739745334));
#48252=CARTESIAN_POINT('Ctrl Pts',(174.866974340314,0.654607543290001,339.874491976275));
#48253=CARTESIAN_POINT('Ctrl Pts',(174.859222366791,0.790386099666195,339.85625793924));
#48254=CARTESIAN_POINT('Ctrl Pts',(174.851470393268,0.925507816721279,339.832332270262));
#48255=CARTESIAN_POINT('Ctrl Pts',(174.843718419745,1.05946177390906,339.802782923694));
#48256=CARTESIAN_POINT('Ctrl Pts',(174.835969729188,1.19335900151648,339.773246091291));
#48257=CARTESIAN_POINT('Ctrl Pts',(174.82822103863,1.32608907197248,339.738090402219));
#48258=CARTESIAN_POINT('Ctrl Pts',(174.820472348073,1.45715002470735,339.697435137178));
#48259=CARTESIAN_POINT('Ctrl Pts',(174.812725269695,1.58818370911642,339.656788330804));
#48260=CARTESIAN_POINT('Ctrl Pts',(174.804978191317,1.71754859346586,339.610644340155));
#48261=CARTESIAN_POINT('Ctrl Pts',(174.797231112939,1.84475706653118,339.559172559575));
#48262=CARTESIAN_POINT('Ctrl Pts',(174.789483969634,1.97196660572588,339.507700347613));
#48263=CARTESIAN_POINT('Ctrl Pts',(174.781736826328,2.09701933525203,339.45090040327));
#48264=CARTESIAN_POINT('Ctrl Pts',(174.773989683022,2.21944721831459,339.388990442871));
#48265=CARTESIAN_POINT('Ctrl Pts',(174.766240797994,2.34190262576438,339.327066563799));
#48266=CARTESIAN_POINT('Ctrl Pts',(174.758491912966,2.4617316637317,339.260030558963));
#48267=CARTESIAN_POINT('Ctrl Pts',(174.750743027938,2.57849086921786,339.188146117301));
#48268=CARTESIAN_POINT('Ctrl Pts',(174.742985918163,2.69537400413122,339.116185376749));
#48269=CARTESIAN_POINT('Ctrl Pts',(174.735228808388,2.80918046432426,339.039366124639));
#48270=CARTESIAN_POINT('Ctrl Pts',(174.727471698614,2.91949531350993,338.957995727245));
#48271=CARTESIAN_POINT('Ctrl Pts',(174.719710443687,3.02986911142376,338.876581848113));
#48272=CARTESIAN_POINT('Ctrl Pts',(174.711949188761,3.13674727612849,338.790612222609));
#48273=CARTESIAN_POINT('Ctrl Pts',(174.704187933835,3.2397487548041,338.700433902699));
#48274=CARTESIAN_POINT('Ctrl Pts',(174.696414263431,3.34291500227752,338.610111326867));
#48275=CARTESIAN_POINT('Ctrl Pts',(174.688640593026,3.44219188821686,338.515566872724));
#48276=CARTESIAN_POINT('Ctrl Pts',(174.680866922621,3.53723534101436,338.417184397246));
#48277=CARTESIAN_POINT('Ctrl Pts',(174.673455118444,3.6278544982194,338.323381649669));
#48278=CARTESIAN_POINT('Ctrl Pts',(174.666043314267,3.71462529364057,338.226090374067));
#48279=CARTESIAN_POINT('Ctrl Pts',(174.65863151009,3.79728531285856,338.125669098809));
#48280=CARTESIAN_POINT('Ctrl Pts',(174.650856431311,3.88399674584863,338.020325877712));
#48281=CARTESIAN_POINT('Ctrl Pts',(174.643081352533,3.96645827508929,337.911205173725));
#48282=CARTESIAN_POINT('Ctrl Pts',(174.635306273754,4.04432282474056,337.79868468245));
#48283=CARTESIAN_POINT('Ctrl Pts',(174.627540762705,4.12209155710639,337.686302654803));
#48284=CARTESIAN_POINT('Ctrl Pts',(174.619775251656,4.19527434514702,337.570529482489));
#48285=CARTESIAN_POINT('Ctrl Pts',(174.612009740607,4.26356345302084,337.451776854562));
#48286=CARTESIAN_POINT('Ctrl Pts',(174.604251929085,4.33178485204538,337.333141970211));
#48287=CARTESIAN_POINT('Ctrl Pts',(174.596494117563,4.39512203325476,337.211533845812));
#48288=CARTESIAN_POINT('Ctrl Pts',(174.588736306041,4.45330999862246,337.087393858061));
#48289=CARTESIAN_POINT('Ctrl Pts',(174.580984332518,4.51145417570094,336.963347289587));
#48290=CARTESIAN_POINT('Ctrl Pts',(174.573232358995,4.5644566846066,336.836773002681));
#48291=CARTESIAN_POINT('Ctrl Pts',(174.565480385472,4.61209818118046,336.70813741533));
#48292=CARTESIAN_POINT('Ctrl Pts',(174.557731694914,4.65971950155225,336.579556305227));
#48293=CARTESIAN_POINT('Ctrl Pts',(174.549983004356,4.70198418977133,336.448915996719));
#48294=CARTESIAN_POINT('Ctrl Pts',(174.542234313799,4.73872091185687,336.316703148789));
#48295=CARTESIAN_POINT('Ctrl Pts',(174.534487235421,4.77544999056055,336.184517808846));
#48296=CARTESIAN_POINT('Ctrl Pts',(174.526740157043,4.80665328626123,336.050760956636));
#48297=CARTESIAN_POINT('Ctrl Pts',(174.518993078665,4.83220937186604,335.91593430384));
#48298=CARTESIAN_POINT('Ctrl Pts',(174.511245935359,4.85776567165545,335.781106521066));
#48299=CARTESIAN_POINT('Ctrl Pts',(174.503498792054,4.87767459415442,335.645209303861));
#48300=CARTESIAN_POINT('Ctrl Pts',(174.495751648748,4.89186594009986,335.508754053144));
#48301=CARTESIAN_POINT('Ctrl Pts',(174.48800276372,4.90606047656115,335.372268124391));
#48302=CARTESIAN_POINT('Ctrl Pts',(174.480253878692,4.91453483817671,335.235224301182));
#48303=CARTESIAN_POINT('Ctrl Pts',(174.472504993664,4.91727078332571,335.098138198228));
#48304=CARTESIAN_POINT('Ctrl Pts',(174.464747883889,4.92000963243516,334.960906590668));
#48305=CARTESIAN_POINT('Ctrl Pts',(174.456990774114,4.91699789029285,334.823633005133));
#48306=CARTESIAN_POINT('Ctrl Pts',(174.449233664339,4.9082694819223,334.686832703926));
#48307=CARTESIAN_POINT('Ctrl Pts',(174.441472409413,4.8995364093694,334.549959301013));
#48308=CARTESIAN_POINT('Ctrl Pts',(174.433711154487,4.88508062479064,334.41356007487));
#48309=CARTESIAN_POINT('Ctrl Pts',(174.425949899561,4.86498776204339,334.278143270678));
#48310=CARTESIAN_POINT('Ctrl Pts',(174.418176229156,4.84486275726399,334.142509843731));
#48311=CARTESIAN_POINT('Ctrl Pts',(174.410402558751,4.81908272824628,334.007862363268));
#48312=CARTESIAN_POINT('Ctrl Pts',(174.402628888347,4.78778427161921,333.874697893481));
#48313=CARTESIAN_POINT('Ctrl Pts',(174.39521708417,4.7579427656778,333.747732261799));
#48314=CARTESIAN_POINT('Ctrl Pts',(174.387805279993,4.72308511271564,333.622114956956));
#48315=CARTESIAN_POINT('Ctrl Pts',(174.380393475815,4.68337079938713,333.498260669108));
#48316=CARTESIAN_POINT('Ctrl Pts',(174.372618397037,4.64170996925989,333.368335913671));
#48317=CARTESIAN_POINT('Ctrl Pts',(174.364843318258,4.59457270640252,333.239940780221));
#48318=CARTESIAN_POINT('Ctrl Pts',(174.35706823948,4.54208880045317,333.113571524998));
#48319=CARTESIAN_POINT('Ctrl Pts',(174.349302728431,4.48966947929138,332.987357775189));
#48320=CARTESIAN_POINT('Ctrl Pts',(174.341537217382,4.43191675461598,332.863165300837));
#48321=CARTESIAN_POINT('Ctrl Pts',(174.333771706333,4.36901029101437,332.741475672146));
#48322=CARTESIAN_POINT('Ctrl Pts',(174.326013894811,4.30616619935458,332.619906699075));
#48323=CARTESIAN_POINT('Ctrl Pts',(174.318256083289,4.23817871619064,332.500835978172));
#48324=CARTESIAN_POINT('Ctrl Pts',(174.310498271766,4.16527559896525,332.384725206185));
#48325=CARTESIAN_POINT('Ctrl Pts',(174.302746298243,4.0924273436475,332.268701811236));
#48326=CARTESIAN_POINT('Ctrl Pts',(174.29499432472,4.0146710242965,332.155634261263));
#48327=CARTESIAN_POINT('Ctrl Pts',(174.287242351197,3.93228016203768,332.045959412983));
#48328=CARTESIAN_POINT('Ctrl Pts',(174.27949366064,3.84992419235792,331.936331012066));
#48329=CARTESIAN_POINT('Ctrl Pts',(174.271744970082,3.76293781778694,331.830092766992));
#48330=CARTESIAN_POINT('Ctrl Pts',(174.263996279525,3.67163756159811,331.72765211526));
#48331=CARTESIAN_POINT('Ctrl Pts',(174.256249201147,3.58035630119013,331.625232777161));
#48332=CARTESIAN_POINT('Ctrl Pts',(174.248502122769,3.4847632043372,331.526609752416));
#48333=CARTESIAN_POINT('Ctrl Pts',(174.240755044391,3.38521445992893,331.432156656636));
#48334=CARTESIAN_POINT('Ctrl Pts',(174.233007901085,3.28566488120637,331.337702769248));
#48335=CARTESIAN_POINT('Ctrl Pts',(174.225260757779,3.18215987235577,331.24741914957));
#48336=CARTESIAN_POINT('Ctrl Pts',(174.217513614474,3.07509149247358,331.161641578042));
#48337=CARTESIAN_POINT('Ctrl Pts',(174.209764729446,2.96799904134648,331.075844721895));
#48338=CARTESIAN_POINT('Ctrl Pts',(174.202015844417,2.85734193003668,330.994556174108));
#48339=CARTESIAN_POINT('Ctrl Pts',(174.194266959389,2.74354387836738,330.918070303157));
#48340=CARTESIAN_POINT('Ctrl Pts',(174.186509849615,2.62962504027024,330.841503249311));
#48341=CARTESIAN_POINT('Ctrl Pts',(174.17875273984,2.51255892710305,330.769749273641));
#48342=CARTESIAN_POINT('Ctrl Pts',(174.170995630065,2.39279719270655,330.70305868587));
#48343=CARTESIAN_POINT('Ctrl Pts',(174.163234375139,2.27297146146842,330.636332460781));
#48344=CARTESIAN_POINT('Ctrl Pts',(174.155473120213,2.15044758774672,330.574675190583));
#48345=CARTESIAN_POINT('Ctrl Pts',(174.147711865287,2.02569930714924,330.518289904566));
#48346=CARTESIAN_POINT('Ctrl Pts',(174.139938194882,1.90075146995822,330.461814420468));
#48347=CARTESIAN_POINT('Ctrl Pts',(174.132164524477,1.77357247810012,330.410627919113));
#48348=CARTESIAN_POINT('Ctrl Pts',(174.124390854073,1.6446542437304,330.364884523436));
#48349=CARTESIAN_POINT('Ctrl Pts',(174.116979049896,1.52173718418788,330.321270493834));
#48350=CARTESIAN_POINT('Ctrl Pts',(174.109567245719,1.39723943647048,330.282604306296));
#48351=CARTESIAN_POINT('Ctrl Pts',(174.102155441542,1.27159602975758,330.248976257731));
#48352=CARTESIAN_POINT('Ctrl Pts',(174.094380362763,1.13979446540783,330.213699998332));
#48353=CARTESIAN_POINT('Ctrl Pts',(174.086605283985,1.00631558083169,330.183856754277));
#48354=CARTESIAN_POINT('Ctrl Pts',(174.078830205206,0.871646925110187,330.159605935417));
#48355=CARTESIAN_POINT('Ctrl Pts',(174.071064694157,0.737143987743028,330.135384958735));
#48356=CARTESIAN_POINT('Ctrl Pts',(174.063299183108,0.601454573357376,330.11674278298));
#48357=CARTESIAN_POINT('Ctrl Pts',(174.055533672059,0.465080871429679,330.103788929639));
#48358=CARTESIAN_POINT('Ctrl Pts',(174.047775860537,0.328842384424646,330.090847920081));
#48359=CARTESIAN_POINT('Ctrl Pts',(174.040018049015,0.191921346693514,330.083584045765));
#48360=CARTESIAN_POINT('Ctrl Pts',(174.032260237493,0.0548292615047352,
330.082055631203));
#48361=CARTESIAN_POINT('Ctrl Pts',(174.02450826397,-0.0821596575426619,
330.080528366821));
#48362=CARTESIAN_POINT('Ctrl Pts',(174.016756290447,-0.219318978563306,
330.084727975516));
#48363=CARTESIAN_POINT('Ctrl Pts',(174.009004316924,-0.356133321447015,
330.094660855776));
#48364=CARTESIAN_POINT('Ctrl Pts',(174.001255626366,-0.492889723375285,
330.104589529455));
#48365=CARTESIAN_POINT('Ctrl Pts',(173.993506935808,-0.629301048709266,
330.120246617246));
#48366=CARTESIAN_POINT('Ctrl Pts',(173.985758245251,-0.764853385657481,
330.141586435785));
#48367=CARTESIAN_POINT('Ctrl Pts',(173.978011166873,-0.900377519809782,
330.162921814397));
#48368=CARTESIAN_POINT('Ctrl Pts',(173.970264088495,-1.03504263518604,330.189937511252));
#48369=CARTESIAN_POINT('Ctrl Pts',(173.962517010117,-1.16834179620082,330.22253618436));
#48370=CARTESIAN_POINT('Ctrl Pts',(173.954769866811,-1.30164207439094,330.255135130676));
#48371=CARTESIAN_POINT('Ctrl Pts',(173.947022723505,-1.43357599570025,330.29331705372));
#48372=CARTESIAN_POINT('Ctrl Pts',(173.9392755802,-1.56364902951877,330.336933972697));
#48373=CARTESIAN_POINT('Ctrl Pts',(173.931526695172,-1.69375130651686,330.380560697684));
#48374=CARTESIAN_POINT('Ctrl Pts',(173.923777810143,-1.82199149299923,330.429624725807));
#48375=CARTESIAN_POINT('Ctrl Pts',(173.916028925115,-1.94789274912631,330.4839290417));
#48376=CARTESIAN_POINT('Ctrl Pts',(173.908271815341,-2.07392763814745,330.538290996755));
#48377=CARTESIAN_POINT('Ctrl Pts',(173.900514705566,-2.19761827817883,330.597904195336));
#48378=CARTESIAN_POINT('Ctrl Pts',(173.892757595791,-2.31850976262574,330.662524289047));
#48379=CARTESIAN_POINT('Ctrl Pts',(173.884996340865,-2.43946584761647,330.727178913669));
#48380=CARTESIAN_POINT('Ctrl Pts',(173.877235085939,-2.55761946001583,330.796845566216));
#48381=CARTESIAN_POINT('Ctrl Pts',(173.869473831012,-2.67254350264052,330.871235743107));
#48382=CARTESIAN_POINT('Ctrl Pts',(173.861700160608,-2.78765138627982,330.945744920038));
#48383=CARTESIAN_POINT('Ctrl Pts',(173.853926490203,-2.89951905730874,331.024992494573));
#48384=CARTESIAN_POINT('Ctrl Pts',(173.846152819798,-3.00775070856979,331.108648212048));
#48385=CARTESIAN_POINT('Ctrl Pts',(173.838741015621,-3.11094415042489,331.188409735748));
#48386=CARTESIAN_POINT('Ctrl Pts',(173.831329211444,-3.21083224740198,331.272178055105));
#48387=CARTESIAN_POINT('Ctrl Pts',(173.823917407267,-3.30710364765362,331.359636209638));
#48388=CARTESIAN_POINT('Ctrl Pts',(173.816258284257,-3.40658745473968,331.450012688541));
#48389=CARTESIAN_POINT('Ctrl Pts',(173.808599161247,-3.50254359561381,331.544633845094));
#48390=CARTESIAN_POINT('Ctrl Pts',(173.800940038236,-3.59457987923933,331.643189228707));
#48391=CARTESIAN_POINT('Ctrl Pts',(173.793290431619,-3.68650180859247,331.741622158123));
#48392=CARTESIAN_POINT('Ctrl Pts',(173.785640825001,-3.77451329351233,331.843979301775));
#48393=CARTESIAN_POINT('Ctrl Pts',(173.777991218384,-3.85825565553903,331.949910434266));
#48394=CARTESIAN_POINT('Ctrl Pts',(173.770233974975,-3.94317634733348,332.057332112327));
#48395=CARTESIAN_POINT('Ctrl Pts',(173.762476731565,-4.0237065286861,332.168428867022));
#48396=CARTESIAN_POINT('Ctrl Pts',(173.754719488156,-4.09951075861579,332.28279654746));
#48397=CARTESIAN_POINT('Ctrl Pts',(173.747083300453,-4.17413202520065,332.395379462406));
#48398=CARTESIAN_POINT('Ctrl Pts',(173.73944711275,-4.24417353419884,332.511131608632));
#48399=CARTESIAN_POINT('Ctrl Pts',(173.731810925048,-4.30935630741304,332.629634779563));
#48400=CARTESIAN_POINT('Ctrl Pts',(173.724177742638,-4.37451342733966,332.748091312466));
#48401=CARTESIAN_POINT('Ctrl Pts',(173.716544560228,-4.43481541967576,332.869296364216));
#48402=CARTESIAN_POINT('Ctrl Pts',(173.708911377818,-4.4900278589622,332.992804720949));
#48403=CARTESIAN_POINT('Ctrl Pts',(173.701279432926,-4.5452313470147,333.116293054075));
#48404=CARTESIAN_POINT('Ctrl Pts',(173.693647488034,-4.59534675937607,333.242083580868));
#48405=CARTESIAN_POINT('Ctrl Pts',(173.686015543143,-4.64018691907406,333.369709100021));
#48406=CARTESIAN_POINT('Ctrl Pts',(173.678165695928,-4.68630732582814,333.500978499933));
#48407=CARTESIAN_POINT('Ctrl Pts',(173.670315848712,-4.72684655661679,333.63418883275));
#48408=CARTESIAN_POINT('Ctrl Pts',(173.662466001497,-4.7616554662562,333.768813465322));
#48409=CARTESIAN_POINT('Ctrl Pts',(173.654828191045,-4.79552413230764,333.899801674092));
#48410=CARTESIAN_POINT('Ctrl Pts',(173.647190380592,-4.8239680256956,334.032128345781));
#48411=CARTESIAN_POINT('Ctrl Pts',(173.63955257014,-4.84690157851197,334.165297567562));
#48412=CARTESIAN_POINT('Ctrl Pts',(173.631596704543,-4.87079013466174,334.304012247202));
#48413=CARTESIAN_POINT('Ctrl Pts',(173.623640838947,-4.88869944154812,334.44364067942));
#48414=CARTESIAN_POINT('Ctrl Pts',(173.615684973351,-4.90059265648145,334.583617150041));
#48415=CARTESIAN_POINT('Ctrl Pts',(173.607729107754,-4.91248587141478,334.723593620662));
#48416=CARTESIAN_POINT('Ctrl Pts',(173.599773242158,-4.91836302723345,334.863917638052));
#48417=CARTESIAN_POINT('Ctrl Pts',(173.591817376561,-4.918248352634,335.004025458105));
#48418=CARTESIAN_POINT('',(171.841817376472,-4.91824887853913,334.996678667656));
#48419=CARTESIAN_POINT('Ctrl Pts',(173.591817376508,-4.91824835263323,335.004025459041));
#48420=CARTESIAN_POINT('Ctrl Pts',(173.579434926919,-4.91806987390456,335.222088220135));
#48421=CARTESIAN_POINT('Ctrl Pts',(173.567052477329,-4.90338612536152,335.439575567829));
#48422=CARTESIAN_POINT('Ctrl Pts',(173.55467002774,-4.87444124616087,335.654985190845));
#48423=CARTESIAN_POINT('Ctrl Pts',(173.551673142825,-4.86743580905111,335.70712009721));
#48424=CARTESIAN_POINT('Ctrl Pts',(173.548676257909,-4.85959517048378,335.759133471016));
#48425=CARTESIAN_POINT('Ctrl Pts',(173.545679372993,-4.85092312038314,335.81100428028));
#48426=CARTESIAN_POINT('Ctrl Pts',(173.537904294215,-4.82842446774871,335.945577225079));
#48427=CARTESIAN_POINT('Ctrl Pts',(173.530129215437,-4.80028609261384,336.079425884722));
#48428=CARTESIAN_POINT('Ctrl Pts',(173.522354136658,-4.7665648997525,336.212040477438));
#48429=CARTESIAN_POINT('Ctrl Pts',(173.514588625609,-4.73288520296578,336.344491879455));
#48430=CARTESIAN_POINT('Ctrl Pts',(173.50682311456,-4.69363645321306,336.475711860921));
#48431=CARTESIAN_POINT('Ctrl Pts',(173.499057603511,-4.64892702622161,336.605197983853));
#48432=CARTESIAN_POINT('Ctrl Pts',(173.491299791989,-4.60426192875721,336.734555720917));
#48433=CARTESIAN_POINT('Ctrl Pts',(173.483541980467,-4.55414705552233,336.862182653514));
#48434=CARTESIAN_POINT('Ctrl Pts',(173.475784168945,-4.49874123741858,336.987589077563));
#48435=CARTESIAN_POINT('Ctrl Pts',(173.468032195422,-4.44337711394991,337.112901129302));
#48436=CARTESIAN_POINT('Ctrl Pts',(173.460280221899,-4.38273012812621,337.235995642447));
#48437=CARTESIAN_POINT('Ctrl Pts',(173.452528248376,-4.31700797704738,337.35640089726));
#48438=CARTESIAN_POINT('Ctrl Pts',(173.444779557818,-4.25131365933858,337.476755160376));
#48439=CARTESIAN_POINT('Ctrl Pts',(173.43703086726,-4.18054863813499,337.594422087979));
#48440=CARTESIAN_POINT('Ctrl Pts',(173.429282176703,-4.10496740407348,337.708952874081));
#48441=CARTESIAN_POINT('Ctrl Pts',(173.421535098325,-4.02940189531899,337.823459831097));
#48442=CARTESIAN_POINT('Ctrl Pts',(173.413788019947,-3.94902238201836,337.934831618447));
#48443=CARTESIAN_POINT('Ctrl Pts',(173.406040941569,-3.86412748124862,338.042647181511));
#48444=CARTESIAN_POINT('Ctrl Pts',(173.398293798263,-3.7792318689779,338.150463648174));
#48445=CARTESIAN_POINT('Ctrl Pts',(173.390546654958,-3.68982103556894,338.254723524006));
#48446=CARTESIAN_POINT('Ctrl Pts',(173.382799511652,-3.59623454723086,338.355038024196));
#48447=CARTESIAN_POINT('Ctrl Pts',(173.375050626624,-3.50262701866331,338.455375077216));
#48448=CARTESIAN_POINT('Ctrl Pts',(173.367301741596,-3.40484223369459,338.551764703801));
#48449=CARTESIAN_POINT('Ctrl Pts',(173.359552856568,-3.30325705769649,338.643854535142));
#48450=CARTESIAN_POINT('Ctrl Pts',(173.351795746793,-3.20156405814299,338.736042111582));
#48451=CARTESIAN_POINT('Ctrl Pts',(173.344038637018,-3.09606289976757,338.823920513126));
#48452=CARTESIAN_POINT('Ctrl Pts',(173.336281527243,-2.98716444081456,338.907176943272));
#48453=CARTESIAN_POINT('Ctrl Pts',(173.328520272317,-2.87820779000694,338.990477862991));
#48454=CARTESIAN_POINT('Ctrl Pts',(173.320759017391,-2.76585054127866,339.069151665864));
#48455=CARTESIAN_POINT('Ctrl Pts',(173.312997762465,-2.65053221897531,339.142929159263));
#48456=CARTESIAN_POINT('Ctrl Pts',(173.30522409206,-2.5350294249385,339.216824672608));
#48457=CARTESIAN_POINT('Ctrl Pts',(173.297450421656,-2.41655642985469,339.285808028042));
#48458=CARTESIAN_POINT('Ctrl Pts',(173.289676751251,-2.29557779408966,339.349655808657));
#48459=CARTESIAN_POINT('Ctrl Pts',(173.282264947074,-2.18023074292691,339.410531459722));
#48460=CARTESIAN_POINT('Ctrl Pts',(173.274853142897,-2.0626063361906,339.466738774062));
#48461=CARTESIAN_POINT('Ctrl Pts',(173.26744133872,-1.94312204504458,339.518125693312));
#48462=CARTESIAN_POINT('Ctrl Pts',(173.259666259941,-1.81778147286245,339.572031238548));
#48463=CARTESIAN_POINT('Ctrl Pts',(173.251891181163,-1.68999799006784,339.620802268559));
#48464=CARTESIAN_POINT('Ctrl Pts',(173.244116102385,-1.56023107746598,339.664210763614));
#48465=CARTESIAN_POINT('Ctrl Pts',(173.236350591336,-1.43062385131145,339.707565841752));
#48466=CARTESIAN_POINT('Ctrl Pts',(173.228585080287,-1.29903841885686,339.745571392122));
#48467=CARTESIAN_POINT('Ctrl Pts',(173.220819569238,-1.1659559392467,339.778046652162));
#48468=CARTESIAN_POINT('Ctrl Pts',(173.213061757715,-1.03300541130252,339.810489712887));
#48469=CARTESIAN_POINT('Ctrl Pts',(173.205303946193,-0.898561167382252,
339.83741330329));
#48470=CARTESIAN_POINT('Ctrl Pts',(173.197546134671,-0.76312096260956,339.858685980687));
#48471=CARTESIAN_POINT('Ctrl Pts',(173.189794161148,-0.627782680886049,
339.87994264972));
#48472=CARTESIAN_POINT('Ctrl Pts',(173.182042187625,-0.491450314723244,
339.895556809719));
#48473=CARTESIAN_POINT('Ctrl Pts',(173.174290214102,-0.354632940132807,
339.905447842988));
#48474=CARTESIAN_POINT('Ctrl Pts',(173.166541523544,-0.21787350778175,339.915334687398));
#48475=CARTESIAN_POINT('Ctrl Pts',(173.158792832987,-0.0806298645773756,
339.919503197615));
#48476=CARTESIAN_POINT('Ctrl Pts',(173.151044142429,0.0565828594638976,
339.917924505573));
#48477=CARTESIAN_POINT('Ctrl Pts',(173.143297064051,0.193767035251864,339.916346141991));
#48478=CARTESIAN_POINT('Ctrl Pts',(173.135549985673,0.330919914069369,339.909022959081));
#48479=CARTESIAN_POINT('Ctrl Pts',(173.127802907296,0.467525823269463,339.895978213501));
#48480=CARTESIAN_POINT('Ctrl Pts',(173.12005576399,0.60413287735857,339.882933358593));
#48481=CARTESIAN_POINT('Ctrl Pts',(173.112308620684,0.740192563582616,339.864166882526));
#48482=CARTESIAN_POINT('Ctrl Pts',(173.104561477378,0.87519418573948,339.83975394));
#48483=CARTESIAN_POINT('Ctrl Pts',(173.09681259235,1.01022615912722,339.815335508927));
#48484=CARTESIAN_POINT('Ctrl Pts',(173.089063707322,1.14419921054186,339.785268154881));
#48485=CARTESIAN_POINT('Ctrl Pts',(173.081314822294,1.2766130820557,339.749678105011));
#48486=CARTESIAN_POINT('Ctrl Pts',(173.073557712519,1.40916749902087,339.714050279495));
#48487=CARTESIAN_POINT('Ctrl Pts',(173.065800602744,1.54015905213462,339.672888150186));
#48488=CARTESIAN_POINT('Ctrl Pts',(173.05804349297,1.66910236517373,339.626367944411));
#48489=CARTESIAN_POINT('Ctrl Pts',(173.050282238044,1.79811458139649,339.579822879725));
#48490=CARTESIAN_POINT('Ctrl Pts',(173.042520983117,1.92507601500787,339.527914181269));
#48491=CARTESIAN_POINT('Ctrl Pts',(173.034759728191,2.04952244434366,339.470865778866));
#48492=CARTESIAN_POINT('Ctrl Pts',(173.026986057787,2.17416794740941,339.413726117611));
#48493=CARTESIAN_POINT('Ctrl Pts',(173.019212387382,2.29629005830769,339.351430500424));
#48494=CARTESIAN_POINT('Ctrl Pts',(173.011438716977,2.41544950072452,339.284248682319));
#48495=CARTESIAN_POINT('Ctrl Pts',(173.0040269128,2.52906204242842,339.22019419401));
#48496=CARTESIAN_POINT('Ctrl Pts',(172.996615108623,2.63998128796015,339.151698323942));
#48497=CARTESIAN_POINT('Ctrl Pts',(172.989203304446,2.74785345059655,339.079029845018));
#48498=CARTESIAN_POINT('Ctrl Pts',(172.981428225668,2.86101274925862,339.002799667473));
#48499=CARTESIAN_POINT('Ctrl Pts',(172.973653146889,2.97117632363346,338.92173661347));
#48500=CARTESIAN_POINT('Ctrl Pts',(172.965878068111,3.07790377563761,338.83610367566));
#48501=CARTESIAN_POINT('Ctrl Pts',(172.958112557062,3.18449989271749,338.750576114633));
#48502=CARTESIAN_POINT('Ctrl Pts',(172.950347046013,3.28766799870819,338.660490101293));
#48503=CARTESIAN_POINT('Ctrl Pts',(172.942581534964,3.38699570369304,338.566152431636));
#48504=CARTESIAN_POINT('Ctrl Pts',(172.934823723441,3.48622492496919,338.471908298054));
#48505=CARTESIAN_POINT('Ctrl Pts',(172.927065911919,3.58162104132301,338.373421164741));
#48506=CARTESIAN_POINT('Ctrl Pts',(172.919308100397,3.67280415593889,338.271038473424));
#48507=CARTESIAN_POINT('Ctrl Pts',(172.911556126874,3.76391865236943,338.168732828328));
#48508=CARTESIAN_POINT('Ctrl Pts',(172.903804153351,3.85082619870627,338.062537751014));
#48509=CARTESIAN_POINT('Ctrl Pts',(172.896052179828,3.93318351156793,337.952837707499));
#48510=CARTESIAN_POINT('Ctrl Pts',(172.88830348927,4.01550594605869,337.843184122018));
#48511=CARTESIAN_POINT('Ctrl Pts',(172.880554798713,4.09328174560817,337.730028834551));
#48512=CARTESIAN_POINT('Ctrl Pts',(172.872806108155,4.16620786803315,337.61378940675));
#48513=CARTESIAN_POINT('Ctrl Pts',(172.865059029777,4.23911881756926,337.497574163533));
#48514=CARTESIAN_POINT('Ctrl Pts',(172.8573119514,4.30718188938616,337.378276387231));
#48515=CARTESIAN_POINT('Ctrl Pts',(172.849564873022,4.37013758044379,337.256342303484));
#48516=CARTESIAN_POINT('Ctrl Pts',(172.841817729716,4.43309379913072,337.134407197813));
#48517=CARTESIAN_POINT('Ctrl Pts',(172.83407058641,4.49094237235991,337.009836087941));
#48518=CARTESIAN_POINT('Ctrl Pts',(172.826323443104,4.5434701323031,336.883099099721));
#48519=CARTESIAN_POINT('Ctrl Pts',(172.818574558076,4.59600970160189,336.756333618335));
#48520=CARTESIAN_POINT('Ctrl Pts',(172.810825673048,4.64322592761838,336.627401650672));
#48521=CARTESIAN_POINT('Ctrl Pts',(172.80307678802,4.68495423918542,336.49679218305));
#48522=CARTESIAN_POINT('Ctrl Pts',(172.795319678245,4.72672684161353,336.366044085188));
#48523=CARTESIAN_POINT('Ctrl Pts',(172.787562568471,4.76299977460549,336.233615303541));
#48524=CARTESIAN_POINT('Ctrl Pts',(172.779805458696,4.79365856655512,336.100009368048));
#48525=CARTESIAN_POINT('Ctrl Pts',(172.77204420377,4.82433374158287,335.966332037814));
#48526=CARTESIAN_POINT('Ctrl Pts',(172.764282948844,4.84938872640018,335.831476684432));
#48527=CARTESIAN_POINT('Ctrl Pts',(172.756521693917,4.86876061139355,335.695954863079));
#48528=CARTESIAN_POINT('Ctrl Pts',(172.748748023513,4.88816348508963,335.560216250977));
#48529=CARTESIAN_POINT('Ctrl Pts',(172.740974353108,4.90186505315065,335.423809429581));
#48530=CARTESIAN_POINT('Ctrl Pts',(172.733200682703,4.90985444070406,335.287249775628));
#48531=CARTESIAN_POINT('Ctrl Pts',(172.725788878526,4.91747192034477,335.157047006422));
#48532=CARTESIAN_POINT('Ctrl Pts',(172.718377074349,4.91989705021166,335.026705600909));
#48533=CARTESIAN_POINT('Ctrl Pts',(172.710965270172,4.91716439287622,334.896668514333));
#48534=CARTESIAN_POINT('Ctrl Pts',(172.703190191394,4.91429779986462,334.760257922784));
#48535=CARTESIAN_POINT('Ctrl Pts',(172.695415112615,4.90574597962765,334.623751152937));
#48536=CARTESIAN_POINT('Ctrl Pts',(172.687640033837,4.89149176362454,334.487660865351));
#48537=CARTESIAN_POINT('Ctrl Pts',(172.679874522788,4.87725508834169,334.351738045527));
#48538=CARTESIAN_POINT('Ctrl Pts',(172.672109011739,4.85733001975963,334.216231073252));
#48539=CARTESIAN_POINT('Ctrl Pts',(172.66434350069,4.83175138132911,334.081652760921));
#48540=CARTESIAN_POINT('Ctrl Pts',(172.656585689167,4.80619810419306,333.947207883378));
#48541=CARTESIAN_POINT('Ctrl Pts',(172.648827877645,4.77500248504693,333.813690214924));
#48542=CARTESIAN_POINT('Ctrl Pts',(172.641070066123,4.7382511110836,333.681607239547));
#48543=CARTESIAN_POINT('Ctrl Pts',(172.6333180926,4.70152739369465,333.549623660798));
#48544=CARTESIAN_POINT('Ctrl Pts',(172.625566119077,4.65925634768551,333.419073001185));
#48545=CARTESIAN_POINT('Ctrl Pts',(172.617814145554,4.61157550839723,333.290451991651));
#48546=CARTESIAN_POINT('Ctrl Pts',(172.610065454996,4.56391486197267,333.16188545319));
#48547=CARTESIAN_POINT('Ctrl Pts',(172.602316764439,4.51084911458962,333.035247305177));
#48548=CARTESIAN_POINT('Ctrl Pts',(172.594568073881,4.45256540923669,332.911018348819));
#48549=CARTESIAN_POINT('Ctrl Pts',(172.586820995503,4.39429383029547,332.786815239334));
#48550=CARTESIAN_POINT('Ctrl Pts',(172.579073917125,4.33080661871464,332.665020678119));
#48551=CARTESIAN_POINT('Ctrl Pts',(172.571326838748,4.26233858317063,332.546094365116));
#48552=CARTESIAN_POINT('Ctrl Pts',(172.563579695442,4.19386997379856,332.427167055396));
#48553=CARTESIAN_POINT('Ctrl Pts',(172.555832552136,4.12042065222392,332.311108380582));
#48554=CARTESIAN_POINT('Ctrl Pts',(172.54808540883,4.04227059996193,332.198352010123));
#48555=CARTESIAN_POINT('Ctrl Pts',(172.540336523802,3.96410297790908,332.085570289637));
#48556=CARTESIAN_POINT('Ctrl Pts',(172.532587638774,3.88123274482247,331.976092672049));
#48557=CARTESIAN_POINT('Ctrl Pts',(172.524838753746,3.79398204082652,331.870322167317));
#48558=CARTESIAN_POINT('Ctrl Pts',(172.517081643971,3.70663872803182,331.764439396679));
#48559=CARTESIAN_POINT('Ctrl Pts',(172.509324534196,3.61490590568282,331.662271900966));
#48560=CARTESIAN_POINT('Ctrl Pts',(172.501567424422,3.51914505569374,331.564188430736));
#48561=CARTESIAN_POINT('Ctrl Pts',(172.493806169496,3.42333303416829,331.466052547836));
#48562=CARTESIAN_POINT('Ctrl Pts',(172.486044914569,3.32348898043557,331.372005306865));
#48563=CARTESIAN_POINT('Ctrl Pts',(172.478283659643,3.22000902815658,331.282376441718));
#48564=CARTESIAN_POINT('Ctrl Pts',(172.470509989239,3.11636354167797,331.192604199597));
#48565=CARTESIAN_POINT('Ctrl Pts',(172.462736318834,3.00907084012689,331.107264700625));
#48566=CARTESIAN_POINT('Ctrl Pts',(172.454962648429,2.89855842978221,331.026645989641));
#48567=CARTESIAN_POINT('Ctrl Pts',(172.447550844252,2.79319039872712,330.949780099048));
#48568=CARTESIAN_POINT('Ctrl Pts',(172.440139040075,2.68489590704514,330.877205542095));
#48569=CARTESIAN_POINT('Ctrl Pts',(172.432727235898,2.57406614904068,330.809132962875));
#48570=CARTESIAN_POINT('Ctrl Pts',(172.42495215712,2.45780429445129,330.737723943769));
#48571=CARTESIAN_POINT('Ctrl Pts',(172.417177078341,2.33838495880929,330.671043705931));
#48572=CARTESIAN_POINT('Ctrl Pts',(172.409401999563,2.21622995843308,330.609384116796));
#48573=CARTESIAN_POINT('Ctrl Pts',(172.401636488514,2.0942252775616,330.547800403711));
#48574=CARTESIAN_POINT('Ctrl Pts',(172.393870977465,1.969491975751,330.491225220878));
#48575=CARTESIAN_POINT('Ctrl Pts',(172.386105466416,1.84248013285272,330.439906796726));
#48576=CARTESIAN_POINT('Ctrl Pts',(172.378347654893,1.71559422256641,330.388639254941));
#48577=CARTESIAN_POINT('Ctrl Pts',(172.370589843371,1.5864346271641,330.342618244968));
#48578=CARTESIAN_POINT('Ctrl Pts',(172.362832031849,1.45547495805827,330.302045582494));
#48579=CARTESIAN_POINT('Ctrl Pts',(172.355080058326,1.32461384025657,330.261503452235));
#48580=CARTESIAN_POINT('Ctrl Pts',(172.347328084803,1.19195571690451,330.226401623726));
#48581=CARTESIAN_POINT('Ctrl Pts',(172.33957611128,1.05799272791318,330.196893250178));
#48582=CARTESIAN_POINT('Ctrl Pts',(172.331827420722,0.924086472327158,330.167397373444));
#48583=CARTESIAN_POINT('Ctrl Pts',(172.324078730165,0.788876831135882,330.143490324142));
#48584=CARTESIAN_POINT('Ctrl Pts',(172.316330039607,0.65286939414139,330.12527491886));
#48585=CARTESIAN_POINT('Ctrl Pts',(172.308582961229,0.516890254630074,330.107063303446));
#48586=CARTESIAN_POINT('Ctrl Pts',(172.300835882851,0.38011403664952,330.09454102846));
#48587=CARTESIAN_POINT('Ctrl Pts',(172.293088804474,0.243054380136059,330.087759408295));
#48588=CARTESIAN_POINT('Ctrl Pts',(172.285341661168,0.105993574930804,330.080977731293));
#48589=CARTESIAN_POINT('Ctrl Pts',(172.277594517862,-0.0313502831487476,
330.07993682439));
#48590=CARTESIAN_POINT('Ctrl Pts',(172.269847374556,-0.168460998147874,
330.08463592858));
#48591=CARTESIAN_POINT('Ctrl Pts',(172.262098489528,-0.305602538546488,
330.089336089229));
#48592=CARTESIAN_POINT('Ctrl Pts',(172.2543496045,-0.442510440995069,330.099778815489));
#48593=CARTESIAN_POINT('Ctrl Pts',(172.246600719472,-0.578671477315011,
330.115911304671));
#48594=CARTESIAN_POINT('Ctrl Pts',(172.238843609697,-0.714977036365965,
330.132060917043));
#48595=CARTESIAN_POINT('Ctrl Pts',(172.231086499922,-0.850533756960454,
330.15391231009));
#48596=CARTESIAN_POINT('Ctrl Pts',(172.223329390148,-0.984835930281048,
330.181361058045));
#48597=CARTESIAN_POINT('Ctrl Pts',(172.215568135222,-1.11920987038891,330.208824473732));
#48598=CARTESIAN_POINT('Ctrl Pts',(172.207806880295,-1.25232754825694,330.241891110077));
#48599=CARTESIAN_POINT('Ctrl Pts',(172.200045625369,-1.38369731296345,330.280406287762));
#48600=CARTESIAN_POINT('Ctrl Pts',(172.192271954965,-1.51527722648011,330.318983077179));
#48601=CARTESIAN_POINT('Ctrl Pts',(172.18449828456,-1.64510326906748,330.36302569923));
#48602=CARTESIAN_POINT('Ctrl Pts',(172.176724614155,-1.77270186949735,330.412330532353));
#48603=CARTESIAN_POINT('Ctrl Pts',(172.169312809978,-1.89436072437896,330.459340213632));
#48604=CARTESIAN_POINT('Ctrl Pts',(172.161901005801,-2.01399458101779,330.511133104955));
#48605=CARTESIAN_POINT('Ctrl Pts',(172.154489201624,-2.13121460661563,330.56749423429));
#48606=CARTESIAN_POINT('Ctrl Pts',(172.146714122846,-2.25417993484834,330.626617790466));
#48607=CARTESIAN_POINT('Ctrl Pts',(172.138939044067,-2.37487742420324,330.690955554701));
#48608=CARTESIAN_POINT('Ctrl Pts',(172.131163965289,-2.4928333681122,330.760310758873));
#48609=CARTESIAN_POINT('Ctrl Pts',(172.12339845424,-2.61064415972271,330.829580617051));
#48610=CARTESIAN_POINT('Ctrl Pts',(172.115632943191,-2.72571978475079,330.903855433897));
#48611=CARTESIAN_POINT('Ctrl Pts',(172.107867432142,-2.83760793858081,330.98289105831));
#48612=CARTESIAN_POINT('Ctrl Pts',(172.100109620619,-2.94938515498055,331.061848318672));
#48613=CARTESIAN_POINT('Ctrl Pts',(172.092351809097,-3.0579808723308,331.145556768763));
#48614=CARTESIAN_POINT('Ctrl Pts',(172.084593997575,-3.16296908120222,331.233727352692));
#48615=CARTESIAN_POINT('Ctrl Pts',(172.076842024052,-3.26787828311715,331.321831585461));
#48616=CARTESIAN_POINT('Ctrl Pts',(172.069090050529,-3.3691850820428,331.414391017976));
#48617=CARTESIAN_POINT('Ctrl Pts',(172.061338077006,-3.46649436303045,331.511074679278));
#48618=CARTESIAN_POINT('Ctrl Pts',(172.053589386448,-3.56376243347976,331.607717394991));
#48619=CARTESIAN_POINT('Ctrl Pts',(172.045840695891,-3.65703607644908,331.708480590676));
#48620=CARTESIAN_POINT('Ctrl Pts',(172.038092005333,-3.7459552276218,331.812994745038));
#48621=CARTESIAN_POINT('Ctrl Pts',(172.030344926955,-3.83485587842246,331.917487154358));
#48622=CARTESIAN_POINT('Ctrl Pts',(172.022597848577,-3.91940358637563,332.025728672528));
#48623=CARTESIAN_POINT('Ctrl Pts',(172.0148507702,-3.99927724007334,332.137315137929));
#48624=CARTESIAN_POINT('Ctrl Pts',(172.007103626894,-4.07915156318909,332.248902538532));
#48625=CARTESIAN_POINT('Ctrl Pts',(171.999356483588,-4.15435152640599,332.363834624441));
#48626=CARTESIAN_POINT('Ctrl Pts',(171.991609340282,-4.22459842473841,332.481676904725));
#48627=CARTESIAN_POINT('Ctrl Pts',(171.983860455254,-4.29486111606491,332.599545678454));
#48628=CARTESIAN_POINT('Ctrl Pts',(171.976111570226,-4.36016832655585,332.720325612808));
#48629=CARTESIAN_POINT('Ctrl Pts',(171.968362685198,-4.4202867219027,332.843556548696));
#48630=CARTESIAN_POINT('Ctrl Pts',(171.960605575423,-4.4804689275356,332.966918283173));
#48631=CARTESIAN_POINT('Ctrl Pts',(171.952848465648,-4.53545114469992,333.092735864107));
#48632=CARTESIAN_POINT('Ctrl Pts',(171.945091355874,-4.58504751919254,333.220527519391));
#48633=CARTESIAN_POINT('Ctrl Pts',(171.937330100948,-4.63467039640191,333.348387462449));
#48634=CARTESIAN_POINT('Ctrl Pts',(171.929568846021,-4.67890157023945,333.478223211998));
#48635=CARTESIAN_POINT('Ctrl Pts',(171.921807591095,-4.71760505331683,333.609537622437));
#48636=CARTESIAN_POINT('Ctrl Pts',(171.914033920691,-4.75637044935367,333.741062093136));
#48637=CARTESIAN_POINT('Ctrl Pts',(171.906260250286,-4.78959038992416,333.874069572022));
#48638=CARTESIAN_POINT('Ctrl Pts',(171.898486579881,-4.81717982817702,334.008051631634));
#48639=CARTESIAN_POINT('Ctrl Pts',(171.891074775704,-4.84348497144162,334.135796794137));
#48640=CARTESIAN_POINT('Ctrl Pts',(171.883662971527,-4.86467196859223,334.264427561831));
#48641=CARTESIAN_POINT('Ctrl Pts',(171.87625116735,-4.8807111744566,334.39350062322));
#48642=CARTESIAN_POINT('Ctrl Pts',(171.86477323707,-4.90554951101645,334.593383346012));
#48643=CARTESIAN_POINT('Ctrl Pts',(171.853295306789,-4.91811256346442,334.794822525422));
#48644=CARTESIAN_POINT('Ctrl Pts',(171.841817376508,-4.9182488785387,334.996678667015));
#48645=CARTESIAN_POINT('',(170.091817376553,-4.91824948312363,334.997745170935));
#48646=CARTESIAN_POINT('Ctrl Pts',(171.841817376472,-4.91824887853913,334.996678667656));
#48647=CARTESIAN_POINT('Ctrl Pts',(171.83415687076,-4.91833985680596,335.131399831482));
#48648=CARTESIAN_POINT('Ctrl Pts',(171.826496365047,-4.91289122752626,335.266338137322));
#48649=CARTESIAN_POINT('Ctrl Pts',(171.818835859335,-4.90187596891744,335.400992578298));
#48650=CARTESIAN_POINT('Ctrl Pts',(171.811183512138,-4.89087244166797,335.535503610962));
#48651=CARTESIAN_POINT('Ctrl Pts',(171.80353116494,-4.87431410850533,335.669730981874));
#48652=CARTESIAN_POINT('Ctrl Pts',(171.795878817742,-4.85222596571158,335.803172609203));
#48653=CARTESIAN_POINT('Ctrl Pts',(171.788232669823,-4.83015571684494,335.936506133521));
#48654=CARTESIAN_POINT('Ctrl Pts',(171.780586521903,-4.80256463531711,336.069054785126));
#48655=CARTESIAN_POINT('Ctrl Pts',(171.772940373984,-4.76952958216479,336.200321051784));
#48656=CARTESIAN_POINT('Ctrl Pts',(171.765297904939,-4.73651042352852,336.331524160868));
#48657=CARTESIAN_POINT('Ctrl Pts',(171.757655435894,-4.69805259911997,336.461445722151));
#48658=CARTESIAN_POINT('Ctrl Pts',(171.75001296685,-4.65428408820265,336.589598279064));
#48659=CARTESIAN_POINT('Ctrl Pts',(171.742372266164,-4.61052570469982,336.717721183288));
#48660=CARTESIAN_POINT('Ctrl Pts',(171.734731565479,-4.5614592076922,336.844075516026));
#48661=CARTESIAN_POINT('Ctrl Pts',(171.727090864793,-4.50726232661123,336.968189366299));
#48662=CARTESIAN_POINT('Ctrl Pts',(171.719450170526,-4.45306549105969,337.092303112306));
#48663=CARTESIAN_POINT('Ctrl Pts',(171.71180947626,-4.39373844137937,337.214176010574));
#48664=CARTESIAN_POINT('Ctrl Pts',(171.704168781993,-4.32950667472082,337.333357027128));
#48665=CARTESIAN_POINT('Ctrl Pts',(171.696526332425,-4.26526015206392,337.452565423202));
#48666=CARTESIAN_POINT('Ctrl Pts',(171.688883882858,-4.19610686327876,337.56908035365));
#48667=CARTESIAN_POINT('Ctrl Pts',(171.68124143329,-4.12231750568051,337.682476737058));
#48668=CARTESIAN_POINT('Ctrl Pts',(171.673591077707,-4.04845181394261,337.795990427565));
#48669=CARTESIAN_POINT('Ctrl Pts',(171.665940722124,-3.96994069795861,337.906378792117));
#48670=CARTESIAN_POINT('Ctrl Pts',(171.658290366541,-3.88709748584564,338.013246786779));
#48671=CARTESIAN_POINT('Ctrl Pts',(171.650635692359,-3.80420750902946,338.120175108049));
#48672=CARTESIAN_POINT('Ctrl Pts',(171.642981018177,-3.71698082689311,338.223578796079));
#48673=CARTESIAN_POINT('Ctrl Pts',(171.635326343995,-3.62576916716357,338.323098104021));
#48674=CARTESIAN_POINT('Ctrl Pts',(171.627660272187,-3.53442169546484,338.42276559382));
#48675=CARTESIAN_POINT('Ctrl Pts',(171.619994200378,-3.43907768254678,338.518536870929));
#48676=CARTESIAN_POINT('Ctrl Pts',(171.612328128571,-3.34012393277351,338.610090743487));
#48677=CARTESIAN_POINT('Ctrl Pts',(171.607556463406,-3.27853121977259,338.667077481328));
#48678=CARTESIAN_POINT('Ctrl Pts',(171.602784798241,-3.21554063039557,338.722431078597));
#48679=CARTESIAN_POINT('Ctrl Pts',(171.598013133076,-3.15125113667784,338.776082538304));
#48680=CARTESIAN_POINT('Ctrl Pts',(171.590238054298,-3.04649611698931,338.863503660994));
#48681=CARTESIAN_POINT('Ctrl Pts',(171.582462975519,-2.93793498948684,338.946700496503));
#48682=CARTESIAN_POINT('Ctrl Pts',(171.574687896741,-2.82594309640998,339.02532342531));
#48683=CARTESIAN_POINT('Ctrl Pts',(171.566922385692,-2.71408901648724,339.103849603598));
#48684=CARTESIAN_POINT('Ctrl Pts',(171.559156874643,-2.59881288796413,339.17781285181));
#48685=CARTESIAN_POINT('Ctrl Pts',(171.551391363594,-2.480524311526,339.246902659872));
#48686=CARTESIAN_POINT('Ctrl Pts',(171.543633552072,-2.36235301855613,339.315923965189));
#48687=CARTESIAN_POINT('Ctrl Pts',(171.53587574055,-2.24117555701862,339.380081250501));
#48688=CARTESIAN_POINT('Ctrl Pts',(171.528117929027,-2.11743150328736,339.439106542018));
#48689=CARTESIAN_POINT('Ctrl Pts',(171.520365955504,-1.99378057088057,339.498087415131));
#48690=CARTESIAN_POINT('Ctrl Pts',(171.512613981981,-1.86756724209513,339.551943813942));
#48691=CARTESIAN_POINT('Ctrl Pts',(171.504862008458,-1.73925644244831,339.600453248312));
#48692=CARTESIAN_POINT('Ctrl Pts',(171.497113317901,-1.61099998250131,339.648942138908));
#48693=CARTESIAN_POINT('Ctrl Pts',(171.489364627343,-1.48064818327629,339.692088430941));
#48694=CARTESIAN_POINT('Ctrl Pts',(171.481615936785,-1.348686535168,339.729717506612));
#48695=CARTESIAN_POINT('Ctrl Pts',(171.473868858408,-1.21675234278274,339.767338753241));
#48696=CARTESIAN_POINT('Ctrl Pts',(171.46612178003,-1.08320934339336,339.799444959649));
#48697=CARTESIAN_POINT('Ctrl Pts',(171.458374701652,-0.948558416906424,
339.825911312096));
#48698=CARTESIAN_POINT('Ctrl Pts',(171.450627558346,-0.813906361915053,
339.852377886356));
#48699=CARTESIAN_POINT('Ctrl Pts',(171.44288041504,-0.678146744841247,339.873204436991));
#48700=CARTESIAN_POINT('Ctrl Pts',(171.435133271735,-0.541790480690989,
339.888317311461));
#48701=CARTESIAN_POINT('Ctrl Pts',(171.427384386706,-0.405403560757368,
339.903433583627));
#48702=CARTESIAN_POINT('Ctrl Pts',(171.419635501678,-0.268420115245306,
339.912833580455));
#48703=CARTESIAN_POINT('Ctrl Pts',(171.41188661665,-0.131355623864658,339.916495577399));
#48704=CARTESIAN_POINT('Ctrl Pts',(171.404129506875,0.0058543491829664,
339.920161461223));
#48705=CARTESIAN_POINT('Ctrl Pts',(171.396372397101,0.143145148586016,339.918077168616));
#48706=CARTESIAN_POINT('Ctrl Pts',(171.388615287326,0.280001294611361,339.910273142862));
#48707=CARTESIAN_POINT('Ctrl Pts',(171.3808540324,0.416930572185307,339.902464946887));
#48708=CARTESIAN_POINT('Ctrl Pts',(171.373092777474,0.553424344803314,339.888930966077));
#48709=CARTESIAN_POINT('Ctrl Pts',(171.365331522547,0.688973800366967,339.869753398778));
#48710=CARTESIAN_POINT('Ctrl Pts',(171.357557852143,0.824740090884081,339.85054515362));
#48711=CARTESIAN_POINT('Ctrl Pts',(171.349784181738,0.959558661130566,339.825675352503));
#48712=CARTESIAN_POINT('Ctrl Pts',(171.342010511333,1.09293153545217,339.795277230913));
#48713=CARTESIAN_POINT('Ctrl Pts',(171.334598707156,1.22009587038676,339.766294149197));
#48714=CARTESIAN_POINT('Ctrl Pts',(171.327186902979,1.34594579689556,339.732285926021));
#48715=CARTESIAN_POINT('Ctrl Pts',(171.319775098802,1.47006555683976,339.693409242874));
#48716=CARTESIAN_POINT('Ctrl Pts',(171.312000020024,1.60026879595247,339.652627097678));
#48717=CARTESIAN_POINT('Ctrl Pts',(171.304224941245,1.72897944518697,339.606358311038));
#48718=CARTESIAN_POINT('Ctrl Pts',(171.296449862467,1.85570038280514,339.554729317068));
#48719=CARTESIAN_POINT('Ctrl Pts',(171.288684351418,1.98226538224199,339.503163855861));
#48720=CARTESIAN_POINT('Ctrl Pts',(171.280918840369,2.1068451832861,339.446251457695));
#48721=CARTESIAN_POINT('Ctrl Pts',(171.27315332932,2.22895701295995,339.384168529707));
#48722=CARTESIAN_POINT('Ctrl Pts',(171.265395517797,2.35094776839938,339.322147157123));
#48723=CARTESIAN_POINT('Ctrl Pts',(171.257637706275,2.47047507595442,339.254965632935));
#48724=CARTESIAN_POINT('Ctrl Pts',(171.249879894753,2.58707571074669,339.182848590299));
#48725=CARTESIAN_POINT('Ctrl Pts',(171.24212792123,2.70358859986355,339.110785818024));
#48726=CARTESIAN_POINT('Ctrl Pts',(171.234375947707,2.81717886892489,339.033795124881));
#48727=CARTESIAN_POINT('Ctrl Pts',(171.226623974184,2.92740782335127,338.952147074475));
#48728=CARTESIAN_POINT('Ctrl Pts',(171.218875283626,3.03759009574995,338.870533602067));
#48729=CARTESIAN_POINT('Ctrl Pts',(171.211126593069,3.14441357135188,338.784266927518));
#48730=CARTESIAN_POINT('Ctrl Pts',(171.203377902511,3.24746868361462,338.693660814347));
#48731=CARTESIAN_POINT('Ctrl Pts',(171.195630824133,3.35050235440044,338.603073552535));
#48732=CARTESIAN_POINT('Ctrl Pts',(171.187883745755,3.44976892799036,338.508148905874));
#48733=CARTESIAN_POINT('Ctrl Pts',(171.180136667377,3.54489239098842,338.409240531088));
#48734=CARTESIAN_POINT('Ctrl Pts',(171.172389524072,3.64001665121254,338.310331327354));
#48735=CARTESIAN_POINT('Ctrl Pts',(171.164642380766,3.7309974606398,338.207438610628));
#48736=CARTESIAN_POINT('Ctrl Pts',(171.15689523746,3.81749639785324,338.100952162623));
#48737=CARTESIAN_POINT('Ctrl Pts',(171.149146352432,3.90401478186425,337.994441774204));
#48738=CARTESIAN_POINT('Ctrl Pts',(171.141397467404,3.98604904221244,337.884336350115));
#48739=CARTESIAN_POINT('Ctrl Pts',(171.133648582376,4.06330195461183,337.771057611842));
#48740=CARTESIAN_POINT('Ctrl Pts',(171.125891472601,4.14063686405067,337.657658638346));
#48741=CARTESIAN_POINT('Ctrl Pts',(171.118134362826,4.21318006723221,337.54107994583));
#48742=CARTESIAN_POINT('Ctrl Pts',(171.110377253052,4.28067820890297,337.421771486809));
#48743=CARTESIAN_POINT('Ctrl Pts',(171.102615998125,4.34821241942249,337.302399273163));
#48744=CARTESIAN_POINT('Ctrl Pts',(171.094854743199,4.41069601859924,337.180294734205));
#48745=CARTESIAN_POINT('Ctrl Pts',(171.087093488273,4.46792278135317,337.055930223127));
#48746=CARTESIAN_POINT('Ctrl Pts',(171.079319817868,4.52524108827738,336.93136676936));
#48747=CARTESIAN_POINT('Ctrl Pts',(171.071546147464,4.57728560619161,336.804536480998));
#48748=CARTESIAN_POINT('Ctrl Pts',(171.063772477059,4.62389889246094,336.675930217759));
#48749=CARTESIAN_POINT('Ctrl Pts',(171.056360672882,4.66834231903945,336.553310607017));
#48750=CARTESIAN_POINT('Ctrl Pts',(171.048948868705,4.70784869513809,336.429076917974));
#48751=CARTESIAN_POINT('Ctrl Pts',(171.041537064528,4.74232478697736,336.303663559865));
#48752=CARTESIAN_POINT('Ctrl Pts',(171.03376198575,4.77849065477695,336.172103319487));
#48753=CARTESIAN_POINT('Ctrl Pts',(171.025986906971,4.80923496270685,336.038829093271));
#48754=CARTESIAN_POINT('Ctrl Pts',(171.018211828193,4.83439501081193,335.904327342248));
#48755=CARTESIAN_POINT('Ctrl Pts',(171.010446317144,4.85952409787605,335.769991104191));
#48756=CARTESIAN_POINT('Ctrl Pts',(171.002680806095,4.87908252681788,335.63443072742));
#48757=CARTESIAN_POINT('Ctrl Pts',(170.994915295046,4.89295738600349,335.498147650054));
#48758=CARTESIAN_POINT('Ctrl Pts',(170.987157483524,4.90681848822583,335.361999697755));
#48759=CARTESIAN_POINT('Ctrl Pts',(170.979399672001,4.91500719587485,335.225130857216));
#48760=CARTESIAN_POINT('Ctrl Pts',(170.971641860479,4.91746173020135,335.088052226009));
#48761=CARTESIAN_POINT('Ctrl Pts',(170.963889886956,4.91991441741294,334.951076750818));
#48762=CARTESIAN_POINT('Ctrl Pts',(170.956137913433,4.916641513422,334.813892188438));
#48763=CARTESIAN_POINT('Ctrl Pts',(170.94838593991,4.9076331381274,334.677013863991));
#48764=CARTESIAN_POINT('Ctrl Pts',(170.940637249353,4.89862857788507,334.540193507596));
#48765=CARTESIAN_POINT('Ctrl Pts',(170.932888558795,4.88389340301586,334.403679520404));
#48766=CARTESIAN_POINT('Ctrl Pts',(170.925139868237,4.86346982400044,334.267986111104));
#48767=CARTESIAN_POINT('Ctrl Pts',(170.917392789859,4.84305049428122,334.13232093395));
#48768=CARTESIAN_POINT('Ctrl Pts',(170.909645711482,4.81694517266051,333.997476381376));
#48769=CARTESIAN_POINT('Ctrl Pts',(170.901898633104,4.78524777419646,333.863960035013));
#48770=CARTESIAN_POINT('Ctrl Pts',(170.894151489798,4.75355011007767,333.730442569654));
#48771=CARTESIAN_POINT('Ctrl Pts',(170.886404346492,4.71626036592176,333.598253713012));
#48772=CARTESIAN_POINT('Ctrl Pts',(170.878657203186,4.67352317824004,333.467888984129));
#48773=CARTESIAN_POINT('Ctrl Pts',(170.870908318158,4.63077638233125,333.337494946487));
#48774=CARTESIAN_POINT('Ctrl Pts',(170.86315943313,4.58257982761819,333.208926224014));
#48775=CARTESIAN_POINT('Ctrl Pts',(170.855410548102,4.52912730357899,333.082660976646));
#48776=CARTESIAN_POINT('Ctrl Pts',(170.847653438327,4.47561804447848,332.956261710041));
#48777=CARTESIAN_POINT('Ctrl Pts',(170.839896328553,4.4168418246148,332.83217116304));
#48778=CARTESIAN_POINT('Ctrl Pts',(170.832139218778,4.35303991359075,332.710845882605));
#48779=CARTESIAN_POINT('Ctrl Pts',(170.824377963852,4.2892039088655,332.58945576982));
#48780=CARTESIAN_POINT('Ctrl Pts',(170.816616708926,4.22033705789302,332.470834205856));
#48781=CARTESIAN_POINT('Ctrl Pts',(170.808855453999,4.14672497232374,332.355410227198));
#48782=CARTESIAN_POINT('Ctrl Pts',(170.801081783595,4.07299513140762,332.239801607791));
#48783=CARTESIAN_POINT('Ctrl Pts',(170.79330811319,3.99450511107566,332.127401115803));
#48784=CARTESIAN_POINT('Ctrl Pts',(170.785534442786,3.91158248449447,332.018606780464));
#48785=CARTESIAN_POINT('Ctrl Pts',(170.778122638608,3.83251992612982,331.914876847608));
#48786=CARTESIAN_POINT('Ctrl Pts',(170.770710834431,3.74942833358566,331.814425115445));
#48787=CARTESIAN_POINT('Ctrl Pts',(170.763299030254,3.66262255670514,331.717565070011));
#48788=CARTESIAN_POINT('Ctrl Pts',(170.755523951476,3.57156217011946,331.615957625219));
#48789=CARTESIAN_POINT('Ctrl Pts',(170.747748872697,3.4761265391429,331.517981749701));
#48790=CARTESIAN_POINT('Ctrl Pts',(170.739973793919,3.3766366929507,331.424037513295));
#48791=CARTESIAN_POINT('Ctrl Pts',(170.73220828287,3.27726927534811,331.330208881253));
#48792=CARTESIAN_POINT('Ctrl Pts',(170.724442771821,3.17385785062971,331.240402282771));
#48793=CARTESIAN_POINT('Ctrl Pts',(170.716677260772,3.06676298584503,331.154984024591));
#48794=CARTESIAN_POINT('Ctrl Pts',(170.708919449249,2.95977430593056,331.069650458862));
#48795=CARTESIAN_POINT('Ctrl Pts',(170.701161637727,2.84910975752933,330.988696816753));
#48796=CARTESIAN_POINT('Ctrl Pts',(170.693403826205,2.73516570146764,330.912451633556));
#48797=CARTESIAN_POINT('Ctrl Pts',(170.685651852682,2.62130739192161,330.836263827278));
#48798=CARTESIAN_POINT('Ctrl Pts',(170.677899879159,2.504174810563,330.764777643716));
#48799=CARTESIAN_POINT('Ctrl Pts',(170.670147905636,2.38419595859192,330.698280263251));
#48800=CARTESIAN_POINT('Ctrl Pts',(170.662399215078,2.26426791773581,330.631811044467));
#48801=CARTESIAN_POINT('Ctrl Pts',(170.654650524521,2.14149634488201,330.570326615735));
#48802=CARTESIAN_POINT('Ctrl Pts',(170.646901833963,2.01633649159924,330.514069749189));
#48803=CARTESIAN_POINT('Ctrl Pts',(170.639154755585,1.89120267886925,330.457824587353));
#48804=CARTESIAN_POINT('Ctrl Pts',(170.631407677207,1.76368193037506,330.40680498446));
#48805=CARTESIAN_POINT('Ctrl Pts',(170.62366059883,1.63425190516625,330.361206646879));
#48806=CARTESIAN_POINT('Ctrl Pts',(170.615913455524,1.5048207952092,330.31560792714));
#48807=CARTESIAN_POINT('Ctrl Pts',(170.608166312218,1.37348074528588,330.275430693219));
#48808=CARTESIAN_POINT('Ctrl Pts',(170.600419168912,1.24072671904426,330.240821470973));
#48809=CARTESIAN_POINT('Ctrl Pts',(170.592670283884,1.10794284687953,330.20620446784));
#48810=CARTESIAN_POINT('Ctrl Pts',(170.584921398856,0.973744743985446,330.177158065924));
#48811=CARTESIAN_POINT('Ctrl Pts',(170.577172513828,0.838639375860506,330.1537780633));
#48812=CARTESIAN_POINT('Ctrl Pts',(170.569415404053,0.703390605501616,330.130373244899));
#48813=CARTESIAN_POINT('Ctrl Pts',(170.561658294278,0.567233032025835,330.112646906821));
#48814=CARTESIAN_POINT('Ctrl Pts',(170.553901184504,0.430681140338857,330.100643224069));
#48815=CARTESIAN_POINT('Ctrl Pts',(170.546139929578,0.294056279686859,330.088633126933));
#48816=CARTESIAN_POINT('Ctrl Pts',(170.538378674651,0.157037071229068,330.082351796361));
#48817=CARTESIAN_POINT('Ctrl Pts',(170.530617419725,0.0201388617503955,
330.081791231683));
#48818=CARTESIAN_POINT('Ctrl Pts',(170.52284374932,-0.116978340248281,330.081229770284));
#48819=CARTESIAN_POINT('Ctrl Pts',(170.515070078916,-0.253973765678893,
330.086407347139));
#48820=CARTESIAN_POINT('Ctrl Pts',(170.507296408511,-0.390335434633327,
330.097263895439));
#48821=CARTESIAN_POINT('Ctrl Pts',(170.499884604334,-0.520349435090383,
330.107615068803));
#48822=CARTESIAN_POINT('Ctrl Pts',(170.492472800157,-0.649787068228315,
330.123128365462));
#48823=CARTESIAN_POINT('Ctrl Pts',(170.48506099598,-0.778214333635241,330.143708666747));
#48824=CARTESIAN_POINT('Ctrl Pts',(170.477285917202,-0.912936201885633,
330.165297669905));
#48825=CARTESIAN_POINT('Ctrl Pts',(170.469510838423,-1.04697190184907,330.192531159925));
#48826=CARTESIAN_POINT('Ctrl Pts',(170.461735759645,-1.17981127895567,330.225355677273));
#48827=CARTESIAN_POINT('Ctrl Pts',(170.453970248596,-1.31248718875235,330.258139801962));
#48828=CARTESIAN_POINT('Ctrl Pts',(170.446204737547,-1.44396932901759,330.296501171654));
#48829=CARTESIAN_POINT('Ctrl Pts',(170.438439226498,-1.5737545410778,330.340334807421));
#48830=CARTESIAN_POINT('Ctrl Pts',(170.430681414975,-1.70341107072154,330.384124982009));
#48831=CARTESIAN_POINT('Ctrl Pts',(170.422923603453,-1.8313736525109,330.43337650082));
#48832=CARTESIAN_POINT('Ctrl Pts',(170.415165791931,-1.95715152052411,330.487933844877));
#48833=CARTESIAN_POINT('Ctrl Pts',(170.407413818408,-2.08283473670317,330.542450132802));
#48834=CARTESIAN_POINT('Ctrl Pts',(170.399661844885,-2.20633615439062,330.602264143578));
#48835=CARTESIAN_POINT('Ctrl Pts',(170.391909871362,-2.32718266146913,330.667171371649));
#48836=CARTESIAN_POINT('Ctrl Pts',(170.384161180805,-2.44797798998007,330.73205111147));
#48837=CARTESIAN_POINT('Ctrl Pts',(170.376412490247,-2.56612030051568,330.802019593937));
#48838=CARTESIAN_POINT('Ctrl Pts',(170.368663799689,-2.68115907806432,330.876825366224));
#48839=CARTESIAN_POINT('Ctrl Pts',(170.360916721311,-2.79617392083476,330.951615574546));
#48840=CARTESIAN_POINT('Ctrl Pts',(170.353169642934,-2.9080861875124,331.031240857861));
#48841=CARTESIAN_POINT('Ctrl Pts',(170.345422564556,-3.01647281571578,331.11540545043));
#48842=CARTESIAN_POINT('Ctrl Pts',(170.33767542125,-3.12486035230351,331.19957074838));
#48843=CARTESIAN_POINT('Ctrl Pts',(170.329928277944,-3.2297218827555,331.288275191734));
#48844=CARTESIAN_POINT('Ctrl Pts',(170.322181134638,-3.33066633712121,331.381181848549));
#48845=CARTESIAN_POINT('Ctrl Pts',(170.31443224961,-3.43163348594351,331.474109392754));
#48846=CARTESIAN_POINT('Ctrl Pts',(170.306683364582,-3.52868151875388,331.571240765711));
#48847=CARTESIAN_POINT('Ctrl Pts',(170.298934479554,-3.62145552878866,331.67220149115));
#48848=CARTESIAN_POINT('Ctrl Pts',(170.291177369779,-3.71432801011585,331.773269377345));
#48849=CARTESIAN_POINT('Ctrl Pts',(170.283420260005,-3.8029171417072,331.878174447005));
#48850=CARTESIAN_POINT('Ctrl Pts',(170.27566315023,-3.88690735855828,331.986507964423));
#48851=CARTESIAN_POINT('Ctrl Pts',(170.267901895304,-3.97094245709576,332.094899371809));
#48852=CARTESIAN_POINT('Ctrl Pts',(170.260140640377,-4.05037351783678,332.206722558982));
#48853=CARTESIAN_POINT('Ctrl Pts',(170.252379385451,-4.12492838499993,332.321539830215));
#48854=CARTESIAN_POINT('Ctrl Pts',(170.244605715047,-4.19960251565316,332.436540771664));
#48855=CARTESIAN_POINT('Ctrl Pts',(170.236832044642,-4.26938466631352,332.554545031503));
#48856=CARTESIAN_POINT('Ctrl Pts',(170.229058374237,-4.33404828673625,332.675089569308));
#48857=CARTESIAN_POINT('Ctrl Pts',(170.22164657006,-4.39570180007076,332.790022729877));
#48858=CARTESIAN_POINT('Ctrl Pts',(170.214234765883,-4.45270246836924,332.907264731988));
#48859=CARTESIAN_POINT('Ctrl Pts',(170.206822961706,-4.50489541642322,333.026399141268));
#48860=CARTESIAN_POINT('Ctrl Pts',(170.198248995252,-4.5652721580458,333.164213687401));
#48861=CARTESIAN_POINT('Ctrl Pts',(170.189675028798,-4.61937956341198,333.304934489102));
#48862=CARTESIAN_POINT('Ctrl Pts',(170.181101062344,-4.66695640459487,333.448000972903));
#48863=CARTESIAN_POINT('Ctrl Pts',(170.172560704663,-4.71434675107962,333.590506655691));
#48864=CARTESIAN_POINT('Ctrl Pts',(170.164020346983,-4.75525750505167,333.735339441107));
#48865=CARTESIAN_POINT('Ctrl Pts',(170.155479989303,-4.78947631491731,333.881921428814));
#48866=CARTESIAN_POINT('Ctrl Pts',(170.146961338724,-4.82360815053345,334.028130847795));
#48867=CARTESIAN_POINT('Ctrl Pts',(170.138442688146,-4.85108189296937,334.176080358734));
#48868=CARTESIAN_POINT('Ctrl Pts',(170.129924037567,-4.87173436043102,334.325176034883));
#48869=CARTESIAN_POINT('Ctrl Pts',(170.12143967778,-4.89230369389797,334.47367154453));
#48870=CARTESIAN_POINT('Ctrl Pts',(170.112955317993,-4.90610646026499,334.623303768268));
#48871=CARTESIAN_POINT('Ctrl Pts',(170.104470958206,-4.91303031194559,334.773469171184));
#48872=CARTESIAN_POINT('Ctrl Pts',(170.100253097655,-4.91647239144224,334.84812144254));
#48873=CARTESIAN_POINT('Ctrl Pts',(170.096035237104,-4.9182151718842,334.92290524704));
#48874=CARTESIAN_POINT('Ctrl Pts',(170.091817376553,-4.91824948312363,334.997745170935));
#48875=CARTESIAN_POINT('',(168.341817376469,-4.91824814939194,335.004266556313));
#48876=CARTESIAN_POINT('Ctrl Pts',(170.091817376508,-4.918249483124,334.997745171737));
#48877=CARTESIAN_POINT('Ctrl Pts',(170.083938194233,-4.91831357827607,335.137550031252));
#48878=CARTESIAN_POINT('Ctrl Pts',(170.076059011959,-4.91241223784542,335.277335856181));
#48879=CARTESIAN_POINT('Ctrl Pts',(170.068179829684,-4.90057678679853,335.416569585053));
#48880=CARTESIAN_POINT('Ctrl Pts',(170.060297759064,-4.88873699711906,335.555854354142));
#48881=CARTESIAN_POINT('Ctrl Pts',(170.052415688443,-4.87095879426482,335.694586253213));
#48882=CARTESIAN_POINT('Ctrl Pts',(170.044533617822,-4.84732532250688,335.832238115135));
#48883=CARTESIAN_POINT('Ctrl Pts',(170.036647192215,-4.82367879282824,335.969966032201));
#48884=CARTESIAN_POINT('Ctrl Pts',(170.028760766608,-4.79417061176356,336.106612356849));
#48885=CARTESIAN_POINT('Ctrl Pts',(170.020874341001,-4.75893485644403,336.24166102243));
#48886=CARTESIAN_POINT('Ctrl Pts',(170.012976316539,-4.72364727861164,336.376908309018));
#48887=CARTESIAN_POINT('Ctrl Pts',(170.005078292078,-4.68261539016203,336.510552881302));
#48888=CARTESIAN_POINT('Ctrl Pts',(169.997180267616,-4.63602320102892,336.642093767731));
#48889=CARTESIAN_POINT('Ctrl Pts',(169.989276218659,-4.58939547206374,336.773734991601));
#48890=CARTESIAN_POINT('Ctrl Pts',(169.981372169701,-4.53719912558592,336.903268985875));
#48891=CARTESIAN_POINT('Ctrl Pts',(169.973468120743,-4.47966576469273,337.030216170544));
#48892=CARTESIAN_POINT('Ctrl Pts',(169.96554943329,-4.42202585058367,337.157398464558));
#48893=CARTESIAN_POINT('Ctrl Pts',(169.957630745837,-4.35902933402799,337.281984041251));
#48894=CARTESIAN_POINT('Ctrl Pts',(169.949712058384,-4.29095368250246,337.403518162427));
#48895=CARTESIAN_POINT('Ctrl Pts',(169.9426696814,-4.23041152771796,337.511602880105));
#48896=CARTESIAN_POINT('Ctrl Pts',(169.935627304416,-4.16585291978915,337.617274393364));
#48897=CARTESIAN_POINT('Ctrl Pts',(169.928584927432,-4.09750046770699,337.720233993546));
#48898=CARTESIAN_POINT('Ctrl Pts',(169.920809848654,-4.02203650137134,337.833905699027));
#48899=CARTESIAN_POINT('Ctrl Pts',(169.913034769875,-3.94171953061327,337.944614398106));
#48900=CARTESIAN_POINT('Ctrl Pts',(169.905259691097,-3.85680956688121,338.051917926045));
#48901=CARTESIAN_POINT('Ctrl Pts',(169.897494180048,-3.77200409026515,338.159089410162));
#48902=CARTESIAN_POINT('Ctrl Pts',(169.889728668999,-3.68261710670557,338.262863757008));
#48903=CARTESIAN_POINT('Ctrl Pts',(169.88196315795,-3.58895261920911,338.362826513451));
#48904=CARTESIAN_POINT('Ctrl Pts',(169.874205346428,-3.49538100032463,338.462690156531));
#48905=CARTESIAN_POINT('Ctrl Pts',(169.866447534905,-3.39754058318325,338.558749446645));
#48906=CARTESIAN_POINT('Ctrl Pts',(169.858689723383,-3.29577623510711,338.650622148429));
#48907=CARTESIAN_POINT('Ctrl Pts',(169.85093774986,-3.19408846793019,338.742425713092));
#48908=CARTESIAN_POINT('Ctrl Pts',(169.843185776337,-3.08848293634901,338.830048699548));
#48909=CARTESIAN_POINT('Ctrl Pts',(169.835433802814,-2.97934177848387,338.913145234908));
#48910=CARTESIAN_POINT('Ctrl Pts',(169.827685112256,-2.87024684196379,338.996206578835));
#48911=CARTESIAN_POINT('Ctrl Pts',(169.819936421699,-2.75761956761028,339.074745048066));
#48912=CARTESIAN_POINT('Ctrl Pts',(169.812187731141,-2.64187546028209,339.148454786407));
#48913=CARTESIAN_POINT('Ctrl Pts',(169.804440652763,-2.5261554344821,339.22214918882));
#48914=CARTESIAN_POINT('Ctrl Pts',(169.796693574386,-2.40732019507464,339.291016648849));
#48915=CARTESIAN_POINT('Ctrl Pts',(169.788946496008,-2.28581420439046,339.354794654804));
#48916=CARTESIAN_POINT('Ctrl Pts',(169.781199352702,-2.16430719536891,339.418573195279));
#48917=CARTESIAN_POINT('Ctrl Pts',(169.773452209396,-2.04012973651922,339.477262014939));
#48918=CARTESIAN_POINT('Ctrl Pts',(169.76570506609,-1.91375050286465,339.530644774785));
#48919=CARTESIAN_POINT('Ctrl Pts',(169.757956181062,-1.78734285647576,339.584039536208));
#48920=CARTESIAN_POINT('Ctrl Pts',(169.750207296034,-1.65873281027521,339.632125711985));
#48921=CARTESIAN_POINT('Ctrl Pts',(169.742458411006,-1.52840822762592,339.674735431254));
#48922=CARTESIAN_POINT('Ctrl Pts',(169.734701301231,-1.39794531711777,339.71739037692));
#48923=CARTESIAN_POINT('Ctrl Pts',(169.726944191456,-1.26576460699429,339.754557132868));
#48924=CARTESIAN_POINT('Ctrl Pts',(169.719187081682,-1.13236884236745,339.786117828401));
#48925=CARTESIAN_POINT('Ctrl Pts',(169.711425826756,-0.99890179530943,339.81769538896));
#48926=CARTESIAN_POINT('Ctrl Pts',(169.703664571829,-0.864218783598727,
339.843660845948));
#48927=CARTESIAN_POINT('Ctrl Pts',(169.695903316903,-0.728830925740224,
339.863947835266));
#48928=CARTESIAN_POINT('Ctrl Pts',(169.688129646499,-0.593226491431694,
339.884267277155));
#48929=CARTESIAN_POINT('Ctrl Pts',(169.680355976094,-0.456915346697097,
339.898890057743));
#48930=CARTESIAN_POINT('Ctrl Pts',(169.672582305689,-0.320412783048802,
339.907801820669));
#48931=CARTESIAN_POINT('Ctrl Pts',(169.665170501512,-0.190264446579206,
339.916298738886));
#48932=CARTESIAN_POINT('Ctrl Pts',(169.657758697335,-0.0599423989477547,
339.919604362407));
#48933=CARTESIAN_POINT('Ctrl Pts',(169.650346893158,0.0701101812161591,
339.917750260535));
#48934=CARTESIAN_POINT('Ctrl Pts',(169.64257181438,0.206537025740678,339.915805283607));
#48935=CARTESIAN_POINT('Ctrl Pts',(169.634796735601,0.343098454126135,339.908175858945));
#48936=CARTESIAN_POINT('Ctrl Pts',(169.627021656823,0.479281933498523,339.894841355011));
#48937=CARTESIAN_POINT('Ctrl Pts',(169.619256145774,0.615297830429725,339.881523260033));
#48938=CARTESIAN_POINT('Ctrl Pts',(169.611490634725,0.750936318449167,339.862514092219));
#48939=CARTESIAN_POINT('Ctrl Pts',(169.603725123676,0.885684361606167,339.837845209813));
#48940=CARTESIAN_POINT('Ctrl Pts',(169.595967312154,1.02029880168614,339.813200786675));
#48941=CARTESIAN_POINT('Ctrl Pts',(169.588209500632,1.15402417187472,339.782907886328));
#48942=CARTESIAN_POINT('Ctrl Pts',(169.580451689109,1.28635241480442,339.747049665574));
#48943=CARTESIAN_POINT('Ctrl Pts',(169.572699715586,1.41858107653441,339.711218429268));
#48944=CARTESIAN_POINT('Ctrl Pts',(169.564947742063,1.54941432798192,339.669830310544));
#48945=CARTESIAN_POINT('Ctrl Pts',(169.557195768541,1.67835452039141,339.623019485832));
#48946=CARTESIAN_POINT('Ctrl Pts',(169.549447077983,1.80724010655317,339.576228485532));
#48947=CARTESIAN_POINT('Ctrl Pts',(169.541698387425,1.93423386157843,339.524019479968));
#48948=CARTESIAN_POINT('Ctrl Pts',(169.533949696868,2.05885373094771,339.466576359704));
#48949=CARTESIAN_POINT('Ctrl Pts',(169.52620261849,2.18344767211244,339.40914519096));
#48950=CARTESIAN_POINT('Ctrl Pts',(169.518455540112,2.30566835528164,339.346482237139));
#48951=CARTESIAN_POINT('Ctrl Pts',(169.510708461734,2.42505450470427,339.27881919596));
#48952=CARTESIAN_POINT('Ctrl Pts',(169.502961318429,2.54444165469767,339.211155587699));
#48953=CARTESIAN_POINT('Ctrl Pts',(169.495214175123,2.66099388350513,339.138492001224));
#48954=CARTESIAN_POINT('Ctrl Pts',(169.487467031817,2.77427564009967,339.061105481916));
#48955=CARTESIAN_POINT('Ctrl Pts',(169.479718146789,2.8875828648381,338.983701564476));
#48956=CARTESIAN_POINT('Ctrl Pts',(169.471969261761,2.997617831565,338.901572821748));
#48957=CARTESIAN_POINT('Ctrl Pts',(169.464220376733,3.10397536323157,338.815038663887));
#48958=CARTESIAN_POINT('Ctrl Pts',(169.456463266958,3.2104457838812,338.728412657776));
#48959=CARTESIAN_POINT('Ctrl Pts',(169.448706157183,3.31323066865106,338.637372142953));
#48960=CARTESIAN_POINT('Ctrl Pts',(169.440949047409,3.41195883332961,338.54227610191));
#48961=CARTESIAN_POINT('Ctrl Pts',(169.433187792482,3.51073975518256,338.447129244583));
#48962=CARTESIAN_POINT('Ctrl Pts',(169.425426537556,3.60545936765833,338.347922825373));
#48963=CARTESIAN_POINT('Ctrl Pts',(169.41766528263,3.6957852682207,338.245050741314));
#48964=CARTESIAN_POINT('Ctrl Pts',(169.409891612225,3.78625566078692,338.142014095446));
#48965=CARTESIAN_POINT('Ctrl Pts',(169.402117941821,3.87231805089456,338.035300371399));
#48966=CARTESIAN_POINT('Ctrl Pts',(169.394344271416,3.95368151216845,337.925335119749));
#48967=CARTESIAN_POINT('Ctrl Pts',(169.386932467239,4.03125748474596,337.820488777018));
#48968=CARTESIAN_POINT('Ctrl Pts',(169.379520663062,4.10456199193852,337.712687049428));
#48969=CARTESIAN_POINT('Ctrl Pts',(169.372108858885,4.17338175166202,337.602319699306));
#48970=CARTESIAN_POINT('Ctrl Pts',(169.364333780106,4.24557457281241,337.486542916587));
#48971=CARTESIAN_POINT('Ctrl Pts',(169.356558701328,4.3130600516395,337.367576778586));
#48972=CARTESIAN_POINT('Ctrl Pts',(169.348783622549,4.37554347769722,337.245841120222));
#48973=CARTESIAN_POINT('Ctrl Pts',(169.3410181115,4.43795001392124,337.124255265336));
#48974=CARTESIAN_POINT('Ctrl Pts',(169.333252600451,4.49536656796597,336.99990701559));
#48975=CARTESIAN_POINT('Ctrl Pts',(169.325487089402,4.54754187645625,336.873244763606));
#48976=CARTESIAN_POINT('Ctrl Pts',(169.31772927788,4.59966545297627,336.746708097613));
#48977=CARTESIAN_POINT('Ctrl Pts',(169.309971466358,4.64655797777329,336.617862354332));
#48978=CARTESIAN_POINT('Ctrl Pts',(169.302213654836,4.68801444018168,336.487179770958));
#48979=CARTESIAN_POINT('Ctrl Pts',(169.294461681313,4.72943970528746,336.356595530373));
#48980=CARTESIAN_POINT('Ctrl Pts',(169.28670970779,4.76543693284398,336.224177572134));
#48981=CARTESIAN_POINT('Ctrl Pts',(169.278957734266,4.79584964837816,336.090416990262));
#48982=CARTESIAN_POINT('Ctrl Pts',(169.271209043709,4.82624948410928,335.956713056075));
#48983=CARTESIAN_POINT('Ctrl Pts',(169.263460353151,4.85106942524451,335.821668009518));
#48984=CARTESIAN_POINT('Ctrl Pts',(169.255711662594,4.87020324192108,335.685786734256));
#48985=CARTESIAN_POINT('Ctrl Pts',(169.247964584216,4.88933307764727,335.549933730228));
#48986=CARTESIAN_POINT('Ctrl Pts',(169.240217505838,4.90277908760817,335.413245230375));
#48987=CARTESIAN_POINT('Ctrl Pts',(169.23247042746,4.91048648858074,335.276234516247));
#48988=CARTESIAN_POINT('Ctrl Pts',(169.224723284154,4.91819395414874,335.139222653837));
#48989=CARTESIAN_POINT('Ctrl Pts',(169.216976140848,4.92016269284566,335.001888962022));
#48990=CARTESIAN_POINT('Ctrl Pts',(169.209228997542,4.91638997638955,334.864749630106));
#48991=CARTESIAN_POINT('Ctrl Pts',(169.201480112514,4.91261641174668,334.727579466357));
#48992=CARTESIAN_POINT('Ctrl Pts',(169.193731227486,4.90309883414778,334.590604140107));
#48993=CARTESIAN_POINT('Ctrl Pts',(169.185982342458,4.88788657785546,334.454337224542));
#48994=CARTESIAN_POINT('Ctrl Pts',(169.178225232683,4.87265817511715,334.317925673865));
#48995=CARTESIAN_POINT('Ctrl Pts',(169.170468122909,4.85172306288239,334.182224424969));
#48996=CARTESIAN_POINT('Ctrl Pts',(169.162711013134,4.82518224811235,334.047739880599));
#48997=CARTESIAN_POINT('Ctrl Pts',(169.154949758208,4.79862725077952,333.913183471989));
#48998=CARTESIAN_POINT('Ctrl Pts',(169.147188503281,4.76646067371024,333.779845443206));
#48999=CARTESIAN_POINT('Ctrl Pts',(169.139427248355,4.72883387123818,333.648218478921));
#49000=CARTESIAN_POINT('Ctrl Pts',(169.131653577951,4.69114687814468,333.51638095439));
#49001=CARTESIAN_POINT('Ctrl Pts',(169.123879907546,4.64798232850219,333.386260335174));
#49002=CARTESIAN_POINT('Ctrl Pts',(169.116106237141,4.59954063991313,333.258331557303));
#49003=CARTESIAN_POINT('Ctrl Pts',(169.108694432964,4.55335392358308,333.136357894821));
#49004=CARTESIAN_POINT('Ctrl Pts',(169.101282628787,4.50237042605856,333.016376870382));
#49005=CARTESIAN_POINT('Ctrl Pts',(169.09387082461,4.44680248762131,332.8987787602));
#49006=CARTESIAN_POINT('Ctrl Pts',(169.086095745832,4.38851099899199,332.77541681633));
#49007=CARTESIAN_POINT('Ctrl Pts',(169.078320667054,4.324990100425,332.654287433897));
#49008=CARTESIAN_POINT('Ctrl Pts',(169.070545588275,4.25643335532864,332.535865637968));
#49009=CARTESIAN_POINT('Ctrl Pts',(169.062780077226,4.18796097367172,332.417589567599));
#49010=CARTESIAN_POINT('Ctrl Pts',(169.055014566177,4.11446526956193,332.302014789336));
#49011=CARTESIAN_POINT('Ctrl Pts',(169.047249055128,4.03618733289036,332.189595246888));
#49012=CARTESIAN_POINT('Ctrl Pts',(169.039491243606,3.95798700902063,332.077287168743));
#49013=CARTESIAN_POINT('Ctrl Pts',(169.031733432084,3.87501411055228,331.968128419376));
#49014=CARTESIAN_POINT('Ctrl Pts',(169.023975620561,3.78755480878344,331.862546951274));
#49015=CARTESIAN_POINT('Ctrl Pts',(169.016223647039,3.70016132291305,331.757044936575));
#49016=CARTESIAN_POINT('Ctrl Pts',(169.008471673515,3.60828840216793,331.655115144611));
#49017=CARTESIAN_POINT('Ctrl Pts',(169.000719699993,3.51226434067182,331.55715491726));
#49018=CARTESIAN_POINT('Ctrl Pts',(168.992971009435,3.4162809454227,331.459236176124));
#49019=CARTESIAN_POINT('Ctrl Pts',(168.985222318877,3.31615017902988,331.365283934538));
#49020=CARTESIAN_POINT('Ctrl Pts',(168.97747362832,3.21223912186442,331.275660744983));
#49021=CARTESIAN_POINT('Ctrl Pts',(168.969726549942,3.10834968426226,331.18605620228));
#49022=CARTESIAN_POINT('Ctrl Pts',(168.961979471564,3.00068181613677,331.100779175191));
#49023=CARTESIAN_POINT('Ctrl Pts',(168.954232393186,2.88963750054809,331.020153498195));
#49024=CARTESIAN_POINT('Ctrl Pts',(168.946485249881,2.77859225430122,330.939527145479));
#49025=CARTESIAN_POINT('Ctrl Pts',(168.938738106575,2.66417082044428,330.863552450261));
#49026=CARTESIAN_POINT('Ctrl Pts',(168.930990963269,2.54680579714443,330.792511046464));
#49027=CARTESIAN_POINT('Ctrl Pts',(168.923242078241,2.42941438769558,330.72145367105));
#49028=CARTESIAN_POINT('Ctrl Pts',(168.915493193213,2.3090784062545,330.655331996425));
#49029=CARTESIAN_POINT('Ctrl Pts',(168.907744308185,2.18625642507057,330.594382460274));
#49030=CARTESIAN_POINT('Ctrl Pts',(168.89998719841,2.06330407936667,330.533368231656));
#49031=CARTESIAN_POINT('Ctrl Pts',(168.892230088635,1.93786081362365,330.477537281851));
#49032=CARTESIAN_POINT('Ctrl Pts',(168.884472978861,1.81040713337798,330.427078715535));
#49033=CARTESIAN_POINT('Ctrl Pts',(168.876711723934,1.68288534596079,330.376593185774));
#49034=CARTESIAN_POINT('Ctrl Pts',(168.868950469008,1.55335137234527,330.331485888366));
#49035=CARTESIAN_POINT('Ctrl Pts',(168.861189214082,1.42230142809693,330.291896166169));
#49036=CARTESIAN_POINT('Ctrl Pts',(168.853415543678,1.29104184664697,330.252243113319));
#49037=CARTESIAN_POINT('Ctrl Pts',(168.845641873273,1.158261827354,330.218125370611));
#49038=CARTESIAN_POINT('Ctrl Pts',(168.837868202868,1.0244692115225,330.189631417745));
#49039=CARTESIAN_POINT('Ctrl Pts',(168.830456398691,0.89690467414496,330.162463865241));
#49040=CARTESIAN_POINT('Ctrl Pts',(168.823044594514,0.768419975064949,330.14040835916));
#49041=CARTESIAN_POINT('Ctrl Pts',(168.815632790337,0.639458215387634,330.123497538884));
#49042=CARTESIAN_POINT('Ctrl Pts',(168.807857711558,0.504175655712586,330.105757868931));
#49043=CARTESIAN_POINT('Ctrl Pts',(168.80008263278,0.367940570799299,330.093623888458));
#49044=CARTESIAN_POINT('Ctrl Pts',(168.792307554001,0.231257167627652,330.087189889186));
#49045=CARTESIAN_POINT('Ctrl Pts',(168.784542042952,0.0947419620855077,
330.080763807359));
#49046=CARTESIAN_POINT('Ctrl Pts',(168.776776531903,-0.0422200773122219,
330.080023768709));
#49047=CARTESIAN_POINT('Ctrl Pts',(168.769011020854,-0.179116752042777,
330.085012690592));
#49048=CARTESIAN_POINT('Ctrl Pts',(168.761253209332,-0.31587769332189,330.089996665945));
#49049=CARTESIAN_POINT('Ctrl Pts',(168.75349539781,-0.452573010809157,330.100698283606));
#49050=CARTESIAN_POINT('Ctrl Pts',(168.745737586288,-0.588687966419104,
330.117108485672));
#49051=CARTESIAN_POINT('Ctrl Pts',(168.737985612765,-0.724700491208062,
330.133506338541));
#49052=CARTESIAN_POINT('Ctrl Pts',(168.730233639242,-0.860133136929075,
330.155604178457));
#49053=CARTESIAN_POINT('Ctrl Pts',(168.722481665719,-0.994474111533304,
330.183340960376));
#49054=CARTESIAN_POINT('Ctrl Pts',(168.714732975161,-1.12875819265524,330.211065995752));
#49055=CARTESIAN_POINT('Ctrl Pts',(168.706984284604,-1.26195114018523,330.244425144507));
#49056=CARTESIAN_POINT('Ctrl Pts',(168.699235594046,-1.39354942775684,330.283305918877));
#49057=CARTESIAN_POINT('Ctrl Pts',(168.691488515668,-1.52512033520574,330.322178603777));
#49058=CARTESIAN_POINT('Ctrl Pts',(168.68374143729,-1.65509686801433,330.366570518525));
#49059=CARTESIAN_POINT('Ctrl Pts',(168.675994358913,-1.7829891707603,330.416318872407));
#49060=CARTESIAN_POINT('Ctrl Pts',(168.668247215607,-1.91088254536701,330.466067643229));
#49061=CARTESIAN_POINT('Ctrl Pts',(168.660500072301,-2.0366912907855,330.521172801024));
#49062=CARTESIAN_POINT('Ctrl Pts',(168.652752928995,-2.15994447135232,330.58142297304));
#49063=CARTESIAN_POINT('Ctrl Pts',(168.645004043967,-2.2832253618506,330.641686690574));
#49064=CARTESIAN_POINT('Ctrl Pts',(168.637255158939,-2.40394919312187,330.707097552424));
#49065=CARTESIAN_POINT('Ctrl Pts',(168.629506273911,-2.52166897991473,330.777397885399));
#49066=CARTESIAN_POINT('Ctrl Pts',(168.621749164136,-2.63951371570567,330.847772835874));
#49067=CARTESIAN_POINT('Ctrl Pts',(168.613992054361,-2.75434770152443,330.923047423733));
#49068=CARTESIAN_POINT('Ctrl Pts',(168.606234944587,-2.86575188609779,331.002919917011));
#49069=CARTESIAN_POINT('Ctrl Pts',(168.59847368966,-2.97721560150531,331.082835091596));
#49070=CARTESIAN_POINT('Ctrl Pts',(168.590712434734,-3.08524555599869,331.167352826612));
#49071=CARTESIAN_POINT('Ctrl Pts',(168.582951179808,-3.18945604248086,331.25613125022));
#49072=CARTESIAN_POINT('Ctrl Pts',(168.575177509403,-3.29383323177945,331.345051690373));
#49073=CARTESIAN_POINT('Ctrl Pts',(168.567403838999,-3.39437845684813,331.438246173079));
#49074=CARTESIAN_POINT('Ctrl Pts',(168.559630168594,-3.49074249114981,331.535335525194));
#49075=CARTESIAN_POINT('Ctrl Pts',(168.552218364417,-3.58262075647029,331.62790534461));
#49076=CARTESIAN_POINT('Ctrl Pts',(168.54480656024,-3.67069814518832,331.72401536928));
#49077=CARTESIAN_POINT('Ctrl Pts',(168.537394756063,-3.75470742271936,331.823310649076));
#49078=CARTESIAN_POINT('Ctrl Pts',(168.529666927997,-3.8422986808223,331.926839672733));
#49079=CARTESIAN_POINT('Ctrl Pts',(168.521939099932,-3.92575403084158,332.034170690932));
#49080=CARTESIAN_POINT('Ctrl Pts',(168.514211271866,-4.00472205233481,332.144937067936));
#49081=CARTESIAN_POINT('Ctrl Pts',(168.506495931509,-4.08356246622131,332.25552445309));
#49082=CARTESIAN_POINT('Ctrl Pts',(168.498780591152,-4.15792976324953,332.369535823212));
#49083=CARTESIAN_POINT('Ctrl Pts',(168.491065250795,-4.22751147335056,332.486570111344));
#49084=CARTESIAN_POINT('Ctrl Pts',(168.483357140694,-4.29702797653107,332.603494723448));
#49085=CARTESIAN_POINT('Ctrl Pts',(168.475649030593,-4.36176761093657,332.723436281665));
#49086=CARTESIAN_POINT('Ctrl Pts',(168.467940920492,-4.42145994481158,332.845963087845));
#49087=CARTESIAN_POINT('Ctrl Pts',(168.460238312771,-4.48110966773853,332.968402429136));
#49088=CARTESIAN_POINT('Ctrl Pts',(168.45253570505,-4.5357190847303,333.093422992699));
#49089=CARTESIAN_POINT('Ctrl Pts',(168.444833097328,-4.58506288522917,333.220567112534));
#49090=CARTESIAN_POINT('Ctrl Pts',(168.437134268494,-4.63438247774049,333.347648855674));
#49091=CARTESIAN_POINT('Ctrl Pts',(168.429435439659,-4.67844145156572,333.476851713406));
#49092=CARTESIAN_POINT('Ctrl Pts',(168.421736610824,-4.71706216808615,333.607697028334));
#49093=CARTESIAN_POINT('Ctrl Pts',(168.414038565493,-4.7556789542093,333.738529027246));
#49094=CARTESIAN_POINT('Ctrl Pts',(168.406340520161,-4.7888584645556,333.871002773357));
#49095=CARTESIAN_POINT('Ctrl Pts',(168.39864247483,-4.8164726598156,334.004623598959));
#49096=CARTESIAN_POINT('Ctrl Pts',(168.390944917703,-4.84408510380512,334.138235950435));
#49097=CARTESIAN_POINT('Ctrl Pts',(168.383247360575,-4.86613286024566,334.272994847622));
#49098=CARTESIAN_POINT('Ctrl Pts',(168.375549803448,-4.88253898479343,334.408395297118));
#49099=CARTESIAN_POINT('Ctrl Pts',(168.36784884037,-4.89895236858437,334.543855657458));
#49100=CARTESIAN_POINT('Ctrl Pts',(168.360147877293,-4.90971909262329,334.679957743058));
#49101=CARTESIAN_POINT('Ctrl Pts',(168.352446914215,-4.91481407985134,334.816191341349));
#49102=CARTESIAN_POINT('Ctrl Pts',(168.34890373498,-4.91715826106239,334.878871820639));
#49103=CARTESIAN_POINT('Ctrl Pts',(168.345360555744,-4.91830252956736,334.941580112913));
#49104=CARTESIAN_POINT('Ctrl Pts',(168.341817376508,-4.91824814939254,335.004266555616));
#49105=CARTESIAN_POINT('',(166.591817376549,-4.91824999464061,335.000229603117));
#49106=CARTESIAN_POINT('Ctrl Pts',(168.341817376469,-4.91824814939194,335.004266556313));
#49107=CARTESIAN_POINT('Ctrl Pts',(168.332452975502,-4.91810442596984,335.169942901091));
#49108=CARTESIAN_POINT('Ctrl Pts',(168.323088574534,-4.90958550624772,335.335252813395));
#49109=CARTESIAN_POINT('Ctrl Pts',(168.313724173567,-4.89282474710446,335.499448752749));
#49110=CARTESIAN_POINT('Ctrl Pts',(168.304233401961,-4.87583780500957,335.665860482084));
#49111=CARTESIAN_POINT('Ctrl Pts',(168.294742630354,-4.85038513728699,335.831127973892));
#49112=CARTESIAN_POINT('Ctrl Pts',(168.285251858748,-4.81665466580062,335.994495295575));
#49113=CARTESIAN_POINT('Ctrl Pts',(168.276553479761,-4.78574038016243,336.144222940162));
#49114=CARTESIAN_POINT('Ctrl Pts',(168.267855100775,-4.74787344150753,336.292354748403));
#49115=CARTESIAN_POINT('Ctrl Pts',(168.259156721789,-4.70323347838745,336.438324688753));
#49116=CARTESIAN_POINT('Ctrl Pts',(168.251381643011,-4.66333187942603,336.568800469044));
#49117=CARTESIAN_POINT('Ctrl Pts',(168.243606564232,-4.61793368071984,336.697820759686));
#49118=CARTESIAN_POINT('Ctrl Pts',(168.235831485454,-4.56716195508446,336.824887596135));
#49119=CARTESIAN_POINT('Ctrl Pts',(168.228065974405,-4.51645270728983,336.951798068753));
#49120=CARTESIAN_POINT('Ctrl Pts',(168.220300463356,-4.46038323312446,337.076759510645));
#49121=CARTESIAN_POINT('Ctrl Pts',(168.212534952307,-4.3991266742254,337.199287968098));
#49122=CARTESIAN_POINT('Ctrl Pts',(168.204777140785,-4.33793085138285,337.321694938227));
#49123=CARTESIAN_POINT('Ctrl Pts',(168.197019329263,-4.2715583523474,337.441673377187));
#49124=CARTESIAN_POINT('Ctrl Pts',(168.18926151774,-4.20023067573399,337.558758553112));
#49125=CARTESIAN_POINT('Ctrl Pts',(168.181509544217,-4.12895667545897,337.675755618729));
#49126=CARTESIAN_POINT('Ctrl Pts',(168.173757570694,-4.05273512239202,337.7898634226));
#49127=CARTESIAN_POINT('Ctrl Pts',(168.166005597171,-3.97183361027012,337.900641452305));
#49128=CARTESIAN_POINT('Ctrl Pts',(168.158256906614,-3.8909663599867,338.011372567448));
#49129=CARTESIAN_POINT('Ctrl Pts',(168.150508216056,-3.80542332268452,338.118776398137));
#49130=CARTESIAN_POINT('Ctrl Pts',(168.142759525498,-3.71551548780974,338.222441267478));
#49131=CARTESIAN_POINT('Ctrl Pts',(168.135012447121,-3.625626359011,338.326084568477));
#49132=CARTESIAN_POINT('Ctrl Pts',(168.127265368743,-3.53137449491998,338.425990160369));
#49133=CARTESIAN_POINT('Ctrl Pts',(168.119518290365,-3.43311100394988,338.521779649135));
#49134=CARTESIAN_POINT('Ctrl Pts',(168.111771147059,-3.33484668943716,338.617569940708));
#49135=CARTESIAN_POINT('Ctrl Pts',(168.104024003753,-3.232570960876,338.709243787506));
#49136=CARTESIAN_POINT('Ctrl Pts',(168.096276860448,-3.12667130480761,338.796460142579));
#49137=CARTESIAN_POINT('Ctrl Pts',(168.088527975419,-3.02074784024828,338.883696105741));
#49138=CARTESIAN_POINT('Ctrl Pts',(168.080779090391,-2.91119912861033,338.966472334594));
#49139=CARTESIAN_POINT('Ctrl Pts',(168.073030205363,-2.79844487379361,339.044488762605));
#49140=CARTESIAN_POINT('Ctrl Pts',(168.065273095589,-2.68557094044573,339.122587998059));
#49141=CARTESIAN_POINT('Ctrl Pts',(168.057515985814,-2.56948498925305,339.195917117869));
#49142=CARTESIAN_POINT('Ctrl Pts',(168.049758876039,-2.45063525086603,339.264219732813));
#49143=CARTESIAN_POINT('Ctrl Pts',(168.041997621113,-2.33172200297893,339.332558846491));
#49144=CARTESIAN_POINT('Ctrl Pts',(168.034236366187,-2.21004237165713,339.395865922884));
#49145=CARTESIAN_POINT('Ctrl Pts',(168.026475111261,-2.0860673061139,339.453931550536));
#49146=CARTESIAN_POINT('Ctrl Pts',(168.018701440856,-1.96189392086918,339.51209006427));
#49147=CARTESIAN_POINT('Ctrl Pts',(168.010927770451,-1.83541812455816,339.564990223423));
#49148=CARTESIAN_POINT('Ctrl Pts',(168.003154100047,-1.70712970206209,339.612471272847));
#49149=CARTESIAN_POINT('Ctrl Pts',(167.995742295869,-1.58481313649632,339.657742067998));
#49150=CARTESIAN_POINT('Ctrl Pts',(167.988330491692,-1.46084917617341,339.69808682958));
#49151=CARTESIAN_POINT('Ctrl Pts',(167.980918687515,-1.33567159055165,339.733409391199));
#49152=CARTESIAN_POINT('Ctrl Pts',(167.973143608737,-1.2043586785751,339.770463216783));
#49153=CARTESIAN_POINT('Ctrl Pts',(167.965368529958,-1.07129519337819,339.802107185413));
#49154=CARTESIAN_POINT('Ctrl Pts',(167.95759345118,-0.93696648573386,339.828175314455));
#49155=CARTESIAN_POINT('Ctrl Pts',(167.949827940131,-0.802803078116049,
339.854211365005));
#49156=CARTESIAN_POINT('Ctrl Pts',(167.942062429082,-0.667377925956069,
339.874685154483));
#49157=CARTESIAN_POINT('Ctrl Pts',(167.934296918033,-0.531191693133408,
339.889480386263));
#49158=CARTESIAN_POINT('Ctrl Pts',(167.926539106511,-0.395140489357063,
339.904260948526));
#49159=CARTESIAN_POINT('Ctrl Pts',(167.918781294988,-0.258330092726615,
339.913374115775));
#49160=CARTESIAN_POINT('Ctrl Pts',(167.911023483466,-0.121271171791649,
339.91675465784));
#49161=CARTESIAN_POINT('Ctrl Pts',(167.903271509943,0.0156846079588316,
339.92013265594));
#49162=CARTESIAN_POINT('Ctrl Pts',(167.89551953642,0.152888150572768,339.917786606029));
#49163=CARTESIAN_POINT('Ctrl Pts',(167.887767562897,0.289824209434218,339.909703146844));
#49164=CARTESIAN_POINT('Ctrl Pts',(167.880018872339,0.426702275793465,339.901623111007));
#49165=CARTESIAN_POINT('Ctrl Pts',(167.872270181782,0.563312694322252,339.887810521575));
#49166=CARTESIAN_POINT('Ctrl Pts',(167.864521491224,0.6991409829054,339.868304114219));
#49167=CARTESIAN_POINT('Ctrl Pts',(167.856774412846,0.834941011278671,339.848801765334));
#49168=CARTESIAN_POINT('Ctrl Pts',(167.849027334469,0.969958846723169,339.823608010398));
#49169=CARTESIAN_POINT('Ctrl Pts',(167.841280256091,1.10368628472728,339.792813333253));
#49170=CARTESIAN_POINT('Ctrl Pts',(167.833533112785,1.23741484349603,339.762018398018));
#49171=CARTESIAN_POINT('Ctrl Pts',(167.825785969479,1.36985260234822,339.72562253466));
#49172=CARTESIAN_POINT('Ctrl Pts',(167.818038826173,1.50050307642865,339.683767028806));
#49173=CARTESIAN_POINT('Ctrl Pts',(167.810289941145,1.63118292350944,339.641902112945));
#49174=CARTESIAN_POINT('Ctrl Pts',(167.802541056117,1.76007431407625,339.594575231341));
#49175=CARTESIAN_POINT('Ctrl Pts',(167.794792171089,1.88669778991771,339.541976938737));
#49176=CARTESIAN_POINT('Ctrl Pts',(167.787035061314,2.01345566522474,339.489322817762));
#49177=CARTESIAN_POINT('Ctrl Pts',(167.779277951539,2.13794045568189,339.431386259172));
#49178=CARTESIAN_POINT('Ctrl Pts',(167.771520841765,2.2596939947986,339.368405442764));
#49179=CARTESIAN_POINT('Ctrl Pts',(167.763759586839,2.38151259511362,339.305390971421));
#49180=CARTESIAN_POINT('Ctrl Pts',(167.755998331912,2.50059669673383,339.237327065117));
#49181=CARTESIAN_POINT('Ctrl Pts',(167.748237076986,2.61651534345585,339.164496430538));
#49182=CARTESIAN_POINT('Ctrl Pts',(167.740463406582,2.73261942223481,339.091549290678));
#49183=CARTESIAN_POINT('Ctrl Pts',(167.732689736177,2.84554760520566,339.013820406845));
#49184=CARTESIAN_POINT('Ctrl Pts',(167.724916065772,2.95489965923097,338.93163465576));
#49185=CARTESIAN_POINT('Ctrl Pts',(167.717504261595,3.05916134883301,338.853274671161));
#49186=CARTESIAN_POINT('Ctrl Pts',(167.710092457418,3.16017213154598,338.770863597745));
#49187=CARTESIAN_POINT('Ctrl Pts',(167.702680653241,3.2576164014527,338.68471416035));
#49188=CARTESIAN_POINT('Ctrl Pts',(167.694905574463,3.35983670529898,338.594342282403));
#49189=CARTESIAN_POINT('Ctrl Pts',(167.687130495684,3.45845508063529,338.499570726072));
#49190=CARTESIAN_POINT('Ctrl Pts',(167.679355416906,3.55306929797189,338.40071781045));
#49191=CARTESIAN_POINT('Ctrl Pts',(167.671589905857,3.6475670864906,338.301986539634));
#49192=CARTESIAN_POINT('Ctrl Pts',(167.663824394808,3.73807025337985,338.199184182286));
#49193=CARTESIAN_POINT('Ctrl Pts',(167.656058883759,3.82421006437014,338.092668822566));
#49194=CARTESIAN_POINT('Ctrl Pts',(167.648301072236,3.91026446748709,337.986259073134));
#49195=CARTESIAN_POINT('Ctrl Pts',(167.640543260714,3.99196388004277,337.876143949598));
#49196=CARTESIAN_POINT('Ctrl Pts',(167.632785449192,4.06897709654346,337.762717584247));
#49197=CARTESIAN_POINT('Ctrl Pts',(167.625033475669,4.14593235815642,337.649376575832));
#49198=CARTESIAN_POINT('Ctrl Pts',(167.617281502146,4.21820822438157,337.532729607516));
#49199=CARTESIAN_POINT('Ctrl Pts',(167.609529528623,4.28551462993841,337.413202730623));
#49200=CARTESIAN_POINT('Ctrl Pts',(167.601780838065,4.35279253119258,337.293726473432));
#49201=CARTESIAN_POINT('Ctrl Pts',(167.594032147508,4.41510496623061,337.171373073328));
#49202=CARTESIAN_POINT('Ctrl Pts',(167.58628345695,4.47220609291166,337.046596131391));
#49203=CARTESIAN_POINT('Ctrl Pts',(167.578536378572,4.52929533922637,336.921845150339));
#49204=CARTESIAN_POINT('Ctrl Pts',(167.570789300194,4.58117527129683,336.794671985621));
#49205=CARTESIAN_POINT('Ctrl Pts',(167.563042221817,4.62764696029223,336.665552963252));
#49206=CARTESIAN_POINT('Ctrl Pts',(167.555295078511,4.67411903876512,336.536432858741));
#49207=CARTESIAN_POINT('Ctrl Pts',(167.547547935205,4.71518265138769,336.40536723183));
#49208=CARTESIAN_POINT('Ctrl Pts',(167.539800791899,4.75068793181425,336.272850044983));
#49209=CARTESIAN_POINT('Ctrl Pts',(167.532051906871,4.78620119458164,336.14030306546));
#49210=CARTESIAN_POINT('Ctrl Pts',(167.524303021843,4.81615353738773,336.006304254103));
#49211=CARTESIAN_POINT('Ctrl Pts',(167.516554136815,4.84044573943344,335.871359917658));
#49212=CARTESIAN_POINT('Ctrl Pts',(167.50879702704,4.8647637254734,335.736272349899));
#49213=CARTESIAN_POINT('Ctrl Pts',(167.501039917265,4.88340950038487,335.600237637585));
#49214=CARTESIAN_POINT('Ctrl Pts',(167.493282807491,4.89633541446301,335.463769955447));
#49215=CARTESIAN_POINT('Ctrl Pts',(167.485521552565,4.90926823573635,335.327229349343));
#49216=CARTESIAN_POINT('Ctrl Pts',(167.477760297638,4.91647508527644,335.190255702535));
#49217=CARTESIAN_POINT('Ctrl Pts',(167.469999042712,4.91796048203675,335.053364404099));
#49218=CARTESIAN_POINT('Ctrl Pts',(167.462225372308,4.91944825494779,334.916254124198));
#49219=CARTESIAN_POINT('Ctrl Pts',(167.454451701903,4.91519629788326,334.779226846796));
#49220=CARTESIAN_POINT('Ctrl Pts',(167.446678031498,4.90526121749234,334.642794945913));
#49221=CARTESIAN_POINT('Ctrl Pts',(167.439266227321,4.89578861748388,334.512713982839));
#49222=CARTESIAN_POINT('Ctrl Pts',(167.431854423144,4.88115011820902,334.383174500114));
#49223=CARTESIAN_POINT('Ctrl Pts',(167.424442618967,4.86143790418352,334.25461113084));
#49224=CARTESIAN_POINT('Ctrl Pts',(167.416667540189,4.84075953582891,334.119746487866));
#49225=CARTESIAN_POINT('Ctrl Pts',(167.40889246141,4.81443217386325,333.985529864994));
#49226=CARTESIAN_POINT('Ctrl Pts',(167.401117382632,4.78250583014581,333.852471766308));
#49227=CARTESIAN_POINT('Ctrl Pts',(167.393351871583,4.75061877382685,333.719577404083));
#49228=CARTESIAN_POINT('Ctrl Pts',(167.385586360534,4.71314653501564,333.587839105886));
#49229=CARTESIAN_POINT('Ctrl Pts',(167.377820849485,4.67019069104927,333.457760728117));
#49230=CARTESIAN_POINT('Ctrl Pts',(167.370063037962,4.62727743792727,333.327811323439));
#49231=CARTESIAN_POINT('Ctrl Pts',(167.36230522644,4.57889152138716,333.19951893269));
#49232=CARTESIAN_POINT('Ctrl Pts',(167.354547414918,4.5251851413841,333.073375361235));
#49233=CARTESIAN_POINT('Ctrl Pts',(167.346795441395,4.47151917713512,332.947326716817));
#49234=CARTESIAN_POINT('Ctrl Pts',(167.339043467872,4.41254087132668,332.823424031213));
#49235=CARTESIAN_POINT('Ctrl Pts',(167.331291494349,4.3484515286403,332.702141787323));
#49236=CARTESIAN_POINT('Ctrl Pts',(167.323542803791,4.28438932782858,332.580910906536));
#49237=CARTESIAN_POINT('Ctrl Pts',(167.315794113234,4.21522057747143,332.462298605102));
#49238=CARTESIAN_POINT('Ctrl Pts',(167.308045422676,4.14119368110637,332.346757086495));
#49239=CARTESIAN_POINT('Ctrl Pts',(167.300298344298,4.0671821866554,332.231239607266));
#49240=CARTESIAN_POINT('Ctrl Pts',(167.292551265921,3.9883147674373,332.118791968955));
#49241=CARTESIAN_POINT('Ctrl Pts',(167.284804187543,3.90488432435392,332.009839222397));
#49242=CARTESIAN_POINT('Ctrl Pts',(167.277057044237,3.82145318204311,331.90088556271));
#49243=CARTESIAN_POINT('Ctrl Pts',(167.269309900931,3.73345917723024,331.795427163536));
#49244=CARTESIAN_POINT('Ctrl Pts',(167.261562757625,3.64123659221255,331.693857362116));
#49245=CARTESIAN_POINT('Ctrl Pts',(167.253813872597,3.54899327359987,331.592264725649));
#49246=CARTESIAN_POINT('Ctrl Pts',(167.246064987569,3.45251974574801,331.494562715903));
#49247=CARTESIAN_POINT('Ctrl Pts',(167.238316102541,3.35218807873302,331.401108761396));
#49248=CARTESIAN_POINT('Ctrl Pts',(167.230558992766,3.25174991864996,331.307555613896));
#49249=CARTESIAN_POINT('Ctrl Pts',(167.222801882992,3.1474457255907,331.21825979548));
#49250=CARTESIAN_POINT('Ctrl Pts',(167.215044773217,3.039682094067,331.13353962525));
#49251=CARTESIAN_POINT('Ctrl Pts',(167.207283518291,2.93186087710422,331.048774183271));
#49252=CARTESIAN_POINT('Ctrl Pts',(167.199522263364,2.82057685511416,330.968589489907));
#49253=CARTESIAN_POINT('Ctrl Pts',(167.191761008438,2.70626587523024,330.893260651677));
#49254=CARTESIAN_POINT('Ctrl Pts',(167.183987338034,2.59177203503238,330.817811311855));
#49255=CARTESIAN_POINT('Ctrl Pts',(167.176213667629,2.4742418961718,330.747233550837));
#49256=CARTESIAN_POINT('Ctrl Pts',(167.168439997224,2.35413695799786,330.681757041864));
#49257=CARTESIAN_POINT('Ctrl Pts',(167.161028193047,2.23962293359131,330.619328480137));
#49258=CARTESIAN_POINT('Ctrl Pts',(167.15361638887,2.12276868704919,330.561537059399));
#49259=CARTESIAN_POINT('Ctrl Pts',(167.146204584693,2.00398959695076,330.508540464636));
#49260=CARTESIAN_POINT('Ctrl Pts',(167.138429505915,1.87938878982209,330.452946348894));
#49261=CARTESIAN_POINT('Ctrl Pts',(167.130654427136,1.75227592203912,330.402453273256));
#49262=CARTESIAN_POINT('Ctrl Pts',(167.122879348358,1.62310735166507,330.357295444736));
#49263=CARTESIAN_POINT('Ctrl Pts',(167.115113837309,1.49409773144018,330.312193185798));
#49264=CARTESIAN_POINT('Ctrl Pts',(167.10734832626,1.36303780739623,330.272413238554));
#49265=CARTESIAN_POINT('Ctrl Pts',(167.099582815211,1.23040625245394,330.238142850061));
#49266=CARTESIAN_POINT('Ctrl Pts',(167.091825003689,1.09790620208455,330.203906440759));
#49267=CARTESIAN_POINT('Ctrl Pts',(167.084067192166,0.963837997882614,330.175168816196));
#49268=CARTESIAN_POINT('Ctrl Pts',(167.076309380644,0.828697573599784,330.152068132285));
#49269=CARTESIAN_POINT('Ctrl Pts',(167.068557407121,0.693658846771776,330.128984832371));
#49270=CARTESIAN_POINT('Ctrl Pts',(167.060805433598,0.557549889651754,330.111530095257));
#49271=CARTESIAN_POINT('Ctrl Pts',(167.053053460075,0.420878642548264,330.099791409466));
#49272=CARTESIAN_POINT('Ctrl Pts',(167.045304769518,0.284265275799041,330.088057695015));
#49273=CARTESIAN_POINT('Ctrl Pts',(167.03755607896,0.147090481320391,330.082035250562));
#49274=CARTESIAN_POINT('Ctrl Pts',(167.029807388402,0.00986895206824741,
330.081759901521));
#49275=CARTESIAN_POINT('Ctrl Pts',(167.022060310024,-0.127324027098686,
330.081484609769));
#49276=CARTESIAN_POINT('Ctrl Pts',(167.014313231647,-0.264563331070165,
330.086954035818));
#49277=CARTESIAN_POINT('Ctrl Pts',(167.006566153269,-0.401333020046105,
330.098151892447));
#49278=CARTESIAN_POINT('Ctrl Pts',(166.998819009963,-0.538103855283608,
330.109349842925));
#49279=CARTESIAN_POINT('Ctrl Pts',(166.991071866657,-0.674404678104511,
330.126276287847));
#49280=CARTESIAN_POINT('Ctrl Pts',(166.983324723351,-0.809723823498836,
330.148862979449));
#49281=CARTESIAN_POINT('Ctrl Pts',(166.975575838323,-0.945073391509929,
330.171454749019));
#49282=CARTESIAN_POINT('Ctrl Pts',(166.967826953295,-1.07944045745707,330.199709233148));
#49283=CARTESIAN_POINT('Ctrl Pts',(166.960078068267,-1.21232310360615,330.233506975253));
#49284=CARTESIAN_POINT('Ctrl Pts',(166.952320958492,-1.34534679276888,330.26734059063));
#49285=CARTESIAN_POINT('Ctrl Pts',(166.944563848718,-1.4768825353558,330.306729120668));
#49286=CARTESIAN_POINT('Ctrl Pts',(166.936806738943,-1.60644261842071,330.351502912099));
#49287=CARTESIAN_POINT('Ctrl Pts',(166.929045484017,-1.73607193425144,330.396300629213));
#49288=CARTESIAN_POINT('Ctrl Pts',(166.921284229091,-1.86372312334087,330.446489198869));
#49289=CARTESIAN_POINT('Ctrl Pts',(166.913522974164,-1.98892898085688,330.501850983837));
#49290=CARTESIAN_POINT('Ctrl Pts',(166.90574930376,-2.1143351269404,330.557301329619));
#49291=CARTESIAN_POINT('Ctrl Pts',(166.897975633355,-2.23728777390671,330.617941254544));
#49292=CARTESIAN_POINT('Ctrl Pts',(166.89020196295,-2.35734404084748,330.683506963335));
#49293=CARTESIAN_POINT('Ctrl Pts',(166.882790158773,-2.47181165967819,330.746020572607));
#49294=CARTESIAN_POINT('Ctrl Pts',(166.875378354596,-2.58364623620141,330.813011547668));
#49295=CARTESIAN_POINT('Ctrl Pts',(166.867966550419,-2.69249038456561,330.884215920202));
#49296=CARTESIAN_POINT('Ctrl Pts',(166.860201822508,-2.80651730386932,330.95881079152));
#49297=CARTESIAN_POINT('Ctrl Pts',(166.852437094596,-2.91762449540572,331.038267340492));
#49298=CARTESIAN_POINT('Ctrl Pts',(166.844672366685,-3.02536873599656,331.122329684752));
#49299=CARTESIAN_POINT('Ctrl Pts',(166.836917201062,-3.13298028919917,331.206288505957));
#49300=CARTESIAN_POINT('Ctrl Pts',(166.829162035438,-3.23723682527444,331.294841598457));
#49301=CARTESIAN_POINT('Ctrl Pts',(166.821406869815,-3.33772247606863,331.387688865111));
#49302=CARTESIAN_POINT('Ctrl Pts',(166.81365938716,-3.4381085766876,331.480444148864));
#49303=CARTESIAN_POINT('Ctrl Pts',(166.805911904505,-3.53473093998224,331.577484876766));
#49304=CARTESIAN_POINT('Ctrl Pts',(166.798164421851,-3.62720559656636,331.678469837148));
#49305=CARTESIAN_POINT('Ctrl Pts',(166.790422749604,-3.71961089959684,331.779379061472));
#49306=CARTESIAN_POINT('Ctrl Pts',(166.782681077357,-3.80787442356198,331.88422634268));
#49307=CARTESIAN_POINT('Ctrl Pts',(166.774939405109,-3.89164828173828,331.992632926671));
#49308=CARTESIAN_POINT('Ctrl Pts',(166.767200970691,-3.97538710285986,332.10099417137));
#49309=CARTESIAN_POINT('Ctrl Pts',(166.759462536272,-4.05463975335757,332.212911448724));
#49310=CARTESIAN_POINT('Ctrl Pts',(166.751724101854,-4.12909812191281,332.327972350046));
#49311=CARTESIAN_POINT('Ctrl Pts',(166.743987234331,-4.20354141396952,332.443009953578));
#49312=CARTESIAN_POINT('Ctrl Pts',(166.736250366808,-4.27319214202715,332.561189586087));
#49313=CARTESIAN_POINT('Ctrl Pts',(166.728513499286,-4.33778533951076,332.682069584559));
#49314=CARTESIAN_POINT('Ctrl Pts',(166.720776511659,-4.4023795397099,332.802951459517));
#49315=CARTESIAN_POINT('Ctrl Pts',(166.713039524033,-4.46191586819535,332.926533438142));
#49316=CARTESIAN_POINT('Ctrl Pts',(166.705302536406,-4.51617537083237,333.052349342827));
#49317=CARTESIAN_POINT('Ctrl Pts',(166.697563741948,-4.57044754478014,333.178194629507));
#49318=CARTESIAN_POINT('Ctrl Pts',(166.68982494749,-4.61944028570309,333.306274520356));
#49319=CARTESIAN_POINT('Ctrl Pts',(166.682086153033,-4.66298298548585,333.436103347542));
#49320=CARTESIAN_POINT('Ctrl Pts',(166.674339136885,-4.70657194500147,333.566070104781));
#49321=CARTESIAN_POINT('Ctrl Pts',(166.666592120738,-4.74469917321079,333.697789137461));
#49322=CARTESIAN_POINT('Ctrl Pts',(166.65884510459,-4.77724397403381,333.830759616222));
#49323=CARTESIAN_POINT('Ctrl Pts',(166.651093865666,-4.80980651451597,333.9638025751));
#49324=CARTESIAN_POINT('Ctrl Pts',(166.643342626742,-4.83678048788805,334.098097955067));
#49325=CARTESIAN_POINT('Ctrl Pts',(166.635591387817,-4.85809665151938,334.233136265692));
#49326=CARTESIAN_POINT('Ctrl Pts',(166.627827928584,-4.87944642140552,334.368387472595));
#49327=CARTESIAN_POINT('Ctrl Pts',(166.620064469351,-4.89512051445102,334.504383560939));
#49328=CARTESIAN_POINT('Ctrl Pts',(166.612301010117,-4.90510166638276,334.640610649923));
#49329=CARTESIAN_POINT('Ctrl Pts',(166.605473132261,-4.91387998081784,334.760420891251));
#49330=CARTESIAN_POINT('Ctrl Pts',(166.598645254405,-4.91825558830559,334.880409615298));
#49331=CARTESIAN_POINT('Ctrl Pts',(166.591817376549,-4.91824999464062,335.000229603117));
#49332=CARTESIAN_POINT('',(164.841817376508,-4.91683592588205,334.995612015269));
#49333=CARTESIAN_POINT('Ctrl Pts',(166.591817376508,-4.91824999464058,335.000229603829));
#49334=CARTESIAN_POINT('Ctrl Pts',(166.591121089721,-4.91824942421341,335.012448491774));
#49335=CARTESIAN_POINT('Ctrl Pts',(166.590424802933,-4.91820331902207,335.02466725531));
#49336=CARTESIAN_POINT('Ctrl Pts',(166.589728516146,-4.91811168125916,335.036885676925));
#49337=CARTESIAN_POINT('Ctrl Pts',(166.581953437367,-4.91708840918464,335.173322547882));
#49338=CARTESIAN_POINT('Ctrl Pts',(166.574178358589,-4.91038172830435,335.30993240212));
#49339=CARTESIAN_POINT('Ctrl Pts',(166.56640327981,-4.89796754502857,335.446202857843));
#49340=CARTESIAN_POINT('Ctrl Pts',(166.558637768761,-4.88556863819563,335.582305624094));
#49341=CARTESIAN_POINT('Ctrl Pts',(166.550872257712,-4.86747623873167,335.718069437295));
#49342=CARTESIAN_POINT('Ctrl Pts',(166.543106746663,-4.84371823824118,335.852981061355));
#49343=CARTESIAN_POINT('Ctrl Pts',(166.535348935141,-4.81998379387741,335.987758920146));
#49344=CARTESIAN_POINT('Ctrl Pts',(166.527591123619,-4.79059499490334,336.121685888821));
#49345=CARTESIAN_POINT('Ctrl Pts',(166.519833312096,-4.75563156393336,336.25425335982));
#49346=CARTESIAN_POINT('Ctrl Pts',(166.512081338573,-4.72069444405382,336.386721069595));
#49347=CARTESIAN_POINT('Ctrl Pts',(166.50432936505,-4.68019114157413,336.517830941627));
#49348=CARTESIAN_POINT('Ctrl Pts',(166.496577391527,-4.634252467892,336.647084432061));
#49349=CARTESIAN_POINT('Ctrl Pts',(166.488828700969,-4.58833324926552,336.776283183564));
#49350=CARTESIAN_POINT('Ctrl Pts',(166.481080010412,-4.53698336834799,336.903626749586));
#49351=CARTESIAN_POINT('Ctrl Pts',(166.473331319854,-4.48038345488503,337.028631844296));
#49352=CARTESIAN_POINT('Ctrl Pts',(166.465584241476,-4.42379531750681,337.153610930652));
#49353=CARTESIAN_POINT('Ctrl Pts',(166.457837163098,-4.36195948139403,337.276252157603));
#49354=CARTESIAN_POINT('Ctrl Pts',(166.450090084721,-4.29510452273087,337.396092694642));
#49355=CARTESIAN_POINT('Ctrl Pts',(166.442342941415,-4.22824900375874,337.51593423606));
#49356=CARTESIAN_POINT('Ctrl Pts',(166.434595798109,-4.15637446876197,337.632974699398));
#49357=CARTESIAN_POINT('Ctrl Pts',(166.426848654803,-4.07975501434121,337.74677667193));
#49358=CARTESIAN_POINT('Ctrl Pts',(166.419099769775,-4.0031183342405,337.860604229561));
#49359=CARTESIAN_POINT('Ctrl Pts',(166.411350884747,-3.92173483024071,337.971191523412));
#49360=CARTESIAN_POINT('Ctrl Pts',(166.403601999719,-3.83592116794736,338.078131227838));
#49361=CARTESIAN_POINT('Ctrl Pts',(166.395844889944,-3.75001642214616,338.185184439172));
#49362=CARTESIAN_POINT('Ctrl Pts',(166.388087780169,-3.65967236995282,338.288582021879));
#49363=CARTESIAN_POINT('Ctrl Pts',(166.380330670395,-3.56524547805433,338.387950375037));
#49364=CARTESIAN_POINT('Ctrl Pts',(166.372569415468,-3.47076812744394,338.487371827466));
#49365=CARTESIAN_POINT('Ctrl Pts',(166.364808160542,-3.37220387055343,338.582759488427));
#49366=CARTESIAN_POINT('Ctrl Pts',(166.357046905616,-3.26994434981216,338.673778301916));
#49367=CARTESIAN_POINT('Ctrl Pts',(166.349273235211,-3.16752124716408,338.764942715844));
#49368=CARTESIAN_POINT('Ctrl Pts',(166.341499564807,-3.06139137105344,338.851724069185));
#49369=CARTESIAN_POINT('Ctrl Pts',(166.333725894402,-2.95197829692954,338.933828567307));
#49370=CARTESIAN_POINT('Ctrl Pts',(166.326314090225,-2.84765842772994,339.012111081287));
#49371=CARTESIAN_POINT('Ctrl Pts',(166.318902286048,-2.74035438432368,339.086142193086));
#49372=CARTESIAN_POINT('Ctrl Pts',(166.311490481871,-2.63045447927052,339.155705992366));
#49373=CARTESIAN_POINT('Ctrl Pts',(166.303715403093,-2.51516805249525,339.228679320669));
#49374=CARTESIAN_POINT('Ctrl Pts',(166.295940324314,-2.39666054176947,339.296966960436));
#49375=CARTESIAN_POINT('Ctrl Pts',(166.288165245536,-2.27534978145381,339.360271371662));
#49376=CARTESIAN_POINT('Ctrl Pts',(166.280399734487,-2.15418830175171,339.423497882781));
#49377=CARTESIAN_POINT('Ctrl Pts',(166.272634223438,-2.03023077934567,339.481753187536));
#49378=CARTESIAN_POINT('Ctrl Pts',(166.264868712389,-1.90392389916115,339.534782999075));
#49379=CARTESIAN_POINT('Ctrl Pts',(166.257110900866,-1.77774225261596,339.587760231402));
#49380=CARTESIAN_POINT('Ctrl Pts',(166.249353089344,-1.64921624199713,339.63552213084));
#49381=CARTESIAN_POINT('Ctrl Pts',(166.241595277822,-1.51881670873112,339.677860501103));
#49382=CARTESIAN_POINT('Ctrl Pts',(166.233843304299,-1.38851530524917,339.7201670104));
#49383=CARTESIAN_POINT('Ctrl Pts',(166.226091330776,-1.25634355570021,339.757057994084));
#49384=CARTESIAN_POINT('Ctrl Pts',(166.218339357253,-1.12279148580239,339.788373663564));
#49385=CARTESIAN_POINT('Ctrl Pts',(166.210590666695,-0.989295975285546,
339.819676070839));
#49386=CARTESIAN_POINT('Ctrl Pts',(166.202841976138,-0.854421686841869,
339.84540777102));
#49387=CARTESIAN_POINT('Ctrl Pts',(166.19509328558,-0.718672774956675,339.865459125821));
#49388=CARTESIAN_POINT('Ctrl Pts',(166.187346207202,-0.582952106766372,
339.88550630877));
#49389=CARTESIAN_POINT('Ctrl Pts',(166.179599128824,-0.44635756352715,339.899875440029));
#49390=CARTESIAN_POINT('Ctrl Pts',(166.171852050447,-0.309402044975992,
339.908508270041));
#49391=CARTESIAN_POINT('Ctrl Pts',(166.164104907141,-0.172445378605723,
339.917141172405));
#49392=CARTESIAN_POINT('Ctrl Pts',(166.156357763835,-0.0351281209893634,
339.920037653043));
#49393=CARTESIAN_POINT('Ctrl Pts',(166.148610620529,0.102033568781341,339.917191496509));
#49394=CARTESIAN_POINT('Ctrl Pts',(166.140861735501,0.239226095411862,339.914344700099));
#49395=CARTESIAN_POINT('Ctrl Pts',(166.133112850473,0.376262593886676,339.905752705545));
#49396=CARTESIAN_POINT('Ctrl Pts',(166.125363965445,0.512629169451043,339.891461376432));
#49397=CARTESIAN_POINT('Ctrl Pts',(166.11760685567,0.649140485907691,339.877154878355));
#49398=CARTESIAN_POINT('Ctrl Pts',(166.109849745896,0.784980069679347,339.857137002415));
#49399=CARTESIAN_POINT('Ctrl Pts',(166.102092636121,0.919640847200704,339.831505332157));
#49400=CARTESIAN_POINT('Ctrl Pts',(166.094331381195,1.05437358313591,339.805859965154));
#49401=CARTESIAN_POINT('Ctrl Pts',(166.086570126268,1.18792587726423,339.774594915447));
#49402=CARTESIAN_POINT('Ctrl Pts',(166.078808871342,1.31980403365141,339.737858205482));
#49403=CARTESIAN_POINT('Ctrl Pts',(166.071035200938,1.45189315210982,339.701062728754));
#49404=CARTESIAN_POINT('Ctrl Pts',(166.063261530533,1.58230240922778,339.658778221557));
#49405=CARTESIAN_POINT('Ctrl Pts',(166.055487860128,1.71055552584989,339.611201888389));
#49406=CARTESIAN_POINT('Ctrl Pts',(166.048076055951,1.83283842903757,339.565840244977));
#49407=CARTESIAN_POINT('Ctrl Pts',(166.040664251774,1.95316114532687,339.515668468144));
#49408=CARTESIAN_POINT('Ctrl Pts',(166.033252447597,2.07113197290002,339.460896256733));
#49409=CARTESIAN_POINT('Ctrl Pts',(166.025477368819,2.19488490214934,339.403439496082));
#49410=CARTESIAN_POINT('Ctrl Pts',(166.01770229004,2.31644064929564,339.340738362288));
#49411=CARTESIAN_POINT('Ctrl Pts',(166.009927211262,2.4353228924535,339.272983205208));
#49412=CARTESIAN_POINT('Ctrl Pts',(166.002161700213,2.55405884344275,339.205311425163));
#49413=CARTESIAN_POINT('Ctrl Pts',(165.994396189164,2.67012750008897,339.132598188145));
#49414=CARTESIAN_POINT('Ctrl Pts',(165.986630678115,2.78307330030879,339.055081511833));
#49415=CARTESIAN_POINT('Ctrl Pts',(165.978872866592,2.89590711443881,338.977641693531));
#49416=CARTESIAN_POINT('Ctrl Pts',(165.97111505507,3.00562391379816,338.895408133582));
#49417=CARTESIAN_POINT('Ctrl Pts',(165.963357243548,3.11179382237577,338.808664105631));
#49418=CARTESIAN_POINT('Ctrl Pts',(165.955605270025,3.21788383473024,338.721985355312));
#49419=CARTESIAN_POINT('Ctrl Pts',(165.947853296502,3.32043196763917,338.630803139432));
#49420=CARTESIAN_POINT('Ctrl Pts',(165.940101322979,3.41903867043276,338.535443060295));
#49421=CARTESIAN_POINT('Ctrl Pts',(165.932352632421,3.51760361322926,338.440123366207));
#49422=CARTESIAN_POINT('Ctrl Pts',(165.924603941864,3.61223016543565,338.340629599091));
#49423=CARTESIAN_POINT('Ctrl Pts',(165.916855251306,3.70255330295679,338.23732638164));
#49424=CARTESIAN_POINT('Ctrl Pts',(165.909108172928,3.79285764799476,338.134044657286));
#49425=CARTESIAN_POINT('Ctrl Pts',(165.901361094551,3.87886010216198,338.026955353184));
#49426=CARTESIAN_POINT('Ctrl Pts',(165.893614016173,3.96023412268692,337.916458255488));
#49427=CARTESIAN_POINT('Ctrl Pts',(165.885866872867,4.0416088252045,337.80596023172));
#49428=CARTESIAN_POINT('Ctrl Pts',(165.878119729561,4.11835478492542,337.692054672129));
#49429=CARTESIAN_POINT('Ctrl Pts',(165.870372586255,4.19018745184681,337.575172262371));
#49430=CARTESIAN_POINT('Ctrl Pts',(165.862623701227,4.26203626827674,337.458263574966));
#49431=CARTESIAN_POINT('Ctrl Pts',(165.854874816199,4.32896938923169,337.338377038592));
#49432=CARTESIAN_POINT('Ctrl Pts',(165.847125931171,4.39074728443907,337.215969617727));
#49433=CARTESIAN_POINT('Ctrl Pts',(165.839368821396,4.45259075134274,337.093432272362));
#49434=CARTESIAN_POINT('Ctrl Pts',(165.831611711622,4.50926788565456,336.968369047061));
#49435=CARTESIAN_POINT('Ctrl Pts',(165.823854601847,4.56058634085738,336.84125915886));
#49436=CARTESIAN_POINT('Ctrl Pts',(165.816093346921,4.6119322190018,336.714081347199));
#49437=CARTESIAN_POINT('Ctrl Pts',(165.808332091994,4.65791358127521,336.584855061469));
#49438=CARTESIAN_POINT('Ctrl Pts',(165.800570837068,4.69838773571041,336.454075564552));
#49439=CARTESIAN_POINT('Ctrl Pts',(165.792797166664,4.73892663560221,336.32308686306));
#49440=CARTESIAN_POINT('Ctrl Pts',(165.785023496259,4.77394062330796,336.190540363461));
#49441=CARTESIAN_POINT('Ctrl Pts',(165.777249825854,4.80333779031722,336.056943297727));
#49442=CARTESIAN_POINT('Ctrl Pts',(165.769838021677,4.83136651212972,335.929565207544));
#49443=CARTESIAN_POINT('Ctrl Pts',(165.7624262175,4.85428952052309,335.801232441144));
#49444=CARTESIAN_POINT('Ctrl Pts',(165.755014413323,4.87207118339821,335.672387869017));
#49445=CARTESIAN_POINT('Ctrl Pts',(165.747239334545,4.89072437853965,335.537228240602));
#49446=CARTESIAN_POINT('Ctrl Pts',(165.739464255766,4.90377844711013,335.401078238262));
#49447=CARTESIAN_POINT('Ctrl Pts',(165.731689176988,4.91113569326316,335.264441420463));
#49448=CARTESIAN_POINT('Ctrl Pts',(165.723923665939,4.91848388585642,335.127972742967));
#49449=CARTESIAN_POINT('Ctrl Pts',(165.71615815489,4.92014918370908,334.991018828542));
#49450=CARTESIAN_POINT('Ctrl Pts',(165.708392643841,4.91608521017967,334.854091574086));
#49451=CARTESIAN_POINT('Ctrl Pts',(165.700634832318,4.91202526609185,334.717300083401));
#49452=CARTESIAN_POINT('Ctrl Pts',(165.692877020796,4.90224736683704,334.580535588265));
#49453=CARTESIAN_POINT('Ctrl Pts',(165.685119209274,4.88675709268995,334.444312876211));
#49454=CARTESIAN_POINT('Ctrl Pts',(165.677367235751,4.87127847546538,334.308192676068));
#49455=CARTESIAN_POINT('Ctrl Pts',(165.669615262228,4.85009608377183,334.172613834289));
#49456=CARTESIAN_POINT('Ctrl Pts',(165.661863288705,4.82326750374017,334.038088543646));
#49457=CARTESIAN_POINT('Ctrl Pts',(165.654114598147,4.79645028562807,333.903620224545));
#49458=CARTESIAN_POINT('Ctrl Pts',(165.64636590759,4.76399171132292,333.770204951688));
#49459=CARTESIAN_POINT('Ctrl Pts',(165.638617217032,4.7260008643441,333.638346999886));
#49460=CARTESIAN_POINT('Ctrl Pts',(165.630870138654,4.68801792167829,333.506516482233));
#49461=CARTESIAN_POINT('Ctrl Pts',(165.623123060276,4.64450510397834,333.376243016509));
#49462=CARTESIAN_POINT('Ctrl Pts',(165.615375981899,4.59562188891985,333.248017546726));
#49463=CARTESIAN_POINT('Ctrl Pts',(165.607628838593,4.54673826417296,333.119791002289));
#49464=CARTESIAN_POINT('Ctrl Pts',(165.599881695287,4.49248429153102,332.993612853262));
#49465=CARTESIAN_POINT('Ctrl Pts',(165.592134551981,4.43306815741772,332.869955452534));
#49466=CARTESIAN_POINT('Ctrl Pts',(165.584385666953,4.37363866529608,332.746270250997));
#49467=CARTESIAN_POINT('Ctrl Pts',(165.576636781925,4.30904487156203,332.62510727771));
#49468=CARTESIAN_POINT('Ctrl Pts',(165.568887896897,4.23954142382082,332.506915248491));
#49469=CARTESIAN_POINT('Ctrl Pts',(165.561130787122,4.16996420440202,332.38859776903));
#49470=CARTESIAN_POINT('Ctrl Pts',(165.553373677348,4.09546711964909,332.273257870297));
#49471=CARTESIAN_POINT('Ctrl Pts',(165.545616567573,4.01634906365282,332.161316632417));
#49472=CARTESIAN_POINT('Ctrl Pts',(165.537855312647,3.93718872949713,332.049315576718));
#49473=CARTESIAN_POINT('Ctrl Pts',(165.53009405772,3.85340274244102,331.940717110001));
#49474=CARTESIAN_POINT('Ctrl Pts',(165.522332802794,3.7653303607965,331.835909240151));
#49475=CARTESIAN_POINT('Ctrl Pts',(165.51455913239,3.67711709204406,331.730933711865));
#49476=CARTESIAN_POINT('Ctrl Pts',(165.506785461985,3.58460399062556,331.629761186163));
#49477=CARTESIAN_POINT('Ctrl Pts',(165.49901179158,3.48816786175894,331.532743443197));
#49478=CARTESIAN_POINT('Ctrl Pts',(165.491599987403,3.39622085789249,331.440241899508));
#49479=CARTESIAN_POINT('Ctrl Pts',(165.484188183226,3.30070805193071,331.351517229077));
#49480=CARTESIAN_POINT('Ctrl Pts',(165.476776379049,3.20198258054458,331.266839058333));
#49481=CARTESIAN_POINT('Ctrl Pts',(165.469001300271,3.09841827971757,331.178010558197));
#49482=CARTESIAN_POINT('Ctrl Pts',(165.461226221492,2.99099114366286,331.093354534888));
#49483=CARTESIAN_POINT('Ctrl Pts',(165.453451142714,2.88007175660924,331.013225647308));
#49484=CARTESIAN_POINT('Ctrl Pts',(165.445685631665,2.76928886292286,330.933195363426));
#49485=CARTESIAN_POINT('Ctrl Pts',(165.437920120616,2.65502258272237,330.857681357425));
#49486=CARTESIAN_POINT('Ctrl Pts',(165.430154609567,2.53767828396757,330.786999645196));
#49487=CARTESIAN_POINT('Ctrl Pts',(165.422396798045,2.42045033242669,330.716388014091));
#49488=CARTESIAN_POINT('Ctrl Pts',(165.414638986523,2.30015076838236,330.650599342314));
#49489=CARTESIAN_POINT('Ctrl Pts',(165.406881175,2.17721550745935,330.589907518364));
#49490=CARTESIAN_POINT('Ctrl Pts',(165.399129201477,2.05437275921865,330.529261366937));
#49491=CARTESIAN_POINT('Ctrl Pts',(165.391377227954,1.92889861112814,330.47370460122));
#49492=CARTESIAN_POINT('Ctrl Pts',(165.383625254431,1.80125494017703,330.423465972705));
#49493=CARTESIAN_POINT('Ctrl Pts',(165.375876563874,1.67366532639633,330.373248620279));
#49494=CARTESIAN_POINT('Ctrl Pts',(165.368127873316,1.54390838013171,330.328345068376));
#49495=CARTESIAN_POINT('Ctrl Pts',(165.360379182759,1.41246718818142,330.288936478372));
#49496=CARTESIAN_POINT('Ctrl Pts',(165.352632104381,1.28105334366896,330.249536087655));
#49497=CARTESIAN_POINT('Ctrl Pts',(165.344885026003,1.14795632465699,330.215628496971));
#49498=CARTESIAN_POINT('Ctrl Pts',(165.337137947625,1.0136752789592,330.187345276116));
#49499=CARTESIAN_POINT('Ctrl Pts',(165.329390804319,0.879393107857031,330.15906181822));
#49500=CARTESIAN_POINT('Ctrl Pts',(165.321643661014,0.743927272758503,330.136402904733));
#49501=CARTESIAN_POINT('Ctrl Pts',(165.313896517708,0.607787646905678,330.119449084502));
#49502=CARTESIAN_POINT('Ctrl Pts',(165.30614763268,0.471617413974657,330.102491452693));
#49503=CARTESIAN_POINT('Ctrl Pts',(165.298398747652,0.334773476658537,330.091241514716));
#49504=CARTESIAN_POINT('Ctrl Pts',(165.290649862624,0.197770974091667,330.085727957845));
#49505=CARTESIAN_POINT('Ctrl Pts',(165.282892752849,0.0606230556530012,
330.080208548827));
#49506=CARTESIAN_POINT('Ctrl Pts',(165.275135643074,-0.0766833730620175,
330.080437699315));
#49507=CARTESIAN_POINT('Ctrl Pts',(165.267378533299,-0.213632468050133,
330.086391933508));
#49508=CARTESIAN_POINT('Ctrl Pts',(165.259617278373,-0.350654744255804,
330.092349349453));
#49509=CARTESIAN_POINT('Ctrl Pts',(165.251856023447,-0.487318916999135,
330.104037911745));
#49510=CARTESIAN_POINT('Ctrl Pts',(165.244094768521,-0.623115110034368,
330.121382304162));
#49511=CARTESIAN_POINT('Ctrl Pts',(165.236321098116,-0.759128532722581,
330.138754441953));
#49512=CARTESIAN_POINT('Ctrl Pts',(165.228547427712,-0.894270815584662,
330.161800423681));
#49513=CARTESIAN_POINT('Ctrl Pts',(165.220773757307,-1.02804222826113,330.190393754224));
#49514=CARTESIAN_POINT('Ctrl Pts',(165.21336195313,-1.15558654949415,330.21765605835));
#49515=CARTESIAN_POINT('Ctrl Pts',(165.205950148953,-1.281884477547,330.24996080437));
#49516=CARTESIAN_POINT('Ctrl Pts',(165.198538344776,-1.40651817528927,330.287156942452));
#49517=CARTESIAN_POINT('Ctrl Pts',(165.190763265997,-1.5372605418223,330.326176174063));
#49518=CARTESIAN_POINT('Ctrl Pts',(165.182988187219,-1.66658458536666,330.370701712855));
#49519=CARTESIAN_POINT('Ctrl Pts',(165.17521310844,-1.79399152129524,330.420613852925));
#49520=CARTESIAN_POINT('Ctrl Pts',(165.167447597391,-1.92124167487801,330.47046457293));
#49521=CARTESIAN_POINT('Ctrl Pts',(165.159682086342,-2.04657905435909,330.525688564075));
#49522=CARTESIAN_POINT('Ctrl Pts',(165.151916575293,-2.16951854737093,330.586115958126));
#49523=CARTESIAN_POINT('Ctrl Pts',(165.144158763771,-2.29233614551744,330.646483438239));
#49524=CARTESIAN_POINT('Ctrl Pts',(165.136400952249,-2.41276024004639,330.712043882871));
#49525=CARTESIAN_POINT('Ctrl Pts',(165.128643140727,-2.53032461331767,330.782578938055));
#49526=CARTESIAN_POINT('Ctrl Pts',(165.120891167204,-2.64780051566999,330.853060913373));
#49527=CARTESIAN_POINT('Ctrl Pts',(165.113139193681,-2.76242064645018,330.928509847599));
#49528=CARTESIAN_POINT('Ctrl Pts',(165.105387220158,-2.87374269550638,331.008661129079));
#49529=CARTESIAN_POINT('Ctrl Pts',(165.0976385296,-2.98501759960871,331.088778466444));
#49530=CARTESIAN_POINT('Ctrl Pts',(165.089889839042,-3.09299688345509,331.1735939623));
#49531=CARTESIAN_POINT('Ctrl Pts',(165.082141148485,-3.19726677859285,331.262799415471));
#49532=CARTESIAN_POINT('Ctrl Pts',(165.074394070107,-3.30151497950807,331.351986308701));
#49533=CARTESIAN_POINT('Ctrl Pts',(165.066646991729,-3.4020550299936,331.445561088553));
#49534=CARTESIAN_POINT('Ctrl Pts',(165.058899913351,-3.49850617267885,331.543175210945));
#49535=CARTESIAN_POINT('Ctrl Pts',(165.051152770045,-3.59495812371749,331.640790151437));
#49536=CARTESIAN_POINT('Ctrl Pts',(165.04340562674,-3.68732082387519,331.742444223952));
#49537=CARTESIAN_POINT('Ctrl Pts',(165.035658483434,-3.77525061624006,331.847752254806));
#49538=CARTESIAN_POINT('Ctrl Pts',(165.027909598406,-3.86320017708907,331.953083961142));
#49539=CARTESIAN_POINT('Ctrl Pts',(165.020160713378,-3.94671459652552,332.062070960508));
#49540=CARTESIAN_POINT('Ctrl Pts',(165.012411828349,-4.02549097946611,332.174295585746));
#49541=CARTESIAN_POINT('Ctrl Pts',(165.004654718575,-4.10435097647348,332.28663932736));
#49542=CARTESIAN_POINT('Ctrl Pts',(164.9968976088,-4.17846266615845,332.402227239048));
#49543=CARTESIAN_POINT('Ctrl Pts',(164.989140499025,-4.24756663703321,332.52061283248));
#49544=CARTESIAN_POINT('Ctrl Pts',(164.981379244099,-4.31670753486047,332.639061687388));
#49545=CARTESIAN_POINT('Ctrl Pts',(164.973617989173,-4.38083519912442,332.760310857596));
#49546=CARTESIAN_POINT('Ctrl Pts',(164.965856734247,-4.43973704155053,332.883890819361));
#49547=CARTESIAN_POINT('Ctrl Pts',(164.958083063842,-4.49873310772847,333.007668468791));
#49548=CARTESIAN_POINT('Ctrl Pts',(164.950309393437,-4.55248649374851,333.133784000674));
#49549=CARTESIAN_POINT('Ctrl Pts',(164.942535723033,-4.60083313928456,333.261748727324));
#49550=CARTESIAN_POINT('Ctrl Pts',(164.935123918856,-4.64692923683975,333.383756665162));
#49551=CARTESIAN_POINT('Ctrl Pts',(164.927712114678,-4.6881105425639,333.507445239027));
#49552=CARTESIAN_POINT('Ctrl Pts',(164.920300310501,-4.72427796183447,333.632381339033));
#49553=CARTESIAN_POINT('Ctrl Pts',(164.910601398758,-4.77160579175578,333.795869766224));
#49554=CARTESIAN_POINT('Ctrl Pts',(164.900902487014,-4.81047037042544,333.961910646757));
#49555=CARTESIAN_POINT('Ctrl Pts',(164.89120357527,-4.84064076570765,334.129724158747));
#49556=CARTESIAN_POINT('Ctrl Pts',(164.881648515377,-4.87036368117776,334.295048702391));
#49557=CARTESIAN_POINT('Ctrl Pts',(164.872093455484,-4.89164840743187,334.462093761431));
#49558=CARTESIAN_POINT('Ctrl Pts',(164.862538395591,-4.90431969220292,334.630092688406));
#49559=CARTESIAN_POINT('Ctrl Pts',(164.85563138923,-4.91347930454422,334.75153302162));
#49560=CARTESIAN_POINT('Ctrl Pts',(164.848724382869,-4.91813903925031,334.873471352709));
#49561=CARTESIAN_POINT('Ctrl Pts',(164.841817376508,-4.91824804142986,334.99561075504));
#49562=CARTESIAN_POINT('',(163.091817376508,-4.91461805696729,335.001889284352));
#49563=CARTESIAN_POINT('Ctrl Pts',(164.841817376508,-4.91584934655102,334.995612895733));
#49564=CARTESIAN_POINT('Ctrl Pts',(164.775232343081,-4.90575230845859,336.172498809948));
#49565=CARTESIAN_POINT('Ctrl Pts',(164.61590129823,-3.89179482935224,339.004282256428));
#49566=CARTESIAN_POINT('Ctrl Pts',(164.363824241953,0.842573010119754,340.754521664661));
#49567=CARTESIAN_POINT('Ctrl Pts',(164.08558620768,5.29506463775386,337.405564247415));
#49568=CARTESIAN_POINT('Ctrl Pts',(163.807348173406,4.88835360234718,331.849056026387));
#49569=CARTESIAN_POINT('Ctrl Pts',(163.529110139132,-0.00432738195248262,
329.184122582086));
#49570=CARTESIAN_POINT('Ctrl Pts',(163.290599873499,-4.19501065200652,331.474786607412));
#49571=CARTESIAN_POINT('Ctrl Pts',(163.144835619292,-4.90756803691727,334.062368982235));
#49572=CARTESIAN_POINT('Ctrl Pts',(163.091817376508,-4.91080196671261,335.001887817365));
#49573=CARTESIAN_POINT('',(161.341817376542,-4.91824867880592,335.003604985961));
#49574=CARTESIAN_POINT('Ctrl Pts',(163.091817376508,-4.91824963659101,335.001890680409));
#49575=CARTESIAN_POINT('Ctrl Pts',(163.08341381012,-4.91819230303736,335.151033141548));
#49576=CARTESIAN_POINT('Ctrl Pts',(163.075010243731,-4.91134684598843,335.299966218502));
#49577=CARTESIAN_POINT('Ctrl Pts',(163.066606677343,-4.8977951958724,335.4480907071));
#49578=CARTESIAN_POINT('Ctrl Pts',(163.058167104356,-4.88418548126286,335.596849861833));
#49579=CARTESIAN_POINT('Ctrl Pts',(163.049727531368,-4.86381206661228,335.744793215169));
#49580=CARTESIAN_POINT('Ctrl Pts',(163.041287958381,-4.83680856621425,335.891328197858));
#49581=CARTESIAN_POINT('Ctrl Pts',(163.032830126397,-4.80974664380272,336.038180208658));
#49582=CARTESIAN_POINT('Ctrl Pts',(163.024372294412,-4.77602603615179,336.183617493372));
#49583=CARTESIAN_POINT('Ctrl Pts',(163.015914462427,-4.7358304020831,336.327061967357));
#49584=CARTESIAN_POINT('Ctrl Pts',(163.007428609945,-4.69550160130289,336.470981667802));
#49585=CARTESIAN_POINT('Ctrl Pts',(162.998942757463,-4.64865492827412,336.612895082275));
#49586=CARTESIAN_POINT('Ctrl Pts',(162.99045690498,-4.59552346688747,336.75224060214));
#49587=CARTESIAN_POINT('Ctrl Pts',(162.984515960182,-4.55832613405275,336.849796391989));
#49588=CARTESIAN_POINT('Ctrl Pts',(162.978575015383,-4.51804937297229,336.946094016319));
#49589=CARTESIAN_POINT('Ctrl Pts',(162.972634070584,-4.47478642980206,337.040948179195));
#49590=CARTESIAN_POINT('Ctrl Pts',(162.964858991806,-4.41816701946718,337.165086445719));
#49591=CARTESIAN_POINT('Ctrl Pts',(162.957083913027,-4.3562885121357,337.287063009754));
#49592=CARTESIAN_POINT('Ctrl Pts',(162.949308834249,-4.28933803542898,337.406400274336));
#49593=CARTESIAN_POINT('Ctrl Pts',(162.9415433232,-4.22246994554613,337.525590686816));
#49594=CARTESIAN_POINT('Ctrl Pts',(162.933777812151,-4.1505424942657,337.642147924453));
#49595=CARTESIAN_POINT('Ctrl Pts',(162.926012301102,-4.0737906161863,337.755614827579));
#49596=CARTESIAN_POINT('Ctrl Pts',(162.91825448958,-3.99711483781751,337.86896922794));
#49597=CARTESIAN_POINT('Ctrl Pts',(162.910496678057,-3.91562436954204,337.9792390698));
#49598=CARTESIAN_POINT('Ctrl Pts',(162.902738866535,-3.82959957442099,338.08599257324));
#49599=CARTESIAN_POINT('Ctrl Pts',(162.894986893012,-3.7436395156861,338.192665741284));
#49600=CARTESIAN_POINT('Ctrl Pts',(162.887234919489,-3.65315216624161,338.295827534825));
#49601=CARTESIAN_POINT('Ctrl Pts',(162.879482945966,-3.55846042171278,338.395076212636));
#49602=CARTESIAN_POINT('Ctrl Pts',(162.871734255409,-3.46380877919412,338.494282858572));
#49603=CARTESIAN_POINT('Ctrl Pts',(162.863985564851,-3.36495655226675,338.589579402627));
#49604=CARTESIAN_POINT('Ctrl Pts',(162.856236874293,-3.26226588930638,338.680598365751));
#49605=CARTESIAN_POINT('Ctrl Pts',(162.848489795915,-3.15959659199617,338.771598391619));
#49606=CARTESIAN_POINT('Ctrl Pts',(162.840742717538,-3.05309073949119,338.858322347698));
#49607=CARTESIAN_POINT('Ctrl Pts',(162.83299563916,-2.94314590279378,338.940440997829));
#49608=CARTESIAN_POINT('Ctrl Pts',(162.825248495854,-2.83320014465285,339.022560336192));
#49609=CARTESIAN_POINT('Ctrl Pts',(162.817501352548,-2.71981565799548,339.100074057718));
#49610=CARTESIAN_POINT('Ctrl Pts',(162.809754209242,-2.6034211963131,339.172694709308));
#49611=CARTESIAN_POINT('Ctrl Pts',(162.802005324214,-2.48700056668453,339.245331687563));
#49612=CARTESIAN_POINT('Ctrl Pts',(162.794256439186,-2.36756894701807,339.313073200009));
#49613=CARTESIAN_POINT('Ctrl Pts',(162.786507554158,-2.24558167316801,339.37567663472));
#49614=CARTESIAN_POINT('Ctrl Pts',(162.778750444383,-2.12346492076511,339.438346517363));
#49615=CARTESIAN_POINT('Ctrl Pts',(162.770993334609,-1.99878744381306,339.495867249428));
#49616=CARTESIAN_POINT('Ctrl Pts',(162.763236224834,-1.87202714897303,339.548043251334));
#49617=CARTESIAN_POINT('Ctrl Pts',(162.755474969908,-1.74519911748454,339.600247134428));
#49618=CARTESIAN_POINT('Ctrl Pts',(162.747713714982,-1.6162864175494,339.64710046297));
#49619=CARTESIAN_POINT('Ctrl Pts',(162.739952460055,-1.48578333676146,339.688457202396));
#49620=CARTESIAN_POINT('Ctrl Pts',(162.732178789651,-1.35507149357504,339.729880099128));
#49621=CARTESIAN_POINT('Ctrl Pts',(162.724405119246,-1.22276456311469,339.765788733787));
#49622=CARTESIAN_POINT('Ctrl Pts',(162.716631448841,-1.08936914487001,339.796087773249));
#49623=CARTESIAN_POINT('Ctrl Pts',(162.709219644664,-0.962183315437024,
339.824976385134));
#49624=CARTESIAN_POINT('Ctrl Pts',(162.701807840487,-0.83400833884291,339.84876584963));
#49625=CARTESIAN_POINT('Ctrl Pts',(162.69439603631,-0.705286834752437,339.867417543547));
#49626=CARTESIAN_POINT('Ctrl Pts',(162.686620957532,-0.570256306305494,
339.886983412542));
#49627=CARTESIAN_POINT('Ctrl Pts',(162.678845878753,-0.434197600447369,
339.90095697342));
#49628=CARTESIAN_POINT('Ctrl Pts',(162.671070799975,-0.297613604147919,
339.909237130668));
#49629=CARTESIAN_POINT('Ctrl Pts',(162.663305288926,-0.161197683151326,
339.917507098655));
#49630=CARTESIAN_POINT('Ctrl Pts',(162.655539777877,-0.0242581442989326,
339.920097579706));
#49631=CARTESIAN_POINT('Ctrl Pts',(162.647774266828,0.112693440500956,339.916958740011));
#49632=CARTESIAN_POINT('Ctrl Pts',(162.640016455305,0.249509237405908,339.913823012484));
#49633=CARTESIAN_POINT('Ctrl Pts',(162.632258643783,0.386336668235516,339.904969277901));
#49634=CARTESIAN_POINT('Ctrl Pts',(162.624500832261,0.522660919506837,339.890399638651));
#49635=CARTESIAN_POINT('Ctrl Pts',(162.616748858738,0.658882582455916,339.875840963517));
#49636=CARTESIAN_POINT('Ctrl Pts',(162.608996885215,0.794601432452124,339.855574986814));
#49637=CARTESIAN_POINT('Ctrl Pts',(162.601244911692,0.929304899375981,339.829655833131));
#49638=CARTESIAN_POINT('Ctrl Pts',(162.593496221134,1.06395131930158,339.803747656225));
#49639=CARTESIAN_POINT('Ctrl Pts',(162.585747530577,1.19758282839051,339.772191137785));
#49640=CARTESIAN_POINT('Ctrl Pts',(162.577998840019,1.32969442640266,339.735091952105));
#49641=CARTESIAN_POINT('Ctrl Pts',(162.570251761641,1.46177853749345,339.698000485222));
#49642=CARTESIAN_POINT('Ctrl Pts',(162.562504683263,1.59234299043,339.655368750501));
#49643=CARTESIAN_POINT('Ctrl Pts',(162.554757604886,1.72089577501953,339.607352905305));
#49644=CARTESIAN_POINT('Ctrl Pts',(162.54701046158,1.84944963700515,339.559336657689));
#49645=CARTESIAN_POINT('Ctrl Pts',(162.539263318274,1.9759914308498,339.505936346361));
#49646=CARTESIAN_POINT('Ctrl Pts',(162.531516174968,2.10004740799503,339.447356961913));
#49647=CARTESIAN_POINT('Ctrl Pts',(162.52376728994,2.22413127555774,339.388764407575));
#49648=CARTESIAN_POINT('Ctrl Pts',(162.516018404912,2.34572786096202,339.324990630027));
#49649=CARTESIAN_POINT('Ctrl Pts',(162.508269519884,2.46438673830471,339.256287239669));
#49650=CARTESIAN_POINT('Ctrl Pts',(162.500512410109,2.58317156140579,339.187510926822));
#49651=CARTESIAN_POINT('Ctrl Pts',(162.492755300334,2.69901210892108,339.113794745235));
#49652=CARTESIAN_POINT('Ctrl Pts',(162.48499819056,2.8114852910926,339.035434737481));
#49653=CARTESIAN_POINT('Ctrl Pts',(162.477236935633,2.92401857533641,338.957032856645));
#49654=CARTESIAN_POINT('Ctrl Pts',(162.469475680707,3.03318059782353,338.873982441555));
#49655=CARTESIAN_POINT('Ctrl Pts',(162.461714425781,3.13858106759404,338.786620121512));
#49656=CARTESIAN_POINT('Ctrl Pts',(162.453940755376,3.24415014376628,338.699118050228));
#49657=CARTESIAN_POINT('Ctrl Pts',(162.446167084972,3.34594535257078,338.607290552411));
#49658=CARTESIAN_POINT('Ctrl Pts',(162.438393414567,3.44361237629537,338.511512048153));
#49659=CARTESIAN_POINT('Ctrl Pts',(162.43098161039,3.53673297656772,338.420192056313));
#49660=CARTESIAN_POINT('Ctrl Pts',(162.423569806213,3.62610087930152,338.32528082828));
#49661=CARTESIAN_POINT('Ctrl Pts',(162.416158002036,3.71144407853293,338.227129671151));
#49662=CARTESIAN_POINT('Ctrl Pts',(162.408382923258,3.80097020218334,338.124167833433));
#49663=CARTESIAN_POINT('Ctrl Pts',(162.400607844479,3.88635004042516,338.017315060586));
#49664=CARTESIAN_POINT('Ctrl Pts',(162.392832765701,3.96722643888965,337.906939532408));
#49665=CARTESIAN_POINT('Ctrl Pts',(162.385067254652,4.04800331379702,337.796699828344));
#49666=CARTESIAN_POINT('Ctrl Pts',(162.377301743603,4.12428754664072,337.682946306585));
#49667=CARTESIAN_POINT('Ctrl Pts',(162.369536232554,4.19576039019223,337.566082190927));
#49668=CARTESIAN_POINT('Ctrl Pts',(162.361778421031,4.26716236821128,337.44933394638));
#49669=CARTESIAN_POINT('Ctrl Pts',(162.354020609509,4.33376224789202,337.3294815769));
#49670=CARTESIAN_POINT('Ctrl Pts',(162.346262797987,4.39528320206433,337.206959137853));
#49671=CARTESIAN_POINT('Ctrl Pts',(162.338510824464,4.45675785976762,337.084528900826));
#49672=CARTESIAN_POINT('Ctrl Pts',(162.330758850941,4.51316102488095,336.959432941574));
#49673=CARTESIAN_POINT('Ctrl Pts',(162.323006877418,4.56426083082374,336.832131581167));
#49674=CARTESIAN_POINT('Ctrl Pts',(162.31525818686,4.61533899596838,336.704884132961));
#49675=CARTESIAN_POINT('Ctrl Pts',(162.307509496303,4.66111812372573,336.575433503225));
#49676=CARTESIAN_POINT('Ctrl Pts',(162.299760805745,4.70141379325786,336.444261543857));
#49677=CARTESIAN_POINT('Ctrl Pts',(162.292013727367,4.74170107893939,336.313116875911));
#49678=CARTESIAN_POINT('Ctrl Pts',(162.28426664899,4.77650706097572,336.180251964101));
#49679=CARTESIAN_POINT('Ctrl Pts',(162.276519570612,4.80569680047546,336.046165056002));
#49680=CARTESIAN_POINT('Ctrl Pts',(162.268772427306,4.83488678461331,335.912077024126));
#49681=CARTESIAN_POINT('Ctrl Pts',(162.261025284,4.85846034918768,335.776767357462));
#49682=CARTESIAN_POINT('Ctrl Pts',(162.253278140694,4.87633350263269,335.640745373453));
#49683=CARTESIAN_POINT('Ctrl Pts',(162.245529255666,4.89421067434204,335.504692808815));
#49684=CARTESIAN_POINT('Ctrl Pts',(162.237780370638,4.90638483382122,335.36792799563));
#49685=CARTESIAN_POINT('Ctrl Pts',(162.23003148561,4.91282381432127,335.230965867474));
#49686=CARTESIAN_POINT('Ctrl Pts',(162.222274375835,4.91926962922176,335.093858366299));
#49687=CARTESIAN_POINT('Ctrl Pts',(162.214517266061,4.91996808664918,334.956553522854));
#49688=CARTESIAN_POINT('Ctrl Pts',(162.206760156286,4.91493917697483,334.819567327964));
#49689=CARTESIAN_POINT('Ctrl Pts',(162.19899890136,4.90990758001193,334.682507932032));
#49690=CARTESIAN_POINT('Ctrl Pts',(162.191237646434,4.89914254824338,334.545767913416));
#49691=CARTESIAN_POINT('Ctrl Pts',(162.183476391507,4.88271595159642,334.409857645541));
#49692=CARTESIAN_POINT('Ctrl Pts',(162.175702721103,4.86626307774824,334.273729965531));
#49693=CARTESIAN_POINT('Ctrl Pts',(162.167929050698,4.84413060427184,334.138435074613));
#49694=CARTESIAN_POINT('Ctrl Pts',(162.160155380293,4.81644164736722,334.004473546305));
#49695=CARTESIAN_POINT('Ctrl Pts',(162.152743576116,4.79004161806783,333.876747959368));
#49696=CARTESIAN_POINT('Ctrl Pts',(162.145331771939,4.75859084167148,333.750234671884));
#49697=CARTESIAN_POINT('Ctrl Pts',(162.137919967762,4.72223754177349,333.625352531896));
#49698=CARTESIAN_POINT('Ctrl Pts',(162.130144888984,4.68410245835693,333.494349546224));
#49699=CARTESIAN_POINT('Ctrl Pts',(162.122369810205,4.64045161163237,333.364727652148));
#49700=CARTESIAN_POINT('Ctrl Pts',(162.114594731427,4.59140133512482,333.236986431614));
#49701=CARTESIAN_POINT('Ctrl Pts',(162.106829220378,4.5424114181052,333.109402404783));
#49702=CARTESIAN_POINT('Ctrl Pts',(162.099063709329,4.48803543041296,332.983694808132));
#49703=CARTESIAN_POINT('Ctrl Pts',(162.09129819828,4.42843995912629,332.86034989054));
#49704=CARTESIAN_POINT('Ctrl Pts',(162.083540386757,4.36890357692294,332.737127269792));
#49705=CARTESIAN_POINT('Ctrl Pts',(162.075782575235,4.30415817888452,332.616263015869));
#49706=CARTESIAN_POINT('Ctrl Pts',(162.068024763713,4.23441896436178,332.498224810909));
#49707=CARTESIAN_POINT('Ctrl Pts',(162.06027279019,4.16473223080954,332.380275433441));
#49708=CARTESIAN_POINT('Ctrl Pts',(162.052520816667,4.09005935892492,332.265148207032));
#49709=CARTESIAN_POINT('Ctrl Pts',(162.044768843144,4.01066196620489,332.153287219381));
#49710=CARTESIAN_POINT('Ctrl Pts',(162.037020152586,3.93129819832779,332.041473604925));
#49711=CARTESIAN_POINT('Ctrl Pts',(162.029271462029,3.84721411490942,331.932923796113));
#49712=CARTESIAN_POINT('Ctrl Pts',(162.021522771471,3.75871511479493,331.828053634074));
#49713=CARTESIAN_POINT('Ctrl Pts',(162.013775693093,3.67023452763659,331.723205291148));
#49714=CARTESIAN_POINT('Ctrl Pts',(162.006028614715,3.57734110279336,331.622035370733));
#49715=CARTESIAN_POINT('Ctrl Pts',(161.998281536338,3.48038080410419,331.524926976174));
#49716=CARTESIAN_POINT('Ctrl Pts',(161.990534393032,3.38341969279435,331.427817767753));
#49717=CARTESIAN_POINT('Ctrl Pts',(161.982787249726,3.2823919158337,331.334770429684));
#49718=CARTESIAN_POINT('Ctrl Pts',(161.97504010642,3.1776803164692,331.246131213158));
#49719=CARTESIAN_POINT('Ctrl Pts',(161.967291221392,3.07294517571416,331.157472068655));
#49720=CARTESIAN_POINT('Ctrl Pts',(161.959542336364,2.96452486280449,331.073223270247));
#49721=CARTESIAN_POINT('Ctrl Pts',(161.951793451336,2.85283498909618,330.993690527744));
#49722=CARTESIAN_POINT('Ctrl Pts',(161.944036341561,2.74102656660185,330.914073368367));
#49723=CARTESIAN_POINT('Ctrl Pts',(161.936279231786,2.62594196986935,330.839182491276));
#49724=CARTESIAN_POINT('Ctrl Pts',(161.928522122012,2.50802592453055,330.769280318388));
#49725=CARTESIAN_POINT('Ctrl Pts',(161.920760867086,2.39004686862736,330.699340792013));
#49726=CARTESIAN_POINT('Ctrl Pts',(161.912999612159,2.26923369336533,330.634395466675));
#49727=CARTESIAN_POINT('Ctrl Pts',(161.905238357233,2.14605447558744,330.574660097765));
#49728=CARTESIAN_POINT('Ctrl Pts',(161.897464686828,2.02267821120514,330.514829171733));
#49729=CARTESIAN_POINT('Ctrl Pts',(161.889691016424,1.89692869968218,330.460225012159));
#49730=CARTESIAN_POINT('Ctrl Pts',(161.881917346019,1.76929350921122,330.411014977061));
#49731=CARTESIAN_POINT('Ctrl Pts',(161.874505541842,1.64759976756455,330.364095680935));
#49732=CARTESIAN_POINT('Ctrl Pts',(161.867093737665,1.52419222532465,330.322079710591));
#49733=CARTESIAN_POINT('Ctrl Pts',(161.859681933488,1.39950331304033,330.285069084357));
#49734=CARTESIAN_POINT('Ctrl Pts',(161.85190685471,1.26870302573515,330.246244457081));
#49735=CARTESIAN_POINT('Ctrl Pts',(161.844131775931,1.13607923179781,330.212805540755));
#49736=CARTESIAN_POINT('Ctrl Pts',(161.836356697153,1.00211499508821,330.184924860491));
#49737=CARTESIAN_POINT('Ctrl Pts',(161.828591186104,0.868315609900354,330.157078489179));
#49738=CARTESIAN_POINT('Ctrl Pts',(161.820825675055,0.733179442988939,330.134776823642));
#49739=CARTESIAN_POINT('Ctrl Pts',(161.813060164006,0.597205541236013,330.118142914421));
#49740=CARTESIAN_POINT('Ctrl Pts',(161.805302352483,0.461366458002645,330.10152549777));
#49741=CARTESIAN_POINT('Ctrl Pts',(161.797544540961,0.324691678384345,330.090564701276));
#49742=CARTESIAN_POINT('Ctrl Pts',(161.789786729439,0.187690942984901,330.085332648854));
#49743=CARTESIAN_POINT('Ctrl Pts',(161.782034755916,0.0507933049835277,
330.080104533718));
#49744=CARTESIAN_POINT('Ctrl Pts',(161.774282782393,-0.0864294115402772,
330.080596596553));
#49745=CARTESIAN_POINT('Ctrl Pts',(161.76653080887,-0.223462187527487,330.08682915896));
#49746=CARTESIAN_POINT('Ctrl Pts',(161.758782118312,-0.360436930052849,
330.093059081874));
#49747=CARTESIAN_POINT('Ctrl Pts',(161.751033427755,-0.497221502372977,
330.10502465134));
#49748=CARTESIAN_POINT('Ctrl Pts',(161.743284737197,-0.633300945972124,
330.122694086452));
#49749=CARTESIAN_POINT('Ctrl Pts',(161.735537658819,-0.76935207710638,330.14035984529));
#49750=CARTESIAN_POINT('Ctrl Pts',(161.727790580441,-0.904697983955155,
330.16372705897));
#49751=CARTESIAN_POINT('Ctrl Pts',(161.720043502064,-1.03882928585775,330.19271211832));
#49752=CARTESIAN_POINT('Ctrl Pts',(161.712296358758,-1.17296171190983,330.221697420594));
#49753=CARTESIAN_POINT('Ctrl Pts',(161.704549215452,-1.30587913065618,330.256300579889));
#49754=CARTESIAN_POINT('Ctrl Pts',(161.696802072146,-1.43708319363397,330.296387031539));
#49755=CARTESIAN_POINT('Ctrl Pts',(161.689053187118,-1.5683167540705,330.336482495475));
#49756=CARTESIAN_POINT('Ctrl Pts',(161.68130430209,-1.69783581849286,330.382063590633));
#49757=CARTESIAN_POINT('Ctrl Pts',(161.673555417062,-1.82515839784708,330.432946257677));
#49758=CARTESIAN_POINT('Ctrl Pts',(161.665798307287,-1.95261611870269,330.48388293211));
#49759=CARTESIAN_POINT('Ctrl Pts',(161.658041197512,-2.07787233381947,330.540132273893));
#49760=CARTESIAN_POINT('Ctrl Pts',(161.650284087738,-2.20046570045315,330.601462315311));
#49761=CARTESIAN_POINT('Ctrl Pts',(161.642522832812,-2.32312457706218,330.662825129542));
#49762=CARTESIAN_POINT('Ctrl Pts',(161.634761577885,-2.44311742807916,330.729273863954));
#49763=CARTESIAN_POINT('Ctrl Pts',(161.627000322959,-2.56000951695535,330.800531660365));
#49764=CARTESIAN_POINT('Ctrl Pts',(161.619226652555,-2.67708859507865,330.871903446027));
#49765=CARTESIAN_POINT('Ctrl Pts',(161.61145298215,-2.7910566739831,330.948099449084));
#49766=CARTESIAN_POINT('Ctrl Pts',(161.603679311745,-2.90150916761735,331.028800230065));
#49767=CARTESIAN_POINT('Ctrl Pts',(161.596267507568,-3.00682007109914,331.105744370276));
#49768=CARTESIAN_POINT('Ctrl Pts',(161.588855703391,-3.10893509916182,331.186783152901));
#49769=CARTESIAN_POINT('Ctrl Pts',(161.581443899214,-3.20753444943506,331.271608145837));
#49770=CARTESIAN_POINT('Ctrl Pts',(161.573781304336,-3.30947007243474,331.359303333249));
#49771=CARTESIAN_POINT('Ctrl Pts',(161.566118709459,-3.40799016563838,331.451340250614));
#49772=CARTESIAN_POINT('Ctrl Pts',(161.558456114581,-3.50269411343921,331.547418790212));
#49773=CARTESIAN_POINT('Ctrl Pts',(161.550803013679,-3.59728072279349,331.643378288241));
#49774=CARTESIAN_POINT('Ctrl Pts',(161.543149912777,-3.68806030934209,331.743369166094));
#49775=CARTESIAN_POINT('Ctrl Pts',(161.535496811876,-3.77466469062467,331.847050660754));
#49776=CARTESIAN_POINT('Ctrl Pts',(161.527851236346,-3.86118391293253,331.950630204339));
#49777=CARTESIAN_POINT('Ctrl Pts',(161.520205660817,-3.9435358393365,332.057892839009));
#49778=CARTESIAN_POINT('Ctrl Pts',(161.512560085287,-4.02138896951369,332.168460874653));
#49779=CARTESIAN_POINT('Ctrl Pts',(161.504920220443,-4.09918394910211,332.278946324068));
#49780=CARTESIAN_POINT('Ctrl Pts',(161.497280355599,-4.17248658767544,332.392731933326));
#49781=CARTESIAN_POINT('Ctrl Pts',(161.489640490754,-4.24100589435396,332.509407286095));
#49782=CARTESIAN_POINT('Ctrl Pts',(161.482003627416,-4.309498281563,332.626036800126));
#49783=CARTESIAN_POINT('Ctrl Pts',(161.474366764078,-4.37321086956943,332.745553453304));
#49784=CARTESIAN_POINT('Ctrl Pts',(161.46672990074,-4.43189642539113,332.867518549411));
#49785=CARTESIAN_POINT('Ctrl Pts',(161.459094273276,-4.4905724841177,332.989463907883));
#49786=CARTESIAN_POINT('Ctrl Pts',(161.451458645813,-4.54422295440155,333.113856557851));
#49787=CARTESIAN_POINT('Ctrl Pts',(161.44382301835,-4.59264719957257,333.240234458015));
#49788=CARTESIAN_POINT('Ctrl Pts',(161.436186862408,-4.64107479629268,333.366621105072));
#49789=CARTESIAN_POINT('Ctrl Pts',(161.428550706467,-4.68427530587899,333.494992898575));
#49790=CARTESIAN_POINT('Ctrl Pts',(161.420914550525,-4.72209695484482,333.624869674705));
#49791=CARTESIAN_POINT('Ctrl Pts',(161.413272626461,-4.75994717314507,333.754844555841));
#49792=CARTESIAN_POINT('Ctrl Pts',(161.405630702397,-4.79241030582818,333.8863263019));
#49793=CARTESIAN_POINT('Ctrl Pts',(161.397988778333,-4.81938498220931,334.018821394569));
#49794=CARTESIAN_POINT('Ctrl Pts',(161.390343575079,-4.84637123356366,334.151373341568));
#49795=CARTESIAN_POINT('Ctrl Pts',(161.382698371826,-4.86786427431226,334.284939103521));
#49796=CARTESIAN_POINT('Ctrl Pts',(161.375053168573,-4.88381441428653,334.419018219471));
#49797=CARTESIAN_POINT('Ctrl Pts',(161.36739888181,-4.89978350513167,334.553256639101));
#49798=CARTESIAN_POINT('Ctrl Pts',(161.359744595046,-4.91019651712291,334.688009229207));
#49799=CARTESIAN_POINT('Ctrl Pts',(161.352090308283,-4.91505583100831,334.822773476671));
#49800=CARTESIAN_POINT('Ctrl Pts',(161.348665997702,-4.91722975007678,334.88306317481));
#49801=CARTESIAN_POINT('Ctrl Pts',(161.345241687122,-4.9182928407637,334.943355239399));
#49802=CARTESIAN_POINT('Ctrl Pts',(161.341817376542,-4.91824867880592,335.003604985961));
#49803=CARTESIAN_POINT('',(159.591817376477,-4.91824852669461,334.996193142206));
#49804=CARTESIAN_POINT('Ctrl Pts',(161.341817376508,-4.91824867880549,335.003604986558));
#49805=CARTESIAN_POINT('Ctrl Pts',(161.328946872652,-4.91808269306071,335.230057750488));
#49806=CARTESIAN_POINT('Ctrl Pts',(161.316076368796,-4.9022757372586,335.45594661472));
#49807=CARTESIAN_POINT('Ctrl Pts',(161.30320586494,-4.87106519079457,335.679637380909));
#49808=CARTESIAN_POINT('Ctrl Pts',(161.295430786162,-4.85221088173329,335.81476910136));
#49809=CARTESIAN_POINT('Ctrl Pts',(161.287655707383,-4.82769933922256,335.949329185067));
#49810=CARTESIAN_POINT('Ctrl Pts',(161.279880628605,-4.7975736730769,336.082806498826));
#49811=CARTESIAN_POINT('Ctrl Pts',(161.272115117556,-4.76748507848133,336.216119560253));
#49812=CARTESIAN_POINT('Ctrl Pts',(161.264349606507,-4.73179619149024,336.348352125223));
#49813=CARTESIAN_POINT('Ctrl Pts',(161.256584095458,-4.69060177250676,336.478999010904));
#49814=CARTESIAN_POINT('Ctrl Pts',(161.248826283936,-4.64944819790967,336.609516359819));
#49815=CARTESIAN_POINT('Ctrl Pts',(161.241068472414,-4.6028000713285,336.738450787843));
#49816=CARTESIAN_POINT('Ctrl Pts',(161.233310660892,-4.55080293398656,336.865308478113));
#49817=CARTESIAN_POINT('Ctrl Pts',(161.225558687369,-4.4988449261394,336.992070703948));
#49818=CARTESIAN_POINT('Ctrl Pts',(161.217806713846,-4.44154606734189,337.116758942513));
#49819=CARTESIAN_POINT('Ctrl Pts',(161.210054740323,-4.37910123310724,337.238896034366));
#49820=CARTESIAN_POINT('Ctrl Pts',(161.202306049765,-4.31668284429689,337.360981401088));
#49821=CARTESIAN_POINT('Ctrl Pts',(161.194557359207,-4.24912299213488,337.48051742266));
#49822=CARTESIAN_POINT('Ctrl Pts',(161.18680866865,-4.17666394771121,337.597048580676));
#49823=CARTESIAN_POINT('Ctrl Pts',(161.179061590272,-4.10421997899693,337.713555493411));
#49824=CARTESIAN_POINT('Ctrl Pts',(161.171314511894,-4.02687905178526,337.827058454403));
#49825=CARTESIAN_POINT('Ctrl Pts',(161.163567433516,-3.94492829733129,337.937128494195));
#49826=CARTESIAN_POINT('Ctrl Pts',(161.15582029021,-3.86297685605107,338.047199456481));
#49827=CARTESIAN_POINT('Ctrl Pts',(161.148073146905,-3.77641574389466,338.153837126662));
#49828=CARTESIAN_POINT('Ctrl Pts',(161.140326003599,-3.68557389822131,338.256643686873));
#49829=CARTESIAN_POINT('Ctrl Pts',(161.132577118571,-3.59471162937241,338.359473360181));
#49830=CARTESIAN_POINT('Ctrl Pts',(161.124828233543,-3.49956697070729,338.458469916748));
#49831=CARTESIAN_POINT('Ctrl Pts',(161.117079348514,-3.40050712908165,338.5532709336));
#49832=CARTESIAN_POINT('Ctrl Pts',(161.10932223874,-3.30134214431666,338.64817257323));
#49833=CARTESIAN_POINT('Ctrl Pts',(161.101565128965,-3.19825395819867,338.738869506801));
#49834=CARTESIAN_POINT('Ctrl Pts',(161.09380801919,-3.09164482727954,338.825037950721));
#49835=CARTESIAN_POINT('Ctrl Pts',(161.086046764264,-2.98497872784963,338.911252440302));
#49836=CARTESIAN_POINT('Ctrl Pts',(161.078285509338,-2.87478824845055,338.992933385753));
#49837=CARTESIAN_POINT('Ctrl Pts',(161.070524254412,-2.76150547943597,339.069799816888));
#49838=CARTESIAN_POINT('Ctrl Pts',(161.062750584007,-2.64804149490968,339.146789209263));
#49839=CARTESIAN_POINT('Ctrl Pts',(161.054976913602,-2.5314756684073,339.218948491291));
#49840=CARTESIAN_POINT('Ctrl Pts',(161.047203243198,-2.41226635401111,339.286041775322));
#49841=CARTESIAN_POINT('Ctrl Pts',(161.039791439021,-2.29860626187827,339.350011850841));
#49842=CARTESIAN_POINT('Ctrl Pts',(161.032379634843,-2.18254350827548,339.409376827658));
#49843=CARTESIAN_POINT('Ctrl Pts',(161.024967830666,-2.06449130336647,339.463973422952));
#49844=CARTESIAN_POINT('Ctrl Pts',(161.017192751888,-1.94065300823737,339.521245960016));
#49845=CARTESIAN_POINT('Ctrl Pts',(161.009417673109,-1.81423396101038,339.573451863338));
#49846=CARTESIAN_POINT('Ctrl Pts',(161.001642594331,-1.68568731369463,339.620350781375));
#49847=CARTESIAN_POINT('Ctrl Pts',(160.993877083282,-1.55729885121218,339.667191987307));
#49848=CARTESIAN_POINT('Ctrl Pts',(160.986111572233,-1.42678836169221,339.708739069256));
#49849=CARTESIAN_POINT('Ctrl Pts',(160.978346061184,-1.29463194444584,339.744798329847));
#49850=CARTESIAN_POINT('Ctrl Pts',(160.970588249662,-1.16260656067179,339.780821837577));
#49851=CARTESIAN_POINT('Ctrl Pts',(160.962830438139,-1.02893887148868,339.81136825));
#49852=CARTESIAN_POINT('Ctrl Pts',(160.955072626617,-0.89412289873917,339.836292723197));
#49853=CARTESIAN_POINT('Ctrl Pts',(160.947320653094,-0.759408379284553,
339.861198439937));
#49854=CARTESIAN_POINT('Ctrl Pts',(160.939568679571,-0.623547679064922,
339.880490567654));
#49855=CARTESIAN_POINT('Ctrl Pts',(160.931816706048,-0.48704750995685,339.89407476297));
#49856=CARTESIAN_POINT('Ctrl Pts',(160.92406801549,-0.350605148751389,339.907653205372));
#49857=CARTESIAN_POINT('Ctrl Pts',(160.916319324933,-0.213524245433846,
339.915528484611));
#49858=CARTESIAN_POINT('Ctrl Pts',(160.908570634375,-0.076318961938044,
339.917657824468));
#49859=CARTESIAN_POINT('Ctrl Pts',(160.900823555997,0.0608577748525656,
339.919786721298));
#49860=CARTESIAN_POINT('Ctrl Pts',(160.89307647762,0.198158449765743,339.9161720506));
#49861=CARTESIAN_POINT('Ctrl Pts',(160.885329399242,0.335066950037492,339.906823127186));
#49862=CARTESIAN_POINT('Ctrl Pts',(160.877582255936,0.471976597734317,339.89747412542));
#49863=CARTESIAN_POINT('Ctrl Pts',(160.86983511263,0.608493674267794,339.88239080171));
#49864=CARTESIAN_POINT('Ctrl Pts',(160.862087969324,0.744105639228933,339.861634484427));
#49865=CARTESIAN_POINT('Ctrl Pts',(160.854339084296,0.879748092638826,339.840873500683));
#49866=CARTESIAN_POINT('Ctrl Pts',(160.846590199268,1.0144846432581,339.814437044568));
#49867=CARTESIAN_POINT('Ctrl Pts',(160.83884131424,1.14781180517559,339.782437780296));
#49868=CARTESIAN_POINT('Ctrl Pts',(160.831084204465,1.28128048192034,339.750404551673));
#49869=CARTESIAN_POINT('Ctrl Pts',(160.823327094691,1.41333640100232,339.712796811621));
#49870=CARTESIAN_POINT('Ctrl Pts',(160.815569984916,1.54348960178851,339.669777608374));
#49871=CARTESIAN_POINT('Ctrl Pts',(160.80780872999,1.67371235228364,339.62673541704));
#49872=CARTESIAN_POINT('Ctrl Pts',(160.800047475063,1.80202999303155,339.578276138538));
#49873=CARTESIAN_POINT('Ctrl Pts',(160.792286220137,1.92797242132446,339.524611077774));
#49874=CARTESIAN_POINT('Ctrl Pts',(160.784512549733,2.0541163164581,339.470860170402));
#49875=CARTESIAN_POINT('Ctrl Pts',(160.776738879328,2.17787705343211,339.411887008077));
#49876=CARTESIAN_POINT('Ctrl Pts',(160.768965208923,2.29880822759548,339.347949378183));
#49877=CARTESIAN_POINT('Ctrl Pts',(160.761553404746,2.41411002650719,339.286988060343));
#49878=CARTESIAN_POINT('Ctrl Pts',(160.754141600569,2.52683951766054,339.221514210066));
#49879=CARTESIAN_POINT('Ctrl Pts',(160.746729796392,2.6366357813195,339.151786942892));
#49880=CARTESIAN_POINT('Ctrl Pts',(160.738954717614,2.75181348692667,339.078642134646));
#49881=CARTESIAN_POINT('Ctrl Pts',(160.731179638835,2.86412714517176,339.000585270662));
#49882=CARTESIAN_POINT('Ctrl Pts',(160.723404560057,2.97312941276129,338.917867348121));
#49883=CARTESIAN_POINT('Ctrl Pts',(160.715639049008,3.08199754612111,338.83525121525));
#49884=CARTESIAN_POINT('Ctrl Pts',(160.707873537959,3.18756208826918,338.747985670306));
#49885=CARTESIAN_POINT('Ctrl Pts',(160.70010802691,3.28940251029697,338.656366254596));
#49886=CARTESIAN_POINT('Ctrl Pts',(160.692350215388,3.39114195724982,338.564837679804));
#49887=CARTESIAN_POINT('Ctrl Pts',(160.684592403866,3.48916434360316,338.46896408481));
#49888=CARTESIAN_POINT('Ctrl Pts',(160.676834592343,3.58308052344825,338.369082519765));
#49889=CARTESIAN_POINT('Ctrl Pts',(160.66908261882,3.67692602838971,338.269276118765));
#49890=CARTESIAN_POINT('Ctrl Pts',(160.661330645297,3.76667121074038,338.165468034779));
#49891=CARTESIAN_POINT('Ctrl Pts',(160.653578671774,3.85196252427038,338.058033318019));
#49892=CARTESIAN_POINT('Ctrl Pts',(160.645829981217,3.9372177168785,337.950644099926));
#49893=CARTESIAN_POINT('Ctrl Pts',(160.638081290659,4.01802254968772,337.839631609313));
#49894=CARTESIAN_POINT('Ctrl Pts',(160.630332600102,4.09406280873805,337.725405067253));
#49895=CARTESIAN_POINT('Ctrl Pts',(160.622585521724,4.17008724697739,337.611202290979));
#49896=CARTESIAN_POINT('Ctrl Pts',(160.614838443346,4.24134886677871,337.493787118539));
#49897=CARTESIAN_POINT('Ctrl Pts',(160.607091364968,4.3075762029348,337.373598600945));
#49898=CARTESIAN_POINT('Ctrl Pts',(160.599344221662,4.37380409413971,337.253409076056));
#49899=CARTESIAN_POINT('Ctrl Pts',(160.591597078357,4.434997428904,337.130446501995));
#49900=CARTESIAN_POINT('Ctrl Pts',(160.583849935051,4.49093041453717,337.005175073226));
#49901=CARTESIAN_POINT('Ctrl Pts',(160.576101050023,4.54687597509297,336.879875480779));
#49902=CARTESIAN_POINT('Ctrl Pts',(160.568352164995,4.59755867387115,336.752266357558));
#49903=CARTESIAN_POINT('Ctrl Pts',(160.560603279966,4.64280078749434,336.622832064676));
#49904=CARTESIAN_POINT('Ctrl Pts',(160.552846170192,4.68809092156441,336.493260388898));
#49905=CARTESIAN_POINT('Ctrl Pts',(160.545089060417,4.72792880581079,336.361860043179));
#49906=CARTESIAN_POINT('Ctrl Pts',(160.537331950642,4.76218640516041,336.229131280623));
#49907=CARTESIAN_POINT('Ctrl Pts',(160.529570695716,4.79646231067577,336.09633159206));
#49908=CARTESIAN_POINT('Ctrl Pts',(160.52180944079,4.82515190782318,335.962202454228));
#49909=CARTESIAN_POINT('Ctrl Pts',(160.514048185864,4.84817848785695,335.827253535732));
#49910=CARTESIAN_POINT('Ctrl Pts',(160.506274515459,4.87124190291443,335.692088742947));
#49911=CARTESIAN_POINT('Ctrl Pts',(160.498500845055,4.88862414874428,335.556101936892));
#49912=CARTESIAN_POINT('Ctrl Pts',(160.49072717465,4.9003004290861,335.419808012309));
#49913=CARTESIAN_POINT('Ctrl Pts',(160.483315370473,4.91143317576882,335.289858602705));
#49914=CARTESIAN_POINT('Ctrl Pts',(160.475903566296,4.91737921432763,335.159630311343));
#49915=CARTESIAN_POINT('Ctrl Pts',(160.468491762119,4.91816112616878,335.029566865614));
#49916=CARTESIAN_POINT('Ctrl Pts',(160.46071668334,4.91898136183845,334.893128622971));
#49917=CARTESIAN_POINT('Ctrl Pts',(160.452941604562,4.91412104467701,334.756440623642));
#49918=CARTESIAN_POINT('Ctrl Pts',(160.445166525784,4.90354916044425,334.620014877125));
#49919=CARTESIAN_POINT('Ctrl Pts',(160.437401014735,4.89299028558807,334.483757011173));
#49920=CARTESIAN_POINT('Ctrl Pts',(160.429635503686,4.87673385816498,334.347761141896));
#49921=CARTESIAN_POINT('Ctrl Pts',(160.421869992637,4.85480083284138,334.212540835381));
#49922=CARTESIAN_POINT('Ctrl Pts',(160.414112181114,4.83288955417625,334.077454600194));
#49923=CARTESIAN_POINT('Ctrl Pts',(160.406354369592,4.80531294055152,333.943142780816));
#49924=CARTESIAN_POINT('Ctrl Pts',(160.39859655807,4.77214383544901,333.810115015522));
#49925=CARTESIAN_POINT('Ctrl Pts',(160.390844584547,4.73899969114995,333.67718735784));
#49926=CARTESIAN_POINT('Ctrl Pts',(160.383092611024,4.70027152642522,333.54554220862));
#49927=CARTESIAN_POINT('Ctrl Pts',(160.375340637501,4.65608340484845,333.415679833621));
#49928=CARTESIAN_POINT('Ctrl Pts',(160.367591946943,4.61191399696739,333.285872455415));
#49929=CARTESIAN_POINT('Ctrl Pts',(160.359843256386,4.56228935687671,333.157846719044));
#49930=CARTESIAN_POINT('Ctrl Pts',(160.352094565828,4.50738356810354,333.032088306735));
#49931=CARTESIAN_POINT('Ctrl Pts',(160.34434748745,4.4524892029383,332.906356059513));
#49932=CARTESIAN_POINT('Ctrl Pts',(160.336600409073,4.39231603095595,332.782890556034));
#49933=CARTESIAN_POINT('Ctrl Pts',(160.328853330695,4.32708635411989,332.662157672877));
#49934=CARTESIAN_POINT('Ctrl Pts',(160.321106187389,4.26185613059634,332.541423777861));
#49935=CARTESIAN_POINT('Ctrl Pts',(160.313359044083,4.19156950349053,332.42342289274));
#49936=CARTESIAN_POINT('Ctrl Pts',(160.305611900777,4.11649463444983,332.308596093663));
#49937=CARTESIAN_POINT('Ctrl Pts',(160.297863015749,4.04140288698472,332.193743479084));
#49938=CARTESIAN_POINT('Ctrl Pts',(160.290114130721,3.96152096932861,332.082066697628));
#49939=CARTESIAN_POINT('Ctrl Pts',(160.282365245693,3.87716001475814,331.973977316268));
#49940=CARTESIAN_POINT('Ctrl Pts',(160.274608135918,3.79270951859882,331.865773207721));
#49941=CARTESIAN_POINT('Ctrl Pts',(160.266851026144,3.70377072964302,331.761164414135));
#49942=CARTESIAN_POINT('Ctrl Pts',(160.259093916369,3.6106950342744,331.660529318595));
#49943=CARTESIAN_POINT('Ctrl Pts',(160.251332661443,3.51756960223016,331.559840446876));
#49944=CARTESIAN_POINT('Ctrl Pts',(160.243571406517,3.42030313593273,331.46312977976));
#49945=CARTESIAN_POINT('Ctrl Pts',(160.23581015159,3.31928271508222,331.370737634194));
#49946=CARTESIAN_POINT('Ctrl Pts',(160.228036481186,3.21810069448084,331.278197691305));
#49947=CARTESIAN_POINT('Ctrl Pts',(160.220262810781,3.11315301873013,331.189990326276));
#49948=CARTESIAN_POINT('Ctrl Pts',(160.212489140376,3.00485925512245,331.106415029898));
#49949=CARTESIAN_POINT('Ctrl Pts',(160.205077336199,2.90160659226398,331.026730183673));
#49950=CARTESIAN_POINT('Ctrl Pts',(160.197665532022,2.7953125864056,330.951256032041));
#49951=CARTESIAN_POINT('Ctrl Pts',(160.190253727845,2.68636259747263,330.880213712169));
#49952=CARTESIAN_POINT('Ctrl Pts',(160.182478649067,2.57207264503745,330.805689396576));
#49953=CARTESIAN_POINT('Ctrl Pts',(160.174703570288,2.45449859379039,330.735806821375));
#49954=CARTESIAN_POINT('Ctrl Pts',(160.16692849151,2.33405421985501,330.670869144819));
#49955=CARTESIAN_POINT('Ctrl Pts',(160.159162980461,2.21375806038963,330.606011378209));
#49956=CARTESIAN_POINT('Ctrl Pts',(160.151397469412,2.09059894689708,330.546086586537));
#49957=CARTESIAN_POINT('Ctrl Pts',(160.143631958363,1.96502008783066,330.491355068657));
#49958=CARTESIAN_POINT('Ctrl Pts',(160.13587414684,1.83956574056873,330.436677817237));
#49959=CARTESIAN_POINT('Ctrl Pts',(160.128116335318,1.71169677825932,330.38718374768));
#49960=CARTESIAN_POINT('Ctrl Pts',(160.120358523796,1.58188118638672,330.34308739886));
#49961=CARTESIAN_POINT('Ctrl Pts',(160.112606550273,1.45216328486356,330.299024233941));
#49962=CARTESIAN_POINT('Ctrl Pts',(160.10485457675,1.32050203820445,330.260350829848));
#49963=CARTESIAN_POINT('Ctrl Pts',(160.097102603227,1.18738526847622,330.22723358138));
#49964=CARTESIAN_POINT('Ctrl Pts',(160.089353912669,1.05432487377899,330.194130358087));
#49965=CARTESIAN_POINT('Ctrl Pts',(160.081605222112,0.919810560541087,330.166578704569));
#49966=CARTESIAN_POINT('Ctrl Pts',(160.073856531554,0.784344955893373,330.144695060795));
#49967=CARTESIAN_POINT('Ctrl Pts',(160.066109453176,0.648907535996137,330.122815970097));
#49968=CARTESIAN_POINT('Ctrl Pts',(160.058362374799,0.51251960400369,330.106602605773));
#49969=CARTESIAN_POINT('Ctrl Pts',(160.050615296421,0.375693225819414,330.096120141911));
#49970=CARTESIAN_POINT('Ctrl Pts',(160.042868153115,0.238865700898394,330.085637590195));
#49971=CARTESIAN_POINT('Ctrl Pts',(160.035121009809,0.101600112188512,330.0808860646));
#49972=CARTESIAN_POINT('Ctrl Pts',(160.027373866503,-0.0355875123107284,
330.081878753887));
#49973=CARTESIAN_POINT('Ctrl Pts',(160.019624981475,-0.172805979500602,
330.082871666352));
#49974=CARTESIAN_POINT('Ctrl Pts',(160.011876096447,-0.309946056813376,
330.089611360657));
#49975=CARTESIAN_POINT('Ctrl Pts',(160.004127211419,-0.446493276734069,
330.102058920696));
#49976=CARTESIAN_POINT('Ctrl Pts',(159.996370101644,-0.583185429284782,
330.114519692704));
#49977=CARTESIAN_POINT('Ctrl Pts',(159.98861299187,-0.719283077552539,330.132700397102));
#49978=CARTESIAN_POINT('Ctrl Pts',(159.980855882095,-0.854277875794783,
330.156510310383));
#49979=CARTESIAN_POINT('Ctrl Pts',(159.973094627169,-0.989344810940912,
330.18033294692));
#49980=CARTESIAN_POINT('Ctrl Pts',(159.965333372242,-1.12330734021289,330.209790702285));
#49981=CARTESIAN_POINT('Ctrl Pts',(159.957572117316,-1.25566981279231,330.244742237928));
#49982=CARTESIAN_POINT('Ctrl Pts',(159.949798446912,-1.38824402219101,330.279749684638));
#49983=CARTESIAN_POINT('Ctrl Pts',(159.942024776507,-1.51921268651118,330.320268357582));
#49984=CARTESIAN_POINT('Ctrl Pts',(159.934251106102,-1.64809690561911,330.366107505327));
#49985=CARTESIAN_POINT('Ctrl Pts',(159.926839301925,-1.77098153331938,330.409812829715));
#49986=CARTESIAN_POINT('Ctrl Pts',(159.919427497748,-1.89197114331462,330.45835433277));
#49987=CARTESIAN_POINT('Ctrl Pts',(159.912015693571,-2.01067123627604,330.511527627119));
#49988=CARTESIAN_POINT('Ctrl Pts',(159.904240614793,-2.13518917438329,330.56730710302));
#49989=CARTESIAN_POINT('Ctrl Pts',(159.896465536014,-2.25758098827673,330.628360159743));
#49990=CARTESIAN_POINT('Ctrl Pts',(159.888690457236,-2.37736782771031,330.694502900446));
#49991=CARTESIAN_POINT('Ctrl Pts',(159.880924946187,-2.497007261812,330.760564248296));
#49992=CARTESIAN_POINT('Ctrl Pts',(159.873159435138,-2.61404776074752,330.831702631058));
#49993=CARTESIAN_POINT('Ctrl Pts',(159.865393924089,-2.72803058813252,330.907686207936));
#49994=CARTESIAN_POINT('Ctrl Pts',(159.857636112566,-2.84190040121241,330.983594446877));
#49995=CARTESIAN_POINT('Ctrl Pts',(159.849878301044,-2.95271825283825,331.064338104241));
#49996=CARTESIAN_POINT('Ctrl Pts',(159.842120489522,-3.06005047889474,331.149639740347));
#49997=CARTESIAN_POINT('Ctrl Pts',(159.834368515999,-3.16730193404739,331.234877184266));
#49998=CARTESIAN_POINT('Ctrl Pts',(159.826616542476,-3.27107267989869,331.324665537417));
#49999=CARTESIAN_POINT('Ctrl Pts',(159.818864568953,-3.37095880299916,331.41868462559));
#50000=CARTESIAN_POINT('Ctrl Pts',(159.811115878395,-3.4708026242671,331.512663896624));
#50001=CARTESIAN_POINT('Ctrl Pts',(159.803367187838,-3.56676481082179,331.610870071731));
#50002=CARTESIAN_POINT('Ctrl Pts',(159.79561849728,-3.65847544542785,331.712943493382));
#50003=CARTESIAN_POINT('Ctrl Pts',(159.787871418902,-3.7501669988704,331.814995677805));
#50004=CARTESIAN_POINT('Ctrl Pts',(159.780124340524,-3.837608498766,331.920913217768));
#50005=CARTESIAN_POINT('Ctrl Pts',(159.772377262147,-3.92046803059277,332.030300775567));
#50006=CARTESIAN_POINT('Ctrl Pts',(159.764630118841,-4.00332825686225,332.139689250138));
#50007=CARTESIAN_POINT('Ctrl Pts',(159.756882975535,-4.08160620245395,332.252547488975));
#50008=CARTESIAN_POINT('Ctrl Pts',(159.749135832229,-4.15501152429481,332.36844869032));
#50009=CARTESIAN_POINT('Ctrl Pts',(159.741386947201,-4.22843334921032,332.484375948716));
#50010=CARTESIAN_POINT('Ctrl Pts',(159.733638062173,-4.29698016141381,332.603347200795));
#50011=CARTESIAN_POINT('Ctrl Pts',(159.725889177145,-4.36040627839692,332.724908760112));
#50012=CARTESIAN_POINT('Ctrl Pts',(159.71813206737,-4.423899716516,332.846599346123));
#50013=CARTESIAN_POINT('Ctrl Pts',(159.710374957595,-4.48226142107828,332.970885384426));
#50014=CARTESIAN_POINT('Ctrl Pts',(159.702617847821,-4.53529258836708,333.097290300544));
#50015=CARTESIAN_POINT('Ctrl Pts',(159.694856592894,-4.58835209381604,333.223762763408));
#50016=CARTESIAN_POINT('Ctrl Pts',(159.687095337968,-4.63607525023321,333.352355993952));
#50017=CARTESIAN_POINT('Ctrl Pts',(159.679334083042,-4.67831268712215,333.482576702429));
#50018=CARTESIAN_POINT('Ctrl Pts',(159.671560412637,-4.72061769014494,333.6130057216));
#50019=CARTESIAN_POINT('Ctrl Pts',(159.663786742233,-4.75741933288212,333.745067044412));
#50020=CARTESIAN_POINT('Ctrl Pts',(159.656013071828,-4.78861886194275,333.878254726978));
#50021=CARTESIAN_POINT('Ctrl Pts',(159.648601267651,-4.81836604541947,334.005242490878));
#50022=CARTESIAN_POINT('Ctrl Pts',(159.641189463474,-4.84302088026373,334.133253827738));
#50023=CARTESIAN_POINT('Ctrl Pts',(159.633777659297,-4.86254175395446,334.261846388921));
#50024=CARTESIAN_POINT('Ctrl Pts',(159.620632863804,-4.89716192016204,334.489904615808));
#50025=CARTESIAN_POINT('Ctrl Pts',(159.607488068311,-4.91574372033797,334.72045707603));
#50026=CARTESIAN_POINT('Ctrl Pts',(159.594343272817,-4.91801323229811,334.95174122421));
#50027=CARTESIAN_POINT('Ctrl Pts',(159.593501307381,-4.91815860166723,334.966555700317));
#50028=CARTESIAN_POINT('Ctrl Pts',(159.592659341944,-4.91823705562696,334.981373162964));
#50029=CARTESIAN_POINT('Ctrl Pts',(159.591817376508,-4.91824852669419,334.996193141659));
#50030=CARTESIAN_POINT('',(157.841817376542,-4.91824974369148,334.99841217802));
#50031=CARTESIAN_POINT('Ctrl Pts',(159.591817376477,-4.91824852669461,334.996193142206));
#50032=CARTESIAN_POINT('Ctrl Pts',(159.584166148112,-4.91835276819738,335.130867365703));
#50033=CARTESIAN_POINT('Ctrl Pts',(159.576514919747,-4.91292126616045,335.265748454898));
#50034=CARTESIAN_POINT('Ctrl Pts',(159.568863691381,-4.90192965851686,335.400335715934));
#50035=CARTESIAN_POINT('Ctrl Pts',(159.561220060556,-4.89094896535318,335.534789334105));
#50036=CARTESIAN_POINT('Ctrl Pts',(159.553576429731,-4.87441917997282,335.668949305156));
#50037=CARTESIAN_POINT('Ctrl Pts',(159.545932798906,-4.85236797623589,335.802314206343));
#50038=CARTESIAN_POINT('Ctrl Pts',(159.537999749994,-4.82948182673326,335.940728830026));
#50039=CARTESIAN_POINT('Ctrl Pts',(159.530066701082,-4.80064787934645,336.078286547999));
#50040=CARTESIAN_POINT('Ctrl Pts',(159.52213365217,-4.76595634042732,336.214431234628));
#50041=CARTESIAN_POINT('Ctrl Pts',(159.514498681209,-4.7325683082593,336.34546039385));
#50042=CARTESIAN_POINT('Ctrl Pts',(159.506863710247,-4.69375501710053,336.47518035946));
#50043=CARTESIAN_POINT('Ctrl Pts',(159.499228739286,-4.64964898909618,336.603105530119));
#50044=CARTESIAN_POINT('Ctrl Pts',(159.491594952606,-4.60554980250131,336.731010857945));
#50045=CARTESIAN_POINT('Ctrl Pts',(159.483961165926,-4.55615964273177,336.857121563007));
#50046=CARTESIAN_POINT('Ctrl Pts',(159.476327379246,-4.50166060189852,336.980968169309));
#50047=CARTESIAN_POINT('Ctrl Pts',(159.468693011005,-4.44715740918385,337.104824210573));
#50048=CARTESIAN_POINT('Ctrl Pts',(159.461058642763,-4.38754472437907,337.226415440962));
#50049=CARTESIAN_POINT('Ctrl Pts',(159.453424274521,-4.32305215521528,337.345293825044));
#50050=CARTESIAN_POINT('Ctrl Pts',(159.445787558591,-4.25853975357349,337.464208766096));
#50051=CARTESIAN_POINT('Ctrl Pts',(159.438150842661,-4.18914467634525,337.58040884784));
#50052=CARTESIAN_POINT('Ctrl Pts',(159.430514126731,-4.11514140890666,337.693472525793));
#50053=CARTESIAN_POINT('Ctrl Pts',(159.422869241791,-4.04105898002964,337.806657148181));
#50054=CARTESIAN_POINT('Ctrl Pts',(159.415224356851,-3.96235874420188,337.916698333462));
#50055=CARTESIAN_POINT('Ctrl Pts',(159.407579471911,-3.87935739097104,338.023205136212));
#50056=CARTESIAN_POINT('Ctrl Pts',(159.399929727442,-3.79630327729702,338.129779640824));
#50057=CARTESIAN_POINT('Ctrl Pts',(159.392279982972,-3.70894286462007,338.232814984739));
#50058=CARTESIAN_POINT('Ctrl Pts',(159.384630238503,-3.61763077036886,338.33195598287));
#50059=CARTESIAN_POINT('Ctrl Pts',(159.376969842564,-3.52619153357005,338.431235024478));
#50060=CARTESIAN_POINT('Ctrl Pts',(159.369309446625,-3.43078992058651,338.526608617573));
#50061=CARTESIAN_POINT('Ctrl Pts',(159.361649050686,-3.33181489974728,338.617760707443));
#50062=CARTESIAN_POINT('Ctrl Pts',(159.359612575465,-3.3055029206965,338.641993002206));
#50063=CARTESIAN_POINT('Ctrl Pts',(159.357576100244,-3.27893856162204,338.665927182308));
#50064=CARTESIAN_POINT('Ctrl Pts',(159.355539625023,-3.25212947502574,338.689557824478));
#50065=CARTESIAN_POINT('Ctrl Pts',(159.347764546244,-3.14977479961162,338.779777485656));
#50066=CARTESIAN_POINT('Ctrl Pts',(159.339989467466,-3.04350126674975,338.865877242081));
#50067=CARTESIAN_POINT('Ctrl Pts',(159.332214388687,-2.93367463500481,338.947497460218));
#50068=CARTESIAN_POINT('Ctrl Pts',(159.324448877638,-2.82398315192221,339.029017239481));
#50069=CARTESIAN_POINT('Ctrl Pts',(159.316683366589,-2.71074758033384,339.106068217542));
#50070=CARTESIAN_POINT('Ctrl Pts',(159.30891785554,-2.59436898147057,339.178328930384));
#50071=CARTESIAN_POINT('Ctrl Pts',(159.301160044018,-2.47810577232699,339.250517996519));
#50072=CARTESIAN_POINT('Ctrl Pts',(159.293402232496,-2.35870606749338,339.317926044473));
#50073=CARTESIAN_POINT('Ctrl Pts',(159.285644420974,-2.23660204226525,339.380273321042));
#50074=CARTESIAN_POINT('Ctrl Pts',(159.277892447451,-2.11458990418783,339.442573679309));
#50075=CARTESIAN_POINT('Ctrl Pts',(159.270140473928,-1.98987784317406,339.499820669568));
#50076=CARTESIAN_POINT('Ctrl Pts',(159.262388500405,-1.86292460336547,339.551779320736));
#50077=CARTESIAN_POINT('Ctrl Pts',(159.254639809847,-1.73602512832963,339.603715967383));
#50078=CARTESIAN_POINT('Ctrl Pts',(159.246891119289,-1.6068867232691,339.650368581628));
#50079=CARTESIAN_POINT('Ctrl Pts',(159.239142428732,-1.47598998319402,339.691549491587));
#50080=CARTESIAN_POINT('Ctrl Pts',(159.231395350354,-1.34512047727888,339.732721833514));
#50081=CARTESIAN_POINT('Ctrl Pts',(159.223648271976,-1.21249373664676,339.768424618352));
#50082=CARTESIAN_POINT('Ctrl Pts',(159.215901193598,-1.07860708589481,339.798519544272));
#50083=CARTESIAN_POINT('Ctrl Pts',(159.208154050293,-0.944719313043811,
339.828614722416));
#50084=CARTESIAN_POINT('Ctrl Pts',(159.200406906987,-0.809571990370545,
339.853101862176));
#50085=CARTESIAN_POINT('Ctrl Pts',(159.192659763681,-0.673673856271418,
339.871893533102));
#50086=CARTESIAN_POINT('Ctrl Pts',(159.184910878653,-0.537745169386592,
339.890689428794));
#50087=CARTESIAN_POINT('Ctrl Pts',(159.177161993625,-0.401065722300536,
339.903787254145));
#50088=CARTESIAN_POINT('Ctrl Pts',(159.169413108597,-0.264150219528999,
339.911151364397));
#50089=CARTESIAN_POINT('Ctrl Pts',(159.161655998822,-0.127089393228288,
339.918523290993));
#50090=CARTESIAN_POINT('Ctrl Pts',(159.153898889047,0.0102075983322991,
339.920149324457));
#50091=CARTESIAN_POINT('Ctrl Pts',(159.146141779273,0.147224641051112,339.916045968822));
#50092=CARTESIAN_POINT('Ctrl Pts',(159.138380524346,0.284314901296692,339.911940420484));
#50093=CARTESIAN_POINT('Ctrl Pts',(159.13061926942,0.421124524948384,339.902099410557));
#50094=CARTESIAN_POINT('Ctrl Pts',(159.122858014494,0.557142664695376,339.886591359391));
#50095=CARTESIAN_POINT('Ctrl Pts',(159.115084344089,0.693378389137686,339.871058500398));
#50096=CARTESIAN_POINT('Ctrl Pts',(159.107310673685,0.828819713232416,339.849840545302));
#50097=CARTESIAN_POINT('Ctrl Pts',(159.09953700328,0.962965243144901,339.823057225764));
#50098=CARTESIAN_POINT('Ctrl Pts',(159.092125199103,1.09086626636593,339.797520676194));
#50099=CARTESIAN_POINT('Ctrl Pts',(159.084713394926,1.21758913919218,339.76692530484));
#50100=CARTESIAN_POINT('Ctrl Pts',(159.077301590749,1.34271402178142,339.731416502297));
#50101=CARTESIAN_POINT('Ctrl Pts',(159.06952651197,1.47397164759447,339.694167307567));
#50102=CARTESIAN_POINT('Ctrl Pts',(159.061751433192,1.60388547623542,339.651393145142));
#50103=CARTESIAN_POINT('Ctrl Pts',(159.053976354414,1.73195515124559,339.60320697086));
#50104=CARTESIAN_POINT('Ctrl Pts',(159.046210843365,1.85986722836722,339.555080092734));
#50105=CARTESIAN_POINT('Ctrl Pts',(159.038445332316,1.98593930487157,339.501554590223));
#50106=CARTESIAN_POINT('Ctrl Pts',(159.030679821267,2.10968401756242,339.442793761648));
#50107=CARTESIAN_POINT('Ctrl Pts',(159.022922009744,2.23330603701076,339.384091194606));
#50108=CARTESIAN_POINT('Ctrl Pts',(159.015164198222,2.35460493406293,339.320163798152));
#50109=CARTESIAN_POINT('Ctrl Pts',(159.0074063867,2.47311158342917,339.251223607199));
#50110=CARTESIAN_POINT('Ctrl Pts',(158.999654413177,2.59152905278352,339.182335295927));
#50111=CARTESIAN_POINT('Ctrl Pts',(158.991902439654,2.70715812039472,339.108441894467));
#50112=CARTESIAN_POINT('Ctrl Pts',(158.984150466131,2.81955294128599,339.029802014217));
#50113=CARTESIAN_POINT('Ctrl Pts',(158.976401775573,2.9319001629039,338.951195438003));
#50114=CARTESIAN_POINT('Ctrl Pts',(158.968653085016,3.04101554245042,338.867846604634));
#50115=CARTESIAN_POINT('Ctrl Pts',(158.960904394458,3.14648118509957,338.780058096685));
#50116=CARTESIAN_POINT('Ctrl Pts',(158.95315731608,3.25192488474078,338.692287853868));
#50117=CARTESIAN_POINT('Ctrl Pts',(158.945410237703,3.35372005767317,338.600080023705));
#50118=CARTESIAN_POINT('Ctrl Pts',(158.937663159325,3.45148127206204,338.503777974003));
#50119=CARTESIAN_POINT('Ctrl Pts',(158.929916016019,3.54924330578419,338.407475117196));
#50120=CARTESIAN_POINT('Ctrl Pts',(158.922168872713,3.64297103506913,338.307078246715));
#50121=CARTESIAN_POINT('Ctrl Pts',(158.914421729407,3.73231563024755,338.202967857895));
#50122=CARTESIAN_POINT('Ctrl Pts',(158.906672844379,3.82168031198779,338.09883406285));
#50123=CARTESIAN_POINT('Ctrl Pts',(158.898923959351,3.90665964423886,337.990985384718));
#50124=CARTESIAN_POINT('Ctrl Pts',(158.891175074323,3.98694511641619,337.879835360083));
#50125=CARTESIAN_POINT('Ctrl Pts',(158.883417964548,4.06731580442318,337.768567359664));
#50126=CARTESIAN_POINT('Ctrl Pts',(158.875660854774,4.14298245088689,337.653991330368));
#50127=CARTESIAN_POINT('Ctrl Pts',(158.867903744999,4.21367963544295,337.53655021483));
#50128=CARTESIAN_POINT('Ctrl Pts',(158.860142490073,4.28441459831389,337.419046342515));
#50129=CARTESIAN_POINT('Ctrl Pts',(158.852381235147,4.35017462060976,337.298674676133));
#50130=CARTESIAN_POINT('Ctrl Pts',(158.84461998022,4.41074078967135,337.175901824263));
#50131=CARTESIAN_POINT('Ctrl Pts',(158.836846309816,4.471403844865,337.052932575841));
#50132=CARTESIAN_POINT('Ctrl Pts',(158.829072639411,4.52685628584907,336.927554823908));
#50133=CARTESIAN_POINT('Ctrl Pts',(158.821298969006,4.57692746455687,336.800254994906));
#50134=CARTESIAN_POINT('Ctrl Pts',(158.813887164829,4.62466781784968,336.678881003571));
#50135=CARTESIAN_POINT('Ctrl Pts',(158.806475360652,4.66751653519789,336.555760125294));
#50136=CARTESIAN_POINT('Ctrl Pts',(158.799063556475,4.70536867922647,336.431324091551));
#50137=CARTESIAN_POINT('Ctrl Pts',(158.791288477697,4.74507606958935,336.300789077119));
#50138=CARTESIAN_POINT('Ctrl Pts',(158.783513398918,4.77941019099073,336.168394213356));
#50139=CARTESIAN_POINT('Ctrl Pts',(158.77573832014,4.80819525881478,336.034621387567));
#50140=CARTESIAN_POINT('Ctrl Pts',(158.767972809091,4.83694490478029,335.901013177757));
#50141=CARTESIAN_POINT('Ctrl Pts',(158.760207298042,4.86015900241358,335.766030758294));
#50142=CARTESIAN_POINT('Ctrl Pts',(158.752441786993,4.8777111325648,335.630172333377));
#50143=CARTESIAN_POINT('Ctrl Pts',(158.744683975471,4.89524585972788,335.494448612483));
#50144=CARTESIAN_POINT('Ctrl Pts',(158.736926163948,4.90712974154233,335.357850999779));
#50145=CARTESIAN_POINT('Ctrl Pts',(158.729168352426,4.91328721207829,335.220888736988));
#50146=CARTESIAN_POINT('Ctrl Pts',(158.721416378903,4.91944004892239,335.084029542642));
#50147=CARTESIAN_POINT('Ctrl Pts',(158.71366440538,4.91987503446681,334.946806633317));
#50148=CARTESIAN_POINT('Ctrl Pts',(158.705912431857,4.91456836825406,334.809734879033));
#50149=CARTESIAN_POINT('Ctrl Pts',(158.6981637413,4.90926394941759,334.672721174718));
#50150=CARTESIAN_POINT('Ctrl Pts',(158.690415050742,4.89822273018065,334.535858887892));
#50151=CARTESIAN_POINT('Ctrl Pts',(158.682666360184,4.88147301181509,334.399663180022));
#50152=CARTESIAN_POINT('Ctrl Pts',(158.674919281806,4.86472677836834,334.263495808807));
#50153=CARTESIAN_POINT('Ctrl Pts',(158.667172203429,4.84227445589549,334.127995128398));
#50154=CARTESIAN_POINT('Ctrl Pts',(158.659425125051,4.81419621043001,333.99367107267));
#50155=CARTESIAN_POINT('Ctrl Pts',(158.651677981745,4.78611772964179,333.859345891177));
#50156=CARTESIAN_POINT('Ctrl Pts',(158.643930838439,4.75241331179268,333.726197736639));
#50157=CARTESIAN_POINT('Ctrl Pts',(158.636183695133,4.71321415177927,333.594725855227));
#50158=CARTESIAN_POINT('Ctrl Pts',(158.628434810105,4.67400617896248,333.463224416145));
#50159=CARTESIAN_POINT('Ctrl Pts',(158.620685925077,4.62930111746466,333.333400374607));
#50160=CARTESIAN_POINT('Ctrl Pts',(158.612937040049,4.57927976624232,333.205736952121));
#50161=CARTESIAN_POINT('Ctrl Pts',(158.605179930274,4.52920532184094,333.077938026359));
#50162=CARTESIAN_POINT('Ctrl Pts',(158.5974228205,4.47380345858585,332.952304665247));
#50163=CARTESIAN_POINT('Ctrl Pts',(158.589665710725,4.41330302220074,332.829299768109));
#50164=CARTESIAN_POINT('Ctrl Pts',(158.581904455799,4.35277025631687,332.706229141086));
#50165=CARTESIAN_POINT('Ctrl Pts',(158.574143200873,4.28713367541245,332.585790119804));
#50166=CARTESIAN_POINT('Ctrl Pts',(158.566381945946,4.21666719439612,332.468419301266));
#50167=CARTESIAN_POINT('Ctrl Pts',(158.558608275542,4.14608798997516,332.350860727669));
#50168=CARTESIAN_POINT('Ctrl Pts',(158.550834605137,4.0706636612342,332.236380491274));
#50169=CARTESIAN_POINT('Ctrl Pts',(158.543060934732,3.99071090708656,332.125385326942));
#50170=CARTESIAN_POINT('Ctrl Pts',(158.535649130555,3.91447997287979,332.019557014213));
#50171=CARTESIAN_POINT('Ctrl Pts',(158.528237326378,3.83413289928455,331.916896841748));
#50172=CARTESIAN_POINT('Ctrl Pts',(158.520825522201,3.74997595087325,331.817726688298));
#50173=CARTESIAN_POINT('Ctrl Pts',(158.513050443423,3.6616942197298,331.713695910215));
#50174=CARTESIAN_POINT('Ctrl Pts',(158.505275364644,3.56894071745207,331.613177157444));
#50175=CARTESIAN_POINT('Ctrl Pts',(158.497500285866,3.47202554621446,331.51657902789));
#50176=CARTESIAN_POINT('Ctrl Pts',(158.489734774817,3.37522963526517,331.420099768485));
#50177=CARTESIAN_POINT('Ctrl Pts',(158.481969263768,3.27428251926863,331.327531806073));
#50178=CARTESIAN_POINT('Ctrl Pts',(158.474203752719,3.16953473610921,331.239251056093));
#50179=CARTESIAN_POINT('Ctrl Pts',(158.466445941196,3.06489081068179,331.151057836734));
#50180=CARTESIAN_POINT('Ctrl Pts',(158.458688129674,2.95645401432336,331.067143620781));
#50181=CARTESIAN_POINT('Ctrl Pts',(158.450930318152,2.84461168620243,330.987847533154));
#50182=CARTESIAN_POINT('Ctrl Pts',(158.443178344629,2.73285352297982,330.908611118347));
#50183=CARTESIAN_POINT('Ctrl Pts',(158.435426371106,2.61769524664332,330.833986139638));
#50184=CARTESIAN_POINT('Ctrl Pts',(158.427674397583,2.4995569425833,330.76427123705));
#50185=CARTESIAN_POINT('Ctrl Pts',(158.419925707025,2.3814686701653,330.694585858765));
#50186=CARTESIAN_POINT('Ctrl Pts',(158.412177016468,2.26040321607023,330.629806619017));
#50187=CARTESIAN_POINT('Ctrl Pts',(158.40442832591,2.13680910600832,330.570188502094));
#50188=CARTESIAN_POINT('Ctrl Pts',(158.396681247532,2.01324071073345,330.510582789218));
#50189=CARTESIAN_POINT('Ctrl Pts',(158.388934169154,1.88714505779272,330.456136232988));
#50190=CARTESIAN_POINT('Ctrl Pts',(158.381187090777,1.75899434390213,330.407057374556));
#50191=CARTESIAN_POINT('Ctrl Pts',(158.373439947471,1.63084255598512,330.357978104796));
#50192=CARTESIAN_POINT('Ctrl Pts',(158.365692804165,1.50063603778561,330.314266762358));
#50193=CARTESIAN_POINT('Ctrl Pts',(158.357945660859,1.36886561314595,330.276083193403));
#50194=CARTESIAN_POINT('Ctrl Pts',(158.350196775831,1.23706556371764,330.237891039972));
#50195=CARTESIAN_POINT('Ctrl Pts',(158.342447890803,1.10370128356213,330.205229241749));
#50196=CARTESIAN_POINT('Ctrl Pts',(158.334699005775,0.9692769646432,330.178207259918));
#50197=CARTESIAN_POINT('Ctrl Pts',(158.326941896,0.834709966362778,330.151156596676));
#50198=CARTESIAN_POINT('Ctrl Pts',(158.319184786225,0.699081065567712,330.129757784895));
#50199=CARTESIAN_POINT('Ctrl Pts',(158.311427676451,0.562903365726845,330.114068884711));
#50200=CARTESIAN_POINT('Ctrl Pts',(158.303666421524,0.426652896877232,330.098371600879));
#50201=CARTESIAN_POINT('Ctrl Pts',(158.295905166598,0.289853434273793,330.088390336852));
#50202=CARTESIAN_POINT('Ctrl Pts',(158.288143911672,0.153020352724308,330.084131019428));
#50203=CARTESIAN_POINT('Ctrl Pts',(158.280370241267,0.0159683828383288,
330.079864888484));
#50204=CARTESIAN_POINT('Ctrl Pts',(158.272596570863,-0.121116922403505,
330.081338990842));
#50205=CARTESIAN_POINT('Ctrl Pts',(158.264822900458,-0.257722147026157,
330.088507115201));
#50206=CARTESIAN_POINT('Ctrl Pts',(158.257411096281,-0.387968365575321,
330.095341561646));
#50207=CARTESIAN_POINT('Ctrl Pts',(158.249999292104,-0.517777906594161,
330.107351820001));
#50208=CARTESIAN_POINT('Ctrl Pts',(158.242587487927,-0.64671435804053,330.124454532916));
#50209=CARTESIAN_POINT('Ctrl Pts',(158.234812409149,-0.781970369055944,
330.142395500737));
#50210=CARTESIAN_POINT('Ctrl Pts',(158.22703733037,-0.916692975011703,330.165997434722));
#50211=CARTESIAN_POINT('Ctrl Pts',(158.219262251592,-1.05037076313152,330.195220679109));
#50212=CARTESIAN_POINT('Ctrl Pts',(158.211496740543,-1.18388405222312,330.224407962434));
#50213=CARTESIAN_POINT('Ctrl Pts',(158.203731229494,-1.31635470347679,330.259202709878));
#50214=CARTESIAN_POINT('Ctrl Pts',(158.195965718445,-1.4472769054165,330.29951357607));
#50215=CARTESIAN_POINT('Ctrl Pts',(158.188207906923,-1.57806929761172,330.339784473921));
#50216=CARTESIAN_POINT('Ctrl Pts',(158.1804500954,-1.70731592464961,330.385560492128));
#50217=CARTESIAN_POINT('Ctrl Pts',(158.172692283878,-1.83452199770111,330.436699428873));
#50218=CARTESIAN_POINT('Ctrl Pts',(158.164940310355,-1.96163234414888,330.487799881946));
#50219=CARTESIAN_POINT('Ctrl Pts',(158.157188336832,-2.08670483190564,330.544255075352));
#50220=CARTESIAN_POINT('Ctrl Pts',(158.149436363309,-2.2092609958955,330.605873361575));
#50221=CARTESIAN_POINT('Ctrl Pts',(158.141687672752,-2.33176525727679,330.667465552418));
#50222=CARTESIAN_POINT('Ctrl Pts',(158.133938982194,-2.45175496592983,330.734216311925));
#50223=CARTESIAN_POINT('Ctrl Pts',(158.126190291636,-2.56877297713006,330.805886451887));
#50224=CARTESIAN_POINT('Ctrl Pts',(158.118443213258,-2.68576664175569,330.877541680277));
#50225=CARTESIAN_POINT('Ctrl Pts',(158.110696134881,-2.79978950562923,330.954114049249));
#50226=CARTESIAN_POINT('Ctrl Pts',(158.102949056503,-2.91041066930885,331.035319332093));
#50227=CARTESIAN_POINT('Ctrl Pts',(158.095201913197,-3.02103276010031,331.116525295516));
#50228=CARTESIAN_POINT('Ctrl Pts',(158.087454769891,-3.12825277874338,331.202364018954));
#50229=CARTESIAN_POINT('Ctrl Pts',(158.079707626585,-3.23167069424558,331.292509260099));
#50230=CARTESIAN_POINT('Ctrl Pts',(158.071958741557,-3.33511186029055,331.382674767807));
#50231=CARTESIAN_POINT('Ctrl Pts',(158.064209856529,-3.43474892765857,331.477148463039));
#50232=CARTESIAN_POINT('Ctrl Pts',(158.056460971501,-3.53021700090189,331.575565595745));
#50233=CARTESIAN_POINT('Ctrl Pts',(158.048703861726,-3.62578640494471,331.674087189413));
#50234=CARTESIAN_POINT('Ctrl Pts',(158.040946751952,-3.71717770289908,331.776560300689));
#50235=CARTESIAN_POINT('Ctrl Pts',(158.033189642177,-3.80406440103096,331.88258486959));
#50236=CARTESIAN_POINT('Ctrl Pts',(158.025428387251,-3.89099752863613,331.98866609463));
#50237=CARTESIAN_POINT('Ctrl Pts',(158.017667132325,-3.97342102526369,332.098302246532));
#50238=CARTESIAN_POINT('Ctrl Pts',(158.009905877398,-4.05105100806086,332.211063142954));
#50239=CARTESIAN_POINT('Ctrl Pts',(158.002132206994,-4.12880517353106,332.324004420062));
#50240=CARTESIAN_POINT('Ctrl Pts',(157.994358536589,-4.20175029402894,332.440080099197));
#50241=CARTESIAN_POINT('Ctrl Pts',(157.986584866184,-4.26964739078003,332.558833430324));
#50242=CARTESIAN_POINT('Ctrl Pts',(157.979173062007,-4.33438386134288,332.672058765317));
#50243=CARTESIAN_POINT('Ctrl Pts',(157.97176125783,-4.39453156998078,332.787717817673));
#50244=CARTESIAN_POINT('Ctrl Pts',(157.964349453653,-4.44992444607144,332.905398489747));
#50245=CARTESIAN_POINT('Ctrl Pts',(157.955919680237,-4.51292521931634,333.039241934245));
#50246=CARTESIAN_POINT('Ctrl Pts',(157.947489906821,-4.56994996202602,333.176070695699));
#50247=CARTESIAN_POINT('Ctrl Pts',(157.939060133405,-4.62072962745642,333.315351439485));
#50248=CARTESIAN_POINT('Ctrl Pts',(157.930658840621,-4.67133772991915,333.454161612668));
#50249=CARTESIAN_POINT('Ctrl Pts',(157.922257547836,-4.71574273886886,333.595406978395));
#50250=CARTESIAN_POINT('Ctrl Pts',(157.913856255052,-4.75372361378086,333.738534635322));
#50251=CARTESIAN_POINT('Ctrl Pts',(157.905472365055,-4.79162581352958,333.88136581167));
#50252=CARTESIAN_POINT('Ctrl Pts',(157.897088475058,-4.82313033157454,334.026071233454));
#50253=CARTESIAN_POINT('Ctrl Pts',(157.88870458506,-4.8480647726888,334.172080304429));
#50254=CARTESIAN_POINT('Ctrl Pts',(157.880348513148,-4.87291648032184,334.317604911419));
#50255=CARTESIAN_POINT('Ctrl Pts',(157.871992441236,-4.89124153432854,334.464424261689));
#50256=CARTESIAN_POINT('Ctrl Pts',(157.863636369324,-4.90291802749534,334.611956345032));
#50257=CARTESIAN_POINT('Ctrl Pts',(157.85636337173,-4.91308106912587,334.740366021073));
#50258=CARTESIAN_POINT('Ctrl Pts',(157.849090374136,-4.91820806567256,334.869315271384));
#50259=CARTESIAN_POINT('Ctrl Pts',(157.841817376542,-4.91824974369148,334.99841217802));
#50260=CARTESIAN_POINT('',(156.091817376458,-4.9182479770399,335.004460811911));
#50261=CARTESIAN_POINT('Ctrl Pts',(157.841817376508,-4.91824974369168,334.998412178619));
#50262=CARTESIAN_POINT('Ctrl Pts',(157.833875574543,-4.91829525428665,335.139380473123));
#50263=CARTESIAN_POINT('Ctrl Pts',(157.825933772579,-4.91227570213308,335.280298249976));
#50264=CARTESIAN_POINT('Ctrl Pts',(157.817991970614,-4.90023038948937,335.420624764398));
#50265=CARTESIAN_POINT('Ctrl Pts',(157.810045362692,-4.88817778766127,335.561036196985));
#50266=CARTESIAN_POINT('Ctrl Pts',(157.80209875477,-4.87009218828604,335.700855292861));
#50267=CARTESIAN_POINT('Ctrl Pts',(157.794152146848,-4.84606460538666,335.839548034908));
#50268=CARTESIAN_POINT('Ctrl Pts',(157.786199405004,-4.82201847579423,335.978347832739));
#50269=CARTESIAN_POINT('Ctrl Pts',(157.778246663161,-4.79202128248692,336.116019187093));
#50270=CARTESIAN_POINT('Ctrl Pts',(157.770293921318,-4.75621479583,336.252039886916));
#50271=CARTESIAN_POINT('Ctrl Pts',(157.762327969214,-4.72034883119262,336.38828653006));
#50272=CARTESIAN_POINT('Ctrl Pts',(157.75436201711,-4.67865438582672,336.522876689614));
#50273=CARTESIAN_POINT('Ctrl Pts',(157.746396065006,-4.63132295370721,336.655303827388));
#50274=CARTESIAN_POINT('Ctrl Pts',(157.738422786762,-4.58394799173754,336.787852755972));
#50275=CARTESIAN_POINT('Ctrl Pts',(157.730449508518,-4.53092584125024,336.918234360921));
#50276=CARTESIAN_POINT('Ctrl Pts',(157.722476230274,-4.47249532858759,337.045963977753));
#50277=CARTESIAN_POINT('Ctrl Pts',(157.714488398953,-4.41395816673132,337.173926730664));
#50278=CARTESIAN_POINT('Ctrl Pts',(157.706500567633,-4.34999308182935,337.299227500727));
#50279=CARTESIAN_POINT('Ctrl Pts',(157.698512736313,-4.28088437930802,337.421407027638));
#50280=CARTESIAN_POINT('Ctrl Pts',(157.694378964002,-4.24512002356409,337.484635997445));
#50281=CARTESIAN_POINT('Ctrl Pts',(157.69024519169,-4.20797883152376,337.547029537613));
#50282=CARTESIAN_POINT('Ctrl Pts',(157.686111419379,-4.16950455071622,337.608527336268));
#50283=CARTESIAN_POINT('Ctrl Pts',(157.678336340601,-4.09713951904733,337.724196558768));
#50284=CARTESIAN_POINT('Ctrl Pts',(157.670561261822,-4.0198431950545,337.837034983697));
#50285=CARTESIAN_POINT('Ctrl Pts',(157.662786183044,-3.93786354806871,337.946593582307));
#50286=CARTESIAN_POINT('Ctrl Pts',(157.655020671995,-3.85598478225767,338.056017362086));
#50287=CARTESIAN_POINT('Ctrl Pts',(157.647255160946,-3.76943439236382,338.16216903613));
#50288=CARTESIAN_POINT('Ctrl Pts',(157.639489649897,-3.67850507197608,338.264626088535));
#50289=CARTESIAN_POINT('Ctrl Pts',(157.631731838374,-3.58766590827436,338.366981554475));
#50290=CARTESIAN_POINT('Ctrl Pts',(157.623974026852,-3.49245671213409,338.465649398344));
#50291=CARTESIAN_POINT('Ctrl Pts',(157.61621621533,-3.39321189705664,338.5602382061));
#50292=CARTESIAN_POINT('Ctrl Pts',(157.608464241807,-3.29404176684969,338.654755832778));
#50293=CARTESIAN_POINT('Ctrl Pts',(157.600712268284,-3.19084234437671,338.745200264654));
#50294=CARTESIAN_POINT('Ctrl Pts',(157.592960294761,-3.08398628283511,338.831215429832));
#50295=CARTESIAN_POINT('Ctrl Pts',(157.585211604203,-2.97717547489891,338.917194167538));
#50296=CARTESIAN_POINT('Ctrl Pts',(157.577462913646,-2.86671141177747,338.998747124787));
#50297=CARTESIAN_POINT('Ctrl Pts',(157.569714223088,-2.75300118246612,339.075557330211));
#50298=CARTESIAN_POINT('Ctrl Pts',(157.56196714471,-2.63931461151771,339.152351554631));
#50299=CARTESIAN_POINT('Ctrl Pts',(157.554220066332,-2.52238354148038,339.224404771324));
#50300=CARTESIAN_POINT('Ctrl Pts',(157.546472987955,-2.40264517940735,339.291442555175));
#50301=CARTESIAN_POINT('Ctrl Pts',(157.538725844649,-2.28290581381164,339.358480900868));
#50302=CARTESIAN_POINT('Ctrl Pts',(157.530978701343,-2.16035945031149,339.420503538931));
#50303=CARTESIAN_POINT('Ctrl Pts',(157.523231558037,-2.03546874738785,339.477281545861));
#50304=CARTESIAN_POINT('Ctrl Pts',(157.515482673009,-1.91054996638286,339.534072317693));
#50305=CARTESIAN_POINT('Ctrl Pts',(157.507733787981,-1.78328615292839,339.585615950371));
#50306=CARTESIAN_POINT('Ctrl Pts',(157.499984902953,-1.65416045643702,339.631731452369));
#50307=CARTESIAN_POINT('Ctrl Pts',(157.492227793178,-1.5248977045971,339.677895901837));
#50308=CARTESIAN_POINT('Ctrl Pts',(157.484470683404,-1.39376949071649,339.71862057987));
#50309=CARTESIAN_POINT('Ctrl Pts',(157.476713573629,-1.26127519151621,339.75377407475));
#50310=CARTESIAN_POINT('Ctrl Pts',(157.468952318703,-1.12871009159858,339.788946354534));
#50311=CARTESIAN_POINT('Ctrl Pts',(157.461191063776,-0.994777833259547,
339.818541434806));
#50312=CARTESIAN_POINT('Ctrl Pts',(157.45342980885,-0.859987555252061,339.842479165398));
#50313=CARTESIAN_POINT('Ctrl Pts',(157.445656138446,-0.724981656728042,
339.866455188557));
#50314=CARTESIAN_POINT('Ctrl Pts',(157.437882468041,-0.589115383350312,
339.884755725418));
#50315=CARTESIAN_POINT('Ctrl Pts',(157.430108797636,-0.45290345059257,339.897352501806));
#50316=CARTESIAN_POINT('Ctrl Pts',(157.422696993459,-0.323032216075101,
339.909362895222));
#50317=CARTESIAN_POINT('Ctrl Pts',(157.415285189282,-0.192847066256581,
339.91618858292));
#50318=CARTESIAN_POINT('Ctrl Pts',(157.407873385105,-0.0627918709568618,
339.917849148097));
#50319=CARTESIAN_POINT('Ctrl Pts',(157.400098306327,0.0736377168784359,
339.91959110252));
#50320=CARTESIAN_POINT('Ctrl Pts',(157.392323227548,0.210355431878305,339.915654321027));
#50321=CARTESIAN_POINT('Ctrl Pts',(157.38454814877,0.346849485754007,339.906004331096));
#50322=CARTESIAN_POINT('Ctrl Pts',(157.376782637721,0.483175575006731,339.896366216092));
#50323=CARTESIAN_POINT('Ctrl Pts',(157.369017126672,0.619278164588814,339.881028908566));
#50324=CARTESIAN_POINT('Ctrl Pts',(157.361251615623,0.754643558566898,339.860009893201));
#50325=CARTESIAN_POINT('Ctrl Pts',(157.353493804101,0.889874737363047,339.839011718251));
#50326=CARTESIAN_POINT('Ctrl Pts',(157.345735992578,1.02436979139278,339.812343105895));
#50327=CARTESIAN_POINT('Ctrl Pts',(157.337978181056,1.1576186019034,339.780073454982));
#50328=CARTESIAN_POINT('Ctrl Pts',(157.330226207533,1.29076713845844,339.747828088005));
#50329=CARTESIAN_POINT('Ctrl Pts',(157.32247423401,1.42267091985141,339.709990163773));
#50330=CARTESIAN_POINT('Ctrl Pts',(157.314722260487,1.55282885360297,339.666680363376));
#50331=CARTESIAN_POINT('Ctrl Pts',(157.30697356993,1.68293166539236,339.623388904705));
#50332=CARTESIAN_POINT('Ctrl Pts',(157.299224879372,1.81128972998111,339.574630302054));
#50333=CARTESIAN_POINT('Ctrl Pts',(157.291476188814,1.93741620016834,339.520575353849));
#50334=CARTESIAN_POINT('Ctrl Pts',(157.283729110436,2.06351642868999,339.466531652227));
#50335=CARTESIAN_POINT('Ctrl Pts',(157.275982032059,2.18738562729551,339.407193950783));
#50336=CARTESIAN_POINT('Ctrl Pts',(157.268234953681,2.30855642822807,339.342781399079));
#50337=CARTESIAN_POINT('Ctrl Pts',(157.260487810375,2.42972824468856,339.278368307536));
#50338=CARTESIAN_POINT('Ctrl Pts',(157.252740667069,2.54820127322909,339.208880464371));
#50339=CARTESIAN_POINT('Ctrl Pts',(157.244993523763,2.66353263614156,339.134583045327));
#50340=CARTESIAN_POINT('Ctrl Pts',(157.237244638735,2.778889927993,339.060268922647));
#50341=CARTESIAN_POINT('Ctrl Pts',(157.229495753707,2.89110382020343,338.981143284074));
#50342=CARTESIAN_POINT('Ctrl Pts',(157.221746868679,2.99976065326719,338.897514475356));
#50343=CARTESIAN_POINT('Ctrl Pts',(157.213989758904,3.10853281581625,338.813796902157));
#50344=CARTESIAN_POINT('Ctrl Pts',(157.20623264913,3.21374006706319,338.725566849672));
#50345=CARTESIAN_POINT('Ctrl Pts',(157.198475539355,3.31500165869355,338.633173140019));
#50346=CARTESIAN_POINT('Ctrl Pts',(157.190714284429,3.41631736128068,338.540730058123));
#50347=CARTESIAN_POINT('Ctrl Pts',(157.182953029503,3.51368292568357,338.444119160867));
#50348=CARTESIAN_POINT('Ctrl Pts',(157.175191774576,3.60675542772115,338.343725220036));
#50349=CARTESIAN_POINT('Ctrl Pts',(157.167418104172,3.69997681542977,338.243170681618));
#50350=CARTESIAN_POINT('Ctrl Pts',(157.159644433767,3.78889116383087,338.138821304335));
#50351=CARTESIAN_POINT('Ctrl Pts',(157.151870763362,3.87319615449022,338.031094622631));
#50352=CARTESIAN_POINT('Ctrl Pts',(157.144458959185,3.95357672755246,337.928382643877));
#50353=CARTESIAN_POINT('Ctrl Pts',(157.137047155008,4.02976724854739,337.822600945287));
#50354=CARTESIAN_POINT('Ctrl Pts',(157.129635350831,4.10154398197392,337.714133384053));
#50355=CARTESIAN_POINT('Ctrl Pts',(157.121860272053,4.17683870691696,337.600349504536));
#50356=CARTESIAN_POINT('Ctrl Pts',(157.114085193274,4.24751398381902,337.48325024289));
#50357=CARTESIAN_POINT('Ctrl Pts',(157.106310114496,4.31326386599218,337.363247317744));
#50358=CARTESIAN_POINT('Ctrl Pts',(157.098544603447,4.37893283874944,337.243392063839));
#50359=CARTESIAN_POINT('Ctrl Pts',(157.090779092398,4.43968829043148,337.12064059548));
#50360=CARTESIAN_POINT('Ctrl Pts',(157.083013581349,4.49526693393644,336.995434352505));
#50361=CARTESIAN_POINT('Ctrl Pts',(157.075255769826,4.55079047105438,336.870352251885));
#50362=CARTESIAN_POINT('Ctrl Pts',(157.067497958304,4.60114725703393,336.742820575235));
#50363=CARTESIAN_POINT('Ctrl Pts',(157.059740146782,4.64611959632103,336.613305847997));
#50364=CARTESIAN_POINT('Ctrl Pts',(157.051988173259,4.69105809249678,336.483888584699));
#50365=CARTESIAN_POINT('Ctrl Pts',(157.044236199736,4.73062007952204,336.35249160894));
#50366=CARTESIAN_POINT('Ctrl Pts',(157.036484226213,4.76463587080769,336.219601607539));
#50367=CARTESIAN_POINT('Ctrl Pts',(157.028735535655,4.7986372563856,336.086767885133));
#50368=CARTESIAN_POINT('Ctrl Pts',(157.020986845098,4.82709702113057,335.952442772559));
#50369=CARTESIAN_POINT('Ctrl Pts',(157.01323815454,4.84989533212657,335.817128098842));
#50370=CARTESIAN_POINT('Ctrl Pts',(157.005491076162,4.87268889974354,335.681841578473));
#50371=CARTESIAN_POINT('Ctrl Pts',(156.997743997785,4.88982329166342,335.545566291684));
#50372=CARTESIAN_POINT('Ctrl Pts',(156.989996919407,4.90122987591784,335.408813852395));
#50373=CARTESIAN_POINT('Ctrl Pts',(156.982249776101,4.9126365557704,335.27206026699));
#50374=CARTESIAN_POINT('Ctrl Pts',(156.974502632795,4.91831529971869,335.134829910631));
#50375=CARTESIAN_POINT('Ctrl Pts',(156.966755489489,4.91824943316335,334.997638710442));
#50376=CARTESIAN_POINT('Ctrl Pts',(156.959006604461,4.91818355179981,334.860416666758));
#50377=CARTESIAN_POINT('Ctrl Pts',(156.951257719433,4.91237049015884,334.72323418756));
#50378=CARTESIAN_POINT('Ctrl Pts',(156.943508834405,4.90084568786444,334.586605991528));
#50379=CARTESIAN_POINT('Ctrl Pts',(156.93575172463,4.8893086530258,334.449832776917));
#50380=CARTESIAN_POINT('Ctrl Pts',(156.927994614856,4.8720478000262,334.313615410806));
#50381=CARTESIAN_POINT('Ctrl Pts',(156.920237505081,4.84915041606605,334.17846284024));
#50382=CARTESIAN_POINT('Ctrl Pts',(156.912476250155,4.82624079647601,334.043238048461));
#50383=CARTESIAN_POINT('Ctrl Pts',(156.904714995229,4.79768872560381,333.909079568115));
#50384=CARTESIAN_POINT('Ctrl Pts',(156.896953740302,4.76363219029968,333.776483993549));
#50385=CARTESIAN_POINT('Ctrl Pts',(156.889180069898,4.72952117563804,333.643676309278));
#50386=CARTESIAN_POINT('Ctrl Pts',(156.881406399493,4.68988821390836,333.512436901189));
#50387=CARTESIAN_POINT('Ctrl Pts',(156.873632729088,4.64492081688073,333.38324594715));
#50388=CARTESIAN_POINT('Ctrl Pts',(156.866220924911,4.60204666300323,333.260068863102));
#50389=CARTESIAN_POINT('Ctrl Pts',(156.858809120734,4.55432363862722,333.138754081685));
#50390=CARTESIAN_POINT('Ctrl Pts',(156.851397316557,4.50195346133741,333.019697474008));
#50391=CARTESIAN_POINT('Ctrl Pts',(156.843622237779,4.44701646565601,332.894805547336));
#50392=CARTESIAN_POINT('Ctrl Pts',(156.835847159,4.38679164601235,332.772004069567));
#50393=CARTESIAN_POINT('Ctrl Pts',(156.828072080222,4.32145966007909,332.651773122373));
#50394=CARTESIAN_POINT('Ctrl Pts',(156.820306569173,4.25620806931384,332.531690127014));
#50395=CARTESIAN_POINT('Ctrl Pts',(156.812541058124,4.18586200183611,332.414171708528));
#50396=CARTESIAN_POINT('Ctrl Pts',(156.804775547075,4.11065019406275,332.29967815908));
#50397=CARTESIAN_POINT('Ctrl Pts',(156.797017735553,4.03551295901557,332.185298130319));
#50398=CARTESIAN_POINT('Ctrl Pts',(156.78925992403,3.95551979771654,332.073937326672));
#50399=CARTESIAN_POINT('Ctrl Pts',(156.781502112508,3.87094521380705,331.96603127666));
#50400=CARTESIAN_POINT('Ctrl Pts',(156.773750138985,3.78643427495443,331.858206429374));
#50401=CARTESIAN_POINT('Ctrl Pts',(156.765998165462,3.69734901605317,331.753831467327));
#50402=CARTESIAN_POINT('Ctrl Pts',(156.758246191939,3.60400687528268,331.653312457755));
#50403=CARTESIAN_POINT('Ctrl Pts',(156.750497501382,3.51070426496394,331.552836018044));
#50404=CARTESIAN_POINT('Ctrl Pts',(156.742748810824,3.4131486238242,331.456212568721));
#50405=CARTESIAN_POINT('Ctrl Pts',(156.735000120266,3.31169710213056,331.363814448321));
#50406=CARTESIAN_POINT('Ctrl Pts',(156.727253041889,3.21026668827332,331.271435552122));
#50407=CARTESIAN_POINT('Ctrl Pts',(156.719505963511,3.10494229494595,331.183280499254));
#50408=CARTESIAN_POINT('Ctrl Pts',(156.711758885133,2.99611700851296,331.099683867454));
#50409=CARTESIAN_POINT('Ctrl Pts',(156.704011741827,2.88729081001919,331.016086535033));
#50410=CARTESIAN_POINT('Ctrl Pts',(156.696264598521,2.77496396987199,330.937047937994));
#50411=CARTESIAN_POINT('Ctrl Pts',(156.688517455215,2.65956131861443,330.862861296134));
#50412=CARTESIAN_POINT('Ctrl Pts',(156.680768570187,2.54413272239081,330.788657975541));
#50413=CARTESIAN_POINT('Ctrl Pts',(156.673019685159,2.42562726776568,330.719308992068));
#50414=CARTESIAN_POINT('Ctrl Pts',(156.665270800131,2.30449697107282,330.655063087591));
#50415=CARTESIAN_POINT('Ctrl Pts',(156.657513690356,2.18323810543156,330.590748991847));
#50416=CARTESIAN_POINT('Ctrl Pts',(156.649756580582,2.05934917821337,330.531548978425));
#50417=CARTESIAN_POINT('Ctrl Pts',(156.641999470807,1.93330540995811,330.477665066105));
#50418=CARTESIAN_POINT('Ctrl Pts',(156.634238215881,1.80719428794308,330.423752359945));
#50419=CARTESIAN_POINT('Ctrl Pts',(156.626476960955,1.67892639580717,330.375161553746));
#50420=CARTESIAN_POINT('Ctrl Pts',(156.618715706028,1.54899400293614,330.332045347117));
#50421=CARTESIAN_POINT('Ctrl Pts',(156.610942035624,1.41885376058149,330.28886016861));
#50422=CARTESIAN_POINT('Ctrl Pts',(156.603168365219,1.28704407271883,330.251167197428));
#50423=CARTESIAN_POINT('Ctrl Pts',(156.595394694815,1.15407020453884,330.21906860272));
#50424=CARTESIAN_POINT('Ctrl Pts',(156.587982890637,1.02728630191402,330.188464205318));
#50425=CARTESIAN_POINT('Ctrl Pts',(156.58057108646,0.899444447246702,330.162945125377));
#50426=CARTESIAN_POINT('Ctrl Pts',(156.573159282283,0.770986697957244,330.142555962847));
#50427=CARTESIAN_POINT('Ctrl Pts',(156.565384203505,0.636232851719303,330.121167466726));
#50428=CARTESIAN_POINT('Ctrl Pts',(156.557609124726,0.500375363599819,330.105356876436));
#50429=CARTESIAN_POINT('Ctrl Pts',(156.549834045948,0.363915708752337,330.095232072827));
#50430=CARTESIAN_POINT('Ctrl Pts',(156.542068534899,0.227623976197869,330.085119728434));
#50431=CARTESIAN_POINT('Ctrl Pts',(156.53430302385,0.0907319373783311,330.080679277895));
#50432=CARTESIAN_POINT('Ctrl Pts',(156.526537512801,-0.0462495558042956,
330.08196746238));
#50433=CARTESIAN_POINT('Ctrl Pts',(156.518779701279,-0.183095231437924,
330.083254369627));
#50434=CARTESIAN_POINT('Ctrl Pts',(156.511021889757,-0.320029796588839,
330.090258604807));
#50435=CARTESIAN_POINT('Ctrl Pts',(156.503264078234,-0.456538456360242,
330.102985021427));
#50436=CARTESIAN_POINT('Ctrl Pts',(156.495512104711,-0.592944389036995,
330.115701861015));
#50437=CARTESIAN_POINT('Ctrl Pts',(156.487760131188,-0.728924666668749,
330.134132274779));
#50438=CARTESIAN_POINT('Ctrl Pts',(156.480008157665,-0.863966034639482,
330.158229068462));
#50439=CARTESIAN_POINT('Ctrl Pts',(156.472259467108,-0.998950212509602,
330.182315657138));
#50440=CARTESIAN_POINT('Ctrl Pts',(156.46451077655,-1.13299588757902,330.21206378435));
#50441=CARTESIAN_POINT('Ctrl Pts',(156.456762085992,-1.26559667792607,330.247374608564));
#50442=CARTESIAN_POINT('Ctrl Pts',(156.449015007615,-1.39816987957107,330.282678086066));
#50443=CARTESIAN_POINT('Ctrl Pts',(156.441267929237,-1.52929841697455,330.32354185797));
#50444=CARTESIAN_POINT('Ctrl Pts',(156.433520850859,-1.65848821499391,330.369816428777));
#50445=CARTESIAN_POINT('Ctrl Pts',(156.425773707553,-1.78767909574841,330.416091387408));
#50446=CARTESIAN_POINT('Ctrl Pts',(156.418026564247,-1.91493083672951,330.467777103585));
#50447=CARTESIAN_POINT('Ctrl Pts',(156.410279420942,-2.03976696297059,330.524675006296));
#50448=CARTESIAN_POINT('Ctrl Pts',(156.402530535914,-2.16463115502318,330.581585700863));
#50449=CARTESIAN_POINT('Ctrl Pts',(156.394781650885,-2.28707829606063,330.643710751659));
#50450=CARTESIAN_POINT('Ctrl Pts',(156.387032765857,-2.40665460175712,330.710804657008));
#50451=CARTESIAN_POINT('Ctrl Pts',(156.379275656083,-2.52635782698008,330.777969776522));
#50452=CARTESIAN_POINT('Ctrl Pts',(156.371518546308,-2.64318378850639,330.850114094315));
#50453=CARTESIAN_POINT('Ctrl Pts',(156.363761436533,-2.75670543533197,330.926947311253));
#50454=CARTESIAN_POINT('Ctrl Pts',(156.356000181607,-2.87028774449553,331.003821585404));
#50455=CARTESIAN_POINT('Ctrl Pts',(156.348238926681,-2.98056190651265,331.085389519002));
#50456=CARTESIAN_POINT('Ctrl Pts',(156.340477671755,-3.08713311781144,331.17131978674));
#50457=CARTESIAN_POINT('Ctrl Pts',(156.33270400135,-3.19387480831718,331.257387514901));
#50458=CARTESIAN_POINT('Ctrl Pts',(156.324930330945,-3.29690141726917,331.347831263932));
#50459=CARTESIAN_POINT('Ctrl Pts',(156.317156660541,-3.39585360046394,331.442281435145));
#50460=CARTESIAN_POINT('Ctrl Pts',(156.309744856364,-3.49019953572415,331.532334928163));
#50461=CARTESIAN_POINT('Ctrl Pts',(156.302333052187,-3.58084163759681,331.626030032698));
#50462=CARTESIAN_POINT('Ctrl Pts',(156.29492124801,-3.66750317839583,331.723019148827));
#50463=CARTESIAN_POINT('Ctrl Pts',(156.287219650529,-3.75755308909672,331.823800431571));
#50464=CARTESIAN_POINT('Ctrl Pts',(156.279518053048,-3.84360256713885,331.928471978928));
#50465=CARTESIAN_POINT('Ctrl Pts',(156.271816455568,-3.9252917545574,332.036679615009));
#50466=CARTESIAN_POINT('Ctrl Pts',(156.264127036115,-4.00685177226002,332.144716149503));
#50467=CARTESIAN_POINT('Ctrl Pts',(156.256437616662,-4.08406498868042,332.256277324793));
#50468=CARTESIAN_POINT('Ctrl Pts',(156.248748197208,-4.15660945517515,332.370973393127));
#50469=CARTESIAN_POINT('Ctrl Pts',(156.241065785242,-4.22908781077588,332.48556493716));
#50470=CARTESIAN_POINT('Ctrl Pts',(156.233383373276,-4.29690566474379,332.603285358931));
#50471=CARTESIAN_POINT('Ctrl Pts',(156.225700961309,-4.35978221692826,332.723713092895));
#50472=CARTESIAN_POINT('Ctrl Pts',(156.218023808879,-4.42261572254353,332.844058379579));
#50473=CARTESIAN_POINT('Ctrl Pts',(156.210346656448,-4.48051447069794,332.967106939896));
#50474=CARTESIAN_POINT('Ctrl Pts',(156.202669504018,-4.53324204575847,333.092409997649));
#50475=CARTESIAN_POINT('Ctrl Pts',(156.194995867573,-4.58594547262022,333.217655669052));
#50476=CARTESIAN_POINT('Ctrl Pts',(156.187322231128,-4.6334822839511,333.345153416556));
#50477=CARTESIAN_POINT('Ctrl Pts',(156.179648594683,-4.67566315401046,333.474432193336));
#50478=CARTESIAN_POINT('Ctrl Pts',(156.171974930537,-4.71784417634117,333.603711436808));
#50479=CARTESIAN_POINT('Ctrl Pts',(156.164301266391,-4.75466908259651,333.734771347252));
#50480=CARTESIAN_POINT('Ctrl Pts',(156.156627602244,-4.78599768438752,333.867123472069));
#50481=CARTESIAN_POINT('Ctrl Pts',(156.148954192266,-4.81732524851066,333.999471213111));
#50482=CARTESIAN_POINT('Ctrl Pts',(156.141280782287,-4.84315678410189,334.133110693588));
#50483=CARTESIAN_POINT('Ctrl Pts',(156.133607372308,-4.86340293630255,334.267541849889));
#50484=CARTESIAN_POINT('Ctrl Pts',(156.125929104274,-4.88366190639211,334.402058114887));
#50485=CARTESIAN_POINT('Ctrl Pts',(156.118250836241,-4.89832837372554,334.537366661299));
#50486=CARTESIAN_POINT('Ctrl Pts',(156.110572568207,-4.90736470654562,334.672960706565));
#50487=CARTESIAN_POINT('Ctrl Pts',(156.104320837641,-4.91472218844808,334.783362874567));
#50488=CARTESIAN_POINT('Ctrl Pts',(156.098069107074,-4.91834820572126,334.893954111272));
#50489=CARTESIAN_POINT('Ctrl Pts',(156.091817376508,-4.9182479770407,335.004460811032));
#50490=CARTESIAN_POINT('',(154.341817376458,-4.91824996390269,334.999404121525));
#50491=CARTESIAN_POINT('Ctrl Pts',(156.091817376458,-4.9182479770399,335.004460811911));
#50492=CARTESIAN_POINT('Ctrl Pts',(156.082140388515,-4.91809283408962,335.175512969368));
#50493=CARTESIAN_POINT('Ctrl Pts',(156.072463400572,-4.90901055079777,335.346167571306));
#50494=CARTESIAN_POINT('Ctrl Pts',(156.062786412629,-4.8911469239986,335.515620820331));
#50495=CARTESIAN_POINT('Ctrl Pts',(156.052937447765,-4.87296582945554,335.688085548563));
#50496=CARTESIAN_POINT('Ctrl Pts',(156.043088482901,-4.84568852631992,335.859305977571));
#50497=CARTESIAN_POINT('Ctrl Pts',(156.033239518037,-4.80951721499421,336.028458662842));
#50498=CARTESIAN_POINT('Ctrl Pts',(156.027720749936,-4.78924898560597,336.123241663542));
#50499=CARTESIAN_POINT('Ctrl Pts',(156.022201981836,-4.76618906848099,336.217375848896));
#50500=CARTESIAN_POINT('Ctrl Pts',(156.016683213735,-4.74037952019043,336.310719293769));
#50501=CARTESIAN_POINT('Ctrl Pts',(156.008908134957,-4.70401791420537,336.442225569104));
#50502=CARTESIAN_POINT('Ctrl Pts',(156.001133056179,-4.66212238829901,336.572425403022));
#50503=CARTESIAN_POINT('Ctrl Pts',(155.9933579774,-4.61480251546809,336.700817687387));
#50504=CARTESIAN_POINT('Ctrl Pts',(155.985592466351,-4.56754087275327,336.829051976872));
#50505=CARTESIAN_POINT('Ctrl Pts',(155.977826955302,-4.51486829833741,336.95548277928));
#50506=CARTESIAN_POINT('Ctrl Pts',(155.970061444253,-4.45694479432792,337.079621639341));
#50507=CARTESIAN_POINT('Ctrl Pts',(155.962303632731,-4.39907872164128,337.20363741536));
#50508=CARTESIAN_POINT('Ctrl Pts',(155.954545821209,-4.33597224442796,337.325365419439));
#50509=CARTESIAN_POINT('Ctrl Pts',(155.946788009687,-4.26783422348802,337.444335104548));
#50510=CARTESIAN_POINT('Ctrl Pts',(155.939036036164,-4.1997474785696,337.563215261196));
#50511=CARTESIAN_POINT('Ctrl Pts',(155.931284062641,-4.12663692004067,337.67934089268));
#50512=CARTESIAN_POINT('Ctrl Pts',(155.923532089118,-4.04875814139768,337.792264417093));
#50513=CARTESIAN_POINT('Ctrl Pts',(155.91578339856,-3.97091234446371,337.905140118327));
#50514=CARTESIAN_POINT('Ctrl Pts',(155.908034708002,-3.88830256520004,338.014816088564));
#50515=CARTESIAN_POINT('Ctrl Pts',(155.900286017445,-3.80122855609768,338.120872398354));
#50516=CARTESIAN_POINT('Ctrl Pts',(155.892538939067,-3.71417266347014,338.226906642243));
#50517=CARTESIAN_POINT('Ctrl Pts',(155.884791860689,-3.62265463636649,338.329322421744));
#50518=CARTESIAN_POINT('Ctrl Pts',(155.877044782311,-3.52701523089275,338.427731994125));
#50519=CARTESIAN_POINT('Ctrl Pts',(155.869297639006,-3.4313750238688,338.526142391273));
#50520=CARTESIAN_POINT('Ctrl Pts',(155.8615504957,-3.33161364199637,338.620546234025));
#50521=CARTESIAN_POINT('Ctrl Pts',(155.853803352394,-3.22810921533688,338.710592130153));
#50522=CARTESIAN_POINT('Ctrl Pts',(155.846054467366,-3.12458151868475,338.800658270511));
#50523=CARTESIAN_POINT('Ctrl Pts',(155.838305582338,-3.01730939756178,338.886364258134));
#50524=CARTESIAN_POINT('Ctrl Pts',(155.83055669731,-2.90670429490668,338.967398795744));
#50525=CARTESIAN_POINT('Ctrl Pts',(155.822799587535,-2.79598179485283,339.048519344249));
#50526=CARTESIAN_POINT('Ctrl Pts',(155.81504247776,-2.68191956226115,339.124958306648));
#50527=CARTESIAN_POINT('Ctrl Pts',(155.807285367986,-2.56495873655645,339.19644727624));
#50528=CARTESIAN_POINT('Ctrl Pts',(155.799524113059,-2.44793541072621,339.267974447252));
#50529=CARTESIAN_POINT('Ctrl Pts',(155.791762858133,-2.3280107470058,339.334546165208));
#50530=CARTESIAN_POINT('Ctrl Pts',(155.784001603207,-2.20564986441646,339.395940370171));
#50531=CARTESIAN_POINT('Ctrl Pts',(155.776227932802,-2.08309324429231,339.457432785854));
#50532=CARTESIAN_POINT('Ctrl Pts',(155.768454262398,-1.95809297420979,339.51373097739));
#50533=CARTESIAN_POINT('Ctrl Pts',(155.760680591993,-1.83113431666315,339.56466101445));
#50534=CARTESIAN_POINT('Ctrl Pts',(155.753268787816,-1.71008561516884,339.613220246032));
#50535=CARTESIAN_POINT('Ctrl Pts',(155.745856983639,-1.5872570201141,339.656899754762));
#50536=CARTESIAN_POINT('Ctrl Pts',(155.738445179462,-1.46307954419439,339.695591689006));
#50537=CARTESIAN_POINT('Ctrl Pts',(155.730670100683,-1.33281576027507,339.736180030204));
#50538=CARTESIAN_POINT('Ctrl Pts',(155.722895021905,-1.20065586920854,339.771407789666));
#50539=CARTESIAN_POINT('Ctrl Pts',(155.715119943126,-1.06708055975425,339.801095931295));
#50540=CARTESIAN_POINT('Ctrl Pts',(155.707354432077,-0.933669623222156,
339.830747539775));
#50541=CARTESIAN_POINT('Ctrl Pts',(155.699588921028,-0.79884711182609,339.85487301001));
#50542=CARTESIAN_POINT('Ctrl Pts',(155.691823409979,-0.663110364345369,
339.873342560009));
#50543=CARTESIAN_POINT('Ctrl Pts',(155.684065598457,-0.527508200244869,
339.891793797396));
#50544=CARTESIAN_POINT('Ctrl Pts',(155.676307786935,-0.39099398879215,339.904600222149));
#50545=CARTESIAN_POINT('Ctrl Pts',(155.668549975413,-0.254076449587683,
339.911682829771));
#50546=CARTESIAN_POINT('Ctrl Pts',(155.66079800189,-0.117261945173489,339.918760107506));
#50547=CARTESIAN_POINT('Ctrl Pts',(155.653046028367,0.0199548940762356,
339.920122121577));
#50548=CARTESIAN_POINT('Ctrl Pts',(155.645294054844,0.157059370680539,339.915741593756));
#50549=CARTESIAN_POINT('Ctrl Pts',(155.637545364286,0.294105783457671,339.911362921091));
#50550=CARTESIAN_POINT('Ctrl Pts',(155.629796673728,0.431039538372006,339.901246556007));
#50551=CARTESIAN_POINT('Ctrl Pts',(155.622047983171,0.56734529451731,339.885417318847));
#50552=CARTESIAN_POINT('Ctrl Pts',(155.614300904793,0.703622691111577,339.869591375092));
#50553=CARTESIAN_POINT('Ctrl Pts',(155.606553826415,0.839271960808397,339.848054968554));
#50554=CARTESIAN_POINT('Ctrl Pts',(155.598806748037,0.973782639789811,339.820884818469));
#50555=CARTESIAN_POINT('Ctrl Pts',(155.591059604731,1.10829444610027,339.793714440672));
#50556=CARTESIAN_POINT('Ctrl Pts',(155.583312461425,1.24166725952586,339.760910302544));
#50557=CARTESIAN_POINT('Ctrl Pts',(155.57556531812,1.37340095897385,339.722600223223));
#50558=CARTESIAN_POINT('Ctrl Pts',(155.567816433092,1.50516427495418,339.684281530984));
#50559=CARTESIAN_POINT('Ctrl Pts',(155.560067548063,1.63528736841611,339.640454543492));
#50560=CARTESIAN_POINT('Ctrl Pts',(155.552318663035,1.7632858074543,339.591296791074));
#50561=CARTESIAN_POINT('Ctrl Pts',(155.544561553261,1.89142010535819,339.54208686211));
#50562=CARTESIAN_POINT('Ctrl Pts',(155.536804443486,2.01742487853805,339.487535005933));
#50563=CARTESIAN_POINT('Ctrl Pts',(155.529047333711,2.14083569221801,339.427866935831));
#50564=CARTESIAN_POINT('Ctrl Pts',(155.521286078785,2.26431245269086,339.36816698102));
#50565=CARTESIAN_POINT('Ctrl Pts',(155.513524823859,2.38519214738026,339.303345549287));
#50566=CARTESIAN_POINT('Ctrl Pts',(155.505763568933,2.50303633875702,339.233673599767));
#50567=CARTESIAN_POINT('Ctrl Pts',(155.497989898528,2.62106904243464,339.163890197833));
#50568=CARTESIAN_POINT('Ctrl Pts',(155.490216228123,2.7360562114223,339.089240985787));
#50569=CARTESIAN_POINT('Ctrl Pts',(155.482442557719,2.84758898061532,339.010039907529));
#50570=CARTESIAN_POINT('Ctrl Pts',(155.475030753541,2.9539298725685,338.93452565852));
#50571=CARTESIAN_POINT('Ctrl Pts',(155.467618949364,3.05713050400697,338.85487396101));
#50572=CARTESIAN_POINT('Ctrl Pts',(155.460207145187,3.15686693448992,338.771388898062));
#50573=CARTESIAN_POINT('Ctrl Pts',(155.452432066409,3.2614917445309,338.683811983489));
#50574=CARTESIAN_POINT('Ctrl Pts',(155.44465698763,3.36263481940249,338.591739673597));
#50575=CARTESIAN_POINT('Ctrl Pts',(155.436881908852,3.45988547556214,338.495479303113));
#50576=CARTESIAN_POINT('Ctrl Pts',(155.429116397803,3.55701645859813,338.399337387144));
#50577=CARTESIAN_POINT('Ctrl Pts',(155.421350886754,3.65026427824316,338.299017937262));
#50578=CARTESIAN_POINT('Ctrl Pts',(155.413585375705,3.73925065950308,338.194868943776));
#50579=CARTESIAN_POINT('Ctrl Pts',(155.405827564183,3.82814881050685,338.090823214321));
#50580=CARTESIAN_POINT('Ctrl Pts',(155.398069752661,3.91279367929503,337.982955792774));
#50581=CARTESIAN_POINT('Ctrl Pts',(155.390311941139,3.99284353193543,337.871651718433));
#50582=CARTESIAN_POINT('Ctrl Pts',(155.382559967616,4.07283314452316,337.760431403939));
#50583=CARTESIAN_POINT('Ctrl Pts',(155.374807994093,4.14823439643133,337.645779900387));
#50584=CARTESIAN_POINT('Ctrl Pts',(155.36705602057,4.21874581647584,337.528115266056));
#50585=CARTESIAN_POINT('Ctrl Pts',(155.359307330012,4.28922737489214,337.410500462768));
#50586=CARTESIAN_POINT('Ctrl Pts',(155.351558639454,4.35482301971102,337.289875401283));
#50587=CARTESIAN_POINT('Ctrl Pts',(155.343809948897,4.41527474235423,337.166686874477));
#50588=CARTESIAN_POINT('Ctrl Pts',(155.336062870519,4.47571388751165,337.043523978072));
#50589=CARTESIAN_POINT('Ctrl Pts',(155.328315792141,4.53101106718072,336.917799027897));
#50590=CARTESIAN_POINT('Ctrl Pts',(155.320568713763,4.58095455494285,336.789982801048));
#50591=CARTESIAN_POINT('Ctrl Pts',(155.312821570458,4.63089846127948,336.662165502977));
#50592=CARTESIAN_POINT('Ctrl Pts',(155.305074427152,4.67548844395684,336.532257257341));
#50593=CARTESIAN_POINT('Ctrl Pts',(155.297327283846,4.7145613445959,336.400747796908));
#50594=CARTESIAN_POINT('Ctrl Pts',(155.289578398818,4.75364302965255,336.269208770356));
#50595=CARTESIAN_POINT('Ctrl Pts',(155.28182951379,4.78720505319706,336.136068187286));
#50596=CARTESIAN_POINT('Ctrl Pts',(155.274080628762,4.8151345503668,336.001829488668));
#50597=CARTESIAN_POINT('Ctrl Pts',(155.266323518987,4.84309369219341,335.867448307707));
#50598=CARTESIAN_POINT('Ctrl Pts',(155.258566409212,4.86540828544163,335.731967066184));
#50599=CARTESIAN_POINT('Ctrl Pts',(155.250809299438,4.88201680492332,335.595898463621));
#50600=CARTESIAN_POINT('Ctrl Pts',(155.243048044511,4.89863419946678,335.459757150348));
#50601=CARTESIAN_POINT('Ctrl Pts',(155.235286789585,4.90953941349002,335.323028240065));
#50602=CARTESIAN_POINT('Ctrl Pts',(155.227525534659,4.91472303860509,335.18622705578));
#50603=CARTESIAN_POINT('Ctrl Pts',(155.219751864255,4.91991495583101,335.049207034183));
#50604=CARTESIAN_POINT('Ctrl Pts',(155.21197819385,4.9193669959516,334.912114898628));
#50605=CARTESIAN_POINT('Ctrl Pts',(155.204204523445,4.91312190072349,334.775464365565));
#50606=CARTESIAN_POINT('Ctrl Pts',(155.196792719268,4.90716751618068,334.64517494769));
#50607=CARTESIAN_POINT('Ctrl Pts',(155.189380915091,4.89603448777209,334.515287231087));
#50608=CARTESIAN_POINT('Ctrl Pts',(155.181969110914,4.87980322267274,334.386238180975));
#50609=CARTESIAN_POINT('Ctrl Pts',(155.174194032135,4.86277641492058,334.250864052502));
#50610=CARTESIAN_POINT('Ctrl Pts',(155.166418953357,4.84008516665706,334.115985073058));
#50611=CARTESIAN_POINT('Ctrl Pts',(155.158643874579,4.81176567778183,333.982112911654));
#50612=CARTESIAN_POINT('Ctrl Pts',(155.15087836353,4.78348103784057,333.848405488468));
#50613=CARTESIAN_POINT('Ctrl Pts',(155.143112852481,4.7495820179819,333.715702796913));
#50614=CARTESIAN_POINT('Ctrl Pts',(155.135347341432,4.71015654437565,333.584511254027));
#50615=CARTESIAN_POINT('Ctrl Pts',(155.127589529909,4.67077016124126,333.453449787938));
#50616=CARTESIAN_POINT('Ctrl Pts',(155.119831718387,4.62586834063437,333.323896860725));
#50617=CARTESIAN_POINT('Ctrl Pts',(155.112073906865,4.57558993847664,333.196348210599));
#50618=CARTESIAN_POINT('Ctrl Pts',(155.104321933342,4.52534937241098,333.068895544877));
#50619=CARTESIAN_POINT('Ctrl Pts',(155.096569959819,4.46974042102218,332.943444516258));
#50620=CARTESIAN_POINT('Ctrl Pts',(155.088817986296,4.40895149507897,332.820474873616));
#50621=CARTESIAN_POINT('Ctrl Pts',(155.081069295738,4.34818831328198,332.69755730869));
#50622=CARTESIAN_POINT('Ctrl Pts',(155.073320605181,4.28224969294531,332.577119389306));
#50623=CARTESIAN_POINT('Ctrl Pts',(155.065571914623,4.21137172848278,332.459619865643));
#50624=CARTESIAN_POINT('Ctrl Pts',(155.057824836245,4.14050851077275,332.342144788737));
#50625=CARTESIAN_POINT('Ctrl Pts',(155.050077757868,4.06470819481683,332.227607226004));
#50626=CARTESIAN_POINT('Ctrl Pts',(155.04233067949,3.98425208980506,332.116439987206));
#50627=CARTESIAN_POINT('Ctrl Pts',(155.034583536184,3.90379531049366,332.00527181672));
#50628=CARTESIAN_POINT('Ctrl Pts',(155.026836392878,3.81868289346691,331.897474343153));
#50629=CARTESIAN_POINT('Ctrl Pts',(155.019089249572,3.7292383710957,331.793449792371));
#50630=CARTESIAN_POINT('Ctrl Pts',(155.011340364544,3.63977373969698,331.689401854661));
#50631=CARTESIAN_POINT('Ctrl Pts',(155.003591479516,3.545975319692,331.589128823943));
#50632=CARTESIAN_POINT('Ctrl Pts',(154.995842594488,3.44820538767936,331.492998051486));
#50633=CARTESIAN_POINT('Ctrl Pts',(154.988085484713,3.35033168165064,331.396765244834));
#50634=CARTESIAN_POINT('Ctrl Pts',(154.980328374939,3.24847832210616,331.304683753611));
#50635=CARTESIAN_POINT('Ctrl Pts',(154.972571265164,3.14304315420253,331.21708276679));
#50636=CARTESIAN_POINT('Ctrl Pts',(154.964810010238,3.03755164511636,331.129434968802));
#50637=CARTESIAN_POINT('Ctrl Pts',(154.957048755311,2.92847482452496,331.04627268282));
#50638=CARTESIAN_POINT('Ctrl Pts',(154.949287500385,2.81624094712037,330.967882691406));
#50639=CARTESIAN_POINT('Ctrl Pts',(154.941513829981,2.70382753208889,330.889367301553));
#50640=CARTESIAN_POINT('Ctrl Pts',(154.933740159576,2.58824729803582,330.815639671812));
#50641=CARTESIAN_POINT('Ctrl Pts',(154.925966489171,2.4699553700999,330.746941861176));
#50642=CARTESIAN_POINT('Ctrl Pts',(154.918554684994,2.35716995986872,330.681441950153));
#50643=CARTESIAN_POINT('Ctrl Pts',(154.911142880817,2.2419198874598,330.620514254845));
#50644=CARTESIAN_POINT('Ctrl Pts',(154.90373107664,2.12461611918627,330.564327626098));
#50645=CARTESIAN_POINT('Ctrl Pts',(154.895955997862,2.00156294379977,330.505387123305));
#50646=CARTESIAN_POINT('Ctrl Pts',(154.888180919083,1.87586079601021,330.451477922936));
#50647=CARTESIAN_POINT('Ctrl Pts',(154.880405840305,1.74795953904585,330.402846477182));
#50648=CARTESIAN_POINT('Ctrl Pts',(154.872640329256,1.62021567272075,330.354274875518));
#50649=CARTESIAN_POINT('Ctrl Pts',(154.864874818207,1.49027844353389,330.310968243642));
#50650=CARTESIAN_POINT('Ctrl Pts',(154.857109307158,1.3586212902708,330.273126693879));
#50651=CARTESIAN_POINT('Ctrl Pts',(154.849351495635,1.2270946754585,330.235322664122));
#50652=CARTESIAN_POINT('Ctrl Pts',(154.841593684113,1.09385190347758,330.202973040348));
#50653=CARTESIAN_POINT('Ctrl Pts',(154.833835872591,0.959384994073779,330.176229328042));
#50654=CARTESIAN_POINT('Ctrl Pts',(154.826083899068,0.825019275283447,330.149505741227));
#50655=CARTESIAN_POINT('Ctrl Pts',(154.818331925545,0.689431634500228,330.128379744851));
#50656=CARTESIAN_POINT('Ctrl Pts',(154.810579952022,0.55312746266412,330.112952519921));
#50657=CARTESIAN_POINT('Ctrl Pts',(154.802831261464,0.416881015725803,330.09753182843));
#50658=CARTESIAN_POINT('Ctrl Pts',(154.795082570907,0.279919028864083,330.087805152105));
#50659=CARTESIAN_POINT('Ctrl Pts',(154.787333880349,0.14275503912601,330.083822210161));
#50660=CARTESIAN_POINT('Ctrl Pts',(154.779586801971,0.00561958750164102,
330.079840096902));
#50661=CARTESIAN_POINT('Ctrl Pts',(154.771839723593,-0.131717392937347,
330.081599352359));
#50662=CARTESIAN_POINT('Ctrl Pts',(154.764092645216,-0.268739710683866,
330.089097635831));
#50663=CARTESIAN_POINT('Ctrl Pts',(154.75634550191,-0.405763176809338,330.096595982145));
#50664=CARTESIAN_POINT('Ctrl Pts',(154.748598358604,-0.542471584691953,
330.109833431053));
#50665=CARTESIAN_POINT('Ctrl Pts',(154.740851215298,-0.678351612092352,
330.128755584774));
#50666=CARTESIAN_POINT('Ctrl Pts',(154.73310233027,-0.814262188207657,330.147681992597));
#50667=CARTESIAN_POINT('Ctrl Pts',(154.725353445242,-0.949343626185989,
330.172295594494));
#50668=CARTESIAN_POINT('Ctrl Pts',(154.717604560214,-1.08309096385484,330.202490539195));
#50669=CARTESIAN_POINT('Ctrl Pts',(154.709847450439,-1.2169802623299,330.232717533121));
#50670=CARTESIAN_POINT('Ctrl Pts',(154.702090340664,-1.34953224996625,330.268537617573));
#50671=CARTESIAN_POINT('Ctrl Pts',(154.69433323089,-1.48025480789057,330.309794379111));
#50672=CARTESIAN_POINT('Ctrl Pts',(154.686571975963,-1.61104721977016,330.351073186944));
#50673=CARTESIAN_POINT('Ctrl Pts',(154.678810721037,-1.74000788669075,330.397794327635));
#50674=CARTESIAN_POINT('Ctrl Pts',(154.671049466111,-1.86666389389016,330.449752867179));
#50675=CARTESIAN_POINT('Ctrl Pts',(154.663275795706,-1.99352250942387,330.501794523452));
#50676=CARTESIAN_POINT('Ctrl Pts',(154.655502125302,-2.11806874282148,330.559090157121));
#50677=CARTESIAN_POINT('Ctrl Pts',(154.647728454897,-2.23985274718433,330.621388035755));
#50678=CARTESIAN_POINT('Ctrl Pts',(154.64031665072,-2.35596767684372,330.68078593315));
#50679=CARTESIAN_POINT('Ctrl Pts',(154.632904846543,-2.4695715028908,330.744730705829));
#50680=CARTESIAN_POINT('Ctrl Pts',(154.625493042366,-2.580299837594,330.812968138333));
#50681=CARTESIAN_POINT('Ctrl Pts',(154.617717963588,-2.69645529782462,330.884550090673));
#50682=CARTESIAN_POINT('Ctrl Pts',(154.609942884809,-2.80981333947447,330.961082346858));
#50683=CARTESIAN_POINT('Ctrl Pts',(154.602167806031,-2.9199232688313,331.042319976724));
#50684=CARTESIAN_POINT('Ctrl Pts',(154.594402294982,-3.02989770091011,331.123457638515));
#50685=CARTESIAN_POINT('Ctrl Pts',(154.586636783933,-3.13663166207078,331.209288923185));
#50686=CARTESIAN_POINT('Ctrl Pts',(154.578871272884,-3.23970066869759,331.299523998221));
#50687=CARTESIAN_POINT('Ctrl Pts',(154.571113461361,-3.34266748210444,331.389669604918));
#50688=CARTESIAN_POINT('Ctrl Pts',(154.563355649839,-3.4419762802728,331.484210056842));
#50689=CARTESIAN_POINT('Ctrl Pts',(154.555597838317,-3.53723339889134,331.582813592403));
#50690=CARTESIAN_POINT('Ctrl Pts',(154.547845864794,-3.63241883350704,331.681342925676));
#50691=CARTESIAN_POINT('Ctrl Pts',(154.540093891271,-3.72355838700805,331.783928976597));
#50692=CARTESIAN_POINT('Ctrl Pts',(154.532341917748,-3.81029347808917,331.890201505993));
#50693=CARTESIAN_POINT('Ctrl Pts',(154.52459322719,-3.89699183680783,331.996429028909));
#50694=CARTESIAN_POINT('Ctrl Pts',(154.516844536632,-3.97928919640726,332.106339622941));
#50695=CARTESIAN_POINT('Ctrl Pts',(154.509095846075,-4.05686584257545,332.21952834975));
#50696=CARTESIAN_POINT('Ctrl Pts',(154.501348767697,-4.13442634827447,332.332693526699));
#50697=CARTESIAN_POINT('Ctrl Pts',(154.493601689319,-4.20726787333821,332.44913515758));
#50698=CARTESIAN_POINT('Ctrl Pts',(154.485854610941,-4.27511304526961,332.568417899255));
#50699=CARTESIAN_POINT('Ctrl Pts',(154.478107467635,-4.34295878580881,332.687701640633));
#50700=CARTESIAN_POINT('Ctrl Pts',(154.47036032433,-4.40580789644616,332.809826200536));
#50701=CARTESIAN_POINT('Ctrl Pts',(154.462613181024,-4.46342833331626,332.934330477581));
#50702=CARTESIAN_POINT('Ctrl Pts',(154.454864295996,-4.52106172448401,333.058862745832));
#50703=CARTESIAN_POINT('Ctrl Pts',(154.447115410968,-4.57346393860177,333.185775441179));
#50704=CARTESIAN_POINT('Ctrl Pts',(154.439366525939,-4.6204507242556,333.314586647963));
#50705=CARTESIAN_POINT('Ctrl Pts',(154.431609416165,-4.66748738216915,333.443534576292));
#50706=CARTESIAN_POINT('Ctrl Pts',(154.42385230639,-4.70909699530752,333.57438467362));
#50707=CARTESIAN_POINT('Ctrl Pts',(154.416095196615,-4.74514478130707,333.706638462403));
#50708=CARTESIAN_POINT('Ctrl Pts',(154.408333941689,-4.78121183009083,333.838962923382));
#50709=CARTESIAN_POINT('Ctrl Pts',(154.400572686763,-4.81171104276371,333.972692189538));
#50710=CARTESIAN_POINT('Ctrl Pts',(154.392811431837,-4.83655883139046,334.107317675206));
#50711=CARTESIAN_POINT('Ctrl Pts',(154.385037761432,-4.86144636838115,334.242158517778));
#50712=CARTESIAN_POINT('Ctrl Pts',(154.377264091027,-4.88066436103362,334.37789805752));
#50713=CARTESIAN_POINT('Ctrl Pts',(154.369490420623,-4.89418105854848,334.514021781717));
#50714=CARTESIAN_POINT('Ctrl Pts',(154.362078616445,-4.90706855054207,334.643808913803));
#50715=CARTESIAN_POINT('Ctrl Pts',(154.354666812268,-4.91477357585445,334.773944980405));
#50716=CARTESIAN_POINT('Ctrl Pts',(154.347255008091,-4.91731271857854,334.903985989534));
#50717=CARTESIAN_POINT('Ctrl Pts',(154.34544246423,-4.91793366152942,334.935787292855));
#50718=CARTESIAN_POINT('Ctrl Pts',(154.343629920369,-4.91824610996808,334.96759463941));
#50719=CARTESIAN_POINT('Ctrl Pts',(154.341817376508,-4.91824996390259,334.999404120642));
#50720=CARTESIAN_POINT('',(152.591817376552,-4.91824825560227,334.995857686006));
#50721=CARTESIAN_POINT('Ctrl Pts',(154.341817376458,-4.91824996390269,334.999404121525));
#50722=CARTESIAN_POINT('Ctrl Pts',(154.334068388395,-4.91826644022024,335.135396025298));
#50723=CARTESIAN_POINT('Ctrl Pts',(154.326319400332,-4.91263828350686,335.271609830519));
#50724=CARTESIAN_POINT('Ctrl Pts',(154.31857041227,-4.90133626904523,335.407536305428));
#50725=CARTESIAN_POINT('Ctrl Pts',(154.310830935574,-4.89004812705442,335.543295939632));
#50726=CARTESIAN_POINT('Ctrl Pts',(154.303091458879,-4.8731000147636,335.678768556545));
#50727=CARTESIAN_POINT('Ctrl Pts',(154.295351982184,-4.8505146831706,335.813443526526));
#50728=CARTESIAN_POINT('Ctrl Pts',(154.28762012185,-4.82795157763601,335.947985963861));
#50729=CARTESIAN_POINT('Ctrl Pts',(154.279888261517,-4.79976235608507,336.081731930328));
#50730=CARTESIAN_POINT('Ctrl Pts',(154.272156401184,-4.7660216451968,336.214174921507));
#50731=CARTESIAN_POINT('Ctrl Pts',(154.264430269083,-4.73230593148192,336.346519790851));
#50732=CARTESIAN_POINT('Ctrl Pts',(154.256704136983,-4.69304701083312,336.477563226027));
#50733=CARTESIAN_POINT('Ctrl Pts',(154.248978004882,-4.64837068851767,336.606808328529));
#50734=CARTESIAN_POINT('Ctrl Pts',(154.241254987576,-4.60371237748629,336.736001325796));
#50735=CARTESIAN_POINT('Ctrl Pts',(154.23353197027,-4.55364113610734,336.863397060586));
#50736=CARTESIAN_POINT('Ctrl Pts',(154.225808952965,-4.49833271458228,336.988513477807));
#50737=CARTESIAN_POINT('Ctrl Pts',(154.218087399298,-4.44303477491628,337.1136061834));
#50738=CARTESIAN_POINT('Ctrl Pts',(154.210365845631,-4.38250178822137,337.236420070549));
#50739=CARTESIAN_POINT('Ctrl Pts',(154.202644291965,-4.31695760137542,337.356493184889));
#50740=CARTESIAN_POINT('Ctrl Pts',(154.194922500902,-4.25141139940418,337.47656999082));
#50741=CARTESIAN_POINT('Ctrl Pts',(154.18720070984,-4.18085387937136,337.593905510588));
#50742=CARTESIAN_POINT('Ctrl Pts',(154.179478918778,-4.10555457456754,337.708062905057));
#50743=CARTESIAN_POINT('Ctrl Pts',(154.171755189466,-4.03023636885367,337.822248954222));
#50744=CARTESIAN_POINT('Ctrl Pts',(154.164031460153,-3.95017422715415,337.93325496234));
#50745=CARTESIAN_POINT('Ctrl Pts',(154.156307730841,-3.86568042395746,338.040673925684));
#50746=CARTESIAN_POINT('Ctrl Pts',(154.148575753182,-3.78109638790026,338.14820760419));
#50747=CARTESIAN_POINT('Ctrl Pts',(154.140843775523,-3.6920714823124,338.252146277603));
#50748=CARTESIAN_POINT('Ctrl Pts',(154.133111797864,-3.59895791905978,338.352116489524));
#50749=CARTESIAN_POINT('Ctrl Pts',(154.125375452798,-3.50579176061177,338.452143169618));
#50750=CARTESIAN_POINT('Ctrl Pts',(154.117639107731,-3.40853262378881,338.548196646541));
#50751=CARTESIAN_POINT('Ctrl Pts',(154.109902762665,-3.30756804918587,338.639941848781));
#50752=CARTESIAN_POINT('Ctrl Pts',(154.102154488962,-3.20644779774817,338.731828512545));
#50753=CARTESIAN_POINT('Ctrl Pts',(154.094406215258,-3.10161099749992,338.819393379673));
#50754=CARTESIAN_POINT('Ctrl Pts',(154.086657941555,-2.99347712926079,338.902342596325));
#50755=CARTESIAN_POINT('Ctrl Pts',(154.080777618976,-2.91141213629057,338.965294444735));
#50756=CARTESIAN_POINT('Ctrl Pts',(154.074897296397,-2.82744881904549,339.02558872054));
#50757=CARTESIAN_POINT('Ctrl Pts',(154.069016973818,-2.74178029713784,339.083114480972));
#50758=CARTESIAN_POINT('Ctrl Pts',(154.06124189504,-2.6285076836539,339.159176178802));
#50759=CARTESIAN_POINT('Ctrl Pts',(154.053466816261,-2.51188855603708,339.230640931774));
#50760=CARTESIAN_POINT('Ctrl Pts',(154.045691737483,-2.39233255663554,339.297200018729));
#50761=CARTESIAN_POINT('Ctrl Pts',(154.037926226434,-2.27292367850251,339.36367720049));
#50762=CARTESIAN_POINT('Ctrl Pts',(154.030160715385,-2.15058545767587,339.425260539293));
#50763=CARTESIAN_POINT('Ctrl Pts',(154.022395204336,-2.02575754522527,339.481683771805));
#50764=CARTESIAN_POINT('Ctrl Pts',(154.014637392813,-1.90105340001345,339.538051060518));
#50765=CARTESIAN_POINT('Ctrl Pts',(154.006879581291,-1.77386482958897,339.589268264628));
#50766=CARTESIAN_POINT('Ctrl Pts',(153.999121769769,-1.6446568780592,339.635114541837));
#50767=CARTESIAN_POINT('Ctrl Pts',(153.991369796246,-1.5155461596102,339.68092631827));
#50768=CARTESIAN_POINT('Ctrl Pts',(153.983617822723,-1.38441945173065,339.721375082611));
#50769=CARTESIAN_POINT('Ctrl Pts',(153.9758658492,-1.25176228377991,339.756287864228));
#50770=CARTESIAN_POINT('Ctrl Pts',(153.968117158642,-1.11916129621872,339.791185860262));
#50771=CARTESIAN_POINT('Ctrl Pts',(153.960368468085,-0.985031514928295,
339.820552437326));
#50772=CARTESIAN_POINT('Ctrl Pts',(153.952619777527,-0.849873947926188,
339.844264375025));
#50773=CARTESIAN_POINT('Ctrl Pts',(153.944872699149,-0.714744501584777,
339.867971379258));
#50774=CARTESIAN_POINT('Ctrl Pts',(153.937125620771,-0.578588079625996,
339.886026016757));
#50775=CARTESIAN_POINT('Ctrl Pts',(153.929378542394,-0.441915820637612,
339.898356200806));
#50776=CARTESIAN_POINT('Ctrl Pts',(153.921631399088,-0.305242416204129,
339.910686488192));
#50777=CARTESIAN_POINT('Ctrl Pts',(153.913884255782,-0.168053555411324,
339.917292191314));
#50778=CARTESIAN_POINT('Ctrl Pts',(153.906137112476,-0.0308650409611062,
339.918153150497));
#50779=CARTESIAN_POINT('Ctrl Pts',(153.898388227448,0.106354316379358,339.919014303242));
#50780=CARTESIAN_POINT('Ctrl Pts',(153.89063934242,0.243572936432081,339.914128139574));
#50781=CARTESIAN_POINT('Ctrl Pts',(153.882890457392,0.380275872842287,339.903526621018));
#50782=CARTESIAN_POINT('Ctrl Pts',(153.875133347617,0.517123907162001,339.892913849901));
#50783=CARTESIAN_POINT('Ctrl Pts',(153.867376237842,0.653454774132652,339.876573636088));
#50784=CARTESIAN_POINT('Ctrl Pts',(153.859619128068,0.788758948637311,339.854589826488));
#50785=CARTESIAN_POINT('Ctrl Pts',(153.851857873142,0.924135425366752,339.832594269444));
#50786=CARTESIAN_POINT('Ctrl Pts',(153.844096618215,1.05848373377354,339.804949186186));
#50787=CARTESIAN_POINT('Ctrl Pts',(153.836335363289,1.19130635864043,339.771789205567));
#50788=CARTESIAN_POINT('Ctrl Pts',(153.828561692885,1.32434145642022,339.738576179785));
#50789=CARTESIAN_POINT('Ctrl Pts',(153.82078802248,1.45584561848945,339.699830738125));
#50790=CARTESIAN_POINT('Ctrl Pts',(153.813014352075,1.58533741116339,339.655737144134));
#50791=CARTESIAN_POINT('Ctrl Pts',(153.805602547898,1.70880132973379,339.613696117551));
#50792=CARTESIAN_POINT('Ctrl Pts',(153.798190743721,1.83043574574425,339.566793749941));
#50793=CARTESIAN_POINT('Ctrl Pts',(153.790778939544,1.94984343437416,339.515229079895));
#50794=CARTESIAN_POINT('Ctrl Pts',(153.783003860766,2.07510364952152,339.461137071766));
#50795=CARTESIAN_POINT('Ctrl Pts',(153.775228781987,2.1983091864865,339.401743237873));
#50796=CARTESIAN_POINT('Ctrl Pts',(153.767453703209,2.31897875408065,339.337224988472));
#50797=CARTESIAN_POINT('Ctrl Pts',(153.75968819216,2.43949983008958,339.272786132884));
#50798=CARTESIAN_POINT('Ctrl Pts',(153.751922681111,2.55749080456709,339.203235591297));
#50799=CARTESIAN_POINT('Ctrl Pts',(153.744157170062,2.67248985057416,339.128798985308));
#50800=CARTESIAN_POINT('Ctrl Pts',(153.736399358539,2.78737487469266,339.054436183429));
#50801=CARTESIAN_POINT('Ctrl Pts',(153.728641547017,2.89927354783543,338.975197169097));
#50802=CARTESIAN_POINT('Ctrl Pts',(153.720883735495,3.00774849695214,338.891353497381));
#50803=CARTESIAN_POINT('Ctrl Pts',(153.713131761972,3.1161418152293,338.807572920688));
#50804=CARTESIAN_POINT('Ctrl Pts',(153.705379788449,3.22111622978268,338.719194821902));
#50805=CARTESIAN_POINT('Ctrl Pts',(153.697627814926,3.32226353812097,338.626533888684));
#50806=CARTESIAN_POINT('Ctrl Pts',(153.689879124368,3.42336801051429,338.533912197426));
#50807=CARTESIAN_POINT('Ctrl Pts',(153.682130433811,3.52064831269694,338.437011542709));
#50808=CARTESIAN_POINT('Ctrl Pts',(153.674381743253,3.61372970182485,338.336186551236));
#50809=CARTESIAN_POINT('Ctrl Pts',(153.666634664875,3.7067917245923,338.235382537245));
#50810=CARTESIAN_POINT('Ctrl Pts',(153.658887586498,3.79565630702035,338.130656097576));
#50811=CARTESIAN_POINT('Ctrl Pts',(153.65114050812,3.87998622343059,338.022398049313));
#50812=CARTESIAN_POINT('Ctrl Pts',(153.643393364814,3.96431684660665,337.914139093742));
#50813=CARTESIAN_POINT('Ctrl Pts',(153.635646221508,4.04411248775849,337.8023487789));
#50814=CARTESIAN_POINT('Ctrl Pts',(153.627899078202,4.11907706374747,337.687449944726));
#50815=CARTESIAN_POINT('Ctrl Pts',(153.620150193174,4.19405849336467,337.572525278855));
#50816=CARTESIAN_POINT('Ctrl Pts',(153.612401308146,4.26420648300821,337.454491030293));
#50817=CARTESIAN_POINT('Ctrl Pts',(153.604652423118,4.32926924278541,337.333797524631));
#50818=CARTESIAN_POINT('Ctrl Pts',(153.596895313343,4.3944010608481,337.212975913634));
#50819=CARTESIAN_POINT('Ctrl Pts',(153.589138203569,4.45443668123103,337.089489751812));
#50820=CARTESIAN_POINT('Ctrl Pts',(153.581381093794,4.50917087931133,336.963812884078));
#50821=CARTESIAN_POINT('Ctrl Pts',(153.573619838868,4.56393432559713,336.838068858644));
#50822=CARTESIAN_POINT('Ctrl Pts',(153.565858583941,4.61339056388664,336.710132159084));
#50823=CARTESIAN_POINT('Ctrl Pts',(153.558097329015,4.65738357242302,336.580494011955));
#50824=CARTESIAN_POINT('Ctrl Pts',(153.550323658611,4.70144695543568,336.450648486039));
#50825=CARTESIAN_POINT('Ctrl Pts',(153.542549988206,4.74002953474878,336.319096448942));
#50826=CARTESIAN_POINT('Ctrl Pts',(153.534776317801,4.77302573011917,336.186342464097));
#50827=CARTESIAN_POINT('Ctrl Pts',(153.527364513624,4.80448594465675,336.059768209186));
#50828=CARTESIAN_POINT('Ctrl Pts',(153.519952709447,4.83086810500045,335.932101671434));
#50829=CARTESIAN_POINT('Ctrl Pts',(153.51254090527,4.85212462580396,335.803784596871));
#50830=CARTESIAN_POINT('Ctrl Pts',(153.504765826492,4.87442299201189,335.669178320247));
#50831=CARTESIAN_POINT('Ctrl Pts',(153.496990747713,4.89115103556317,335.533430744201));
#50832=CARTESIAN_POINT('Ctrl Pts',(153.489215668935,4.90219749024882,335.397042603631));
#50833=CARTESIAN_POINT('Ctrl Pts',(153.481450157886,4.91323035156871,335.260822297352));
#50834=CARTESIAN_POINT('Ctrl Pts',(153.473684646837,4.91859550396333,335.123963380825));
#50835=CARTESIAN_POINT('Ctrl Pts',(153.465919135788,4.91823275638964,334.986976310968));
#50836=CARTESIAN_POINT('Ctrl Pts',(153.458161324266,4.91787036848122,334.85012506419));
#50837=CARTESIAN_POINT('Ctrl Pts',(153.450403512743,4.91179138362069,334.713146305302));
#50838=CARTESIAN_POINT('Ctrl Pts',(153.442645701221,4.89998747060739,334.576554784664));
#50839=CARTESIAN_POINT('Ctrl Pts',(153.434893727698,4.888192440413,334.440066053478));
#50840=CARTESIAN_POINT('Ctrl Pts',(153.427141754175,4.87068109082493,334.303964368362));
#50841=CARTESIAN_POINT('Ctrl Pts',(153.419389780652,4.84749714762111,334.168763291051));
#50842=CARTESIAN_POINT('Ctrl Pts',(153.411641090095,4.82432302283088,334.033619471474));
#50843=CARTESIAN_POINT('Ctrl Pts',(153.403892399537,4.79548114844775,333.899375885559));
#50844=CARTESIAN_POINT('Ctrl Pts',(153.396143708979,4.76106694277791,333.766539571414));
#50845=CARTESIAN_POINT('Ctrl Pts',(153.388396630602,4.72665989727107,333.633730894974));
#50846=CARTESIAN_POINT('Ctrl Pts',(153.380649552224,4.68668292451343,333.502329286061));
#50847=CARTESIAN_POINT('Ctrl Pts',(153.372902473846,4.64128217876355,333.372829818491));
#50848=CARTESIAN_POINT('Ctrl Pts',(153.36515533054,4.59588105251152,333.24332926559));
#50849=CARTESIAN_POINT('Ctrl Pts',(153.357408187234,4.54505619191907,333.115731254692));
#50850=CARTESIAN_POINT('Ctrl Pts',(153.349661043928,4.48900294453701,332.990513591378));
#50851=CARTESIAN_POINT('Ctrl Pts',(153.3419121589,4.43293709519505,332.865267776475));
#50852=CARTESIAN_POINT('Ctrl Pts',(153.334163273872,4.37164067971588,332.742403730741));
#50853=CARTESIAN_POINT('Ctrl Pts',(153.326414388844,4.30535612853699,332.622376886685));
#50854=CARTESIAN_POINT('Ctrl Pts',(153.318657279069,4.23900122225063,332.502222644897));
#50855=CARTESIAN_POINT('Ctrl Pts',(153.310900169295,4.16764779334477,332.384911963116));
#50856=CARTESIAN_POINT('Ctrl Pts',(153.30314305952,4.09158324929788,332.27087384378));
#50857=CARTESIAN_POINT('Ctrl Pts',(153.295381804594,4.01547805879082,332.156774786119));
#50858=CARTESIAN_POINT('Ctrl Pts',(153.287620549668,3.93465696705778,332.0459520911));
#50859=CARTESIAN_POINT('Ctrl Pts',(153.279859294741,3.84944862466571,331.938802791626));
#50860=CARTESIAN_POINT('Ctrl Pts',(153.272085624337,3.76410397669504,331.831482088191));
#50861=CARTESIAN_POINT('Ctrl Pts',(153.264311953932,3.67435830969433,331.727846818396));
#50862=CARTESIAN_POINT('Ctrl Pts',(153.256538283527,3.58057878629284,331.628258815145));
#50863=CARTESIAN_POINT('Ctrl Pts',(153.24912647935,3.49116472226735,331.533306657404));
#50864=CARTESIAN_POINT('Ctrl Pts',(153.241714675173,3.39808410779581,331.44203364685));
#50865=CARTESIAN_POINT('Ctrl Pts',(153.234302870996,3.3016826653762,331.35471885314));
#50866=CARTESIAN_POINT('Ctrl Pts',(153.226527792218,3.20055630109902,331.263124501293));
#50867=CARTESIAN_POINT('Ctrl Pts',(153.218752713439,3.0954557725751,331.175596730001));
#50868=CARTESIAN_POINT('Ctrl Pts',(153.210977634661,2.98674194593264,331.092500081778));
#50869=CARTESIAN_POINT('Ctrl Pts',(153.203212123612,2.87816189857511,331.009505689271));
#50870=CARTESIAN_POINT('Ctrl Pts',(153.195446612563,2.76597770772391,330.930931805466));
#50871=CARTESIAN_POINT('Ctrl Pts',(153.187681101514,2.6505860546638,330.857105283824));
#50872=CARTESIAN_POINT('Ctrl Pts',(153.179923289992,2.53530881276349,330.783351961392));
#50873=CARTESIAN_POINT('Ctrl Pts',(153.172165478469,2.41683076458076,330.714336843177));
#50874=CARTESIAN_POINT('Ctrl Pts',(153.164407666947,2.29558026618454,330.650345496019));
#50875=CARTESIAN_POINT('Ctrl Pts',(153.156655693424,2.1744210126331,330.586402304378));
#50876=CARTESIAN_POINT('Ctrl Pts',(153.148903719901,2.05049380595286,330.527475540505));
#50877=CARTESIAN_POINT('Ctrl Pts',(153.141151746378,1.92425417369,330.473806352183));
#50878=CARTESIAN_POINT('Ctrl Pts',(153.13340305582,1.79806800398664,330.420159892794));
#50879=CARTESIAN_POINT('Ctrl Pts',(153.125654365263,1.6695717154537,330.371766733043));
#50880=CARTESIAN_POINT('Ctrl Pts',(153.117905674705,1.53924332357645,330.328821021056));
#50881=CARTESIAN_POINT('Ctrl Pts',(153.110158596327,1.40894204760965,330.285884244283));
#50882=CARTESIAN_POINT('Ctrl Pts',(153.10241151795,1.2768097975067,330.248392783141));
#50883=CARTESIAN_POINT('Ctrl Pts',(153.094664439572,1.1433419838573,330.216491646244));
#50884=CARTESIAN_POINT('Ctrl Pts',(153.086917296266,1.00987305161915,330.184590241986));
#50885=CARTESIAN_POINT('Ctrl Pts',(153.07917015296,0.875068913674467,330.158279346289));
#50886=CARTESIAN_POINT('Ctrl Pts',(153.071423009654,0.739437080699412,330.137653255249));
#50887=CARTESIAN_POINT('Ctrl Pts',(153.063674124626,0.603774754808598,330.117022527026));
#50888=CARTESIAN_POINT('Ctrl Pts',(153.055925239598,0.467284749958108,330.10207920542));
#50889=CARTESIAN_POINT('Ctrl Pts',(153.04817635457,0.330481242081419,330.092865886168));
#50890=CARTESIAN_POINT('Ctrl Pts',(153.040419244795,0.193532529548,330.083642787804));
#50891=CARTESIAN_POINT('Ctrl Pts',(153.032662135021,0.0562700398851874,
330.080161867232));
#50892=CARTESIAN_POINT('Ctrl Pts',(153.024905025246,-0.0807899369280585,
330.082413595208));
#50893=CARTESIAN_POINT('Ctrl Pts',(153.01714377032,-0.217923154210515,330.084666526436));
#50894=CARTESIAN_POINT('Ctrl Pts',(153.009382515393,-0.354853253000151,
330.092658187437));
#50895=CARTESIAN_POINT('Ctrl Pts',(153.001621260467,-0.491068508180668,
330.106327066224));
#50896=CARTESIAN_POINT('Ctrl Pts',(152.993847590063,-0.627501663376957,
330.120017810762));
#50897=CARTESIAN_POINT('Ctrl Pts',(152.986073919658,-0.763217302728808,
330.139403865706));
#50898=CARTESIAN_POINT('Ctrl Pts',(152.978300249253,-0.897712460460137,
330.164372284715));
#50899=CARTESIAN_POINT('Ctrl Pts',(152.970888445076,-1.02594683624091,330.188178417812));
#50900=CARTESIAN_POINT('Ctrl Pts',(152.963476640899,-1.15307151949375,330.217058829054));
#50901=CARTESIAN_POINT('Ctrl Pts',(152.956064836722,-1.27866474430995,330.25087381362));
#50902=CARTESIAN_POINT('Ctrl Pts',(152.948289757944,-1.41041366719782,330.28634617131));
#50903=CARTESIAN_POINT('Ctrl Pts',(152.940514679165,-1.54089356405185,330.327361148579));
#50904=CARTESIAN_POINT('Ctrl Pts',(152.932739600387,-1.66960259792616,330.373812560272));
#50905=CARTESIAN_POINT('Ctrl Pts',(152.924974089338,-1.79815324714006,330.420206810546));
#50906=CARTESIAN_POINT('Ctrl Pts',(152.917208578289,-1.92493700512896,330.472024052882));
#50907=CARTESIAN_POINT('Ctrl Pts',(152.90944306724,-2.04946434684033,330.529107588688));
#50908=CARTESIAN_POINT('Ctrl Pts',(152.901685255718,-2.17386821932953,330.586134526001));
#50909=CARTESIAN_POINT('Ctrl Pts',(152.893927444195,-2.29601977474991,330.648417203783));
#50910=CARTESIAN_POINT('Ctrl Pts',(152.886169632673,-2.4154470658049,330.71574994488));
#50911=CARTESIAN_POINT('Ctrl Pts',(152.87841765915,-2.53478448403676,330.783032015955));
#50912=CARTESIAN_POINT('Ctrl Pts',(152.870665685627,-2.65140137940108,330.855356394774));
#50913=CARTESIAN_POINT('Ctrl Pts',(152.862913712104,-2.76484845348901,330.93247051741));
#50914=CARTESIAN_POINT('Ctrl Pts',(152.855165021547,-2.87824748267329,331.009551982169));
#50915=CARTESIAN_POINT('Ctrl Pts',(152.847416330989,-2.98847903797123,331.091418937004));
#50916=CARTESIAN_POINT('Ctrl Pts',(152.839667640431,-3.09512117447386,331.177774473187));
#50917=CARTESIAN_POINT('Ctrl Pts',(152.831920562054,-3.20174112318953,331.264112042379));
#50918=CARTESIAN_POINT('Ctrl Pts',(152.824173483676,-3.30477283498708,331.354936089525));
#50919=CARTESIAN_POINT('Ctrl Pts',(152.816426405298,-3.4038262739316,331.449908485772));
#50920=CARTESIAN_POINT('Ctrl Pts',(152.808679261992,-3.50288054303916,331.544881677979));
#50921=CARTESIAN_POINT('Ctrl Pts',(152.800932118686,-3.59795619065016,331.644003018117));
#50922=CARTESIAN_POINT('Ctrl Pts',(152.793184975381,-3.68869927801971,331.746896758657));
#50923=CARTESIAN_POINT('Ctrl Pts',(152.785436090353,-3.77946276636137,331.849813631894));
#50924=CARTESIAN_POINT('Ctrl Pts',(152.777687205324,-3.86589149772046,331.95650430009));
#50925=CARTESIAN_POINT('Ctrl Pts',(152.769938320296,-3.94767140233244,332.06655943273));
#50926=CARTESIAN_POINT('Ctrl Pts',(152.762181210522,-4.0295381089806,332.176731379025));
#50927=CARTESIAN_POINT('Ctrl Pts',(152.754424100747,-4.10674589862775,332.290274609093));
#50928=CARTESIAN_POINT('Ctrl Pts',(152.746666990972,-4.17902339048772,332.406749806853));
#50929=CARTESIAN_POINT('Ctrl Pts',(152.738905736046,-4.2513395051283,332.523287245235));
#50930=CARTESIAN_POINT('Ctrl Pts',(152.73114448112,-4.31871988040013,332.642759432912));
#50931=CARTESIAN_POINT('Ctrl Pts',(152.723383226194,-4.38093931922371,332.764702761649));
#50932=CARTESIAN_POINT('Ctrl Pts',(152.715609555789,-4.44325828887223,332.886841159971));
#50933=CARTESIAN_POINT('Ctrl Pts',(152.707835885384,-4.50039966150176,333.01145824317));
#50934=CARTESIAN_POINT('Ctrl Pts',(152.70006221498,-4.55218623245835,333.138069934848));
#50935=CARTESIAN_POINT('Ctrl Pts',(152.692650410803,-4.60156212607905,333.25878782182));
#50936=CARTESIAN_POINT('Ctrl Pts',(152.685238606625,-4.64607043265146,333.381318527738));
#50937=CARTESIAN_POINT('Ctrl Pts',(152.677826802448,-4.6856003912053,333.505231778356));
#50938=CARTESIAN_POINT('Ctrl Pts',(152.66845128616,-4.73560357011186,333.661975085615));
#50939=CARTESIAN_POINT('Ctrl Pts',(152.659075769872,-4.77777038081238,333.821331555862));
#50940=CARTESIAN_POINT('Ctrl Pts',(152.649700253583,-4.8118660837572,333.982587667419));
#50941=CARTESIAN_POINT('Ctrl Pts',(152.640053107411,-4.84694961622879,334.14851573276));
#50942=CARTESIAN_POINT('Ctrl Pts',(152.63040596124,-4.87348721353554,334.316455231313));
#50943=CARTESIAN_POINT('Ctrl Pts',(152.620758815068,-4.89127597027851,334.485604777359));
#50944=CARTESIAN_POINT('Ctrl Pts',(152.611111668896,-4.90906472702148,334.654754323405));
#50945=CARTESIAN_POINT('Ctrl Pts',(152.601464522724,-4.91810444946375,334.82511392033));
#50946=CARTESIAN_POINT('Ctrl Pts',(152.591817376552,-4.91824825560227,334.995857686006));
#50947=CARTESIAN_POINT('',(150.841817376458,-4.91824934725888,335.002533907583));
#50948=CARTESIAN_POINT('Ctrl Pts',(152.591817376508,-4.91824825560293,334.995857686791));
#50949=CARTESIAN_POINT('Ctrl Pts',(152.583807851161,-4.91836765036206,335.137617383878));
#50950=CARTESIAN_POINT('Ctrl Pts',(152.575798325814,-4.91235312101776,335.279476192963));
#50951=CARTESIAN_POINT('Ctrl Pts',(152.567788800466,-4.90021012118859,335.420860821057));
#50952=CARTESIAN_POINT('Ctrl Pts',(152.560077369643,-4.88851905347684,335.556983466507));
#50953=CARTESIAN_POINT('Ctrl Pts',(152.552365938819,-4.87114755500484,335.692666168221));
#50954=CARTESIAN_POINT('Ctrl Pts',(152.544654507995,-4.84815353813783,335.827399742048));
#50955=CARTESIAN_POINT('Ctrl Pts',(152.536943499239,-4.8251607797939,335.962125941552));
#50956=CARTESIAN_POINT('Ctrl Pts',(152.529232490482,-4.79654618123677,336.095902727458));
#50957=CARTESIAN_POINT('Ctrl Pts',(152.521521481725,-4.76241910271695,336.228229356666));
#50958=CARTESIAN_POINT('Ctrl Pts',(152.513809188586,-4.72828633982835,336.360578026829));
#50959=CARTESIAN_POINT('Ctrl Pts',(152.506096895447,-4.68863936876036,336.491475677609));
#50960=CARTESIAN_POINT('Ctrl Pts',(152.498384602308,-4.64363779901445,336.620435451989));
#50961=CARTESIAN_POINT('Ctrl Pts',(152.490669317794,-4.59861877446086,336.749445246138));
#50962=CARTESIAN_POINT('Ctrl Pts',(152.482954033279,-4.54824114900427,336.876515296162));
#50963=CARTESIAN_POINT('Ctrl Pts',(152.475238748765,-4.49271299228432,337.001177910996));
#50964=CARTESIAN_POINT('Ctrl Pts',(152.467514516525,-4.43712043733058,337.125985102072));
#50965=CARTESIAN_POINT('Ctrl Pts',(152.459790284285,-4.37636558809715,337.248378924183));
#50966=CARTESIAN_POINT('Ctrl Pts',(152.452066052045,-4.31070304883258,337.367915177384));
#50967=CARTESIAN_POINT('Ctrl Pts',(152.444336503922,-4.24499532004474,337.487533696461));
#50968=CARTESIAN_POINT('Ctrl Pts',(152.436606955799,-4.17437337887094,337.604290393913));
#50969=CARTESIAN_POINT('Ctrl Pts',(152.428877407677,-4.0991349989026,337.717770285229));
#50970=CARTESIAN_POINT('Ctrl Pts',(152.421136704814,-4.02378804020096,337.831413942735));
#50971=CARTESIAN_POINT('Ctrl Pts',(152.413396001951,-3.94381157655401,337.941771038094));
#50972=CARTESIAN_POINT('Ctrl Pts',(152.405655299089,-3.85954365291573,338.048459587027));
#50973=CARTESIAN_POINT('Ctrl Pts',(152.403633122117,-3.83752954674917,338.076330845052));
#50974=CARTESIAN_POINT('Ctrl Pts',(152.401610945146,-3.81522275940396,338.1039519362));
#50975=CARTESIAN_POINT('Ctrl Pts',(152.399588768174,-3.79262971843772,338.13131647735));
#50976=CARTESIAN_POINT('Ctrl Pts',(152.391813689396,-3.7057616174606,338.236530544255));
#50977=CARTESIAN_POINT('Ctrl Pts',(152.384038610617,-3.6143747021492,338.338293325041));
#50978=CARTESIAN_POINT('Ctrl Pts',(152.376263531839,-3.51877352575847,338.436192069271));
#50979=CARTESIAN_POINT('Ctrl Pts',(152.36849802079,-3.42328999270159,338.533970342864));
#50980=CARTESIAN_POINT('Ctrl Pts',(152.360732509741,-3.32360278753055,338.627893763896));
#50981=CARTESIAN_POINT('Ctrl Pts',(152.352966998692,-3.22005733709591,338.717581715082));
#50982=CARTESIAN_POINT('Ctrl Pts',(152.34520918717,-3.11661455227666,338.807180740405));
#50983=CARTESIAN_POINT('Ctrl Pts',(152.337451375648,-3.00932142862713,338.892552398822));
#50984=CARTESIAN_POINT('Ctrl Pts',(152.329693564125,-2.89856068800378,338.973352362988));
#50985=CARTESIAN_POINT('Ctrl Pts',(152.321941590602,-2.78788329835027,339.054091522617));
#50986=CARTESIAN_POINT('Ctrl Pts',(152.314189617079,-2.67374380029645,339.130265606399));
#50987=CARTESIAN_POINT('Ctrl Pts',(152.306437643556,-2.55655820592767,339.201570325748));
#50988=CARTESIAN_POINT('Ctrl Pts',(152.298688952999,-2.43942223972767,339.272844847505));
#50989=CARTESIAN_POINT('Ctrl Pts',(152.290940262441,-2.31924307620051,339.339253903599));
#50990=CARTESIAN_POINT('Ctrl Pts',(152.283191571884,-2.19646575499314,339.400536472936));
#50991=CARTESIAN_POINT('Ctrl Pts',(152.275444493506,-2.07371397863294,339.461806291923));
#50992=CARTESIAN_POINT('Ctrl Pts',(152.267697415128,-1.94836546933115,339.517951571258));
#50993=CARTESIAN_POINT('Ctrl Pts',(152.25995033675,-1.82088956307833,339.568757408921));
#50994=CARTESIAN_POINT('Ctrl Pts',(152.252203193444,-1.69341258845472,339.619563672386));
#50995=CARTESIAN_POINT('Ctrl Pts',(152.244456050138,-1.56380854441616,339.665030260208));
#50996=CARTESIAN_POINT('Ctrl Pts',(152.236708906833,-1.43256605030295,339.704990709238));
#50997=CARTESIAN_POINT('Ctrl Pts',(152.228960021804,-1.30129405009066,339.744960142226));
#50998=CARTESIAN_POINT('Ctrl Pts',(152.221211136776,-1.16838324066433,339.779420859315));
#50999=CARTESIAN_POINT('Ctrl Pts',(152.213462251748,-1.03433628902268,339.808256597116));
#51000=CARTESIAN_POINT('Ctrl Pts',(152.205705141974,-0.900147058561605,
339.837122941467));
#51001=CARTESIAN_POINT('Ctrl Pts',(152.197948032199,-0.764819659696912,
339.860352297742));
#51002=CARTESIAN_POINT('Ctrl Pts',(152.190190922424,-0.628866364604577,
339.877879678505));
#51003=CARTESIAN_POINT('Ctrl Pts',(152.182429667498,-0.492840420418242,
339.895416425339));
#51004=CARTESIAN_POINT('Ctrl Pts',(152.174668412572,-0.356188302785288,
339.907245091643));
#51005=CARTESIAN_POINT('Ctrl Pts',(152.166907157646,-0.219425259392771,
339.913352787867));
#51006=CARTESIAN_POINT('Ctrl Pts',(152.159133487241,-0.0824434397018431,
339.919470254415));
#51007=CARTESIAN_POINT('Ctrl Pts',(152.151359816836,0.0546492692580443,
339.919848462023));
#51008=CARTESIAN_POINT('Ctrl Pts',(152.143586146431,0.191338874009855,339.914526680952));
#51009=CARTESIAN_POINT('Ctrl Pts',(152.136174342254,0.32166554477545,339.909452630071));
#51010=CARTESIAN_POINT('Ctrl Pts',(152.128762538077,0.451625508863558,339.899197339723));
#51011=CARTESIAN_POINT('Ctrl Pts',(152.1213507339,0.580781267816581,339.883838263237));
#51012=CARTESIAN_POINT('Ctrl Pts',(152.113575655122,0.716267335250423,339.86772639266));
#51013=CARTESIAN_POINT('Ctrl Pts',(152.105800576343,0.851296532281904,339.84594686575));
#51014=CARTESIAN_POINT('Ctrl Pts',(152.098025497565,0.985356957022539,339.818532424893));
#51015=CARTESIAN_POINT('Ctrl Pts',(152.090259986516,1.11925241187564,339.791151719251));
#51016=CARTESIAN_POINT('Ctrl Pts',(152.082494475467,1.25218108715821,339.758149974135));
#51017=CARTESIAN_POINT('Ctrl Pts',(152.074728964418,1.38363598338646,339.7196116925));
#51018=CARTESIAN_POINT('Ctrl Pts',(152.066971152896,1.51496054170246,339.681111621683));
#51019=CARTESIAN_POINT('Ctrl Pts',(152.059213341373,1.64481385627521,339.637086048002));
#51020=CARTESIAN_POINT('Ctrl Pts',(152.051455529851,1.77269926213441,339.587670475146));
#51021=CARTESIAN_POINT('Ctrl Pts',(152.043703556328,1.90048843017039,339.538292089076));
#51022=CARTESIAN_POINT('Ctrl Pts',(152.035951582805,2.02631227404551,339.483531917705));
#51023=CARTESIAN_POINT('Ctrl Pts',(152.028199609282,2.14968978298609,339.423575126459));
#51024=CARTESIAN_POINT('Ctrl Pts',(152.020450918724,2.27301504147835,339.363643726949));
#51025=CARTESIAN_POINT('Ctrl Pts',(152.012702228167,2.39389567478669,339.298520255233));
#51026=CARTESIAN_POINT('Ctrl Pts',(152.004953537609,2.51187134821484,339.228437701151));
#51027=CARTESIAN_POINT('Ctrl Pts',(151.997206459231,2.6298224758187,339.158369728331));
#51028=CARTESIAN_POINT('Ctrl Pts',(151.989459380854,2.74486950989806,339.08334492493));
#51029=CARTESIAN_POINT('Ctrl Pts',(151.981712302476,2.85657775012334,339.00364166978));
#51030=CARTESIAN_POINT('Ctrl Pts',(151.97396515917,2.96828692657116,338.923937746641));
#51031=CARTESIAN_POINT('Ctrl Pts',(151.966218015864,3.07665693516562,338.839555520571));
#51032=CARTESIAN_POINT('Ctrl Pts',(151.958470872558,3.1812833735312,338.750815799235));
#51033=CARTESIAN_POINT('Ctrl Pts',(151.95072198753,3.28593333414165,338.662056127327));
#51034=CARTESIAN_POINT('Ctrl Pts',(151.942973102502,3.38683775173035,338.568937263524));
#51035=CARTESIAN_POINT('Ctrl Pts',(151.935224217474,3.48362683597688,338.471818994441));
#51036=CARTESIAN_POINT('Ctrl Pts',(151.927467107699,3.58051865315734,338.374597643024));
#51037=CARTESIAN_POINT('Ctrl Pts',(151.919709997925,3.67328613503527,338.273368683815));
#51038=CARTESIAN_POINT('Ctrl Pts',(151.91195288815,3.761597412422,338.168527728987));
#51039=CARTESIAN_POINT('Ctrl Pts',(151.904191633224,3.84995588053175,338.063630750505));
#51040=CARTESIAN_POINT('Ctrl Pts',(151.896430378297,3.93385316032766,337.955118239508));
#51041=CARTESIAN_POINT('Ctrl Pts',(151.888669123371,4.01299958262628,337.843416503494));
#51042=CARTESIAN_POINT('Ctrl Pts',(151.880895452967,4.0922726134067,337.731536081106));
#51043=CARTESIAN_POINT('Ctrl Pts',(151.873121782562,4.16677938744925,337.616456567235));
#51044=CARTESIAN_POINT('Ctrl Pts',(151.865348112157,4.23627477659072,337.498631441354));
#51045=CARTESIAN_POINT('Ctrl Pts',(151.85793630798,4.30253513864828,337.386291103428));
#51046=CARTESIAN_POINT('Ctrl Pts',(151.850524503803,4.36424003987656,337.271455270997));
#51047=CARTESIAN_POINT('Ctrl Pts',(151.843112699626,4.42121785691321,337.154533760286));
#51048=CARTESIAN_POINT('Ctrl Pts',(151.835337620848,4.48098832649089,337.031881578044));
#51049=CARTESIAN_POINT('Ctrl Pts',(151.827562542069,4.53574550415438,336.906546493819));
#51050=CARTESIAN_POINT('Ctrl Pts',(151.819787463291,4.58523990418909,336.778976695612));
#51051=CARTESIAN_POINT('Ctrl Pts',(151.812021952242,4.63467339821358,336.651563880164));
#51052=CARTESIAN_POINT('Ctrl Pts',(151.804256441193,4.67885686032506,336.521922183288));
#51053=CARTESIAN_POINT('Ctrl Pts',(151.796490930144,4.71758698434946,336.390523681063));
#51054=CARTESIAN_POINT('Ctrl Pts',(151.788733118621,4.75627870734306,336.259255460836));
#51055=CARTESIAN_POINT('Ctrl Pts',(151.780975307099,4.78952774268754,336.126234274207));
#51056=CARTESIAN_POINT('Ctrl Pts',(151.773217495577,4.81717926441125,335.991951106167));
#51057=CARTESIAN_POINT('Ctrl Pts',(151.765465522054,4.84480997748797,335.85776899047));
#51058=CARTESIAN_POINT('Ctrl Pts',(151.757713548531,4.86685148281693,335.722327164955));
#51059=CARTESIAN_POINT('Ctrl Pts',(151.749961575008,4.88319918742346,335.58613032548));
#51060=CARTESIAN_POINT('Ctrl Pts',(151.74221288445,4.8995399687674,335.449991165447));
#51061=CARTESIAN_POINT('Ctrl Pts',(151.734464193893,4.91019169886501,335.313098014693));
#51062=CARTESIAN_POINT('Ctrl Pts',(151.726715503335,4.91510119032694,335.175964062657));
#51063=CARTESIAN_POINT('Ctrl Pts',(151.718968424957,4.92000966032816,335.038858642485));
#51064=CARTESIAN_POINT('Ctrl Pts',(151.71122134658,4.91917825410186,334.901512911064));
#51065=CARTESIAN_POINT('Ctrl Pts',(151.703474268202,4.91260582505575,334.764443063935));
#51066=CARTESIAN_POINT('Ctrl Pts',(151.695727124896,4.90603334092635,334.627372068028));
#51067=CARTESIAN_POINT('Ctrl Pts',(151.68797998159,4.89371975672828,334.490577351451));
#51068=CARTESIAN_POINT('Ctrl Pts',(151.680232838284,4.87571600114181,334.354572592223));
#51069=CARTESIAN_POINT('Ctrl Pts',(151.672483953256,4.85770819792885,334.218537256238));
#51070=CARTESIAN_POINT('Ctrl Pts',(151.664735068228,4.8340077290053,334.083292618424));
#51071=CARTESIAN_POINT('Ctrl Pts',(151.6569861832,4.80471703184798,333.949344344531));
#51072=CARTESIAN_POINT('Ctrl Pts',(151.649229073425,4.77539524524206,333.815253896555));
#51073=CARTESIAN_POINT('Ctrl Pts',(151.641471963651,4.7404714612595,333.682462943592));
#51074=CARTESIAN_POINT('Ctrl Pts',(151.633714853876,4.700098765155,333.551464649969));
#51075=CARTESIAN_POINT('Ctrl Pts',(151.62595359895,4.65970449517258,333.420396355047));
#51076=CARTESIAN_POINT('Ctrl Pts',(151.618192344023,4.61385564178444,333.291122996449));
#51077=CARTESIAN_POINT('Ctrl Pts',(151.610431089097,4.56275393944487,333.164118862622));
#51078=CARTESIAN_POINT('Ctrl Pts',(151.602657418693,4.51157049103557,333.036911563571));
#51079=CARTESIAN_POINT('Ctrl Pts',(151.594883748288,4.45511756334005,332.91198109953));
#51080=CARTESIAN_POINT('Ctrl Pts',(151.587110077883,4.39364384400625,332.789779007763));
#51081=CARTESIAN_POINT('Ctrl Pts',(151.579698273706,4.33503174109739,332.673265452768));
#51082=CARTESIAN_POINT('Ctrl Pts',(151.572286469529,4.27185590237207,332.559232226702));
#51083=CARTESIAN_POINT('Ctrl Pts',(151.564874665352,4.20436807578962,332.448045426388));
#51084=CARTESIAN_POINT('Ctrl Pts',(151.557099586574,4.13357246979034,332.331409029781));
#51085=CARTESIAN_POINT('Ctrl Pts',(151.549324507795,4.05780777435867,332.217536545091));
#51086=CARTESIAN_POINT('Ctrl Pts',(151.541549429017,3.97731586931176,332.106880310423));
#51087=CARTESIAN_POINT('Ctrl Pts',(151.533783917968,3.89692301467819,331.996360245295));
#51088=CARTESIAN_POINT('Ctrl Pts',(151.526018406919,3.81181475258537,331.889048868374));
#51089=CARTESIAN_POINT('Ctrl Pts',(151.51825289587,3.72227804124411,331.785372611612));
#51090=CARTESIAN_POINT('Ctrl Pts',(151.510495084348,3.63283010581321,331.681799150162));
#51091=CARTESIAN_POINT('Ctrl Pts',(151.502737272826,3.53896271294899,331.581853930165));
#51092=CARTESIAN_POINT('Ctrl Pts',(151.494979461303,3.44100495718743,331.485932848235));
#51093=CARTESIAN_POINT('Ctrl Pts',(151.48722748778,3.34312091774286,331.390083949961));
#51094=CARTESIAN_POINT('Ctrl Pts',(151.479475514257,3.24115292041716,331.298253434458));
#51095=CARTESIAN_POINT('Ctrl Pts',(151.471723540734,3.13546877346369,331.210802376078));
#51096=CARTESIAN_POINT('Ctrl Pts',(151.463974850177,3.02982938380956,331.123388353274));
#51097=CARTESIAN_POINT('Ctrl Pts',(151.456226159619,2.9204772752052,331.04035034739));
#51098=CARTESIAN_POINT('Ctrl Pts',(151.448477469062,2.80781521685033,330.962010801089));
#51099=CARTESIAN_POINT('Ctrl Pts',(151.440730390684,2.69517659877782,330.883687553985));
#51100=CARTESIAN_POINT('Ctrl Pts',(151.432983312306,2.57922972146833,330.81006104505));
#51101=CARTESIAN_POINT('Ctrl Pts',(151.425236233928,2.46040804427769,330.741411581503));
#51102=CARTESIAN_POINT('Ctrl Pts',(151.417489090622,2.34158537124667,330.672761542608));
#51103=CARTESIAN_POINT('Ctrl Pts',(151.409741947317,2.21988818872619,330.60908882784));
#51104=CARTESIAN_POINT('Ctrl Pts',(151.401994804011,2.09577601995414,330.550628590836));
#51105=CARTESIAN_POINT('Ctrl Pts',(151.394245918983,1.97163594813191,330.49215521073));
#51106=CARTESIAN_POINT('Ctrl Pts',(151.386497033955,1.84508016320923,330.438896806818));
#51107=CARTESIAN_POINT('Ctrl Pts',(151.378748148927,1.7165893250997,330.391040881994));
#51108=CARTESIAN_POINT('Ctrl Pts',(151.370991039152,1.58796210548695,330.343134162396));
#51109=CARTESIAN_POINT('Ctrl Pts',(151.363233929377,1.45739609673067,330.300641513222));
#51110=CARTESIAN_POINT('Ctrl Pts',(151.355476819602,1.3253888544502,330.26370108133));
#51111=CARTESIAN_POINT('Ctrl Pts',(151.347715564676,1.19331107172027,330.226740909652));
#51112=CARTESIAN_POINT('Ctrl Pts',(151.33995430975,1.05979090117466,330.195338956567));
#51113=CARTESIAN_POINT('Ctrl Pts',(151.332193054824,0.925336352174291,330.169582243962));
#51114=CARTESIAN_POINT('Ctrl Pts',(151.324419384419,0.790666719713976,330.143784329011));
#51115=CARTESIAN_POINT('Ctrl Pts',(151.316645714015,0.655060108782703,330.123649757679));
#51116=CARTESIAN_POINT('Ctrl Pts',(151.30887204361,0.51903080585563,330.109213755941));
#51117=CARTESIAN_POINT('Ctrl Pts',(151.301460239433,0.389333699706613,330.095449753558));
#51118=CARTESIAN_POINT('Ctrl Pts',(151.294048435256,0.259252655752013,330.08686574229));
#51119=CARTESIAN_POINT('Ctrl Pts',(151.286636631079,0.129231767886393,330.083448137905));
#51120=CARTESIAN_POINT('Ctrl Pts',(151.2788615523,-0.00716183100589846,
330.079863026549));
#51121=CARTESIAN_POINT('Ctrl Pts',(151.271086473522,-0.143920256820354,
330.081952239839));
#51122=CARTESIAN_POINT('Ctrl Pts',(151.263311394744,-0.280532233746121,
330.08975716198));
#51123=CARTESIAN_POINT('Ctrl Pts',(151.255545883695,-0.416976100936998,
330.097552479667));
#51124=CARTESIAN_POINT('Ctrl Pts',(151.247780372645,-0.553273491307314,
330.111049489388));
#51125=CARTESIAN_POINT('Ctrl Pts',(151.240014861596,-0.688910519575954,
330.130237648661));
#51126=CARTESIAN_POINT('Ctrl Pts',(151.232257050074,-0.824413063335708,
330.149406782818));
#51127=CARTESIAN_POINT('Ctrl Pts',(151.224499238552,-0.959256163457514,
330.174255782655));
#51128=CARTESIAN_POINT('Ctrl Pts',(151.21674142703,-1.09292881009604,330.204722147929));
#51129=CARTESIAN_POINT('Ctrl Pts',(151.208989453507,-1.22650086382965,330.235165586298));
#51130=CARTESIAN_POINT('Ctrl Pts',(151.201237479984,-1.35890383770935,330.271217889468));
#51131=CARTESIAN_POINT('Ctrl Pts',(151.193485506461,-1.48963505445896,330.312765157683));
#51132=CARTESIAN_POINT('Ctrl Pts',(151.185736815903,-1.6203109064604,330.354294830606));
#51133=CARTESIAN_POINT('Ctrl Pts',(151.177988125346,-1.74931603773501,330.401314721953));
#51134=CARTESIAN_POINT('Ctrl Pts',(151.170239434788,-1.87616133784369,330.453660626737));
#51135=CARTESIAN_POINT('Ctrl Pts',(151.16249235641,-2.00298024672811,330.505995640519));
#51136=CARTESIAN_POINT('Ctrl Pts',(151.154745278032,-2.12763985718702,330.563654314594));
#51137=CARTESIAN_POINT('Ctrl Pts',(151.146998199654,-2.24966988316949,330.626423834062));
#51138=CARTESIAN_POINT('Ctrl Pts',(151.139251056349,-2.37170093188103,330.6891938796));
#51139=CARTESIAN_POINT('Ctrl Pts',(151.131503913043,-2.49110200457205,330.757074677176));
#51140=CARTESIAN_POINT('Ctrl Pts',(151.123756769737,-2.60742668113987,330.829807059022));
#51141=CARTESIAN_POINT('Ctrl Pts',(151.116007884709,-2.72377750996423,330.902555792652));
#51142=CARTESIAN_POINT('Ctrl Pts',(151.108258999681,-2.83705023502251,330.98015807382));
#51143=CARTESIAN_POINT('Ctrl Pts',(151.100510114653,-2.94682706847255,331.062311173922));
#51144=CARTESIAN_POINT('Ctrl Pts',(151.092753004878,-3.05672042018824,331.144551472174));
#51145=CARTESIAN_POINT('Ctrl Pts',(151.084995895103,-3.16311015463384,331.231352003745));
#51146=CARTESIAN_POINT('Ctrl Pts',(151.077238785329,-3.26561084527332,331.322369122691));
#51147=CARTESIAN_POINT('Ctrl Pts',(151.069477530402,-3.36816630900461,331.413434878276));
#51148=CARTESIAN_POINT('Ctrl Pts',(151.061716275476,-3.46682830695273,331.508721439558));
#51149=CARTESIAN_POINT('Ctrl Pts',(151.05395502055,-3.56124874754242,331.607848703164));
#51150=CARTESIAN_POINT('Ctrl Pts',(151.046181350145,-3.65582023006556,331.707134538086));
#51151=CARTESIAN_POINT('Ctrl Pts',(151.038407679741,-3.74613633893139,331.810273058389));
#51152=CARTESIAN_POINT('Ctrl Pts',(151.030634009336,-3.83188914194493,331.9168508524));
#51153=CARTESIAN_POINT('Ctrl Pts',(151.023222205159,-3.91365013134875,332.018467424461));
#51154=CARTESIAN_POINT('Ctrl Pts',(151.015810400982,-3.99126292648982,332.123210048434));
#51155=CARTESIAN_POINT('Ctrl Pts',(151.008398596804,-4.06449862595056,332.230697925082));
#51156=CARTESIAN_POINT('Ctrl Pts',(151.00050640211,-4.14248104222782,332.345152547666));
#51157=CARTESIAN_POINT('Ctrl Pts',(150.992614207416,-4.2157420164164,332.463074658565));
#51158=CARTESIAN_POINT('Ctrl Pts',(150.984722012722,-4.28396339709006,332.584044562726));
#51159=CARTESIAN_POINT('Ctrl Pts',(150.976840276783,-4.35209437062295,332.704854157274));
#51160=CARTESIAN_POINT('Ctrl Pts',(150.968958540845,-4.41519886088457,332.82870318226));
#51161=CARTESIAN_POINT('Ctrl Pts',(150.961076804906,-4.47300097256328,332.955141725706));
#51162=CARTESIAN_POINT('Ctrl Pts',(150.953203992128,-4.5307376446544,333.081437124103));
#51163=CARTESIAN_POINT('Ctrl Pts',(150.945331179351,-4.58318373356687,333.210315865706));
#51164=CARTESIAN_POINT('Ctrl Pts',(150.937458366573,-4.63010851960001,333.341302270084));
#51165=CARTESIAN_POINT('Ctrl Pts',(150.929488284068,-4.6776130680765,333.473907030225));
#51166=CARTESIAN_POINT('Ctrl Pts',(150.921518201563,-4.71945875524838,333.608671554959));
#51167=CARTESIAN_POINT('Ctrl Pts',(150.913548119057,-4.75545540311106,333.745078898288));
#51168=CARTESIAN_POINT('Ctrl Pts',(150.905689535788,-4.7909484678868,333.879577940842));
#51169=CARTESIAN_POINT('Ctrl Pts',(150.897830952519,-4.82075498173637,334.015673759918));
#51170=CARTESIAN_POINT('Ctrl Pts',(150.88997236925,-4.84474209496655,334.152853557076));
#51171=CARTESIAN_POINT('Ctrl Pts',(150.881946537126,-4.8692397095272,334.292952858064));
#51172=CARTESIAN_POINT('Ctrl Pts',(150.873920705003,-4.88766729808636,334.434182418524));
#51173=CARTESIAN_POINT('Ctrl Pts',(150.865894872879,-4.8999380593034,334.575983399511));
#51174=CARTESIAN_POINT('Ctrl Pts',(150.857869040755,-4.91220882052043,334.717784380498));
#51175=CARTESIAN_POINT('Ctrl Pts',(150.849843208632,-4.91832270088092,334.860156367047));
#51176=CARTESIAN_POINT('Ctrl Pts',(150.841817376508,-4.91824934725933,335.002533906699));
#51177=CARTESIAN_POINT('',(149.091817376546,-4.91824904199947,335.003069751012));
#51178=CARTESIAN_POINT('Ctrl Pts',(150.841817376458,-4.91824934725888,335.002533907583));
#51179=CARTESIAN_POINT('Ctrl Pts',(150.833275004512,-4.91817127259594,335.154074817202));
#51180=CARTESIAN_POINT('Ctrl Pts',(150.824732632566,-4.911085205369,335.305373671443));
#51181=CARTESIAN_POINT('Ctrl Pts',(150.81619026062,-4.89708260457338,335.455812490488));
#51182=CARTESIAN_POINT('Ctrl Pts',(150.807602559515,-4.88300570051299,335.60704959662));
#51183=CARTESIAN_POINT('Ctrl Pts',(150.799014858409,-4.86193875138165,335.757417279804));
#51184=CARTESIAN_POINT('Ctrl Pts',(150.790427157303,-4.83402492592403,335.906303524237));
#51185=CARTESIAN_POINT('Ctrl Pts',(150.781816020346,-4.80603492358686,336.055596079497));
#51186=CARTESIAN_POINT('Ctrl Pts',(150.773204883389,-4.77116074209068,336.20339887848));
#51187=CARTESIAN_POINT('Ctrl Pts',(150.764593746432,-4.72959553291164,336.349114212201));
#51188=CARTESIAN_POINT('Ctrl Pts',(150.755951736087,-4.68788130057508,336.49535197705));
#51189=CARTESIAN_POINT('Ctrl Pts',(150.747309725742,-4.63942809708577,336.63948706579));
#51190=CARTESIAN_POINT('Ctrl Pts',(150.738667715397,-4.58447845653032,336.780938051733));
#51191=CARTESIAN_POINT('Ctrl Pts',(150.735831997775,-4.56644773707678,336.827352605462));
#51192=CARTESIAN_POINT('Ctrl Pts',(150.732996280153,-4.54771791320033,336.873478355996));
#51193=CARTESIAN_POINT('Ctrl Pts',(150.730160562531,-4.52829862265166,336.919295351579));
#51194=CARTESIAN_POINT('Ctrl Pts',(150.722385483752,-4.47505407084348,337.044918138305));
#51195=CARTESIAN_POINT('Ctrl Pts',(150.714610404974,-4.41649393344499,337.168522111345));
#51196=CARTESIAN_POINT('Ctrl Pts',(150.706835326195,-4.35279236519956,337.289624791961));
#51197=CARTESIAN_POINT('Ctrl Pts',(150.699069815146,-4.28916918578925,337.410578448018));
#51198=CARTESIAN_POINT('Ctrl Pts',(150.691304304097,-4.22041734439196,337.529036593359));
#51199=CARTESIAN_POINT('Ctrl Pts',(150.683538793048,-4.14675933748497,337.64453588735));
#51200=CARTESIAN_POINT('Ctrl Pts',(150.675780981526,-4.07317436270628,337.759920663454));
#51201=CARTESIAN_POINT('Ctrl Pts',(150.668023170004,-3.9946931118216,337.872352099019));
#51202=CARTESIAN_POINT('Ctrl Pts',(150.660265358481,-3.9115841789396,337.981390996426));
#51203=CARTESIAN_POINT('Ctrl Pts',(150.652513384958,-3.82853778816521,338.090347838605));
#51204=CARTESIAN_POINT('Ctrl Pts',(150.644761411435,-3.74087088308443,338.195916914615));
#51205=CARTESIAN_POINT('Ctrl Pts',(150.637009437912,-3.64889538647973,338.29768790534));
#51206=CARTESIAN_POINT('Ctrl Pts',(150.629260747355,-3.55695884155242,338.399415795991));
#51207=CARTESIAN_POINT('Ctrl Pts',(150.621512056797,-3.46071759581903,338.497348511143));
#51208=CARTESIAN_POINT('Ctrl Pts',(150.61376336624,-3.36052373623727,338.591108920749));
#51209=CARTESIAN_POINT('Ctrl Pts',(150.606016287862,-3.26035072282476,338.684849822719));
#51210=CARTESIAN_POINT('Ctrl Pts',(150.598269209484,-3.15622701654611,338.774419878914));
#51211=CARTESIAN_POINT('Ctrl Pts',(150.590522131106,-3.04854114736669,338.859479231103));
#51212=CARTESIAN_POINT('Ctrl Pts',(150.5827749878,-2.94085437567601,338.944539296171));
#51213=CARTESIAN_POINT('Ctrl Pts',(150.575027844494,-2.82960568826708,339.025088339549));
#51214=CARTESIAN_POINT('Ctrl Pts',(150.567280701189,-2.71521591517816,339.100827428271));
#51215=CARTESIAN_POINT('Ctrl Pts',(150.559531816161,-2.60080042483987,339.176583544749));
#51216=CARTESIAN_POINT('Ctrl Pts',(150.551782931133,-2.48324276944337,339.247527338997));
#51217=CARTESIAN_POINT('Ctrl Pts',(150.544034046104,-2.36299156328245,339.313403984599));
#51218=CARTESIAN_POINT('Ctrl Pts',(150.53627693633,-2.24261272124873,339.379350552354));
#51219=CARTESIAN_POINT('Ctrl Pts',(150.528519826555,-2.1195349607506,339.440219039662));
#51220=CARTESIAN_POINT('Ctrl Pts',(150.52076271678,-1.99423072945102,339.495801025425));
#51221=CARTESIAN_POINT('Ctrl Pts',(150.513001461854,-1.8688595395767,339.551412712424));
#51222=CARTESIAN_POINT('Ctrl Pts',(150.505240206928,-1.74125987164417,339.601732125612));
#51223=CARTESIAN_POINT('Ctrl Pts',(150.497478952002,-1.61192188696308,339.646599928209));
#51224=CARTESIAN_POINT('Ctrl Pts',(150.489705281597,-1.48237700365775,339.691539504667));
#51225=CARTESIAN_POINT('Ctrl Pts',(150.481931611192,-1.35108862138193,339.731009931196));
#51226=CARTESIAN_POINT('Ctrl Pts',(150.474157940788,-1.21856057878688,339.764902221277));
#51227=CARTESIAN_POINT('Ctrl Pts',(150.466746136611,-1.09220174846003,339.7972168171));
#51228=CARTESIAN_POINT('Ctrl Pts',(150.459334332434,-0.964716354347555,
339.824460853759));
#51229=CARTESIAN_POINT('Ctrl Pts',(150.451922528257,-0.836545810924017,
339.846583762685));
#51230=CARTESIAN_POINT('Ctrl Pts',(150.444147449478,-0.70209324736589,339.869790981279));
#51231=CARTESIAN_POINT('Ctrl Pts',(150.4363723707,-0.566461778935172,339.887435714621));
#51232=CARTESIAN_POINT('Ctrl Pts',(150.428597291922,-0.43015137742047,339.899403316222));
#51233=CARTESIAN_POINT('Ctrl Pts',(150.420831780873,-0.294008714532869,
339.911356190926));
#51234=CARTESIAN_POINT('Ctrl Pts',(150.413066269824,-0.15718916656197,339.91764580031));
#51235=CARTESIAN_POINT('Ctrl Pts',(150.405300758775,-0.0202027721430652,
339.918208506204));
#51236=CARTESIAN_POINT('Ctrl Pts',(150.397542947252,0.116647799867042,339.918770654173));
#51237=CARTESIAN_POINT('Ctrl Pts',(150.38978513573,0.253664500759507,339.913617197079));
#51238=CARTESIAN_POINT('Ctrl Pts',(150.382027324208,0.390332648203933,339.902736326404));
#51239=CARTESIAN_POINT('Ctrl Pts',(150.374275350685,0.526897948533226,339.891863643931));
#51240=CARTESIAN_POINT('Ctrl Pts',(150.366523377162,0.663114829432412,339.875272157738));
#51241=CARTESIAN_POINT('Ctrl Pts',(150.358771403639,0.798469445487928,339.853002123132));
#51242=CARTESIAN_POINT('Ctrl Pts',(150.351022713081,0.933766738783276,339.830741519898));
#51243=CARTESIAN_POINT('Ctrl Pts',(150.343274022524,1.06820210864563,339.802807214691));
#51244=CARTESIAN_POINT('Ctrl Pts',(150.335525331966,1.20126788391611,339.769291198236));
#51245=CARTESIAN_POINT('Ctrl Pts',(150.327778253588,1.33430597374067,339.735782155068));
#51246=CARTESIAN_POINT('Ctrl Pts',(150.32003117521,1.46597465697226,339.696693806012));
#51247=CARTESIAN_POINT('Ctrl Pts',(150.312284096833,1.59577788371615,339.652168957416));
#51248=CARTESIAN_POINT('Ctrl Pts',(150.304536953527,1.72558219833606,339.607643735658));
#51249=CARTESIAN_POINT('Ctrl Pts',(150.296789810221,1.85352065555674,339.557682050305));
#51250=CARTESIAN_POINT('Ctrl Pts',(150.289042666915,1.97911414098799,339.502476016531));
#51251=CARTESIAN_POINT('Ctrl Pts',(150.281293781887,2.10473586250115,339.44725757127));
#51252=CARTESIAN_POINT('Ctrl Pts',(150.273544896859,2.22801120539586,339.386792588686));
#51253=CARTESIAN_POINT('Ctrl Pts',(150.265796011831,2.34848310976586,339.321320416915));
#51254=CARTESIAN_POINT('Ctrl Pts',(150.258038902056,2.46908288425991,339.255778752304));
#51255=CARTESIAN_POINT('Ctrl Pts',(150.250281792282,2.58687293221568,339.185219468868));
#51256=CARTESIAN_POINT('Ctrl Pts',(150.242524682507,2.70142231934475,339.10992706931));
#51257=CARTESIAN_POINT('Ctrl Pts',(150.234763427581,2.81603291800372,339.034594435901));
#51258=CARTESIAN_POINT('Ctrl Pts',(150.227002172654,2.92739908805709,338.95452387472));
#51259=CARTESIAN_POINT('Ctrl Pts',(150.219240917728,3.03512158539585,338.870041346596));
#51260=CARTESIAN_POINT('Ctrl Pts',(150.211467247324,3.14301640362368,338.78542367396));
#51261=CARTESIAN_POINT('Ctrl Pts',(150.203693576919,3.24725560433177,338.696380184997));
#51262=CARTESIAN_POINT('Ctrl Pts',(150.195919906514,3.34747488242671,338.603275589519));
#51263=CARTESIAN_POINT('Ctrl Pts',(150.188508102337,3.44302892901514,338.51450503536));
#51264=CARTESIAN_POINT('Ctrl Pts',(150.18109629816,3.53492868253356,338.422043159167));
#51265=CARTESIAN_POINT('Ctrl Pts',(150.173684493983,3.62289274409264,338.326233790235));
#51266=CARTESIAN_POINT('Ctrl Pts',(150.165909415205,3.71516818633996,338.22572851873));
#51267=CARTESIAN_POINT('Ctrl Pts',(150.158134336426,3.80340398914119,338.121221701023));
#51268=CARTESIAN_POINT('Ctrl Pts',(150.150359257648,3.88723318039331,338.013071732261));
#51269=CARTESIAN_POINT('Ctrl Pts',(150.142593746599,3.97095921448882,337.905054848921));
#51270=CARTESIAN_POINT('Ctrl Pts',(150.13482823555,4.05028918931382,337.79340404065));
#51271=CARTESIAN_POINT('Ctrl Pts',(150.127062724501,4.12489357900246,337.678513771554));
#51272=CARTESIAN_POINT('Ctrl Pts',(150.119304912978,4.19942399822149,337.563737416494));
#51273=CARTESIAN_POINT('Ctrl Pts',(150.111547101456,4.26923794507597,337.445728318251));
#51274=CARTESIAN_POINT('Ctrl Pts',(150.103789289934,4.33404696539169,337.324912893912));
#51275=CARTESIAN_POINT('Ctrl Pts',(150.096037316411,4.39880721486438,337.204188387011));
#51276=CARTESIAN_POINT('Ctrl Pts',(150.088285342888,4.45856985053881,337.080662100605));
#51277=CARTESIAN_POINT('Ctrl Pts',(150.080533369365,4.51309065272202,336.95478792272));
#51278=CARTESIAN_POINT('Ctrl Pts',(150.072784678807,4.56758836531311,336.828967052624));
#51279=CARTESIAN_POINT('Ctrl Pts',(150.06503598825,4.61684850464463,336.700800626637));
#51280=CARTESIAN_POINT('Ctrl Pts',(150.057287297692,4.66067369768583,336.570765337725));
#51281=CARTESIAN_POINT('Ctrl Pts',(150.049540219314,4.70448977252959,336.440757103742));
#51282=CARTESIAN_POINT('Ctrl Pts',(150.041793140937,4.74287302553924,336.308881150421));
#51283=CARTESIAN_POINT('Ctrl Pts',(150.034046062559,4.77567510455741,336.175631897411));
#51284=CARTESIAN_POINT('Ctrl Pts',(150.026298919253,4.80847745848857,336.042381527644));
#51285=CARTESIAN_POINT('Ctrl Pts',(150.018551775947,4.83569845169829,335.907758214774));
#51286=CARTESIAN_POINT('Ctrl Pts',(150.010804632641,4.85724036164861,335.772268820859));
#51287=CARTESIAN_POINT('Ctrl Pts',(150.003055747613,4.87878711467762,335.636748966052));
#51288=CARTESIAN_POINT('Ctrl Pts',(149.995306862585,4.89465218243718,335.500363028692));
#51289=CARTESIAN_POINT('Ctrl Pts',(149.987557977557,4.90478949653835,335.363624885214));
#51290=CARTESIAN_POINT('Ctrl Pts',(149.979800867782,4.91493757048945,335.226741606458));
#51291=CARTESIAN_POINT('Ctrl Pts',(149.972043758008,4.91934571747228,335.089505765234));
#51292=CARTESIAN_POINT('Ctrl Pts',(149.964286648233,4.91801997860885,334.952433704115));
#51293=CARTESIAN_POINT('Ctrl Pts',(149.956525393307,4.91669353131296,334.815288396069));
#51294=CARTESIAN_POINT('Ctrl Pts',(149.948764138381,4.90962711299133,334.678307432676));
#51295=CARTESIAN_POINT('Ctrl Pts',(149.941002883454,4.89687877716162,334.542002942931));
#51296=CARTESIAN_POINT('Ctrl Pts',(149.93322921305,4.88411004814925,334.405480410423));
#51297=CARTESIAN_POINT('Ctrl Pts',(149.925455542645,4.86564129136798,334.26963690151));
#51298=CARTESIAN_POINT('Ctrl Pts',(149.91768187224,4.8415820526893,334.134976133522));
#51299=CARTESIAN_POINT('Ctrl Pts',(149.910270068063,4.81864277735936,334.006583856681));
#51300=CARTESIAN_POINT('Ctrl Pts',(149.902858263886,4.79062184291682,333.879266966682));
#51301=CARTESIAN_POINT('Ctrl Pts',(149.895446459709,4.75765610166489,333.753448163617));
#51302=CARTESIAN_POINT('Ctrl Pts',(149.887671380931,4.72307461123441,333.621462606218));
#51303=CARTESIAN_POINT('Ctrl Pts',(149.879896302152,4.68294205453384,333.490708601553));
#51304=CARTESIAN_POINT('Ctrl Pts',(149.872121223374,4.6373612240282,333.36168869247));
#51305=CARTESIAN_POINT('Ctrl Pts',(149.864355712325,4.59183648363631,333.2328275506));
#51306=CARTESIAN_POINT('Ctrl Pts',(149.856590201276,4.54087693832692,333.105696623462));
#51307=CARTESIAN_POINT('Ctrl Pts',(149.848824690227,4.48463597602692,332.980786483547));
#51308=CARTESIAN_POINT('Ctrl Pts',(149.841066878704,4.42845077680477,332.8560001924));
#51309=CARTESIAN_POINT('Ctrl Pts',(149.833309067182,4.3669947410451,332.733430660655));
#51310=CARTESIAN_POINT('Ctrl Pts',(149.82555125566,4.30047035286795,332.613551214335));
#51311=CARTESIAN_POINT('Ctrl Pts',(149.817799282137,4.23399602640254,332.493761981099));
#51312=CARTESIAN_POINT('Ctrl Pts',(149.810047308614,4.16246112818873,332.376659144269));
#51313=CARTESIAN_POINT('Ctrl Pts',(149.802295335091,4.08611518106168,332.262693698251));
#51314=CARTESIAN_POINT('Ctrl Pts',(149.794546644533,4.00980156648857,332.148776516666));
#51315=CARTESIAN_POINT('Ctrl Pts',(149.786797953976,3.92868117250317,332.037994407293));
#51316=CARTESIAN_POINT('Ctrl Pts',(149.779049263418,3.84304805051992,331.930771311242));
#51317=CARTESIAN_POINT('Ctrl Pts',(149.77130218504,3.75743274522292,331.823570523852));
#51318=CARTESIAN_POINT('Ctrl Pts',(149.763555106662,3.66730682325951,331.719927582142));
#51319=CARTESIAN_POINT('Ctrl Pts',(149.755808028285,3.57300577079482,331.62023479745));
#51320=CARTESIAN_POINT('Ctrl Pts',(149.748060884979,3.47870392799654,331.520541177236));
#51321=CARTESIAN_POINT('Ctrl Pts',(149.740313741673,3.38022715350794,331.424798064034));
#51322=CARTESIAN_POINT('Ctrl Pts',(149.732566598367,3.27794879517396,331.333361926953));
#51323=CARTESIAN_POINT('Ctrl Pts',(149.724817713339,3.1756474424936,331.241905233087));
#51324=CARTESIAN_POINT('Ctrl Pts',(149.717068828311,3.06954309660301,331.154757702613));
#51325=CARTESIAN_POINT('Ctrl Pts',(149.709319943283,2.96004295691114,331.072236163446));
#51326=CARTESIAN_POINT('Ctrl Pts',(149.701562833508,2.85042659263962,330.989627035065));
#51327=CARTESIAN_POINT('Ctrl Pts',(149.693805723733,2.73740754722742,330.911653941946));
#51328=CARTESIAN_POINT('Ctrl Pts',(149.686048613959,2.6214232933585,330.838591226575));
#51329=CARTESIAN_POINT('Ctrl Pts',(149.678287359033,2.50537706121282,330.765489468825));
#51330=CARTESIAN_POINT('Ctrl Pts',(149.670526104106,2.38636280230974,330.697303511489));
#51331=CARTESIAN_POINT('Ctrl Pts',(149.66276484918,2.2648425929373,330.634261678511));
#51332=CARTESIAN_POINT('Ctrl Pts',(149.654991178776,2.14312799083321,330.571118999145));
#51333=CARTESIAN_POINT('Ctrl Pts',(149.647217508371,2.01889978206228,330.513137053365));
#51334=CARTESIAN_POINT('Ctrl Pts',(149.639443837966,1.89264083483156,330.460496312059));
#51335=CARTESIAN_POINT('Ctrl Pts',(149.632032033789,1.77225927197126,330.410306009927));
#51336=CARTESIAN_POINT('Ctrl Pts',(149.624620229612,1.65003204751828,330.36497093688));
#51337=CARTESIAN_POINT('Ctrl Pts',(149.617208425435,1.52638867762962,330.324604758172));
#51338=CARTESIAN_POINT('Ctrl Pts',(149.609433346657,1.3966851778673,330.282260112801));
#51339=CARTESIAN_POINT('Ctrl Pts',(149.601658267878,1.26501331659337,330.245249941333));
#51340=CARTESIAN_POINT('Ctrl Pts',(149.5938831891,1.13185131971292,330.213759758165));
#51341=CARTESIAN_POINT('Ctrl Pts',(149.586117678051,0.998853187147241,330.182308325671));
#51342=CARTESIAN_POINT('Ctrl Pts',(149.578352167002,0.86436894427227,330.15636345505));
#51343=CARTESIAN_POINT('Ctrl Pts',(149.570586655953,0.728894130971136,330.136061636047));
#51344=CARTESIAN_POINT('Ctrl Pts',(149.56282884443,0.593553641341721,330.115779946356));
#51345=CARTESIAN_POINT('Ctrl Pts',(149.555071032908,0.457224919894869,330.101130231268));
#51346=CARTESIAN_POINT('Ctrl Pts',(149.547313221386,0.320415572356604,330.092198361436));
#51347=CARTESIAN_POINT('Ctrl Pts',(149.539561247863,0.183709178190882,330.08327321312));
#51348=CARTESIAN_POINT('Ctrl Pts',(149.53180927434,0.0465232663262014,330.08005737079));
#51349=CARTESIAN_POINT('Ctrl Pts',(149.524057300817,-0.090627881296994,
330.082585064322));
#51350=CARTESIAN_POINT('Ctrl Pts',(149.516308610259,-0.227720945327791,
330.085111687374));
#51351=CARTESIAN_POINT('Ctrl Pts',(149.508559919702,-0.364778884404885,
330.093377001246));
#51352=CARTESIAN_POINT('Ctrl Pts',(149.500811229144,-0.501286069311462,
330.107363150691));
#51353=CARTESIAN_POINT('Ctrl Pts',(149.493064150766,-0.637764852758043,
330.121346390201));
#51354=CARTESIAN_POINT('Ctrl Pts',(149.485317072388,-0.773692721365163,
330.141048057943));
#51355=CARTESIAN_POINT('Ctrl Pts',(149.477569994011,-0.908558221347149,
330.166398338617));
#51356=CARTESIAN_POINT('Ctrl Pts',(149.469822850705,-1.04342485163183,330.191748831751));
#51357=CARTESIAN_POINT('Ctrl Pts',(149.462075707399,-1.17722871138541,330.222747960036));
#51358=CARTESIAN_POINT('Ctrl Pts',(149.454328564093,-1.30946799818671,330.259274673193));
#51359=CARTESIAN_POINT('Ctrl Pts',(149.446579679065,-1.44173701518701,330.295809598331));
#51360=CARTESIAN_POINT('Ctrl Pts',(149.438830794037,-1.57244038260137,330.337874477164));
#51361=CARTESIAN_POINT('Ctrl Pts',(149.431081909009,-1.70109131411029,330.385298340785));
#51362=CARTESIAN_POINT('Ctrl Pts',(149.423324799234,-1.82987879704736,330.432772540586));
#51363=CARTESIAN_POINT('Ctrl Pts',(149.415567689459,-1.95660912503818,330.485616952247));
#51364=CARTESIAN_POINT('Ctrl Pts',(149.407810579685,-2.08081485606185,330.543612158116));
#51365=CARTESIAN_POINT('Ctrl Pts',(149.400049324759,-2.20508695865685,330.601638354769));
#51366=CARTESIAN_POINT('Ctrl Pts',(149.392288069832,-2.32683142939363,330.664820650114));
#51367=CARTESIAN_POINT('Ctrl Pts',(149.384526814906,-2.44560620980308,330.732894033531));
#51368=CARTESIAN_POINT('Ctrl Pts',(149.376753144502,-2.56457099115257,330.801076312177));
#51369=CARTESIAN_POINT('Ctrl Pts',(149.368979474097,-2.68055625832943,330.87416510536));
#51370=CARTESIAN_POINT('Ctrl Pts',(149.361205803692,-2.79314894181757,330.951852022057));
#51371=CARTESIAN_POINT('Ctrl Pts',(149.353793999515,-2.90050040880148,331.025922594092));
#51372=CARTESIAN_POINT('Ctrl Pts',(149.346382195338,-3.00476780345651,331.104172665388));
#51373=CARTESIAN_POINT('Ctrl Pts',(149.338970391161,-3.10562310640945,331.186302557434));
#51374=CARTESIAN_POINT('Ctrl Pts',(149.331298440607,-3.21001832231312,331.271315120594));
#51375=CARTESIAN_POINT('Ctrl Pts',(149.323626490054,-3.31110645320642,331.36076925575));
#51376=CARTESIAN_POINT('Ctrl Pts',(149.315954539501,-3.408478394479,331.454374794642));
#51377=CARTESIAN_POINT('Ctrl Pts',(149.308292078548,-3.50572989430311,331.54786455083));
#51378=CARTESIAN_POINT('Ctrl Pts',(149.300629617595,-3.59927405891711,331.645495223002));
#51379=CARTESIAN_POINT('Ctrl Pts',(149.292967156642,-3.68873314137439,331.746935156775));
#51380=CARTESIAN_POINT('Ctrl Pts',(149.285312223662,-3.77810433489762,331.848275431046));
#51381=CARTESIAN_POINT('Ctrl Pts',(149.277657290682,-3.86339816508794,331.953417223214));
#51382=CARTESIAN_POINT('Ctrl Pts',(149.270002357702,-3.94427257793943,332.061990998411));
#51383=CARTESIAN_POINT('Ctrl Pts',(149.262353071697,-4.02508733046593,332.170484679714));
#51384=CARTESIAN_POINT('Ctrl Pts',(149.254703785692,-4.10148891324412,332.28240498521));
#51385=CARTESIAN_POINT('Ctrl Pts',(149.247054499687,-4.17317488513449,332.397348574899));
#51386=CARTESIAN_POINT('Ctrl Pts',(149.239408214288,-4.24483273657044,332.512247075347));
#51387=CARTESIAN_POINT('Ctrl Pts',(149.231761928889,-4.31177844248423,332.630166161405));
#51388=CARTESIAN_POINT('Ctrl Pts',(149.224115643491,-4.37375254171764,332.750673041481));
#51389=CARTESIAN_POINT('Ctrl Pts',(149.216470598857,-4.43571658439673,332.871160366873));
#51390=CARTESIAN_POINT('Ctrl Pts',(149.208825554224,-4.49271044121826,332.994234293507));
#51391=CARTESIAN_POINT('Ctrl Pts',(149.20118050959,-4.54452059642395,333.119437421627));
#51392=CARTESIAN_POINT('Ctrl Pts',(149.193534947129,-4.59633426092566,333.244649030223));
#51393=CARTESIAN_POINT('Ctrl Pts',(149.185889384667,-4.64296337287306,333.371989755078));
#51394=CARTESIAN_POINT('Ctrl Pts',(149.178243822206,-4.68424276676859,333.500982733763));
#51395=CARTESIAN_POINT('Ctrl Pts',(149.170592019132,-4.7255558545542,333.630081001669));
#51396=CARTESIAN_POINT('Ctrl Pts',(149.162940216057,-4.76151038023566,333.760833833398));
#51397=CARTESIAN_POINT('Ctrl Pts',(149.155288412982,-4.79199117641293,333.892749518997));
#51398=CARTESIAN_POINT('Ctrl Pts',(149.147633370225,-4.82248487779625,334.024721056127));
#51399=CARTESIAN_POINT('Ctrl Pts',(149.139978327468,-4.84750015936146,334.157856032681));
#51400=CARTESIAN_POINT('Ctrl Pts',(149.132323284711,-4.86697334089238,334.291654348822));
#51401=CARTESIAN_POINT('Ctrl Pts',(149.124657930291,-4.88647275361318,334.42563289689));
#51402=CARTESIAN_POINT('Ctrl Pts',(149.116992575872,-4.90041511348892,334.560276169459));
#51403=CARTESIAN_POINT('Ctrl Pts',(149.109327221452,-4.90878875424659,334.695080291417));
#51404=CARTESIAN_POINT('Ctrl Pts',(149.103490606483,-4.91516467821747,334.797723915313));
#51405=CARTESIAN_POINT('Ctrl Pts',(149.097653991514,-4.91831308596907,334.900460715021));
#51406=CARTESIAN_POINT('Ctrl Pts',(149.091817376545,-4.91824904199947,335.003069751012));
#51407=CARTESIAN_POINT('',(147.341817376463,-4.91824822950257,334.995826812387));
#51408=CARTESIAN_POINT('Ctrl Pts',(149.091817376508,-4.91824904199906,335.003069751671));
#51409=CARTESIAN_POINT('Ctrl Pts',(149.081455703301,-4.91813534547636,335.185230354129));
#51410=CARTESIAN_POINT('Ctrl Pts',(149.071094030094,-4.90790203713303,335.367074026762));
#51411=CARTESIAN_POINT('Ctrl Pts',(149.060732356887,-4.88765040461514,335.547774209657));
#51412=CARTESIAN_POINT('Ctrl Pts',(149.052957278108,-4.87245420656191,335.683366032445));
#51413=CARTESIAN_POINT('Ctrl Pts',(149.04518219933,-4.85158739502761,335.81853928431));
#51414=CARTESIAN_POINT('Ctrl Pts',(149.037407120552,-4.82507925338847,335.952781853847));
#51415=CARTESIAN_POINT('Ctrl Pts',(149.029641609503,-4.79860373170523,336.086859229356));
#51416=CARTESIAN_POINT('Ctrl Pts',(149.021876098454,-4.76650076753593,336.22000782148));
#51417=CARTESIAN_POINT('Ctrl Pts',(149.014110587405,-4.72885143676541,336.351720071428));
#51418=CARTESIAN_POINT('Ctrl Pts',(149.006352775883,-4.69123943541598,336.483301728297));
#51419=CARTESIAN_POINT('Ctrl Pts',(148.998594964361,-4.64809211799609,336.613449503702));
#51420=CARTESIAN_POINT('Ctrl Pts',(148.990837152838,-4.59954162977641,336.741665828583));
#51421=CARTESIAN_POINT('Ctrl Pts',(148.983085179315,-4.55102767733875,336.869785666614));
#51422=CARTESIAN_POINT('Ctrl Pts',(148.975333205792,-4.49711878525,336.995976583124));
#51423=CARTESIAN_POINT('Ctrl Pts',(148.967581232269,-4.43799686513836,337.119756327393));
#51424=CARTESIAN_POINT('Ctrl Pts',(148.959832541712,-4.37889998319499,337.243483650866));
#51425=CARTESIAN_POINT('Ctrl Pts',(148.952083851154,-4.31459463234466,337.364801481087));
#51426=CARTESIAN_POINT('Ctrl Pts',(148.944335160597,-4.24531068722392,337.483247919851));
#51427=CARTESIAN_POINT('Ctrl Pts',(148.936588082219,-4.17604115720661,337.601669714844));
#51428=CARTESIAN_POINT('Ctrl Pts',(148.928841003841,-4.10179529050457,337.717220969504));
#51429=CARTESIAN_POINT('Ctrl Pts',(148.921093925463,-4.02284852288737,337.829465112774));
#51430=CARTESIAN_POINT('Ctrl Pts',(148.913346782157,-3.9439010936203,337.941710196758));
#51431=CARTESIAN_POINT('Ctrl Pts',(148.905599638851,-3.86025290972531,338.050647794355));
#51432=CARTESIAN_POINT('Ctrl Pts',(148.897852495546,-3.77222203952135,338.155871345136));
#51433=CARTESIAN_POINT('Ctrl Pts',(148.890103610518,-3.68417137810882,338.261118552405));
#51434=CARTESIAN_POINT('Ctrl Pts',(148.882354725489,-3.59173632047028,338.36264975157));
#51435=CARTESIAN_POINT('Ctrl Pts',(148.874605840461,-3.49527414681052,338.460092730136));
#51436=CARTESIAN_POINT('Ctrl Pts',(148.866848730687,-3.39870958720293,338.557639135686));
#51437=CARTESIAN_POINT('Ctrl Pts',(148.859091620912,-3.29810964843672,338.651088374295));
#51438=CARTESIAN_POINT('Ctrl Pts',(148.851334511137,-3.1938676916432,338.740105911706));
#51439=CARTESIAN_POINT('Ctrl Pts',(148.843573256211,-3.08957003128094,338.829171017243));
#51440=CARTESIAN_POINT('Ctrl Pts',(148.835812001285,-2.98162678240673,338.913799461767));
#51441=CARTESIAN_POINT('Ctrl Pts',(148.828050746359,-2.87046228586948,338.993698702694));
#51442=CARTESIAN_POINT('Ctrl Pts',(148.820277075954,-2.7591199623663,339.073725756368));
#51443=CARTESIAN_POINT('Ctrl Pts',(148.812503405549,-2.644546420926,339.149008274211));
#51444=CARTESIAN_POINT('Ctrl Pts',(148.804729735145,-2.52719347465679,339.219298070077));
#51445=CARTESIAN_POINT('Ctrl Pts',(148.797317930967,-2.41530333626886,339.286315859035));
#51446=CARTESIAN_POINT('Ctrl Pts',(148.78990612679,-2.30088698494053,339.348795149962));
#51447=CARTESIAN_POINT('Ctrl Pts',(148.782494322613,-2.1843530681089,339.406561554812));
#51448=CARTESIAN_POINT('Ctrl Pts',(148.774719243835,-2.06210747687777,339.46715926324));
#51449=CARTESIAN_POINT('Ctrl Pts',(148.766944165056,-1.93714517653106,339.52276191907));
#51450=CARTESIAN_POINT('Ctrl Pts',(148.759169086278,-1.80991265938974,339.573117014453));
#51451=CARTESIAN_POINT('Ctrl Pts',(148.751403575229,-1.68283670996075,339.623410144685));
#51452=CARTESIAN_POINT('Ctrl Pts',(148.74363806418,-1.55349646226297,339.668468420492));
#51453=CARTESIAN_POINT('Ctrl Pts',(148.735872553131,-1.42236260812602,339.708085351128));
#51454=CARTESIAN_POINT('Ctrl Pts',(148.728114741609,-1.29135877358727,339.747663001462));
#51455=CARTESIAN_POINT('Ctrl Pts',(148.720356930086,-1.15856524341956,339.781809930885));
#51456=CARTESIAN_POINT('Ctrl Pts',(148.712599118564,-1.02447194544925,339.810368000007));
#51457=CARTESIAN_POINT('Ctrl Pts',(148.704847145041,-0.890479556938012,
339.838904578275));
#51458=CARTESIAN_POINT('Ctrl Pts',(148.697095171518,-0.755189728278357,
339.861860586579));
#51459=CARTESIAN_POINT('Ctrl Pts',(148.689343197995,-0.619106437210259,
339.87912802475));
#51460=CARTESIAN_POINT('Ctrl Pts',(148.681594507437,-0.483080777496722,
339.896388150151));
#51461=CARTESIAN_POINT('Ctrl Pts',(148.67384581688,-0.34626271067641,339.907964447875));
#51462=CARTESIAN_POINT('Ctrl Pts',(148.666097126322,-0.20916505515901,339.913800264785));
#51463=CARTESIAN_POINT('Ctrl Pts',(148.658350047944,-0.0720959239539022,
339.919634867505));
#51464=CARTESIAN_POINT('Ctrl Pts',(148.650602969567,0.0652522899670618,
339.919731348455));
#51465=CARTESIAN_POINT('Ctrl Pts',(148.642855891189,0.202363410588895,339.914085073801));
#51466=CARTESIAN_POINT('Ctrl Pts',(148.635108747883,0.33947568033384,339.908438751826));
#51467=CARTESIAN_POINT('Ctrl Pts',(148.627361604577,0.476350462273005,339.897049594331));
#51468=CARTESIAN_POINT('Ctrl Pts',(148.619614461271,0.612473746048041,339.879965058574));
#51469=CARTESIAN_POINT('Ctrl Pts',(148.611865576243,0.74862763322711,339.86287668185));
#51470=CARTESIAN_POINT('Ctrl Pts',(148.604116691215,0.884029298289136,339.840090427594));
#51471=CARTESIAN_POINT('Ctrl Pts',(148.596367806187,1.01817239498544,339.811705314812));
#51472=CARTESIAN_POINT('Ctrl Pts',(148.588610696412,1.15245787255071,339.783290073778));
#51473=CARTESIAN_POINT('Ctrl Pts',(148.580853586638,1.28548173023891,339.749264184192));
#51474=CARTESIAN_POINT('Ctrl Pts',(148.573096476863,1.41674978077693,339.709777396138));
#51475=CARTESIAN_POINT('Ctrl Pts',(148.565335221937,1.54808797676402,339.670269507607));
#51476=CARTESIAN_POINT('Ctrl Pts',(148.557573967011,1.67766812698108,339.625295034071));
#51477=CARTESIAN_POINT('Ctrl Pts',(148.549812712084,1.80501459094619,339.575052501226));
#51478=CARTESIAN_POINT('Ctrl Pts',(148.54203904168,1.93256476775153,339.524729596702));
#51479=CARTESIAN_POINT('Ctrl Pts',(148.534265371275,2.05787376058951,339.4691219515));
#51480=CARTESIAN_POINT('Ctrl Pts',(148.52649170087,2.18048836243721,339.408475197137));
#51481=CARTESIAN_POINT('Ctrl Pts',(148.519079896693,2.2973952250702,339.350651563781));
#51482=CARTESIAN_POINT('Ctrl Pts',(148.511668092516,2.41185264666031,339.288247542365));
#51483=CARTESIAN_POINT('Ctrl Pts',(148.504256288339,2.52349283800256,339.221512401859));
#51484=CARTESIAN_POINT('Ctrl Pts',(148.496481209561,2.64060484768084,339.151506373324));
#51485=CARTESIAN_POINT('Ctrl Pts',(148.488706130782,2.75498657825241,339.076512696558));
#51486=CARTESIAN_POINT('Ctrl Pts',(148.480931052004,2.86618406786426,338.996770189994));
#51487=CARTESIAN_POINT('Ctrl Pts',(148.473165540955,2.97724472188597,338.91712581166));
#51488=CARTESIAN_POINT('Ctrl Pts',(148.465400029906,3.0851286168589,338.8327444565));
#51489=CARTESIAN_POINT('Ctrl Pts',(148.457634518857,3.18940739195331,338.743910195324));
#51490=CARTESIAN_POINT('Ctrl Pts',(148.449876707334,3.29358277433861,338.655164013577));
#51491=CARTESIAN_POINT('Ctrl Pts',(148.442118895812,3.39415985464853,338.561973963895));
#51492=CARTESIAN_POINT('Ctrl Pts',(148.43436108429,3.49074052203594,338.46466645874));
#51493=CARTESIAN_POINT('Ctrl Pts',(148.426609110767,3.58724850940835,338.367432180568));
#51494=CARTESIAN_POINT('Ctrl Pts',(148.418857137244,3.67976579575248,338.266086890675));
#51495=CARTESIAN_POINT('Ctrl Pts',(148.411105163721,3.76792883014986,338.160995949606));
#51496=CARTESIAN_POINT('Ctrl Pts',(148.403356473163,3.85605452744983,338.055949514613));
#51497=CARTESIAN_POINT('Ctrl Pts',(148.395607782606,3.9398293897504,337.947160882284));
#51498=CARTESIAN_POINT('Ctrl Pts',(148.387859092048,4.01892826075413,337.835030634299));
#51499=CARTESIAN_POINT('Ctrl Pts',(148.38011201367,4.09801067457713,337.722923715948));
#51500=CARTESIAN_POINT('Ctrl Pts',(148.372364935293,4.17241880705802,337.607476884044));
#51501=CARTESIAN_POINT('Ctrl Pts',(148.364617856915,4.2418694290466,337.489121694377));
#51502=CARTESIAN_POINT('Ctrl Pts',(148.356870713609,4.31132063309823,337.37076551278));
#51503=CARTESIAN_POINT('Ctrl Pts',(148.349123570303,4.37581404596444,337.249501261922));
#51504=CARTESIAN_POINT('Ctrl Pts',(148.341376426997,4.43511141496652,337.125786865924));
#51505=CARTESIAN_POINT('Ctrl Pts',(148.333627541969,4.49442211527608,337.002044656303));
#51506=CARTESIAN_POINT('Ctrl Pts',(148.325878656941,4.54853427825956,336.875851557831));
#51507=CARTESIAN_POINT('Ctrl Pts',(148.318129771913,4.59725715810314,336.747686952738));
#51508=CARTESIAN_POINT('Ctrl Pts',(148.310372662138,4.64603175291481,336.619386312408));
#51509=CARTESIAN_POINT('Ctrl Pts',(148.302615552364,4.68940549875342,336.489110351278));
#51510=CARTESIAN_POINT('Ctrl Pts',(148.294858442589,4.7272368905704,336.357355680332));
#51511=CARTESIAN_POINT('Ctrl Pts',(148.287097187663,4.76508849827353,336.225530603903));
#51512=CARTESIAN_POINT('Ctrl Pts',(148.279335932736,4.7973917585791,336.092225622849));
#51513=CARTESIAN_POINT('Ctrl Pts',(148.27157467781,4.82405621962199,335.957948147045));
#51514=CARTESIAN_POINT('Ctrl Pts',(148.263801007406,4.85076333511261,335.82345587104));
#51515=CARTESIAN_POINT('Ctrl Pts',(148.256027337001,4.87181356617842,335.687988378028));
#51516=CARTESIAN_POINT('Ctrl Pts',(148.248253666596,4.88716821327738,335.55205970477));
#51517=CARTESIAN_POINT('Ctrl Pts',(148.240841862419,4.90180809785978,335.422458543956));
#51518=CARTESIAN_POINT('Ctrl Pts',(148.233430058242,4.91127070330743,335.292438459569));
#51519=CARTESIAN_POINT('Ctrl Pts',(148.226018254065,4.91556661337236,335.162443627142));
#51520=CARTESIAN_POINT('Ctrl Pts',(148.218243175287,4.92007307878642,335.026077360743));
#51521=CARTESIAN_POINT('Ctrl Pts',(148.210468096508,4.91890781370885,334.889307941644));
#51522=CARTESIAN_POINT('Ctrl Pts',(148.20269301773,4.91202598084666,334.752646354409));
#51523=CARTESIAN_POINT('Ctrl Pts',(148.194927506681,4.90515261651792,334.616152937957));
#51524=CARTESIAN_POINT('Ctrl Pts',(148.187161995632,4.89257670071302,334.479767475994));
#51525=CARTESIAN_POINT('Ctrl Pts',(148.179396484583,4.87430530401293,334.344003913296));
#51526=CARTESIAN_POINT('Ctrl Pts',(148.17163867306,4.85605202345587,334.208374960565));
#51527=CARTESIAN_POINT('Ctrl Pts',(148.163880861538,4.83211455182281,334.073367064888));
#51528=CARTESIAN_POINT('Ctrl Pts',(148.156123050016,4.80255193569416,333.939491646681));
#51529=CARTESIAN_POINT('Ctrl Pts',(148.148371076493,4.77301156637163,333.805716973971));
#51530=CARTESIAN_POINT('Ctrl Pts',(148.14061910297,4.73785456227512,333.673073462562));
#51531=CARTESIAN_POINT('Ctrl Pts',(148.132867129447,4.69719142461954,333.542064547732));
#51532=CARTESIAN_POINT('Ctrl Pts',(148.125118438889,4.65654550782691,333.411111115255));
#51533=CARTESIAN_POINT('Ctrl Pts',(148.117369748332,4.61039821098941,333.281791275045));
#51534=CARTESIAN_POINT('Ctrl Pts',(148.109621057774,4.55891043105675,333.1545952357));
#51535=CARTESIAN_POINT('Ctrl Pts',(148.101873979396,4.50743336358673,333.027425660553));
#51536=CARTESIAN_POINT('Ctrl Pts',(148.094126901019,4.45061816971201,332.902379369441));
#51537=CARTESIAN_POINT('Ctrl Pts',(148.086379822641,4.38867448235786,332.779928075399));
#51538=CARTESIAN_POINT('Ctrl Pts',(148.078632679335,4.32673027585597,332.657475755097));
#51539=CARTESIAN_POINT('Ctrl Pts',(148.070885536029,4.25965766658299,332.537618824031));
#51540=CARTESIAN_POINT('Ctrl Pts',(148.063138392723,4.18771280050651,332.420805442978));
#51541=CARTESIAN_POINT('Ctrl Pts',(148.055389507695,4.11575175969674,332.303965799797));
#51542=CARTESIAN_POINT('Ctrl Pts',(148.047640622667,4.03891648732571,332.19017140097));
#51543=CARTESIAN_POINT('Ctrl Pts',(148.039891737639,3.95750688263241,332.079842069953));
#51544=CARTESIAN_POINT('Ctrl Pts',(148.032134627864,3.87601086894355,331.969395634244));
#51545=CARTESIAN_POINT('Ctrl Pts',(148.024377518089,3.78993105657182,331.862421928229));
#51546=CARTESIAN_POINT('Ctrl Pts',(148.016620408315,3.69960847978766,331.759308691223));
#51547=CARTESIAN_POINT('Ctrl Pts',(148.008859153389,3.60923763750641,331.656140353799));
#51548=CARTESIAN_POINT('Ctrl Pts',(148.001097898462,3.51461978271333,331.556836878762));
#51549=CARTESIAN_POINT('Ctrl Pts',(147.993336643536,3.41613265850166,331.461748917612));
#51550=CARTESIAN_POINT('Ctrl Pts',(147.985562973132,3.31748798698816,331.366508846713));
#51551=CARTESIAN_POINT('Ctrl Pts',(147.977789302727,3.21496196993356,331.275498024731));
#51552=CARTESIAN_POINT('Ctrl Pts',(147.970015632322,3.10896592927525,331.189027169723));
#51553=CARTESIAN_POINT('Ctrl Pts',(147.962603828145,3.00790402981133,331.106581553821));
#51554=CARTESIAN_POINT('Ctrl Pts',(147.955192023968,2.90368812576625,331.028262918812));
#51555=CARTESIAN_POINT('Ctrl Pts',(147.947780219791,2.79669746129601,330.954302733461));
#51556=CARTESIAN_POINT('Ctrl Pts',(147.940005141013,2.68446286565063,330.87671753911));
#51557=CARTESIAN_POINT('Ctrl Pts',(147.932230062234,2.56881995148624,330.803683654871));
#51558=CARTESIAN_POINT('Ctrl Pts',(147.924454983456,2.45017415259188,330.735515308449));
#51559=CARTESIAN_POINT('Ctrl Pts',(147.916689472407,2.33167435490649,330.667430847517));
#51560=CARTESIAN_POINT('Ctrl Pts',(147.908923961358,2.21017936063772,330.604200204149));
#51561=CARTESIAN_POINT('Ctrl Pts',(147.901158450309,2.08612518320945,330.54609555755));
#51562=CARTESIAN_POINT('Ctrl Pts',(147.893400638787,1.96219400585928,330.488048521877));
#51563=CARTESIAN_POINT('Ctrl Pts',(147.885642827264,1.8357090466844,330.435117533354));
#51564=CARTESIAN_POINT('Ctrl Pts',(147.877885015742,1.70713232351747,330.387529697385));
#51565=CARTESIAN_POINT('Ctrl Pts',(147.870133042219,1.57865235841213,330.339977672773));
#51566=CARTESIAN_POINT('Ctrl Pts',(147.862381068696,1.4480841276178,330.297760932452));
#51567=CARTESIAN_POINT('Ctrl Pts',(147.854629095173,1.31591077914885,330.261058991313));
#51568=CARTESIAN_POINT('Ctrl Pts',(147.846880404616,1.1837934061714,330.224372593466));
#51569=CARTESIAN_POINT('Ctrl Pts',(147.839131714058,1.05007264337058,330.193196453978));
#51570=CARTESIAN_POINT('Ctrl Pts',(147.8313830235,0.915247788187289,330.16766055117));
#51571=CARTESIAN_POINT('Ctrl Pts',(147.823635945122,0.780450984441242,330.14212996132));
#51572=CARTESIAN_POINT('Ctrl Pts',(147.815888866745,0.64455092903888,330.122237346673));
#51573=CARTESIAN_POINT('Ctrl Pts',(147.808141788367,0.508057739939603,330.10806169342));
#51574=CARTESIAN_POINT('Ctrl Pts',(147.800394645061,0.371563406896028,330.093885921361));
#51575=CARTESIAN_POINT('Ctrl Pts',(147.792647501755,0.234476319023631,330.08542724664));
#51576=CARTESIAN_POINT('Ctrl Pts',(147.784900358449,0.097311959562549,330.082712796162));
#51577=CARTESIAN_POINT('Ctrl Pts',(147.777151473421,-0.0398832373586683,
330.079997735418));
#51578=CARTESIAN_POINT('Ctrl Pts',(147.769402588393,-0.177155349716091,
330.083029476437));
#51579=CARTESIAN_POINT('Ctrl Pts',(147.761653703365,-0.313989046323042,
330.091783018112));
#51580=CARTESIAN_POINT('Ctrl Pts',(147.75389659359,-0.450967979629376,330.100545850887));
#51581=CARTESIAN_POINT('Ctrl Pts',(147.746139483816,-0.587507176933875,
330.115042591069));
#51582=CARTESIAN_POINT('Ctrl Pts',(147.738382374041,-0.723096026763421,
330.135196283653));
#51583=CARTESIAN_POINT('Ctrl Pts',(147.730621119115,-0.858757330939025,
330.155360745727));
#51584=CARTESIAN_POINT('Ctrl Pts',(147.722859864189,-0.993466892044418,
330.181188110031));
#51585=CARTESIAN_POINT('Ctrl Pts',(147.715098609262,-1.12672542128919,330.212550481987));
#51586=CARTESIAN_POINT('Ctrl Pts',(147.707324938858,-1.26019712075186,330.243963023517));
#51587=CARTESIAN_POINT('Ctrl Pts',(147.699551268453,-1.39221277335739,330.280928160581));
#51588=CARTESIAN_POINT('Ctrl Pts',(147.691777598048,-1.52228849975986,330.323268151155));
#51589=CARTESIAN_POINT('Ctrl Pts',(147.684365793871,-1.6463091698045,330.363637204982));
#51590=CARTESIAN_POINT('Ctrl Pts',(147.676953989694,-1.76856618642563,330.408891874718));
#51591=CARTESIAN_POINT('Ctrl Pts',(147.669542185517,-1.8886596718276,330.458838506889));
#51592=CARTESIAN_POINT('Ctrl Pts',(147.661767106739,-2.01463929668861,330.511233172287));
#51593=CARTESIAN_POINT('Ctrl Pts',(147.65399202796,-2.13863606449778,330.568956940496));
#51594=CARTESIAN_POINT('Ctrl Pts',(147.646216949182,-2.26016633098809,330.631838920236));
#51595=CARTESIAN_POINT('Ctrl Pts',(147.638451438133,-2.38154704674857,330.694643519696));
#51596=CARTESIAN_POINT('Ctrl Pts',(147.630685927084,-2.50046695650412,330.762593523059));
#51597=CARTESIAN_POINT('Ctrl Pts',(147.622920416035,-2.61646122707147,330.835469569119));
#51598=CARTESIAN_POINT('Ctrl Pts',(147.615162604513,-2.73234048898173,330.908273358368));
#51599=CARTESIAN_POINT('Ctrl Pts',(147.60740479299,-2.84529955557861,330.985993263907));
#51600=CARTESIAN_POINT('Ctrl Pts',(147.599646981468,-2.95489742472289,331.068363664851));
#51601=CARTESIAN_POINT('Ctrl Pts',(147.591895007945,-3.06441281799505,331.150672079455));
#51602=CARTESIAN_POINT('Ctrl Pts',(147.584143034422,-3.17057173727117,331.237623789698));
#51603=CARTESIAN_POINT('Ctrl Pts',(147.576391060899,-3.27296176553896,331.328909651913));
#51604=CARTESIAN_POINT('Ctrl Pts',(147.568642370342,-3.37530843156909,331.42015685451));
#51605=CARTESIAN_POINT('Ctrl Pts',(147.560893679784,-3.47388909002619,331.515734298793));
#51606=CARTESIAN_POINT('Ctrl Pts',(147.553144989226,-3.56832424087003,331.61529245362));
#51607=CARTESIAN_POINT('Ctrl Pts',(147.545397910849,-3.66273974369194,331.714829894542));
#51608=CARTESIAN_POINT('Ctrl Pts',(147.537650832471,-3.75301118566073,331.818346115207));
#51609=CARTESIAN_POINT('Ctrl Pts',(147.529903754093,-3.8387960915049,331.925454890501));
#51610=CARTESIAN_POINT('Ctrl Pts',(147.522156610787,-3.9245817163092,332.032564563469));
#51611=CARTESIAN_POINT('Ctrl Pts',(147.514409467481,-4.00588048564268,332.143266546036));
#51612=CARTESIAN_POINT('Ctrl Pts',(147.506662324176,-4.08239063035362,332.257142037272));
#51613=CARTESIAN_POINT('Ctrl Pts',(147.498913439147,-4.15891797616937,332.371043130135));
#51614=CARTESIAN_POINT('Ctrl Pts',(147.491164554119,-4.23065433713573,332.488118827016));
#51615=CARTESIAN_POINT('Ctrl Pts',(147.483415669091,-4.29734186194209,332.60792224539));
#51616=CARTESIAN_POINT('Ctrl Pts',(147.475658559317,-4.36410016957633,332.727852824351));
#51617=CARTESIAN_POINT('Ctrl Pts',(147.467901449542,-4.42579874576242,332.850516566235));
#51618=CARTESIAN_POINT('Ctrl Pts',(147.460144339767,-4.48222598243681,332.975442442194));
#51619=CARTESIAN_POINT('Ctrl Pts',(147.452383084841,-4.53868337202223,333.100435074547));
#51620=CARTESIAN_POINT('Ctrl Pts',(147.444621829915,-4.58986366352323,333.227691887182));
#51621=CARTESIAN_POINT('Ctrl Pts',(147.436860574989,-4.63560421240568,333.356723806408));
#51622=CARTESIAN_POINT('Ctrl Pts',(147.429086904584,-4.68141793125959,333.485962134653));
#51623=CARTESIAN_POINT('Ctrl Pts',(147.421313234179,-4.72177440356769,333.616980870084));
#51624=CARTESIAN_POINT('Ctrl Pts',(147.413539563775,-4.75656124150922,333.749276921828));
#51625=CARTESIAN_POINT('Ctrl Pts',(147.406127759598,-4.78972874377483,333.875414560533));
#51626=CARTESIAN_POINT('Ctrl Pts',(147.398715955421,-4.81783341332766,334.002712992552));
#51627=CARTESIAN_POINT('Ctrl Pts',(147.391304151244,-4.84082170068331,334.130731155112));
#51628=CARTESIAN_POINT('Ctrl Pts',(147.379424478014,-4.87766743154478,334.335919244597));
#51629=CARTESIAN_POINT('Ctrl Pts',(147.367544804784,-4.9014749885021,334.54351405225));
#51630=CARTESIAN_POINT('Ctrl Pts',(147.355665131553,-4.91200260903515,334.752182665393));
#51631=CARTESIAN_POINT('Ctrl Pts',(147.351049213205,-4.91609317919156,334.833262107687));
#51632=CARTESIAN_POINT('Ctrl Pts',(147.346433294857,-4.91817922566193,334.914503377089));
#51633=CARTESIAN_POINT('Ctrl Pts',(147.341817376508,-4.9182482295019,334.995826811598));
#51634=CARTESIAN_POINT('',(145.591817376546,-4.91824992125433,334.999119896715));
#51635=CARTESIAN_POINT('Ctrl Pts',(147.341817376463,-4.91824822950257,334.995826812387));
#51636=CARTESIAN_POINT('Ctrl Pts',(147.334169792718,-4.91836255399992,335.13056224939));
#51637=CARTESIAN_POINT('Ctrl Pts',(147.326522208973,-4.91293610271415,335.265491128996));
#51638=CARTESIAN_POINT('Ctrl Pts',(147.318874625228,-4.90194789167757,335.400112396431));
#51639=CARTESIAN_POINT('Ctrl Pts',(147.311234006876,-4.8909696886645,335.534611051295));
#51640=CARTESIAN_POINT('Ctrl Pts',(147.303593388523,-4.87443983411927,335.668802251474));
#51641=CARTESIAN_POINT('Ctrl Pts',(147.29595277017,-4.85238939625965,335.80218464805));
#51642=CARTESIAN_POINT('Ctrl Pts',(147.288316847756,-4.83035251064086,335.935485067552));
#51643=CARTESIAN_POINT('Ctrl Pts',(147.280680925341,-4.80280185530966,336.067977275241));
#51644=CARTESIAN_POINT('Ctrl Pts',(147.273045002927,-4.76982031462235,336.199165221609));
#51645=CARTESIAN_POINT('Ctrl Pts',(147.265411530115,-4.73684935440743,336.330311082906));
#51646=CARTESIAN_POINT('Ctrl Pts',(147.257778057303,-4.69845107032931,336.460153123703));
#51647=CARTESIAN_POINT('Ctrl Pts',(147.250144584491,-4.65475932115117,336.588206134183));
#51648=CARTESIAN_POINT('Ctrl Pts',(147.242511794147,-4.61107147821453,336.71624769614));
#51649=CARTESIAN_POINT('Ctrl Pts',(147.234879003802,-4.56209124152275,336.842500163918));
#51650=CARTESIAN_POINT('Ctrl Pts',(147.227246213458,-4.50800197027956,336.966494672878));
#51651=CARTESIAN_POINT('Ctrl Pts',(147.219612339209,-4.45390501802296,337.09050678983));
#51652=CARTESIAN_POINT('Ctrl Pts',(147.211978464961,-4.39469775039546,337.212259940699));
#51653=CARTESIAN_POINT('Ctrl Pts',(147.204344590713,-4.33061094379842,337.331306911574));
#51654=CARTESIAN_POINT('Ctrl Pts',(147.196703192206,-4.26646097062505,337.45047122001));
#51655=CARTESIAN_POINT('Ctrl Pts',(147.189061793699,-4.1974220439605,337.566923664982));
#51656=CARTESIAN_POINT('Ctrl Pts',(147.181420395192,-4.12377021101172,337.680242957135));
#51657=CARTESIAN_POINT('Ctrl Pts',(147.173775272607,-4.05008248343362,337.793617476074));
#51658=CARTESIAN_POINT('Ctrl Pts',(147.166130150023,-3.97177760672654,337.903855472973));
#51659=CARTESIAN_POINT('Ctrl Pts',(147.158485027438,-3.88917315145926,338.010567265561));
#51660=CARTESIAN_POINT('Ctrl Pts',(147.150827780779,-3.80643769731258,338.117448287826));
#51661=CARTESIAN_POINT('Ctrl Pts',(147.143170534121,-3.71938930263166,338.220791625409));
#51662=CARTESIAN_POINT('Ctrl Pts',(147.135513287463,-3.62838423958904,338.320242592402));
#51663=CARTESIAN_POINT('Ctrl Pts',(147.128030897298,-3.53945731598285,338.417422554139));
#51664=CARTESIAN_POINT('Ctrl Pts',(147.120548507134,-3.44675278395714,338.510885810321));
#51665=CARTESIAN_POINT('Ctrl Pts',(147.113066116969,-3.3506331052346,338.600338991901));
#51666=CARTESIAN_POINT('Ctrl Pts',(147.105291038191,-3.25075351357949,338.693291313083));
#51667=CARTESIAN_POINT('Ctrl Pts',(147.097515959413,-3.14684517639639,338.782231120297));
#51668=CARTESIAN_POINT('Ctrl Pts',(147.089740880634,-3.03926400149785,338.8667890286));
#51669=CARTESIAN_POINT('Ctrl Pts',(147.081975369585,-2.93181521208375,338.951242883014));
#51670=CARTESIAN_POINT('Ctrl Pts',(147.074209858536,-2.82070288215537,339.031325328226));
#51671=CARTESIAN_POINT('Ctrl Pts',(147.066444347487,-2.70631924063376,339.106704181004));
#51672=CARTESIAN_POINT('Ctrl Pts',(147.058686535965,-2.59204901082594,339.18200829543));
#51673=CARTESIAN_POINT('Ctrl Pts',(147.050928724443,-2.47451424847793,339.252617884604));
#51674=CARTESIAN_POINT('Ctrl Pts',(147.043170912921,-2.35413941223203,339.318241620182));
#51675=CARTESIAN_POINT('Ctrl Pts',(147.035418939398,-2.2338551618677,339.383815971819));
#51676=CARTESIAN_POINT('Ctrl Pts',(147.027666965875,-2.11073543349573,339.444411751719));
#51677=CARTESIAN_POINT('Ctrl Pts',(147.019914992352,-1.98523245490647,339.499781679425));
#51678=CARTESIAN_POINT('Ctrl Pts',(147.012166301794,-1.85978262690325,339.555128157933));
#51679=CARTESIAN_POINT('Ctrl Pts',(147.004417611236,-1.73195191299756,339.605253028605));
#51680=CARTESIAN_POINT('Ctrl Pts',(146.996668920679,-1.602215661884,339.649955702511));
#51681=CARTESIAN_POINT('Ctrl Pts',(146.988921842301,-1.47250640348097,339.694649075653));
#51682=CARTESIAN_POINT('Ctrl Pts',(146.981174763923,-1.34089276578264,339.733922368712));
#51683=CARTESIAN_POINT('Ctrl Pts',(146.973427685545,-1.20786815492982,339.767623892759));
#51684=CARTESIAN_POINT('Ctrl Pts',(146.965680542239,-1.0748424292029,339.801325699258));
#51685=CARTESIAN_POINT('Ctrl Pts',(146.957933398934,-0.9404060856384,339.82945554761));
#51686=CARTESIAN_POINT('Ctrl Pts',(146.950186255628,-0.805065314541873,
339.851912293294));
#51687=CARTESIAN_POINT('Ctrl Pts',(146.9424373706,-0.669694115966915,339.874374087732));
#51688=CARTESIAN_POINT('Ctrl Pts',(146.934688485572,-0.533418470773759,
339.891160177561));
#51689=CARTESIAN_POINT('Ctrl Pts',(146.926939600544,-0.396751932446336,
339.902221023842));
#51690=CARTESIAN_POINT('Ctrl Pts',(146.919182490769,-0.259940334842683,
339.91329361022));
#51691=CARTESIAN_POINT('Ctrl Pts',(146.911425380994,-0.122737405522813,
339.918628782426));
#51692=CARTESIAN_POINT('Ctrl Pts',(146.90366827122,0.0143404839101443,339.918229093182));
#51693=CARTESIAN_POINT('Ctrl Pts',(146.895907016293,0.1514916233845,339.917829190357));
#51694=CARTESIAN_POINT('Ctrl Pts',(146.888145761367,0.288517199548139,339.911688337227));
#51695=CARTESIAN_POINT('Ctrl Pts',(146.880384506441,0.424904702899062,339.899861126191));
#51696=CARTESIAN_POINT('Ctrl Pts',(146.872610836036,0.561510381806624,339.888014995471));
#51697=CARTESIAN_POINT('Ctrl Pts',(146.864837165632,0.697475560361569,339.870464379769));
#51698=CARTESIAN_POINT('Ctrl Pts',(146.857063495227,0.832295792667097,339.847315419488));
#51699=CARTESIAN_POINT('Ctrl Pts',(146.84965169105,0.960840110722838,339.825244048878));
#51700=CARTESIAN_POINT('Ctrl Pts',(146.842239886873,1.08834339670137,339.798083870115));
#51701=CARTESIAN_POINT('Ctrl Pts',(146.834828082696,1.2143820356245,339.76596887674));
#51702=CARTESIAN_POINT('Ctrl Pts',(146.827053003917,1.34659820369113,339.732279831874));
#51703=CARTESIAN_POINT('Ctrl Pts',(146.819277925139,1.47762034853376,339.693031527398));
#51704=CARTESIAN_POINT('Ctrl Pts',(146.81150284636,1.60694524433394,339.648323358396));
#51705=CARTESIAN_POINT('Ctrl Pts',(146.803737335311,1.73611099761656,339.603670205643));
#51706=CARTESIAN_POINT('Ctrl Pts',(146.795971824262,1.86358329162759,339.553570683163));
#51707=CARTESIAN_POINT('Ctrl Pts',(146.788206313213,1.9888705288252,339.498174861215));
#51708=CARTESIAN_POINT('Ctrl Pts',(146.780448501691,2.11403354336215,339.442833964387));
#51709=CARTESIAN_POINT('Ctrl Pts',(146.772690690169,2.23701545733739,339.382207375514));
#51710=CARTESIAN_POINT('Ctrl Pts',(146.764932878647,2.35734158760555,339.316494376441));
#51711=CARTESIAN_POINT('Ctrl Pts',(146.757180905124,2.4775771686453,339.250830828484));
#51712=CARTESIAN_POINT('Ctrl Pts',(146.749428931601,2.59516060234791,339.18008867574));
#51713=CARTESIAN_POINT('Ctrl Pts',(146.741676958078,2.70963921889573,339.104514388563));
#51714=CARTESIAN_POINT('Ctrl Pts',(146.73392826752,2.82406935368132,339.028972107142));
#51715=CARTESIAN_POINT('Ctrl Pts',(146.726179576962,2.93539696101511,338.948601976354));
#51716=CARTESIAN_POINT('Ctrl Pts',(146.718430886405,3.0431961229348,338.863695176881));
#51717=CARTESIAN_POINT('Ctrl Pts',(146.710683808027,3.15097285633847,338.778806042977));
#51718=CARTESIAN_POINT('Ctrl Pts',(146.702936729649,3.25522229767815,338.689382359558));
#51719=CARTESIAN_POINT('Ctrl Pts',(146.695189651271,3.35554987812313,338.595756954791));
#51720=CARTESIAN_POINT('Ctrl Pts',(146.687442507965,3.4558782994101,338.502130765353));
#51721=CARTESIAN_POINT('Ctrl Pts',(146.679695364659,3.55228450847258,338.40430305101));
#51722=CARTESIAN_POINT('Ctrl Pts',(146.671948221354,3.64440952210466,338.302644742883));
#51723=CARTESIAN_POINT('Ctrl Pts',(146.664199336325,3.73655524739532,338.200963579811));
#51724=CARTESIAN_POINT('Ctrl Pts',(146.656450451297,3.82441759955697,338.095450398846));
#51725=CARTESIAN_POINT('Ctrl Pts',(146.648701566269,3.90767700698123,337.986510249708));
#51726=CARTESIAN_POINT('Ctrl Pts',(146.640944456495,3.99102478680095,337.877454470369));
#51727=CARTESIAN_POINT('Ctrl Pts',(146.63318734672,4.06975962468716,337.764964767821));
#51728=CARTESIAN_POINT('Ctrl Pts',(146.625430236945,4.14360422897478,337.649476751384));
#51729=CARTESIAN_POINT('Ctrl Pts',(146.617668982019,4.21748829345771,337.533927021844));
#51730=CARTESIAN_POINT('Ctrl Pts',(146.609907727093,4.28647672083974,337.415376123545));
#51731=CARTESIAN_POINT('Ctrl Pts',(146.602146472166,4.35033807073274,337.29428457974));
#51732=CARTESIAN_POINT('Ctrl Pts',(146.594372801762,4.41430157797325,337.172999328929));
#51733=CARTESIAN_POINT('Ctrl Pts',(146.586599131357,4.47312145060014,337.049165664382));
#51734=CARTESIAN_POINT('Ctrl Pts',(146.578825460952,4.52661395972237,336.923265224078));
#51735=CARTESIAN_POINT('Ctrl Pts',(146.571413656775,4.57761637967503,336.80322547956));
#51736=CARTESIAN_POINT('Ctrl Pts',(146.564001852598,4.623776150096,336.681307315039));
#51737=CARTESIAN_POINT('Ctrl Pts',(146.556590048421,4.6649767066401,336.55793946898));
#51738=CARTESIAN_POINT('Ctrl Pts',(146.548814969643,4.70819662519083,336.42852499729));
#51739=CARTESIAN_POINT('Ctrl Pts',(146.541039890864,4.74609548925451,336.297106170838));
#51740=CARTESIAN_POINT('Ctrl Pts',(146.533264812086,4.77848455791275,336.164159951334));
#51741=CARTESIAN_POINT('Ctrl Pts',(146.525499301037,4.81083376975999,336.031377330616));
#51742=CARTESIAN_POINT('Ctrl Pts',(146.517733789988,4.8376865851279,335.897071432756));
#51743=CARTESIAN_POINT('Ctrl Pts',(146.509968278939,4.85890316966208,335.761736864244));
#51744=CARTESIAN_POINT('Ctrl Pts',(146.502210467417,4.88009871789099,335.626536480349));
#51745=CARTESIAN_POINT('Ctrl Pts',(146.494452655895,4.89566909624876,335.490309839191));
#51746=CARTESIAN_POINT('Ctrl Pts',(146.486694844372,4.90552500680314,335.353563954793));
#51747=CARTESIAN_POINT('Ctrl Pts',(146.478942870849,4.91537350047228,335.21692097601));
#51748=CARTESIAN_POINT('Ctrl Pts',(146.471190897326,4.91951605792517,335.079759920044));
#51749=CARTESIAN_POINT('Ctrl Pts',(146.463438923803,4.91791497572711,334.942594825851));
#51750=CARTESIAN_POINT('Ctrl Pts',(146.455690233246,4.91631457158831,334.805487821158));
#51751=CARTESIAN_POINT('Ctrl Pts',(146.447941542688,4.90897537029277,334.668377171675));
#51752=CARTESIAN_POINT('Ctrl Pts',(146.440192852131,4.89591174323791,334.531778615477));
#51753=CARTESIAN_POINT('Ctrl Pts',(146.432445773753,4.88285083417977,334.395208479749));
#51754=CARTESIAN_POINT('Ctrl Pts',(146.424698695375,4.86406790556275,334.259150614234));
#51755=CARTESIAN_POINT('Ctrl Pts',(146.416951616997,4.83962931585833,334.124116932699));
#51756=CARTESIAN_POINT('Ctrl Pts',(146.409204473691,4.81519052133499,333.989082119452));
#51757=CARTESIAN_POINT('Ctrl Pts',(146.401457330386,4.78509604079177,333.855071891931));
#51758=CARTESIAN_POINT('Ctrl Pts',(146.39371018708,4.74946353171188,333.722588858887));
#51759=CARTESIAN_POINT('Ctrl Pts',(146.385961302052,4.71382301168763,333.590076040846));
#51760=CARTESIAN_POINT('Ctrl Pts',(146.378212417024,4.67264208708522,333.459091477888));
#51761=CARTESIAN_POINT('Ctrl Pts',(146.370463531996,4.62608843431994,333.33012310024));
#51762=CARTESIAN_POINT('Ctrl Pts',(146.362706422221,4.57948536902639,333.201017834224));
#51763=CARTESIAN_POINT('Ctrl Pts',(146.354949312446,4.52749831687509,333.073933396604));
#51764=CARTESIAN_POINT('Ctrl Pts',(146.347192202672,4.47034353260724,332.949338701058));
#51765=CARTESIAN_POINT('Ctrl Pts',(146.339430947746,4.41315820665017,332.824677426091));
#51766=CARTESIAN_POINT('Ctrl Pts',(146.331669692819,4.35079982371003,332.702508892184));
#51767=CARTESIAN_POINT('Ctrl Pts',(146.323908437893,4.2835304019407,332.583276938052));
#51768=CARTESIAN_POINT('Ctrl Pts',(146.316134767489,4.21615337101961,332.463854251652));
#51769=CARTESIAN_POINT('Ctrl Pts',(146.308361097084,4.1438498087889,332.347377864433));
#51770=CARTESIAN_POINT('Ctrl Pts',(146.300587426679,4.06692530865479,332.234262919885));
#51771=CARTESIAN_POINT('Ctrl Pts',(146.293175622502,3.99358166250822,332.126413503219));
#51772=CARTESIAN_POINT('Ctrl Pts',(146.285763818325,3.91603777737317,332.021619853009));
#51773=CARTESIAN_POINT('Ctrl Pts',(146.278352014148,3.83459110891659,331.920212005686));
#51774=CARTESIAN_POINT('Ctrl Pts',(146.27057693537,3.74915249662236,331.813833857688));
#51775=CARTESIAN_POINT('Ctrl Pts',(146.262801856591,3.65914885174212,331.710845626556));
#51776=CARTESIAN_POINT('Ctrl Pts',(146.255026777813,3.56487912301256,331.611664139904));
#51777=CARTESIAN_POINT('Ctrl Pts',(146.247261266764,3.47072539918574,331.512604702386));
#51778=CARTESIAN_POINT('Ctrl Pts',(146.239495755715,3.37231630359424,331.417342969261));
#51779=CARTESIAN_POINT('Ctrl Pts',(146.231730244666,3.26999208899414,331.326264190172));
#51780=CARTESIAN_POINT('Ctrl Pts',(146.223972433143,3.16776932915076,331.235275715957));
#51781=CARTESIAN_POINT('Ctrl Pts',(146.216214621621,3.06163946549021,331.148462200403));
#51782=CARTESIAN_POINT('Ctrl Pts',(146.208456810099,2.95198053268774,331.066173110426));
#51783=CARTESIAN_POINT('Ctrl Pts',(146.200704836576,2.84240412170976,330.9839459456));
#51784=CARTESIAN_POINT('Ctrl Pts',(146.192952863053,2.72930423908257,330.906236662977));
#51785=CARTESIAN_POINT('Ctrl Pts',(146.18520088953,2.61309274763999,330.833355144156));
#51786=CARTESIAN_POINT('Ctrl Pts',(146.177452198972,2.49693047183283,330.760504490701));
#51787=CARTESIAN_POINT('Ctrl Pts',(146.169703508415,2.37765953861018,330.692477741803));
#51788=CARTESIAN_POINT('Ctrl Pts',(146.161954817857,2.25572142030991,330.629541907711));
#51789=CARTESIAN_POINT('Ctrl Pts',(146.154207739479,2.13380867225376,330.566619167945));
#51790=CARTESIAN_POINT('Ctrl Pts',(146.146460661101,2.00923019003613,330.508785415307));
#51791=CARTESIAN_POINT('Ctrl Pts',(146.138713582724,1.88245236324088,330.456261873454));
#51792=CARTESIAN_POINT('Ctrl Pts',(146.130966439418,1.75567347392478,330.403737891403));
#51793=CARTESIAN_POINT('Ctrl Pts',(146.123219296112,1.62669556437602,330.356524358513));
#51794=CARTESIAN_POINT('Ctrl Pts',(146.115472152806,1.49600496023121,330.314794324529));
#51795=CARTESIAN_POINT('Ctrl Pts',(146.107723267778,1.36528497406453,330.273054908748));
#51796=CARTESIAN_POINT('Ctrl Pts',(146.09997438275,1.23285189937561,330.236801563894));
#51797=CARTESIAN_POINT('Ctrl Pts',(146.092225497722,1.09920678643203,330.206157334334));
#51798=CARTESIAN_POINT('Ctrl Pts',(146.084468387947,0.965419821184767,330.175480578672));
#51799=CARTESIAN_POINT('Ctrl Pts',(146.076711278172,0.830418629427339,330.150424918622));
#51800=CARTESIAN_POINT('Ctrl Pts',(146.068954168397,0.694714558523137,330.131062257055));
#51801=CARTESIAN_POINT('Ctrl Pts',(146.061192913471,0.55893797170251,330.1116892487));
#51802=CARTESIAN_POINT('Ctrl Pts',(146.053431658545,0.422458146055808,330.098015339546));
#51803=CARTESIAN_POINT('Ctrl Pts',(146.045670403619,0.285790108086479,330.090060379534));
#51804=CARTESIAN_POINT('Ctrl Pts',(146.037896733214,0.148903445796363,330.082092694178));
#51805=CARTESIAN_POINT('Ctrl Pts',(146.03012306281,0.0118283605679736,330.079862245649));
#51806=CARTESIAN_POINT('Ctrl Pts',(146.022349392405,-0.124920670453566,
330.083336711896));
#51807=CARTESIAN_POINT('Ctrl Pts',(146.014937588228,-0.255304001179753,
330.086649440902));
#51808=CARTESIAN_POINT('Ctrl Pts',(146.007525784051,-0.385390663026766,
330.095147891052));
#51809=CARTESIAN_POINT('Ctrl Pts',(146.000113979874,-0.514742150990681,
330.108760527178));
#51810=CARTESIAN_POINT('Ctrl Pts',(145.992338901095,-0.650433540699215,
330.12304035915));
#51811=CARTESIAN_POINT('Ctrl Pts',(145.984563822317,-0.785744678068278,
330.142993502945));
#51812=CARTESIAN_POINT('Ctrl Pts',(145.976788743539,-0.920163265549295,
330.16859413553));
#51813=CARTESIAN_POINT('Ctrl Pts',(145.96902323249,-1.05441644240055,330.194163264907));
#51814=CARTESIAN_POINT('Ctrl Pts',(145.961257721441,-1.18777887444255,330.225365982945));
#51815=CARTESIAN_POINT('Ctrl Pts',(145.953492210392,-1.31974246674086,330.262124644529));
#51816=CARTESIAN_POINT('Ctrl Pts',(145.945734398869,-1.4515752167533,330.298846859793));
#51817=CARTESIAN_POINT('Ctrl Pts',(145.937976587347,-1.5820115130247,330.341113951702));
#51818=CARTESIAN_POINT('Ctrl Pts',(145.930218775825,-1.71055290511402,330.388797139432));
#51819=CARTESIAN_POINT('Ctrl Pts',(145.922466802302,-1.83899756572923,330.436444444052));
#51820=CARTESIAN_POINT('Ctrl Pts',(145.914714828779,-1.96554979550052,330.489499596449));
#51821=CARTESIAN_POINT('Ctrl Pts',(145.906962855256,-2.08972612576906,330.547783947091));
#51822=CARTESIAN_POINT('Ctrl Pts',(145.899214164699,-2.21384986728844,330.606043614277));
#51823=CARTESIAN_POINT('Ctrl Pts',(145.891465474141,-2.33559935745553,330.669527909354));
#51824=CARTESIAN_POINT('Ctrl Pts',(145.883716783583,-2.45451115564039,330.738010083384));
#51825=CARTESIAN_POINT('Ctrl Pts',(145.875969705206,-2.57339821323243,330.806478009125));
#51826=CARTESIAN_POINT('Ctrl Pts',(145.868222626828,-2.68944841469473,330.879941550535));
#51827=CARTESIAN_POINT('Ctrl Pts',(145.86047554845,-2.80222333816824,330.958128227476));
#51828=CARTESIAN_POINT('Ctrl Pts',(145.852728405144,-2.9149992068047,331.036315559698));
#51829=CARTESIAN_POINT('Ctrl Pts',(145.844981261838,-3.02449942147651,331.119225883701));
#51830=CARTESIAN_POINT('Ctrl Pts',(145.837234118532,-3.13031528225225,331.206543885031));
#51831=CARTESIAN_POINT('Ctrl Pts',(145.829485233504,-3.2361549326792,331.2938815173));
#51832=CARTESIAN_POINT('Ctrl Pts',(145.821736348476,-3.3383082795207,331.385628550024));
#51833=CARTESIAN_POINT('Ctrl Pts',(145.813987463448,-3.43640070509199,331.481430225711));
#51834=CARTESIAN_POINT('Ctrl Pts',(145.806230353673,-3.53459724697764,331.577333586286));
#51835=CARTESIAN_POINT('Ctrl Pts',(145.798473243899,-3.62872397727944,331.677299913212));
#51836=CARTESIAN_POINT('Ctrl Pts',(145.790716134124,-3.71844371193972,331.780938114351));
#51837=CARTESIAN_POINT('Ctrl Pts',(145.782954879198,-3.80821138995743,331.884631696431));
#51838=CARTESIAN_POINT('Ctrl Pts',(145.775193624272,-3.89356713675331,331.992000756635));
#51839=CARTESIAN_POINT('Ctrl Pts',(145.767432369345,-3.9742155496948,332.102622940129));
#51840=CARTESIAN_POINT('Ctrl Pts',(145.759658698941,-4.05499297381374,332.213422083066));
#51841=CARTESIAN_POINT('Ctrl Pts',(145.751885028536,-4.13104779955029,332.327484422921));
#51842=CARTESIAN_POINT('Ctrl Pts',(145.744111358131,-4.20212879410281,332.44435983357));
#51843=CARTESIAN_POINT('Ctrl Pts',(145.736699553954,-4.2699009512586,332.555794665736));
#51844=CARTESIAN_POINT('Ctrl Pts',(145.729287749777,-4.33315178031912,332.669786313979));
#51845=CARTESIAN_POINT('Ctrl Pts',(145.7218759456,-4.39170413651322,332.785927318304));
#51846=CARTESIAN_POINT('Ctrl Pts',(145.713571284239,-4.45730995642682,332.916059157731));
#51847=CARTESIAN_POINT('Ctrl Pts',(145.705266622878,-4.51720247461374,333.049256694741));
#51848=CARTESIAN_POINT('Ctrl Pts',(145.696961961517,-4.5711045508882,333.185010675693));
#51849=CARTESIAN_POINT('Ctrl Pts',(145.688673606317,-4.62490079070571,333.320498104383));
#51850=CARTESIAN_POINT('Ctrl Pts',(145.680385251117,-4.67272992078372,333.458531684975));
#51851=CARTESIAN_POINT('Ctrl Pts',(145.672096895917,-4.71436127248231,333.598578987235));
#51852=CARTESIAN_POINT('Ctrl Pts',(145.663831156675,-4.75587902710266,333.738244150466));
#51853=CARTESIAN_POINT('Ctrl Pts',(145.655565417434,-4.79123264186159,333.879911781521));
#51854=CARTESIAN_POINT('Ctrl Pts',(145.647299678193,-4.82024026447434,334.023031804386));
#51855=CARTESIAN_POINT('Ctrl Pts',(145.639048009204,-4.84919850922091,334.165908202966));
#51856=CARTESIAN_POINT('Ctrl Pts',(145.630796340215,-4.87183222725879,334.310231764971));
#51857=CARTESIAN_POINT('Ctrl Pts',(145.622544671226,-4.88800928385938,334.455437511938));
#51858=CARTESIAN_POINT('Ctrl Pts',(145.614311813416,-4.9041494619198,334.600312236018));
#51859=CARTESIAN_POINT('Ctrl Pts',(145.606078955605,-4.91386229371922,334.746064828373));
#51860=CARTESIAN_POINT('Ctrl Pts',(145.597846097795,-4.91706672384905,334.892120920859));
#51861=CARTESIAN_POINT('Ctrl Pts',(145.595836524046,-4.91784889922728,334.927772027219));
#51862=CARTESIAN_POINT('Ctrl Pts',(145.593826950296,-4.91824353667277,334.963441166378));
#51863=CARTESIAN_POINT('Ctrl Pts',(145.591817376546,-4.91824992125433,334.999119896715));
#51864=CARTESIAN_POINT('',(143.841817376479,-4.91824791238371,335.004531537633));
#51865=CARTESIAN_POINT('Ctrl Pts',(145.591817376508,-4.91824992125445,334.999119897395));
#51866=CARTESIAN_POINT('Ctrl Pts',(145.583803417168,-4.91827538224464,335.141402754277));
#51867=CARTESIAN_POINT('Ctrl Pts',(145.575789457829,-4.91212223074461,335.283602918125));
#51868=CARTESIAN_POINT('Ctrl Pts',(145.567775498489,-4.89983804479466,335.425170786018));
#51869=CARTESIAN_POINT('Ctrl Pts',(145.559754410428,-4.88754293159453,335.566864583908));
#51870=CARTESIAN_POINT('Ctrl Pts',(145.551733322367,-4.8691059386561,335.707924614929));
#51871=CARTESIAN_POINT('Ctrl Pts',(145.543712234306,-4.84462623023812,335.847808794357));
#51872=CARTESIAN_POINT('Ctrl Pts',(145.535372707391,-4.8191746723359,335.993246404623));
#51873=CARTESIAN_POINT('Ctrl Pts',(145.527033180476,-4.78719084347461,336.137412462189));
#51874=CARTESIAN_POINT('Ctrl Pts',(145.518693653561,-4.74884357895388,336.27971392316));
#51875=CARTESIAN_POINT('Ctrl Pts',(145.51064889121,-4.71185171681918,336.416985671003));
#51876=CARTESIAN_POINT('Ctrl Pts',(145.502604128858,-4.66893876593736,336.552522083412));
#51877=CARTESIAN_POINT('Ctrl Pts',(145.494559366506,-4.62030584446402,336.685810477519));
#51878=CARTESIAN_POINT('Ctrl Pts',(145.486505755188,-4.57161942842521,336.819245484342));
#51879=CARTESIAN_POINT('Ctrl Pts',(145.478452143871,-4.51720062509598,336.950427217436));
#51880=CARTESIAN_POINT('Ctrl Pts',(145.470398532553,-4.45729755886688,337.078865443991));
#51881=CARTESIAN_POINT('Ctrl Pts',(145.462330474305,-4.39728703582481,337.20753406881));
#51882=CARTESIAN_POINT('Ctrl Pts',(145.454262416057,-4.33177275744791,337.333449045181));
#51883=CARTESIAN_POINT('Ctrl Pts',(145.44619435781,-4.26104785800794,337.456146211907));
#51884=CARTESIAN_POINT('Ctrl Pts',(145.445342208982,-4.25357788960786,337.4691054945));
#51885=CARTESIAN_POINT('Ctrl Pts',(145.444490060154,-4.24604983198606,337.482028909192));
#51886=CARTESIAN_POINT('Ctrl Pts',(145.443637911326,-4.23846405740514,337.494915929763));
#51887=CARTESIAN_POINT('Ctrl Pts',(145.435862832548,-4.16925080142035,337.612498207501));
#51888=CARTESIAN_POINT('Ctrl Pts',(145.428087753769,-4.09503156604459,337.727383963553));
#51889=CARTESIAN_POINT('Ctrl Pts',(145.420312674991,-4.01604209742396,337.839117633036));
#51890=CARTESIAN_POINT('Ctrl Pts',(145.412547163942,-3.93714983037308,337.950713807126));
#51891=CARTESIAN_POINT('Ctrl Pts',(145.404781652893,-3.85349923332459,338.059165296312));
#51892=CARTESIAN_POINT('Ctrl Pts',(145.397016141844,-3.76537147672452,338.164041830439));
#51893=CARTESIAN_POINT('Ctrl Pts',(145.389258330321,-3.67733109905178,338.268814379177));
#51894=CARTESIAN_POINT('Ctrl Pts',(145.381500518799,-3.58482264576081,338.370018729445));
#51895=CARTESIAN_POINT('Ctrl Pts',(145.373742707277,-3.4881698323431,338.467254574333));
#51896=CARTESIAN_POINT('Ctrl Pts',(145.365990733754,-3.39158975323255,338.564417246163));
#51897=CARTESIAN_POINT('Ctrl Pts',(145.358238760231,-3.29087179618737,338.657617080845));
#51898=CARTESIAN_POINT('Ctrl Pts',(145.350486786708,-3.18637885737033,338.746488067484));
#51899=CARTESIAN_POINT('Ctrl Pts',(145.34273809615,-3.08193017137491,338.835321417209));
#51900=CARTESIAN_POINT('Ctrl Pts',(145.334989405593,-2.97370998045297,338.919829312427));
#51901=CARTESIAN_POINT('Ctrl Pts',(145.327240715035,-2.86211666047963,338.999683898048));
#51902=CARTESIAN_POINT('Ctrl Pts',(145.319493636657,-2.75054655842864,339.079521869256));
#51903=CARTESIAN_POINT('Ctrl Pts',(145.311746558279,-2.63560504094371,339.154708229283));
#51904=CARTESIAN_POINT('Ctrl Pts',(145.303999479902,-2.51772174055153,339.224956839975));
#51905=CARTESIAN_POINT('Ctrl Pts',(145.296252336596,-2.39983745218363,339.295206039419));
#51906=CARTESIAN_POINT('Ctrl Pts',(145.28850519329,-2.27901166750761,339.360517206893));
#51907=CARTESIAN_POINT('Ctrl Pts',(145.280758049984,-2.15570069062842,339.420649001552));
#51908=CARTESIAN_POINT('Ctrl Pts',(145.273009164956,-2.03236199082387,339.480794315115));
#51909=CARTESIAN_POINT('Ctrl Pts',(145.265260279928,-1.90653733827704,339.535757767482));
#51910=CARTESIAN_POINT('Ctrl Pts',(145.2575113949,-1.77870481565397,339.585345378624));
#51911=CARTESIAN_POINT('Ctrl Pts',(145.249754285125,-1.65073661027051,339.634985622569));
#51912=CARTESIAN_POINT('Ctrl Pts',(145.24199717535,-1.52075664258323,339.679238485487));
#51913=CARTESIAN_POINT('Ctrl Pts',(145.234240065576,-1.3892605562768,339.717959110598));
#51914=CARTESIAN_POINT('Ctrl Pts',(145.226478810649,-1.25769420266614,339.756700426773));
#51915=CARTESIAN_POINT('Ctrl Pts',(145.218717555723,-1.12461049516579,339.789903519973));
#51916=CARTESIAN_POINT('Ctrl Pts',(145.210956300797,-0.990516221003158,
339.817474512484));
#51917=CARTESIAN_POINT('Ctrl Pts',(145.203182630392,-0.856207439703273,
339.845089609596));
#51918=CARTESIAN_POINT('Ctrl Pts',(145.195408959988,-0.720885247368624,
339.86705453966));
#51919=CARTESIAN_POINT('Ctrl Pts',(145.187635289583,-0.585063407588459,
339.883327131332));
#51920=CARTESIAN_POINT('Ctrl Pts',(145.180223485406,-0.455564107127322,
339.898842229946));
#51921=CARTESIAN_POINT('Ctrl Pts',(145.172811681229,-0.325610916447216,
339.909182997698));
#51922=CARTESIAN_POINT('Ctrl Pts',(145.165399877052,-0.195648072444255,
339.914357017378));
#51923=CARTESIAN_POINT('Ctrl Pts',(145.157624798274,-0.059315362316982,
339.919784631174));
#51924=CARTESIAN_POINT('Ctrl Pts',(145.149849719495,0.0774588078877579,
339.919543367492));
#51925=CARTESIAN_POINT('Ctrl Pts',(145.142074640717,0.214163768174801,339.913584937996));
#51926=CARTESIAN_POINT('Ctrl Pts',(145.134309129668,0.350700504304823,339.907633840727));
#51927=CARTESIAN_POINT('Ctrl Pts',(145.126543618619,0.487167813204997,339.895979592806));
#51928=CARTESIAN_POINT('Ctrl Pts',(145.11877810757,0.623051714060567,339.878625792588));
#51929=CARTESIAN_POINT('Ctrl Pts',(145.111020296048,0.758800885633423,339.861289198714));
#51930=CARTESIAN_POINT('Ctrl Pts',(145.103262484525,0.893967415083862,339.838264347795));
#51931=CARTESIAN_POINT('Ctrl Pts',(145.095504673003,1.02803949476319,339.809606830055));
#51932=CARTESIAN_POINT('Ctrl Pts',(145.08775269948,1.16201068095075,339.780970878005));
#51933=CARTESIAN_POINT('Ctrl Pts',(145.080000725957,1.29488867601812,339.746710777554));
#51934=CARTESIAN_POINT('Ctrl Pts',(145.072248752434,1.42616930966034,339.706933626331));
#51935=CARTESIAN_POINT('Ctrl Pts',(145.064500061876,1.55739434587615,339.667173320755));
#51936=CARTESIAN_POINT('Ctrl Pts',(145.056751371319,1.68702299284331,339.621900724596));
#51937=CARTESIAN_POINT('Ctrl Pts',(145.049002680761,1.81456396617585,339.571273419427));
#51938=CARTESIAN_POINT('Ctrl Pts',(145.041255602383,1.94207840354359,339.52065664769));
#51939=CARTESIAN_POINT('Ctrl Pts',(145.033508524006,2.06750566817488,339.464687527071));
#51940=CARTESIAN_POINT('Ctrl Pts',(145.025761445628,2.19037264157943,339.403572498951));
#51941=CARTESIAN_POINT('Ctrl Pts',(145.018014302322,2.31324064472761,339.342456958629));
#51942=CARTESIAN_POINT('Ctrl Pts',(145.010267159016,2.43354796387937,339.276195598864));
#51943=CARTESIAN_POINT('Ctrl Pts',(145.00252001571,2.55084471803529,339.205041532134));
#51944=CARTESIAN_POINT('Ctrl Pts',(144.994771130682,2.66816784299142,339.133871468459));
#51945=CARTESIAN_POINT('Ctrl Pts',(144.987022245654,2.78247872199062,339.057806711659));
#51946=CARTESIAN_POINT('Ctrl Pts',(144.979273360626,2.89335551512492,338.977144317924));
#51947=CARTESIAN_POINT('Ctrl Pts',(144.971516250851,3.00434999403337,338.89639630829));
#51948=CARTESIAN_POINT('Ctrl Pts',(144.963759141077,3.11190278931912,338.811041143815));
#51949=CARTESIAN_POINT('Ctrl Pts',(144.956002031302,3.21562386658751,338.721417231531));
#51950=CARTESIAN_POINT('Ctrl Pts',(144.948240776376,3.31940036908317,338.631745427093));
#51951=CARTESIAN_POINT('Ctrl Pts',(144.94047952145,3.4193407889823,338.537800597164));
#51952=CARTESIAN_POINT('Ctrl Pts',(144.932718266523,3.51509193086257,338.439958107315));
#51953=CARTESIAN_POINT('Ctrl Pts',(144.924944596119,3.61099624336468,338.34195910137));
#51954=CARTESIAN_POINT('Ctrl Pts',(144.917170925714,3.70269762471466,338.240050266868));
#51955=CARTESIAN_POINT('Ctrl Pts',(144.909397255309,3.78988258517244,338.13464081724));
#51956=CARTESIAN_POINT('Ctrl Pts',(144.901985451132,3.87300906474586,338.034138202851));
#51957=CARTESIAN_POINT('Ctrl Pts',(144.894573646955,3.95202996514973,337.930453775162));
#51958=CARTESIAN_POINT('Ctrl Pts',(144.887161842778,4.02671126083791,337.823965205937));
#51959=CARTESIAN_POINT('Ctrl Pts',(144.879386764,4.10505290929151,337.712257314721));
#51960=CARTESIAN_POINT('Ctrl Pts',(144.871611685221,4.17886637711192,337.597110435425));
#51961=CARTESIAN_POINT('Ctrl Pts',(144.863836606443,4.24783470477198,337.478927869752));
#51962=CARTESIAN_POINT('Ctrl Pts',(144.856071095394,4.31671816251407,337.360890735251));
#51963=CARTESIAN_POINT('Ctrl Pts',(144.848305584345,4.38076814814295,337.239825681523));
#51964=CARTESIAN_POINT('Ctrl Pts',(144.840540073296,4.4397095430825,337.116166873279));
#51965=CARTESIAN_POINT('Ctrl Pts',(144.832782261774,4.49859249745728,336.992630673103));
#51966=CARTESIAN_POINT('Ctrl Pts',(144.825024450251,4.55237677404497,336.866506186839));
#51967=CARTESIAN_POINT('Ctrl Pts',(144.817266638729,4.60083215136461,336.738253887517));
#51968=CARTESIAN_POINT('Ctrl Pts',(144.809514665206,4.64925106447635,336.610098102118));
#51969=CARTESIAN_POINT('Ctrl Pts',(144.801762691683,4.69234892276857,336.47981805504));
#51970=CARTESIAN_POINT('Ctrl Pts',(144.79401071816,4.72994295144147,336.347895670521));
#51971=CARTESIAN_POINT('Ctrl Pts',(144.786262027602,4.76752105902087,336.21602915521));
#51972=CARTESIAN_POINT('Ctrl Pts',(144.778513337045,4.79959986602726,336.082522060948));
#51973=CARTESIAN_POINT('Ctrl Pts',(144.770764646487,4.82604602399348,335.947872795683));
#51974=CARTESIAN_POINT('Ctrl Pts',(144.763017568109,4.85248667961569,335.813251545323));
#51975=CARTESIAN_POINT('Ctrl Pts',(144.755270489731,4.87329694194463,335.677488979946));
#51976=CARTESIAN_POINT('Ctrl Pts',(144.747523411354,4.88839438038178,335.541094672263));
#51977=CARTESIAN_POINT('Ctrl Pts',(144.739776268048,4.90349194534996,335.404699221465));
#51978=CARTESIAN_POINT('Ctrl Pts',(144.732029124742,4.91287654792509,335.267672406302));
#51979=CARTESIAN_POINT('Ctrl Pts',(144.724281981436,4.9165175793662,335.130529514988));
#51980=CARTESIAN_POINT('Ctrl Pts',(144.716533096408,4.92015942938846,334.993355791042));
#51981=CARTESIAN_POINT('Ctrl Pts',(144.70878421138,4.91805512840861,334.856066329677));
#51982=CARTESIAN_POINT('Ctrl Pts',(144.701035326352,4.91022619553396,334.719176619221));
#51983=CARTESIAN_POINT('Ctrl Pts',(144.693278216577,4.90238895294901,334.582141612611));
#51984=CARTESIAN_POINT('Ctrl Pts',(144.685521106803,4.88881496307622,334.445507595341));
#51985=CARTESIAN_POINT('Ctrl Pts',(144.677763997028,4.869577729618,334.309785687117));
#51986=CARTESIAN_POINT('Ctrl Pts',(144.670002742102,4.85033021639736,334.173991253446));
#51987=CARTESIAN_POINT('Ctrl Pts',(144.662241487176,4.82541350047232,334.039110284189));
#51988=CARTESIAN_POINT('Ctrl Pts',(144.654480232249,4.79495210045156,333.905642920763));
#51989=CARTESIAN_POINT('Ctrl Pts',(144.646706561845,4.76444197211805,333.771962053053));
#51990=CARTESIAN_POINT('Ctrl Pts',(144.63893289144,4.72836953832865,333.639699687236));
#51991=CARTESIAN_POINT('Ctrl Pts',(144.631159221035,4.68690926809982,333.50934089239));
#51992=CARTESIAN_POINT('Ctrl Pts',(144.623747416858,4.64737898342487,333.385050330807));
#51993=CARTESIAN_POINT('Ctrl Pts',(144.616335612681,4.60295127959753,333.262490376587));
#51994=CARTESIAN_POINT('Ctrl Pts',(144.608923808504,4.55381710421111,333.142062206667));
#51995=CARTESIAN_POINT('Ctrl Pts',(144.601148729726,4.50227471652589,333.015731493403));
#51996=CARTESIAN_POINT('Ctrl Pts',(144.593373650947,4.44538995202806,332.891347590057));
#51997=CARTESIAN_POINT('Ctrl Pts',(144.585598572169,4.38333043073824,332.769395284354));
#51998=CARTESIAN_POINT('Ctrl Pts',(144.57783306112,4.3213472776404,332.647593048726));
#51999=CARTESIAN_POINT('Ctrl Pts',(144.570067550071,4.25420221356236,332.528216802081));
#52000=CARTESIAN_POINT('Ctrl Pts',(144.562302039022,4.18211145442319,332.411732848935));
#52001=CARTESIAN_POINT('Ctrl Pts',(144.5545442275,4.1100921734815,332.295364389967));
#52002=CARTESIAN_POINT('Ctrl Pts',(144.546786415977,4.03313716043688,332.181882847809));
#52003=CARTESIAN_POINT('Ctrl Pts',(144.539028604455,3.95150905083111,332.071731008992));
#52004=CARTESIAN_POINT('Ctrl Pts',(144.531276630932,3.86994236896703,331.961662062928));
#52005=CARTESIAN_POINT('Ctrl Pts',(144.523524657409,3.78370982205343,331.854918145497));
#52006=CARTESIAN_POINT('Ctrl Pts',(144.515772683886,3.69311776053167,331.751913752785));
#52007=CARTESIAN_POINT('Ctrl Pts',(144.508023993329,3.60256406480104,331.648952982494));
#52008=CARTESIAN_POINT('Ctrl Pts',(144.500275302771,3.50765478413935,331.54972887997));
#52009=CARTESIAN_POINT('Ctrl Pts',(144.492526612213,3.40873687791834,331.454623297925));
#52010=CARTESIAN_POINT('Ctrl Pts',(144.484779533836,3.30983955239397,331.35953750339));
#52011=CARTESIAN_POINT('Ctrl Pts',(144.477032455458,3.20693554184033,331.26856879565));
#52012=CARTESIAN_POINT('Ctrl Pts',(144.46928537708,3.10040874889419,331.182062251387));
#52013=CARTESIAN_POINT('Ctrl Pts',(144.461538233774,2.99388106315089,331.095554982117));
#52014=CARTESIAN_POINT('Ctrl Pts',(144.453791090468,2.88373083788279,331.013510197317));
#52015=CARTESIAN_POINT('Ctrl Pts',(144.446043947163,2.77037482579719,330.936232488553));
#52016=CARTESIAN_POINT('Ctrl Pts',(144.438295062134,2.65699332887353,330.85893740612));
#52017=CARTESIAN_POINT('Ctrl Pts',(144.430546177106,2.54040493386412,330.786411752494));
#52018=CARTESIAN_POINT('Ctrl Pts',(144.422797292078,2.42105477112437,330.718916392113));
#52019=CARTESIAN_POINT('Ctrl Pts',(144.415040182304,2.3015779288887,330.651349391459));
#52020=CARTESIAN_POINT('Ctrl Pts',(144.407283072529,2.17933380401186,330.588823542329));
#52021=CARTESIAN_POINT('Ctrl Pts',(144.399525962754,2.05479198503054,330.531553630091));
#52022=CARTESIAN_POINT('Ctrl Pts',(144.391764707828,1.93018361488353,330.474253114643));
#52023=CARTESIAN_POINT('Ctrl Pts',(144.384003452902,1.80327546556876,330.422214280706));
#52024=CARTESIAN_POINT('Ctrl Pts',(144.376242197976,1.67455550083665,330.375603073144));
#52025=CARTESIAN_POINT('Ctrl Pts',(144.368468527571,1.54562962611045,330.328917302839));
#52026=CARTESIAN_POINT('Ctrl Pts',(144.360694857166,1.41488651724197,330.287676626628));
#52027=CARTESIAN_POINT('Ctrl Pts',(144.352921186762,1.28282849436297,330.251996828503));
#52028=CARTESIAN_POINT('Ctrl Pts',(144.345509382584,1.15691780421781,330.217977933563));
#52029=CARTESIAN_POINT('Ctrl Pts',(144.338097578407,1.02981214420768,330.189013913817));
#52030=CARTESIAN_POINT('Ctrl Pts',(144.33068577423,0.901952205277398,330.16516129722));
#52031=CARTESIAN_POINT('Ctrl Pts',(144.322910695452,0.76782546986766,330.140139592831));
#52032=CARTESIAN_POINT('Ctrl Pts',(144.315135616673,0.632444781813479,330.120663937634));
#52033=CARTESIAN_POINT('Ctrl Pts',(144.307360537895,0.496308518264394,330.10685572283));
#52034=CARTESIAN_POINT('Ctrl Pts',(144.299595026846,0.360339779054511,330.093064499914));
#52035=CARTESIAN_POINT('Ctrl Pts',(144.291829515797,0.223617699514287,330.084926879907));
#52036=CARTESIAN_POINT('Ctrl Pts',(144.284064004748,0.0866514119003903,
330.082513386361));
#52037=CARTESIAN_POINT('Ctrl Pts',(144.276306193226,-0.0501790732406641,
330.080102285801));
#52038=CARTESIAN_POINT('Ctrl Pts',(144.268548381703,-0.187252896300901,
330.083404024002));
#52039=CARTESIAN_POINT('Ctrl Pts',(144.260790570181,-0.32405558147598,330.092437362334));
#52040=CARTESIAN_POINT('Ctrl Pts',(144.253038596658,-0.460755318292714,
330.101463902793));
#52041=CARTESIAN_POINT('Ctrl Pts',(144.245286623135,-0.597183934901157,
330.116213432497));
#52042=CARTESIAN_POINT('Ctrl Pts',(144.237534649612,-0.732827088897107,
330.136652642441));
#52043=CARTESIAN_POINT('Ctrl Pts',(144.229785959054,-0.868412797936255,
330.157083196367));
#52044=CARTESIAN_POINT('Ctrl Pts',(144.222037268497,-1.00321332026162,330.183198579923));
#52045=CARTESIAN_POINT('Ctrl Pts',(144.214288577939,-1.13671978815685,330.214913669983));
#52046=CARTESIAN_POINT('Ctrl Pts',(144.206541499561,-1.27019847891647,330.246622161454));
#52047=CARTESIAN_POINT('Ctrl Pts',(144.198794421184,-1.40238327072859,330.283927951749));
#52048=CARTESIAN_POINT('Ctrl Pts',(144.191047342806,-1.53277622950449,330.326694949742));
#52049=CARTESIAN_POINT('Ctrl Pts',(144.1833001995,-1.66317028109897,330.369462306164));
#52050=CARTESIAN_POINT('Ctrl Pts',(144.175553056194,-1.79177209829666,330.417690839761));
#52051=CARTESIAN_POINT('Ctrl Pts',(144.167805912888,-1.9181000147502,330.471194926262));
#52052=CARTESIAN_POINT('Ctrl Pts',(144.16005702786,-2.04445633240138,330.524711041618));
#52053=CARTESIAN_POINT('Ctrl Pts',(144.152308142832,-2.1685373721823,330.583504917588));
#52054=CARTESIAN_POINT('Ctrl Pts',(144.144559257804,-2.28988288204651,330.647343403275));
#52055=CARTESIAN_POINT('Ctrl Pts',(144.136802148029,-2.41135718928842,330.711249647791));
#52056=CARTESIAN_POINT('Ctrl Pts',(144.129045038255,-2.53008982009006,330.780211015667));
#52057=CARTESIAN_POINT('Ctrl Pts',(144.12128792848,-2.64564603554945,330.853948852573));
#52058=CARTESIAN_POINT('Ctrl Pts',(144.113526673554,-2.76126400055581,330.927726092621));
#52059=CARTESIAN_POINT('Ctrl Pts',(144.105765418628,-2.87370184779567,331.006284663817));
#52060=CARTESIAN_POINT('Ctrl Pts',(144.098004163701,-2.98255596550833,331.089304029318));
#52061=CARTESIAN_POINT('Ctrl Pts',(144.090230493297,-3.09158421433367,331.172456198748));
#52062=CARTESIAN_POINT('Ctrl Pts',(144.082456822892,-3.19701697703763,331.26008317199));
#52063=CARTESIAN_POINT('Ctrl Pts',(144.074683152487,-3.29848505414383,331.351825194691));
#52064=CARTESIAN_POINT('Ctrl Pts',(144.06727134831,-3.39522976784731,331.439296604163));
#52065=CARTESIAN_POINT('Ctrl Pts',(144.059859544133,-3.48837039592104,331.530508372303));
#52066=CARTESIAN_POINT('Ctrl Pts',(144.052447739957,-3.57762091964424,331.625120503214));
#52067=CARTESIAN_POINT('Ctrl Pts',(144.044765905567,-3.67012305893822,331.723179586202));
#52068=CARTESIAN_POINT('Ctrl Pts',(144.037084071178,-3.75875446931306,331.82521850884));
#52069=CARTESIAN_POINT('Ctrl Pts',(144.029402236789,-3.84314688427203,331.930895067221));
#52070=CARTESIAN_POINT('Ctrl Pts',(144.021586200944,-3.92901363262143,332.038417792448));
#52071=CARTESIAN_POINT('Ctrl Pts',(144.013770165099,-4.01049154587189,332.149706204312));
#52072=CARTESIAN_POINT('Ctrl Pts',(144.005954129254,-4.08723028545093,332.264359004512));
#52073=CARTESIAN_POINT('Ctrl Pts',(143.998291178797,-4.16246601507074,332.376766207489));
#52074=CARTESIAN_POINT('Ctrl Pts',(143.99062822834,-4.23314624883612,332.492406882745));
#52075=CARTESIAN_POINT('Ctrl Pts',(143.982965277882,-4.29898060686261,332.610868608821));
#52076=CARTESIAN_POINT('Ctrl Pts',(143.975307371956,-4.3647716260445,332.729252351386));
#52077=CARTESIAN_POINT('Ctrl Pts',(143.967649466029,-4.42572291897584,332.850453102647));
#52078=CARTESIAN_POINT('Ctrl Pts',(143.959991560102,-4.48158777971099,332.974030100114));
#52079=CARTESIAN_POINT('Ctrl Pts',(143.952336941738,-4.53742865749236,333.097554045601));
#52080=CARTESIAN_POINT('Ctrl Pts',(143.944682323373,-4.58818728196023,333.223451843142));
#52081=CARTESIAN_POINT('Ctrl Pts',(143.937027705009,-4.63366346606154,333.351259284852));
#52082=CARTESIAN_POINT('Ctrl Pts',(143.929093510967,-4.68080061278168,333.483734738782));
#52083=CARTESIAN_POINT('Ctrl Pts',(143.921159316925,-4.72226191421726,333.618261577884));
#52084=CARTESIAN_POINT('Ctrl Pts',(143.913225122884,-4.75787970222818,333.754301881825));
#52085=CARTESIAN_POINT('Ctrl Pts',(143.905569724747,-4.79224593357283,333.885561929641));
#52086=CARTESIAN_POINT('Ctrl Pts',(143.89791432661,-4.82117231235154,334.018230459332));
#52087=CARTESIAN_POINT('Ctrl Pts',(143.890258928474,-4.84455974513305,334.151811378091));
#52088=CARTESIAN_POINT('Ctrl Pts',(143.882601961923,-4.86795196945959,334.285419664496));
#52089=CARTESIAN_POINT('Ctrl Pts',(143.874944995372,-4.88580292996572,334.419940315398));
#52090=CARTESIAN_POINT('Ctrl Pts',(143.867288028821,-4.89806518468095,334.554870233397));
#52091=CARTESIAN_POINT('Ctrl Pts',(143.859625608661,-4.91033617308153,334.689896254067));
#52092=CARTESIAN_POINT('Ctrl Pts',(143.851963188502,-4.91701048961626,334.825331723587));
#52093=CARTESIAN_POINT('Ctrl Pts',(143.844300768342,-4.91809275560886,334.96067176933));
#52094=CARTESIAN_POINT('Ctrl Pts',(143.843472971064,-4.91820967648035,334.975293014203));
#52095=CARTESIAN_POINT('Ctrl Pts',(143.842645173786,-4.91826138136206,334.989913148133));
#52096=CARTESIAN_POINT('Ctrl Pts',(143.841817376508,-4.91824791238418,335.004531537123));
#52097=CARTESIAN_POINT('',(142.091817376456,-4.91824980134024,334.998602102778));
#52098=CARTESIAN_POINT('Ctrl Pts',(143.841817376479,-4.9182479123837,335.004531537634));
#52099=CARTESIAN_POINT('Ctrl Pts',(143.831755391686,-4.91808419516746,335.182219978545));
#52100=CARTESIAN_POINT('Ctrl Pts',(143.821693406893,-4.90828766482633,335.359479490191));
#52101=CARTESIAN_POINT('Ctrl Pts',(143.811631422101,-4.88901797353475,335.535430963761));
#52102=CARTESIAN_POINT('Ctrl Pts',(143.801323074948,-4.86927647407371,335.715690515827));
#52103=CARTESIAN_POINT('Ctrl Pts',(143.791014727794,-4.83959221489103,335.89457752059));
#52104=CARTESIAN_POINT('Ctrl Pts',(143.780706380641,-4.80018467176683,336.071172338811));
#52105=CARTESIAN_POINT('Ctrl Pts',(143.778540822322,-4.79190600869851,336.108271048443));
#52106=CARTESIAN_POINT('Ctrl Pts',(143.776375264002,-4.78319839576932,336.14526867524));
#52107=CARTESIAN_POINT('Ctrl Pts',(143.774209705682,-4.77406413220818,336.182156810268));
#52108=CARTESIAN_POINT('Ctrl Pts',(143.766434626904,-4.74126907047998,336.314597554635));
#52109=CARTESIAN_POINT('Ctrl Pts',(143.758659548125,-4.7029068095277,336.445881859782));
#52110=CARTESIAN_POINT('Ctrl Pts',(143.750884469347,-4.65907334251896,336.575505839891));
#52111=CARTESIAN_POINT('Ctrl Pts',(143.743118958298,-4.61529381538194,336.704970309439));
#52112=CARTESIAN_POINT('Ctrl Pts',(143.735353447249,-4.56605660228122,336.832778152466));
#52113=CARTESIAN_POINT('Ctrl Pts',(143.7275879362,-4.51150844896089,336.958436768817));
#52114=CARTESIAN_POINT('Ctrl Pts',(143.719830124678,-4.45701438029341,337.083970794284));
#52115=CARTESIAN_POINT('Ctrl Pts',(143.712072313155,-4.397220005314,337.207359477575));
#52116=CARTESIAN_POINT('Ctrl Pts',(143.704314501633,-4.33232139449749,337.328126800086));
#52117=CARTESIAN_POINT('Ctrl Pts',(143.69656252811,-4.2674716219436,337.448803241358));
#52118=CARTESIAN_POINT('Ctrl Pts',(143.688810554587,-4.1975254433542,337.566861905406));
#52119=CARTESIAN_POINT('Ctrl Pts',(143.681058581064,-4.12272626535064,337.68184846766));
#52120=CARTESIAN_POINT('Ctrl Pts',(143.673309890507,-4.04795876484348,337.796786333036));
#52121=CARTESIAN_POINT('Ctrl Pts',(143.665561199949,-3.96834256536025,337.90865435732));
#52122=CARTESIAN_POINT('Ctrl Pts',(143.657812509391,-3.88416596355725,338.017024665137));
#52123=CARTESIAN_POINT('Ctrl Pts',(143.650065431014,-3.80000687539927,338.125372425606));
#52124=CARTESIAN_POINT('Ctrl Pts',(143.642318352636,-3.71128951183635,338.230223608614));
#52125=CARTESIAN_POINT('Ctrl Pts',(143.634571274258,-3.61834402784686,338.331181405845));
#52126=CARTESIAN_POINT('Ctrl Pts',(143.626824130952,-3.52539776488478,338.432140049198));
#52127=CARTESIAN_POINT('Ctrl Pts',(143.619076987646,-3.42822357556011,338.529204954125));
#52128=CARTESIAN_POINT('Ctrl Pts',(143.61132984434,-3.32718995734353,338.622014639707));
#52129=CARTESIAN_POINT('Ctrl Pts',(143.603580959312,-3.22613362462457,338.714845190877));
#52130=CARTESIAN_POINT('Ctrl Pts',(143.595832074284,-3.12121642422502,338.803418354673));
#52131=CARTESIAN_POINT('Ctrl Pts',(143.588083189256,-3.01284123768635,338.887411830382));
#52132=CARTESIAN_POINT('Ctrl Pts',(143.580326079481,-2.90435102060488,338.971494457634));
#52133=CARTESIAN_POINT('Ctrl Pts',(143.572568969707,-2.79239579496854,339.050987446816));
#52134=CARTESIAN_POINT('Ctrl Pts',(143.564811859932,-2.67740928685603,339.125610569741));
#52135=CARTESIAN_POINT('Ctrl Pts',(143.557050605006,-2.56236133363025,339.200273568876));
#52136=CARTESIAN_POINT('Ctrl Pts',(143.54928935008,-2.44427920661862,339.270061317661));
#52137=CARTESIAN_POINT('Ctrl Pts',(143.541528095153,-2.32362185501996,339.334739269826));
#52138=CARTESIAN_POINT('Ctrl Pts',(143.533754424749,-2.20277149098079,339.399520685637));
#52139=CARTESIAN_POINT('Ctrl Pts',(143.525980754344,-2.07933802244679,339.459175800561));
#52140=CARTESIAN_POINT('Ctrl Pts',(143.518207083939,-1.95380183518605,339.513517636093));
#52141=CARTESIAN_POINT('Ctrl Pts',(143.510795279762,-1.83410938764405,339.565329846108));
#52142=CARTESIAN_POINT('Ctrl Pts',(143.503383475585,-1.71250584741837,339.612312207165));
#52143=CARTESIAN_POINT('Ctrl Pts',(143.495971671408,-1.58941915571576,339.654345261145));
#52144=CARTESIAN_POINT('Ctrl Pts',(143.48819659263,-1.46029961859701,339.698438480311));
#52145=CARTESIAN_POINT('Ctrl Pts',(143.480421513851,-1.32913982494351,339.73722430726));
#52146=CARTESIAN_POINT('Ctrl Pts',(143.472646435073,-1.19641545050181,339.770510783166));
#52147=CARTESIAN_POINT('Ctrl Pts',(143.464880924024,-1.0638544018525,339.803756297943));
#52148=CARTESIAN_POINT('Ctrl Pts',(143.457115412975,-0.929732978750773,
339.831515832492));
#52149=CARTESIAN_POINT('Ctrl Pts',(143.449349901926,-0.7945448317185,339.853646214228));
#52150=CARTESIAN_POINT('Ctrl Pts',(143.441592090404,-0.659490724127554,
339.875754653626));
#52151=CARTESIAN_POINT('Ctrl Pts',(143.433834278881,-0.523372380664144,
339.892244984619));
#52152=CARTESIAN_POINT('Ctrl Pts',(143.426076467359,-0.386696200512076,
339.903024486071));
#52153=CARTESIAN_POINT('Ctrl Pts',(143.418324493836,-0.250122873519823,
339.913795875606));
#52154=CARTESIAN_POINT('Ctrl Pts',(143.410572520313,-0.112992933505257,
339.918864959115));
#52155=CARTESIAN_POINT('Ctrl Pts',(143.40282054679,0.0241798470182742,339.918190561324));
#52156=CARTESIAN_POINT('Ctrl Pts',(143.395071856232,0.16129453478772,339.917516449141));
#52157=CARTESIAN_POINT('Ctrl Pts',(143.387323165675,0.298451636924919,339.911103695385));
#52158=CARTESIAN_POINT('Ctrl Pts',(143.379574475117,0.435135330035015,339.898963186946));
#52159=CARTESIAN_POINT('Ctrl Pts',(143.371827396739,0.571790584961155,339.886825204442));
#52160=CARTESIAN_POINT('Ctrl Pts',(143.364080318362,0.707972237680056,339.868961872205));
#52161=CARTESIAN_POINT('Ctrl Pts',(143.356333239984,0.843167937808599,339.845436088852));
#52162=CARTESIAN_POINT('Ctrl Pts',(143.348586096678,0.97836477100728,339.82191010833));
#52163=CARTESIAN_POINT('Ctrl Pts',(143.340838953372,1.11257525004651,339.792721649046));
#52164=CARTESIAN_POINT('Ctrl Pts',(143.333091810066,1.24529598278496,339.757984970317));
#52165=CARTESIAN_POINT('Ctrl Pts',(143.325342925038,1.37804655396183,339.723240482045));
#52166=CARTESIAN_POINT('Ctrl Pts',(143.31759404001,1.50930633430796,339.682945391176));
#52167=CARTESIAN_POINT('Ctrl Pts',(143.309845154982,1.63858627195674,339.637264073983));
#52168=CARTESIAN_POINT('Ctrl Pts',(143.302088045207,1.76800342866715,339.591534270168));
#52169=CARTESIAN_POINT('Ctrl Pts',(143.294330935433,1.89543617576038,339.540406950224));
#52170=CARTESIAN_POINT('Ctrl Pts',(143.286573825658,2.02041414930605,339.484095196111));
#52171=CARTESIAN_POINT('Ctrl Pts',(143.278812570732,2.14545890708468,339.427753350797));
#52172=CARTESIAN_POINT('Ctrl Pts',(143.271051315805,2.26804592837122,339.366221726309));
#52173=CARTESIAN_POINT('Ctrl Pts',(143.263290060879,2.38772961445817,339.299759336374));
#52174=CARTESIAN_POINT('Ctrl Pts',(143.255516390475,2.50760475543804,339.233190628276));
#52175=CARTESIAN_POINT('Ctrl Pts',(143.24774272007,2.62456694669851,339.161675596944));
#52176=CARTESIAN_POINT('Ctrl Pts',(143.239969049665,2.73819898972141,339.08551702422));
#52177=CARTESIAN_POINT('Ctrl Pts',(143.232557245488,2.84654143380387,339.012903651378));
#52178=CARTESIAN_POINT('Ctrl Pts',(143.225145441311,2.95185655676719,338.93606949152));
#52179=CARTESIAN_POINT('Ctrl Pts',(143.217733637134,3.05381232018853,338.855309763892));
#52180=CARTESIAN_POINT('Ctrl Pts',(143.209958558356,3.16076523928528,338.770591761444));
#52181=CARTESIAN_POINT('Ctrl Pts',(143.202183479577,3.26435915891964,338.681285929282));
#52182=CARTESIAN_POINT('Ctrl Pts',(143.194408400799,3.36417524137779,338.587688393353));
#52183=CARTESIAN_POINT('Ctrl Pts',(143.18664288975,3.4638684937919,338.494206035151));
#52184=CARTESIAN_POINT('Ctrl Pts',(143.178877378701,3.55979287654325,338.396442746096));
#52185=CARTESIAN_POINT('Ctrl Pts',(143.171111867652,3.65156085012984,338.294736168542));
#52186=CARTESIAN_POINT('Ctrl Pts',(143.163354056129,3.74323783550341,338.193130433356));
#52187=CARTESIAN_POINT('Ctrl Pts',(143.155596244607,3.8307663527579,338.087589478695));
#52188=CARTESIAN_POINT('Ctrl Pts',(143.147838433085,3.91379438905707,337.97848896971));
#52189=CARTESIAN_POINT('Ctrl Pts',(143.140086459562,3.99675994412591,337.869470562318));
#52190=CARTESIAN_POINT('Ctrl Pts',(143.132334486039,4.07523152364888,337.756898242171));
#52191=CARTESIAN_POINT('Ctrl Pts',(143.124582512516,4.14889647067288,337.641181769235));
#52192=CARTESIAN_POINT('Ctrl Pts',(143.116833821958,4.22253022054811,337.525514302293));
#52193=CARTESIAN_POINT('Ctrl Pts',(143.109085131401,4.29136117714352,337.406705659966));
#52194=CARTESIAN_POINT('Ctrl Pts',(143.101336440843,4.3551193538416,337.285195500673));
#52195=CARTESIAN_POINT('Ctrl Pts',(143.093589362465,4.41886426511851,337.163710622583));
#52196=CARTESIAN_POINT('Ctrl Pts',(143.085842284088,4.4775383143312,337.039525691432));
#52197=CARTESIAN_POINT('Ctrl Pts',(143.07809520571,4.53091713207614,336.913105591639));
#52198=CARTESIAN_POINT('Ctrl Pts',(143.070348062404,4.58429639718699,336.786684432323));
#52199=CARTESIAN_POINT('Ctrl Pts',(143.062600919098,4.6323801902699,336.658028427091));
#52200=CARTESIAN_POINT('Ctrl Pts',(143.054853775792,4.67499218005093,336.527622721408));
#52201=CARTESIAN_POINT('Ctrl Pts',(143.047104890764,4.71761374991191,336.397187697754));
#52202=CARTESIAN_POINT('Ctrl Pts',(143.039356005736,4.75476094717216,336.265002562355));
#52203=CARTESIAN_POINT('Ctrl Pts',(143.031607120708,4.7863073453195,336.131567522793));
#52204=CARTESIAN_POINT('Ctrl Pts',(143.023850010933,4.81788722713978,335.997990853902));
#52205=CARTESIAN_POINT('Ctrl Pts',(143.016092901159,4.84385434458669,335.863162011706));
#52206=CARTESIAN_POINT('Ctrl Pts',(143.008335791384,4.86413334191449,335.727591846144));
#52207=CARTESIAN_POINT('Ctrl Pts',(143.000574536458,4.88442317569007,335.591949236221));
#52208=CARTESIAN_POINT('Ctrl Pts',(142.992813281531,4.89901879119825,335.455564902048));
#52209=CARTESIAN_POINT('Ctrl Pts',(142.985052026605,4.90789685957971,335.318953724273));
#52210=CARTESIAN_POINT('Ctrl Pts',(142.977278356201,4.91678912997724,335.182124013135));
#52211=CARTESIAN_POINT('Ctrl Pts',(142.969504685796,4.91994556740354,335.04506712424));
#52212=CARTESIAN_POINT('Ctrl Pts',(142.961731015391,4.91739501751266,334.908297741349));
#52213=CARTESIAN_POINT('Ctrl Pts',(142.954319211214,4.91496319633284,334.777895006138));
#52214=CARTESIAN_POINT('Ctrl Pts',(142.946907407037,4.90734376813904,334.647753899798));
#52215=CARTESIAN_POINT('Ctrl Pts',(142.93949560286,4.89460530405207,334.518313400596));
#52216=CARTESIAN_POINT('Ctrl Pts',(142.931720524082,4.88124248989416,334.382528636944));
#52217=CARTESIAN_POINT('Ctrl Pts',(142.923945445303,4.86220392450461,334.247085789694));
#52218=CARTESIAN_POINT('Ctrl Pts',(142.916170366525,4.83751196939024,334.112497319155));
#52219=CARTESIAN_POINT('Ctrl Pts',(142.908404855476,4.8128503992986,333.978074468299));
#52220=CARTESIAN_POINT('Ctrl Pts',(142.900639344427,4.78254935149013,333.844504283022));
#52221=CARTESIAN_POINT('Ctrl Pts',(142.892873833378,4.74668303676358,333.712295371212));
#52222=CARTESIAN_POINT('Ctrl Pts',(142.885116021856,4.7108522835925,333.580217544924));
#52223=CARTESIAN_POINT('Ctrl Pts',(142.877358210334,4.66946734627238,333.44949868092));
#52224=CARTESIAN_POINT('Ctrl Pts',(142.869600398811,4.62265363529868,333.320638088273));
#52225=CARTESIAN_POINT('Ctrl Pts',(142.861848425288,4.57587515312704,333.191874467308));
#52226=CARTESIAN_POINT('Ctrl Pts',(142.854096451765,4.52367616186882,333.06496670014));
#52227=CARTESIAN_POINT('Ctrl Pts',(142.846344478242,4.46623204080221,332.940399451298));
#52228=CARTESIAN_POINT('Ctrl Pts',(142.838595787685,4.408812247355,332.815884956761));
#52229=CARTESIAN_POINT('Ctrl Pts',(142.830847097127,4.34615190548417,332.693709363314));
#52230=CARTESIAN_POINT('Ctrl Pts',(142.82309840657,4.27847462808346,332.574337632863));
#52231=CARTESIAN_POINT('Ctrl Pts',(142.815351328192,4.21081143150557,332.454990738697));
#52232=CARTESIAN_POINT('Ctrl Pts',(142.807604249814,4.13813356827702,332.338446886982));
#52233=CARTESIAN_POINT('Ctrl Pts',(142.799857171436,4.06071055046379,332.225146330371));
#52234=CARTESIAN_POINT('Ctrl Pts',(142.79211002813,3.98328688377115,332.111844824193));
#52235=CARTESIAN_POINT('Ctrl Pts',(142.784362884825,3.90111820370109,332.001786990056));
#52236=CARTESIAN_POINT('Ctrl Pts',(142.776615741519,3.8145170564545,331.895383648739));
#52237=CARTESIAN_POINT('Ctrl Pts',(142.768866856491,3.72789643943142,331.788956385692));
#52238=CARTESIAN_POINT('Ctrl Pts',(142.761117971463,3.6368416189717,331.686185553469));
#52239=CARTESIAN_POINT('Ctrl Pts',(142.753369086435,3.54170481366177,331.587448157847));
#52240=CARTESIAN_POINT('Ctrl Pts',(142.74561197666,3.4464670291637,331.488605961332));
#52241=CARTESIAN_POINT('Ctrl Pts',(142.737854866885,3.34713887655722,331.393806035297));
#52242=CARTESIAN_POINT('Ctrl Pts',(142.73009775711,3.24410916113689,331.303388198211));
#52243=CARTESIAN_POINT('Ctrl Pts',(142.722336502184,3.14102438993088,331.212922044724));
#52244=CARTESIAN_POINT('Ctrl Pts',(142.714575247258,3.03423441873966,331.126842891306));
#52245=CARTESIAN_POINT('Ctrl Pts',(142.706813992332,2.92415959710192,331.045448987157));
#52246=CARTESIAN_POINT('Ctrl Pts',(142.699040321927,2.8139086916229,330.963924879288));
#52247=CARTESIAN_POINT('Ctrl Pts',(142.691266651523,2.70036275917778,330.887101216812));
#52248=CARTESIAN_POINT('Ctrl Pts',(142.683492981118,2.58397021836186,330.815232267722));
#52249=CARTESIAN_POINT('Ctrl Pts',(142.676081176941,2.47299577832311,330.746708835502));
#52250=CARTESIAN_POINT('Ctrl Pts',(142.668669372764,2.35943403576318,330.682689355086));
#52251=CARTESIAN_POINT('Ctrl Pts',(142.661257568587,2.24369124464108,330.623353719888));
#52252=CARTESIAN_POINT('Ctrl Pts',(142.653482489808,2.12227555454633,330.561109868456));
#52253=CARTESIAN_POINT('Ctrl Pts',(142.64570741103,1.998075914582,330.503823907906));
#52254=CARTESIAN_POINT('Ctrl Pts',(142.637932332251,1.87153536465084,330.451754355649));
#52255=CARTESIAN_POINT('Ctrl Pts',(142.630166821202,1.74515053092237,330.39974887829));
#52256=CARTESIAN_POINT('Ctrl Pts',(142.622401310153,1.61643087688516,330.352947184328));
#52257=CARTESIAN_POINT('Ctrl Pts',(142.614635799104,1.48584426148408,330.31156210523));
#52258=CARTESIAN_POINT('Ctrl Pts',(142.606877987582,1.35538712309224,330.270218059559));
#52259=CARTESIAN_POINT('Ctrl Pts',(142.59912017606,1.22306707733535,330.234280058301));
#52260=CARTESIAN_POINT('Ctrl Pts',(142.591362364538,1.08937187067994,330.203912845885));
#52261=CARTESIAN_POINT('Ctrl Pts',(142.583610391015,0.955777273907336,330.173568485759));
#52262=CARTESIAN_POINT('Ctrl Pts',(142.575858417491,0.820809955689621,330.148786656344));
#52263=CARTESIAN_POINT('Ctrl Pts',(142.568106443968,0.68497238856128,330.12968215725));
#52264=CARTESIAN_POINT('Ctrl Pts',(142.560357753411,0.54919234872331,330.110585748923));
#52265=CARTESIAN_POINT('Ctrl Pts',(142.552609062853,0.412543179255915,330.097161943154));
#52266=CARTESIAN_POINT('Ctrl Pts',(142.544860372296,0.275536886312012,330.089474316656));
#52267=CARTESIAN_POINT('Ctrl Pts',(142.537113293918,0.138559098671562,330.081788289633));
#52268=CARTESIAN_POINT('Ctrl Pts',(142.52936621554,0.00122472536296278,
330.079836089889));
#52269=CARTESIAN_POINT('Ctrl Pts',(142.521619137162,-0.135950167323248,
330.083629324949));
#52270=CARTESIAN_POINT('Ctrl Pts',(142.513871993856,-0.273126209666995,
330.0874225918));
#52271=CARTESIAN_POINT('Ctrl Pts',(142.50612485055,-0.41014237799747,330.096961378694));
#52272=CARTESIAN_POINT('Ctrl Pts',(142.498377707244,-0.546484067674328,
330.112205177559));
#52273=CARTESIAN_POINT('Ctrl Pts',(142.490628822216,-0.682856409857596,
330.127452403554));
#52274=CARTESIAN_POINT('Ctrl Pts',(142.482879937188,-0.818553583268342,
330.148407150344));
#52275=CARTESIAN_POINT('Ctrl Pts',(142.47513105216,-0.953067950019553,330.174977249261));
#52276=CARTESIAN_POINT('Ctrl Pts',(142.467373942385,-1.08772509170952,330.201575549957));
#52277=CARTESIAN_POINT('Ctrl Pts',(142.459616832611,-1.22119653480356,330.233801032961));
#52278=CARTESIAN_POINT('Ctrl Pts',(142.451859722836,-1.35298611384692,330.271510638879));
#52279=CARTESIAN_POINT('Ctrl Pts',(142.44409846791,-1.4848461170275,330.309240395604));
#52280=CARTESIAN_POINT('Ctrl Pts',(142.436337212983,-1.61502209457335,330.352459991508));
#52281=CARTESIAN_POINT('Ctrl Pts',(142.428575958057,-1.74303576711506,330.400977345451));
#52282=CARTESIAN_POINT('Ctrl Pts',(142.420802287653,-1.87125421981323,330.449572311348));
#52283=CARTESIAN_POINT('Ctrl Pts',(142.413028617248,-1.99730309586012,330.503481816431));
#52284=CARTESIAN_POINT('Ctrl Pts',(142.405254946843,-2.1207259108454,330.562466374937));
#52285=CARTESIAN_POINT('Ctrl Pts',(142.397843142666,-2.23840336409796,330.618705188052));
#52286=CARTESIAN_POINT('Ctrl Pts',(142.390431338489,-2.35369348604368,330.679557065814));
#52287=CARTESIAN_POINT('Ctrl Pts',(142.383019534312,-2.46622515314727,330.744777731248));
#52288=CARTESIAN_POINT('Ctrl Pts',(142.375244455534,-2.58427233247129,330.813195055778));
#52289=CARTESIAN_POINT('Ctrl Pts',(142.367469376755,-2.69965687059855,330.886636462385));
#52290=CARTESIAN_POINT('Ctrl Pts',(142.359694297977,-2.81192162040989,330.96486928797));
#52291=CARTESIAN_POINT('Ctrl Pts',(142.351928786928,-2.92404822129954,331.043005843082));
#52292=CARTESIAN_POINT('Ctrl Pts',(142.344163275879,-3.03306235495441,331.125921864191));
#52293=CARTESIAN_POINT('Ctrl Pts',(142.33639776483,-3.13853186153162,331.21333909405));
#52294=CARTESIAN_POINT('Ctrl Pts',(142.328639953308,-3.24389679478593,331.300669649471));
#52295=CARTESIAN_POINT('Ctrl Pts',(142.320882141786,-3.34572379602886,331.392492284269));
#52296=CARTESIAN_POINT('Ctrl Pts',(142.313124330263,-3.44361038055605,331.488485994699));
#52297=CARTESIAN_POINT('Ctrl Pts',(142.30537235674,-3.54142330232418,331.584407466817));
#52298=CARTESIAN_POINT('Ctrl Pts',(142.297620383217,-3.63530143168714,331.68449349423));
#52299=CARTESIAN_POINT('Ctrl Pts',(142.289868409694,-3.72487631448255,331.78838366172));
#52300=CARTESIAN_POINT('Ctrl Pts',(142.282119719137,-3.81441326226192,331.892229831662));
#52301=CARTESIAN_POINT('Ctrl Pts',(142.274371028579,-3.89965033344395,331.99987664199));
#52302=CARTESIAN_POINT('Ctrl Pts',(142.266622338022,-3.98025698910588,332.110927940813));
#52303=CARTESIAN_POINT('Ctrl Pts',(142.258875259644,-4.06084687387988,332.221956134486));
#52304=CARTESIAN_POINT('Ctrl Pts',(142.251128181266,-4.13680802993508,332.336387091603));
#52305=CARTESIAN_POINT('Ctrl Pts',(142.243381102888,-4.20785142317407,332.453793122507));
#52306=CARTESIAN_POINT('Ctrl Pts',(142.235633959582,-4.27889541182511,332.571200137387));
#52307=CARTESIAN_POINT('Ctrl Pts',(142.227886816276,-4.34502135309445,332.691581941372));
#52308=CARTESIAN_POINT('Ctrl Pts',(142.220139672971,-4.40598482898517,332.814483871198));
#52309=CARTESIAN_POINT('Ctrl Pts',(142.212390787943,-4.46696201075934,332.937413431987));
#52310=CARTESIAN_POINT('Ctrl Pts',(142.204641902914,-4.52277424396893,333.062863895951));
#52311=CARTESIAN_POINT('Ctrl Pts',(142.196893017886,-4.57322432322255,333.190358501806));
#52312=CARTESIAN_POINT('Ctrl Pts',(142.189135908112,-4.62372795071169,333.317988431753));
#52313=CARTESIAN_POINT('Ctrl Pts',(142.181378798337,-4.6688579110012,333.447666473691));
#52314=CARTESIAN_POINT('Ctrl Pts',(142.173621688562,-4.70846600219053,333.578897973854));
#52315=CARTESIAN_POINT('Ctrl Pts',(142.165860433636,-4.74809525867737,333.710199599935));
#52316=CARTESIAN_POINT('Ctrl Pts',(142.15809917871,-4.78219666937835,333.84305595992));
#52317=CARTESIAN_POINT('Ctrl Pts',(142.150337923784,-4.8106729350113,333.976960912355));
#52318=CARTESIAN_POINT('Ctrl Pts',(142.142564253379,-4.83919475338887,334.111080069075));
#52319=CARTESIAN_POINT('Ctrl Pts',(142.134790582974,-4.86207337996778,334.246250784604));
#52320=CARTESIAN_POINT('Ctrl Pts',(142.12701691257,-4.87926317352832,334.381959591976));
#52321=CARTESIAN_POINT('Ctrl Pts',(142.119605108393,-4.89565277806326,334.511351121717));
#52322=CARTESIAN_POINT('Ctrl Pts',(142.112193304215,-4.90687123616648,334.641231487608));
#52323=CARTESIAN_POINT('Ctrl Pts',(142.104781500038,-4.91292312931696,334.771156411664));
#52324=CARTESIAN_POINT('Ctrl Pts',(142.100460125528,-4.91645162199873,334.846907772819));
#52325=CARTESIAN_POINT('Ctrl Pts',(142.096138751018,-4.91822823969099,334.922741370048));
#52326=CARTESIAN_POINT('Ctrl Pts',(142.091817376508,-4.91824980133998,334.998602101861));
#52327=CARTESIAN_POINT('',(140.34181737656,-4.91824854457842,334.996216317635));
#52328=CARTESIAN_POINT('Ctrl Pts',(142.091817376456,-4.91824980134024,334.998602102778));
#52329=CARTESIAN_POINT('Ctrl Pts',(142.084099485954,-4.91828830999909,335.134087888651));
#52330=CARTESIAN_POINT('Ctrl Pts',(142.076381595451,-4.91272412795323,335.269800248869));
#52331=CARTESIAN_POINT('Ctrl Pts',(142.068663704949,-4.90152721851429,335.405233252169));
#52332=CARTESIAN_POINT('Ctrl Pts',(142.060955124243,-4.89034381547907,335.540502887816));
#52333=CARTESIAN_POINT('Ctrl Pts',(142.053246543537,-4.87354123299007,335.675493444912));
#52334=CARTESIAN_POINT('Ctrl Pts',(142.045537962831,-4.85114141364458,335.809697503592));
#52335=CARTESIAN_POINT('Ctrl Pts',(142.037836769446,-4.82876306059277,335.943772951246));
#52336=CARTESIAN_POINT('Ctrl Pts',(142.030135576062,-4.80079820753371,336.077063010813));
#52337=CARTESIAN_POINT('Ctrl Pts',(142.022434382677,-4.76732068138356,336.209064342106));
#52338=CARTESIAN_POINT('Ctrl Pts',(142.01473866125,-4.73386694214605,336.340971881997));
#52339=CARTESIAN_POINT('Ctrl Pts',(142.007042939823,-4.69490842178153,336.471592132325));
#52340=CARTESIAN_POINT('Ctrl Pts',(141.999347218396,-4.65057012951809,336.600431358395));
#52341=CARTESIAN_POINT('Ctrl Pts',(141.991654256198,-4.60624773433632,336.729224390361));
#52342=CARTESIAN_POINT('Ctrl Pts',(141.983961294,-4.55654953029598,336.856237292492));
#52343=CARTESIAN_POINT('Ctrl Pts',(141.976268331802,-4.50165046563169,336.980991203357));
#52344=CARTESIAN_POINT('Ctrl Pts',(141.968576551801,-4.4467598374387,337.105725942989));
#52345=CARTESIAN_POINT('Ctrl Pts',(141.960884771799,-4.38667009786801,337.228202018312));
#52346=CARTESIAN_POINT('Ctrl Pts',(141.953192991797,-4.32160425576246,337.347960757567));
#52347=CARTESIAN_POINT('Ctrl Pts',(141.945500668206,-4.25653381535751,337.46772796035));
#52348=CARTESIAN_POINT('Ctrl Pts',(141.937808344615,-4.18648676258374,337.58477709614));
#52349=CARTESIAN_POINT('Ctrl Pts',(141.930116021023,-4.11173172203353,337.698674731887));
#52350=CARTESIAN_POINT('Ctrl Pts',(141.922421427981,-4.03695462665031,337.81260597063));
#52351=CARTESIAN_POINT('Ctrl Pts',(141.914726834938,-3.95746699849299,337.923383528075));
#52352=CARTESIAN_POINT('Ctrl Pts',(141.907032241896,-3.87358009018564,338.030603957533));
#52353=CARTESIAN_POINT('Ctrl Pts',(141.899329328923,-3.7896024775064,338.137940321194));
#52354=CARTESIAN_POINT('Ctrl Pts',(141.891626415951,-3.7012163327452,338.241711565036));
#52355=CARTESIAN_POINT('Ctrl Pts',(141.883923502978,-3.60877264417177,338.34154800432));
#52356=CARTESIAN_POINT('Ctrl Pts',(141.87621587781,-3.51627240391097,338.441445517749));
#52357=CARTESIAN_POINT('Ctrl Pts',(141.868508252642,-3.41970995802508,338.53740315405));
#52358=CARTESIAN_POINT('Ctrl Pts',(141.860800627474,-3.31947139594085,338.629089791398));
#52359=CARTESIAN_POINT('Ctrl Pts',(141.853081740675,-3.21908637504751,338.720910392318));
#52360=CARTESIAN_POINT('Ctrl Pts',(141.845362853877,-3.11501481747229,338.808447280764));
#52361=CARTESIAN_POINT('Ctrl Pts',(141.837643967079,-3.00767429655744,338.891410848051));
#52362=CARTESIAN_POINT('Ctrl Pts',(141.833943799974,-2.95621896693819,338.931180710026));
#52363=CARTESIAN_POINT('Ctrl Pts',(141.83024363287,-2.90401286654154,338.969900317586));
#52364=CARTESIAN_POINT('Ctrl Pts',(141.826543465765,-2.8511040643387,339.00754147537));
#52365=CARTESIAN_POINT('Ctrl Pts',(141.818768386987,-2.73992797592005,339.0866360024));
#52366=CARTESIAN_POINT('Ctrl Pts',(141.810993308208,-2.62528238681406,339.161225684943));
#52367=CARTESIAN_POINT('Ctrl Pts',(141.80321822943,-2.50756844823521,339.230990846116));
#52368=CARTESIAN_POINT('Ctrl Pts',(141.795452718381,-2.38999936415181,339.300670156816));
#52369=CARTESIAN_POINT('Ctrl Pts',(141.787687207332,-2.26936977639406,339.365536561453));
#52370=CARTESIAN_POINT('Ctrl Pts',(141.779921696283,-2.14611198114213,339.425312014638));
#52371=CARTESIAN_POINT('Ctrl Pts',(141.77216388476,-2.02297639635301,339.485028200287));
#52372=CARTESIAN_POINT('Ctrl Pts',(141.764406073238,-1.89721813934193,339.539663310216));
#52373=CARTESIAN_POINT('Ctrl Pts',(141.756648261716,-1.76929611732149,339.588984017376));
#52374=CARTESIAN_POINT('Ctrl Pts',(141.748896288193,-1.64147036067944,339.638267609139));
#52375=CARTESIAN_POINT('Ctrl Pts',(141.74114431467,-1.51148444332078,339.68224461841));
#52376=CARTESIAN_POINT('Ctrl Pts',(141.733392341147,-1.37981904371207,339.720729018818));
#52377=CARTESIAN_POINT('Ctrl Pts',(141.725643650589,-1.24820940447816,339.75919712106));
#52378=CARTESIAN_POINT('Ctrl Pts',(141.717894960032,-1.11492207203931,339.792177131502));
#52379=CARTESIAN_POINT('Ctrl Pts',(141.710146269474,-0.980454542108751,
339.819532337619));
#52380=CARTESIAN_POINT('Ctrl Pts',(141.702399191096,-0.846014989270887,
339.846881852258));
#52381=CARTESIAN_POINT('Ctrl Pts',(141.694652112719,-0.710396110145814,
339.868608812485));
#52382=CARTESIAN_POINT('Ctrl Pts',(141.686905034341,-0.574106908938165,
339.884627347056));
#52383=CARTESIAN_POINT('Ctrl Pts',(141.679157891035,-0.437816565495971,
339.900646015878));
#52384=CARTESIAN_POINT('Ctrl Pts',(141.671410747729,-0.300856276967944,
339.910956117993));
#52385=CARTESIAN_POINT('Ctrl Pts',(141.663663604423,-0.163741113026549,
339.91552356422));
#52386=CARTESIAN_POINT('Ctrl Pts',(141.655914719395,-0.0265951226849824,
339.920092037306));
#52387=CARTESIAN_POINT('Ctrl Pts',(141.648165834367,0.110705421775169,339.918915272406));
#52388=CARTESIAN_POINT('Ctrl Pts',(141.640416949339,0.247644898413444,339.912011305646));
#52389=CARTESIAN_POINT('Ctrl Pts',(141.632659839564,0.38472972402698,339.905100010943));
#52390=CARTESIAN_POINT('Ctrl Pts',(141.62490272979,0.521452325263485,339.892449390898));
#52391=CARTESIAN_POINT('Ctrl Pts',(141.617145620015,0.657301097510161,339.874129494557));
#52392=CARTESIAN_POINT('Ctrl Pts',(141.609384365089,0.793222462997171,339.855799808649));
#52393=CARTESIAN_POINT('Ctrl Pts',(141.601623110163,0.928268684415273,339.831794878306));
#52394=CARTESIAN_POINT('Ctrl Pts',(141.593861855236,1.06193879055035,339.802235840484));
#52395=CARTESIAN_POINT('Ctrl Pts',(141.586088184832,1.19582272529216,339.772629517834));
#52396=CARTESIAN_POINT('Ctrl Pts',(141.578314514427,1.32832576784411,339.73745143367));
#52397=CARTESIAN_POINT('Ctrl Pts',(141.570540844022,1.45896168153539,339.696872776041));
#52398=CARTESIAN_POINT('Ctrl Pts',(141.563129039845,1.58351646201547,339.658183064686));
#52399=CARTESIAN_POINT('Ctrl Pts',(141.555717235668,1.70637376017856,339.614584354454));
#52400=CARTESIAN_POINT('Ctrl Pts',(141.548305431491,1.82713111825514,339.566264878345));
#52401=CARTESIAN_POINT('Ctrl Pts',(141.540530352713,1.95380715416844,339.515577120775));
#52402=CARTESIAN_POINT('Ctrl Pts',(141.532755273934,2.07857251614802,339.459533956218));
#52403=CARTESIAN_POINT('Ctrl Pts',(141.524980195156,2.2009412951417,339.398299725785));
#52404=CARTESIAN_POINT('Ctrl Pts',(141.517214684107,2.3231594915624,339.337140847971));
#52405=CARTESIAN_POINT('Ctrl Pts',(141.509449173058,2.44298662674593,339.270803787689));
#52406=CARTESIAN_POINT('Ctrl Pts',(141.501683662009,2.55995494612406,339.199501605705));
#52407=CARTESIAN_POINT('Ctrl Pts',(141.493925850487,2.67680729107278,339.128270120042));
#52408=CARTESIAN_POINT('Ctrl Pts',(141.486168038964,2.79080612947718,339.052083511731));
#52409=CARTESIAN_POINT('Ctrl Pts',(141.478410227442,2.90150691061789,338.971201418984));
#52410=CARTESIAN_POINT('Ctrl Pts',(141.470658253919,3.01212438591053,338.890380192575));
#52411=CARTESIAN_POINT('Ctrl Pts',(141.462906280396,3.11944842968799,338.804870744657));
#52412=CARTESIAN_POINT('Ctrl Pts',(141.455154306873,3.22306248570729,338.714976618463));
#52413=CARTESIAN_POINT('Ctrl Pts',(141.447405616315,3.32663266111236,338.625120562485));
#52414=CARTESIAN_POINT('Ctrl Pts',(141.439656925758,3.42649567909903,338.530883777119));
#52415=CARTESIAN_POINT('Ctrl Pts',(141.4319082352,3.52226735171192,338.432610634133));
#52416=CARTESIAN_POINT('Ctrl Pts',(141.424161156822,3.61801909822841,338.334357937695));
#52417=CARTESIAN_POINT('Ctrl Pts',(141.416414078445,3.70968091991194,338.232070833809));
#52418=CARTESIAN_POINT('Ctrl Pts',(141.408667000067,3.7969051544197,338.12613088511));
#52419=CARTESIAN_POINT('Ctrl Pts',(141.400919856761,3.88413011995038,338.020190048533));
#52420=CARTESIAN_POINT('Ctrl Pts',(141.393172713455,3.96691717567762,337.910596607839));
#52421=CARTESIAN_POINT('Ctrl Pts',(141.385425570149,4.04495892152719,337.79776524849));
#52422=CARTESIAN_POINT('Ctrl Pts',(141.377676685121,4.12301821281847,337.684908522256));
#52423=CARTESIAN_POINT('Ctrl Pts',(141.369927800093,4.19632984901999,337.56881275023));
#52424=CARTESIAN_POINT('Ctrl Pts',(141.362178915065,4.26462996447618,337.449921290285));
#52425=CARTESIAN_POINT('Ctrl Pts',(141.35442180529,4.33300257438036,337.330903637717));
#52426=CARTESIAN_POINT('Ctrl Pts',(141.346664695515,4.3963528427654,337.209084709089));
#52427=CARTESIAN_POINT('Ctrl Pts',(141.338907585741,4.45446281675794,337.084932631195));
#52428=CARTESIAN_POINT('Ctrl Pts',(141.331146330815,4.51260384286263,336.9607142104));
#52429=CARTESIAN_POINT('Ctrl Pts',(141.323385075888,4.56549884417424,336.834160516513));
#52430=CARTESIAN_POINT('Ctrl Pts',(141.315623820962,4.61297858307357,336.705758381074));
#52431=CARTESIAN_POINT('Ctrl Pts',(141.307850150558,4.66053427408147,336.577150844065));
#52432=CARTESIAN_POINT('Ctrl Pts',(141.300076480153,4.70265727196453,336.446689328896));
#52433=CARTESIAN_POINT('Ctrl Pts',(141.292302809748,4.73922840184171,336.314875362031));
#52434=CARTESIAN_POINT('Ctrl Pts',(141.284891005571,4.77409713682437,336.189197367038));
#52435=CARTESIAN_POINT('Ctrl Pts',(141.277479201394,4.80391918483866,336.062290280168));
#52436=CARTESIAN_POINT('Ctrl Pts',(141.270067397217,4.82863504203796,335.934594400424));
#52437=CARTESIAN_POINT('Ctrl Pts',(141.262292318439,4.8545622970235,335.800639765225));
#52438=CARTESIAN_POINT('Ctrl Pts',(141.25451723966,4.87495210072176,335.665393738487));
#52439=CARTESIAN_POINT('Ctrl Pts',(141.246742160882,4.88967969780799,335.529353865901));
#52440=CARTESIAN_POINT('Ctrl Pts',(141.238976649833,4.90438917164842,335.393481399039));
#52441=CARTESIAN_POINT('Ctrl Pts',(141.231211138784,4.91345026094549,335.256817414925));
#52442=CARTESIAN_POINT('Ctrl Pts',(141.223445627735,4.91678900420613,335.11987055776));
#52443=CARTESIAN_POINT('Ctrl Pts',(141.215687816213,4.92012443709311,334.983059483803));
#52444=CARTESIAN_POINT('Ctrl Pts',(141.20793000469,4.91774880550751,334.845966483187));
#52445=CARTESIAN_POINT('Ctrl Pts',(141.200172193168,4.90963987285681,334.709105893228));
#52446=CARTESIAN_POINT('Ctrl Pts',(141.192420219645,4.90153704243507,334.572348295204));
#52447=CARTESIAN_POINT('Ctrl Pts',(141.184668246122,4.88770952175685,334.435823148333));
#52448=CARTESIAN_POINT('Ctrl Pts',(141.176916272599,4.86818714431858,334.30004500831));
#52449=CARTESIAN_POINT('Ctrl Pts',(141.169167582041,4.84867303461875,334.16432437041));
#52450=CARTESIAN_POINT('Ctrl Pts',(141.161418891484,4.8234689205225,334.029350496234));
#52451=CARTESIAN_POINT('Ctrl Pts',(141.153670200926,4.79265648544831,333.895632816953));
#52452=CARTESIAN_POINT('Ctrl Pts',(141.145923122548,4.76185046115863,333.761942958753));
#52453=CARTESIAN_POINT('Ctrl Pts',(141.138176044171,4.72543852456782,333.629509156234));
#52454=CARTESIAN_POINT('Ctrl Pts',(141.130428965793,4.68355339979543,333.498830251516));
#52455=CARTESIAN_POINT('Ctrl Pts',(141.122681822487,4.6416679239854,333.368150251582));
#52456=CARTESIAN_POINT('Ctrl Pts',(141.114934679181,4.59430928780583,333.239225551006));
#52457=CARTESIAN_POINT('Ctrl Pts',(141.107187535875,4.54165985729162,333.112539059168));
#52458=CARTESIAN_POINT('Ctrl Pts',(141.099438650847,4.48899859006762,332.985824085517));
#52459=CARTESIAN_POINT('Ctrl Pts',(141.091689765819,4.43104431154616,332.861348682783));
#52460=CARTESIAN_POINT('Ctrl Pts',(141.083940880791,4.368027057974,332.739574667611));
#52461=CARTESIAN_POINT('Ctrl Pts',(141.076183771016,4.30494291723782,332.617671400241));
#52462=CARTESIAN_POINT('Ctrl Pts',(141.068426661242,4.23678524652287,332.498475595788));
#52463=CARTESIAN_POINT('Ctrl Pts',(141.060669551467,4.16382975683014,332.382423865742));
#52464=CARTESIAN_POINT('Ctrl Pts',(141.052908296541,4.09083528205633,332.266310121363));
#52465=CARTESIAN_POINT('Ctrl Pts',(141.045147041614,4.01303810128669,332.153344120883));
#52466=CARTESIAN_POINT('Ctrl Pts',(141.037385786688,3.93075601736213,332.043931632308));
#52467=CARTESIAN_POINT('Ctrl Pts',(141.029612116284,3.84834230891896,331.934344119408));
#52468=CARTESIAN_POINT('Ctrl Pts',(141.021838445879,3.76142960871022,331.828321780095));
#52469=CARTESIAN_POINT('Ctrl Pts',(141.014064775474,3.67037516867392,331.726236235816));
#52470=CARTESIAN_POINT('Ctrl Pts',(141.006652971297,3.58355933472722,331.628902798184));
#52471=CARTESIAN_POINT('Ctrl Pts',(140.99924116712,3.49297887930251,331.535148095149));
#52472=CARTESIAN_POINT('Ctrl Pts',(140.991829362943,3.39897185827788,331.445260435822));
#52473=CARTESIAN_POINT('Ctrl Pts',(140.984054284164,3.300357273121,331.350967114549));
#52474=CARTESIAN_POINT('Ctrl Pts',(140.976279205386,3.19766009663694,331.260631508139));
#52475=CARTESIAN_POINT('Ctrl Pts',(140.968504126608,3.09123121334857,331.174627776527));
#52476=CARTESIAN_POINT('Ctrl Pts',(140.960738615559,2.98493329757667,331.088729877982));
#52477=CARTESIAN_POINT('Ctrl Pts',(140.95297310451,2.87491311308065,331.0071534911));
#52478=CARTESIAN_POINT('Ctrl Pts',(140.945207593461,2.76155836481314,330.930236068243));
#52479=CARTESIAN_POINT('Ctrl Pts',(140.937449781938,2.6483160081081,330.853394909234));
#52480=CARTESIAN_POINT('Ctrl Pts',(140.929691970416,2.53174598857351,330.781203739487));
#52481=CARTESIAN_POINT('Ctrl Pts',(140.921934158894,2.41226878993646,330.713959595664));
#52482=CARTESIAN_POINT('Ctrl Pts',(140.914182185371,2.29288150168152,330.646766055192));
#52483=CARTESIAN_POINT('Ctrl Pts',(140.906430211848,2.17059172818094,330.584512321546));
#52484=CARTESIAN_POINT('Ctrl Pts',(140.898678238325,2.04584831491121,330.527451762711));
#52485=CARTESIAN_POINT('Ctrl Pts',(140.890929547767,1.92115773055034,330.470415369057));
#52486=CARTESIAN_POINT('Ctrl Pts',(140.88318085721,1.79401592786528,330.418567938191));
#52487=CARTESIAN_POINT('Ctrl Pts',(140.875432166652,1.66489550198094,330.372116463222));
#52488=CARTESIAN_POINT('Ctrl Pts',(140.867685088274,1.53580194067945,330.32567465287));
#52489=CARTESIAN_POINT('Ctrl Pts',(140.859938009896,1.4047309425843,330.284626697571));
#52490=CARTESIAN_POINT('Ctrl Pts',(140.852190931519,1.27217381931185,330.249130938875));
#52491=CARTESIAN_POINT('Ctrl Pts',(140.844443788213,1.13961558508326,330.21363488269));
#52492=CARTESIAN_POINT('Ctrl Pts',(140.836696644907,1.00557157840645,330.183691217026));
#52493=CARTESIAN_POINT('Ctrl Pts',(140.828949501601,0.870546576806936,330.159407916369));
#52494=CARTESIAN_POINT('Ctrl Pts',(140.821200616573,0.735491218720127,330.13511915631));
#52495=CARTESIAN_POINT('Ctrl Pts',(140.813451731545,0.59945481147108,330.116493362703));
#52496=CARTESIAN_POINT('Ctrl Pts',(140.805702846517,0.462950192340578,330.103587008645));
#52497=CARTESIAN_POINT('Ctrl Pts',(140.797945736742,0.326300685797207,330.090666955649));
#52498=CARTESIAN_POINT('Ctrl Pts',(140.790188626967,0.189182364391768,330.08347850579));
#52499=CARTESIAN_POINT('Ctrl Pts',(140.782431517193,0.0521115870834784,
330.082026083336));
#52500=CARTESIAN_POINT('Ctrl Pts',(140.774670262266,-0.0850324364653443,
330.080572884753));
#52501=CARTESIAN_POINT('Ctrl Pts',(140.76690900734,-0.222128474808211,330.084861808945));
#52502=CARTESIAN_POINT('Ctrl Pts',(140.759147752414,-0.358663327620432,
330.094845193073));
#52503=CARTESIAN_POINT('Ctrl Pts',(140.751374082009,-0.49541659170078,330.104844547362));
#52504=CARTESIAN_POINT('Ctrl Pts',(140.743600411605,-0.631606487849166,
330.120556519806));
#52505=CARTESIAN_POINT('Ctrl Pts',(140.7358267412,-0.766727182138997,330.141881795317));
#52506=CARTESIAN_POINT('Ctrl Pts',(140.728414937023,-0.89555797560102,330.162214374123));
#52507=CARTESIAN_POINT('Ctrl Pts',(140.721003132846,-1.02341658748591,330.187649362083));
#52508=CARTESIAN_POINT('Ctrl Pts',(140.713591328669,-1.14987763108054,330.218058501399));
#52509=CARTESIAN_POINT('Ctrl Pts',(140.705816249891,-1.28253690713004,330.249958083217));
#52510=CARTESIAN_POINT('Ctrl Pts',(140.698041171112,-1.41407738074459,330.287432549786));
#52511=CARTESIAN_POINT('Ctrl Pts',(140.690266092334,-1.54399452910135,330.330389314236));
#52512=CARTESIAN_POINT('Ctrl Pts',(140.682500581285,-1.67375180613595,330.373293217652));
#52513=CARTESIAN_POINT('Ctrl Pts',(140.674735070236,-1.80188936500791,330.421665874178));
#52514=CARTESIAN_POINT('Ctrl Pts',(140.666969559187,-1.92791362543145,330.475363869285));
#52515=CARTESIAN_POINT('Ctrl Pts',(140.659211747664,-2.05381293243391,330.529008622673));
#52516=CARTESIAN_POINT('Ctrl Pts',(140.651453936142,-2.17760275356042,330.587968054733));
#52517=CARTESIAN_POINT('Ctrl Pts',(140.64369612462,-2.29880575647429,330.65204931531));
#52518=CARTESIAN_POINT('Ctrl Pts',(140.635944151097,-2.41991755028547,330.716082352706));
#52519=CARTESIAN_POINT('Ctrl Pts',(140.628192177574,-2.53844605646218,330.785229364786));
#52520=CARTESIAN_POINT('Ctrl Pts',(140.620440204051,-2.65393531641671,330.85925001977));
#52521=CARTESIAN_POINT('Ctrl Pts',(140.612691513493,-2.76937566660064,330.933239326962));
#52522=CARTESIAN_POINT('Ctrl Pts',(140.604942822936,-2.88177900216035,331.012097961445));
#52523=CARTESIAN_POINT('Ctrl Pts',(140.597194132378,-2.99071550983518,331.095540523743));
#52524=CARTESIAN_POINT('Ctrl Pts',(140.589447054,-3.09962935235966,331.17896572512));
#52525=CARTESIAN_POINT('Ctrl Pts',(140.581699975622,-3.20507749161174,331.266972719751));
#52526=CARTESIAN_POINT('Ctrl Pts',(140.573952897245,-3.30666089789679,331.359234040917));
#52527=CARTESIAN_POINT('Ctrl Pts',(140.566205753939,-3.40824515554856,331.45149613532));
#52528=CARTESIAN_POINT('Ctrl Pts',(140.558458610633,-3.50596432628149,331.54801236458));
#52529=CARTESIAN_POINT('Ctrl Pts',(140.550711467327,-3.59945444796407,331.648416681696));
#52530=CARTESIAN_POINT('Ctrl Pts',(140.542962582299,-3.69296558821096,331.748843571834));
#52531=CARTESIAN_POINT('Ctrl Pts',(140.535213697271,-3.78224552114894,331.853160003231));
#52532=CARTESIAN_POINT('Ctrl Pts',(140.527464812243,-3.86696923166633,331.960965280908));
#52533=CARTESIAN_POINT('Ctrl Pts',(140.519707702468,-3.95178286880537,332.068884984221));
#52534=CARTESIAN_POINT('Ctrl Pts',(140.511950592694,-4.03203038121057,332.18030062329));
#52535=CARTESIAN_POINT('Ctrl Pts',(140.504193482919,-4.10742861695991,332.294780375075));
#52536=CARTESIAN_POINT('Ctrl Pts',(140.496432227993,-4.18286714311568,332.409321301179));
#52537=CARTESIAN_POINT('Ctrl Pts',(140.488670973067,-4.25345102817896,332.526929267616));
#52538=CARTESIAN_POINT('Ctrl Pts',(140.48090971814,-4.31894263070444,332.647146920187));
#52539=CARTESIAN_POINT('Ctrl Pts',(140.473136047736,-4.38453899845021,332.767556881824));
#52540=CARTESIAN_POINT('Ctrl Pts',(140.465362377331,-4.44502663300238,332.890584520821));
#52541=CARTESIAN_POINT('Ctrl Pts',(140.457588706926,-4.50021531477412,333.015750725546));
#52542=CARTESIAN_POINT('Ctrl Pts',(140.450176902749,-4.55283495013235,333.135090413329));
#52543=CARTESIAN_POINT('Ctrl Pts',(140.442765098572,-4.60063775754223,333.256373779252));
#52544=CARTESIAN_POINT('Ctrl Pts',(140.435353294395,-4.64350139056349,333.379173698901));
#52545=CARTESIAN_POINT('Ctrl Pts',(140.426243114137,-4.69618700043698,333.530112576524));
#52546=CARTESIAN_POINT('Ctrl Pts',(140.417132933879,-4.74154784846308,333.683732773459));
#52547=CARTESIAN_POINT('Ctrl Pts',(140.408022753621,-4.77934383766862,333.839372779985));
#52548=CARTESIAN_POINT('Ctrl Pts',(140.398953508521,-4.8169699965573,333.994313442688));
#52549=CARTESIAN_POINT('Ctrl Pts',(140.389884263422,-4.84709904108127,334.151255712227));
#52550=CARTESIAN_POINT('Ctrl Pts',(140.380815018322,-4.86954082486031,334.30952536794));
#52551=CARTESIAN_POINT('Ctrl Pts',(140.371821738399,-4.89179463333796,334.46646933642));
#52552=CARTESIAN_POINT('Ctrl Pts',(140.362828458477,-4.90648934504363,334.62471843884));
#52553=CARTESIAN_POINT('Ctrl Pts',(140.353835178554,-4.91348676092799,334.783595488297));
#52554=CARTESIAN_POINT('Ctrl Pts',(140.349829244556,-4.91660366448597,334.854365105098));
#52555=CARTESIAN_POINT('Ctrl Pts',(140.345823310558,-4.91819395609712,334.925259061498));
#52556=CARTESIAN_POINT('Ctrl Pts',(140.34181737656,-4.91824854457842,334.996216317635));
#52557=CARTESIAN_POINT('',(138.591817376453,-4.91824901572479,335.003111562653));
#52558=CARTESIAN_POINT('Ctrl Pts',(140.341817376508,-4.91824854457913,334.996216318558));
#52559=CARTESIAN_POINT('Ctrl Pts',(140.334071246083,-4.91835410033541,335.133423811481));
#52560=CARTESIAN_POINT('Ctrl Pts',(140.326325115657,-4.91271371046934,335.270696396518));
#52561=CARTESIAN_POINT('Ctrl Pts',(140.318578985232,-4.90133781675005,335.407517691145));
#52562=CARTESIAN_POINT('Ctrl Pts',(140.310833980913,-4.8899635768191,335.544319095162));
#52563=CARTESIAN_POINT('Ctrl Pts',(140.303088976593,-4.87285552357827,335.680668950269));
#52564=CARTESIAN_POINT('Ctrl Pts',(140.295343972274,-4.85007611703448,335.816054361836));
#52565=CARTESIAN_POINT('Ctrl Pts',(140.287598422206,-4.82729510535177,335.951449313265));
#52566=CARTESIAN_POINT('Ctrl Pts',(140.279852872139,-4.79884200950008,336.085879300777));
#52567=CARTESIAN_POINT('Ctrl Pts',(140.272107322072,-4.76483065272342,336.218840397003));
#52568=CARTESIAN_POINT('Ctrl Pts',(140.264359554399,-4.73080955825472,336.351839560932));
#52569=CARTESIAN_POINT('Ctrl Pts',(140.256611786726,-4.69122713253466,336.483368618452));
#52570=CARTESIAN_POINT('Ctrl Pts',(140.248864019053,-4.64624731565618,336.612937985249));
#52571=CARTESIAN_POINT('Ctrl Pts',(140.241107324421,-4.60121567314095,336.742656641557));
#52572=CARTESIAN_POINT('Ctrl Pts',(140.233350629789,-4.55077434550523,336.87041072746));
#52573=CARTESIAN_POINT('Ctrl Pts',(140.225593935157,-4.49513599603105,336.995729300202));
#52574=CARTESIAN_POINT('Ctrl Pts',(140.21783269349,-4.43946503092494,337.121121335664));
#52575=CARTESIAN_POINT('Ctrl Pts',(140.210071451823,-4.37859114722553,337.244074663837));
#52576=CARTESIAN_POINT('Ctrl Pts',(140.202310210156,-4.31277293739774,337.364143111774));
#52577=CARTESIAN_POINT('Ctrl Pts',(140.194535978122,-4.24684456442897,337.484412524117));
#52578=CARTESIAN_POINT('Ctrl Pts',(140.186761746087,-4.17595553096736,337.601787073513));
#52579=CARTESIAN_POINT('Ctrl Pts',(140.178987514052,-4.10040821333633,337.715848955024));
#52580=CARTESIAN_POINT('Ctrl Pts',(140.171696762742,-4.02955919537855,337.822817310021));
#52581=CARTESIAN_POINT('Ctrl Pts',(140.164406011431,-3.9546138388079,337.926872302788));
#52582=CARTESIAN_POINT('Ctrl Pts',(140.157115260121,-3.87585246189446,338.027697269564));
#52583=CARTESIAN_POINT('Ctrl Pts',(140.149340181342,-3.79185893583497,338.135220078411));
#52584=CARTESIAN_POINT('Ctrl Pts',(140.141565102564,-3.70325499232363,338.239414958504));
#52585=CARTESIAN_POINT('Ctrl Pts',(140.133790023785,-3.61033392100321,338.339861081146));
#52586=CARTESIAN_POINT('Ctrl Pts',(140.126024512736,-3.51752719497677,338.440183598439));
#52587=CARTESIAN_POINT('Ctrl Pts',(140.118259001687,-3.42041417438976,338.536766252812));
#52588=CARTESIAN_POINT('Ctrl Pts',(140.110493490638,-3.31932987578775,338.62921923259));
#52589=CARTESIAN_POINT('Ctrl Pts',(140.102735679116,-3.21834580256201,338.72158054497));
#52590=CARTESIAN_POINT('Ctrl Pts',(140.094977867594,-3.11339857380751,338.809820069109));
#52591=CARTESIAN_POINT('Ctrl Pts',(140.087220056072,-3.00486146800485,338.893583262318));
#52592=CARTESIAN_POINT('Ctrl Pts',(140.079468082549,-2.89640603981643,338.977283421067));
#52593=CARTESIAN_POINT('Ctrl Pts',(140.071716109026,-2.78436641996992,339.056513716034));
#52594=CARTESIAN_POINT('Ctrl Pts',(140.063964135503,-2.66915024685847,339.130958729181));
#52595=CARTESIAN_POINT('Ctrl Pts',(140.056215444945,-2.55398286786457,339.20537221482));
#52596=CARTESIAN_POINT('Ctrl Pts',(140.048466754388,-2.43564193887897,339.275004237657));
#52597=CARTESIAN_POINT('Ctrl Pts',(140.04071806383,-2.31456528433585,339.339581847027));
#52598=CARTESIAN_POINT('Ctrl Pts',(140.032970985452,-2.19351382080196,339.404146020487));
#52599=CARTESIAN_POINT('Ctrl Pts',(140.025223907074,-2.06972810853936,339.46365768838));
#52600=CARTESIAN_POINT('Ctrl Pts',(140.017476828696,-1.94367150558177,339.5178893458));
#52601=CARTESIAN_POINT('Ctrl Pts',(140.009729685391,-1.81761384614856,339.572121457732));
#52602=CARTESIAN_POINT('Ctrl Pts',(140.001982542085,-1.68928561711503,339.621073316455));
#52603=CARTESIAN_POINT('Ctrl Pts',(139.994235398779,-1.55917076163119,339.664565317216));
#52604=CARTESIAN_POINT('Ctrl Pts',(139.986486513751,-1.42902665356533,339.708067095902));
#52605=CARTESIAN_POINT('Ctrl Pts',(139.978737628723,-1.29709549040808,339.746106450163));
#52606=CARTESIAN_POINT('Ctrl Pts',(139.970988743695,-1.16387661422478,339.778553577115));
#52607=CARTESIAN_POINT('Ctrl Pts',(139.96323163392,-1.03051633814994,339.811035143783));
#52608=CARTESIAN_POINT('Ctrl Pts',(139.955474524145,-0.895865999125841,
339.837912533483));
#52609=CARTESIAN_POINT('Ctrl Pts',(139.947717414371,-0.760435926352462,
339.859106941035));
#52610=CARTESIAN_POINT('Ctrl Pts',(139.939956159445,-0.62493348407827,339.8803126742));
#52611=CARTESIAN_POINT('Ctrl Pts',(139.932194904518,-0.488650865980823,
339.895829329916));
#52612=CARTESIAN_POINT('Ctrl Pts',(139.924433649592,-0.352102783357451,
339.90563010147));
#52613=CARTESIAN_POINT('Ctrl Pts',(139.916659979188,-0.21533626830303,339.915446551065));
#52614=CARTESIAN_POINT('Ctrl Pts',(139.908886308783,-0.0783038310392436,
339.919528833328));
#52615=CARTESIAN_POINT('Ctrl Pts',(139.901112638378,0.0584796615429201,
339.9179023162));
#52616=CARTESIAN_POINT('Ctrl Pts',(139.893700834201,0.188895849637867,339.916351513836));
#52617=CARTESIAN_POINT('Ctrl Pts',(139.886289030024,0.319085460811378,339.90961145535));
#52618=CARTESIAN_POINT('Ctrl Pts',(139.878877225847,0.448609063566037,339.897747744687));
#52619=CARTESIAN_POINT('Ctrl Pts',(139.871102147068,0.584481003922257,339.885302558225));
#52620=CARTESIAN_POINT('Ctrl Pts',(139.86332706829,0.720049379420246,339.867179440163));
#52621=CARTESIAN_POINT('Ctrl Pts',(139.855551989512,0.85480159037561,339.843397289464));
#52622=CARTESIAN_POINT('Ctrl Pts',(139.847786478463,0.989387980156876,339.819644404216));
#52623=CARTESIAN_POINT('Ctrl Pts',(139.840020967414,1.12315982250328,339.790246409582));
#52624=CARTESIAN_POINT('Ctrl Pts',(139.832255456365,1.25560801978681,339.755274078657));
#52625=CARTESIAN_POINT('Ctrl Pts',(139.824497644842,1.38792489429724,339.7203364229));
#52626=CARTESIAN_POINT('Ctrl Pts',(139.81673983332,1.51892036000345,339.679835528984));
#52627=CARTESIAN_POINT('Ctrl Pts',(139.808982021798,1.64809427199002,339.633893431353));
#52628=CARTESIAN_POINT('Ctrl Pts',(139.801230048275,1.77717097651059,339.587985906607));
#52629=CARTESIAN_POINT('Ctrl Pts',(139.793478074752,1.90442848898363,339.536645458858));
#52630=CARTESIAN_POINT('Ctrl Pts',(139.785726101229,2.02938097112651,339.480044189127));
#52631=CARTESIAN_POINT('Ctrl Pts',(139.777977410671,2.15428053581937,339.423466890067));
#52632=CARTESIAN_POINT('Ctrl Pts',(139.770228720114,2.27687665643151,339.361633361231));
#52633=CARTESIAN_POINT('Ctrl Pts',(139.762480029556,2.39670287100438,339.294764069261));
#52634=CARTESIAN_POINT('Ctrl Pts',(139.754732951178,2.51650415473262,339.227908690006));
#52635=CARTESIAN_POINT('Ctrl Pts',(139.7469858728,2.63353633761827,339.156019821988));
#52636=CARTESIAN_POINT('Ctrl Pts',(139.739238794422,2.74735735631053,339.079363996903));
#52637=CARTESIAN_POINT('Ctrl Pts',(139.731491651117,2.8611793289324,339.002707529368));
#52638=CARTESIAN_POINT('Ctrl Pts',(139.723744507811,2.97178975947713,338.921284243423));
#52639=CARTESIAN_POINT('Ctrl Pts',(139.715997364505,3.07877572506905,338.835403902749));
#52640=CARTESIAN_POINT('Ctrl Pts',(139.708248479477,3.18578574337701,338.749504254353));
#52641=CARTESIAN_POINT('Ctrl Pts',(139.700499594449,3.28916937050212,338.659145801915));
#52642=CARTESIAN_POINT('Ctrl Pts',(139.692750709421,3.38854722978495,338.564678209042));
#52643=CARTESIAN_POINT('Ctrl Pts',(139.684993599646,3.4880305697548,338.470110347289));
#52644=CARTESIAN_POINT('Ctrl Pts',(139.677236489871,3.58349936483849,338.371424902356));
#52645=CARTESIAN_POINT('Ctrl Pts',(139.669479380097,3.67461117766518,338.269008374948));
#52646=CARTESIAN_POINT('Ctrl Pts',(139.66171812517,3.76577167773145,338.166537119422));
#52647=CARTESIAN_POINT('Ctrl Pts',(139.653956870244,3.85257030910377,338.060331111155));
#52648=CARTESIAN_POINT('Ctrl Pts',(139.646195615318,3.93470598962873,337.950808675207));
#52649=CARTESIAN_POINT('Ctrl Pts',(139.638421944913,4.01697306047458,337.841111039056));
#52650=CARTESIAN_POINT('Ctrl Pts',(139.630648274509,4.09456205344434,337.728086696275));
#52651=CARTESIAN_POINT('Ctrl Pts',(139.622874604104,4.16721567696262,337.612182337467));
#52652=CARTESIAN_POINT('Ctrl Pts',(139.615462799927,4.23648725682591,337.501673354448));
#52653=CARTESIAN_POINT('Ctrl Pts',(139.60805099575,4.30127246673542,337.388546700549));
#52654=CARTESIAN_POINT('Ctrl Pts',(139.600639191573,4.36138867285053,337.273207405151));
#52655=CARTESIAN_POINT('Ctrl Pts',(139.592864112795,4.42445135330487,337.152214987305));
#52656=CARTESIAN_POINT('Ctrl Pts',(139.585089034016,4.4825750635807,337.028405189037));
#52657=CARTESIAN_POINT('Ctrl Pts',(139.577313955238,4.53549829911642,336.90221929367));
#52658=CARTESIAN_POINT('Ctrl Pts',(139.569548444189,4.58835640924168,336.776188678081));
#52659=CARTESIAN_POINT('Ctrl Pts',(139.56178293314,4.63602662809492,336.647788140201));
#52660=CARTESIAN_POINT('Ctrl Pts',(139.554017422091,4.67829296834463,336.517484090473));
#52661=CARTESIAN_POINT('Ctrl Pts',(139.546259610569,4.72051740139483,336.387309237589));
#52662=CARTESIAN_POINT('Ctrl Pts',(139.538501799046,4.75734849866355,336.255234998172));
#52663=CARTESIAN_POINT('Ctrl Pts',(139.530743987524,4.78861822440726,336.121747994594));
#52664=CARTESIAN_POINT('Ctrl Pts',(139.522992014001,4.81986441869061,335.988361444219));
#52665=CARTESIAN_POINT('Ctrl Pts',(139.515240040478,4.84555748291161,335.853564624869));
#52666=CARTESIAN_POINT('Ctrl Pts',(139.507488066955,4.8655792255192,335.71785922206));
#52667=CARTESIAN_POINT('Ctrl Pts',(139.499739376398,4.885592488907,335.582211290568));
#52668=CARTESIAN_POINT('Ctrl Pts',(139.49199068584,4.89993915077576,335.445655926812));
#52669=CARTESIAN_POINT('Ctrl Pts',(139.484241995282,4.90855217689696,335.308704695753));
#52670=CARTESIAN_POINT('Ctrl Pts',(139.476494916905,4.91716341100615,335.171781958542));
#52671=CARTESIAN_POINT('Ctrl Pts',(139.468747838527,4.92004335767285,335.034463907715));
#52672=CARTESIAN_POINT('Ctrl Pts',(139.461000760149,4.91717692324133,334.897266519367));
#52673=CARTESIAN_POINT('Ctrl Pts',(139.453253616843,4.91431046478634,334.760067981174));
#52674=CARTESIAN_POINT('Ctrl Pts',(139.445506473537,4.90569753733867,334.622990498267));
#52675=CARTESIAN_POINT('Ctrl Pts',(139.437759330231,4.89137517152524,334.486548937204));
#52676=CARTESIAN_POINT('Ctrl Pts',(139.430010445203,4.87704958573992,334.350076701182));
#52677=CARTESIAN_POINT('Ctrl Pts',(139.422261560175,4.85701204816055,334.214241060158));
#52678=CARTESIAN_POINT('Ctrl Pts',(139.414512675147,4.83135129589439,334.0795502631));
#52679=CARTESIAN_POINT('Ctrl Pts',(139.406755565372,4.80566330704062,333.944716503838));
#52680=CARTESIAN_POINT('Ctrl Pts',(139.398998455598,4.77434025405274,333.811030400492));
#52681=CARTESIAN_POINT('Ctrl Pts',(139.391241345823,4.73752184110986,333.678989073661));
#52682=CARTESIAN_POINT('Ctrl Pts',(139.383480090897,4.70068375358436,333.546877188167));
#52683=CARTESIAN_POINT('Ctrl Pts',(139.375718835971,4.65834457536707,333.416412202106));
#52684=CARTESIAN_POINT('Ctrl Pts',(139.367957581045,4.61069315209675,333.288073681577));
#52685=CARTESIAN_POINT('Ctrl Pts',(139.36018391064,4.5629655020787,333.159529861241));
#52686=CARTESIAN_POINT('Ctrl Pts',(139.352410240235,4.50990877711769,333.03311966455));
#52687=CARTESIAN_POINT('Ctrl Pts',(139.344636569831,4.45175937363502,332.909301183395));
#52688=CARTESIAN_POINT('Ctrl Pts',(139.337224765653,4.39631683887354,332.791246482325));
#52689=CARTESIAN_POINT('Ctrl Pts',(139.329812961476,4.33624521661356,332.675547893546));
#52690=CARTESIAN_POINT('Ctrl Pts',(139.322401157299,4.27178627105111,332.56257818239));
#52691=CARTESIAN_POINT('Ctrl Pts',(139.31462607852,4.20416800055442,332.444071489173));
#52692=CARTESIAN_POINT('Ctrl Pts',(139.306850999742,4.13150777459266,332.32819343514));
#52693=CARTESIAN_POINT('Ctrl Pts',(139.299075920964,4.05403516260341,332.215402728782));
#52694=CARTESIAN_POINT('Ctrl Pts',(139.291310409915,3.97665788559533,332.102750818569));
#52695=CARTESIAN_POINT('Ctrl Pts',(139.283544898866,3.89448022472525,331.993179015868));
#52696=CARTESIAN_POINT('Ctrl Pts',(139.275779387817,3.80777751134433,331.887121350486));
#52697=CARTESIAN_POINT('Ctrl Pts',(139.268021576294,3.72116076395599,331.781168841588));
#52698=CARTESIAN_POINT('Ctrl Pts',(139.260263764772,3.63002813845001,331.678723836771));
#52699=CARTESIAN_POINT('Ctrl Pts',(139.25250595325,3.53469791217641,331.580190980163));
#52700=CARTESIAN_POINT('Ctrl Pts',(139.244753979727,3.43943942492125,331.481732272655));
#52701=CARTESIAN_POINT('Ctrl Pts',(139.237002006204,3.33998989508302,331.387180133224));
#52702=CARTESIAN_POINT('Ctrl Pts',(139.229250032681,3.23670724048409,331.296905442485));
#52703=CARTESIAN_POINT('Ctrl Pts',(139.221501342123,3.13346832615099,331.206668983131));
#52704=CARTESIAN_POINT('Ctrl Pts',(139.213752651566,3.02639980943565,331.12070662622));
#52705=CARTESIAN_POINT('Ctrl Pts',(139.206003961008,2.91589560016169,331.039351579418));
#52706=CARTESIAN_POINT('Ctrl Pts',(139.19825688263,2.80541438221152,330.958013459214));
#52707=CARTESIAN_POINT('Ctrl Pts',(139.190509804252,2.69149920811127,330.88128097401));
#52708=CARTESIAN_POINT('Ctrl Pts',(139.182762725875,2.57457580512539,330.809446040657));
#52709=CARTESIAN_POINT('Ctrl Pts',(139.175015582569,2.45765142220858,330.737610505259));
#52710=CARTESIAN_POINT('Ctrl Pts',(139.167268439263,2.33771909316038,330.670672808193));
#52711=CARTESIAN_POINT('Ctrl Pts',(139.159521295957,2.21523181965056,330.608880433453));
#52712=CARTESIAN_POINT('Ctrl Pts',(139.151772410929,2.09271700840138,330.547074166477));
#52713=CARTESIAN_POINT('Ctrl Pts',(139.144023525901,1.96764645860009,330.490415699704));
#52714=CARTESIAN_POINT('Ctrl Pts',(139.136274640873,1.84049558838708,330.439105454889));
#52715=CARTESIAN_POINT('Ctrl Pts',(139.128517531098,1.71320975892637,330.387740748849));
#52716=CARTESIAN_POINT('Ctrl Pts',(139.120760421323,1.58383956126605,330.341735750927));
#52717=CARTESIAN_POINT('Ctrl Pts',(139.113003311549,1.45287863667205,330.301242001379));
#52718=CARTESIAN_POINT('Ctrl Pts',(139.105242056622,1.32184773074736,330.260726613267));
#52719=CARTESIAN_POINT('Ctrl Pts',(139.097480801696,1.18922478186493,330.225728441459));
#52720=CARTESIAN_POINT('Ctrl Pts',(139.08971954677,1.05551526260032,330.196348202365));
#52721=CARTESIAN_POINT('Ctrl Pts',(139.081945876365,0.92159185168082,330.166920964464));
#52722=CARTESIAN_POINT('Ctrl Pts',(139.074172205961,0.786578782169621,330.143129685555));
#52723=CARTESIAN_POINT('Ctrl Pts',(139.066398535556,0.650989200978109,330.12502347465));
#52724=CARTESIAN_POINT('Ctrl Pts',(139.058986731379,0.521711347413453,330.10776011222));
#52725=CARTESIAN_POINT('Ctrl Pts',(139.051574927202,0.391909734077998,330.095664475779));
#52726=CARTESIAN_POINT('Ctrl Pts',(139.044163123025,0.262028659770151,330.088734985367));
#52727=CARTESIAN_POINT('Ctrl Pts',(139.036388044247,0.125781727113219,330.081465859988));
#52728=CARTESIAN_POINT('Ctrl Pts',(139.028612965468,-0.0109832181841689,
330.079859130018));
#52729=CARTESIAN_POINT('Ctrl Pts',(139.02083788669,-0.147756205169704,330.083969979106));
#52730=CARTESIAN_POINT('Ctrl Pts',(139.013072375641,-0.284360884287172,
330.088075769532));
#52731=CARTESIAN_POINT('Ctrl Pts',(139.005306864592,-0.420973198440031,
330.097885128071));
#52732=CARTESIAN_POINT('Ctrl Pts',(138.997541353543,-0.5570791651115,330.113401401148));
#52733=CARTESIAN_POINT('Ctrl Pts',(138.989783542021,-0.693050182321493,
330.128902289796));
#52734=CARTESIAN_POINT('Ctrl Pts',(138.982025730498,-0.828515465290936,
330.150098788414));
#52735=CARTESIAN_POINT('Ctrl Pts',(138.974267918976,-0.96296250200261,330.176942226944));
#52736=CARTESIAN_POINT('Ctrl Pts',(138.966515945453,-1.09730836305528,330.203765464935));
#52737=CARTESIAN_POINT('Ctrl Pts',(138.95876397193,-1.23063712129286,330.236227108192));
#52738=CARTESIAN_POINT('Ctrl Pts',(138.951011998407,-1.36244320542227,330.274226880763));
#52739=CARTESIAN_POINT('Ctrl Pts',(138.943263307849,-1.49419346959636,330.312210560409));
#52740=CARTESIAN_POINT('Ctrl Pts',(138.935514617292,-1.62442196743454,330.355727596477));
#52741=CARTESIAN_POINT('Ctrl Pts',(138.927765926734,-1.75263533029214,330.404627059584));
#52742=CARTESIAN_POINT('Ctrl Pts',(138.920018848356,-1.88082201728869,330.453516348748));
#52743=CARTESIAN_POINT('Ctrl Pts',(138.912271769979,-2.00699403826913,330.50778569827));
#52744=CARTESIAN_POINT('Ctrl Pts',(138.904524691601,-2.13067552867567,330.567235077967));
#52745=CARTESIAN_POINT('Ctrl Pts',(138.896777548295,-2.25435805565244,330.626684955908));
#52746=CARTESIAN_POINT('Ctrl Pts',(138.889030404989,-2.37554965813174,330.691314781282));
#52747=CARTESIAN_POINT('Ctrl Pts',(138.881283261683,-2.49379707634702,330.760877543111));
#52748=CARTESIAN_POINT('Ctrl Pts',(138.873534376655,-2.61207107909245,330.830455944125));
#52749=CARTESIAN_POINT('Ctrl Pts',(138.865785491627,-2.72739924360139,330.904969290283));
#52750=CARTESIAN_POINT('Ctrl Pts',(138.858036606599,-2.83935575491062,330.98412625204));
#52751=CARTESIAN_POINT('Ctrl Pts',(138.850279496824,-2.95143109801757,331.063367231813));
#52752=CARTESIAN_POINT('Ctrl Pts',(138.84252238705,-3.06012731945807,331.147261446876));
#52753=CARTESIAN_POINT('Ctrl Pts',(138.834765277275,-3.16504984818297,331.235475790884));
#52754=CARTESIAN_POINT('Ctrl Pts',(138.827004022349,-3.27002844415259,331.323737273818));
#52755=CARTESIAN_POINT('Ctrl Pts',(138.819242767422,-3.37122904102209,331.41632322196));
#52756=CARTESIAN_POINT('Ctrl Pts',(138.811481512496,-3.4682934040009,331.512863076066));
#52757=CARTESIAN_POINT('Ctrl Pts',(138.803707842092,-3.56551303832708,331.609557362476));
#52758=CARTESIAN_POINT('Ctrl Pts',(138.795934171687,-3.65858295128743,331.710217906844));
#52759=CARTESIAN_POINT('Ctrl Pts',(138.788160501282,-3.74718415282704,331.81443976869));
#52760=CARTESIAN_POINT('Ctrl Pts',(138.780748697105,-3.83166094711786,331.913810077792));
#52761=CARTESIAN_POINT('Ctrl Pts',(138.773336892928,-3.91207552684104,332.016417380716));
#52762=CARTESIAN_POINT('Ctrl Pts',(138.765925088751,-3.98818878504526,332.121887202117));
#52763=CARTESIAN_POINT('Ctrl Pts',(138.758087643193,-4.06867303735473,332.233413891644));
#52764=CARTESIAN_POINT('Ctrl Pts',(138.750250197634,-4.14460103872594,332.348492846247));
#52765=CARTESIAN_POINT('Ctrl Pts',(138.742412752076,-4.21564609093278,332.466719301281));
#52766=CARTESIAN_POINT('Ctrl Pts',(138.734585232324,-4.28660116746858,332.584796027315));
#52767=CARTESIAN_POINT('Ctrl Pts',(138.726757712572,-4.3526854049202,332.706011997598));
#52768=CARTESIAN_POINT('Ctrl Pts',(138.718930192819,-4.41361341164634,332.829930942335));
#52769=CARTESIAN_POINT('Ctrl Pts',(138.711110983938,-4.4744767280467,332.953718316102));
#52770=CARTESIAN_POINT('Ctrl Pts',(138.703291775057,-4.53019454163685,333.080202611903));
#52771=CARTESIAN_POINT('Ctrl Pts',(138.695472566176,-4.58052586943205,333.208920486979));
#52772=CARTESIAN_POINT('Ctrl Pts',(138.687660059247,-4.6308140575474,333.337528036177));
#52773=CARTESIAN_POINT('Ctrl Pts',(138.679847552318,-4.67572481157235,333.468364999081));
#52774=CARTESIAN_POINT('Ctrl Pts',(138.67203504539,-4.71506416979987,333.600945698992));
#52775=CARTESIAN_POINT('Ctrl Pts',(138.66422801327,-4.75437595999206,333.733433489675));
#52776=CARTESIAN_POINT('Ctrl Pts',(138.65642098115,-4.78812402253395,333.867662217685));
#52777=CARTESIAN_POINT('Ctrl Pts',(138.64861394903,-4.8161635297853,334.003128936689));
#52778=CARTESIAN_POINT('Ctrl Pts',(138.640810107855,-4.84419157653209,334.138540286784));
#52779=CARTESIAN_POINT('Ctrl Pts',(138.63300626668,-4.86651563677257,334.275188246238));
#52780=CARTESIAN_POINT('Ctrl Pts',(138.625202425506,-4.88304152665067,334.412557652612));
#52781=CARTESIAN_POINT('Ctrl Pts',(138.617399514567,-4.89956544660317,334.549910684224));
#52782=CARTESIAN_POINT('Ctrl Pts',(138.609596603629,-4.91029252386777,334.687984612255));
#52783=CARTESIAN_POINT('Ctrl Pts',(138.601793692691,-4.915180212012,334.826257242034));
#52784=CARTESIAN_POINT('Ctrl Pts',(138.598468253963,-4.91726324327712,334.88518616762));
#52785=CARTESIAN_POINT('Ctrl Pts',(138.595142815236,-4.91828631742129,334.94415112711));
#52786=CARTESIAN_POINT('Ctrl Pts',(138.591817376508,-4.9182490157254,335.003111561684));
#52787=CARTESIAN_POINT('',(136.841817376545,-4.91824939834121,335.002432738434));
#52788=CARTESIAN_POINT('Ctrl Pts',(138.591817376453,-4.91824901572479,335.003111562653));
#52789=CARTESIAN_POINT('Ctrl Pts',(138.58309093916,-4.91815113059199,335.157832361097));
#52790=CARTESIAN_POINT('Ctrl Pts',(138.574364501866,-4.91074827991025,335.312277323951));
#52791=CARTESIAN_POINT('Ctrl Pts',(138.565638064572,-4.89614264762376,335.465800640424));
#52792=CARTESIAN_POINT('Ctrl Pts',(138.556877973935,-4.88148068898621,335.619916016731));
#52793=CARTESIAN_POINT('Ctrl Pts',(138.548117883297,-4.85956039717657,335.773102436575));
#52794=CARTESIAN_POINT('Ctrl Pts',(138.539357792659,-4.83053502206984,335.924723992906));
#52795=CARTESIAN_POINT('Ctrl Pts',(138.530549670193,-4.80135049999856,336.077176894582));
#52796=CARTESIAN_POINT('Ctrl Pts',(138.521741547726,-4.76498286359781,336.228047539157));
#52797=CARTESIAN_POINT('Ctrl Pts',(138.51293342526,-4.72163668021889,336.376709890468));
#52798=CARTESIAN_POINT('Ctrl Pts',(138.504517968332,-4.68022286693529,336.518744883622));
#52799=CARTESIAN_POINT('Ctrl Pts',(138.496102511405,-4.63243927253342,336.658764102443));
#52800=CARTESIAN_POINT('Ctrl Pts',(138.487687054477,-4.57850424739586,336.796241052609));
#52801=CARTESIAN_POINT('Ctrl Pts',(138.479911975699,-4.52867343333853,336.923256629656));
#52802=CARTESIAN_POINT('Ctrl Pts',(138.472136896921,-4.47347442654302,337.048397755958));
#52803=CARTESIAN_POINT('Ctrl Pts',(138.464361818142,-4.41306828170672,337.171177423311));
#52804=CARTESIAN_POINT('Ctrl Pts',(138.456596307093,-4.35273647047733,337.293806002466));
#52805=CARTESIAN_POINT('Ctrl Pts',(138.448830796044,-4.28721044162563,337.414078557257));
#52806=CARTESIAN_POINT('Ctrl Pts',(138.441065284995,-4.2167000910404,337.531525904414));
#52807=CARTESIAN_POINT('Ctrl Pts',(138.433307473473,-4.14625965167311,337.648856802184));
#52808=CARTESIAN_POINT('Ctrl Pts',(138.425549661951,-4.07084492526617,337.763367733909));
#52809=CARTESIAN_POINT('Ctrl Pts',(138.417791850428,-3.99071254084815,337.874612404972));
#52810=CARTESIAN_POINT('Ctrl Pts',(138.410039876905,-3.91064045859046,337.985773360892));
#52811=CARTESIAN_POINT('Ctrl Pts',(138.402287903382,-3.82585801233367,338.093672632728));
#52812=CARTESIAN_POINT('Ctrl Pts',(138.394535929859,-3.73666592425114,338.197891623092));
#52813=CARTESIAN_POINT('Ctrl Pts',(138.386787239302,-3.64751160907086,338.302066476651));
#52814=CARTESIAN_POINT('Ctrl Pts',(138.379038548744,-3.55395161998393,338.402563852336));
#52815=CARTESIAN_POINT('Ctrl Pts',(138.371289858187,-3.45632772543574,338.498997244481));
#52816=CARTESIAN_POINT('Ctrl Pts',(138.363542779809,-3.35872414235418,338.595410572853));
#52817=CARTESIAN_POINT('Ctrl Pts',(138.355795701431,-3.25705861353494,338.68776132502));
#52818=CARTESIAN_POINT('Ctrl Pts',(138.348048623053,-3.15171034420147,338.775699268845));
#52819=CARTESIAN_POINT('Ctrl Pts',(138.340301479747,-3.04636119194804,338.863637949674));
#52820=CARTESIAN_POINT('Ctrl Pts',(138.332554336442,-2.93732953768893,338.947163497914));
#52821=CARTESIAN_POINT('Ctrl Pts',(138.324807193136,-2.8250279807187,339.025965719012));
#52822=CARTESIAN_POINT('Ctrl Pts',(138.317058308108,-2.71270117597431,339.104785656521));
#52823=CARTESIAN_POINT('Ctrl Pts',(138.30930942308,-2.5971033255634,339.178879929343));
#52824=CARTESIAN_POINT('Ctrl Pts',(138.301560538052,-2.47867599464065,339.247981682646));
#52825=CARTESIAN_POINT('Ctrl Pts',(138.293803428277,-2.36012296372523,339.317156781263));
#52826=CARTESIAN_POINT('Ctrl Pts',(138.286046318502,-2.23873479118307,339.381328577586));
#52827=CARTESIAN_POINT('Ctrl Pts',(138.278289208727,-2.11497812069718,339.440275961184));
#52828=CARTESIAN_POINT('Ctrl Pts',(138.270527953801,-1.99115531860351,339.49925484438));
#52829=CARTESIAN_POINT('Ctrl Pts',(138.262766698875,-1.86496185607697,339.55300359893));
#52830=CARTESIAN_POINT('Ctrl Pts',(138.255005443949,-1.73688341022672,339.601349702183));
#52831=CARTESIAN_POINT('Ctrl Pts',(138.247231773544,-1.60860008060386,339.649773143445));
#52832=CARTESIAN_POINT('Ctrl Pts',(138.23945810314,-1.47842611341864,339.6927765405));
#52833=CARTESIAN_POINT('Ctrl Pts',(138.231684432735,-1.34686221858047,339.730237333016));
#52834=CARTESIAN_POINT('Ctrl Pts',(138.224272628558,-1.22142265469901,339.765954316629));
#52835=CARTESIAN_POINT('Ctrl Pts',(138.216860824381,-1.09471993302537,339.79663303183));
#52836=CARTESIAN_POINT('Ctrl Pts',(138.209449020204,-0.967193940522633,
339.822211001596));
#52837=CARTESIAN_POINT('Ctrl Pts',(138.201673941425,-0.833417519247343,
339.849042623854));
#52838=CARTESIAN_POINT('Ctrl Pts',(138.193898862647,-0.698312326475554,
339.870345645459));
#52839=CARTESIAN_POINT('Ctrl Pts',(138.186123783868,-0.562375053734725,
339.885991952658));
#52840=CARTESIAN_POINT('Ctrl Pts',(138.178358272819,-0.426605060462241,
339.90161900608));
#52841=CARTESIAN_POINT('Ctrl Pts',(138.17059276177,-0.290005409141113,339.911603151117));
#52842=CARTESIAN_POINT('Ctrl Pts',(138.162827250721,-0.153084232702914,
339.915866991711));
#52843=CARTESIAN_POINT('Ctrl Pts',(138.155069439199,-0.0162988140096955,
339.920126604695));
#52844=CARTESIAN_POINT('Ctrl Pts',(138.147311627677,0.120807107216111,339.918677188149));
#52845=CARTESIAN_POINT('Ctrl Pts',(138.139553816155,0.257719355618189,339.911493031273));
#52846=CARTESIAN_POINT('Ctrl Pts',(138.131801842632,0.394528573211468,339.904314280702));
#52847=CARTESIAN_POINT('Ctrl Pts',(138.124049869109,0.531144019313606,339.89140940014));
#52848=CARTESIAN_POINT('Ctrl Pts',(138.116297895586,0.667050948427387,339.872804746212));
#52849=CARTESIAN_POINT('Ctrl Pts',(138.108549205028,0.802900320876047,339.854207971365));
#52850=CARTESIAN_POINT('Ctrl Pts',(138.10080051447,0.938041386672704,339.829916277048));
#52851=CARTESIAN_POINT('Ctrl Pts',(138.093051823913,1.07196417444173,339.800007903245));
#52852=CARTESIAN_POINT('Ctrl Pts',(138.085304745535,1.20585909845621,339.770105752128));
#52853=CARTESIAN_POINT('Ctrl Pts',(138.077557667157,1.33853586738105,339.734589331088));
#52854=CARTESIAN_POINT('Ctrl Pts',(138.069810588779,1.46949475383565,339.69358799118));
#52855=CARTESIAN_POINT('Ctrl Pts',(138.062063445473,1.60045473785176,339.652586307642));
#52856=CARTESIAN_POINT('Ctrl Pts',(138.054316302168,1.72969643766128,339.606099730335));
#52857=CARTESIAN_POINT('Ctrl Pts',(138.046569158862,1.85673572289206,339.554307358736));
#52858=CARTESIAN_POINT('Ctrl Pts',(138.038820273834,1.98380356925116,339.502503343113));
#52859=CARTESIAN_POINT('Ctrl Pts',(138.031071388805,2.10866765385973,339.445391307083));
#52860=CARTESIAN_POINT('Ctrl Pts',(138.023322503777,2.23086461655405,339.383198161743));
#52861=CARTESIAN_POINT('Ctrl Pts',(138.015565394003,2.35319128036728,339.320939003956));
#52862=CARTESIAN_POINT('Ctrl Pts',(138.007808284228,2.47284481835479,339.25358814113));
#52863=CARTESIAN_POINT('Ctrl Pts',(138.000051174453,2.5893867663664,339.181418328351));
#52864=CARTESIAN_POINT('Ctrl Pts',(137.992289919527,2.7059909906687,339.109209950331));
#52865=CARTESIAN_POINT('Ctrl Pts',(137.984528664601,2.81947998860143,339.032177710663));
#52866=CARTESIAN_POINT('Ctrl Pts',(137.976767409675,2.92944585443495,338.950636663683));
#52867=CARTESIAN_POINT('Ctrl Pts',(137.96899373927,3.03958762981602,338.868965177601));
#52868=CARTESIAN_POINT('Ctrl Pts',(137.961220068865,3.14619470686088,338.782770717136));
#52869=CARTESIAN_POINT('Ctrl Pts',(137.953446398461,3.24889305911077,338.692408015504));
#52870=CARTESIAN_POINT('Ctrl Pts',(137.946034594284,3.34681077835521,338.606251719374));
#52871=CARTESIAN_POINT('Ctrl Pts',(137.938622790106,3.4411752773667,338.516306710775));
#52872=CARTESIAN_POINT('Ctrl Pts',(137.931210985929,3.53169596980812,338.422909090137));
#52873=CARTESIAN_POINT('Ctrl Pts',(137.923435907151,3.62665335103383,338.324933773893));
#52874=CARTESIAN_POINT('Ctrl Pts',(137.915660828373,3.71768068852464,338.222849222306));
#52875=CARTESIAN_POINT('Ctrl Pts',(137.907885749594,3.80440146040663,338.117003784174));
#52876=CARTESIAN_POINT('Ctrl Pts',(137.900120238545,3.89101551685791,338.011288595592));
#52877=CARTESIAN_POINT('Ctrl Pts',(137.892354727496,3.97333330683864,337.90182202834));
#52878=CARTESIAN_POINT('Ctrl Pts',(137.884589216447,4.05101476646574,337.788989498793));
#52879=CARTESIAN_POINT('Ctrl Pts',(137.876831404925,4.12861920469948,337.676268843027));
#52880=CARTESIAN_POINT('Ctrl Pts',(137.869073593403,4.20159624051518,337.560189186381));
#52881=CARTESIAN_POINT('Ctrl Pts',(137.86131578188,4.26964600336404,337.441168996292));
#52882=CARTESIAN_POINT('Ctrl Pts',(137.853563808357,4.33764455660831,337.322238372671));
#52883=CARTESIAN_POINT('Ctrl Pts',(137.845811834834,4.40072302410854,337.200371958127));
#52884=CARTESIAN_POINT('Ctrl Pts',(137.838059861311,4.45862501138884,337.076016876212));
#52885=CARTESIAN_POINT('Ctrl Pts',(137.830311170754,4.51650247714317,336.951714458749));
#52886=CARTESIAN_POINT('Ctrl Pts',(137.822562480196,4.56920765824678,336.82492582376));
#52887=CARTESIAN_POINT('Ctrl Pts',(137.814813789639,4.61653037359807,336.6961221572));
#52888=CARTESIAN_POINT('Ctrl Pts',(137.807066711261,4.6638432430632,336.567345289319));
#52889=CARTESIAN_POINT('Ctrl Pts',(137.799319632883,4.70577573955716,336.436554590439));
#52890=CARTESIAN_POINT('Ctrl Pts',(137.791572554505,4.74216620598345,336.304240291253));
#52891=CARTESIAN_POINT('Ctrl Pts',(137.783825411199,4.77855697739688,336.171924883147));
#52892=CARTESIAN_POINT('Ctrl Pts',(137.776078267894,4.80940552244599,336.038086226146));
#52893=CARTESIAN_POINT('Ctrl Pts',(137.768331124588,4.83460045897783,335.903228356813));
#52894=CARTESIAN_POINT('Ctrl Pts',(137.76058223956,4.85980105986628,335.768340168568));
#52895=CARTESIAN_POINT('Ctrl Pts',(137.752833354532,4.87934545121814,335.632432696179));
#52896=CARTESIAN_POINT('Ctrl Pts',(137.745084469504,4.89317369664371,335.496018383706));
#52897=CARTESIAN_POINT('Ctrl Pts',(137.737327359729,4.90701661951185,335.359459279672));
#52898=CARTESIAN_POINT('Ctrl Pts',(137.729570249954,4.9151312372168,335.222392650415));
#52899=CARTESIAN_POINT('Ctrl Pts',(137.721813140179,4.9175096372201,335.085334813221));
#52900=CARTESIAN_POINT('Ctrl Pts',(137.714051885253,4.91988930816432,334.948203736701));
#52901=CARTESIAN_POINT('Ctrl Pts',(137.706290630327,4.9165266631952,334.811081852164));
#52902=CARTESIAN_POINT('Ctrl Pts',(137.698529375401,4.90746589703005,334.67448267022));
#52903=CARTESIAN_POINT('Ctrl Pts',(137.690755704996,4.89839063659193,334.537664974103));
#52904=CARTESIAN_POINT('Ctrl Pts',(137.682982034592,4.8835990824101,334.401372040259));
#52905=CARTESIAN_POINT('Ctrl Pts',(137.675208364187,4.86318713003702,334.266110362015));
#52906=CARTESIAN_POINT('Ctrl Pts',(137.66779656001,4.84372535895781,334.137145147436));
#52907=CARTESIAN_POINT('Ctrl Pts',(137.660384755833,4.81915472738283,334.009117621842));
#52908=CARTESIAN_POINT('Ctrl Pts',(137.652972951656,4.78960061639348,333.882454028711));
#52909=CARTESIAN_POINT('Ctrl Pts',(137.645197872877,4.7585979703873,333.74958227557));
#52910=CARTESIAN_POINT('Ctrl Pts',(137.637422794099,4.722013008543,333.617791637017));
#52911=CARTESIAN_POINT('Ctrl Pts',(137.62964771532,4.67993490720645,333.487587249852));
#52912=CARTESIAN_POINT('Ctrl Pts',(137.621882204271,4.6379085856524,333.357543087474));
#52913=CARTESIAN_POINT('Ctrl Pts',(137.614116693222,4.59040269343587,333.229081660976));
#52914=CARTESIAN_POINT('Ctrl Pts',(137.606351182173,4.5375573073284,333.102697508247));
#52915=CARTESIAN_POINT('Ctrl Pts',(137.598593370651,4.48476431757512,332.976438665774));
#52916=CARTESIAN_POINT('Ctrl Pts',(137.590835559129,4.42664251935187,332.852253356599));
#52917=CARTESIAN_POINT('Ctrl Pts',(137.583077747607,4.36338153369391,332.730620205008));
#52918=CARTESIAN_POINT('Ctrl Pts',(137.575325774084,4.30016815393381,332.60907858622));
#52919=CARTESIAN_POINT('Ctrl Pts',(137.567573800561,4.23182346424373,332.490085647576));
#52920=CARTESIAN_POINT('Ctrl Pts',(137.559821827038,4.15858471059526,332.37409896087));
#52921=CARTESIAN_POINT('Ctrl Pts',(137.55207313648,4.08537697360243,332.258161394595));
#52922=CARTESIAN_POINT('Ctrl Pts',(137.544324445923,4.00727950324135,332.145227877867));
#52923=CARTESIAN_POINT('Ctrl Pts',(137.536575755365,3.92457478877911,332.035730142214));
#52924=CARTESIAN_POINT('Ctrl Pts',(137.528828676987,3.84188728172347,331.926255188479));
#52925=CARTESIAN_POINT('Ctrl Pts',(137.521081598609,3.75459467267662,331.820214905654));
#52926=CARTESIAN_POINT('Ctrl Pts',(137.513334520231,3.66302172515755,331.718010526598));
#52927=CARTESIAN_POINT('Ctrl Pts',(137.505587376926,3.57144801016907,331.61580529097));
#52928=CARTESIAN_POINT('Ctrl Pts',(137.49784023362,3.47559414598997,331.51743631435));
#52929=CARTESIAN_POINT('Ctrl Pts',(137.490093090314,3.37582371244424,331.423270023471));
#52930=CARTESIAN_POINT('Ctrl Pts',(137.482344205286,3.27603084838684,331.329082562011));
#52931=CARTESIAN_POINT('Ctrl Pts',(137.474595320258,3.17231994701299,331.239099934683));
#52932=CARTESIAN_POINT('Ctrl Pts',(137.46684643523,3.06508949844719,331.153649856161));
#52933=CARTESIAN_POINT('Ctrl Pts',(137.459089325455,2.95774523437535,331.068109080043));
#52934=CARTESIAN_POINT('Ctrl Pts',(137.45133221568,2.84687426690146,330.987110706925));
#52935=CARTESIAN_POINT('Ctrl Pts',(137.443575105906,2.73290649631855,330.910940799538));
#52936=CARTESIAN_POINT('Ctrl Pts',(137.435813850979,2.61887782500306,330.834730189389));
#52937=CARTESIAN_POINT('Ctrl Pts',(137.428052596053,2.50174938678771,330.763353389507));
#52938=CARTESIAN_POINT('Ctrl Pts',(137.420291341127,2.38197691999697,330.69705112567));
#52939=CARTESIAN_POINT('Ctrl Pts',(137.412517670722,2.26201285629313,330.630642799817));
#52940=CARTESIAN_POINT('Ctrl Pts',(137.404744000318,2.13939666183432,330.569325406303));
#52941=CARTESIAN_POINT('Ctrl Pts',(137.396970329913,2.01460615225117,330.513292397112));
#52942=CARTESIAN_POINT('Ctrl Pts',(137.389558525736,1.89562467091261,330.45986773798));
#52943=CARTESIAN_POINT('Ctrl Pts',(137.382146721559,1.77466701468582,330.411246665947));
#52944=CARTESIAN_POINT('Ctrl Pts',(137.374734917382,1.65215947170289,330.367554410189));
#52945=CARTESIAN_POINT('Ctrl Pts',(137.366959838603,1.52364746910659,330.321720666823));
#52946=CARTESIAN_POINT('Ctrl Pts',(137.359184759825,1.39302368741873,330.281166265078));
#52947=CARTESIAN_POINT('Ctrl Pts',(137.351409681047,1.2607611653886,330.246089573167));
#52948=CARTESIAN_POINT('Ctrl Pts',(137.343644169998,1.12866140081207,330.211056045359));
#52949=CARTESIAN_POINT('Ctrl Pts',(137.335878658949,0.994927282499733,330.181486914625));
#52950=CARTESIAN_POINT('Ctrl Pts',(137.3281131479,0.860050481492069,330.157532010247));
#52951=CARTESIAN_POINT('Ctrl Pts',(137.320355336377,0.725307411225288,330.133600857226));
#52952=CARTESIAN_POINT('Ctrl Pts',(137.312597524855,0.589424295316403,330.11527292078));
#52953=CARTESIAN_POINT('Ctrl Pts',(137.304839713333,0.452906233959485,330.102647755599));
#52954=CARTESIAN_POINT('Ctrl Pts',(137.29708773981,0.316490906772975,330.090032091255));
#52955=CARTESIAN_POINT('Ctrl Pts',(137.289335766287,0.179441972855275,330.083110691971));
#52956=CARTESIAN_POINT('Ctrl Pts',(137.281583792764,0.0422726014990651,
330.081931670903));
#52957=CARTESIAN_POINT('Ctrl Pts',(137.273835102206,-0.0948386785468911,
330.080753149152));
#52958=CARTESIAN_POINT('Ctrl Pts',(137.266086411649,-0.232069904538951,
330.085312172089));
#52959=CARTESIAN_POINT('Ctrl Pts',(137.258337721091,-0.368905153072199,
330.095604823168));
#52960=CARTESIAN_POINT('Ctrl Pts',(137.250590642713,-0.505711931889073,
330.105895332774));
#52961=CARTESIAN_POINT('Ctrl Pts',(137.242843564335,-0.642122507591071,
330.121917068401));
#52962=CARTESIAN_POINT('Ctrl Pts',(137.235096485958,-0.777623726731592,
330.143614059599));
#52963=CARTESIAN_POINT('Ctrl Pts',(137.227349342652,-0.913126081502839,
330.165311232639));
#52964=CARTESIAN_POINT('Ctrl Pts',(137.219602199346,-1.04771867855369,330.19268369432));
#52965=CARTESIAN_POINT('Ctrl Pts',(137.21185505604,-1.18089662792125,330.225623997142));
#52966=CARTESIAN_POINT('Ctrl Pts',(137.204106171012,-1.31410451851905,330.258571705644));
#52967=CARTESIAN_POINT('Ctrl Pts',(137.196357285984,-1.44589674919798,330.297089652335));
#52968=CARTESIAN_POINT('Ctrl Pts',(137.188608400956,-1.57578209182491,330.341020083582));
#52969=CARTESIAN_POINT('Ctrl Pts',(137.180851291181,-1.70580529609669,330.384997143044));
#52970=CARTESIAN_POINT('Ctrl Pts',(137.173094181406,-1.83391719835138,330.434398037541));
#52971=CARTESIAN_POINT('Ctrl Pts',(137.165337071632,-1.95964459861807,330.489016059704));
#52972=CARTESIAN_POINT('Ctrl Pts',(137.157575816706,-2.08543918358747,330.543663267992));
#52973=CARTESIAN_POINT('Ctrl Pts',(137.149814561779,-2.20884637611177,330.603532988498));
#52974=CARTESIAN_POINT('Ctrl Pts',(137.142053306853,-2.32941711859297,330.66837225167));
#52975=CARTESIAN_POINT('Ctrl Pts',(137.134279636448,-2.45018073496818,330.733315236532));
#52976=CARTESIAN_POINT('Ctrl Pts',(137.126505966044,-2.56809849786118,330.803243450332));
#52977=CARTESIAN_POINT('Ctrl Pts',(137.118732295639,-2.68274915591487,330.877859775682));
#52978=CARTESIAN_POINT('Ctrl Pts',(137.111320491462,-2.79206279825319,330.949002693136));
#52979=CARTESIAN_POINT('Ctrl Pts',(137.103908687285,-2.89840642334555,331.024406914823));
#52980=CARTESIAN_POINT('Ctrl Pts',(137.096496883108,-3.00144403433597,331.10378173465));
#52981=CARTESIAN_POINT('Ctrl Pts',(137.0888096411,-3.10831073408376,331.186106285428));
#52982=CARTESIAN_POINT('Ctrl Pts',(137.081122399092,-3.21197535388208,331.272975499635));
#52983=CARTESIAN_POINT('Ctrl Pts',(137.073435157085,-3.31202019753984,331.364108737381));
#52984=CARTESIAN_POINT('Ctrl Pts',(137.065757414217,-3.41194141559018,331.455129361608));
#52985=CARTESIAN_POINT('Ctrl Pts',(137.058079671349,-3.50825146044264,331.550403263087));
#52986=CARTESIAN_POINT('Ctrl Pts',(137.050401928481,-3.60056292736444,331.64960753514));
#52987=CARTESIAN_POINT('Ctrl Pts',(137.042731734852,-3.69278362784953,331.748714263318));
#52988=CARTESIAN_POINT('Ctrl Pts',(137.035061541224,-3.78101330033598,331.851743383204));
#52989=CARTESIAN_POINT('Ctrl Pts',(137.027391347595,-3.86489924062372,331.958333199983));
#52990=CARTESIAN_POINT('Ctrl Pts',(137.019659098802,-3.94946385424595,332.065785374222));
#52991=CARTESIAN_POINT('Ctrl Pts',(137.011926850008,-4.02961382326933,332.17685584937));
#52992=CARTESIAN_POINT('Ctrl Pts',(137.004194601214,-4.10502693804777,332.291137341909));
#52993=CARTESIAN_POINT('Ctrl Pts',(136.996533077252,-4.17975026903995,332.404373531904));
#52994=CARTESIAN_POINT('Ctrl Pts',(136.98887155329,-4.2498228205061,332.520761897589));
#52995=CARTESIAN_POINT('Ctrl Pts',(136.981210029328,-4.31497315532209,332.639875060225));
#52996=CARTESIAN_POINT('Ctrl Pts',(136.97354976724,-4.3801127597011,332.758968604599));
#52997=CARTESIAN_POINT('Ctrl Pts',(136.965889505151,-4.44033156764303,332.880785702081));
#52998=CARTESIAN_POINT('Ctrl Pts',(136.958229243063,-4.49540342799684,333.004873166424));
#52999=CARTESIAN_POINT('Ctrl Pts',(136.950568494165,-4.55047878816579,333.128968516522));
#53000=CARTESIAN_POINT('Ctrl Pts',(136.942907745268,-4.60040638841005,333.25533415402));
#53001=CARTESIAN_POINT('Ctrl Pts',(136.93524699637,-4.64500789524381,333.38349614426));
#53002=CARTESIAN_POINT('Ctrl Pts',(136.927461194718,-4.69033746944431,333.513750228902));
#53003=CARTESIAN_POINT('Ctrl Pts',(136.919675393066,-4.73016538867476,333.645859426881));
#53004=CARTESIAN_POINT('Ctrl Pts',(136.911889591414,-4.76435723487632,333.779310358452));
#53005=CARTESIAN_POINT('Ctrl Pts',(136.904218941153,-4.7980433863726,333.910787561284));
#53006=CARTESIAN_POINT('Ctrl Pts',(136.896548290893,-4.82625901319341,334.043566673714));
#53007=CARTESIAN_POINT('Ctrl Pts',(136.888877640632,-4.84892739854841,334.177147555083));
#53008=CARTESIAN_POINT('Ctrl Pts',(136.881034263284,-4.87210622878695,334.313736400026));
#53009=CARTESIAN_POINT('Ctrl Pts',(136.873190885936,-4.88948496247125,334.451163108186));
#53010=CARTESIAN_POINT('Ctrl Pts',(136.865347508588,-4.90103778268651,334.588889655714));
#53011=CARTESIAN_POINT('Ctrl Pts',(136.857504131241,-4.91259060290177,334.726616203242));
#53012=CARTESIAN_POINT('Ctrl Pts',(136.849660753893,-4.91831755439441,334.864642146975));
#53013=CARTESIAN_POINT('Ctrl Pts',(136.841817376545,-4.91824939834121,335.002432738434));
#53014=CARTESIAN_POINT('',(135.091817376461,-4.91824801995541,334.995586758035));
#53015=CARTESIAN_POINT('Ctrl Pts',(136.841817376508,-4.91824939834089,335.00243273908));
#53016=CARTESIAN_POINT('Ctrl Pts',(136.83396453395,-4.91818116002039,335.140389613106));
#53017=CARTESIAN_POINT('Ctrl Pts',(136.826111691392,-4.91230893124131,335.27819838096));
#53018=CARTESIAN_POINT('Ctrl Pts',(136.818258848834,-4.90066665130595,335.415511053136));
#53019=CARTESIAN_POINT('Ctrl Pts',(136.810483770055,-4.8891396605396,335.551463968978));
#53020=CARTESIAN_POINT('Ctrl Pts',(136.802708691277,-4.8719328169481,335.68715168536));
#53021=CARTESIAN_POINT('Ctrl Pts',(136.794933612498,-4.84906155608663,335.822061486619));
#53022=CARTESIAN_POINT('Ctrl Pts',(136.787168101449,-4.82621843976769,335.956805272779));
#53023=CARTESIAN_POINT('Ctrl Pts',(136.7794025904,-4.79772484003616,336.090772666826));
#53024=CARTESIAN_POINT('Ctrl Pts',(136.771637079351,-4.76364808905692,336.223454104625));
#53025=CARTESIAN_POINT('Ctrl Pts',(136.763879267829,-4.72960512527555,336.356003988393));
#53026=CARTESIAN_POINT('Ctrl Pts',(136.756121456307,-4.68999012323058,336.487270077145));
#53027=CARTESIAN_POINT('Ctrl Pts',(136.748363644785,-4.64492173574745,336.616751412952));
#53028=CARTESIAN_POINT('Ctrl Pts',(136.740611671262,-4.59988726365504,336.746135309947));
#53029=CARTESIAN_POINT('Ctrl Pts',(136.732859697739,-4.54940770260102,336.873736759671));
#53030=CARTESIAN_POINT('Ctrl Pts',(136.725107724216,-4.49365186749657,336.999068772265));
#53031=CARTESIAN_POINT('Ctrl Pts',(136.717359033658,-4.43791964502142,337.124347706677));
#53032=CARTESIAN_POINT('Ctrl Pts',(136.7096103431,-4.37691575131309,337.247358759147));
#53033=CARTESIAN_POINT('Ctrl Pts',(136.701861652543,-4.31085749670005,337.367633988953));
#53034=CARTESIAN_POINT('Ctrl Pts',(136.694114574165,-4.24481298605862,337.487884194493));
#53035=CARTESIAN_POINT('Ctrl Pts',(136.686367495787,-4.17371639427106,337.605399367181));
#53036=CARTESIAN_POINT('Ctrl Pts',(136.678620417409,-4.09783126049797,337.719735653145));
#53037=CARTESIAN_POINT('Ctrl Pts',(136.670873274103,-4.02194549073439,337.834072897356));
#53038=CARTESIAN_POINT('Ctrl Pts',(136.663126130798,-3.9412713150868,337.94523087603));
#53039=CARTESIAN_POINT('Ctrl Pts',(136.655378987492,-3.85611570058006,338.05279458304));
#53040=CARTESIAN_POINT('Ctrl Pts',(136.647630102464,-3.77094094128306,338.160382472656));
#53041=CARTESIAN_POINT('Ctrl Pts',(136.639881217436,-3.68128298084066,338.264374176238));
#53042=CARTESIAN_POINT('Ctrl Pts',(136.632132332408,-3.5874889119204,338.36438796356));
#53043=CARTESIAN_POINT('Ctrl Pts',(136.624375222633,-3.49359528900647,338.464507906549));
#53044=CARTESIAN_POINT('Ctrl Pts',(136.616618112858,-3.39555705576614,338.56064121347));
#53045=CARTESIAN_POINT('Ctrl Pts',(136.608861003083,-3.29375839067746,338.652442843679));
#53046=CARTESIAN_POINT('Ctrl Pts',(136.601099748157,-3.19190532763704,338.744293529744));
#53047=CARTESIAN_POINT('Ctrl Pts',(136.593338493231,-3.08628812955419,338.831807677567));
#53048=CARTESIAN_POINT('Ctrl Pts',(136.585577238305,-2.97732307791898,338.914681385782));
#53049=CARTESIAN_POINT('Ctrl Pts',(136.5778035679,-2.86818371771286,338.997687664922));
#53050=CARTESIAN_POINT('Ctrl Pts',(136.570029897496,-2.7556861230471,339.076038447212));
#53051=CARTESIAN_POINT('Ctrl Pts',(136.562256227091,-2.64027523614145,339.149473429234));
#53052=CARTESIAN_POINT('Ctrl Pts',(136.554844422914,-2.5302367537881,339.219489995175));
#53053=CARTESIAN_POINT('Ctrl Pts',(136.547432618737,-2.41755035166708,339.285037977773));
#53054=CARTESIAN_POINT('Ctrl Pts',(136.54002081456,-2.30261981609416,339.345932011092));
#53055=CARTESIAN_POINT('Ctrl Pts',(136.532245735781,-2.18205619261169,339.409810642378));
#53056=CARTESIAN_POINT('Ctrl Pts',(136.524470657003,-2.05864188673958,339.468769449604));
#53057=CARTESIAN_POINT('Ctrl Pts',(136.516695578225,-1.93281640508159,339.522543952992));
#53058=CARTESIAN_POINT('Ctrl Pts',(136.508930067176,-1.80714575968917,339.576252283431));
#53059=CARTESIAN_POINT('Ctrl Pts',(136.501164556127,-1.67907019818954,339.624788851499));
#53060=CARTESIAN_POINT('Ctrl Pts',(136.493399045078,-1.54905466123114,339.667934523857));
#53061=CARTESIAN_POINT('Ctrl Pts',(136.485641233555,-1.41916803505622,339.711037417156));
#53062=CARTESIAN_POINT('Ctrl Pts',(136.477883422033,-1.2873456298699,339.748759929458));
#53063=CARTESIAN_POINT('Ctrl Pts',(136.470125610511,-1.15407292173654,339.780930741374));
#53064=CARTESIAN_POINT('Ctrl Pts',(136.462373636988,-1.02090050554241,339.813077343734));
#53065=CARTESIAN_POINT('Ctrl Pts',(136.454621663465,-0.886280337208536,
339.839680470125));
#53066=CARTESIAN_POINT('Ctrl Pts',(136.446869689942,-0.750713292333256,
339.860618542451));
#53067=CARTESIAN_POINT('Ctrl Pts',(136.439120999384,-0.615203660182013,
339.88154774749));
#53068=CARTESIAN_POINT('Ctrl Pts',(136.431372308827,-0.478748334545758,
339.896816610674));
#53069=CARTESIAN_POINT('Ctrl Pts',(136.423623618269,-0.341858415849529,
339.906354643318));
#53070=CARTESIAN_POINT('Ctrl Pts',(136.415876539891,-0.204996978244212,
339.915890691495));
#53071=CARTESIAN_POINT('Ctrl Pts',(136.408129461513,-0.0677015171162233,
339.919698253643));
#53072=CARTESIAN_POINT('Ctrl Pts',(136.400382383136,0.0695121051806816,
339.917758750664));
#53073=CARTESIAN_POINT('Ctrl Pts',(136.39263523983,0.206726877459855,339.915819231431));
#53074=CARTESIAN_POINT('Ctrl Pts',(136.384888096524,0.34385941870464,339.908132556525));
#53075=CARTESIAN_POINT('Ctrl Pts',(136.377140953218,0.480394623938193,339.894732277438));
#53076=CARTESIAN_POINT('Ctrl Pts',(136.36939206819,0.616960525184561,339.881328985684));
#53077=CARTESIAN_POINT('Ctrl Pts',(136.361643183162,0.75292843426079,339.862209571831));
#53078=CARTESIAN_POINT('Ctrl Pts',(136.353894298134,0.887789514315184,339.837459337377));
#53079=CARTESIAN_POINT('Ctrl Pts',(136.346137188359,1.02279373731342,339.812682832768));
#53080=CARTESIAN_POINT('Ctrl Pts',(136.338380078584,1.15668839945633,339.782263639385));
#53081=CARTESIAN_POINT('Ctrl Pts',(136.33062296881,1.28897544768678,339.746338099816));
#53082=CARTESIAN_POINT('Ctrl Pts',(136.322861713884,1.42133318588603,339.710393362786));
#53083=CARTESIAN_POINT('Ctrl Pts',(136.315100458957,1.55208122601918,339.668936534622));
#53084=CARTESIAN_POINT('Ctrl Pts',(136.307339204031,1.68073873714333,339.622153216842));
#53085=CARTESIAN_POINT('Ctrl Pts',(136.299565533627,1.8096020583559,339.575295061001));
#53086=CARTESIAN_POINT('Ctrl Pts',(136.291791863222,1.93636780630809,339.523093537679));
#53087=CARTESIAN_POINT('Ctrl Pts',(136.284018192817,2.06057630253733,339.465781943168));
#53088=CARTESIAN_POINT('Ctrl Pts',(136.27660638864,2.17900286338367,339.411138217169));
#53089=CARTESIAN_POINT('Ctrl Pts',(136.269194584463,2.29510463848692,339.351849592093));
#53090=CARTESIAN_POINT('Ctrl Pts',(136.261782780286,2.40850723773322,339.288155308322));
#53091=CARTESIAN_POINT('Ctrl Pts',(136.254007701508,2.52746803617814,339.221339177967));
#53092=CARTESIAN_POINT('Ctrl Pts',(136.246232622729,2.6438343174242,339.149463448876));
#53093=CARTESIAN_POINT('Ctrl Pts',(136.238457543951,2.75714583254226,339.072754586345));
#53094=CARTESIAN_POINT('Ctrl Pts',(136.230692032902,2.87031791062721,338.996140118953));
#53095=CARTESIAN_POINT('Ctrl Pts',(136.222926521853,2.98044238149894,338.914704568925));
#53096=CARTESIAN_POINT('Ctrl Pts',(136.215161010804,3.08708336519596,338.828720329148));
#53097=CARTESIAN_POINT('Ctrl Pts',(136.207403199282,3.19361861404717,338.742821342995));
#53098=CARTESIAN_POINT('Ctrl Pts',(136.199645387759,3.29667694683085,338.65238288609));
#53099=CARTESIAN_POINT('Ctrl Pts',(136.191887576237,3.39585157846239,338.557720494861));
#53100=CARTESIAN_POINT('Ctrl Pts',(136.184135602714,3.49495157803855,338.463129340083));
#53101=CARTESIAN_POINT('Ctrl Pts',(136.176383629191,3.59017341216274,338.364320846713));
#53102=CARTESIAN_POINT('Ctrl Pts',(136.168631655668,3.68114379069314,338.261650418843));
#53103=CARTESIAN_POINT('Ctrl Pts',(136.160882965111,3.77207564321429,338.159023471961));
#53104=CARTESIAN_POINT('Ctrl Pts',(136.153134274553,3.8587593625195,338.052538135483));
#53105=CARTESIAN_POINT('Ctrl Pts',(136.145385583995,3.94085908740338,337.942586059188));
#53106=CARTESIAN_POINT('Ctrl Pts',(136.137638505617,4.02294173075376,337.832656859342));
#53107=CARTESIAN_POINT('Ctrl Pts',(136.12989142724,4.10044204302277,337.719262667365));
#53108=CARTESIAN_POINT('Ctrl Pts',(136.122144348862,4.17306523793142,337.602827228701));
#53109=CARTESIAN_POINT('Ctrl Pts',(136.114397205556,4.24568904149237,337.486390814196));
#53110=CARTESIAN_POINT('Ctrl Pts',(136.10665006225,4.31343543930706,337.366913433816));
#53111=CARTESIAN_POINT('Ctrl Pts',(136.098902918944,4.37605389268097,337.244846406962));
#53112=CARTESIAN_POINT('Ctrl Pts',(136.091154033916,4.43868642401258,337.12275193685));
#53113=CARTESIAN_POINT('Ctrl Pts',(136.083405148888,4.49618853844671,336.998067009452));
#53114=CARTESIAN_POINT('Ctrl Pts',(136.07565626386,4.54835660701591,336.871265678068));
#53115=CARTESIAN_POINT('Ctrl Pts',(136.067899154085,4.60058004731211,336.744329758441));
#53116=CARTESIAN_POINT('Ctrl Pts',(136.060142044311,4.64745798319112,336.615273309535));
#53117=CARTESIAN_POINT('Ctrl Pts',(136.052384934536,4.68883554295597,336.484588937589));
#53118=CARTESIAN_POINT('Ctrl Pts',(136.04462367961,4.73023521356575,336.353834732094));
#53119=CARTESIAN_POINT('Ctrl Pts',(136.036862424684,4.76612854915706,336.221451247247));
#53120=CARTESIAN_POINT('Ctrl Pts',(136.029101169757,4.7964114207934,336.087943263678));
#53121=CARTESIAN_POINT('Ctrl Pts',(136.021327499353,4.8267427351552,335.954221710846));
#53122=CARTESIAN_POINT('Ctrl Pts',(136.013553828948,4.85144558055753,335.819372449372));
#53123=CARTESIAN_POINT('Ctrl Pts',(136.005780158543,4.87046738243523,335.683908282692));
#53124=CARTESIAN_POINT('Ctrl Pts',(135.998368354366,4.88860371485924,335.554750005561));
#53125=CARTESIAN_POINT('Ctrl Pts',(135.990956550189,4.90157597759195,335.425033068943));
#53126=CARTESIAN_POINT('Ctrl Pts',(135.983544746012,4.90938274900289,335.295201772171));
#53127=CARTESIAN_POINT('Ctrl Pts',(135.975769667233,4.9175721535358,335.159007056798));
#53128=CARTESIAN_POINT('Ctrl Pts',(135.967994588455,4.92010279141976,335.022256087093));
#53129=CARTESIAN_POINT('Ctrl Pts',(135.960219509677,4.91691603504921,334.885458449565));
#53130=CARTESIAN_POINT('Ctrl Pts',(135.952453998628,4.91373320018525,334.74882915024));
#53131=CARTESIAN_POINT('Ctrl Pts',(135.944688487579,4.90484697894459,334.61215368439));
#53132=CARTESIAN_POINT('Ctrl Pts',(135.93692297653,4.89025055265981,334.475946000196));
#53133=CARTESIAN_POINT('Ctrl Pts',(135.929165165007,4.87566859877419,334.339873366317));
#53134=CARTESIAN_POINT('Ctrl Pts',(135.921407353485,4.85538774829809,334.204267977238));
#53135=CARTESIAN_POINT('Ctrl Pts',(135.913649541963,4.82945320779463,334.06964266208));
#53136=CARTESIAN_POINT('Ctrl Pts',(135.90589756844,4.80353818385534,333.935118656741));
#53137=CARTESIAN_POINT('Ctrl Pts',(135.898145594917,4.77197801206601,333.801573639564));
#53138=CARTESIAN_POINT('Ctrl Pts',(135.890393621394,4.73486955059473,333.669513847742));
#53139=CARTESIAN_POINT('Ctrl Pts',(135.882644930836,4.69777680457891,333.53750998332));
#53140=CARTESIAN_POINT('Ctrl Pts',(135.874896240279,4.65514054779613,333.406990468744));
#53141=CARTESIAN_POINT('Ctrl Pts',(135.867147549721,4.60710837313153,333.278449681037));
#53142=CARTESIAN_POINT('Ctrl Pts',(135.859400471343,4.55908619196203,333.149935637314));
#53143=CARTESIAN_POINT('Ctrl Pts',(135.851653392965,4.50567046270539,333.023399867495));
#53144=CARTESIAN_POINT('Ctrl Pts',(135.843906314588,4.44705799617459,332.899319576623));
#53145=CARTESIAN_POINT('Ctrl Pts',(135.836159171282,4.3884450384149,332.775238245839));
#53146=CARTESIAN_POINT('Ctrl Pts',(135.828412027976,4.32463542346004,332.653612788476));
#53147=CARTESIAN_POINT('Ctrl Pts',(135.82066488467,4.25587309455981,332.534898122693));
#53148=CARTESIAN_POINT('Ctrl Pts',(135.812915999642,4.18709530642819,332.416156767333));
#53149=CARTESIAN_POINT('Ctrl Pts',(135.805167114614,4.11336278453372,332.300327843917));
#53150=CARTESIAN_POINT('Ctrl Pts',(135.797418229586,4.03496397509108,332.187839125829));
#53151=CARTESIAN_POINT('Ctrl Pts',(135.789661119811,3.95648195234205,332.075231011054));
#53152=CARTESIAN_POINT('Ctrl Pts',(135.781904010036,3.87332397211809,331.965970504916));
#53153=CARTESIAN_POINT('Ctrl Pts',(135.774146900262,3.78582046755282,331.860454419831));
#53154=CARTESIAN_POINT('Ctrl Pts',(135.766385645335,3.69827020391256,331.754881950324));
#53155=CARTESIAN_POINT('Ctrl Pts',(135.758624390409,3.60637005067453,331.653058178861));
#53156=CARTESIAN_POINT('Ctrl Pts',(135.750863135483,3.51048813849675,331.55534383545));
#53157=CARTESIAN_POINT('Ctrl Pts',(135.743089465078,3.41445284650732,331.457473180934));
#53158=CARTESIAN_POINT('Ctrl Pts',(135.735315794674,3.31442335274736,331.363725358191));
#53159=CARTESIAN_POINT('Ctrl Pts',(135.727542124269,3.21080243345159,331.274422085657));
#53160=CARTESIAN_POINT('Ctrl Pts',(135.720130320092,3.11200509287935,331.189275901945));
#53161=CARTESIAN_POINT('Ctrl Pts',(135.712718515915,3.00994338920189,331.108169971903));
#53162=CARTESIAN_POINT('Ctrl Pts',(135.705306711738,2.90499017388142,331.031345926872));
#53163=CARTESIAN_POINT('Ctrl Pts',(135.69753163296,2.79489288883805,330.950756506548));
#53164=CARTESIAN_POINT('Ctrl Pts',(135.689756554181,2.68126555432611,330.874624642686));
#53165=CARTESIAN_POINT('Ctrl Pts',(135.681981475403,2.56450496575192,330.803275402992));
#53166=CARTESIAN_POINT('Ctrl Pts',(135.674215964354,2.4478880585154,330.732013963079));
#53167=CARTESIAN_POINT('Ctrl Pts',(135.666450453305,2.32814589923475,330.665523639092));
#53168=CARTESIAN_POINT('Ctrl Pts',(135.658684942256,2.20570698792708,330.604088291843));
#53169=CARTESIAN_POINT('Ctrl Pts',(135.650927130733,2.08338947515639,330.54271385792));
#53170=CARTESIAN_POINT('Ctrl Pts',(135.643169319211,1.95838087855779,330.486384600692));
#53171=CARTESIAN_POINT('Ctrl Pts',(135.635411507689,1.8311369109464,330.435340026259));
#53172=CARTESIAN_POINT('Ctrl Pts',(135.627659534166,1.70398869845582,330.384333864488));
#53173=CARTESIAN_POINT('Ctrl Pts',(135.619907560643,1.57460882457687,330.338604614647));
#53174=CARTESIAN_POINT('Ctrl Pts',(135.61215558712,1.44347541047631,330.298344780628));
#53175=CARTESIAN_POINT('Ctrl Pts',(135.604406896562,1.31239753145448,330.258101996673));
#53176=CARTESIAN_POINT('Ctrl Pts',(135.596658206005,1.17956796212342,330.223324136061));
#53177=CARTESIAN_POINT('Ctrl Pts',(135.588909515447,1.04548230564657,330.19415462056));
#53178=CARTESIAN_POINT('Ctrl Pts',(135.581162437069,0.911424546810491,330.164991174022));
#53179=CARTESIAN_POINT('Ctrl Pts',(135.573415358692,0.776111602352436,330.141433834658));
#53180=CARTESIAN_POINT('Ctrl Pts',(135.565668280314,0.640051269799193,330.123575343089));
#53181=CARTESIAN_POINT('Ctrl Pts',(135.557921137008,0.503989796929267,330.105716701849));
#53182=CARTESIAN_POINT('Ctrl Pts',(135.550173993702,0.367181311020722,330.093557054537));
#53183=CARTESIAN_POINT('Ctrl Pts',(135.542426850396,0.230140374147949,330.087137446388));
#53184=CARTESIAN_POINT('Ctrl Pts',(135.534677965368,0.0930686275632914,
330.080716394974));
#53185=CARTESIAN_POINT('Ctrl Pts',(135.52692908034,-0.0442352836071517,
330.080037968927));
#53186=CARTESIAN_POINT('Ctrl Pts',(135.519180195312,-0.181255540800347,
330.085091100394));
#53187=CARTESIAN_POINT('Ctrl Pts',(135.511423085537,-0.318421232710352,
330.090149595307));
#53188=CARTESIAN_POINT('Ctrl Pts',(135.503665975763,-0.45530227799531,330.100951785737));
#53189=CARTESIAN_POINT('Ctrl Pts',(135.495908865988,-0.591386172300536,
330.11743454138));
#53190=CARTESIAN_POINT('Ctrl Pts',(135.488147611062,-0.72754278548776,330.13392610488));
#53191=CARTESIAN_POINT('Ctrl Pts',(135.480386356136,-0.862901013372442,
330.156104218956));
#53192=CARTESIAN_POINT('Ctrl Pts',(135.47262510121,-0.996958293773339,330.18385452639));
#53193=CARTESIAN_POINT('Ctrl Pts',(135.464851430805,-1.13123002213371,330.211649225271));
#53194=CARTESIAN_POINT('Ctrl Pts',(135.4570777604,-1.26419626506519,330.245033834474));
#53195=CARTESIAN_POINT('Ctrl Pts',(135.449304089996,-1.39536851733881,330.283843751176));
#53196=CARTESIAN_POINT('Ctrl Pts',(135.441892285818,-1.5204346697122,330.320847056919));
#53197=CARTESIAN_POINT('Ctrl Pts',(135.434480481641,-1.64386982076507,330.36278184833));
#53198=CARTESIAN_POINT('Ctrl Pts',(135.427068677464,-1.76526900622609,330.409465347244));
#53199=CARTESIAN_POINT('Ctrl Pts',(135.419293598686,-1.89261832739498,330.458436943502));
#53200=CARTESIAN_POINT('Ctrl Pts',(135.411518519907,-2.01812950655818,330.512789273245));
#53201=CARTESIAN_POINT('Ctrl Pts',(135.403743441129,-2.1413144585852,330.572364575538));
#53202=CARTESIAN_POINT('Ctrl Pts',(135.39597793008,-2.26434782368662,330.631866566629));
#53203=CARTESIAN_POINT('Ctrl Pts',(135.388212419031,-2.38506030882731,330.696578573431));
#53204=CARTESIAN_POINT('Ctrl Pts',(135.380446907982,-2.50298132344674,330.766293874514));
#53205=CARTESIAN_POINT('Ctrl Pts',(135.37268909646,-2.62078541903669,330.835940052673));
#53206=CARTESIAN_POINT('Ctrl Pts',(135.364931284937,-2.73580321778343,330.910579455236));
#53207=CARTESIAN_POINT('Ctrl Pts',(135.357173473415,-2.84758670154397,330.989958474069));
#53208=CARTESIAN_POINT('Ctrl Pts',(135.349421499892,-2.95928606468785,331.069277757673));
#53209=CARTESIAN_POINT('Ctrl Pts',(135.341669526369,-3.06775564004161,331.153329332784));
#53210=CARTESIAN_POINT('Ctrl Pts',(135.333917552846,-3.17257480817746,331.241815312013));
#53211=CARTESIAN_POINT('Ctrl Pts',(135.326168862289,-3.27734958533356,331.330263817378));
#53212=CARTESIAN_POINT('Ctrl Pts',(135.318420171731,-3.37847673199928,331.423142740093));
#53213=CARTESIAN_POINT('Ctrl Pts',(135.310671481173,-3.47556744244087,331.520112930633));
#53214=CARTESIAN_POINT('Ctrl Pts',(135.302924402796,-3.57263795234923,331.617062945715));
#53215=CARTESIAN_POINT('Ctrl Pts',(135.295177324418,-3.66567342009562,331.718102259436));
#53216=CARTESIAN_POINT('Ctrl Pts',(135.28743024604,-3.75432105973468,331.822854041292));
#53217=CARTESIAN_POINT('Ctrl Pts',(135.279683102734,-3.84296944232629,331.92760670107));
#53218=CARTESIAN_POINT('Ctrl Pts',(135.271935959428,-3.9272296709603,332.03607159267));
#53219=CARTESIAN_POINT('Ctrl Pts',(135.264188816122,-4.00678877075849,332.1478382218));
#53220=CARTESIAN_POINT('Ctrl Pts',(135.256439931094,-4.08636575713126,332.259629978441));
#53221=CARTESIAN_POINT('Ctrl Pts',(135.248691046066,-4.16123928489915,332.374724631333));
#53222=CARTESIAN_POINT('Ctrl Pts',(135.240942161038,-4.23113952223255,332.492682428191));
#53223=CARTESIAN_POINT('Ctrl Pts',(135.233185051264,-4.30111395240018,332.610765426674));
#53224=CARTESIAN_POINT('Ctrl Pts',(135.225427941489,-4.3661043478492,332.731717302955));
#53225=CARTESIAN_POINT('Ctrl Pts',(135.217670831714,-4.42588645068561,332.855072917757));
#53226=CARTESIAN_POINT('Ctrl Pts',(135.209909576788,-4.48570049916629,332.978494449857));
#53227=CARTESIAN_POINT('Ctrl Pts',(135.202148321862,-4.5403005538521,333.104321921533));
#53228=CARTESIAN_POINT('Ctrl Pts',(135.194387066936,-4.5895108149345,333.232070832273));
#53229=CARTESIAN_POINT('Ctrl Pts',(135.186613396531,-4.63879979639705,333.360024099638));
#53230=CARTESIAN_POINT('Ctrl Pts',(135.178839726126,-4.68268162994043,333.489904577677));
#53231=CARTESIAN_POINT('Ctrl Pts',(135.171066055722,-4.72103037537972,333.621212395892));
#53232=CARTESIAN_POINT('Ctrl Pts',(135.163654251545,-4.7575939774922,333.746407803576));
#53233=CARTESIAN_POINT('Ctrl Pts',(135.156242447368,-4.78912795969681,333.872900377318));
#53234=CARTESIAN_POINT('Ctrl Pts',(135.148830643191,-4.8155668746477,334.000250662268));
#53235=CARTESIAN_POINT('Ctrl Pts',(135.137812995018,-4.85486832623043,334.189556882562));
#53236=CARTESIAN_POINT('Ctrl Pts',(135.126795346845,-4.88301770679793,334.381251455537));
#53237=CARTESIAN_POINT('Ctrl Pts',(135.115777698672,-4.89978751616537,334.574247303086));
#53238=CARTESIAN_POINT('Ctrl Pts',(135.107790924617,-4.91194407410313,334.714151409988));
#53239=CARTESIAN_POINT('Ctrl Pts',(135.099804150563,-4.91812163449033,334.85473906561));
#53240=CARTESIAN_POINT('Ctrl Pts',(135.091817376508,-4.91824801995467,334.995586757208));
#53241=CARTESIAN_POINT('',(133.341817376552,-4.9182499977156,334.999850098394));
#53242=CARTESIAN_POINT('Ctrl Pts',(135.091817376461,-4.91824801995541,334.995586758035));
#53243=CARTESIAN_POINT('Ctrl Pts',(135.084167745614,-4.9183690703268,335.130488889871));
#53244=CARTESIAN_POINT('Ctrl Pts',(135.076518114767,-4.91293562494658,335.265568161034));
#53245=CARTESIAN_POINT('Ctrl Pts',(135.068868483919,-4.90193073749584,335.400322504106));
#53246=CARTESIAN_POINT('Ctrl Pts',(135.06122511569,-4.89093485955304,335.534966526165));
#53247=CARTESIAN_POINT('Ctrl Pts',(135.053581747462,-4.87437664553979,335.669285749588));
#53248=CARTESIAN_POINT('Ctrl Pts',(135.045938379233,-4.85229121336668,335.80277832755));
#53249=CARTESIAN_POINT('Ctrl Pts',(135.038298771281,-4.83021664647481,335.936205231706));
#53250=CARTESIAN_POINT('Ctrl Pts',(135.030659163329,-4.80262033353919,336.068805902345));
#53251=CARTESIAN_POINT('Ctrl Pts',(135.023019555377,-4.76958917031008,336.200084250776));
#53252=CARTESIAN_POINT('Ctrl Pts',(135.015381769418,-4.73656588477817,336.331331290256));
#53253=CARTESIAN_POINT('Ctrl Pts',(135.007743983458,-4.69811042400476,336.461256243887));
#53254=CARTESIAN_POINT('Ctrl Pts',(135.000106197498,-4.65436055645448,336.589374365284));
#53255=CARTESIAN_POINT('Ctrl Pts',(134.99246846978,-4.61061102251683,336.717491509721));
#53256=CARTESIAN_POINT('Ctrl Pts',(134.984830742062,-4.56156729253725,336.843801467951));
#53257=CARTESIAN_POINT('Ctrl Pts',(134.977193014344,-4.50741647584148,336.967836318349));
#53258=CARTESIAN_POINT('Ctrl Pts',(134.969553581374,-4.45325356905772,337.091898861631));
#53259=CARTESIAN_POINT('Ctrl Pts',(134.961914148403,-4.39398146988125,337.213684917937));
#53260=CARTESIAN_POINT('Ctrl Pts',(134.954274715433,-4.32983449128601,337.332748666396));
#53261=CARTESIAN_POINT('Ctrl Pts',(134.946627408995,-4.26562140056087,337.451935126137));
#53262=CARTESIAN_POINT('Ctrl Pts',(134.938980102556,-4.19652359055122,337.568393321046));
#53263=CARTESIAN_POINT('Ctrl Pts',(134.931332796118,-4.12282035733366,337.681703817288));
#53264=CARTESIAN_POINT('Ctrl Pts',(134.923681212767,-4.04907590407508,337.795077684743));
#53265=CARTESIAN_POINT('Ctrl Pts',(134.916029629416,-3.9707211331318,337.905300021115));
#53266=CARTESIAN_POINT('Ctrl Pts',(134.908378046065,-3.88807654125674,338.011983378412));
#53267=CARTESIAN_POINT('Ctrl Pts',(134.900715028075,-3.80530844407937,338.118826164898));
#53268=CARTESIAN_POINT('Ctrl Pts',(134.893052010084,-3.71823798485626,338.222119105096));
#53269=CARTESIAN_POINT('Ctrl Pts',(134.885388992094,-3.62722382843509,338.321510253022));
#53270=CARTESIAN_POINT('Ctrl Pts',(134.880456864368,-3.56864463093292,338.385481111109));
#53271=CARTESIAN_POINT('Ctrl Pts',(134.875524736642,-3.50843246631769,338.447836396263));
#53272=CARTESIAN_POINT('Ctrl Pts',(134.870592608916,-3.44669009985623,338.508491188254));
#53273=CARTESIAN_POINT('Ctrl Pts',(134.862817530138,-3.34935852413608,338.604108295562));
#53274=CARTESIAN_POINT('Ctrl Pts',(134.855042451359,-3.24789125660164,338.69582320963));
#53275=CARTESIAN_POINT('Ctrl Pts',(134.847267372581,-3.14263409442908,338.783257063832));
#53276=CARTESIAN_POINT('Ctrl Pts',(134.839501861532,-3.03750645789572,338.870583325109));
#53277=CARTESIAN_POINT('Ctrl Pts',(134.831736350483,-2.92859850396048,338.953638761191));
#53278=CARTESIAN_POINT('Ctrl Pts',(134.823970839434,-2.81629334282869,339.032080712193));
#53279=CARTESIAN_POINT('Ctrl Pts',(134.816213027912,-2.70409953259089,339.110444887772));
#53280=CARTESIAN_POINT('Ctrl Pts',(134.808455216389,-2.58851553672762,339.184204458973));
#53281=CARTESIAN_POINT('Ctrl Pts',(134.800697404867,-2.46995778728785,339.253056735046));
#53282=CARTESIAN_POINT('Ctrl Pts',(134.792945431344,-2.35148925631404,339.321857197597));
#53283=CARTESIAN_POINT('Ctrl Pts',(134.785193457821,-2.2300517627301,339.385757520038));
#53284=CARTESIAN_POINT('Ctrl Pts',(134.777441484298,-2.10609068775804,339.444498293108));
#53285=CARTESIAN_POINT('Ctrl Pts',(134.769692793741,-1.98218211037504,339.503214189425));
#53286=CARTESIAN_POINT('Ctrl Pts',(134.761944103183,-1.85575242973706,339.556774715293));
#53287=CARTESIAN_POINT('Ctrl Pts',(134.754195412625,-1.72727140112299,339.60496651121));
#53288=CARTESIAN_POINT('Ctrl Pts',(134.746448334247,-1.59881710406028,339.653148280421));
#53289=CARTESIAN_POINT('Ctrl Pts',(134.73870125587,-1.46831267370358,339.695963404303));
#53290=CARTESIAN_POINT('Ctrl Pts',(134.730954177492,-1.33624723745171,339.733246917593));
#53291=CARTESIAN_POINT('Ctrl Pts',(134.723207034186,-1.20418069436397,339.770530743354));
#53292=CARTESIAN_POINT('Ctrl Pts',(134.71545989088,-1.07055349545786,339.802282759856));
#53293=CARTESIAN_POINT('Ctrl Pts',(134.707712747574,-0.935868913327415,
339.828388182361));
#53294=CARTESIAN_POINT('Ctrl Pts',(134.699963862546,-0.80115405124334,339.85449947392));
#53295=CARTESIAN_POINT('Ctrl Pts',(134.692214977518,-0.665381716551916,
339.874961571007));
#53296=CARTESIAN_POINT('Ctrl Pts',(134.68446609249,-0.529063936707968,339.889711076677));
#53297=CARTESIAN_POINT('Ctrl Pts',(134.676708982715,-0.392601467764392,
339.904476237624));
#53298=CARTESIAN_POINT('Ctrl Pts',(134.66895187294,-0.255592786399069,339.913516652822));
#53299=CARTESIAN_POINT('Ctrl Pts',(134.661194763166,-0.118554144661556,
339.916820921824));
#53300=CARTESIAN_POINT('Ctrl Pts',(134.65343350824,0.0185577261445966,339.920126956521));
#53301=CARTESIAN_POINT('Ctrl Pts',(134.645672253313,0.155699198609651,339.917690744246));
#53302=CARTESIAN_POINT('Ctrl Pts',(134.637910998387,0.292356475275361,339.909553009579));
#53303=CARTESIAN_POINT('Ctrl Pts',(134.630137327982,0.429232359047048,339.901402257188));
#53304=CARTESIAN_POINT('Ctrl Pts',(134.622363657578,0.565622110155068,339.887531796357));
#53305=CARTESIAN_POINT('Ctrl Pts',(134.614589987173,0.701018598987366,339.868034098727));
#53306=CARTESIAN_POINT('Ctrl Pts',(134.607178182996,0.830112348688905,339.849444023613));
#53307=CARTESIAN_POINT('Ctrl Pts',(134.599766378819,0.958302944793477,339.825738869831));
#53308=CARTESIAN_POINT('Ctrl Pts',(134.592354574642,1.085163306511,339.797041136024));
#53309=CARTESIAN_POINT('Ctrl Pts',(134.584579495864,1.21824147245513,339.766936840795));
#53310=CARTESIAN_POINT('Ctrl Pts',(134.576804417085,1.35027626100033,339.731243053419));
#53311=CARTESIAN_POINT('Ctrl Pts',(134.569029338307,1.48076194442432,339.690045535647));
#53312=CARTESIAN_POINT('Ctrl Pts',(134.561263827258,1.61108705690768,339.648898714044));
#53313=CARTESIAN_POINT('Ctrl Pts',(134.553498316209,1.73986648803078,339.602261754314));
#53314=CARTESIAN_POINT('Ctrl Pts',(134.54573280516,1.86660476487117,339.550271389078));
#53315=CARTESIAN_POINT('Ctrl Pts',(134.537974993637,1.99321738034113,339.49833257244));
#53316=CARTESIAN_POINT('Ctrl Pts',(134.530217182115,2.11779250972559,339.441051060743));
#53317=CARTESIAN_POINT('Ctrl Pts',(134.522459370593,2.23985025863769,339.378613237245));
#53318=CARTESIAN_POINT('Ctrl Pts',(134.51470739707,2.36181615522302,339.31622240019));
#53319=CARTESIAN_POINT('Ctrl Pts',(134.506955423547,2.48126809547787,339.248683152153));
#53320=CARTESIAN_POINT('Ctrl Pts',(134.499203450024,2.5977469152836,339.176229642469));
#53321=CARTESIAN_POINT('Ctrl Pts',(134.491454759466,2.71417640623994,339.103806816888));
#53322=CARTESIAN_POINT('Ctrl Pts',(134.483706068909,2.82763494983268,339.02647407503));
#53323=CARTESIAN_POINT('Ctrl Pts',(134.475957378351,2.93768891596891,338.944510983062));
#53324=CARTESIAN_POINT('Ctrl Pts',(134.468210299973,3.04771998445822,338.862564944199));
#53325=CARTESIAN_POINT('Ctrl Pts',(134.460463221595,3.15434757116053,338.775990704786));
#53326=CARTESIAN_POINT('Ctrl Pts',(134.452716143218,3.25716825836363,338.685110310317));
#53327=CARTESIAN_POINT('Ctrl Pts',(134.444968999912,3.35998980730299,338.594229154184));
#53328=CARTESIAN_POINT('Ctrl Pts',(134.437221856606,3.45900410023385,338.499042029872));
#53329=CARTESIAN_POINT('Ctrl Pts',(134.4294747133,3.55384226254359,338.399910033436));
#53330=CARTESIAN_POINT('Ctrl Pts',(134.421725828272,3.64870174648582,338.300755750022));
#53331=CARTESIAN_POINT('Ctrl Pts',(134.413976943244,3.73938296138243,338.197655112053));
#53332=CARTESIAN_POINT('Ctrl Pts',(134.406228058216,3.82555550795274,338.091004386615));
#53333=CARTESIAN_POINT('Ctrl Pts',(134.398470948441,3.91181951895428,337.984240460994));
#53334=CARTESIAN_POINT('Ctrl Pts',(134.390713838666,3.99356505600683,337.873919225285));
#53335=CARTESIAN_POINT('Ctrl Pts',(134.382956728892,4.07050315862327,337.760468637412));
#53336=CARTESIAN_POINT('Ctrl Pts',(134.375195473966,4.14748237450166,337.646957425173));
#53337=CARTESIAN_POINT('Ctrl Pts',(134.367434219039,4.21964883155236,337.530313860941));
#53338=CARTESIAN_POINT('Ctrl Pts',(134.359672964113,4.28675873065632,337.410992046366));
#53339=CARTESIAN_POINT('Ctrl Pts',(134.351899293709,4.35397598372786,337.291479355775));
#53340=CARTESIAN_POINT('Ctrl Pts',(134.344125623304,4.41612033766883,337.169280202078));
#53341=CARTESIAN_POINT('Ctrl Pts',(134.336351952899,4.47299511692283,337.044871083097));
#53342=CARTESIAN_POINT('Ctrl Pts',(134.328940148722,4.52722236151892,336.926253238535));
#53343=CARTESIAN_POINT('Ctrl Pts',(134.321528344545,4.57665947910355,336.805626812531));
#53344=CARTESIAN_POINT('Ctrl Pts',(134.314116540368,4.62117836347678,336.683417237477));
#53345=CARTESIAN_POINT('Ctrl Pts',(134.30634146159,4.66787925098841,336.555217807104));
#53346=CARTESIAN_POINT('Ctrl Pts',(134.298566382811,4.70931518392665,336.42487098012));
#53347=CARTESIAN_POINT('Ctrl Pts',(134.290791304033,4.74528460288934,336.292848444359));
#53348=CARTESIAN_POINT('Ctrl Pts',(134.283025792984,4.7812097591921,336.160988370733));
#53349=CARTESIAN_POINT('Ctrl Pts',(134.275260281935,4.81168168434252,336.027457064775));
#53350=CARTESIAN_POINT('Ctrl Pts',(134.267494770886,4.83654723088881,335.892745174102));
#53351=CARTESIAN_POINT('Ctrl Pts',(134.259736959363,4.86138812317328,335.75816685066));
#53352=CARTESIAN_POINT('Ctrl Pts',(134.251979147841,4.88063362856871,335.622410653875));
#53353=CARTESIAN_POINT('Ctrl Pts',(134.244221336319,4.89418078234591,335.485980999851));
#53354=CARTESIAN_POINT('Ctrl Pts',(134.236469362796,4.90771774146024,335.349654013468));
#53355=CARTESIAN_POINT('Ctrl Pts',(134.228717389273,4.91556484592206,335.212654965999));
#53356=CARTESIAN_POINT('Ctrl Pts',(134.22096541575,4.91767051685054,335.075496689986));
#53357=CARTESIAN_POINT('Ctrl Pts',(134.213216725192,4.91977529602614,334.938396500585));
#53358=CARTESIAN_POINT('Ctrl Pts',(134.205468034635,4.91614347176402,334.801137606774));
#53359=CARTESIAN_POINT('Ctrl Pts',(134.197719344077,4.90677547509316,334.664235946647));
#53360=CARTESIAN_POINT('Ctrl Pts',(134.189972265699,4.89740942751224,334.527362770052));
#53361=CARTESIAN_POINT('Ctrl Pts',(134.182225187322,4.88230960806394,334.390847069019));
#53362=CARTESIAN_POINT('Ctrl Pts',(134.174478108944,4.8615285192027,334.255202363404));
#53363=CARTESIAN_POINT('Ctrl Pts',(134.166730965638,4.84074725617597,334.119556520956));
#53364=CARTESIAN_POINT('Ctrl Pts',(134.158983822332,4.81428468795787,333.984782074852));
#53365=CARTESIAN_POINT('Ctrl Pts',(134.151236679026,4.78224484870461,333.851384629418));
#53366=CARTESIAN_POINT('Ctrl Pts',(134.143487793998,4.75019780621522,333.717957193405));
#53367=CARTESIAN_POINT('Ctrl Pts',(134.13573890897,4.71257108885928,333.585907754082));
#53368=CARTESIAN_POINT('Ctrl Pts',(134.127990023942,4.6695191280734,333.455728594108));
#53369=CARTESIAN_POINT('Ctrl Pts',(134.120232914167,4.62642147149155,333.325411260628));
#53370=CARTESIAN_POINT('Ctrl Pts',(134.112475804392,4.57788719144039,333.196968543683));
#53371=CARTESIAN_POINT('Ctrl Pts',(134.104718694618,4.52411979376921,333.070875028899));
#53372=CARTESIAN_POINT('Ctrl Pts',(134.096957439692,4.47032366451993,332.944714133773));
#53373=CARTESIAN_POINT('Ctrl Pts',(134.089196184765,4.41128901369633,332.820905294822));
#53374=CARTESIAN_POINT('Ctrl Pts',(134.081434929839,4.34726577137163,332.699899268388));
#53375=CARTESIAN_POINT('Ctrl Pts',(134.073661259435,4.28314011272427,332.578699671748));
#53376=CARTESIAN_POINT('Ctrl Pts',(134.06588758903,4.21401011313568,332.460312184876));
#53377=CARTESIAN_POINT('Ctrl Pts',(134.058113918625,4.14017003736031,332.345160056756));
#53378=CARTESIAN_POINT('Ctrl Pts',(134.050702114448,4.06976723487698,332.235368287904));
#53379=CARTESIAN_POINT('Ctrl Pts',(134.043290310271,3.99508316082387,332.128517680378));
#53380=CARTESIAN_POINT('Ctrl Pts',(134.035878506094,3.91640624476005,332.024946187293));
#53381=CARTESIAN_POINT('Ctrl Pts',(134.028103427315,3.83387313867383,331.916298346808));
#53382=CARTESIAN_POINT('Ctrl Pts',(134.020328348537,3.74668507194117,331.810915839423));
#53383=CARTESIAN_POINT('Ctrl Pts',(134.012553269759,3.65512962156838,331.709223418092));
#53384=CARTESIAN_POINT('Ctrl Pts',(134.00478775871,3.56368683600598,331.60765613576));
#53385=CARTESIAN_POINT('Ctrl Pts',(133.997022247661,3.46788761923814,331.509770192132));
#53386=CARTESIAN_POINT('Ctrl Pts',(133.989256736612,3.36806169043975,331.415959889748));
#53387=CARTESIAN_POINT('Ctrl Pts',(133.981498925089,3.26833473934002,331.322242600552));
#53388=CARTESIAN_POINT('Ctrl Pts',(133.973741113567,3.16458930450799,331.232593176711));
#53389=CARTESIAN_POINT('Ctrl Pts',(133.965983302045,3.05719384008437,331.147371171959));
#53390=CARTESIAN_POINT('Ctrl Pts',(133.958231328522,2.94987919415438,331.06221329947));
#53391=CARTESIAN_POINT('Ctrl Pts',(133.950479354999,2.83892029088234,330.981476456328));
#53392=CARTESIAN_POINT('Ctrl Pts',(133.942727381476,2.72472046980289,330.905481539431));
#53393=CARTESIAN_POINT('Ctrl Pts',(133.934978690918,2.6105690124148,330.829518806427));
#53394=CARTESIAN_POINT('Ctrl Pts',(133.927230000361,2.49317969181753,330.758294221576));
#53395=CARTESIAN_POINT('Ctrl Pts',(133.919481309803,2.37298660461303,330.692086626123));
#53396=CARTESIAN_POINT('Ctrl Pts',(133.911734231425,2.25281852458419,330.625892805714));
#53397=CARTESIAN_POINT('Ctrl Pts',(133.903987153047,2.12984818041996,330.56471408693));
#53398=CARTESIAN_POINT('Ctrl Pts',(133.89624007467,2.00453581401394,330.508784214399));
#53399=CARTESIAN_POINT('Ctrl Pts',(133.888492931364,1.87922239736976,330.452853873121));
#53400=CARTESIAN_POINT('Ctrl Pts',(133.880745788058,1.75156727626953,330.402172625147));
#53401=CARTESIAN_POINT('Ctrl Pts',(133.872998644752,1.62205192302869,330.356926597447));
#53402=CARTESIAN_POINT('Ctrl Pts',(133.865249759724,1.49250745198675,330.311670397479));
#53403=CARTESIAN_POINT('Ctrl Pts',(133.857500874696,1.36110228552649,330.271851978221));
#53404=CARTESIAN_POINT('Ctrl Pts',(133.849751989668,1.22833396635186,330.237607877379));
#53405=CARTESIAN_POINT('Ctrl Pts',(133.841994879893,1.09542472551155,330.203327429494));
#53406=CARTESIAN_POINT('Ctrl Pts',(133.834237770119,0.961149820794958,330.174633216842));
#53407=CARTESIAN_POINT('Ctrl Pts',(133.826480660344,0.826018470073655,330.151610932526));
#53408=CARTESIAN_POINT('Ctrl Pts',(133.818719405418,0.690814909479144,330.128576345839));
#53409=CARTESIAN_POINT('Ctrl Pts',(133.810958150491,0.554754378491972,330.11121977626));
#53410=CARTESIAN_POINT('Ctrl Pts',(133.803196895565,0.418351179238423,330.099574982379));
#53411=CARTESIAN_POINT('Ctrl Pts',(133.795423225161,0.281729779319628,330.087911560622));
#53412=CARTESIAN_POINT('Ctrl Pts',(133.787649554756,0.144765006466774,330.081978189881));
#53413=CARTESIAN_POINT('Ctrl Pts',(133.779875884351,0.00797202332331137,
330.081756460956));
#53414=CARTESIAN_POINT('Ctrl Pts',(133.772464080174,-0.122453213544662,
330.081545053566));
#53415=CARTESIAN_POINT('Ctrl Pts',(133.765052275997,-0.252722006812522,
330.086525489933));
#53416=CARTESIAN_POINT('Ctrl Pts',(133.75764047182,-0.382394078711341,330.09663810931));
#53417=CARTESIAN_POINT('Ctrl Pts',(133.749865393042,-0.518421765126657,
330.107246378287));
#53418=CARTESIAN_POINT('Ctrl Pts',(133.742090314263,-0.654222629583345,
330.123536162085));
#53419=CARTESIAN_POINT('Ctrl Pts',(133.734315235485,-0.789283863840687,
330.145495489261));
#53420=CARTESIAN_POINT('Ctrl Pts',(133.726549724436,-0.924178896651132,
330.167427794088));
#53421=CARTESIAN_POINT('Ctrl Pts',(133.718784213387,-1.05833572810374,330.195015698463));
#53422=CARTESIAN_POINT('Ctrl Pts',(133.711018702338,-1.19124435081706,330.228195314229));
#53423=CARTESIAN_POINT('Ctrl Pts',(133.703260890815,-1.32402119424423,330.261342032309));
#53424=CARTESIAN_POINT('Ctrl Pts',(133.695503079293,-1.45555191503853,330.300069334448));
#53425=CARTESIAN_POINT('Ctrl Pts',(133.687745267771,-1.58533476511591,330.344261954855));
#53426=CARTESIAN_POINT('Ctrl Pts',(133.679993294248,-1.71501994948217,330.388421318913));
#53427=CARTESIAN_POINT('Ctrl Pts',(133.672241320725,-1.84295951270638,330.438037689376));
#53428=CARTESIAN_POINT('Ctrl Pts',(133.664489347202,-1.96866533557613,330.492945545148));
#53429=CARTESIAN_POINT('Ctrl Pts',(133.656740656644,-2.09431792195539,330.547830147411));
#53430=CARTESIAN_POINT('Ctrl Pts',(133.648991966087,-2.21773829203901,330.608001621764));
#53431=CARTESIAN_POINT('Ctrl Pts',(133.641243275529,-2.33845704769644,330.67324582411));
#53432=CARTESIAN_POINT('Ctrl Pts',(133.633496197151,-2.45915068680881,330.738476451856));
#53433=CARTESIAN_POINT('Ctrl Pts',(133.625749118773,-2.57714348588889,330.808777522553));
#53434=CARTESIAN_POINT('Ctrl Pts',(133.618002040396,-2.69198982079654,330.883888501604));
#53435=CARTESIAN_POINT('Ctrl Pts',(133.61025489709,-2.80683711822673,330.959000110157));
#53436=CARTESIAN_POINT('Ctrl Pts',(133.602507753784,-2.91853757176185,331.038921493524));
#53437=CARTESIAN_POINT('Ctrl Pts',(133.594760610478,-3.02667411096457,331.123348495348));
#53438=CARTESIAN_POINT('Ctrl Pts',(133.58701172545,-3.13483496155682,331.207794478155));
#53439=CARTESIAN_POINT('Ctrl Pts',(133.579262840422,-3.23942999539763,331.296747854596));
#53440=CARTESIAN_POINT('Ctrl Pts',(133.571513955394,-3.3400751461114,331.389864118786));
#53441=CARTESIAN_POINT('Ctrl Pts',(133.563756845619,-3.44082712262855,331.483079217541));
#53442=CARTESIAN_POINT('Ctrl Pts',(133.555999735845,-3.53762055384682,331.580465764607));
#53443=CARTESIAN_POINT('Ctrl Pts',(133.54824262607,-3.63010781159711,331.681641921269));
#53444=CARTESIAN_POINT('Ctrl Pts',(133.540481371144,-3.72264449158048,331.782872143233));
#53445=CARTESIAN_POINT('Ctrl Pts',(133.532720116218,-3.81087016169437,331.887895710745));
#53446=CARTESIAN_POINT('Ctrl Pts',(133.524958861291,-3.89447811522964,331.996298404885));
#53447=CARTESIAN_POINT('Ctrl Pts',(133.517185190887,-3.97821981424292,332.104874508007));
#53448=CARTESIAN_POINT('Ctrl Pts',(133.509411520482,-4.05732880990968,332.216840220149));
#53449=CARTESIAN_POINT('Ctrl Pts',(133.501637850077,-4.13154179885157,332.331752367781));
#53450=CARTESIAN_POINT('Ctrl Pts',(133.4942260459,-4.20230015530368,332.441315327294));
#53451=CARTESIAN_POINT('Ctrl Pts',(133.486814241723,-4.26860791896853,332.553556334611));
#53452=CARTESIAN_POINT('Ctrl Pts',(133.479402437546,-4.33027700027737,332.66807286491));
#53453=CARTESIAN_POINT('Ctrl Pts',(133.471206716576,-4.39846857291137,332.794701349199));
#53454=CARTESIAN_POINT('Ctrl Pts',(133.463010995606,-4.46118481695896,332.924476920584));
#53455=CARTESIAN_POINT('Ctrl Pts',(133.454815274636,-4.51814030822212,333.056911937735));
#53456=CARTESIAN_POINT('Ctrl Pts',(133.44663396167,-4.57499567224022,333.189114135307));
#53457=CARTESIAN_POINT('Ctrl Pts',(133.438452648704,-4.62611033588138,333.323966161439));
#53458=CARTESIAN_POINT('Ctrl Pts',(133.430271335738,-4.67124452783009,333.460955613467));
#53459=CARTESIAN_POINT('Ctrl Pts',(133.42210923541,-4.71627272861936,333.597623365467));
#53460=CARTESIAN_POINT('Ctrl Pts',(133.413947135081,-4.75534836193544,333.736418222766));
#53461=CARTESIAN_POINT('Ctrl Pts',(133.405785034752,-4.78827983031108,333.876808418329));
#53462=CARTESIAN_POINT('Ctrl Pts',(133.397634429049,-4.82116492154199,334.017000903412));
#53463=CARTESIAN_POINT('Ctrl Pts',(133.389483823346,-4.84792301213026,334.158783932328));
#53464=CARTESIAN_POINT('Ctrl Pts',(133.381333217643,-4.86841183606882,334.30160952403));
#53465=CARTESIAN_POINT('Ctrl Pts',(133.373197820997,-4.8888624277958,334.444168602718));
#53466=CARTESIAN_POINT('Ctrl Pts',(133.36506242435,-4.90306703361276,334.587766040657));
#53467=CARTESIAN_POINT('Ctrl Pts',(133.356927027704,-4.91093422629604,334.731843166236));
#53468=CARTESIAN_POINT('Ctrl Pts',(133.35189047732,-4.91580473403529,334.821040009816));
#53469=CARTESIAN_POINT('Ctrl Pts',(133.346853926936,-4.91824727202096,334.910420451796));
#53470=CARTESIAN_POINT('Ctrl Pts',(133.341817376552,-4.9182499977156,334.999850098394));
#53471=CARTESIAN_POINT('',(131.591817376536,-4.91824796507461,335.004473984742));
#53472=CARTESIAN_POINT('Ctrl Pts',(133.341817376508,-4.91824999771563,334.99985009918));
#53473=CARTESIAN_POINT('Ctrl Pts',(133.333720689468,-4.91825437948074,335.143615932019));
#53474=CARTESIAN_POINT('Ctrl Pts',(133.325624002429,-4.91195079819547,335.287266411861));
#53475=CARTESIAN_POINT('Ctrl Pts',(133.317527315389,-4.89939538494284,335.430241704744));
#53476=CARTESIAN_POINT('Ctrl Pts',(133.309420634577,-4.88682447449389,335.573393472597));
#53477=CARTESIAN_POINT('Ctrl Pts',(133.301313953765,-4.86798636506514,335.715868055862));
#53478=CARTESIAN_POINT('Ctrl Pts',(133.293207272952,-4.84298863388882,335.857113851553));
#53479=CARTESIAN_POINT('Ctrl Pts',(133.285082101954,-4.81793388644398,335.998681808809));
#53480=CARTESIAN_POINT('Ctrl Pts',(133.276956930956,-4.78669148748155,336.139015042695));
#53481=CARTESIAN_POINT('Ctrl Pts',(133.268831759958,-4.74941987798039,336.277573436302));
#53482=CARTESIAN_POINT('Ctrl Pts',(133.260696913547,-4.71210388563228,336.416296824554));
#53483=CARTESIAN_POINT('Ctrl Pts',(133.252562067136,-4.66874445716667,336.553240834597));
#53484=CARTESIAN_POINT('Ctrl Pts',(133.244427220724,-4.61954894920918,336.687883458169));
#53485=CARTESIAN_POINT('Ctrl Pts',(133.236273866015,-4.57024151226322,336.82283241891));
#53486=CARTESIAN_POINT('Ctrl Pts',(133.228120511306,-4.51507157414448,336.955469211743));
#53487=CARTESIAN_POINT('Ctrl Pts',(133.219967156596,-4.45429415459308,337.085292940298));
#53488=CARTESIAN_POINT('Ctrl Pts',(133.213699572155,-4.40757380171516,337.185090043479));
#53489=CARTESIAN_POINT('Ctrl Pts',(133.207431987714,-4.3575408460764,337.283225320956));
#53490=CARTESIAN_POINT('Ctrl Pts',(133.201164403272,-4.30432863347267,337.379482733194));
#53491=CARTESIAN_POINT('Ctrl Pts',(133.193389324494,-4.23831769275951,337.498892207476));
#53492=CARTESIAN_POINT('Ctrl Pts',(133.185614245716,-4.16722974095943,337.615741404958));
#53493=CARTESIAN_POINT('Ctrl Pts',(133.177839166937,-4.09128812889158,337.72956855728));
#53494=CARTESIAN_POINT('Ctrl Pts',(133.170073655888,-4.01543996781198,337.843255638044));
#53495=CARTESIAN_POINT('Ctrl Pts',(133.162308144839,-3.93475024535724,337.953927750988));
#53496=CARTESIAN_POINT('Ctrl Pts',(133.15454263379,-3.84948840351955,338.061147185888));
#53497=CARTESIAN_POINT('Ctrl Pts',(133.146784822268,-3.76431109904648,338.168260312406));
#53498=CARTESIAN_POINT('Ctrl Pts',(133.139027010746,-3.67457093836872,338.271927269557));
#53499=CARTESIAN_POINT('Ctrl Pts',(133.131269199224,-3.58058070259055,338.371739149866));
#53500=CARTESIAN_POINT('Ctrl Pts',(133.123517225701,-3.48666119744514,338.47147591857));
#53501=CARTESIAN_POINT('Ctrl Pts',(133.115765252178,-3.38849825017902,338.567363101447));
#53502=CARTESIAN_POINT('Ctrl Pts',(133.108013278655,-3.28644473493321,338.659025015866));
#53503=CARTESIAN_POINT('Ctrl Pts',(133.100264588097,-3.1844344394118,338.750648111409));
#53504=CARTESIAN_POINT('Ctrl Pts',(133.09251589754,-3.07853714317919,338.838049236849));
#53505=CARTESIAN_POINT('Ctrl Pts',(133.084767206982,-2.96914221809585,338.920889892769));
#53506=CARTESIAN_POINT('Ctrl Pts',(133.077020128604,-2.85977005354035,339.003713313));
#53507=CARTESIAN_POINT('Ctrl Pts',(133.069273050226,-2.74690201901675,339.081977915207));
#53508=CARTESIAN_POINT('Ctrl Pts',(133.061525971848,-2.6309598588071,339.155386057137));
#53509=CARTESIAN_POINT('Ctrl Pts',(133.053778828543,-2.5150167268906,339.228794814297));
#53510=CARTESIAN_POINT('Ctrl Pts',(133.046031685237,-2.39599974814581,339.297346820904));
#53511=CARTESIAN_POINT('Ctrl Pts',(133.038284541931,-2.27435853910797,339.360788494996));
#53512=CARTESIAN_POINT('Ctrl Pts',(133.030535656903,-2.15268998254395,339.424244432123));
#53513=CARTESIAN_POINT('Ctrl Pts',(133.022786771875,-2.02839636818998,339.482587569812));
#53514=CARTESIAN_POINT('Ctrl Pts',(133.015037886847,-1.90195036286914,339.535611081175));
#53515=CARTESIAN_POINT('Ctrl Pts',(133.007280777072,-1.77537014645164,339.588690872242));
#53516=CARTESIAN_POINT('Ctrl Pts',(132.999523667297,-1.64663333645803,339.636439606561));
#53517=CARTESIAN_POINT('Ctrl Pts',(132.991766557523,-1.51623148161709,339.678699088064));
#53518=CARTESIAN_POINT('Ctrl Pts',(132.984005302597,-1.38575994419436,339.720981151683));
#53519=CARTESIAN_POINT('Ctrl Pts',(132.97624404767,-1.25362196538693,339.757768012881));
#53520=CARTESIAN_POINT('Ctrl Pts',(132.968482792744,-1.12032161084018,339.788952134944));
#53521=CARTESIAN_POINT('Ctrl Pts',(132.96070912234,-0.986808019168632,339.82018614144));
#53522=CARTESIAN_POINT('Ctrl Pts',(132.952935451935,-0.852128720274987,
339.845799425893));
#53523=CARTESIAN_POINT('Ctrl Pts',(132.94516178153,-0.716796150713376,339.865735950586));
#53524=CARTESIAN_POINT('Ctrl Pts',(132.937749977353,-0.587763344823718,
339.884744425258));
#53525=CARTESIAN_POINT('Ctrl Pts',(132.930338173176,-0.458137005228234,
339.898592722226));
#53526=CARTESIAN_POINT('Ctrl Pts',(132.922926368999,-0.328361411517108,
339.907276418333));
#53527=CARTESIAN_POINT('Ctrl Pts',(132.915151290221,-0.192225129376943,
339.916385728254));
#53528=CARTESIAN_POINT('Ctrl Pts',(132.907376211442,-0.0554943766009946,
339.919840158553));
#53529=CARTESIAN_POINT('Ctrl Pts',(132.899601132664,0.0813216680008721,
339.917577640344));
#53530=CARTESIAN_POINT('Ctrl Pts',(132.891835621615,0.217969351749859,339.915317906308));
#53531=CARTESIAN_POINT('Ctrl Pts',(132.884070110566,0.354701731405614,339.907355227934));
#53532=CARTESIAN_POINT('Ctrl Pts',(132.876304599517,0.491004916581289,339.893679314625));
#53533=CARTESIAN_POINT('Ctrl Pts',(132.868546787994,0.627172956751564,339.880016961025));
#53534=CARTESIAN_POINT('Ctrl Pts',(132.860788976472,0.762912262889284,339.860652684312));
#53535=CARTESIAN_POINT('Ctrl Pts',(132.85303116495,0.897709712172195,339.835628225492));
#53536=CARTESIAN_POINT('Ctrl Pts',(132.845279191427,1.0324057221004,339.810622598371));
#53537=CARTESIAN_POINT('Ctrl Pts',(132.837527217904,1.16616090319948,339.77996533846));
#53538=CARTESIAN_POINT('Ctrl Pts',(132.829775244381,1.29846837548461,339.743749881725));
#53539=CARTESIAN_POINT('Ctrl Pts',(132.822026553823,1.43071981547639,339.707549762258));
#53540=CARTESIAN_POINT('Ctrl Pts',(132.814277863266,1.56152438985654,339.665796230687));
#53541=CARTESIAN_POINT('Ctrl Pts',(132.806529172708,1.69038673579029,339.61863353666));
#53542=CARTESIAN_POINT('Ctrl Pts',(132.79878209433,1.81922227083668,339.571480655226));
#53543=CARTESIAN_POINT('Ctrl Pts',(132.791035015953,1.94611601438184,339.518920984138));
#53544=CARTESIAN_POINT('Ctrl Pts',(132.783287937575,2.07058944267369,339.461148105857));
#53545=CARTESIAN_POINT('Ctrl Pts',(132.775540794269,2.19506391417259,339.403374743383));
#53546=CARTESIAN_POINT('Ctrl Pts',(132.767793650963,2.31711767541261,339.340388251129));
#53547=CARTESIAN_POINT('Ctrl Pts',(132.760046507657,2.43629417060654,339.272429493481));
#53548=CARTESIAN_POINT('Ctrl Pts',(132.752297622629,2.55549745920697,339.204455457262));
#53549=CARTESIAN_POINT('Ctrl Pts',(132.744548737601,2.67182185507944,339.131507124796));
#53550=CARTESIAN_POINT('Ctrl Pts',(132.736799852573,2.78483764594164,339.053870045801));
#53551=CARTESIAN_POINT('Ctrl Pts',(132.729042742798,2.89797339293189,338.976150562009));
#53552=CARTESIAN_POINT('Ctrl Pts',(132.721285633024,3.00779319709961,338.893732611968));
#53553=CARTESIAN_POINT('Ctrl Pts',(132.713528523249,3.11389802277347,338.806943940521));
#53554=CARTESIAN_POINT('Ctrl Pts',(132.705767268323,3.22005954747363,338.720108891982));
#53555=CARTESIAN_POINT('Ctrl Pts',(132.698006013397,3.32250184627625,338.628898727987));
#53556=CARTESIAN_POINT('Ctrl Pts',(132.69024475847,3.42086171042138,338.533679133803));
#53557=CARTESIAN_POINT('Ctrl Pts',(132.682471088066,3.51937891829367,338.4383072193));
#53558=CARTESIAN_POINT('Ctrl Pts',(132.674697417661,3.61380037215368,338.338913341511));
#53559=CARTESIAN_POINT('Ctrl Pts',(132.666923747256,3.70380163986602,338.235898094042));
#53560=CARTESIAN_POINT('Ctrl Pts',(132.659511943079,3.78961332691325,338.137678231127));
#53561=CARTESIAN_POINT('Ctrl Pts',(132.652100138902,3.87140690558669,338.036166784809));
#53562=CARTESIAN_POINT('Ctrl Pts',(132.644688334725,3.94893823118078,337.931734965651));
#53563=CARTESIAN_POINT('Ctrl Pts',(132.636913255947,4.03026959799639,337.822184631949));
#53564=CARTESIAN_POINT('Ctrl Pts',(132.629138177168,4.10716735806855,337.709074215367));
#53565=CARTESIAN_POINT('Ctrl Pts',(132.62136309839,4.17930377047498,337.592798306192));
#53566=CARTESIAN_POINT('Ctrl Pts',(132.613597587341,4.25135141443341,337.476665481927));
#53567=CARTESIAN_POINT('Ctrl Pts',(132.605832076292,4.31864916464669,337.35737524465));
#53568=CARTESIAN_POINT('Ctrl Pts',(132.598066565243,4.38091027195633,337.23535416692));
#53569=CARTESIAN_POINT('Ctrl Pts',(132.59030875372,4.44310964719692,337.113454073444));
#53570=CARTESIAN_POINT('Ctrl Pts',(132.582550942198,4.50028214106122,336.988828873789));
#53571=CARTESIAN_POINT('Ctrl Pts',(132.574793130676,4.55218517424933,336.861932652339));
#53572=CARTESIAN_POINT('Ctrl Pts',(132.567041157153,4.60404914875895,336.735131924319));
#53573=CARTESIAN_POINT('Ctrl Pts',(132.55928918363,4.65065140821951,336.60606393654));
#53574=CARTESIAN_POINT('Ctrl Pts',(132.551537210107,4.69179622308286,336.475205498758));
#53575=CARTESIAN_POINT('Ctrl Pts',(132.543788519549,4.73292361309269,336.344402479602));
#53576=CARTESIAN_POINT('Ctrl Pts',(132.536039828992,4.76859803838411,336.211810890662));
#53577=CARTESIAN_POINT('Ctrl Pts',(132.528291138434,4.79867273231001,336.077925354876));
#53578=CARTESIAN_POINT('Ctrl Pts',(132.520544060056,4.82874116894465,335.944067675094));
#53579=CARTESIAN_POINT('Ctrl Pts',(132.512796981678,4.85321210600861,335.808916965088));
#53580=CARTESIAN_POINT('Ctrl Pts',(132.505049903301,4.87198937446404,335.672980384268));
#53581=CARTESIAN_POINT('Ctrl Pts',(132.497302759995,4.89076680029106,335.537042664169));
#53582=CARTESIAN_POINT('Ctrl Pts',(132.489555616689,4.90385040884697,335.400319447316));
#53583=CARTESIAN_POINT('Ctrl Pts',(132.481808473383,4.91119567959973,335.263325006752));
#53584=CARTESIAN_POINT('Ctrl Pts',(132.474059588355,4.91854260172529,335.12629976693));
#53585=CARTESIAN_POINT('Ctrl Pts',(132.466310703327,4.92014859796904,334.989003572297));
#53586=CARTESIAN_POINT('Ctrl Pts',(132.458561818299,4.91602125120837,334.851952304416));
#53587=CARTESIAN_POINT('Ctrl Pts',(132.450804708524,4.91188952363919,334.714755568904));
#53588=CARTESIAN_POINT('Ctrl Pts',(132.443047598749,4.9020123086338,334.577804670768));
#53589=CARTESIAN_POINT('Ctrl Pts',(132.435290488975,4.88644927272418,334.441612529158));
#53590=CARTESIAN_POINT('Ctrl Pts',(132.427529234048,4.87087792042578,334.305347610822));
#53591=CARTESIAN_POINT('Ctrl Pts',(132.419767979122,4.84961475365808,334.169842642872));
#53592=CARTESIAN_POINT('Ctrl Pts',(132.412006724196,4.82277073186459,334.035600948585));
#53593=CARTESIAN_POINT('Ctrl Pts',(132.404233053791,4.79588376838469,333.901144511336));
#53594=CARTESIAN_POINT('Ctrl Pts',(132.396459383387,4.76339820266194,333.7679557659));
#53595=CARTESIAN_POINT('Ctrl Pts',(132.388685712982,4.72547533356174,333.636524318369));
#53596=CARTESIAN_POINT('Ctrl Pts',(132.381273908805,4.68931778314214,333.511211036341));
#53597=CARTESIAN_POINT('Ctrl Pts',(132.373862104628,4.64821784101662,333.387495402718));
#53598=CARTESIAN_POINT('Ctrl Pts',(132.366450300451,4.60235554535699,333.265783607325));
#53599=CARTESIAN_POINT('Ctrl Pts',(132.358675221672,4.55424540197007,333.138106354279));
#53600=CARTESIAN_POINT('Ctrl Pts',(132.350900142894,4.50074222992901,333.012230850606));
#53601=CARTESIAN_POINT('Ctrl Pts',(132.343125064116,4.4420004892061,332.888646236086));
#53602=CARTESIAN_POINT('Ctrl Pts',(132.335359553067,4.38333103393465,332.765213700302));
#53603=CARTESIAN_POINT('Ctrl Pts',(132.327594042018,4.31943600264773,332.64406679415));
#53604=CARTESIAN_POINT('Ctrl Pts',(132.319828530968,4.25051893288553,332.525677494003));
#53605=CARTESIAN_POINT('Ctrl Pts',(132.312070719446,4.18167019459909,332.407405577193));
#53606=CARTESIAN_POINT('Ctrl Pts',(132.304312907924,4.10780952243509,332.291886160856));
#53607=CARTESIAN_POINT('Ctrl Pts',(132.296555096402,4.02918749205899,332.179568966215));
#53608=CARTESIAN_POINT('Ctrl Pts',(132.288803122879,3.95062462725389,332.067336293825));
#53609=CARTESIAN_POINT('Ctrl Pts',(132.281051149356,3.86730775941755,331.958301365523));
#53610=CARTESIAN_POINT('Ctrl Pts',(132.273299175833,3.77953192755591,331.852886803579));
#53611=CARTESIAN_POINT('Ctrl Pts',(132.265550485275,3.69179326881099,331.747516884765));
#53612=CARTESIAN_POINT('Ctrl Pts',(132.257801794718,3.59959965147738,331.645764582577));
#53613=CARTESIAN_POINT('Ctrl Pts',(132.25005310416,3.50328759068137,331.548020985076));
#53614=CARTESIAN_POINT('Ctrl Pts',(132.242306025782,3.40699556841402,331.450297723946));
#53615=CARTESIAN_POINT('Ctrl Pts',(132.234558947404,3.3065870812436,331.356581786774));
#53616=CARTESIAN_POINT('Ctrl Pts',(132.226811869027,3.2024365677531,331.267228497213));
#53617=CARTESIAN_POINT('Ctrl Pts',(132.219064725721,3.09828518138123,331.177874458786));
#53618=CARTESIAN_POINT('Ctrl Pts',(132.211317582415,2.99039200279513,331.09288339541));
#53619=CARTESIAN_POINT('Ctrl Pts',(132.203570439109,2.8791654025531,331.012571048001));
#53620=CARTESIAN_POINT('Ctrl Pts',(132.195821554081,2.76791379620974,330.932240644671));
#53621=CARTESIAN_POINT('Ctrl Pts',(132.188072669053,2.65332759377652,330.856591279197));
#53622=CARTESIAN_POINT('Ctrl Pts',(132.180323784025,2.53584471459587,330.785895748091));
#53623=CARTESIAN_POINT('Ctrl Pts',(132.17256667425,2.41823713787328,330.715125180018));
#53624=CARTESIAN_POINT('Ctrl Pts',(132.164809564475,2.29772707811779,330.649319151615));
#53625=CARTESIAN_POINT('Ctrl Pts',(132.157052454701,2.17477814896891,330.588705058005));
#53626=CARTESIAN_POINT('Ctrl Pts',(132.149291199775,2.05176351984357,330.528058574163));
#53627=CARTESIAN_POINT('Ctrl Pts',(132.141529944848,1.92630778180462,330.472609711296));
#53628=CARTESIAN_POINT('Ctrl Pts',(132.133768689922,1.79889423665548,330.422537538349));
#53629=CARTESIAN_POINT('Ctrl Pts',(132.125995019518,1.67127687135808,330.372385266243));
#53630=CARTESIAN_POINT('Ctrl Pts',(132.118221349113,1.54169581023032,330.327626998984));
#53631=CARTESIAN_POINT('Ctrl Pts',(132.110447678708,1.41065006155037,330.288392050865));
#53632=CARTESIAN_POINT('Ctrl Pts',(132.103035874531,1.28570452399904,330.250983499021));
#53633=CARTESIAN_POINT('Ctrl Pts',(132.095624070354,1.15942787132853,330.218595689027));
#53634=CARTESIAN_POINT('Ctrl Pts',(132.088212266177,1.03225910621512,330.191297035568));
#53635=CARTESIAN_POINT('Ctrl Pts',(132.080437187398,0.898857421107762,330.162660393784));
#53636=CARTESIAN_POINT('Ctrl Pts',(132.07266210862,0.764052388230484,330.139533894822));
#53637=CARTESIAN_POINT('Ctrl Pts',(132.064887029842,0.628338922813376,330.122052351595));
#53638=CARTESIAN_POINT('Ctrl Pts',(132.057121518793,0.492792461454992,330.104592320521));
#53639=CARTESIAN_POINT('Ctrl Pts',(132.049356007744,0.356340175790856,330.092763473144));
#53640=CARTESIAN_POINT('Ctrl Pts',(132.041590496695,0.219489106663411,330.086650063902));
#53641=CARTESIAN_POINT('Ctrl Pts',(132.033832685172,0.0827737257694367,
330.080542716123));
#53642=CARTESIAN_POINT('Ctrl Pts',(132.02607487365,-0.0543392637600575,
330.080139546411));
#53643=CARTESIAN_POINT('Ctrl Pts',(132.018317062128,-0.19133608088388,330.085473210303));
#53644=CARTESIAN_POINT('Ctrl Pts',(132.010565088605,-0.328229803559003,
330.090802860443));
#53645=CARTESIAN_POINT('Ctrl Pts',(132.002813115082,-0.465007138834769,
330.101860735967));
#53646=CARTESIAN_POINT('Ctrl Pts',(131.995061141559,-0.601153032092159,
330.118627437441));
#53647=CARTESIAN_POINT('Ctrl Pts',(131.987312451001,-0.737241267482229,
330.135387038206));
#53648=CARTESIAN_POINT('Ctrl Pts',(131.979563760443,-0.872698205589537,
330.157850608628));
#53649=CARTESIAN_POINT('Ctrl Pts',(131.971815069886,-1.00701286447879,330.185946806144));
#53650=CARTESIAN_POINT('Ctrl Pts',(131.964067991508,-1.14129957808145,330.214037158012));
#53651=CARTESIAN_POINT('Ctrl Pts',(131.95632091313,-1.27444410283695,330.247757725972));
#53652=CARTESIAN_POINT('Ctrl Pts',(131.948573834752,-1.40594500930237,330.286985922648));
#53653=CARTESIAN_POINT('Ctrl Pts',(131.940826691446,-1.53744701787186,330.326214448094));
#53654=CARTESIAN_POINT('Ctrl Pts',(131.933079548141,-1.66730500611248,330.370950582588));
#53655=CARTESIAN_POINT('Ctrl Pts',(131.925332404835,-1.79503246800941,330.421021784143));
#53656=CARTESIAN_POINT('Ctrl Pts',(131.917583519807,-1.92278864575208,330.471104242767));
#53657=CARTESIAN_POINT('Ctrl Pts',(131.909834634779,-2.04841298017952,330.526524012566));
#53658=CARTESIAN_POINT('Ctrl Pts',(131.90208574975,-2.17143908760112,330.587060463666));
#53659=CARTESIAN_POINT('Ctrl Pts',(131.894328639976,-2.29459577620373,330.647661168781));
#53660=CARTESIAN_POINT('Ctrl Pts',(131.886571530201,-2.41514837759722,330.713389231081));
#53661=CARTESIAN_POINT('Ctrl Pts',(131.878814420426,-2.53265478242858,330.783977844515));
#53662=CARTESIAN_POINT('Ctrl Pts',(131.8710531655,-2.6502239789256,330.854604178247));
#53663=CARTESIAN_POINT('Ctrl Pts',(131.863291910574,-2.76474340916123,330.930096023493));
#53664=CARTESIAN_POINT('Ctrl Pts',(131.855530655648,-2.87580094790362,331.010143865935));
#53665=CARTESIAN_POINT('Ctrl Pts',(131.847756985243,-2.98703614251424,331.090319758837));
#53666=CARTESIAN_POINT('Ctrl Pts',(131.839983314838,-3.09479807186334,331.175065970988));
#53667=CARTESIAN_POINT('Ctrl Pts',(131.832209644434,-3.19870795079148,331.264032855064));
#53668=CARTESIAN_POINT('Ctrl Pts',(131.824797840257,-3.29778079985462,331.34885830928));
#53669=CARTESIAN_POINT('Ctrl Pts',(131.81738603608,-3.39335194275258,331.437520138104));
#53670=CARTESIAN_POINT('Ctrl Pts',(131.809974231903,-3.48512627858102,331.529686197929));
#53671=CARTESIAN_POINT('Ctrl Pts',(131.802305934558,-3.58007656045564,331.625041759816));
#53672=CARTESIAN_POINT('Ctrl Pts',(131.794637637212,-3.67128062595262,331.724468265431));
#53673=CARTESIAN_POINT('Ctrl Pts',(131.786969339867,-3.75836182038182,331.827635032094));
#53674=CARTESIAN_POINT('Ctrl Pts',(131.779310663728,-3.84533375638371,331.930672358197));
#53675=CARTESIAN_POINT('Ctrl Pts',(131.771651987588,-3.9281928520073,332.037440307722));
#53676=CARTESIAN_POINT('Ctrl Pts',(131.763993311449,-4.0065979590162,332.147570183632));
#53677=CARTESIAN_POINT('Ctrl Pts',(131.756343468794,-4.08491263390531,332.257573036207));
#53678=CARTESIAN_POINT('Ctrl Pts',(131.74869362614,-4.15878331438801,332.370929770508));
#53679=CARTESIAN_POINT('Ctrl Pts',(131.741043783485,-4.22790843468976,332.487237908122));
#53680=CARTESIAN_POINT('Ctrl Pts',(131.73339888633,-4.29698886672092,332.603470854409));
#53681=CARTESIAN_POINT('Ctrl Pts',(131.725753989175,-4.36132963354344,332.722651065717));
#53682=CARTESIAN_POINT('Ctrl Pts',(131.71810909202,-4.42067198370221,332.84434643901));
#53683=CARTESIAN_POINT('Ctrl Pts',(131.710467374888,-4.47998964941481,332.96599119107));
#53684=CARTESIAN_POINT('Ctrl Pts',(131.702825657756,-4.53431285765914,333.090148663068));
#53685=CARTESIAN_POINT('Ctrl Pts',(131.695183940624,-4.58342867096348,333.216361953565));
#53686=CARTESIAN_POINT('Ctrl Pts',(131.68754364097,-4.63253537367045,333.342551832489));
#53687=CARTESIAN_POINT('Ctrl Pts',(131.679903341317,-4.6764364583927,333.470796395842));
#53688=CARTESIAN_POINT('Ctrl Pts',(131.672263041663,-4.71496724219373,333.600619077042));
#53689=CARTESIAN_POINT('Ctrl Pts',(131.664619815753,-4.75351278339635,333.730491480703));
#53690=CARTESIAN_POINT('Ctrl Pts',(131.656976589842,-4.78668379738941,333.861942824209));
#53691=CARTESIAN_POINT('Ctrl Pts',(131.649333363932,-4.81436559811462,333.994481750444));
#53692=CARTESIAN_POINT('Ctrl Pts',(131.641688538834,-4.84205319068665,334.12704840772));
#53693=CARTESIAN_POINT('Ctrl Pts',(131.634043713736,-4.86424921182576,334.260702704538));
#53694=CARTESIAN_POINT('Ctrl Pts',(131.626398888638,-4.88089039629261,334.39494462908));
#53695=CARTESIAN_POINT('Ctrl Pts',(131.618747285445,-4.89754633525291,334.529305575896));
#53696=CARTESIAN_POINT('Ctrl Pts',(131.611095682253,-4.90863756668902,334.66425478993));
#53697=CARTESIAN_POINT('Ctrl Pts',(131.60344407906,-4.91415282542032,334.799288587984));
#53698=CARTESIAN_POINT('Ctrl Pts',(131.599568511552,-4.91694632594542,334.867683744793));
#53699=CARTESIAN_POINT('Ctrl Pts',(131.595692944044,-4.91831016231917,334.936100601925));
#53700=CARTESIAN_POINT('Ctrl Pts',(131.591817376536,-4.91824796507461,335.004473984742));
#53701=CARTESIAN_POINT('',(129.841817376473,-4.91824953106053,334.997852274953));
#53702=CARTESIAN_POINT('Ctrl Pts',(131.591817376508,-4.91824796507415,335.004473985242));
#53703=CARTESIAN_POINT('Ctrl Pts',(131.581074090443,-4.91807555087569,335.194008759026));
#53704=CARTESIAN_POINT('Ctrl Pts',(131.570330804377,-4.90694353044546,335.383064788424));
#53705=CARTESIAN_POINT('Ctrl Pts',(131.559587518311,-4.88503791690134,335.570602850445));
#53706=CARTESIAN_POINT('Ctrl Pts',(131.550303744751,-4.86610825658985,335.732663219235));
#53707=CARTESIAN_POINT('Ctrl Pts',(131.54101997119,-4.83913421272028,335.893590931491));
#53708=CARTESIAN_POINT('Ctrl Pts',(131.531736197629,-4.80426271790346,336.052731114703));
#53709=CARTESIAN_POINT('Ctrl Pts',(131.523961118851,-4.77505814741838,336.18600961974));
#53710=CARTESIAN_POINT('Ctrl Pts',(131.516186040072,-4.74025716358077,336.318282532187));
#53711=CARTESIAN_POINT('Ctrl Pts',(131.508410961294,-4.69994210963483,336.449043556482));
#53712=CARTESIAN_POINT('Ctrl Pts',(131.500645450245,-4.65967666592935,336.579643671011));
#53713=CARTESIAN_POINT('Ctrl Pts',(131.492879939196,-4.61391076720518,336.708735229245));
#53714=CARTESIAN_POINT('Ctrl Pts',(131.485114428147,-4.56277779568918,336.835821845841));
#53715=CARTESIAN_POINT('Ctrl Pts',(131.477356616625,-4.51169552266329,336.962782455686));
#53716=CARTESIAN_POINT('Ctrl Pts',(131.469598805102,-4.45525691182909,337.087741719651));
#53717=CARTESIAN_POINT('Ctrl Pts',(131.46184099358,-4.39364510016533,337.210218495148));
#53718=CARTESIAN_POINT('Ctrl Pts',(131.454089020057,-4.33207965334384,337.332603102987));
#53719=CARTESIAN_POINT('Ctrl Pts',(131.446337046534,-4.26534892946257,337.452508593045));
#53720=CARTESIAN_POINT('Ctrl Pts',(131.438585073011,-4.19368397053202,337.569474229838));
#53721=CARTESIAN_POINT('Ctrl Pts',(131.430836382454,-4.12204936175401,337.686390331615));
#53722=CARTESIAN_POINT('Ctrl Pts',(131.423087691896,-4.04548487787832,337.800368723805));
#53723=CARTESIAN_POINT('Ctrl Pts',(131.415339001338,-3.96426714921201,337.910973897543));
#53724=CARTESIAN_POINT('Ctrl Pts',(131.40759192296,-3.88306631857247,338.021556058951));
#53725=CARTESIAN_POINT('Ctrl Pts',(131.399844844583,-3.79721440005633,338.12876608303));
#53726=CARTESIAN_POINT('Ctrl Pts',(131.392097766205,-3.70703070643482,338.232198385627));
#53727=CARTESIAN_POINT('Ctrl Pts',(131.384350622899,-3.61684625698725,338.335631555086));
#53728=CARTESIAN_POINT('Ctrl Pts',(131.376603479593,-3.52233021689897,338.435286645299));
#53729=CARTESIAN_POINT('Ctrl Pts',(131.368856336287,-3.4238411819727,338.53079235061));
#53730=CARTESIAN_POINT('Ctrl Pts',(131.361107451259,-3.32533000462047,338.626319527632));
#53731=CARTESIAN_POINT('Ctrl Pts',(131.353358566231,-3.22284433558728,338.717695191391));
#53732=CARTESIAN_POINT('Ctrl Pts',(131.345609681203,-3.11677820083286,338.804586273081));
#53733=CARTESIAN_POINT('Ctrl Pts',(131.337852571428,-3.010599486387,338.891569581862));
#53734=CARTESIAN_POINT('Ctrl Pts',(131.330095461654,-2.90083301752187,338.974058551969));
#53735=CARTESIAN_POINT('Ctrl Pts',(131.322338351879,-2.78790479026287,339.051761338348));
#53736=CARTESIAN_POINT('Ctrl Pts',(131.314577096953,-2.67491621777008,339.129505646611));
#53737=CARTESIAN_POINT('Ctrl Pts',(131.306815842027,-2.55876285115244,339.202458467142));
#53738=CARTESIAN_POINT('Ctrl Pts',(131.2990545871,-2.4398971346612,339.270372938605));
#53739=CARTESIAN_POINT('Ctrl Pts',(131.291280916696,-2.3208412717617,339.33839605109));
#53740=CARTESIAN_POINT('Ctrl Pts',(131.283507246291,-2.19906473601633,339.401364529178));
#53741=CARTESIAN_POINT('Ctrl Pts',(131.275733575886,-2.07504268568888,339.459078482721));
#53742=CARTESIAN_POINT('Ctrl Pts',(131.268321771709,-1.95679389164187,339.514105837842));
#53743=CARTESIAN_POINT('Ctrl Pts',(131.260909967532,-1.83650420126968,339.56435674466));
#53744=CARTESIAN_POINT('Ctrl Pts',(131.253498163355,-1.71459817180724,339.609700225799));
#53745=CARTESIAN_POINT('Ctrl Pts',(131.245723084577,-1.58671716470171,339.657266126021));
#53746=CARTESIAN_POINT('Ctrl Pts',(131.237948005798,-1.4566532414712,339.699581699009));
#53747=CARTESIAN_POINT('Ctrl Pts',(131.23017292702,-1.32487671751047,339.736442203374));
#53748=CARTESIAN_POINT('Ctrl Pts',(131.222407415971,-1.19326235295174,339.773257348541));
#53749=CARTESIAN_POINT('Ctrl Pts',(131.214641904922,-1.05993995373909,339.804630677363));
#53750=CARTESIAN_POINT('Ctrl Pts',(131.206876393873,-0.925399121672873,
339.83040573121));
#53751=CARTESIAN_POINT('Ctrl Pts',(131.19911858235,-0.790991687233353,339.856155229016));
#53752=CARTESIAN_POINT('Ctrl Pts',(131.191360770828,-0.655368605507206,
339.876317424993));
#53753=CARTESIAN_POINT('Ctrl Pts',(131.183602959306,-0.51903358548839,339.890785949071));
#53754=CARTESIAN_POINT('Ctrl Pts',(131.175850985783,-0.38280116189571,339.905243585127));
#53755=CARTESIAN_POINT('Ctrl Pts',(131.16809901226,-0.245858253533314,339.914016036624));
#53756=CARTESIAN_POINT('Ctrl Pts',(131.160347038737,-0.108717332789754,
339.91704826131));
#53757=CARTESIAN_POINT('Ctrl Pts',(131.152598348179,0.028365508692543,339.920079201847));
#53758=CARTESIAN_POINT('Ctrl Pts',(131.144849657622,0.165645805802129,339.917374742017));
#53759=CARTESIAN_POINT('Ctrl Pts',(131.137100967064,0.302607629310269,339.908931827311));
#53760=CARTESIAN_POINT('Ctrl Pts',(131.129353888686,0.439540956767055,339.900490669223));
#53761=CARTESIAN_POINT('Ctrl Pts',(131.121606810308,0.576155552531599,339.886313455111));
#53762=CARTESIAN_POINT('Ctrl Pts',(131.113859731931,0.711937553774379,339.86644921704));
#53763=CARTESIAN_POINT('Ctrl Pts',(131.106112588625,0.847720693001064,339.846584812486));
#53764=CARTESIAN_POINT('Ctrl Pts',(131.098365445319,0.98267083703049,339.821033345487));
#53765=CARTESIAN_POINT('Ctrl Pts',(131.090618302013,1.11628169025015,339.789895432106));
#53766=CARTESIAN_POINT('Ctrl Pts',(131.082869416985,1.24992258202608,339.758750518261));
#53767=CARTESIAN_POINT('Ctrl Pts',(131.075120531957,1.38222320323586,339.72201674753));
#53768=CARTESIAN_POINT('Ctrl Pts',(131.067371646929,1.51269023915775,339.679845222105));
#53769=CARTESIAN_POINT('Ctrl Pts',(131.059614537154,1.64329575413968,339.637628935386));
#53770=CARTESIAN_POINT('Ctrl Pts',(131.051857427379,1.77206342362917,339.589963484894));
#53771=CARTESIAN_POINT('Ctrl Pts',(131.044100317605,1.89851729800148,339.537049165668));
#53772=CARTESIAN_POINT('Ctrl Pts',(131.036339062678,2.02503874528109,339.484106570722));
#53773=CARTESIAN_POINT('Ctrl Pts',(131.028577807752,2.14924358000155,339.425909683931));
#53774=CARTESIAN_POINT('Ctrl Pts',(131.020816552826,2.27067936765368,339.362705384485));
#53775=CARTESIAN_POINT('Ctrl Pts',(131.013042882421,2.39230941299019,339.299399978758));
#53776=CARTESIAN_POINT('Ctrl Pts',(131.005269212017,2.51116122061661,339.231071348485));
#53777=CARTESIAN_POINT('Ctrl Pts',(130.997495541612,2.62680956324,339.158010892358));
#53778=CARTESIAN_POINT('Ctrl Pts',(130.990083737435,2.73707444768979,339.088351418042));
#53779=CARTESIAN_POINT('Ctrl Pts',(130.982671933258,2.84442716096901,339.014390900217));
#53780=CARTESIAN_POINT('Ctrl Pts',(130.975260129081,2.9485278091276,338.936415478745));
#53781=CARTESIAN_POINT('Ctrl Pts',(130.967485050303,3.05773074015337,338.854618249589));
#53782=CARTESIAN_POINT('Ctrl Pts',(130.959709971524,3.16369986016846,338.768144106363));
#53783=CARTESIAN_POINT('Ctrl Pts',(130.951934892746,3.2660084831235,338.677277750003));
#53784=CARTESIAN_POINT('Ctrl Pts',(130.944169381697,3.36819120880474,338.586523210479));
#53785=CARTESIAN_POINT('Ctrl Pts',(130.936403870648,3.46672211058377,338.491387469099));
#53786=CARTESIAN_POINT('Ctrl Pts',(130.928638359599,3.56120466743245,338.392197573721));
#53787=CARTESIAN_POINT('Ctrl Pts',(130.920880548077,3.65559354455092,338.293106025412));
#53788=CARTESIAN_POINT('Ctrl Pts',(130.913122736554,3.74594179686235,338.189968603747));
#53789=CARTESIAN_POINT('Ctrl Pts',(130.905364925032,3.83188738966656,338.083151325416));
#53790=CARTESIAN_POINT('Ctrl Pts',(130.897612951509,3.91776830568666,337.976414430474));
#53791=CARTESIAN_POINT('Ctrl Pts',(130.889860977986,3.99925291279998,337.866003494152));
#53792=CARTESIAN_POINT('Ctrl Pts',(130.882109004463,4.07601759658679,337.752319678892));
#53793=CARTESIAN_POINT('Ctrl Pts',(130.874360313905,4.15274977048444,337.638684008795));
#53794=CARTESIAN_POINT('Ctrl Pts',(130.866611623348,4.22476577842427,337.521778539813));
#53795=CARTESIAN_POINT('Ctrl Pts',(130.85886293279,4.29178385289398,337.402035474871));
#53796=CARTESIAN_POINT('Ctrl Pts',(130.851115854412,4.35878798369353,337.282317323473));
#53797=CARTESIAN_POINT('Ctrl Pts',(130.843368776035,4.42079605860149,337.159763091306));
#53798=CARTESIAN_POINT('Ctrl Pts',(130.835621697657,4.47757122906411,337.034831430649));
#53799=CARTESIAN_POINT('Ctrl Pts',(130.827874554351,4.53434687535731,336.909898722944));
#53800=CARTESIAN_POINT('Ctrl Pts',(130.820127411045,4.58588936801282,336.782588902859));
#53801=CARTESIAN_POINT('Ctrl Pts',(130.812380267739,4.63200933161903,336.6533821743));
#53802=CARTESIAN_POINT('Ctrl Pts',(130.804631382711,4.6781396639722,336.524146397326));
#53803=CARTESIAN_POINT('Ctrl Pts',(130.796882497683,4.71884491002831,336.393013231315));
#53804=CARTESIAN_POINT('Ctrl Pts',(130.789133612655,4.75398517394242,336.260479285207));
#53805=CARTESIAN_POINT('Ctrl Pts',(130.78137650288,4.78916273609574,336.127804666199));
#53806=CARTESIAN_POINT('Ctrl Pts',(130.773619393106,4.81876341652676,335.993726675483));
#53807=CARTESIAN_POINT('Ctrl Pts',(130.765862283331,4.84269808395704,335.858753940392));
#53808=CARTESIAN_POINT('Ctrl Pts',(130.758101028405,4.8666455413083,335.723709080187));
#53809=CARTESIAN_POINT('Ctrl Pts',(130.750339773478,4.8849209005688,335.587768910098));
#53810=CARTESIAN_POINT('Ctrl Pts',(130.742578518552,4.89748692944257,335.45144749245));
#53811=CARTESIAN_POINT('Ctrl Pts',(130.734804848148,4.91007305986728,335.314908004961));
#53812=CARTESIAN_POINT('Ctrl Pts',(130.727031177743,4.91693158976578,335.177986441799));
#53813=CARTESIAN_POINT('Ctrl Pts',(130.719257507338,4.91807744762636,335.04119807822));
#53814=CARTESIAN_POINT('Ctrl Pts',(130.711845703161,4.91916996552786,334.910777245874));
#53815=CARTESIAN_POINT('Ctrl Pts',(130.704433898984,4.91506970126257,334.780477778956));
#53816=CARTESIAN_POINT('Ctrl Pts',(130.697022094807,4.90583333982647,334.650740348241));
#53817=CARTESIAN_POINT('Ctrl Pts',(130.689247016028,4.89614427680274,334.514644099578));
#53818=CARTESIAN_POINT('Ctrl Pts',(130.68147193725,4.8807722962662,334.378736285021));
#53819=CARTESIAN_POINT('Ctrl Pts',(130.673696858472,4.85972590500248,334.243529781982));
#53820=CARTESIAN_POINT('Ctrl Pts',(130.665931347423,4.83870541266309,334.108489659153));
#53821=CARTESIAN_POINT('Ctrl Pts',(130.658165836374,4.8120244627596,333.974149513234));
#53822=CARTESIAN_POINT('Ctrl Pts',(130.650400325325,4.77974349653092,333.841019771579));
#53823=CARTESIAN_POINT('Ctrl Pts',(130.642642513802,4.74749453697426,333.70802202845));
#53824=CARTESIAN_POINT('Ctrl Pts',(130.63488470228,4.70965670226278,333.576232678699));
#53825=CARTESIAN_POINT('Ctrl Pts',(130.627126890758,4.66634186589082,333.446154237662));
#53826=CARTESIAN_POINT('Ctrl Pts',(130.619374917235,4.62305962530683,333.316173684777));
#53827=CARTESIAN_POINT('Ctrl Pts',(130.611622943712,4.57430870993389,333.187901847236));
#53828=CARTESIAN_POINT('Ctrl Pts',(130.603870970189,4.52025133949755,333.061827951324));
#53829=CARTESIAN_POINT('Ctrl Pts',(130.596122279631,4.46621686238968,332.935807447781));
#53830=CARTESIAN_POINT('Ctrl Pts',(130.588373589074,4.40688055362788,332.81198339301));
#53831=CARTESIAN_POINT('Ctrl Pts',(130.580624898516,4.34245338130343,332.690826621125));
#53832=CARTESIAN_POINT('Ctrl Pts',(130.572877820138,4.27803961359029,332.569695056918));
#53833=CARTESIAN_POINT('Ctrl Pts',(130.56513074176,4.20853727253625,332.451230016657));
#53834=CARTESIAN_POINT('Ctrl Pts',(130.557383663382,4.13420387628524,332.335878874411));
#53835=CARTESIAN_POINT('Ctrl Pts',(130.549636520077,4.0598698570488,332.220526765412));
#53836=CARTESIAN_POINT('Ctrl Pts',(130.541889376771,3.98070491358631,332.108288935043));
#53837=CARTESIAN_POINT('Ctrl Pts',(130.534142233465,3.89701037770713,331.999584499016));
#53838=CARTESIAN_POINT('Ctrl Pts',(130.526393348437,3.81329702551945,331.890855623925));
#53839=CARTESIAN_POINT('Ctrl Pts',(130.518644463409,3.72505229292445,331.78566203356));
#53840=CARTESIAN_POINT('Ctrl Pts',(130.510895578381,3.63261808330605,331.684390112915));
#53841=CARTESIAN_POINT('Ctrl Pts',(130.503138468606,3.54008576306248,331.583010701206));
#53842=CARTESIAN_POINT('Ctrl Pts',(130.495381358831,3.44335534690867,331.485561563359));
#53843=CARTESIAN_POINT('Ctrl Pts',(130.487624249057,3.34280631637109,331.392392899202));
#53844=CARTESIAN_POINT('Ctrl Pts',(130.47986299413,3.24220355564657,331.299174448689));
#53845=CARTESIAN_POINT('Ctrl Pts',(130.472101739204,3.13777841199752,331.210241282919));
#53846=CARTESIAN_POINT('Ctrl Pts',(130.464340484278,3.02994302286966,331.125902899944));
#53847=CARTESIAN_POINT('Ctrl Pts',(130.456566813873,2.92193513226267,331.041429603042));
#53848=CARTESIAN_POINT('Ctrl Pts',(130.448793143469,2.810506412777,330.961566004546));
#53849=CARTESIAN_POINT('Ctrl Pts',(130.441019473064,2.69609824902881,330.886578395778));
#53850=CARTESIAN_POINT('Ctrl Pts',(130.433607668887,2.58701581282919,330.815081478239));
#53851=CARTESIAN_POINT('Ctrl Pts',(130.42619586471,2.47522532301588,330.748016959806));
#53852=CARTESIAN_POINT('Ctrl Pts',(130.418784060533,2.36112802454671,330.685575645095));
#53853=CARTESIAN_POINT('Ctrl Pts',(130.411008981755,2.24143847760014,330.620073895546));
#53854=CARTESIAN_POINT('Ctrl Pts',(130.403233902976,2.11883203616041,330.55945300508));
#53855=CARTESIAN_POINT('Ctrl Pts',(130.395458824198,1.99374459329656,330.503983367557));
#53856=CARTESIAN_POINT('Ctrl Pts',(130.387693313149,1.86881107849457,330.448581988955));
#53857=CARTESIAN_POINT('Ctrl Pts',(130.3799278021,1.74140299082494,330.398319407549));
#53858=CARTESIAN_POINT('Ctrl Pts',(130.372162291051,1.61198226776083,330.353421018542));
#53859=CARTESIAN_POINT('Ctrl Pts',(130.364404479528,1.48268986572056,330.308567146419));
#53860=CARTESIAN_POINT('Ctrl Pts',(130.356646668006,1.35138916641562,330.269067009641));
#53861=CARTESIAN_POINT('Ctrl Pts',(130.348888856484,1.21856328688035,330.235098471283));
#53862=CARTESIAN_POINT('Ctrl Pts',(130.341136882961,1.08583736303154,330.201155495328));
#53863=CARTESIAN_POINT('Ctrl Pts',(130.333384909438,0.951588920647927,330.17273592859));
#53864=CARTESIAN_POINT('Ctrl Pts',(130.325632935915,0.816317146952556,330.149968105456));
#53865=CARTESIAN_POINT('Ctrl Pts',(130.317884245357,0.681102660933657,330.12720992451));
#53866=CARTESIAN_POINT('Ctrl Pts',(130.3101355548,0.544866090218616,330.110098791372));
#53867=CARTESIAN_POINT('Ctrl Pts',(130.302386864242,0.40811753619882,330.098712093832));
#53868=CARTESIAN_POINT('Ctrl Pts',(130.294639785864,0.271397433857881,330.087327765389));
#53869=CARTESIAN_POINT('Ctrl Pts',(130.286892707487,0.134165949374462,330.081665535942));
#53870=CARTESIAN_POINT('Ctrl Pts',(130.279145629109,-0.00306135300955948,
330.081750952766));
#53871=CARTESIAN_POINT('Ctrl Pts',(130.271398485803,-0.140289805490502,
330.081836370306));
#53872=CARTESIAN_POINT('Ctrl Pts',(130.263651342497,-0.277513684927922,
330.087669529956));
#53873=CARTESIAN_POINT('Ctrl Pts',(130.255904199191,-0.41421748004531,330.099223842928));
#53874=CARTESIAN_POINT('Ctrl Pts',(130.248155314163,-0.550952009078004,
330.110780753555));
#53875=CARTESIAN_POINT('Ctrl Pts',(130.240406429135,-0.687165831711539,
330.12806134406));
#53876=CARTESIAN_POINT('Ctrl Pts',(130.232657544107,-0.822349005022078,
330.150987195682));
#53877=CARTESIAN_POINT('Ctrl Pts',(130.224900434332,-0.957675663149658,
330.17393738104));
#53878=CARTESIAN_POINT('Ctrl Pts',(130.217143324558,-1.09196910072239,330.202544731517));
#53879=CARTESIAN_POINT('Ctrl Pts',(130.209386214783,-1.22472946800457,330.236679646224));
#53880=CARTESIAN_POINT('Ctrl Pts',(130.201624959857,-1.35756077818208,330.270832801537));
#53881=CARTESIAN_POINT('Ctrl Pts',(130.193863704931,-1.48885701172631,330.310519293661));
#53882=CARTESIAN_POINT('Ctrl Pts',(130.186102450004,-1.61813487390069,330.355560034583));
#53883=CARTESIAN_POINT('Ctrl Pts',(130.1783287796,-1.74761953852298,330.400672826011));
#53884=CARTESIAN_POINT('Ctrl Pts',(130.170555109195,-1.87507901620582,330.451156837735));
#53885=CARTESIAN_POINT('Ctrl Pts',(130.16278143879,-2.00005051835259,330.506785005529));
#53886=CARTESIAN_POINT('Ctrl Pts',(130.155369634613,-2.11920456700869,330.55982366873));
#53887=CARTESIAN_POINT('Ctrl Pts',(130.147957830436,-2.23609679989502,330.617538217474));
#53888=CARTESIAN_POINT('Ctrl Pts',(130.140546026259,-2.35034962866728,330.679694491645));
#53889=CARTESIAN_POINT('Ctrl Pts',(130.132770947481,-2.47020232891869,330.744897229967));
#53890=CARTESIAN_POINT('Ctrl Pts',(130.124995868702,-2.58752910962054,330.81519416001));
#53891=CARTESIAN_POINT('Ctrl Pts',(130.117220789924,-2.70186670405607,330.890365055627));
#53892=CARTESIAN_POINT('Ctrl Pts',(130.109455278875,-2.81606359880259,330.965443448671));
#53893=CARTESIAN_POINT('Ctrl Pts',(130.101689767826,-2.9272783027243,331.04538366086));
#53894=CARTESIAN_POINT('Ctrl Pts',(130.093924256777,-3.03507129531473,331.129919213394));
#53895=CARTESIAN_POINT('Ctrl Pts',(130.086166445255,-3.142757410839,331.214370948682));
#53896=CARTESIAN_POINT('Ctrl Pts',(130.078408633732,-3.24702826098043,331.303408717377));
#53897=CARTESIAN_POINT('Ctrl Pts',(130.07065082221,-3.34747283453631,331.396722507974));
#53898=CARTESIAN_POINT('Ctrl Pts',(130.062898848687,-3.44784182036548,331.489966076985));
#53899=CARTESIAN_POINT('Ctrl Pts',(130.055146875164,-3.54438997568825,331.587478997974));
#53900=CARTESIAN_POINT('Ctrl Pts',(130.047394901641,-3.63673924253068,331.688910942856));
#53901=CARTESIAN_POINT('Ctrl Pts',(130.039646211084,-3.72904939940371,331.79029993125));
#53902=CARTESIAN_POINT('Ctrl Pts',(130.031897520526,-3.81716394197539,331.895604354067));
#53903=CARTESIAN_POINT('Ctrl Pts',(130.024148829968,-3.90074174807203,332.004437135137));
#53904=CARTESIAN_POINT('Ctrl Pts',(130.016401751591,-3.98430216510805,332.113247272638));
#53905=CARTESIAN_POINT('Ctrl Pts',(130.008654673213,-4.06332748524398,332.225583998392));
#53906=CARTESIAN_POINT('Ctrl Pts',(130.000907594835,-4.13751722383503,332.341027588528));
#53907=CARTESIAN_POINT('Ctrl Pts',(129.993160451529,-4.21170758420752,332.456472146192));
#53908=CARTESIAN_POINT('Ctrl Pts',(129.985413308223,-4.28106207088147,332.575023291347));
#53909=CARTESIAN_POINT('Ctrl Pts',(129.977666164917,-4.34532407020271,332.696233130845));
#53910=CARTESIAN_POINT('Ctrl Pts',(129.969917279889,-4.40960051698553,332.817470220887));
#53911=CARTESIAN_POINT('Ctrl Pts',(129.962168394861,-4.46878201513965,332.941366849416));
#53912=CARTESIAN_POINT('Ctrl Pts',(129.954419509833,-4.52265854929574,333.067451757657));
#53913=CARTESIAN_POINT('Ctrl Pts',(129.946662400058,-4.57659226856202,333.193670493723));
#53914=CARTESIAN_POINT('Ctrl Pts',(129.938905290284,-4.62520962206125,333.322081789236));
#53915=CARTESIAN_POINT('Ctrl Pts',(129.931148180509,-4.66834909657316,333.45219517541));
#53916=CARTESIAN_POINT('Ctrl Pts',(129.923386925583,-4.71151162344086,333.582378090017));
#53917=CARTESIAN_POINT('Ctrl Pts',(129.915625670657,-4.74919033128616,333.714264531986));
#53918=CARTESIAN_POINT('Ctrl Pts',(129.90786441573,-4.78127428052794,333.84735117366));
#53919=CARTESIAN_POINT('Ctrl Pts',(129.900090745326,-4.81340955363239,333.980650710589));
#53920=CARTESIAN_POINT('Ctrl Pts',(129.892317074921,-4.83993210814188,334.115153900117));
#53921=CARTESIAN_POINT('Ctrl Pts',(129.884543404516,-4.8607824457437,334.250348695959));
#53922=CARTESIAN_POINT('Ctrl Pts',(129.877131600339,-4.88066219511398,334.37925014153));
#53923=CARTESIAN_POINT('Ctrl Pts',(129.869719796162,-4.89538589427849,334.508779967937));
#53924=CARTESIAN_POINT('Ctrl Pts',(129.862307991985,-4.90494611875688,334.638493935608));
#53925=CARTESIAN_POINT('Ctrl Pts',(129.855477786826,-4.91375615919946,334.758029340216));
#53926=CARTESIAN_POINT('Ctrl Pts',(129.848647581667,-4.91819714564155,334.877890695419));
#53927=CARTESIAN_POINT('Ctrl Pts',(129.841817376508,-4.91824953106026,334.997852274342));
#53928=CARTESIAN_POINT('',(128.091817376563,-4.91824887636649,334.996675451945));
#53929=CARTESIAN_POINT('Ctrl Pts',(129.841817376473,-4.91824953106053,334.997852274953));
#53930=CARTESIAN_POINT('Ctrl Pts',(129.834124842131,-4.91830853024261,335.1329592804));
#53931=CARTESIAN_POINT('Ctrl Pts',(129.826432307789,-4.91279613065993,335.268293179147));
#53932=CARTESIAN_POINT('Ctrl Pts',(129.818739773447,-4.90168251187349,335.403350486914));
#53933=CARTESIAN_POINT('Ctrl Pts',(129.811056230747,-4.89058188356311,335.538249929025));
#53934=CARTESIAN_POINT('Ctrl Pts',(129.803372688047,-4.87389309065989,335.672873028552));
#53935=CARTESIAN_POINT('Ctrl Pts',(129.795689145347,-4.85163830171469,335.806714851627));
#53936=CARTESIAN_POINT('Ctrl Pts',(129.788012653009,-4.82940393360061,335.940433862426));
#53937=CARTESIAN_POINT('Ctrl Pts',(129.780336160671,-4.80161379497764,336.073372630984));
#53938=CARTESIAN_POINT('Ctrl Pts',(129.772659668334,-4.768341939498,336.205030377428));
#53939=CARTESIAN_POINT('Ctrl Pts',(129.764801763724,-4.73428379744144,336.339799483827));
#53940=CARTESIAN_POINT('Ctrl Pts',(129.756943859115,-4.69448163524061,336.473225839371));
#53941=CARTESIAN_POINT('Ctrl Pts',(129.749085954506,-4.64907069308588,336.60478183975));
#53942=CARTESIAN_POINT('Ctrl Pts',(129.741416910387,-4.60475117838075,336.733175962766));
#53943=CARTESIAN_POINT('Ctrl Pts',(129.733747866268,-4.55508957025285,336.859788217815));
#53944=CARTESIAN_POINT('Ctrl Pts',(129.726078822148,-4.50026218666953,336.98414296706));
#53945=CARTESIAN_POINT('Ctrl Pts',(129.71841056241,-4.44544041076472,337.108484997451));
#53946=CARTESIAN_POINT('Ctrl Pts',(129.710742302671,-4.38545407126322,337.230569615472));
#53947=CARTESIAN_POINT('Ctrl Pts',(129.703074042932,-4.32052742086686,337.349941673327));
#53948=CARTESIAN_POINT('Ctrl Pts',(129.695404824386,-4.25559265230907,337.469328656972));
#53949=CARTESIAN_POINT('Ctrl Pts',(129.68773560584,-4.18571653553597,337.586002054872));
#53950=CARTESIAN_POINT('Ctrl Pts',(129.680066387293,-4.11116875989336,337.699532272483));
#53951=CARTESIAN_POINT('Ctrl Pts',(129.672066684828,-4.0334085525173,337.817954763144));
#53952=CARTESIAN_POINT('Ctrl Pts',(129.664066982363,-3.95056533088207,337.932956728345));
#53953=CARTESIAN_POINT('Ctrl Pts',(129.656067279898,-3.86299387396652,338.044086298415));
#53954=CARTESIAN_POINT('Ctrl Pts',(129.648386724832,-3.7789160723258,338.150782364438));
#53955=CARTESIAN_POINT('Ctrl Pts',(129.640706169766,-3.69048034393063,338.25390879637));
#53956=CARTESIAN_POINT('Ctrl Pts',(129.6330256147,-3.59803973352374,338.353102017309));
#53957=CARTESIAN_POINT('Ctrl Pts',(129.625339857815,-3.50553651575038,338.452362418964));
#53958=CARTESIAN_POINT('Ctrl Pts',(129.61765410093,-3.40902329967104,338.547684026976));
#53959=CARTESIAN_POINT('Ctrl Pts',(129.609968344045,-3.30888767288203,338.638742286938));
#53960=CARTESIAN_POINT('Ctrl Pts',(129.602272103373,-3.20861545569685,338.729924755278));
#53961=CARTESIAN_POINT('Ctrl Pts',(129.594575862701,-3.10471127504674,338.816832019167));
#53962=CARTESIAN_POINT('Ctrl Pts',(129.586879622029,-2.99759335683159,338.89918159741));
#53963=CARTESIAN_POINT('Ctrl Pts',(129.585943067257,-2.98455818787116,338.909202709509));
#53964=CARTESIAN_POINT('Ctrl Pts',(129.585006512484,-2.97147546006877,338.919156384379));
#53965=CARTESIAN_POINT('Ctrl Pts',(129.584069957712,-2.95834595254926,338.929042159043));
#53966=CARTESIAN_POINT('Ctrl Pts',(129.576294878933,-2.84934757008491,339.011111760372));
#53967=CARTESIAN_POINT('Ctrl Pts',(129.568519800155,-2.73675923381156,339.088771907027));
#53968=CARTESIAN_POINT('Ctrl Pts',(129.560744721376,-2.62097331088899,339.161692199828));
#53969=CARTESIAN_POINT('Ctrl Pts',(129.552979210327,-2.50532986991576,339.234522759566));
#53970=CARTESIAN_POINT('Ctrl Pts',(129.545213699278,-2.38649699907022,339.302624864524));
#53971=CARTESIAN_POINT('Ctrl Pts',(129.537448188229,-2.26489932397997,339.365708890287));
#53972=CARTESIAN_POINT('Ctrl Pts',(129.529690376707,-2.14342221333894,339.428730368055));
#53973=CARTESIAN_POINT('Ctrl Pts',(129.521932565185,-2.01918609854448,339.486743489193));
#53974=CARTESIAN_POINT('Ctrl Pts',(129.514174753663,-1.89264341481996,339.539502612274));
#53975=CARTESIAN_POINT('Ctrl Pts',(129.50642278014,-1.76619595847742,339.592222032441));
#53976=CARTESIAN_POINT('Ctrl Pts',(129.498670806617,-1.63744574748366,339.639695174586));
#53977=CARTESIAN_POINT('Ctrl Pts',(129.490918833094,-1.50686825842056,339.681723092438));
#53978=CARTESIAN_POINT('Ctrl Pts',(129.483170142536,-1.37634606900174,339.723733211441));
#53979=CARTESIAN_POINT('Ctrl Pts',(129.475421451978,-1.24399851195549,339.760302573226));
#53980=CARTESIAN_POINT('Ctrl Pts',(129.467672761421,-1.11031920741886,339.791281072963));
#53981=CARTESIAN_POINT('Ctrl Pts',(129.459925683043,-0.97666771597813,339.822253127365));
#53982=CARTESIAN_POINT('Ctrl Pts',(129.452178604665,-0.841685408725561,
339.847636545272));
#53983=CARTESIAN_POINT('Ctrl Pts',(129.444431526287,-0.7058787838073,339.867331733617));
#53984=CARTESIAN_POINT('Ctrl Pts',(129.436684382981,-0.570071020698901,
339.887027087026));
#53985=CARTESIAN_POINT('Ctrl Pts',(129.428937239676,-0.433439312972735,
339.901034059688));
#53986=CARTESIAN_POINT('Ctrl Pts',(129.42119009637,-0.296497621167412,339.909304657805));
#53987=CARTESIAN_POINT('Ctrl Pts',(129.413441211342,-0.159525141962369,
339.917577115328));
#53988=CARTESIAN_POINT('Ctrl Pts',(129.405692326314,-0.0222429300879784,
339.92011060847));
#53989=CARTESIAN_POINT('Ctrl Pts',(129.397943441285,0.114833093437252,339.916909234789));
#53990=CARTESIAN_POINT('Ctrl Pts',(129.390186331511,0.252054610870299,339.913704463136));
#53991=CARTESIAN_POINT('Ctrl Pts',(129.382429221736,0.389069111394956,339.904752674354));
#53992=CARTESIAN_POINT('Ctrl Pts',(129.374672111961,0.525363284476724,339.890110068477));
#53993=CARTESIAN_POINT('Ctrl Pts',(129.366910857035,0.661730288806791,339.875459638061));
#53994=CARTESIAN_POINT('Ctrl Pts',(129.359149602109,0.797375812352754,339.855112389056));
#53995=CARTESIAN_POINT('Ctrl Pts',(129.351388347183,0.931795793713294,339.829175878068));
#53996=CARTESIAN_POINT('Ctrl Pts',(129.343614676778,1.06643080323655,339.803197877116));
#53997=CARTESIAN_POINT('Ctrl Pts',(129.335841006373,1.19983597241944,339.77161283752));
#53998=CARTESIAN_POINT('Ctrl Pts',(129.328067335969,1.33152061665565,339.734578746829));
#53999=CARTESIAN_POINT('Ctrl Pts',(129.320655531791,1.45707530902113,339.699268601968));
#54000=CARTESIAN_POINT('Ctrl Pts',(129.313243727614,1.58106577881586,339.659005384936));
#54001=CARTESIAN_POINT('Ctrl Pts',(129.305831923437,1.70308462919649,339.613966385692));
#54002=CARTESIAN_POINT('Ctrl Pts',(129.298056844659,1.83108398690973,339.566719890931));
#54003=CARTESIAN_POINT('Ctrl Pts',(129.29028176588,1.9573180701139,339.514068318486));
#54004=CARTESIAN_POINT('Ctrl Pts',(129.282506687102,2.08129670670435,339.456162820315));
#54005=CARTESIAN_POINT('Ctrl Pts',(129.274741176053,2.20512277968961,339.398328578547));
#54006=CARTESIAN_POINT('Ctrl Pts',(129.266975665004,2.3266985776872,339.335253438956));
#54007=CARTESIAN_POINT('Ctrl Pts',(129.259210153955,2.44555076005456,339.267137745901));
#54008=CARTESIAN_POINT('Ctrl Pts',(129.251452342433,2.56428510013716,339.199089589755));
#54009=CARTESIAN_POINT('Ctrl Pts',(129.24369453091,2.68030086174008,339.126011019002));
#54010=CARTESIAN_POINT('Ctrl Pts',(129.235936719388,2.79314664108628,339.048149565405));
#54011=CARTESIAN_POINT('Ctrl Pts',(129.228184745865,2.90590750040521,338.970346705021));
#54012=CARTESIAN_POINT('Ctrl Pts',(129.220432772342,3.01550280528449,338.887768347053));
#54013=CARTESIAN_POINT('Ctrl Pts',(129.212680798819,3.12150794989926,338.800706668663));
#54014=CARTESIAN_POINT('Ctrl Pts',(129.204932108261,3.2274682012721,338.713681860944));
#54015=CARTESIAN_POINT('Ctrl Pts',(129.197183417704,3.32984101498881,338.622177756724));
#54016=CARTESIAN_POINT('Ctrl Pts',(129.189434727146,3.42823303851712,338.52652822137));
#54017=CARTESIAN_POINT('Ctrl Pts',(129.181687648768,3.52660459076311,338.430898586701));
#54018=CARTESIAN_POINT('Ctrl Pts',(129.173940570391,3.62099672014969,338.33112550874));
#54019=CARTESIAN_POINT('Ctrl Pts',(129.166193492013,3.71105158153307,338.227581017062));
#54020=CARTESIAN_POINT('Ctrl Pts',(129.158446348707,3.80110719766293,338.124035657582));
#54021=CARTESIAN_POINT('Ctrl Pts',(129.150699205401,3.88682521677621,338.016719116272));
#54022=CARTESIAN_POINT('Ctrl Pts',(129.142952062095,3.96788714632693,337.906037621318));
#54023=CARTESIAN_POINT('Ctrl Pts',(129.135203177067,4.04896730032052,337.795331242813));
#54024=CARTESIAN_POINT('Ctrl Pts',(129.127454292039,4.12538905085071,337.681258720571));
#54025=CARTESIAN_POINT('Ctrl Pts',(129.119705407011,4.19687664917404,337.564256121006));
#54026=CARTESIAN_POINT('Ctrl Pts',(129.111948297236,4.26844012517271,337.447129333673));
#54027=CARTESIAN_POINT('Ctrl Pts',(129.104191187462,4.33505878313159,337.327066590542));
#54028=CARTESIAN_POINT('Ctrl Pts',(129.096434077687,4.39650210107624,337.204529958456));
#54029=CARTESIAN_POINT('Ctrl Pts',(129.088672822761,4.45797825236537,337.081927846713));
#54030=CARTESIAN_POINT('Ctrl Pts',(129.080911567834,4.51427339271712,336.956849568132));
#54031=CARTESIAN_POINT('Ctrl Pts',(129.073150312908,4.56520519222738,336.829777203749));
#54032=CARTESIAN_POINT('Ctrl Pts',(129.065376642504,4.61621846601826,336.702501564996));
#54033=CARTESIAN_POINT('Ctrl Pts',(129.057602972099,4.66185112421688,336.573225834882));
#54034=CARTESIAN_POINT('Ctrl Pts',(129.049829301694,4.70197048432592,336.442448136686));
#54035=CARTESIAN_POINT('Ctrl Pts',(129.042417497517,4.7402222785698,336.317758171804));
#54036=CARTESIAN_POINT('Ctrl Pts',(129.03500569334,4.77346243816642,336.191703203493));
#54037=CARTESIAN_POINT('Ctrl Pts',(129.027593889163,4.80161958421862,336.064721762222));
#54038=CARTESIAN_POINT('Ctrl Pts',(129.019818810385,4.83115679587456,335.931516582256));
#54039=CARTESIAN_POINT('Ctrl Pts',(129.012043731606,4.85519347106497,335.796870861606));
#54040=CARTESIAN_POINT('Ctrl Pts',(129.004268652828,4.87359145644578,335.661278593453));
#54041=CARTESIAN_POINT('Ctrl Pts',(128.996503141779,4.89196680193436,335.525853180217));
#54042=CARTESIAN_POINT('Ctrl Pts',(128.98873763073,4.90471721171743,335.389483920691));
#54043=CARTESIAN_POINT('Ctrl Pts',(128.980972119681,4.91175500785868,335.252677274948));
#54044=CARTESIAN_POINT('Ctrl Pts',(128.973214308159,4.91878582600455,335.116006273393));
#54045=CARTESIAN_POINT('Ctrl Pts',(128.965456496636,4.92011528238229,334.978899136492));
#54046=CARTESIAN_POINT('Ctrl Pts',(128.957698685114,4.91570725124464,334.84186941295));
#54047=CARTESIAN_POINT('Ctrl Pts',(128.949946711591,4.91130253729023,334.704942808621));
#54048=CARTESIAN_POINT('Ctrl Pts',(128.942194738068,4.90116894239111,334.568093890794));
#54049=CARTESIAN_POINT('Ctrl Pts',(128.934442764545,4.88532238597772,334.431837833392));
#54050=CARTESIAN_POINT('Ctrl Pts',(128.926694073988,4.86948254059035,334.295639480511));
#54051=CARTESIAN_POINT('Ctrl Pts',(128.91894538343,4.84793459084983,334.16003387613));
#54052=CARTESIAN_POINT('Ctrl Pts',(128.911196692872,4.82074642564162,334.025532472494));
#54053=CARTESIAN_POINT('Ctrl Pts',(128.903449614495,4.79356391715833,333.891059052999));
#54054=CARTESIAN_POINT('Ctrl Pts',(128.895702536117,4.76074360476628,333.757689760168));
#54055=CARTESIAN_POINT('Ctrl Pts',(128.887955457739,4.72240468553071,333.625926840166));
#54056=CARTESIAN_POINT('Ctrl Pts',(128.880208314433,4.6840654449781,333.494162815863));
#54057=CARTESIAN_POINT('Ctrl Pts',(128.872461171127,4.64020761453386,333.364005566553));
#54058=CARTESIAN_POINT('Ctrl Pts',(128.864714027822,4.59100044555316,333.235942752791));
#54059=CARTESIAN_POINT('Ctrl Pts',(128.856965142794,4.5417822137561,333.107851147789));
#54060=CARTESIAN_POINT('Ctrl Pts',(128.849216257766,4.48721239046338,332.981855280117));
#54061=CARTESIAN_POINT('Ctrl Pts',(128.841467372737,4.42750844975837,332.858423013334));
#54062=CARTESIAN_POINT('Ctrl Pts',(128.833710262963,4.36774113867383,332.734859734267));
#54063=CARTESIAN_POINT('Ctrl Pts',(128.825953153188,4.30282899494784,332.613865844036));
#54064=CARTESIAN_POINT('Ctrl Pts',(128.818196043413,4.23303583177944,332.495885244368));
#54065=CARTESIAN_POINT('Ctrl Pts',(128.810434788487,4.16320537337622,332.377841599641));
#54066=CARTESIAN_POINT('Ctrl Pts',(128.802673533561,4.08848891114797,332.262814781585));
#54067=CARTESIAN_POINT('Ctrl Pts',(128.794912278635,4.00919316814962,332.151218997016));
#54068=CARTESIAN_POINT('Ctrl Pts',(128.78713860823,3.92977057780487,332.039444695561));
#54069=CARTESIAN_POINT('Ctrl Pts',(128.779364937826,3.84575430812722,331.931112704347));
#54070=CARTESIAN_POINT('Ctrl Pts',(128.771591267421,3.75749143949776,331.826604162005));
#54071=CARTESIAN_POINT('Ctrl Pts',(128.764179463244,3.67333722863829,331.726960517454));
#54072=CARTESIAN_POINT('Ctrl Pts',(128.756767659067,3.58532307419928,331.630792581717));
#54073=CARTESIAN_POINT('Ctrl Pts',(128.74935585489,3.49377911859015,331.53839769283));
#54074=CARTESIAN_POINT('Ctrl Pts',(128.741580776111,3.3977483210208,331.441474255209));
#54075=CARTESIAN_POINT('Ctrl Pts',(128.733805697333,3.29752948615606,331.348396776828));
#54076=CARTESIAN_POINT('Ctrl Pts',(128.726030618555,3.1934632606972,331.259548761837));
#54077=CARTESIAN_POINT('Ctrl Pts',(128.718265107506,3.08952509535413,331.170810079984));
#54078=CARTESIAN_POINT('Ctrl Pts',(128.710499596457,2.98174925406078,331.086290757184));
#54079=CARTESIAN_POINT('Ctrl Pts',(128.702734085408,2.87051418233513,331.006338598289));
#54080=CARTESIAN_POINT('Ctrl Pts',(128.694976273886,2.75938940050737,330.926465712193));
#54081=CARTESIAN_POINT('Ctrl Pts',(128.687218462363,2.64481252916569,330.85115120498));
#54082=CARTESIAN_POINT('Ctrl Pts',(128.679460650841,2.52719587265771,330.780703366233));
#54083=CARTESIAN_POINT('Ctrl Pts',(128.671708677318,2.40966772641242,330.710308541717));
#54084=CARTESIAN_POINT('Ctrl Pts',(128.663956703795,2.28910468220214,330.644773296033));
#54085=CARTESIAN_POINT('Ctrl Pts',(128.656204730272,2.16594857568623,330.584363032361));
#54086=CARTESIAN_POINT('Ctrl Pts',(128.648456039714,2.04284462585513,330.523978352471));
#54087=CARTESIAN_POINT('Ctrl Pts',(128.640707349157,1.91715014808726,330.468714509535));
#54088=CARTESIAN_POINT('Ctrl Pts',(128.632958658599,1.78933197205771,330.418791190497));
#54089=CARTESIAN_POINT('Ctrl Pts',(128.625211580221,1.66154038966724,330.368878258421));
#54090=CARTESIAN_POINT('Ctrl Pts',(128.617464501844,1.53162635175188,330.324303782223));
#54091=CARTESIAN_POINT('Ctrl Pts',(128.609717423466,1.40007671219846,330.285239320765));
#54092=CARTESIAN_POINT('Ctrl Pts',(128.60197028016,1.26852597013235,330.246174531909));
#54093=CARTESIAN_POINT('Ctrl Pts',(128.594223136854,1.13533997378885,330.212619961172));
#54094=CARTESIAN_POINT('Ctrl Pts',(128.586475993548,1.00102039895376,330.184697182588));
#54095=CARTESIAN_POINT('Ctrl Pts',(128.57872710852,0.866670626226927,330.15676812637));
#54096=CARTESIAN_POINT('Ctrl Pts',(128.570978223492,0.731187150498339,330.134473461334));
#54097=CARTESIAN_POINT('Ctrl Pts',(128.563229338464,0.595081095921843,330.117883496702));
#54098=CARTESIAN_POINT('Ctrl Pts',(128.555472228689,0.458830576972364,330.10127592331));
#54099=CARTESIAN_POINT('Ctrl Pts',(128.547715118915,0.321956547757211,330.090385193177));
#54100=CARTESIAN_POINT('Ctrl Pts',(128.53995800914,0.184975059170039,330.085229680851));
#54101=CARTESIAN_POINT('Ctrl Pts',(128.532196754214,0.0479203720552305,
330.080071413585));
#54102=CARTESIAN_POINT('Ctrl Pts',(128.524435499288,-0.0892414981793248,
330.080654469191));
#54103=CARTESIAN_POINT('Ctrl Pts',(128.516674244361,-0.22599625073994,330.086945068783));
#54104=CARTESIAN_POINT('Ctrl Pts',(128.508900573957,-0.362969766336476,
330.093245731285));
#54105=CARTESIAN_POINT('Ctrl Pts',(128.501126903552,-0.499534473285334,
330.105272148331));
#54106=CARTESIAN_POINT('Ctrl Pts',(128.493353233147,-0.635182038869866,
330.122938708608));
#54107=CARTESIAN_POINT('Ctrl Pts',(128.48594142897,-0.764515177642398,330.139782886253));
#54108=CARTESIAN_POINT('Ctrl Pts',(128.478529624793,-0.893014355676524,
330.161753878278));
#54109=CARTESIAN_POINT('Ctrl Pts',(128.471117820616,-1.02025087607247,330.188734967561));
#54110=CARTESIAN_POINT('Ctrl Pts',(128.463342741838,-1.15372363734993,330.217038480401));
#54111=CARTESIAN_POINT('Ctrl Pts',(128.455567663059,-1.28622863674198,330.250945072378));
#54112=CARTESIAN_POINT('Ctrl Pts',(128.447792584281,-1.41725903395184,330.290375822512));
#54113=CARTESIAN_POINT('Ctrl Pts',(128.440027073232,-1.54812818991649,330.329758050598));
#54114=CARTESIAN_POINT('Ctrl Pts',(128.432261562183,-1.67752598350064,330.374650799553));
#54115=CARTESIAN_POINT('Ctrl Pts',(128.424496051134,-1.80495513959806,330.424924043632));
#54116=CARTESIAN_POINT('Ctrl Pts',(128.416738239611,-1.93225794931522,330.475147441642));
#54117=CARTESIAN_POINT('Ctrl Pts',(128.408980428089,-2.05759564469798,330.530740575745));
#54118=CARTESIAN_POINT('Ctrl Pts',(128.401222616567,-2.18048585691809,330.591523563602));
#54119=CARTESIAN_POINT('Ctrl Pts',(128.393470643044,-2.30328359035696,330.652260810333));
#54120=CARTESIAN_POINT('Ctrl Pts',(128.385718669521,-2.42363715771364,330.718179964457));
#54121=CARTESIAN_POINT('Ctrl Pts',(128.377966695998,-2.54108427316294,330.789053101833));
#54122=CARTESIAN_POINT('Ctrl Pts',(128.370218005441,-2.65848164968912,330.859896224393));
#54123=CARTESIAN_POINT('Ctrl Pts',(128.362469314883,-2.77297468848427,330.935688955871));
#54124=CARTESIAN_POINT('Ctrl Pts',(128.354720624325,-2.88412602178613,331.016157614444));
#54125=CARTESIAN_POINT('Ctrl Pts',(128.346973545947,-2.99525422912493,331.09660953084));
#54126=CARTESIAN_POINT('Ctrl Pts',(128.33922646757,-3.10304179749696,331.181735210164));
#54127=CARTESIAN_POINT('Ctrl Pts',(128.331479389192,-3.20708099481977,331.27121808694));
#54128=CARTESIAN_POINT('Ctrl Pts',(128.323732245886,-3.31112106409162,331.360701713668));
#54129=CARTESIAN_POINT('Ctrl Pts',(128.31598510258,-3.41141240331253,331.454542355806));
#54130=CARTESIAN_POINT('Ctrl Pts',(128.308237959274,-3.50758129272998,331.552383934167));
#54131=CARTESIAN_POINT('Ctrl Pts',(128.300489074246,-3.60377180295506,331.650247509391));
#54132=CARTESIAN_POINT('Ctrl Pts',(128.292740189218,-3.69583774517671,331.752113532026));
#54133=CARTESIAN_POINT('Ctrl Pts',(128.28499130419,-3.78344339626242,331.857590235221));
#54134=CARTESIAN_POINT('Ctrl Pts',(128.277234194415,-3.87114203289136,331.963178892478));
#54135=CARTESIAN_POINT('Ctrl Pts',(128.26947708464,-3.95437067124238,332.072385584739));
#54136=CARTESIAN_POINT('Ctrl Pts',(128.261719974866,-4.03283459501543,332.184786297322));
#54137=CARTESIAN_POINT('Ctrl Pts',(128.25395871994,-4.11134044740058,332.297247073251));
#54138=CARTESIAN_POINT('Ctrl Pts',(128.246197465013,-4.18507630183322,332.412904940996));
#54139=CARTESIAN_POINT('Ctrl Pts',(128.238436210087,-4.25379224602821,332.531309134353));
#54140=CARTESIAN_POINT('Ctrl Pts',(128.230662539683,-4.32261811333938,332.649902735831));
#54141=CARTESIAN_POINT('Ctrl Pts',(128.222888869278,-4.38640784168429,332.771251095724));
#54142=CARTESIAN_POINT('Ctrl Pts',(128.215115198873,-4.44495833544178,332.89488041701));
#54143=CARTESIAN_POINT('Ctrl Pts',(128.207703394696,-4.50078328962875,333.012754763648));
#54144=CARTESIAN_POINT('Ctrl Pts',(128.200291590519,-4.55184569221968,333.132702228346));
#54145=CARTESIAN_POINT('Ctrl Pts',(128.192879786342,-4.59801170064182,333.254299148405));
#54146=CARTESIAN_POINT('Ctrl Pts',(128.183991545777,-4.6533740090564,333.400118256892));
#54147=CARTESIAN_POINT('Ctrl Pts',(128.175103305213,-4.70184091569508,333.548691672308));
#54148=CARTESIAN_POINT('Ctrl Pts',(128.166215064648,-4.74316593011621,333.699400129984));
#54149=CARTESIAN_POINT('Ctrl Pts',(128.15735782075,-4.78434682853533,333.849583010097));
#54150=CARTESIAN_POINT('Ctrl Pts',(128.148500576852,-4.81843545617234,334.001885917024));
#54151=CARTESIAN_POINT('Ctrl Pts',(128.139643332954,-4.84523439894587,334.155673829748));
#54152=CARTESIAN_POINT('Ctrl Pts',(128.130845505093,-4.87185356943344,334.308430104589));
#54153=CARTESIAN_POINT('Ctrl Pts',(128.122047677233,-4.89128044364123,334.462651363844));
#54154=CARTESIAN_POINT('Ctrl Pts',(128.113249849372,-4.90336889032551,334.617695686804));
#54155=CARTESIAN_POINT('Ctrl Pts',(128.106105691769,-4.91318515061795,334.743597340738));
#54156=CARTESIAN_POINT('Ctrl Pts',(128.098961534166,-4.91816327654134,334.870041323959));
#54157=CARTESIAN_POINT('Ctrl Pts',(128.091817376563,-4.91824887636649,334.996675451945));
#54158=CARTESIAN_POINT('',(126.341816235661,-4.91546218483043,335.003626104507));
#54159=CARTESIAN_POINT('Ctrl Pts',(128.091817376508,-4.91824887636714,334.996675452912));
#54160=CARTESIAN_POINT('Ctrl Pts',(128.084031730335,-4.9183421623491,335.134680319095));
#54161=CARTESIAN_POINT('Ctrl Pts',(128.076246084161,-4.91262254950206,335.272721930806));
#54162=CARTESIAN_POINT('Ctrl Pts',(128.068460437988,-4.90110745943531,335.41027884855));
#54163=CARTESIAN_POINT('Ctrl Pts',(128.060674700231,-4.88959223391519,335.547837384393));
#54164=CARTESIAN_POINT('Ctrl Pts',(128.052888962474,-4.87228142675415,335.684910830953));
#54165=CARTESIAN_POINT('Ctrl Pts',(128.045103224717,-4.84924442610522,335.820982069468));
#54166=CARTESIAN_POINT('Ctrl Pts',(128.03731577343,-4.82620235534134,335.95708325532));
#54167=CARTESIAN_POINT('Ctrl Pts',(128.029528322144,-4.79743164625134,336.092181414168));
#54168=CARTESIAN_POINT('Ctrl Pts',(128.021740870857,-4.76305291408951,336.225769146325));
#54169=CARTESIAN_POINT('Ctrl Pts',(128.013950083339,-4.72865945369409,336.359414108962));
#54170=CARTESIAN_POINT('Ctrl Pts',(128.006159295821,-4.68865328308514,336.491546983912));
#54171=CARTESIAN_POINT('Ctrl Pts',(127.998368508303,-4.64320493090818,336.621675378148));
#54172=CARTESIAN_POINT('Ctrl Pts',(127.990567897971,-4.5976992763457,336.751967841421));
#54173=CARTESIAN_POINT('Ctrl Pts',(127.982767287639,-4.54673786409452,336.880250412829));
#54174=CARTESIAN_POINT('Ctrl Pts',(127.974966677307,-4.49053968726436,337.006049944444));
#54175=CARTESIAN_POINT('Ctrl Pts',(127.967160619224,-4.43430226303195,337.131937331308));
#54176=CARTESIAN_POINT('Ctrl Pts',(127.959354561141,-4.37282095856092,337.255337879206));
#54177=CARTESIAN_POINT('Ctrl Pts',(127.951548503058,-4.30636039055699,337.375803705937));
#54178=CARTESIAN_POINT('Ctrl Pts',(127.943729882914,-4.23979286951245,337.496463394785));
#54179=CARTESIAN_POINT('Ctrl Pts',(127.935911262771,-4.16823027956881,337.614178600881));
#54180=CARTESIAN_POINT('Ctrl Pts',(127.928092642628,-4.09198055196934,337.728530414858));
#54181=CARTESIAN_POINT('Ctrl Pts',(127.923609012441,-4.04825473153978,337.794106083666));
#54182=CARTESIAN_POINT('Ctrl Pts',(127.919125382254,-4.00298829587374,337.85857629584));
#54183=CARTESIAN_POINT('Ctrl Pts',(127.914641752068,-3.95624505407418,337.921867234255));
#54184=CARTESIAN_POINT('Ctrl Pts',(127.906866673289,-3.87518743508755,338.031620271782));
#54185=CARTESIAN_POINT('Ctrl Pts',(127.899091594511,-3.78943116206288,338.138171167979));
#54186=CARTESIAN_POINT('Ctrl Pts',(127.891316515732,-3.69925804687033,338.241091323176));
#54187=CARTESIAN_POINT('Ctrl Pts',(127.883551004683,-3.60919589543658,338.343884828569));
#54188=CARTESIAN_POINT('Ctrl Pts',(127.875785493634,-3.51472797145635,338.443056191533));
#54189=CARTESIAN_POINT('Ctrl Pts',(127.868019982585,-3.41617863654083,338.538206690647));
#54190=CARTESIAN_POINT('Ctrl Pts',(127.860262171063,-3.31772701357783,338.633262847764));
#54191=CARTESIAN_POINT('Ctrl Pts',(127.852504359541,-3.21520231228766,338.724305805037));
#54192=CARTESIAN_POINT('Ctrl Pts',(127.844746548019,-3.10896809520671,338.810971063323));
#54193=CARTESIAN_POINT('Ctrl Pts',(127.836994574496,-3.00281382274318,338.897571103254));
#54194=CARTESIAN_POINT('Ctrl Pts',(127.829242600973,-2.89295589254402,338.979799755368));
#54195=CARTESIAN_POINT('Ctrl Pts',(127.82149062745,-2.77979327165223,339.057330702491));
#54196=CARTESIAN_POINT('Ctrl Pts',(127.813741936892,-2.66667857519761,339.134828815212));
#54197=CARTESIAN_POINT('Ctrl Pts',(127.805993246334,-2.55026229341606,339.207632959419));
#54198=CARTESIAN_POINT('Ctrl Pts',(127.798244555777,-2.43097471582919,339.275458454189));
#54199=CARTESIAN_POINT('Ctrl Pts',(127.790497477399,-2.31171195701911,339.343269837299));
#54200=CARTESIAN_POINT('Ctrl Pts',(127.782750399021,-2.18957943024431,339.406104438273));
#54201=CARTESIAN_POINT('Ctrl Pts',(127.775003320643,-2.06503417723717,339.463722315438));
#54202=CARTESIAN_POINT('Ctrl Pts',(127.767256177337,-1.94048788042103,339.521340675497));
#54203=CARTESIAN_POINT('Ctrl Pts',(127.759509034032,-1.81352917179135,339.573742060426));
#54204=CARTESIAN_POINT('Ctrl Pts',(127.751761890726,-1.6846369649321,339.620733855015));
#54205=CARTESIAN_POINT('Ctrl Pts',(127.744013005698,-1.55571578036802,339.667736214358));
#54206=CARTESIAN_POINT('Ctrl Pts',(127.73626412067,-1.42486059974457,339.709326429418));
#54207=CARTESIAN_POINT('Ctrl Pts',(127.728515235641,-1.29256707557367,339.745361252596));
#54208=CARTESIAN_POINT('Ctrl Pts',(127.720758125867,-1.16013313368955,339.781434323508));
#54209=CARTESIAN_POINT('Ctrl Pts',(127.713001016092,-1.02625817631579,339.811940120738));
#54210=CARTESIAN_POINT('Ctrl Pts',(127.705243906317,-0.891450217033445,
339.836786078901));
#54211=CARTESIAN_POINT('Ctrl Pts',(127.697482651391,-0.756570220688029,
339.86164531395));
#54212=CARTESIAN_POINT('Ctrl Pts',(127.689721396465,-0.620756615827872,
339.880838628801));
#54213=CARTESIAN_POINT('Ctrl Pts',(127.681960141539,-0.484523201517907,
339.894325319152));
#54214=CARTESIAN_POINT('Ctrl Pts',(127.674186471134,-0.348071858143504,
339.907833583812));
#54215=CARTESIAN_POINT('Ctrl Pts',(127.66641280073,-0.211199753796001,339.915616959843));
#54216=CARTESIAN_POINT('Ctrl Pts',(127.658639130325,-0.0744222528240178,
339.917686894342));
#54217=CARTESIAN_POINT('Ctrl Pts',(127.651227326148,0.055988222569004,339.919660472892));
#54218=CARTESIAN_POINT('Ctrl Pts',(127.643815521971,0.186312416243332,339.916440567866));
#54219=CARTESIAN_POINT('Ctrl Pts',(127.636403717794,0.316109284535064,339.90808088592));
#54220=CARTESIAN_POINT('Ctrl Pts',(127.628628639016,0.452267883988871,339.899311471059));
#54221=CARTESIAN_POINT('Ctrl Pts',(127.620853560237,0.588276445791939,339.884857995364));
#54222=CARTESIAN_POINT('Ctrl Pts',(127.613078481459,0.723622046764772,339.864725500574));
#54223=CARTESIAN_POINT('Ctrl Pts',(127.60531297041,0.858801096358901,339.8446177801));
#54224=CARTESIAN_POINT('Ctrl Pts',(127.597547459361,0.9933184254372,339.818845002392));
#54225=CARTESIAN_POINT('Ctrl Pts',(127.589781948312,1.12666320997102,339.787464159009));
#54226=CARTESIAN_POINT('Ctrl Pts',(127.582024136789,1.25987578276284,339.756114429824));
#54227=CARTESIAN_POINT('Ctrl Pts',(127.574266325267,1.39191774658354,339.719167789464));
#54228=CARTESIAN_POINT('Ctrl Pts',(127.566508513745,1.52228584177884,339.676732714024));
#54229=CARTESIAN_POINT('Ctrl Pts',(127.558756540222,1.65255583084842,339.634329572323));
#54230=CARTESIAN_POINT('Ctrl Pts',(127.551004566699,1.78115408835958,339.58644633704));
#54231=CARTESIAN_POINT('Ctrl Pts',(127.543252593176,1.90759030328039,339.533241919127));
#54232=CARTESIAN_POINT('Ctrl Pts',(127.535503902618,2.03397297238907,339.480060033317));
#54233=CARTESIAN_POINT('Ctrl Pts',(127.527755212061,2.15819506049739,339.421561598265));
#54234=CARTESIAN_POINT('Ctrl Pts',(127.520006521503,2.27978431899547,339.35795439643));
#54235=CARTESIAN_POINT('Ctrl Pts',(127.512259443125,2.4013482798327,339.294360428604));
#54236=CARTESIAN_POINT('Ctrl Pts',(127.504512364748,2.52028015450945,339.225659989292));
#54237=CARTESIAN_POINT('Ctrl Pts',(127.49676528637,2.63613083944876,339.152107568429));
#54238=CARTESIAN_POINT('Ctrl Pts',(127.489018143064,2.75198249532831,339.078554531127));
#54239=CARTESIAN_POINT('Ctrl Pts',(127.481270999758,2.86475257997815,339.000149640671));
#54240=CARTESIAN_POINT('Ctrl Pts',(127.473523856452,2.97401995153915,338.917191390569));
#54241=CARTESIAN_POINT('Ctrl Pts',(127.465774971424,3.08331188872535,338.834214489691));
#54242=CARTESIAN_POINT('Ctrl Pts',(127.458026086396,3.18909923456191,338.746682428447));
#54243=CARTESIAN_POINT('Ctrl Pts',(127.450277201368,3.29099330307165,338.654934492113));
#54244=CARTESIAN_POINT('Ctrl Pts',(127.442520091593,3.39299552299822,338.563089173571));
#54245=CARTESIAN_POINT('Ctrl Pts',(127.434762981818,3.49109591987966,338.467019303122));
#54246=CARTESIAN_POINT('Ctrl Pts',(127.427005872044,3.58494173821103,338.367101987783));
#54247=CARTESIAN_POINT('Ctrl Pts',(127.419244617118,3.6788377047472,338.267131279825));
#54248=CARTESIAN_POINT('Ctrl Pts',(127.411483362191,3.76847430725011,338.16330932602));
#54249=CARTESIAN_POINT('Ctrl Pts',(127.403722107265,3.8535392704469,338.05604616353));
#54250=CARTESIAN_POINT('Ctrl Pts',(127.395948436861,3.93874030986212,337.948611414936));
#54251=CARTESIAN_POINT('Ctrl Pts',(127.388174766456,4.01935486620013,337.837724773732));
#54252=CARTESIAN_POINT('Ctrl Pts',(127.380401096051,4.09511367234788,337.723825815475));
#54253=CARTESIAN_POINT('Ctrl Pts',(127.372989291874,4.16734588784317,337.615228881127));
#54254=CARTESIAN_POINT('Ctrl Pts',(127.365577487697,4.23516410021169,337.503894010952));
#54255=CARTESIAN_POINT('Ctrl Pts',(127.35816568352,4.29837479849395,337.390221151729));
#54256=CARTESIAN_POINT('Ctrl Pts',(127.350390604741,4.36468364139377,337.270976847062));
#54257=CARTESIAN_POINT('Ctrl Pts',(127.342615525963,4.42613144229161,337.148782740788));
#54258=CARTESIAN_POINT('Ctrl Pts',(127.334840447185,4.48244486872974,337.024072889324));
#54259=CARTESIAN_POINT('Ctrl Pts',(127.327074936136,4.53868899791155,336.899516501273));
#54260=CARTESIAN_POINT('Ctrl Pts',(127.319309425087,4.58981116466563,336.77245088059));
#54261=CARTESIAN_POINT('Ctrl Pts',(127.311543914038,4.63558285821723,336.643336431502));
#54262=CARTESIAN_POINT('Ctrl Pts',(127.303786102515,4.68130916900118,336.514349999767));
#54263=CARTESIAN_POINT('Ctrl Pts',(127.296028290993,4.72169543409043,336.383319148303));
#54264=CARTESIAN_POINT('Ctrl Pts',(127.288270479471,4.75656053066944,336.250725781528));
#54265=CARTESIAN_POINT('Ctrl Pts',(127.280518505948,4.79139939015789,336.118232195464));
#54266=CARTESIAN_POINT('Ctrl Pts',(127.272766532425,4.82072525217029,335.984178811048));
#54267=CARTESIAN_POINT('Ctrl Pts',(127.265014558902,4.84440641288281,335.849063937121));
#54268=CARTESIAN_POINT('Ctrl Pts',(127.257265868344,4.86807754460964,335.714006284424));
#54269=CARTESIAN_POINT('Ctrl Pts',(127.249517177787,4.88610866230272,335.577888420526));
#54270=CARTESIAN_POINT('Ctrl Pts',(127.241768487229,4.89841893384281,335.441219912368));
#54271=CARTESIAN_POINT('Ctrl Pts',(127.234021408851,4.9107266441281,335.304579839235));
#54272=CARTESIAN_POINT('Ctrl Pts',(127.226274330473,4.91731584074766,335.167389738777));
#54273=CARTESIAN_POINT('Ctrl Pts',(127.218527252096,4.91815749400375,335.03016499088));
#54274=CARTESIAN_POINT('Ctrl Pts',(127.21078010879,4.9189991543137,334.892939092907));
#54275=CARTESIAN_POINT('Ctrl Pts',(127.203032965484,4.91409317278428,334.755678937783));
#54276=CARTESIAN_POINT('Ctrl Pts',(127.195285822178,4.90346265494926,334.618900204647));
#54277=CARTESIAN_POINT('Ctrl Pts',(127.18753693715,4.89282974714812,334.482090720748));
#54278=CARTESIAN_POINT('Ctrl Pts',(127.179788052122,4.87646977234223,334.345763263832));
#54279=CARTESIAN_POINT('Ctrl Pts',(127.172039167094,4.8544577024734,334.210428294962));
#54280=CARTESIAN_POINT('Ctrl Pts',(127.164282057319,4.83242226876619,334.074949680158));
#54281=CARTESIAN_POINT('Ctrl Pts',(127.156524947544,4.80472281889676,333.940466044152));
#54282=CARTESIAN_POINT('Ctrl Pts',(127.14876783777,4.77148557395651,333.80747810082));
#54283=CARTESIAN_POINT('Ctrl Pts',(127.141006582843,4.73823056809527,333.674419092983));
#54284=CARTESIAN_POINT('Ctrl Pts',(127.133245327917,4.69943198115799,333.542857745119));
#54285=CARTESIAN_POINT('Ctrl Pts',(127.125484072991,4.65526563207258,333.413278550802));
#54286=CARTESIAN_POINT('Ctrl Pts',(127.117710402586,4.61102863122245,333.283492072005));
#54287=CARTESIAN_POINT('Ctrl Pts',(127.109936732182,4.56140685106839,333.155694447515));
#54288=CARTESIAN_POINT('Ctrl Pts',(127.102163061777,4.50662422418817,333.030349989348));
#54289=CARTESIAN_POINT('Ctrl Pts',(127.0947512576,4.45439174176941,332.910840345866));
#54290=CARTESIAN_POINT('Ctrl Pts',(127.087339453423,4.39746820033474,332.793560877603));
#54291=CARTESIAN_POINT('Ctrl Pts',(127.079927649246,4.3360852037804,332.678890746204));
#54292=CARTESIAN_POINT('Ctrl Pts',(127.072152570468,4.27169364371413,332.558600290081));
#54293=CARTESIAN_POINT('Ctrl Pts',(127.064377491689,4.20219094379099,332.440801280973));
#54294=CARTESIAN_POINT('Ctrl Pts',(127.056602412911,4.12779419543709,332.32595846281));
#54295=CARTESIAN_POINT('Ctrl Pts',(127.048836901862,4.05348899701846,332.211256966047));
#54296=CARTESIAN_POINT('Ctrl Pts',(127.041071390813,3.97430194358009,332.099504747005));
#54297=CARTESIAN_POINT('Ctrl Pts',(127.033305879764,3.89049653856631,331.991143116414));
#54298=CARTESIAN_POINT('Ctrl Pts',(127.025548068241,3.80677422685534,331.882888926695));
#54299=CARTESIAN_POINT('Ctrl Pts',(127.017790256719,3.7184429138411,331.778018942502));
#54300=CARTESIAN_POINT('Ctrl Pts',(127.010032445197,3.62580982728122,331.676946260006));
#54301=CARTESIAN_POINT('Ctrl Pts',(127.002280471674,3.53324645005668,331.575949637908));
#54302=CARTESIAN_POINT('Ctrl Pts',(126.994528498151,3.43638800585055,331.478744916613));
#54303=CARTESIAN_POINT('Ctrl Pts',(126.986776524628,3.33558226070226,331.385712512183));
#54304=CARTESIAN_POINT('Ctrl Pts',(126.97902783407,3.234819206847,331.292719507032));
#54305=CARTESIAN_POINT('Ctrl Pts',(126.971279143513,3.13011246355691,331.20389556889));
#54306=CARTESIAN_POINT('Ctrl Pts',(126.963530452955,3.02184679364613,331.119584427122));
#54307=CARTESIAN_POINT('Ctrl Pts',(126.955783374577,2.91360364931215,331.035290826992));
#54308=CARTESIAN_POINT('Ctrl Pts',(126.948036296199,2.80180335939311,330.955508395656));
#54309=CARTESIAN_POINT('Ctrl Pts',(126.940289217822,2.68686360819564,330.880540446435));
#54310=CARTESIAN_POINT('Ctrl Pts',(126.932542074516,2.57192289369231,330.805571868911));
#54311=CARTESIAN_POINT('Ctrl Pts',(126.92479493121,2.45384299282088,330.73541806752));
#54312=CARTESIAN_POINT('Ctrl Pts',(126.917047787904,2.33307005490071,330.670338675898));
#54313=CARTESIAN_POINT('Ctrl Pts',(126.909298902876,2.21226996466015,330.605244653047));
#54314=CARTESIAN_POINT('Ctrl Pts',(126.901550017848,2.08877597661861,330.545227495481));
#54315=CARTESIAN_POINT('Ctrl Pts',(126.89380113282,1.96305791999246,330.490500397466));
#54316=CARTESIAN_POINT('Ctrl Pts',(126.886044023045,1.83720642492219,330.435715211544));
#54317=CARTESIAN_POINT('Ctrl Pts',(126.87828691327,1.70912650460396,330.386231457769));
#54318=CARTESIAN_POINT('Ctrl Pts',(126.870529803496,1.57930752549295,330.342213959141));
#54319=CARTESIAN_POINT('Ctrl Pts',(126.86276854857,1.44941917527031,330.298172938969));
#54320=CARTESIAN_POINT('Ctrl Pts',(126.855007293643,1.3177902894592,330.259604104139));
#54321=CARTESIAN_POINT('Ctrl Pts',(126.847246038717,1.18492343475327,330.226621792035));
#54322=CARTESIAN_POINT('Ctrl Pts',(126.839472368313,1.05184403638106,330.193586718981));
#54323=CARTESIAN_POINT('Ctrl Pts',(126.831698697908,0.917523094966202,330.166156104909));
#54324=CARTESIAN_POINT('Ctrl Pts',(126.823925027503,0.782472243155901,330.144392906012));
#54325=CARTESIAN_POINT('Ctrl Pts',(126.816513223326,0.653708040988915,330.123642789258));
#54326=CARTESIAN_POINT('Ctrl Pts',(126.809101419149,0.524280639535785,330.108044359889));
#54327=CARTESIAN_POINT('Ctrl Pts',(126.801689614972,0.394634218071375,330.09760804337));
#54328=CARTESIAN_POINT('Ctrl Pts',(126.793914536194,0.258633439293941,330.08666021189));
#54329=CARTESIAN_POINT('Ctrl Pts',(126.786139457415,0.121961840411086,330.081358711897));
#54330=CARTESIAN_POINT('Ctrl Pts',(126.778364378637,-0.0148722848646814,
330.081772486185));
#54331=CARTESIAN_POINT('Ctrl Pts',(126.770598867588,-0.151538027038381,
330.082185751298));
#54332=CARTESIAN_POINT('Ctrl Pts',(126.762833356539,-0.288365510528269,
330.088300295852));
#54333=CARTESIAN_POINT('Ctrl Pts',(126.75506784549,-0.424841030892516,330.100133352736));
#54334=CARTESIAN_POINT('Ctrl Pts',(126.747310033968,-0.561181235380335,
330.11195467711));
#54335=CARTESIAN_POINT('Ctrl Pts',(126.739552222445,-0.697169784312663,
330.129483196804));
#54336=CARTESIAN_POINT('Ctrl Pts',(126.731794410923,-0.832293037737173,
330.152684107484));
#54337=CARTESIAN_POINT('Ctrl Pts',(126.7240424374,-0.967314606629349,330.175867558744));
#54338=CARTESIAN_POINT('Ctrl Pts',(126.716290463877,-1.10147179243474,330.204714838563));
#54339=CARTESIAN_POINT('Ctrl Pts',(126.708538490354,-1.23425649901202,330.239139368019));
#54340=CARTESIAN_POINT('Ctrl Pts',(126.700789799796,-1.36698497118668,330.273549318666));
#54341=CARTESIAN_POINT('Ctrl Pts',(126.693041109239,-1.49834174261167,330.313531723274));
#54342=CARTESIAN_POINT('Ctrl Pts',(126.685292418681,-1.62782954669492,330.358949038267));
#54343=CARTESIAN_POINT('Ctrl Pts',(126.677545340303,-1.75729040975898,330.404356903807));
#54344=CARTESIAN_POINT('Ctrl Pts',(126.669798261926,-1.8848827103274,330.455197301244));
#54345=CARTESIAN_POINT('Ctrl Pts',(126.662051183548,-2.01012535281237,330.511283131174));
#54346=CARTESIAN_POINT('Ctrl Pts',(126.654304040242,-2.13536904495128,330.567369431158));
#54347=CARTESIAN_POINT('Ctrl Pts',(126.646556896936,-2.25826268299133,330.628701091568));
#54348=CARTESIAN_POINT('Ctrl Pts',(126.63880975363,-2.37834649847276,330.695043438581));
#54349=CARTESIAN_POINT('Ctrl Pts',(126.631060868602,-2.49845731134499,330.761400700762));
#54350=CARTESIAN_POINT('Ctrl Pts',(126.623311983574,-2.61575670256436,330.832770702192));
#54351=CARTESIAN_POINT('Ctrl Pts',(126.615563098546,-2.72981114097713,330.90887372511));
#54352=CARTESIAN_POINT('Ctrl Pts',(126.607805988771,-2.84398663794966,330.985057524563));
#54353=CARTESIAN_POINT('Ctrl Pts',(126.600048878997,-2.95490997629735,331.065984163479));
#54354=CARTESIAN_POINT('Ctrl Pts',(126.592291769222,-3.06217772857411,331.151331318349));
#54355=CARTESIAN_POINT('Ctrl Pts',(126.584530514296,-3.16950280130805,331.236724080009));
#54356=CARTESIAN_POINT('Ctrl Pts',(126.576769259369,-3.27316810032359,331.326541808661));
#54357=CARTESIAN_POINT('Ctrl Pts',(126.569008004443,-3.37280550919827,331.42042375977));
#54358=CARTESIAN_POINT('Ctrl Pts',(126.561234334039,-3.47260230545519,331.514455891404));
#54359=CARTESIAN_POINT('Ctrl Pts',(126.553460663634,-3.5683580627684,331.612564957409));
#54360=CARTESIAN_POINT('Ctrl Pts',(126.545686993229,-3.65974296614989,331.714354784184));
#54361=CARTESIAN_POINT('Ctrl Pts',(126.538275189052,-3.74687388029247,331.811406270033));
#54362=CARTESIAN_POINT('Ctrl Pts',(126.530863384875,-3.83003152579536,331.911803327957));
#54363=CARTESIAN_POINT('Ctrl Pts',(126.523451580698,-3.90896676476953,332.015178079947));
#54364=CARTESIAN_POINT('Ctrl Pts',(126.515660696377,-3.99193918295398,332.123839981315));
#54365=CARTESIAN_POINT('Ctrl Pts',(126.507869812057,-4.07051127335644,332.236139666177));
#54366=CARTESIAN_POINT('Ctrl Pts',(126.500078927736,-4.1443478090152,332.351686517723));
#54367=CARTESIAN_POINT('Ctrl Pts',(126.492297552703,-4.21809422231923,332.467092336726));
#54368=CARTESIAN_POINT('Ctrl Pts',(126.484516177669,-4.28711637205158,332.585737114575));
#54369=CARTESIAN_POINT('Ctrl Pts',(126.476734802636,-4.35111936196286,332.707197487691));
#54370=CARTESIAN_POINT('Ctrl Pts',(126.468961266412,-4.4150578764814,332.828535503941));
#54371=CARTESIAN_POINT('Ctrl Pts',(126.461187730187,-4.47398711153813,332.952683131024));
#54372=CARTESIAN_POINT('Ctrl Pts',(126.453414193963,-4.52765577805612,333.079188656339));
#54373=CARTESIAN_POINT('Ctrl Pts',(126.445646831812,-4.58128181862964,333.205593705569));
#54374=CARTESIAN_POINT('Ctrl Pts',(126.437879469662,-4.62965545476653,333.334352570164));
#54375=CARTESIAN_POINT('Ctrl Pts',(126.430112107512,-4.67257178717879,333.464989916593));
#54376=CARTESIAN_POINT('Ctrl Pts',(126.422349084645,-4.71546414412489,333.595554281686));
#54377=CARTESIAN_POINT('Ctrl Pts',(126.414586061778,-4.75290514467762,333.727994671824));
#54378=CARTESIAN_POINT('Ctrl Pts',(126.406823038911,-4.78473852488,333.86181710124));
#54379=CARTESIAN_POINT('Ctrl Pts',(126.399062681011,-4.81656097700833,333.995593590784));
#54380=CARTESIAN_POINT('Ctrl Pts',(126.39130232311,-4.84277955234705,334.130750797493));
#54381=CARTESIAN_POINT('Ctrl Pts',(126.38354196521,-4.86328833123651,334.266781294729));
#54382=CARTESIAN_POINT('Ctrl Pts',(126.375780911624,-4.88379894865548,334.402823986553));
#54383=CARTESIAN_POINT('Ctrl Pts',(126.368019858039,-4.89859868215799,334.539739742315));
#54384=CARTESIAN_POINT('Ctrl Pts',(126.360258804454,-4.9076330630066,334.677012722566));
#54385=CARTESIAN_POINT('Ctrl Pts',(126.354111661805,-4.91478874453972,334.785739789338));
#54386=CARTESIAN_POINT('Ctrl Pts',(126.347964519157,-4.91832857672598,334.894690727873));
#54387=CARTESIAN_POINT('Ctrl Pts',(126.341817376508,-4.91824867662815,335.003607955855));
#54388=CARTESIAN_POINT('',(124.59181841765,-4.92215355118558,335.001694350306));
#54389=CARTESIAN_POINT('Ctrl Pts',(126.341815268991,-4.91310111576097,335.003641482346));
#54390=CARTESIAN_POINT('Ctrl Pts',(126.309614694802,-4.91695460512051,335.573588454469));
#54391=CARTESIAN_POINT('Ctrl Pts',(126.184668109188,-4.56166528194609,337.7804684251));
#54392=CARTESIAN_POINT('Ctrl Pts',(125.96697551215,-1.29737390949771,340.669327103404));
#54393=CARTESIAN_POINT('Ctrl Pts',(125.688737477876,4.06537464531311,339.158987600327));
#54394=CARTESIAN_POINT('Ctrl Pts',(125.410499443602,5.69738889295149,333.832006562988));
#54395=CARTESIAN_POINT('Ctrl Pts',(125.132261409328,2.1009934468505,329.576875863238));
#54396=CARTESIAN_POINT('Ctrl Pts',(124.859368043239,-3.31733371268366,330.284605127136));
#54397=CARTESIAN_POINT('Ctrl Pts',(124.679220688574,-4.91870118483923,333.46478909301));
#54398=CARTESIAN_POINT('Ctrl Pts',(124.591819345333,-4.92563197232975,335.001679248013));
#54399=CARTESIAN_POINT('',(122.841817376472,-4.91824791957163,334.995476270419));
#54400=CARTESIAN_POINT('Ctrl Pts',(124.591817376508,-4.91824970227757,335.001711299682));
#54401=CARTESIAN_POINT('Ctrl Pts',(124.586473364599,-4.91821705436066,335.095540924806));
#54402=CARTESIAN_POINT('Ctrl Pts',(124.58112935269,-4.91549949813635,335.189320593499));
#54403=CARTESIAN_POINT('Ctrl Pts',(124.57578534078,-4.91010442639044,335.282944490035));
#54404=CARTESIAN_POINT('Ctrl Pts',(124.568010262002,-4.90225505993097,335.419159225979));
#54405=CARTESIAN_POINT('Ctrl Pts',(124.560235183224,-4.8887207487364,335.555262327574));
#54406=CARTESIAN_POINT('Ctrl Pts',(124.552460104445,-4.8695030692698,335.690740849286));
#54407=CARTESIAN_POINT('Ctrl Pts',(124.544694593396,-4.85030903838123,335.826052656051));
#54408=CARTESIAN_POINT('Ctrl Pts',(124.536929082347,-4.82544560914213,335.960741028896));
#54409=CARTESIAN_POINT('Ctrl Pts',(124.529163571298,-4.79496632083138,336.094294770431));
#54410=CARTESIAN_POINT('Ctrl Pts',(124.521405759776,-4.76451725282374,336.227716093042));
#54411=CARTESIAN_POINT('Ctrl Pts',(124.513647948254,-4.72846349306716,336.360004644515));
#54412=CARTESIAN_POINT('Ctrl Pts',(124.505890136731,-4.68691011530145,336.490656443848));
#54413=CARTESIAN_POINT('Ctrl Pts',(124.498138163208,-4.64538800777035,336.621209923558));
#54414=CARTESIAN_POINT('Ctrl Pts',(124.490386189685,-4.59837463797649,336.750128731792));
#54415=CARTESIAN_POINT('Ctrl Pts',(124.482634216162,-4.54602560084518,336.876921495151));
#54416=CARTESIAN_POINT('Ctrl Pts',(124.474885525605,-4.49369873356204,337.0036605617));
#54417=CARTESIAN_POINT('Ctrl Pts',(124.467136835047,-4.43604084209907,337.128275013629));
#54418=CARTESIAN_POINT('Ctrl Pts',(124.45938814449,-4.37325651379635,337.250291209386));
#54419=CARTESIAN_POINT('Ctrl Pts',(124.451641066112,-4.31048524829749,337.372282018654));
#54420=CARTESIAN_POINT('Ctrl Pts',(124.443893987734,-4.24258984622571,337.491675299677));
#54421=CARTESIAN_POINT('Ctrl Pts',(124.436146909356,-4.16982175769608,337.608020239865));
#54422=CARTESIAN_POINT('Ctrl Pts',(124.42839976605,-4.09705305929994,337.724366155135));
#54423=CARTESIAN_POINT('Ctrl Pts',(124.420652622744,-4.01941180026238,337.837663347221));
#54424=CARTESIAN_POINT('Ctrl Pts',(124.412905479439,-3.93719362216656,337.947488667335));
#54425=CARTESIAN_POINT('Ctrl Pts',(124.40515659441,-3.85495695967874,338.057338678514));
#54426=CARTESIAN_POINT('Ctrl Pts',(124.397407709382,-3.76814156476404,338.163714951669));
#54427=CARTESIAN_POINT('Ctrl Pts',(124.389658824354,-3.67708408910537,338.266226517581));
#54428=CARTESIAN_POINT('Ctrl Pts',(124.38190171458,-3.5859299641011,338.368846890328));
#54429=CARTESIAN_POINT('Ctrl Pts',(124.374144604805,-3.49052502400119,338.467594068925));
#54430=CARTESIAN_POINT('Ctrl Pts',(124.36638749503,-3.39124398410291,338.562112758292));
#54431=CARTESIAN_POINT('Ctrl Pts',(124.358626240104,-3.2919098915913,338.656681955424));
#54432=CARTESIAN_POINT('Ctrl Pts',(124.350864985178,-3.18869586608189,338.74701790363));
#54433=CARTESIAN_POINT('Ctrl Pts',(124.343103730252,-3.08200982573676,338.83280556467));
#54434=CARTESIAN_POINT('Ctrl Pts',(124.335330059847,-2.97515312249605,338.918730458009));
#54435=CARTESIAN_POINT('Ctrl Pts',(124.327556389442,-2.86481362045928,339.000092292927));
#54436=CARTESIAN_POINT('Ctrl Pts',(124.319782719038,-2.7514290660605,339.07661883881));
#54437=CARTESIAN_POINT('Ctrl Pts',(124.312370914861,-2.64332258994761,339.14958305557));
#54438=CARTESIAN_POINT('Ctrl Pts',(124.304959110683,-2.53244842075332,339.218151866638));
#54439=CARTESIAN_POINT('Ctrl Pts',(124.297547306506,-2.41920518882687,339.282129063545));
#54440=CARTESIAN_POINT('Ctrl Pts',(124.289772227728,-2.30041156876948,339.349241973449));
#54441=CARTESIAN_POINT('Ctrl Pts',(124.28199714895,-2.17863537461952,339.411513880292));
#54442=CARTESIAN_POINT('Ctrl Pts',(124.274222070171,-2.05430880633529,339.468668525491));
#54443=CARTESIAN_POINT('Ctrl Pts',(124.266456559122,-1.93013522980844,339.525752838261));
#54444=CARTESIAN_POINT('Ctrl Pts',(124.258691048073,-1.80341787540803,339.577732257139));
#54445=CARTESIAN_POINT('Ctrl Pts',(124.250925537024,-1.67461559310128,339.624375166208));
#54446=CARTESIAN_POINT('Ctrl Pts',(124.243167725502,-1.54594101863225,339.670971828697));
#54447=CARTESIAN_POINT('Ctrl Pts',(124.23540991398,-1.41518599527714,339.712242378862));
#54448=CARTESIAN_POINT('Ctrl Pts',(124.227652102457,-1.28283119284316,339.748002442414));
#54449=CARTESIAN_POINT('Ctrl Pts',(124.219900128934,-1.1505759915954,339.783735595384));
#54450=CARTESIAN_POINT('Ctrl Pts',(124.212148155411,-1.01672378336661,339.813966414233));
#54451=CARTESIAN_POINT('Ctrl Pts',(124.204396181888,-0.881771975873617,
339.838559831713));
#54452=CARTESIAN_POINT('Ctrl Pts',(124.196647491331,-0.746877320551128,
339.863142833865));
#54453=CARTESIAN_POINT('Ctrl Pts',(124.188898800773,-0.610884375911698,
339.882093113171));
#54454=CARTESIAN_POINT('Ctrl Pts',(124.181150110216,-0.474302151189679,
339.895326396868));
#54455=CARTESIAN_POINT('Ctrl Pts',(124.173403031838,-0.337748343540318,
339.90855692727));
#54456=CARTESIAN_POINT('Ctrl Pts',(124.16565595346,-0.200605888485871,339.91607279033));
#54457=CARTESIAN_POINT('Ctrl Pts',(124.157908875082,-0.0633899580356592,
339.917841475253));
#54458=CARTESIAN_POINT('Ctrl Pts',(124.150161731776,0.0738271224160726,
339.919610175));
#54459=CARTESIAN_POINT('Ctrl Pts',(124.142414588471,0.211117288649995,339.9156315955));
#54460=CARTESIAN_POINT('Ctrl Pts',(124.134667445165,0.34796471720093,339.905925357981));
#54461=CARTESIAN_POINT('Ctrl Pts',(124.126918560137,0.484842911959203,339.896216938294));
#54462=CARTESIAN_POINT('Ctrl Pts',(124.119169675109,0.621277781148712,339.880778325859));
#54463=CARTESIAN_POINT('Ctrl Pts',(124.111420790081,0.756758368867927,339.859681042378));
#54464=CARTESIAN_POINT('Ctrl Pts',(124.103663680306,0.892382757082815,339.838561366023));
#54465=CARTESIAN_POINT('Ctrl Pts',(124.095906570531,1.02705045366658,339.811771080969));
#54466=CARTESIAN_POINT('Ctrl Pts',(124.088149460756,1.16025990345685,339.779433022748));
#54467=CARTESIAN_POINT('Ctrl Pts',(124.08038820583,1.29354053611778,339.747077684102));
#54468=CARTESIAN_POINT('Ctrl Pts',(124.072626950904,1.42536099381965,339.709168773126));
#54469=CARTESIAN_POINT('Ctrl Pts',(124.064865695978,1.55523560626181,339.665878831637));
#54470=CARTESIAN_POINT('Ctrl Pts',(124.057092025573,1.68531797575783,339.622519640349));
#54471=CARTESIAN_POINT('Ctrl Pts',(124.049318355169,1.81344791435055,339.573762356511));
#54472=CARTESIAN_POINT('Ctrl Pts',(124.041544684764,1.93915960779533,339.519827770833));
#54473=CARTESIAN_POINT('Ctrl Pts',(124.034132880587,2.05901939166561,339.468403853095));
#54474=CARTESIAN_POINT('Ctrl Pts',(124.02672107641,2.17668074265337,339.412273916969));
#54475=CARTESIAN_POINT('Ctrl Pts',(124.019309272233,2.29176294311589,339.35166699956));
#54476=CARTESIAN_POINT('Ctrl Pts',(124.011534193454,2.41248566503534,339.288089556591));
#54477=CARTESIAN_POINT('Ctrl Pts',(124.003759114676,2.5307515261828,339.219384258902));
#54478=CARTESIAN_POINT('Ctrl Pts',(123.995984035898,2.64609432662721,339.145765053291));
#54479=CARTESIAN_POINT('Ctrl Pts',(123.988218524849,2.76129519041259,339.0722364408));
#54480=CARTESIAN_POINT('Ctrl Pts',(123.980453013799,2.87357982418608,338.993806160222));
#54481=CARTESIAN_POINT('Ctrl Pts',(123.97268750275,2.98250514713447,338.91073472762));
#54482=CARTESIAN_POINT('Ctrl Pts',(123.964929691228,3.09132247030802,338.827745660586));
#54483=CARTESIAN_POINT('Ctrl Pts',(123.957171879706,3.19678680226941,338.740124834709));
#54484=CARTESIAN_POINT('Ctrl Pts',(123.949414068184,3.29848298073142,338.648176679977));
#54485=CARTESIAN_POINT('Ctrl Pts',(123.941662094661,3.40010262959414,338.556297719146));
#54486=CARTESIAN_POINT('Ctrl Pts',(123.933910121138,3.49795948042143,338.460098172359));
#54487=CARTESIAN_POINT('Ctrl Pts',(123.926158147615,3.59167077642494,338.359923227735));
#54488=CARTESIAN_POINT('Ctrl Pts',(123.918409457057,3.68534238563896,338.259790707261));
#54489=CARTESIAN_POINT('Ctrl Pts',(123.9106607665,3.77487166541158,338.15568642233));
#54490=CARTESIAN_POINT('Ctrl Pts',(123.902912075942,3.8599122948756,338.047992804842));
#54491=CARTESIAN_POINT('Ctrl Pts',(123.895164997564,3.94493523092639,337.94032159391));
#54492=CARTESIAN_POINT('Ctrl Pts',(123.887417919186,4.02547113217919,337.82906284241));
#54493=CARTESIAN_POINT('Ctrl Pts',(123.879670840809,4.10121387047949,337.714632176021));
#54494=CARTESIAN_POINT('Ctrl Pts',(123.871923697503,4.17695724357684,337.600200550592));
#54495=CARTESIAN_POINT('Ctrl Pts',(123.864176554197,4.24790715785358,337.48259728319));
#54496=CARTESIAN_POINT('Ctrl Pts',(123.856429410891,4.31380097154295,337.362266758945));
#54497=CARTESIAN_POINT('Ctrl Pts',(123.848680525863,4.37970959956056,337.241909181843));
#54498=CARTESIAN_POINT('Ctrl Pts',(123.840931640835,4.44055967734475,337.118823470575));
#54499=CARTESIAN_POINT('Ctrl Pts',(123.833182755807,4.49613484146449,336.993478003357));
#54500=CARTESIAN_POINT('Ctrl Pts',(123.825425646032,4.55176899363768,336.867999493165));
#54501=CARTESIAN_POINT('Ctrl Pts',(123.817668536257,4.60211688924213,336.74025679363));
#54502=CARTESIAN_POINT('Ctrl Pts',(123.809911426483,4.64701040301992,336.610738146542));
#54503=CARTESIAN_POINT('Ctrl Pts',(123.802150171557,4.69192790645605,336.48115028883));
#54504=CARTESIAN_POINT('Ctrl Pts',(123.79438891663,4.73138510798403,336.34978496674));
#54505=CARTESIAN_POINT('Ctrl Pts',(123.786627661704,4.76526427763109,336.217143963068));
#54506=CARTESIAN_POINT('Ctrl Pts',(123.7788539913,4.79919764290838,336.084290777018));
#54507=CARTESIAN_POINT('Ctrl Pts',(123.771080320895,4.82753506460514,335.950158214146));
#54508=CARTESIAN_POINT('Ctrl Pts',(123.76330665049,4.85021013152304,335.815257470111));
#54509=CARTESIAN_POINT('Ctrl Pts',(123.755894846313,4.87182966862059,335.686636388166));
#54510=CARTESIAN_POINT('Ctrl Pts',(123.748483042136,4.88830211627918,335.557317318753));
#54511=CARTESIAN_POINT('Ctrl Pts',(123.741071237959,4.89961404852394,335.427744360579));
#54512=CARTESIAN_POINT('Ctrl Pts',(123.733296159181,4.91148041226454,335.291820645746));
#54513=CARTESIAN_POINT('Ctrl Pts',(123.725521080402,4.91770510523584,335.155187981128));
#54514=CARTESIAN_POINT('Ctrl Pts',(123.717746001624,4.91821575232965,335.018354183078));
#54515=CARTESIAN_POINT('Ctrl Pts',(123.709980490575,4.91872577103971,334.881688767728));
#54516=CARTESIAN_POINT('Ctrl Pts',(123.702214979526,4.91353573309087,334.744823098551));
#54517=CARTESIAN_POINT('Ctrl Pts',(123.694449468477,4.90262493554631,334.608270751846));
#54518=CARTESIAN_POINT('Ctrl Pts',(123.686691656954,4.89172495608928,334.47185379719));
#54519=CARTESIAN_POINT('Ctrl Pts',(123.678933845432,4.87511553586719,334.335749933896));
#54520=CARTESIAN_POINT('Ctrl Pts',(123.67117603391,4.852828008416,334.200473025325));
#54521=CARTESIAN_POINT('Ctrl Pts',(123.663424060387,4.830557253036,334.065297916917));
#54522=CARTESIAN_POINT('Ctrl Pts',(123.655672086864,4.80261695882242,333.930948908676));
#54523=CARTESIAN_POINT('Ctrl Pts',(123.647920113341,4.76909027017057,333.797934670051));
#54524=CARTESIAN_POINT('Ctrl Pts',(123.640171422783,4.73557778009128,333.664976763035));
#54525=CARTESIAN_POINT('Ctrl Pts',(123.632422732226,4.69648369639993,333.533352879573));
#54526=CARTESIAN_POINT('Ctrl Pts',(123.624674041668,4.65194220014464,333.403561204113));
#54527=CARTESIAN_POINT('Ctrl Pts',(123.61692696329,4.60740997111966,333.273796532895));
#54528=CARTESIAN_POINT('Ctrl Pts',(123.609179884912,4.55743271069921,333.145863680911));
#54529=CARTESIAN_POINT('Ctrl Pts',(123.601432806535,4.50219426387252,333.02024499676));
#54530=CARTESIAN_POINT('Ctrl Pts',(123.593685663229,4.44695535409447,332.894625259804));
#54531=CARTESIAN_POINT('Ctrl Pts',(123.585938519923,4.38645532730135,332.771320087173));
#54532=CARTESIAN_POINT('Ctrl Pts',(123.578191376617,4.32092574589757,332.650790822226));
#54533=CARTESIAN_POINT('Ctrl Pts',(123.570442491589,4.25538143205276,332.53023445974));
#54534=CARTESIAN_POINT('Ctrl Pts',(123.562693606561,4.184805500195,332.412455590129));
#54535=CARTESIAN_POINT('Ctrl Pts',(123.554944721533,4.1094747328909,332.297889624343));
#54536=CARTESIAN_POINT('Ctrl Pts',(123.547187611758,4.03406400873195,332.183202057058));
#54537=CARTESIAN_POINT('Ctrl Pts',(123.539430501983,3.95388858269473,332.071734532926));
#54538=CARTESIAN_POINT('Ctrl Pts',(123.531673392209,3.86926804549347,331.963892647711));
#54539=CARTESIAN_POINT('Ctrl Pts',(123.523912137283,3.78460228978281,331.855993135241));
#54540=CARTESIAN_POINT('Ctrl Pts',(123.516150882356,3.69548694368209,331.75172341917));
#54541=CARTESIAN_POINT('Ctrl Pts',(123.50838962743,3.60228025660474,331.651454044607));
#54542=CARTESIAN_POINT('Ctrl Pts',(123.500615957026,3.50892446920409,331.551024271723));
#54543=CARTESIAN_POINT('Ctrl Pts',(123.492842286621,3.41146454037353,331.454607902971));
#54544=CARTESIAN_POINT('Ctrl Pts',(123.485068616216,3.31029440653752,331.362537422248));
#54545=CARTESIAN_POINT('Ctrl Pts',(123.477656812039,3.21383376677184,331.274752844554));
#54546=CARTESIAN_POINT('Ctrl Pts',(123.470245007862,3.11400078901798,331.190918843107));
#54547=CARTESIAN_POINT('Ctrl Pts',(123.462833203685,3.0111616597879,331.11128703539));
#54548=CARTESIAN_POINT('Ctrl Pts',(123.455058124907,2.90328207849218,331.027752235566));
#54549=CARTESIAN_POINT('Ctrl Pts',(123.447283046128,2.79175329442391,330.948577983643));
#54550=CARTESIAN_POINT('Ctrl Pts',(123.43950796735,2.67696317486632,330.874099949961));
#54551=CARTESIAN_POINT('Ctrl Pts',(123.431742456301,2.56231431185874,330.799713566242));
#54552=CARTESIAN_POINT('Ctrl Pts',(123.423976945252,2.44441242340842,330.730012112935));
#54553=CARTESIAN_POINT('Ctrl Pts',(123.416211434203,2.3236781832345,330.665290925188));
#54554=CARTESIAN_POINT('Ctrl Pts',(123.40845362268,2.20306365141118,330.600633908686));
#54555=CARTESIAN_POINT('Ctrl Pts',(123.400695811158,2.07962269878878,330.540947514431));
#54556=CARTESIAN_POINT('Ctrl Pts',(123.392937999636,1.95380440040298,330.486483474333));
#54557=CARTESIAN_POINT('Ctrl Pts',(123.385186026113,1.82808078427677,330.432060420153));
#54558=CARTESIAN_POINT('Ctrl Pts',(123.37743405259,1.69998374062414,330.382852052333));
#54559=CARTESIAN_POINT('Ctrl Pts',(123.369682079067,1.56998601463972,330.339063723206));
#54560=CARTESIAN_POINT('Ctrl Pts',(123.361933388509,1.44004334276939,330.295293938462));
#54561=CARTESIAN_POINT('Ctrl Pts',(123.354184697952,1.30820195918995,330.256939751555));
#54562=CARTESIAN_POINT('Ctrl Pts',(123.346436007394,1.17495341089747,330.224157922971));
#54563=CARTESIAN_POINT('Ctrl Pts',(123.338688929016,1.04173258607837,330.19138291492));
#54564=CARTESIAN_POINT('Ctrl Pts',(123.330941850639,0.907105558209408,330.164178052432));
#54565=CARTESIAN_POINT('Ctrl Pts',(123.323194772261,0.771577433590507,330.142649762836));
#54566=CARTESIAN_POINT('Ctrl Pts',(123.315447628955,0.636048173115384,330.121121292813));
#54567=CARTESIAN_POINT('Ctrl Pts',(123.307700485649,0.4996181868615,330.105269551895));
#54568=CARTESIAN_POINT('Ctrl Pts',(123.299953342343,0.362800740003776,330.095149473679));
#54569=CARTESIAN_POINT('Ctrl Pts',(123.292204457315,0.225952533679329,330.085027120254));
#54570=CARTESIAN_POINT('Ctrl Pts',(123.284455572287,0.0887170831463317,
330.080639022528));
#54571=CARTESIAN_POINT('Ctrl Pts',(123.276706687259,-0.0483896823070491,
330.081988053985));
#54572=CARTESIAN_POINT('Ctrl Pts',(123.268949577484,-0.18564197429786,330.083338517318));
#54573=CARTESIAN_POINT('Ctrl Pts',(123.26119246771,-0.322764916889646,330.090438270227));
#54574=CARTESIAN_POINT('Ctrl Pts',(123.253435357935,-0.459244487077345,
330.103238053204));
#54575=CARTESIAN_POINT('Ctrl Pts',(123.245674103009,-0.595796987583629,
330.116044675976));
#54576=CARTESIAN_POINT('Ctrl Pts',(123.237912848082,-0.731705043536764,
330.134557345343));
#54577=CARTESIAN_POINT('Ctrl Pts',(123.230151593156,-0.86646318633607,330.158675324952));
#54578=CARTESIAN_POINT('Ctrl Pts',(123.222377922752,-1.00143689824623,330.182831885469));
#54579=CARTESIAN_POINT('Ctrl Pts',(123.214604252347,-1.13525663942247,330.212611589337));
#54580=CARTESIAN_POINT('Ctrl Pts',(123.206830581942,-1.26742963545979,330.247863093128));
#54581=CARTESIAN_POINT('Ctrl Pts',(123.199418777765,-1.39344994673317,330.281473630936));
#54582=CARTESIAN_POINT('Ctrl Pts',(123.192006973588,-1.5179730997478,330.320057923196));
#54583=CARTESIAN_POINT('Ctrl Pts',(123.184595169411,-1.64058933946203,330.363444200514));
#54584=CARTESIAN_POINT('Ctrl Pts',(123.176820090632,-1.76921536633913,330.408956968525));
#54585=CARTESIAN_POINT('Ctrl Pts',(123.169045011854,-1.89614930846979,330.459898171677));
#54586=CARTESIAN_POINT('Ctrl Pts',(123.161269933076,-2.0208989962603,330.516123294579));
#54587=CARTESIAN_POINT('Ctrl Pts',(123.153504422027,-2.14549517161785,330.572279228888));
#54588=CARTESIAN_POINT('Ctrl Pts',(123.145738910978,-2.26791208776777,330.63370598636));
#54589=CARTESIAN_POINT('Ctrl Pts',(123.137973399929,-2.38767374039788,330.700209636283));
#54590=CARTESIAN_POINT('Ctrl Pts',(123.130215588406,-2.50731664900086,330.766647347644));
#54591=CARTESIAN_POINT('Ctrl Pts',(123.122457776884,-2.6243091937875,330.838151745465));
#54592=CARTESIAN_POINT('Ctrl Pts',(123.114699965362,-2.73819666775436,330.91448141955));
#54593=CARTESIAN_POINT('Ctrl Pts',(123.106947991839,-2.85199843778543,330.990753653135));
#54594=CARTESIAN_POINT('Ctrl Pts',(123.099196018316,-2.96269946462649,331.071843718571));
#54595=CARTESIAN_POINT('Ctrl Pts',(123.091444044793,-3.06987123357102,331.157465202266));
#54596=CARTESIAN_POINT('Ctrl Pts',(123.083695354235,-3.17699761520774,331.243050425213));
#54597=CARTESIAN_POINT('Ctrl Pts',(123.075946663678,-3.28059740694012,331.333163006079));
#54598=CARTESIAN_POINT('Ctrl Pts',(123.06819797312,-3.3802727812472,331.427474424604));
#54599=CARTESIAN_POINT('Ctrl Pts',(123.060450894742,-3.47992741726014,331.52176622085));
#54600=CARTESIAN_POINT('Ctrl Pts',(123.052703816364,-3.57565897619402,331.62025484862));
#54601=CARTESIAN_POINT('Ctrl Pts',(123.044956737986,-3.66710461903429,331.722573147184));
#54602=CARTESIAN_POINT('Ctrl Pts',(123.037209594681,-3.75855102827707,331.824892303275));
#54603=CARTESIAN_POINT('Ctrl Pts',(123.029462451375,-3.84571118930982,331.931040902738));
#54604=CARTESIAN_POINT('Ctrl Pts',(123.021715308069,-3.92826115006238,332.04061705766));
#54605=CARTESIAN_POINT('Ctrl Pts',(123.013966423041,-4.01082966979873,332.150217847628));
#54606=CARTESIAN_POINT('Ctrl Pts',(123.006217538013,-4.08878569164476,332.263247414303));
#54607=CARTESIAN_POINT('Ctrl Pts',(122.998468652985,-4.16184760028338,332.379273456746));
#54608=CARTESIAN_POINT('Ctrl Pts',(122.99071154321,-4.23498705758672,332.49542265043));
#54609=CARTESIAN_POINT('Ctrl Pts',(122.982954433435,-4.30322181624805,332.614574341928));
#54610=CARTESIAN_POINT('Ctrl Pts',(122.975197323661,-4.36631513229625,332.736269621183));
#54611=CARTESIAN_POINT('Ctrl Pts',(122.967436068734,-4.42944216339519,332.858029930504));
#54612=CARTESIAN_POINT('Ctrl Pts',(122.959674813808,-4.48742211225222,332.982336181877));
#54613=CARTESIAN_POINT('Ctrl Pts',(122.951913558882,-4.54006615215355,333.108708801752));
#54614=CARTESIAN_POINT('Ctrl Pts',(122.944139888478,-4.59279440536205,333.235283576634));
#54615=CARTESIAN_POINT('Ctrl Pts',(122.936366218073,-4.64016955758274,333.36393095843));
#54616=CARTESIAN_POINT('Ctrl Pts',(122.928592547668,-4.68205220822821,333.494154662017));
#54617=CARTESIAN_POINT('Ctrl Pts',(122.921180743491,-4.7219852114098,333.618316420872));
#54618=CARTESIAN_POINT('Ctrl Pts',(122.913768939314,-4.75692548012175,333.743910771334));
#54619=CARTESIAN_POINT('Ctrl Pts',(122.906357135137,-4.78679571694647,333.870500187374));
#54620=CARTESIAN_POINT('Ctrl Pts',(122.895600508699,-4.83014588803358,334.054217272555));
#54621=CARTESIAN_POINT('Ctrl Pts',(122.884843882261,-4.86293462881886,334.240514229832));
#54622=CARTESIAN_POINT('Ctrl Pts',(122.874087255823,-4.88491651648687,334.428358775582));
#54623=CARTESIAN_POINT('Ctrl Pts',(122.863330629385,-4.90689840415487,334.616203321333));
#54624=CARTESIAN_POINT('Ctrl Pts',(122.852574002947,-4.91807327065724,334.805596101312));
#54625=CARTESIAN_POINT('Ctrl Pts',(122.841817376508,-4.91824791957104,334.995476269776));
#54626=CARTESIAN_POINT('',(121.091817376452,-4.9182499653126,335.000584125506));
#54627=CARTESIAN_POINT('Ctrl Pts',(122.841817376472,-4.91824791957163,334.995476270419));
#54628=CARTESIAN_POINT('Ctrl Pts',(122.834159905798,-4.9183722493281,335.130648931646));
#54629=CARTESIAN_POINT('Ctrl Pts',(122.826502435125,-4.91291978064133,335.265979802592));
#54630=CARTESIAN_POINT('Ctrl Pts',(122.818844964452,-4.90187821147916,335.400965163482));
#54631=CARTESIAN_POINT('Ctrl Pts',(122.810898053469,-4.89041928842385,335.541052758035));
#54632=CARTESIAN_POINT('Ctrl Pts',(122.802951142486,-4.87294038696696,335.680767772425));
#54633=CARTESIAN_POINT('Ctrl Pts',(122.795004231503,-4.84948717539217,335.819546946921));
#54634=CARTESIAN_POINT('Ctrl Pts',(122.787355074242,-4.82691270538579,335.953126363205));
#54635=CARTESIAN_POINT('Ctrl Pts',(122.77970591698,-4.7988036110565,336.085838369296));
#54636=CARTESIAN_POINT('Ctrl Pts',(122.772056759719,-4.76525336520633,336.217186685718));
#54637=CARTESIAN_POINT('Ctrl Pts',(122.764408668907,-4.73170779695223,336.348516689477));
#54638=CARTESIAN_POINT('Ctrl Pts',(122.756760578096,-4.69272268492862,336.478482992305));
#54639=CARTESIAN_POINT('Ctrl Pts',(122.749112487284,-4.64844220410786,336.606601424613));
#54640=CARTESIAN_POINT('Ctrl Pts',(122.741463706305,-4.60415772739081,336.734731418403));
#54641=CARTESIAN_POINT('Ctrl Pts',(122.733814925325,-4.55457706320149,336.861012830311));
#54642=CARTESIAN_POINT('Ctrl Pts',(122.726166144346,-4.49989347265338,336.984979042023));
#54643=CARTESIAN_POINT('Ctrl Pts',(122.718514916266,-4.44519238699958,337.108984914664));
#54644=CARTESIAN_POINT('Ctrl Pts',(122.710863688186,-4.3853852907965,337.230673746815));
#54645=CARTESIAN_POINT('Ctrl Pts',(122.703212460106,-4.32071231699118,337.349601697374));
#54646=CARTESIAN_POINT('Ctrl Pts',(122.695552944593,-4.25596929260321,337.468658464835));
#54647=CARTESIAN_POINT('Ctrl Pts',(122.687893429079,-4.18635006378195,337.584948029246));
#54648=CARTESIAN_POINT('Ctrl Pts',(122.680233913565,-4.11213931729558,337.69805361282));
#54649=CARTESIAN_POINT('Ctrl Pts',(122.672569467805,-4.03788080313057,337.811231999747));
#54650=CARTESIAN_POINT('Ctrl Pts',(122.664905022045,-3.9590251217713,337.921222000921));
#54651=CARTESIAN_POINT('Ctrl Pts',(122.657240576285,-3.87589767980065,338.02763938378));
#54652=CARTESIAN_POINT('Ctrl Pts',(122.649565403942,-3.79265389890404,338.134205700417));
#54653=CARTESIAN_POINT('Ctrl Pts',(122.641890231599,-3.70512668721262,338.237189117517));
#54654=CARTESIAN_POINT('Ctrl Pts',(122.634215059256,-3.6136788986125,338.336241580015));
#54655=CARTESIAN_POINT('Ctrl Pts',(122.632183073125,-3.58946828419969,338.36246551624));
#54656=CARTESIAN_POINT('Ctrl Pts',(122.630151086994,-3.56498305269611,338.38841414331));
#54657=CARTESIAN_POINT('Ctrl Pts',(122.628119100863,-3.54023031797993,338.41408148089));
#54658=CARTESIAN_POINT('Ctrl Pts',(122.620344022085,-3.44551782980707,338.51229355462));
#54659=CARTESIAN_POINT('Ctrl Pts',(122.612568943306,-3.34656572341985,338.606716605221));
#54660=CARTESIAN_POINT('Ctrl Pts',(122.604793864528,-3.24370943285665,338.696962561035));
#54661=CARTESIAN_POINT('Ctrl Pts',(122.597028353479,-3.1409797135072,338.787097463455));
#54662=CARTESIAN_POINT('Ctrl Pts',(122.58926284243,-3.03435566025973,338.873065243246));
#54663=CARTESIAN_POINT('Ctrl Pts',(122.581497331381,-2.92421098485638,338.954513014082));
#54664=CARTESIAN_POINT('Ctrl Pts',(122.573739519859,-2.81417551821922,339.035880029216));
#54665=CARTESIAN_POINT('Ctrl Pts',(122.565981708336,-2.70062668838819,339.112735723133));
#54666=CARTESIAN_POINT('Ctrl Pts',(122.558223896814,-2.58397259673982,339.1847662637));
#54667=CARTESIAN_POINT('Ctrl Pts',(122.550471923291,-2.46740629099456,339.256742599));
#54668=CARTESIAN_POINT('Ctrl Pts',(122.542719949768,-2.3477397059761,339.323900803905));
#54669=CARTESIAN_POINT('Ctrl Pts',(122.534967976245,-2.22541105112032,339.385969529768));
#54670=CARTESIAN_POINT('Ctrl Pts',(122.527219285688,-2.10313420252278,339.448011969488));
#54671=CARTESIAN_POINT('Ctrl Pts',(122.51947059513,-1.9781978742298,339.504969040604));
#54672=CARTESIAN_POINT('Ctrl Pts',(122.511721904572,-1.85106588508885,339.556614768834));
#54673=CARTESIAN_POINT('Ctrl Pts',(122.503974826194,-1.72396034682007,339.60824975174));
#54674=CARTESIAN_POINT('Ctrl Pts',(122.496227747817,-1.59466041826794,339.654575442801));
#54675=CARTESIAN_POINT('Ctrl Pts',(122.488480669439,-1.463650590928,339.695413720874));
#54676=CARTESIAN_POINT('Ctrl Pts',(122.480733526133,-1.33263966559965,339.736252341212));
#54677=CARTESIAN_POINT('Ctrl Pts',(122.472986382827,-1.19991918606457,339.77160334051));
#54678=CARTESIAN_POINT('Ctrl Pts',(122.465239239521,-1.06598913971513,339.801338377631));
#54679=CARTESIAN_POINT('Ctrl Pts',(122.457490354493,-0.93202898304785,339.831080099819));
#54680=CARTESIAN_POINT('Ctrl Pts',(122.449741469465,-0.796859099951614,
339.855203262722));
#54681=CARTESIAN_POINT('Ctrl Pts',(122.441992584437,-0.660989617969191,
339.873630657676));
#54682=CARTESIAN_POINT('Ctrl Pts',(122.434235474662,-0.524975922714567,
339.892077611657));
#54683=CARTESIAN_POINT('Ctrl Pts',(122.426478364888,-0.388261533177497,
339.904816668529));
#54684=CARTESIAN_POINT('Ctrl Pts',(122.418721255113,-0.25136220488622,339.911822482995));
#54685=CARTESIAN_POINT('Ctrl Pts',(122.410960000187,-0.114389721971095,
339.918832041144));
#54686=CARTESIAN_POINT('Ctrl Pts',(122.40319874526,0.0227675059574034,339.920102248649));
#54687=CARTESIAN_POINT('Ctrl Pts',(122.395437490334,0.159594768660187,339.915659932534));
#54688=CARTESIAN_POINT('Ctrl Pts',(122.38766381993,0.296640910391301,339.91121051016));
#54689=CARTESIAN_POINT('Ctrl Pts',(122.379890149525,0.433355642122252,339.901030332424));
#54690=CARTESIAN_POINT('Ctrl Pts',(122.37211647912,0.569229520832275,339.885198134683));
#54691=CARTESIAN_POINT('Ctrl Pts',(122.364704674943,0.698778437799172,339.870102929556));
#54692=CARTESIAN_POINT('Ctrl Pts',(122.357292870766,0.827562739132954,339.849870110281));
#54693=CARTESIAN_POINT('Ctrl Pts',(122.349881066589,0.955152190086452,339.824610591154));
#54694=CARTESIAN_POINT('Ctrl Pts',(122.342105987811,1.08899518010035,339.79811302775));
#54695=CARTESIAN_POINT('Ctrl Pts',(122.334330909032,1.22194620041557,339.765999821112));
#54696=CARTESIAN_POINT('Ctrl Pts',(122.326555830254,1.3534973906889,339.728343037037));
#54697=CARTESIAN_POINT('Ctrl Pts',(122.318790319205,1.48488669884765,339.690732592033));
#54698=CARTESIAN_POINT('Ctrl Pts',(122.311024808156,1.61487923221551,339.647592249408));
#54699=CARTESIAN_POINT('Ctrl Pts',(122.303259297107,1.74297600428424,339.599045304298));
#54700=CARTESIAN_POINT('Ctrl Pts',(122.295501485584,1.87094576803062,339.550546493627));
#54701=CARTESIAN_POINT('Ctrl Pts',(122.287743674062,1.99702314794207,339.496651886121));
#54702=CARTESIAN_POINT('Ctrl Pts',(122.27998586254,2.12072338880957,339.43753483036));
#54703=CARTESIAN_POINT('Ctrl Pts',(122.272233889017,2.24433054132276,339.378462262058));
#54704=CARTESIAN_POINT('Ctrl Pts',(122.264481915494,2.3655637642055,339.314175235953));
#54705=CARTESIAN_POINT('Ctrl Pts',(122.256729941971,2.48395773432029,339.244895409384));
#54706=CARTESIAN_POINT('Ctrl Pts',(122.248981251413,2.6023015645186,339.175644922863));
#54707=CARTESIAN_POINT('Ctrl Pts',(122.241232560856,2.71780819683018,339.101406038379));
#54708=CARTESIAN_POINT('Ctrl Pts',(122.233483870298,2.83003660566866,339.022446503445));
#54709=CARTESIAN_POINT('Ctrl Pts',(122.22573679192,2.9422416644492,338.943503396702));
#54710=CARTESIAN_POINT('Ctrl Pts',(122.217989713542,3.05116953694549,338.85984181789));
#54711=CARTESIAN_POINT('Ctrl Pts',(122.210242635165,3.15640825113983,338.771772794673));
#54712=CARTESIAN_POINT('Ctrl Pts',(122.202495491859,3.26164784733589,338.683703033353));
#54713=CARTESIAN_POINT('Ctrl Pts',(122.194748348553,3.36319792380149,338.591226004805));
#54714=CARTESIAN_POINT('Ctrl Pts',(122.187001205247,3.4606799838699,338.494692706339));
#54715=CARTESIAN_POINT('Ctrl Pts',(122.179252320219,3.55818395997528,338.398137705139));
#54716=CARTESIAN_POINT('Ctrl Pts',(122.171503435191,3.65161782209463,338.297524894353));
#54717=CARTESIAN_POINT('Ctrl Pts',(122.163754550163,3.74064058453279,338.193241469079));
#54718=CARTESIAN_POINT('Ctrl Pts',(122.155997440388,3.8297578366506,338.0888473563));
#54719=CARTESIAN_POINT('Ctrl Pts',(122.148240330613,3.91445438219807,337.980775144105));
#54720=CARTESIAN_POINT('Ctrl Pts',(122.140483220839,3.99442980286522,337.869444826527));
#54721=CARTESIAN_POINT('Ctrl Pts',(122.132721965912,4.07444795984006,337.758055017587));
#54722=CARTESIAN_POINT('Ctrl Pts',(122.124960710986,4.14973975054163,337.643403960666));
#54723=CARTESIAN_POINT('Ctrl Pts',(122.11719945606,4.2200491951423,337.525939004228));
#54724=CARTESIAN_POINT('Ctrl Pts',(122.109425785655,4.29047111194052,337.408286142141));
#54725=CARTESIAN_POINT('Ctrl Pts',(122.101652115251,4.35589456932713,337.287810729236));
#54726=CARTESIAN_POINT('Ctrl Pts',(122.093878444846,4.41611008869309,337.164983775238));
#54727=CARTESIAN_POINT('Ctrl Pts',(122.086466640669,4.47352256114517,337.047874445499));
#54728=CARTESIAN_POINT('Ctrl Pts',(122.079054836492,4.52620092686151,336.928627839548));
#54729=CARTESIAN_POINT('Ctrl Pts',(122.071643032315,4.57400563133066,336.80766577305));
#54730=CARTESIAN_POINT('Ctrl Pts',(122.063867953537,4.62415338676901,336.680774995344));
#54731=CARTESIAN_POINT('Ctrl Pts',(122.056092874758,4.66909613202267,336.551595347209));
#54732=CARTESIAN_POINT('Ctrl Pts',(122.04831779598,4.70861963638458,336.420592898178));
#54733=CARTESIAN_POINT('Ctrl Pts',(122.040552284931,4.74809450455819,336.289751656001));
#54734=CARTESIAN_POINT('Ctrl Pts',(122.032786773882,4.78216328886125,336.157092446636));
#54735=CARTESIAN_POINT('Ctrl Pts',(122.025021262833,4.81065964057301,336.023101600557));
#54736=CARTESIAN_POINT('Ctrl Pts',(122.01726345131,4.83912773806905,335.889243606792));
#54737=CARTESIAN_POINT('Ctrl Pts',(122.009505639788,4.86203431741517,335.754056983689));
#54738=CARTESIAN_POINT('Ctrl Pts',(122.001747828266,4.87926282227019,335.618043181106));
#54739=CARTESIAN_POINT('Ctrl Pts',(121.993995854743,4.89647836212897,335.482131733224));
#54740=CARTESIAN_POINT('Ctrl Pts',(121.98624388122,4.90802428363638,335.34539473109));
#54741=CARTESIAN_POINT('Ctrl Pts',(121.978491907697,4.91383517012843,335.208343426364));
#54742=CARTESIAN_POINT('Ctrl Pts',(121.970743217139,4.91964359570659,335.071350162947));
#54743=CARTESIAN_POINT('Ctrl Pts',(121.962994526582,4.91972180043954,334.934043251389));
#54744=CARTESIAN_POINT('Ctrl Pts',(121.955245836024,4.91405627467309,334.796938453059));
#54745=CARTESIAN_POINT('Ctrl Pts',(121.947498757646,4.90839192766659,334.659862180527));
#54746=CARTESIAN_POINT('Ctrl Pts',(121.939751679269,4.8969862432901,334.522988327875));
#54747=CARTESIAN_POINT('Ctrl Pts',(121.932004600891,4.87987782964372,334.386831646078));
#54748=CARTESIAN_POINT('Ctrl Pts',(121.924257457585,4.86276927261236,334.250673823156));
#54749=CARTESIAN_POINT('Ctrl Pts',(121.916510314279,4.83995793971277,334.115233570902));
#54750=CARTESIAN_POINT('Ctrl Pts',(121.908763170973,4.81153416580831,333.981019120023));
#54751=CARTESIAN_POINT('Ctrl Pts',(121.901014285945,4.78310400163598,333.846774494885));
#54752=CARTESIAN_POINT('Ctrl Pts',(121.893265400917,4.74905896659284,333.713756601827));
#54753=CARTESIAN_POINT('Ctrl Pts',(121.885516515889,4.70954013437084,333.582461716478));
#54754=CARTESIAN_POINT('Ctrl Pts',(121.877759406114,4.66997935645208,333.451027473381));
#54755=CARTESIAN_POINT('Ctrl Pts',(121.87000229634,4.62493328828028,333.321320266108));
#54756=CARTESIAN_POINT('Ctrl Pts',(121.862245186565,4.57459253821262,333.193820005695));
#54757=CARTESIAN_POINT('Ctrl Pts',(121.854483931639,4.52422488765774,333.066251613219));
#54758=CARTESIAN_POINT('Ctrl Pts',(121.846722676712,4.46855707611087,332.940892874562));
#54759=CARTESIAN_POINT('Ctrl Pts',(121.838961421786,4.40782676306542,332.818201134544));
#54760=CARTESIAN_POINT('Ctrl Pts',(121.831187751382,4.34699930131107,332.695313127728));
#54761=CARTESIAN_POINT('Ctrl Pts',(121.823414080977,4.28109334315855,332.575100987863));
#54762=CARTESIAN_POINT('Ctrl Pts',(121.815640410572,4.21039160983818,332.457995760369));
#54763=CARTESIAN_POINT('Ctrl Pts',(121.808228606395,4.14298105921344,332.346341809388));
#54764=CARTESIAN_POINT('Ctrl Pts',(121.800816802218,4.07121133062631,332.237512266963));
#54765=CARTESIAN_POINT('Ctrl Pts',(121.793404998041,3.9953616169164,332.131852756121));
#54766=CARTESIAN_POINT('Ctrl Pts',(121.785629919263,3.91579428279319,332.02101455791));
#54767=CARTESIAN_POINT('Ctrl Pts',(121.777854840484,3.83148545901994,331.913314724682));
#54768=CARTESIAN_POINT('Ctrl Pts',(121.770079761706,3.74271114088354,331.809185624577));
#54769=CARTESIAN_POINT('Ctrl Pts',(121.762314250657,3.65404606519725,331.705184661959));
#54770=CARTESIAN_POINT('Ctrl Pts',(121.754548739608,3.56092667993508,331.604745984242));
#54771=CARTESIAN_POINT('Ctrl Pts',(121.746783228559,3.46367192992948,331.508272658938));
#54772=CARTESIAN_POINT('Ctrl Pts',(121.739025417036,3.36651360829175,331.411894987217));
#54773=CARTESIAN_POINT('Ctrl Pts',(121.731267605514,3.2652283573074,331.319475117187));
#54774=CARTESIAN_POINT('Ctrl Pts',(121.723509793992,3.16017478153703,331.231382426852));
#54775=CARTESIAN_POINT('Ctrl Pts',(121.715757820469,3.05520026191402,331.143356029061));
#54776=CARTESIAN_POINT('Ctrl Pts',(121.708005846946,2.94646336029635,331.059650579522));
#54777=CARTESIAN_POINT('Ctrl Pts',(121.700253873423,2.83435859840053,330.980597756112));
#54778=CARTESIAN_POINT('Ctrl Pts',(121.692505182865,2.72230131293766,330.901578411619));
#54779=CARTESIAN_POINT('Ctrl Pts',(121.684756492308,2.60687932276282,330.827207999078));
#54780=CARTESIAN_POINT('Ctrl Pts',(121.67700780175,2.48851903176425,330.757776987115));
#54781=CARTESIAN_POINT('Ctrl Pts',(121.669260723372,2.37018336661294,330.688360420855));
#54782=CARTESIAN_POINT('Ctrl Pts',(121.661513644995,2.24891095356835,330.623881408687));
#54783=CARTESIAN_POINT('Ctrl Pts',(121.653766566617,2.12515555076475,330.564586045525));
#54784=CARTESIAN_POINT('Ctrl Pts',(121.646019423311,2.00139911077143,330.50529018541));
#54785=CARTESIAN_POINT('Ctrl Pts',(121.638272280005,1.87515999201355,330.451178229849));
#54786=CARTESIAN_POINT('Ctrl Pts',(121.630525136699,1.74691446191379,330.402449247126));
#54787=CARTESIAN_POINT('Ctrl Pts',(121.622776251671,1.61864009949674,330.353709309092));
#54788=CARTESIAN_POINT('Ctrl Pts',(121.615027366643,1.48835879344688,330.31035489088));
#54789=CARTESIAN_POINT('Ctrl Pts',(121.607278481615,1.35656421559843,330.272535923832));
#54790=CARTESIAN_POINT('Ctrl Pts',(121.59952137184,1.22462974962296,330.234676815341));
#54791=CARTESIAN_POINT('Ctrl Pts',(121.591764262066,1.0911791796142,330.202365002629));
#54792=CARTESIAN_POINT('Ctrl Pts',(121.584007152291,0.956719222120495,330.175699906461));
#54793=CARTESIAN_POINT('Ctrl Pts',(121.576245897365,0.822187413524834,330.149020561317));
#54794=CARTESIAN_POINT('Ctrl Pts',(121.568484642439,0.686645528730564,330.127994005098));
#54795=CARTESIAN_POINT('Ctrl Pts',(121.560723387512,0.550606769942869,330.112667880388));
#54796=CARTESIAN_POINT('Ctrl Pts',(121.552949717108,0.414350393475856,330.097317238873));
#54797=CARTESIAN_POINT('Ctrl Pts',(121.545176046703,0.277595944810239,330.087685278473));
#54798=CARTESIAN_POINT('Ctrl Pts',(121.537402376298,0.140858895915563,330.083767516284));
#54799=CARTESIAN_POINT('Ctrl Pts',(121.529990572121,0.0104869895433629,
330.080032126868));
#54800=CARTESIAN_POINT('Ctrl Pts',(121.522578767944,-0.119868812743053,
330.081490912733));
#54801=CARTESIAN_POINT('Ctrl Pts',(121.515166963767,-0.249766781901038,
330.088096131116));
#54802=CARTESIAN_POINT('Ctrl Pts',(121.507391884989,-0.386031437473093,
330.095025090928));
#54803=CARTESIAN_POINT('Ctrl Pts',(121.49961680621,-0.522222867092972,330.107639619914));
#54804=CARTESIAN_POINT('Ctrl Pts',(121.491841727432,-0.657828126280897,
330.125941606959));
#54805=CARTESIAN_POINT('Ctrl Pts',(121.484076216383,-0.793266514564706,
330.144221072244));
#54806=CARTESIAN_POINT('Ctrl Pts',(121.476310705334,-0.928119783977434,
330.168174018243));
#54807=CARTESIAN_POINT('Ctrl Pts',(121.468545194285,-1.06187638709854,330.197750360402));
#54808=CARTESIAN_POINT('Ctrl Pts',(121.460787382762,-1.19550037015804,330.227297377531));
#54809=CARTESIAN_POINT('Ctrl Pts',(121.45302957124,-1.32802947161284,330.262456611185));
#54810=CARTESIAN_POINT('Ctrl Pts',(121.445271759718,-1.45895901211281,330.303126394773));
#54811=CARTESIAN_POINT('Ctrl Pts',(121.437519786195,-1.58979002398029,330.343765573059));
#54812=CARTESIAN_POINT('Ctrl Pts',(121.429767812672,-1.71902349906192,330.389906931666));
#54813=CARTESIAN_POINT('Ctrl Pts',(121.422015839149,-1.84616702401678,330.441398198797));
#54814=CARTESIAN_POINT('Ctrl Pts',(121.414267148591,-1.97325670361412,330.492867659346));
#54815=CARTESIAN_POINT('Ctrl Pts',(121.406518458034,-2.098257831939,330.549682375705));
#54816=CARTESIAN_POINT('Ctrl Pts',(121.398769767476,-2.22069539611521,330.611640964988));
#54817=CARTESIAN_POINT('Ctrl Pts',(121.391022689098,-2.34310748613375,330.673586663269));
#54818=CARTESIAN_POINT('Ctrl Pts',(121.38327561072,-2.46295672437351,330.740673929343));
#54819=CARTESIAN_POINT('Ctrl Pts',(121.375528532343,-2.57979060980841,330.812654364392));
#54820=CARTESIAN_POINT('Ctrl Pts',(121.367781389037,-2.69662547442369,330.884635402707));
#54821=CARTESIAN_POINT('Ctrl Pts',(121.360034245731,-2.81044460304188,330.961509486766));
#54822=CARTESIAN_POINT('Ctrl Pts',(121.352287102425,-2.92082285926509,331.042983840405));
#54823=CARTESIAN_POINT('Ctrl Pts',(121.344538217397,-3.03122593086363,331.124476511209));
#54824=CARTESIAN_POINT('Ctrl Pts',(121.336789332369,-3.13818627630762,331.210571277526));
#54825=CARTESIAN_POINT('Ctrl Pts',(121.329040447341,-3.24131066097623,331.300934136631));
#54826=CARTESIAN_POINT('Ctrl Pts',(121.321283337566,-3.34454450293235,331.391392907809));
#54827=CARTESIAN_POINT('Ctrl Pts',(121.313526227791,-3.44393395640828,331.486128563262));
#54828=CARTESIAN_POINT('Ctrl Pts',(121.305769118017,-3.53912120296185,331.584768796517));
#54829=CARTESIAN_POINT('Ctrl Pts',(121.298007863091,-3.63435931453638,331.683461739958));
#54830=CARTESIAN_POINT('Ctrl Pts',(121.290246608164,-3.72539048549737,331.786063126467));
#54831=CARTESIAN_POINT('Ctrl Pts',(121.282485353238,-3.81189692901671,331.892167175498));
#54832=CARTESIAN_POINT('Ctrl Pts',(121.274711682834,-3.89854175465324,331.998440956428));
#54833=CARTESIAN_POINT('Ctrl Pts',(121.266938012429,-3.9806471547837,332.108228283385));
#54834=CARTESIAN_POINT('Ctrl Pts',(121.259164342024,-4.05793794771738,332.221093259036));
#54835=CARTESIAN_POINT('Ctrl Pts',(121.251752537847,-4.13163083564451,332.328704342916));
#54836=CARTESIAN_POINT('Ctrl Pts',(121.24434073367,-4.20094711591959,332.439112750813));
#54837=CARTESIAN_POINT('Ctrl Pts',(121.236928929493,-4.26568789151947,332.551921187003));
#54838=CARTESIAN_POINT('Ctrl Pts',(121.228828213401,-4.33644618871474,332.675214934724));
#54839=CARTESIAN_POINT('Ctrl Pts',(121.220727497309,-4.40194677956996,332.801737972689));
#54840=CARTESIAN_POINT('Ctrl Pts',(121.212626781217,-4.46189582822964,332.931022310288));
#54841=CARTESIAN_POINT('Ctrl Pts',(121.20453903916,-4.52174886302869,333.060099587247));
#54842=CARTESIAN_POINT('Ctrl Pts',(121.196451297102,-4.57606792476237,333.191929043033));
#54843=CARTESIAN_POINT('Ctrl Pts',(121.188363555044,-4.62460398813504,333.326016423191));
#54844=CARTESIAN_POINT('Ctrl Pts',(121.180292334472,-4.67304090296312,333.459829892206));
#54845=CARTESIAN_POINT('Ctrl Pts',(121.1722211139,-4.71571825763362,333.595891766523));
#54846=CARTESIAN_POINT('Ctrl Pts',(121.164149893328,-4.75243452649791,333.733686794726));
#54847=CARTESIAN_POINT('Ctrl Pts',(121.156088312233,-4.78910694503617,333.871317254004));
#54848=CARTESIAN_POINT('Ctrl Pts',(121.148026731138,-4.81983236969226,334.010676413363));
#54849=CARTESIAN_POINT('Ctrl Pts',(121.139965150044,-4.84445818720349,334.151231518648));
#54850=CARTESIAN_POINT('Ctrl Pts',(121.13191558772,-4.86904729081765,334.291577074517));
#54851=CARTESIAN_POINT('Ctrl Pts',(121.123866025396,-4.8875548596542,334.433114683237));
#54852=CARTESIAN_POINT('Ctrl Pts',(121.115816463072,-4.89987883100826,334.575299512671));
#54853=CARTESIAN_POINT('Ctrl Pts',(121.107816767551,-4.91212645572145,334.716603511261));
#54854=CARTESIAN_POINT('Ctrl Pts',(121.099817072029,-4.91826683467075,334.858546396624));
#54855=CARTESIAN_POINT('Ctrl Pts',(121.091817376508,-4.91824996531272,335.00058412452));
#54856=CARTESIAN_POINT('',(119.341817376544,-4.91824813200487,335.004286552297));
#54857=CARTESIAN_POINT('Ctrl Pts',(121.091817376452,-4.9182499653126,335.000584125506));
#54858=CARTESIAN_POINT('Ctrl Pts',(121.083626109023,-4.91823269194814,335.14602328768));
#54859=CARTESIAN_POINT('Ctrl Pts',(121.075434841593,-4.91175990151259,335.291314156804));
#54860=CARTESIAN_POINT('Ctrl Pts',(121.067243574164,-4.89889653869584,335.435885037199));
#54861=CARTESIAN_POINT('Ctrl Pts',(121.059038712186,-4.88601182733872,335.580695853086));
#54862=CARTESIAN_POINT('Ctrl Pts',(121.050833850209,-4.866715397838,335.724783977587));
#54863=CARTESIAN_POINT('Ctrl Pts',(121.042628988231,-4.84112349270298,335.867586532226));
#54864=CARTESIAN_POINT('Ctrl Pts',(121.034402112649,-4.81546292461099,336.010772225424));
#54865=CARTESIAN_POINT('Ctrl Pts',(121.026175237067,-4.78347315885324,336.152665136094));
#54866=CARTESIAN_POINT('Ctrl Pts',(121.017948361485,-4.74532117486993,336.292714202688));
#54867=CARTESIAN_POINT('Ctrl Pts',(121.009709509761,-4.70711365174982,336.432967143457));
#54868=CARTESIAN_POINT('Ctrl Pts',(121.001470658036,-4.66272609908869,336.571370578572));
#54869=CARTESIAN_POINT('Ctrl Pts',(120.993231806312,-4.61237422615327,336.707391888354));
#54870=CARTESIAN_POINT('Ctrl Pts',(120.98497374741,-4.56190496824396,336.843730303677));
#54871=CARTESIAN_POINT('Ctrl Pts',(120.976715688508,-4.50544371147639,336.977675195475));
#54872=CARTESIAN_POINT('Ctrl Pts',(120.968457629606,-4.44325357566152,337.108715420551));
#54873=CARTESIAN_POINT('Ctrl Pts',(120.965202051477,-4.41873633155052,337.160375465098));
#54874=CARTESIAN_POINT('Ctrl Pts',(120.961946473348,-4.39332920629337,337.211584371123));
#54875=CARTESIAN_POINT('Ctrl Pts',(120.958690895219,-4.36705018454127,337.262312035993));
#54876=CARTESIAN_POINT('Ctrl Pts',(120.950915816441,-4.30428976035348,337.383461513903));
#54877=CARTESIAN_POINT('Ctrl Pts',(120.943140737662,-4.23638500062128,337.502188829417));
#54878=CARTESIAN_POINT('Ctrl Pts',(120.935365658884,-4.16354669774589,337.618026347879));
#54879=CARTESIAN_POINT('Ctrl Pts',(120.927600147835,-4.09079802703937,337.7337213209));
#54880=CARTESIAN_POINT('Ctrl Pts',(120.919834636786,-4.01312809889304,337.846533244715));
#54881=CARTESIAN_POINT('Ctrl Pts',(120.912069125737,-3.93079443009848,337.956017288652));
#54882=CARTESIAN_POINT('Ctrl Pts',(120.904311314215,-3.84854239537604,338.06539277884));
#54883=CARTESIAN_POINT('Ctrl Pts',(120.896553502693,-3.7616360556645,338.17144664516));
#54884=CARTESIAN_POINT('Ctrl Pts',(120.88879569117,-3.67037702928781,338.273761678158));
#54885=CARTESIAN_POINT('Ctrl Pts',(120.881043717647,-3.57918667822284,338.375999715849));
#54886=CARTESIAN_POINT('Ctrl Pts',(120.873291744124,-3.48365041941673,338.474504230006));
#54887=CARTESIAN_POINT('Ctrl Pts',(120.865539770601,-3.38411084731969,338.568890140583));
#54888=CARTESIAN_POINT('Ctrl Pts',(120.857791080044,-3.28461343029036,338.663236078672));
#54889=CARTESIAN_POINT('Ctrl Pts',(120.850042389486,-3.18111635505688,338.753466613945));
#54890=CARTESIAN_POINT('Ctrl Pts',(120.842293698929,-3.07399970514535,338.839232849837));
#54891=CARTESIAN_POINT('Ctrl Pts',(120.834546620551,-2.96690534174746,338.924981241347));
#54892=CARTESIAN_POINT('Ctrl Pts',(120.826799542173,-2.85619320653498,339.006266936845));
#54893=CARTESIAN_POINT('Ctrl Pts',(120.819052463795,-2.74227684758727,339.082781007314));
#54894=CARTESIAN_POINT('Ctrl Pts',(120.811305320489,-2.62835953391086,339.159295719045));
#54895=CARTESIAN_POINT('Ctrl Pts',(120.803558177183,-2.51123826741195,339.231038508042));
#54896=CARTESIAN_POINT('Ctrl Pts',(120.795811033878,-2.39135564874566,339.297743736394));
#54897=CARTESIAN_POINT('Ctrl Pts',(120.788062148849,-2.27144607792167,339.364463961497));
#54898=CARTESIAN_POINT('Ctrl Pts',(120.780313263821,-2.14877426107984,339.426144182292));
#54899=CARTESIAN_POINT('Ctrl Pts',(120.772564378793,-2.02380710405849,339.482564876057));
#54900=CARTESIAN_POINT('Ctrl Pts',(120.764807269019,-1.89870730560532,339.53904545533));
#54901=CARTESIAN_POINT('Ctrl Pts',(120.757050159244,-1.77130765705046,339.590255194877));
#54902=CARTESIAN_POINT('Ctrl Pts',(120.749293049469,-1.64209525323747,339.636022674858));
#54903=CARTESIAN_POINT('Ctrl Pts',(120.741531794543,-1.51281380244726,339.681814611516));
#54904=CARTESIAN_POINT('Ctrl Pts',(120.733770539617,-1.38171803961448,339.722158378908));
#54905=CARTESIAN_POINT('Ctrl Pts',(120.726009284691,-1.24930894073323,339.756932859848));
#54906=CARTESIAN_POINT('Ctrl Pts',(120.718235614286,-1.11668803044583,339.791762968625));
#54907=CARTESIAN_POINT('Ctrl Pts',(120.710461943881,-0.982749967949554,
339.821005904622));
#54908=CARTESIAN_POINT('Ctrl Pts',(120.702688273476,-0.848005488581748,
339.844591804666));
#54909=CARTESIAN_POINT('Ctrl Pts',(120.695276469299,-0.719533397145381,
339.867079775389));
#54910=CARTESIAN_POINT('Ctrl Pts',(120.687864665122,-0.590328561915231,
339.884425489532));
#54911=CARTESIAN_POINT('Ctrl Pts',(120.680452860945,-0.460834980762146,
339.896612521224));
#54912=CARTESIAN_POINT('Ctrl Pts',(120.672677782167,-0.3249945334561,339.909396875642));
#54913=CARTESIAN_POINT('Ctrl Pts',(120.664902703388,-0.188407039038985,
339.916544477495));
#54914=CARTESIAN_POINT('Ctrl Pts',(120.65712762461,-0.0515798133325195,
339.917979522665));
#54915=CARTESIAN_POINT('Ctrl Pts',(120.649362113561,0.0850790377618662,
339.919412801921));
#54916=CARTESIAN_POINT('Ctrl Pts',(120.641596602512,0.22197664605461,339.915147507451));
#54917=CARTESIAN_POINT('Ctrl Pts',(120.633831091463,0.35859958683003,339.905159467217));
#54918=CARTESIAN_POINT('Ctrl Pts',(120.62607327994,0.495087065561858,339.895181330153));
#54919=CARTESIAN_POINT('Ctrl Pts',(120.618315468418,0.63130003141299,339.87949176746));
#54920=CARTESIAN_POINT('Ctrl Pts',(120.610557656896,0.766724421070416,339.858118640445));
#54921=CARTESIAN_POINT('Ctrl Pts',(120.602805683373,0.902046899580025,339.836761597385));
#54922=CARTESIAN_POINT('Ctrl Pts',(120.59505370985,1.03658159854575,339.809729563976));
#54923=CARTESIAN_POINT('Ctrl Pts',(120.587301736327,1.16981929842708,339.777102246292));
#54924=CARTESIAN_POINT('Ctrl Pts',(120.579553045769,1.3030005720634,339.744488746296));
#54925=CARTESIAN_POINT('Ctrl Pts',(120.571804355212,1.43488556022777,339.706284767782));
#54926=CARTESIAN_POINT('Ctrl Pts',(120.564055664654,1.56497518335109,339.662621123145));
#54927=CARTESIAN_POINT('Ctrl Pts',(120.556308586276,1.69503774024178,339.618966563093));
#54928=CARTESIAN_POINT('Ctrl Pts',(120.548561507898,1.82330530476455,339.569854720659));
#54929=CARTESIAN_POINT('Ctrl Pts',(120.540814429521,1.94929429732398,339.515466178029));
#54930=CARTESIAN_POINT('Ctrl Pts',(120.533067286215,2.07528434579248,339.461077179569));
#54931=CARTESIAN_POINT('Ctrl Pts',(120.525320142909,2.19899542534465,339.401411547624));
#54932=CARTESIAN_POINT('Ctrl Pts',(120.517572999603,2.31996463878292,339.336697722611));
#54933=CARTESIAN_POINT('Ctrl Pts',(120.509824114575,2.44096104866867,339.271969348555));
#54934=CARTESIAN_POINT('Ctrl Pts',(120.502075229547,2.55921402122576,339.202190707367));
#54935=CARTESIAN_POINT('Ctrl Pts',(120.494326344519,2.67428628557384,339.127635633785));
#54936=CARTESIAN_POINT('Ctrl Pts',(120.486569234744,2.78948068881218,339.053001426678));
#54937=CARTESIAN_POINT('Ctrl Pts',(120.478812124969,2.90148731133285,338.973580872739));
#54938=CARTESIAN_POINT('Ctrl Pts',(120.471055015195,3.00989840756412,338.889690815302));
#54939=CARTESIAN_POINT('Ctrl Pts',(120.463293760269,3.1183674352189,338.8057559297));
#54940=CARTESIAN_POINT('Ctrl Pts',(120.455532505342,3.22323680945756,338.717347033389));
#54941=CARTESIAN_POINT('Ctrl Pts',(120.447771250416,3.32413357339789,338.624819864312));
#54942=CARTESIAN_POINT('Ctrl Pts',(120.439997580012,3.42519173927832,338.532144681918));
#54943=CARTESIAN_POINT('Ctrl Pts',(120.432223909607,3.52226431900991,338.435338338349));
#54944=CARTESIAN_POINT('Ctrl Pts',(120.424450239202,3.61501617496263,338.334792514874));
#54945=CARTESIAN_POINT('Ctrl Pts',(120.417038435025,3.70345040970563,338.238927123672));
#54946=CARTESIAN_POINT('Ctrl Pts',(120.409626630848,3.78795694089722,338.139662782483));
#54947=CARTESIAN_POINT('Ctrl Pts',(120.402214826671,3.86828168294719,338.037363969608));
#54948=CARTESIAN_POINT('Ctrl Pts',(120.394439747893,3.95254337988039,337.930051187182));
#54949=CARTESIAN_POINT('Ctrl Pts',(120.386664669114,4.0324692813839,337.819059826652));
#54950=CARTESIAN_POINT('Ctrl Pts',(120.378889590336,4.10772110445711,337.704775478759));
#54951=CARTESIAN_POINT('Ctrl Pts',(120.371124079287,4.18288032537127,337.590631765032));
#54952=CARTESIAN_POINT('Ctrl Pts',(120.363358568238,4.25337669928546,337.473203450056));
#54953=CARTESIAN_POINT('Ctrl Pts',(120.355593057189,4.31891205584332,337.352909202751));
#54954=CARTESIAN_POINT('Ctrl Pts',(120.347835245667,4.38438243390441,337.232734227543));
#54955=CARTESIAN_POINT('Ctrl Pts',(120.340077434145,4.44490139763382,337.109699315942));
#54956=CARTESIAN_POINT('Ctrl Pts',(120.332319622622,4.50021418704429,336.984251832108));
#54957=CARTESIAN_POINT('Ctrl Pts',(120.324567649099,4.55548535182662,336.858898751485));
#54958=CARTESIAN_POINT('Ctrl Pts',(120.316815675576,4.60555798343984,336.731137068577));
#54959=CARTESIAN_POINT('Ctrl Pts',(120.309063702053,4.65022354050941,336.601438130491));
#54960=CARTESIAN_POINT('Ctrl Pts',(120.301315011496,4.69487018168905,336.471794119983));
#54961=CARTESIAN_POINT('Ctrl Pts',(120.293566320938,4.73411417576512,336.340214854875));
#54962=CARTESIAN_POINT('Ctrl Pts',(120.285817630381,4.76779544507966,336.207190811917));
#54963=CARTESIAN_POINT('Ctrl Pts',(120.278070552003,4.8014697067248,336.074194445723));
#54964=CARTESIAN_POINT('Ctrl Pts',(120.270323473625,4.82958344982151,335.93975427827));
#54965=CARTESIAN_POINT('Ctrl Pts',(120.262576395247,4.85202683711541,335.804374685338));
#54966=CARTESIAN_POINT('Ctrl Pts',(120.254829251941,4.8744704125065,335.668993957794));
#54967=CARTESIAN_POINT('Ctrl Pts',(120.247082108636,4.89124347337942,335.53267417468));
#54968=CARTESIAN_POINT('Ctrl Pts',(120.23933496533,4.90228761992001,335.395928218341));
#54969=CARTESIAN_POINT('Ctrl Pts',(120.231586080302,4.91333424941921,335.259151518609));
#54970=CARTESIAN_POINT('Ctrl Pts',(120.223837195274,4.91864937018671,335.121948844524));
#54971=CARTESIAN_POINT('Ctrl Pts',(120.216088310246,4.91822662333291,334.984836094191));
#54972=CARTESIAN_POINT('Ctrl Pts',(120.208331200471,4.91780342777122,334.847577810967));
#54973=CARTESIAN_POINT('Ctrl Pts',(120.200574090696,4.91163019998556,334.710410033646));
#54974=CARTESIAN_POINT('Ctrl Pts',(120.192816980921,4.89975272576887,334.573847106286));
#54975=CARTESIAN_POINT('Ctrl Pts',(120.185055725995,4.88786890460974,334.437211204065));
#54976=CARTESIAN_POINT('Ctrl Pts',(120.177294471069,4.87027481338499,334.301181183282));
#54977=CARTESIAN_POINT('Ctrl Pts',(120.169533216143,4.84706777135025,334.166263181551));
#54978=CARTESIAN_POINT('Ctrl Pts',(120.161759545738,4.82382360561142,334.031129354987));
#54979=CARTESIAN_POINT('Ctrl Pts',(120.153985875334,4.79494862894768,333.897111484485));
#54980=CARTESIAN_POINT('Ctrl Pts',(120.146212204929,4.76059085229275,333.76470335564));
#54981=CARTESIAN_POINT('Ctrl Pts',(120.138800400752,4.72783243840713,333.638458857048));
#54982=CARTESIAN_POINT('Ctrl Pts',(120.131388596575,4.69009026920121,333.513677881297));
#54983=CARTESIAN_POINT('Ctrl Pts',(120.123976792398,4.64753334196125,333.390771334503));
#54984=CARTESIAN_POINT('Ctrl Pts',(120.116201713619,4.60289057294669,333.26184077173));
#54985=CARTESIAN_POINT('Ctrl Pts',(120.108426634841,4.55280806143128,333.134565582146));
#54986=CARTESIAN_POINT('Ctrl Pts',(120.100651556063,4.49742699455212,333.009438900417));
#54987=CARTESIAN_POINT('Ctrl Pts',(120.092886045014,4.44211407760149,332.884466195036));
#54988=CARTESIAN_POINT('Ctrl Pts',(120.085120533965,4.38151573532091,332.761637090968));
#54989=CARTESIAN_POINT('Ctrl Pts',(120.077355022916,4.31582267824842,332.641428891804));
#54990=CARTESIAN_POINT('Ctrl Pts',(120.069597211393,4.25019475603324,332.521339879419));
#54991=CARTESIAN_POINT('Ctrl Pts',(120.061839399871,4.17948235788482,332.403866941295));
#54992=CARTESIAN_POINT('Ctrl Pts',(120.054081588349,4.10392381662172,332.289466404955));
#54993=CARTESIAN_POINT('Ctrl Pts',(120.046329614826,4.02842213555707,332.175151958648));
#54994=CARTESIAN_POINT('Ctrl Pts',(120.038577641303,3.94808178485716,332.063905636886));
#54995=CARTESIAN_POINT('Ctrl Pts',(120.03082566778,3.86318627665475,331.956157879527));
#54996=CARTESIAN_POINT('Ctrl Pts',(120.023076977222,3.77832672175049,331.848455753407));
#54997=CARTESIAN_POINT('Ctrl Pts',(120.015328286665,3.68891608761505,331.744249551188));
#54998=CARTESIAN_POINT('Ctrl Pts',(120.007579596107,3.59528019940558,331.6439393107));
#54999=CARTESIAN_POINT('Ctrl Pts',(119.999832517729,3.50166379292471,331.543649940597));
#55000=CARTESIAN_POINT('Ctrl Pts',(119.992085439351,3.40382414751369,331.447255205462));
#55001=CARTESIAN_POINT('Ctrl Pts',(119.984338360974,3.3021259642863,331.355120416463));
#55002=CARTESIAN_POINT('Ctrl Pts',(119.976591217668,3.20042692873025,331.262984855286));
#55003=CARTESIAN_POINT('Ctrl Pts',(119.968844074362,3.09486958053087,331.175109573889));
#55004=CARTESIAN_POINT('Ctrl Pts',(119.961096931056,2.98585360990486,331.091821231991));
#55005=CARTESIAN_POINT('Ctrl Pts',(119.953348046028,2.87681313017418,331.008514165105));
#55006=CARTESIAN_POINT('Ctrl Pts',(119.945599161,2.76431279127489,330.929796327023));
#55007=CARTESIAN_POINT('Ctrl Pts',(119.937850275972,2.64878298176728,330.855952247138));
#55008=CARTESIAN_POINT('Ctrl Pts',(119.930093166197,2.53313054772618,330.782029788383));
#55009=CARTESIAN_POINT('Ctrl Pts',(119.922336056422,2.41444254965641,330.712991632335));
#55010=CARTESIAN_POINT('Ctrl Pts',(119.914578946648,2.29317628776919,330.649077617825));
#55011=CARTESIAN_POINT('Ctrl Pts',(119.906817691722,2.17184522506901,330.585129449709));
#55012=CARTESIAN_POINT('Ctrl Pts',(119.899056436795,2.04793350620948,330.526311046727));
#55013=CARTESIAN_POINT('Ctrl Pts',(119.891295181869,1.92191941813962,330.472814471145));
#55014=CARTESIAN_POINT('Ctrl Pts',(119.883521511465,1.79570374859674,330.419232318476));
#55015=CARTESIAN_POINT('Ctrl Pts',(119.87574784106,1.66737935542803,330.370989142701));
#55016=CARTESIAN_POINT('Ctrl Pts',(119.867974170655,1.53744157068174,330.328227693986));
#55017=CARTESIAN_POINT('Ctrl Pts',(119.860562366478,1.4135524210764,330.287456800996));
#55018=CARTESIAN_POINT('Ctrl Pts',(119.853150562301,1.28819698307923,330.251668850366));
#55019=CARTESIAN_POINT('Ctrl Pts',(119.845738758124,1.16181225053775,330.220944093547));
#55020=CARTESIAN_POINT('Ctrl Pts',(119.837963679345,1.02923302577381,330.188713424873));
#55021=CARTESIAN_POINT('Ctrl Pts',(119.830188600567,0.895102082840413,330.161952969137));
#55022=CARTESIAN_POINT('Ctrl Pts',(119.822413521789,0.759910513660583,330.140810862528));
#55023=CARTESIAN_POINT('Ctrl Pts',(119.81464801074,0.624885306313346,330.119694772627));
#55024=CARTESIAN_POINT('Ctrl Pts',(119.806882499691,0.488802452118738,330.104183335316));
#55025=CARTESIAN_POINT('Ctrl Pts',(119.799116988641,0.35216653026329,330.094374474396));
#55026=CARTESIAN_POINT('Ctrl Pts',(119.791359177119,0.215666083322119,330.084575338989));
#55027=CARTESIAN_POINT('Ctrl Pts',(119.783601365597,0.0786140473633463,
330.08046755576));
#55028=CARTESIAN_POINT('Ctrl Pts',(119.775843554075,-0.0584768664984696,
330.082097650564));
#55029=CARTESIAN_POINT('Ctrl Pts',(119.768091580552,-0.195464615099969,
330.083726518671));
#55030=CARTESIAN_POINT('Ctrl Pts',(119.760339607029,-0.33249079409725,330.091084665543));
#55031=CARTESIAN_POINT('Ctrl Pts',(119.752587633506,-0.469040012749843,
330.104166615484));
#55032=CARTESIAN_POINT('Ctrl Pts',(119.744838942948,-0.605531402727407,
330.117243025212));
#55033=CARTESIAN_POINT('Ctrl Pts',(119.737090252391,-0.741545845827129,
330.136038379577));
#55034=CARTESIAN_POINT('Ctrl Pts',(119.729341561833,-0.876570619014289,
330.160495168679));
#55035=CARTESIAN_POINT('Ctrl Pts',(119.721594483455,-1.01156729916968,330.184946869341));
#55036=CARTESIAN_POINT('Ctrl Pts',(119.713847405077,-1.14557433460566,330.215057592174));
#55037=CARTESIAN_POINT('Ctrl Pts',(119.706100326699,-1.2780871666694,330.250718343065));
#55038=CARTESIAN_POINT('Ctrl Pts',(119.698353183394,-1.41060110931822,330.286379392828));
#55039=CARTESIAN_POINT('Ctrl Pts',(119.690606040088,-1.54162044617135,330.32759046185));
#55040=CARTESIAN_POINT('Ctrl Pts',(119.682858896782,-1.67065418679368,330.374192216418));
#55041=CARTESIAN_POINT('Ctrl Pts',(119.675110011754,-1.79971693694032,330.42080444805));
#55042=CARTESIAN_POINT('Ctrl Pts',(119.667361126726,-1.92679283500087,330.472809644105));
#55043=CARTESIAN_POINT('Ctrl Pts',(119.659612241698,-2.05140970619441,330.529999856842));
#55044=CARTESIAN_POINT('Ctrl Pts',(119.651855131923,-2.17615884702256,330.587250771862));
#55045=CARTESIAN_POINT('Ctrl Pts',(119.644098022148,-2.29844339137983,330.64969753389));
#55046=CARTESIAN_POINT('Ctrl Pts',(119.636340912373,-2.4178141822908,330.717085379976));
#55047=CARTESIAN_POINT('Ctrl Pts',(119.628579657447,-2.53724876113577,330.784509235973));
#55048=CARTESIAN_POINT('Ctrl Pts',(119.620818402521,-2.6537661521668,330.85687923105));
#55049=CARTESIAN_POINT('Ctrl Pts',(119.613057147595,-2.76694601761512,330.93389709942));
#55050=CARTESIAN_POINT('Ctrl Pts',(119.60528347719,-2.88030693396285,331.01103817128));
#55051=CARTESIAN_POINT('Ctrl Pts',(119.597509806786,-2.9903193420906,331.092841740572));
#55052=CARTESIAN_POINT('Ctrl Pts',(119.589736136381,-3.09659514774521,331.178968522315));
#55053=CARTESIAN_POINT('Ctrl Pts',(119.582324332204,-3.1979237890775,331.261086081647));
#55054=CARTESIAN_POINT('Ctrl Pts',(119.574912528027,-3.29585566065839,331.3471332302));
#55055=CARTESIAN_POINT('Ctrl Pts',(119.56750072385,-3.39008679488294,331.436785919193));
#55056=CARTESIAN_POINT('Ctrl Pts',(119.559839911898,-3.48748372848824,331.529450589625));
#55057=CARTESIAN_POINT('Ctrl Pts',(119.552179099946,-3.58125425540994,331.62627909888));
#55058=CARTESIAN_POINT('Ctrl Pts',(119.544518287994,-3.6710133393594,331.726951860307));
#55059=CARTESIAN_POINT('Ctrl Pts',(119.536867029122,-3.76066049316255,331.827499082163));
#55060=CARTESIAN_POINT('Ctrl Pts',(119.529215770251,-3.84630588625596,331.931880724812));
#55061=CARTESIAN_POINT('Ctrl Pts',(119.52156451138,-3.9275989146357,332.039738216263));
#55062=CARTESIAN_POINT('Ctrl Pts',(119.513921918135,-4.00879987255432,332.147473551003));
#55063=CARTESIAN_POINT('Ctrl Pts',(119.506279324889,-4.0856580361039,332.258676578967));
#55064=CARTESIAN_POINT('Ctrl Pts',(119.498636731643,-4.1578614217354,332.372953852681));
#55065=CARTESIAN_POINT('Ctrl Pts',(119.490998992335,-4.23001894980219,332.487158547008));
#55066=CARTESIAN_POINT('Ctrl Pts',(119.483361253027,-4.29752736264881,332.604433265854));
#55067=CARTESIAN_POINT('Ctrl Pts',(119.475723513719,-4.36011666172829,332.724353771207));
#55068=CARTESIAN_POINT('Ctrl Pts',(119.468088858547,-4.42268068710995,332.844225852394));
#55069=CARTESIAN_POINT('Ctrl Pts',(119.460454203374,-4.48032936256405,332.966741238522));
#55070=CARTESIAN_POINT('Ctrl Pts',(119.452819548202,-4.53283781220414,333.091449652026));
#55071=CARTESIAN_POINT('Ctrl Pts',(119.44518621024,-4.58533720254364,333.216136549545));
#55072=CARTESIAN_POINT('Ctrl Pts',(119.437552872277,-4.63269797568408,333.343015349837));
#55073=CARTESIAN_POINT('Ctrl Pts',(119.429919534315,-4.67474296352263,333.471614810496));
#55074=CARTESIAN_POINT('Ctrl Pts',(119.42228264376,-4.7168075193005,333.600274121962));
#55075=CARTESIAN_POINT('Ctrl Pts',(119.414645753205,-4.75355121777498,333.730655311085));
#55076=CARTESIAN_POINT('Ctrl Pts',(119.407008862651,-4.78484645242896,333.862270906948));
#55077=CARTESIAN_POINT('Ctrl Pts',(119.399370303069,-4.81614852659181,333.993915267126));
#55078=CARTESIAN_POINT('Ctrl Pts',(119.391731743488,-4.84199968370608,334.126794176089));
#55079=CARTESIAN_POINT('Ctrl Pts',(119.384093183906,-4.8623235094944,334.26041014642));
#55080=CARTESIAN_POINT('Ctrl Pts',(119.376446474425,-4.88266901962485,334.394168677235));
#55081=CARTESIAN_POINT('Ctrl Pts',(119.368799764944,-4.89747536912074,334.52866543954));
#55082=CARTESIAN_POINT('Ctrl Pts',(119.361153055464,-4.90671803989672,334.663397653823));
#55083=CARTESIAN_POINT('Ctrl Pts',(119.354707829157,-4.91450846334283,334.77696017558));
#55084=CARTESIAN_POINT('Ctrl Pts',(119.348262602851,-4.91834713849611,334.890689783422));
#55085=CARTESIAN_POINT('Ctrl Pts',(119.341817376544,-4.91824813200487,335.004286552297));
#55086=CARTESIAN_POINT('',(117.59181737647,-4.91824919068085,334.99717849913));
#55087=CARTESIAN_POINT('Ctrl Pts',(119.341817376508,-4.91824813200431,335.00428655294));
#55088=CARTESIAN_POINT('Ctrl Pts',(119.330327476319,-4.91807163317883,335.206795429156));
#55089=CARTESIAN_POINT('Ctrl Pts',(119.318837576129,-4.90538450625377,335.408779786107));
#55090=CARTESIAN_POINT('Ctrl Pts',(119.30734767594,-4.88039897662853,335.609006478966));
#55091=CARTESIAN_POINT('Ctrl Pts',(119.301319347152,-4.86728998655602,335.714058073562));
#55092=CARTESIAN_POINT('Ctrl Pts',(119.295291018364,-4.85079630954624,335.818626478205));
#55093=CARTESIAN_POINT('Ctrl Pts',(119.289262689576,-4.83095322623972,335.922536713841));
#55094=CARTESIAN_POINT('Ctrl Pts',(119.281487610798,-4.80536047220388,336.056555659453));
#55095=CARTESIAN_POINT('Ctrl Pts',(119.273712532019,-4.7741461771936,336.18972059339));
#55096=CARTESIAN_POINT('Ctrl Pts',(119.265937453241,-4.73737897440254,336.321523180042));
#55097=CARTESIAN_POINT('Ctrl Pts',(119.258171942192,-4.70065701599525,336.45316357522));
#55098=CARTESIAN_POINT('Ctrl Pts',(119.250406431143,-4.65839584995196,336.583444585877));
#55099=CARTESIAN_POINT('Ctrl Pts',(119.242640920094,-4.61071539758645,336.711866403946));
#55100=CARTESIAN_POINT('Ctrl Pts',(119.234883108572,-4.56308222052834,336.840160891408));
#55101=CARTESIAN_POINT('Ctrl Pts',(119.227125297049,-4.51004058536871,336.966599490669));
#55102=CARTESIAN_POINT('Ctrl Pts',(119.219367485527,-4.4517605618634,337.090696286489));
#55103=CARTESIAN_POINT('Ctrl Pts',(119.211615512004,-4.39352439592375,337.214699695535));
#55104=CARTESIAN_POINT('Ctrl Pts',(119.203863538481,-4.33005785359038,337.336364456498));
#55105=CARTESIAN_POINT('Ctrl Pts',(119.196111564958,-4.26157944355582,337.455223759408));
#55106=CARTESIAN_POINT('Ctrl Pts',(119.1883628744,-4.19313003416872,337.574032725332));
#55107=CARTESIAN_POINT('Ctrl Pts',(119.180614183843,-4.11967317336198,337.690038258295));
#55108=CARTESIAN_POINT('Ctrl Pts',(119.172865493285,-4.04147362309771,337.802797533948));
#55109=CARTESIAN_POINT('Ctrl Pts',(119.165118414907,-3.96329034290301,337.915533349092));
#55110=CARTESIAN_POINT('Ctrl Pts',(119.15737133653,-3.88036655858897,338.025023929376));
#55111=CARTESIAN_POINT('Ctrl Pts',(119.149624258152,-3.79301050755723,338.13085521097));
#55112=CARTESIAN_POINT('Ctrl Pts',(119.141877114846,-3.70565372439767,338.236687379532));
#55113=CARTESIAN_POINT('Ctrl Pts',(119.13412997154,-3.61386484925101,338.338859886787));
#55114=CARTESIAN_POINT('Ctrl Pts',(119.126382828234,-3.517992314405,338.436991873468));
#55115=CARTESIAN_POINT('Ctrl Pts',(119.118633943206,-3.42209822537779,338.535145922304));
#55116=CARTESIAN_POINT('Ctrl Pts',(119.110885058178,-3.32211892284697,338.629257363426));
#55117=CARTESIAN_POINT('Ctrl Pts',(119.10313617315,-3.21843928947237,338.718982603143));
#55118=CARTESIAN_POINT('Ctrl Pts',(119.095379063375,-3.11464960946366,338.808803078157));
#55119=CARTESIAN_POINT('Ctrl Pts',(119.0876219536,-3.00715204895311,338.894227795661));
#55120=CARTESIAN_POINT('Ctrl Pts',(119.079864843826,-2.89636456285004,338.974953506843));
#55121=CARTESIAN_POINT('Ctrl Pts',(119.0721035889,-2.7855178754567,339.055722355265));
#55122=CARTESIAN_POINT('Ctrl Pts',(119.064342333973,-2.67137808453528,339.131786977321));
#55123=CARTESIAN_POINT('Ctrl Pts',(119.056581079047,-2.55439079901421,339.202888376868));
#55124=CARTESIAN_POINT('Ctrl Pts',(119.048807408643,-2.43721637196238,339.274103515483));
#55125=CARTESIAN_POINT('Ctrl Pts',(119.041033738238,-2.31718569035163,339.340339377091));
#55126=CARTESIAN_POINT('Ctrl Pts',(119.033260067833,-2.19476833798042,339.401383305859));
#55127=CARTESIAN_POINT('Ctrl Pts',(119.025848263656,-2.07804954281425,339.459585625057));
#55128=CARTESIAN_POINT('Ctrl Pts',(119.018436459479,-1.95916153794591,339.513068384374));
#55129=CARTESIAN_POINT('Ctrl Pts',(119.011024655302,-1.83852518662641,339.561689182818));
#55130=CARTESIAN_POINT('Ctrl Pts',(119.003249576524,-1.71197608837132,339.612693031428));
#55131=CARTESIAN_POINT('Ctrl Pts',(118.995474497745,-1.58310300836854,339.658507451582));
#55132=CARTESIAN_POINT('Ctrl Pts',(118.987699418967,-1.45237055823626,339.698915068829));
#55133=CARTESIAN_POINT('Ctrl Pts',(118.979933907918,-1.32179898270666,339.739272961931));
#55134=CARTESIAN_POINT('Ctrl Pts',(118.972168396869,-1.18937295953024,339.774237176192));
#55135=CARTESIAN_POINT('Ctrl Pts',(118.96440288582,-1.05557768427809,339.803638081179));
#55136=CARTESIAN_POINT('Ctrl Pts',(118.956645074297,-0.921915067430979,
339.833009835083));
#55137=CARTESIAN_POINT('Ctrl Pts',(118.948887262775,-0.786886279549922,
339.856829173589));
#55138=CARTESIAN_POINT('Ctrl Pts',(118.941129451253,-0.650991971630229,
339.874976155365));
#55139=CARTESIAN_POINT('Ctrl Pts',(118.93337747773,-0.515199928486656,339.893109480961));
#55140=CARTESIAN_POINT('Ctrl Pts',(118.925625504207,-0.378544047622639,
339.905578894793));
#55141=CARTESIAN_POINT('Ctrl Pts',(118.917873530684,-0.241535127094092,
339.912315527822));
#55142=CARTESIAN_POINT('Ctrl Pts',(118.910124840126,-0.104584229924731,
339.919049307883));
#55143=CARTESIAN_POINT('Ctrl Pts',(118.902376149569,0.0327190199491614,
339.920055116779));
#55144=CARTESIAN_POINT('Ctrl Pts',(118.894627459011,0.169858964197006,339.915315960829));
#55145=CARTESIAN_POINT('Ctrl Pts',(118.886880380633,0.306970375333988,339.910577790901));
#55146=CARTESIAN_POINT('Ctrl Pts',(118.879133302255,0.443918158031927,339.900097047129));
#55147=CARTESIAN_POINT('Ctrl Pts',(118.871386223877,0.580187312238033,339.883908859225));
#55148=CARTESIAN_POINT('Ctrl Pts',(118.863639080572,0.716457608510856,339.867720535648));
#55149=CARTESIAN_POINT('Ctrl Pts',(118.855891937266,0.852048876802527,339.84582471864));
#55150=CARTESIAN_POINT('Ctrl Pts',(118.84814479396,0.986452287726923,339.818308307543));
#55151=CARTESIAN_POINT('Ctrl Pts',(118.840395908932,1.12088591539142,339.790785710172));
#55152=CARTESIAN_POINT('Ctrl Pts',(118.832647023904,1.25413077142126,339.757640082614));
#55153=CARTESIAN_POINT('Ctrl Pts',(118.824898138876,1.38568963845844,339.719009142645));
#55154=CARTESIAN_POINT('Ctrl Pts',(118.817141029101,1.51738814343649,339.680337199398));
#55155=CARTESIAN_POINT('Ctrl Pts',(118.809383919326,1.6473967090434,339.636168423715));
#55156=CARTESIAN_POINT('Ctrl Pts',(118.801626809552,1.775234147499,339.586690177465));
#55157=CARTESIAN_POINT('Ctrl Pts',(118.793865554625,1.90313989819427,339.537185491622));
#55158=CARTESIAN_POINT('Ctrl Pts',(118.786104299699,2.0288718518561,339.482365837952));
#55159=CARTESIAN_POINT('Ctrl Pts',(118.778343044773,2.15197106854176,339.422465780835));
#55160=CARTESIAN_POINT('Ctrl Pts',(118.770569374368,2.27526720385618,339.362469903149));
#55161=CARTESIAN_POINT('Ctrl Pts',(118.762795703964,2.39592184214174,339.297377567569));
#55162=CARTESIAN_POINT('Ctrl Pts',(118.755022033559,2.51350203783212,339.227468576857));
#55163=CARTESIAN_POINT('Ctrl Pts',(118.747610229382,2.62560884712367,339.160813866482));
#55164=CARTESIAN_POINT('Ctrl Pts',(118.740198425205,2.73492076166339,339.089780996731));
#55165=CARTESIAN_POINT('Ctrl Pts',(118.732786621028,2.8410902801649,339.014646819143));
#55166=CARTESIAN_POINT('Ctrl Pts',(118.72501154225,2.95246348303192,338.935830091697));
#55167=CARTESIAN_POINT('Ctrl Pts',(118.717236463471,3.06073042467197,338.852250780912));
#55168=CARTESIAN_POINT('Ctrl Pts',(118.709461384693,3.16545688226668,338.764181954822));
#55169=CARTESIAN_POINT('Ctrl Pts',(118.701695873644,3.2700544672881,338.67622150303));
#55170=CARTESIAN_POINT('Ctrl Pts',(118.693930362595,3.3711199407333,338.583782777539));
#55171=CARTESIAN_POINT('Ctrl Pts',(118.686164851546,3.46824808958798,338.487181992895));
#55172=CARTESIAN_POINT('Ctrl Pts',(118.678407040023,3.5652799356003,338.39067698821));
#55173=CARTESIAN_POINT('Ctrl Pts',(118.670649228501,3.65838195058581,338.290018410587));
#55174=CARTESIAN_POINT('Ctrl Pts',(118.662891416979,3.74718234233851,338.185562360992));
#55175=CARTESIAN_POINT('Ctrl Pts',(118.655139443456,3.83591590898038,338.081184917886));
#55176=CARTESIAN_POINT('Ctrl Pts',(118.647387469933,3.92035404354363,337.973015987562));
#55177=CARTESIAN_POINT('Ctrl Pts',(118.63963549641,4.00016241044551,337.861447842013));
#55178=CARTESIAN_POINT('Ctrl Pts',(118.631886805852,4.07993697845662,337.749926945639));
#55179=CARTESIAN_POINT('Ctrl Pts',(118.624138115295,4.15508545158094,337.635010014491));
#55180=CARTESIAN_POINT('Ctrl Pts',(118.616389424737,4.2253144871583,337.517121480404));
#55181=CARTESIAN_POINT('Ctrl Pts',(118.608642346359,4.29552891099824,337.399257474011));
#55182=CARTESIAN_POINT('Ctrl Pts',(118.600895267982,4.36082573324415,337.278423430048));
#55183=CARTESIAN_POINT('Ctrl Pts',(118.593148189604,4.42095579913912,337.155071433748));
#55184=CARTESIAN_POINT('Ctrl Pts',(118.585401046298,4.48108636898191,337.03171840364));
#55185=CARTESIAN_POINT('Ctrl Pts',(118.577653902992,4.53604992483119,336.905847730457));
#55186=CARTESIAN_POINT('Ctrl Pts',(118.569906759686,4.58564418541981,336.777934325903));
#55187=CARTESIAN_POINT('Ctrl Pts',(118.562157874658,4.63524959585112,336.649992163701));
#55188=CARTESIAN_POINT('Ctrl Pts',(118.55440898963,4.6794831676924,336.520006720644));
#55189=CARTESIAN_POINT('Ctrl Pts',(118.546660104602,4.71819163791801,336.388470644407));
#55190=CARTESIAN_POINT('Ctrl Pts',(118.538902994827,4.75694119371387,336.25679495442));
#55191=CARTESIAN_POINT('Ctrl Pts',(118.531145885053,4.79015382268305,336.123565719065));
#55192=CARTESIAN_POINT('Ctrl Pts',(118.523388775278,4.81772668309809,335.989288971668));
#55193=CARTESIAN_POINT('Ctrl Pts',(118.515627520352,4.84531427756812,335.854940471071));
#55194=CARTESIAN_POINT('Ctrl Pts',(118.507866265426,4.86725603589562,335.719543728712));
#55195=CARTESIAN_POINT('Ctrl Pts',(118.500105010499,4.88350084953506,335.583611613224));
#55196=CARTESIAN_POINT('Ctrl Pts',(118.492331340095,4.89977164958214,335.447462050652));
#55197=CARTESIAN_POINT('Ctrl Pts',(118.48455766969,4.91032726384758,335.310775793485));
#55198=CARTESIAN_POINT('Ctrl Pts',(118.476783999286,4.9151686927531,335.174068332214));
#55199=CARTESIAN_POINT('Ctrl Pts',(118.469372195108,4.91978475197834,335.043724636154));
#55200=CARTESIAN_POINT('Ctrl Pts',(118.461960390931,4.91920664565874,334.91336195346));
#55201=CARTESIAN_POINT('Ctrl Pts',(118.454548586754,4.91347913127396,334.78342232563));
#55202=CARTESIAN_POINT('Ctrl Pts',(118.446773507976,4.90747089434785,334.647113969572));
#55203=CARTESIAN_POINT('Ctrl Pts',(118.438998429197,4.89577672329974,334.510840427728));
#55204=CARTESIAN_POINT('Ctrl Pts',(118.431223350419,4.87839126398238,334.37511462011));
#55205=CARTESIAN_POINT('Ctrl Pts',(118.42345783937,4.86102719857951,334.239555831739));
#55206=CARTESIAN_POINT('Ctrl Pts',(118.415692328321,4.83798582903697,334.104543820485));
#55207=CARTESIAN_POINT('Ctrl Pts',(118.407926817272,4.80931378289956,333.970590460452));
#55208=CARTESIAN_POINT('Ctrl Pts',(118.400169005749,4.78067016517937,333.836769915565));
#55209=CARTESIAN_POINT('Ctrl Pts',(118.392411194227,4.74640706230068,333.70400631278));
#55210=CARTESIAN_POINT('Ctrl Pts',(118.384653382705,4.70662272906663,333.572805006759));
#55211=CARTESIAN_POINT('Ctrl Pts',(118.376901409182,4.666868334805,333.441702433881));
#55212=CARTESIAN_POINT('Ctrl Pts',(118.369149435659,4.62160109328377,333.312160190188));
#55213=CARTESIAN_POINT('Ctrl Pts',(118.361397462136,4.57096994622283,333.184671706487));
#55214=CARTESIAN_POINT('Ctrl Pts',(118.353648771578,4.5203602414827,333.057237214235));
#55215=CARTESIAN_POINT('Ctrl Pts',(118.345900081021,4.46439129326101,332.931855114586));
#55216=CARTESIAN_POINT('Ctrl Pts',(118.338151390463,4.40326127079749,332.809001770061));
#55217=CARTESIAN_POINT('Ctrl Pts',(118.330404312085,4.34214396694569,332.6861739862));
#55218=CARTESIAN_POINT('Ctrl Pts',(118.322657233707,4.275867898744,332.565874260683));
#55219=CARTESIAN_POINT('Ctrl Pts',(118.31491015533,4.20467840237431,332.448556762319));
#55220=CARTESIAN_POINT('Ctrl Pts',(118.307163012024,4.13348830936811,332.331238280722));
#55221=CARTESIAN_POINT('Ctrl Pts',(118.299415868718,4.05738490883286,332.216902410295));
#55222=CARTESIAN_POINT('Ctrl Pts',(118.291668725412,3.97665809815358,332.105976255645));
#55223=CARTESIAN_POINT('Ctrl Pts',(118.283919840384,3.89591313837344,331.995025162441));
#55224=CARTESIAN_POINT('Ctrl Pts',(118.276170955356,3.81054293003373,331.887485626396));
#55225=CARTESIAN_POINT('Ctrl Pts',(118.268422070328,3.72087881165768,331.783753129585));
#55226=CARTESIAN_POINT('Ctrl Pts',(118.260664960553,3.63111952285988,331.679910530029));
#55227=CARTESIAN_POINT('Ctrl Pts',(118.252907850778,3.53705747580378,331.579883337826));
#55228=CARTESIAN_POINT('Ctrl Pts',(118.245150741004,3.43906255114998,331.484031878447));
#55229=CARTESIAN_POINT('Ctrl Pts',(118.237389486077,3.34101526114174,331.388129199113));
#55230=CARTESIAN_POINT('Ctrl Pts',(118.229628231151,3.23903119637746,331.296406960074));
#55231=CARTESIAN_POINT('Ctrl Pts',(118.221866976225,3.13351398126666,331.209185682244));
#55232=CARTESIAN_POINT('Ctrl Pts',(118.21409330582,3.02782797299966,331.121824878794));
#55233=CARTESIAN_POINT('Ctrl Pts',(118.206319635416,2.91859783183401,331.038979660755));
#55234=CARTESIAN_POINT('Ctrl Pts',(118.198545965011,2.80625758610726,330.960928148335));
#55235=CARTESIAN_POINT('Ctrl Pts',(118.191134160834,2.69914680584742,330.886509952596));
#55236=CARTESIAN_POINT('Ctrl Pts',(118.183722356657,2.5892091983047,330.81644936672));
#55237=CARTESIAN_POINT('Ctrl Pts',(118.17631055248,2.47684070644631,330.750947967206));
#55238=CARTESIAN_POINT('Ctrl Pts',(118.168535473702,2.35896470007272,330.682236148983));
#55239=CARTESIAN_POINT('Ctrl Pts',(118.160760394923,2.23804098450162,330.618324594035));
#55240=CARTESIAN_POINT('Ctrl Pts',(118.152985316145,2.1144979876788,330.55949537523));
#55241=CARTESIAN_POINT('Ctrl Pts',(118.145219805096,1.99110701837866,330.500738549524));
#55242=CARTESIAN_POINT('Ctrl Pts',(118.137454294047,1.86510353058753,330.447051782462));
#55243=CARTESIAN_POINT('Ctrl Pts',(118.129688782998,1.73694320299964,330.398672868394));
#55244=CARTESIAN_POINT('Ctrl Pts',(118.121930971475,1.60890994674965,330.35034192216));
#55245=CARTESIAN_POINT('Ctrl Pts',(118.114173159953,1.47872446979597,330.307308492901));
#55246=CARTESIAN_POINT('Ctrl Pts',(118.106415348431,1.34686490696827,330.269763432462));
#55247=CARTESIAN_POINT('Ctrl Pts',(118.098663374908,1.21510457264324,330.232246625871));
#55248=CARTESIAN_POINT('Ctrl Pts',(118.090911401385,1.08167303443826,330.200210073806));
#55249=CARTESIAN_POINT('Ctrl Pts',(118.083159427862,0.947065829757921,330.173795551719));
#55250=CARTESIAN_POINT('Ctrl Pts',(118.075410737304,0.812515631308635,330.147392216199));
#55251=CARTESIAN_POINT('Ctrl Pts',(118.067662046747,0.676791139423746,330.12660625026));
#55252=CARTESIAN_POINT('Ctrl Pts',(118.059913356189,0.540400178256569,330.111528796255));
#55253=CARTESIAN_POINT('Ctrl Pts',(118.052166277811,0.404037594368023,330.096454479241));
#55254=CARTESIAN_POINT('Ctrl Pts',(118.044419199434,0.26700920527441,330.087086354655));
#55255=CARTESIAN_POINT('Ctrl Pts',(118.036672121056,0.129829696703436,330.083463890873));
#55256=CARTESIAN_POINT('Ctrl Pts',(118.02892497775,-0.00735096156394813,
330.07984139673));
#55257=CARTESIAN_POINT('Ctrl Pts',(118.021177834444,-0.144682351096794,
330.081964669756));
#55258=CARTESIAN_POINT('Ctrl Pts',(118.013430691138,-0.281648430409271,
330.089821059865));
#55259=CARTESIAN_POINT('Ctrl Pts',(118.00568180611,-0.418645302604203,330.097679216257));
#55260=CARTESIAN_POINT('Ctrl Pts',(117.997932921082,-0.555276310993658,
330.111273032172));
#55261=CARTESIAN_POINT('Ctrl Pts',(117.990184036054,-0.691029579977796,
330.13053789602));
#55262=CARTESIAN_POINT('Ctrl Pts',(117.982426926279,-0.826926938884273,
330.149823207794));
#55263=CARTESIAN_POINT('Ctrl Pts',(117.974669816505,-0.961944309735628,
330.174791536629));
#55264=CARTESIAN_POINT('Ctrl Pts',(117.96691270673,-1.095578523506,330.205326834775));
#55265=CARTESIAN_POINT('Ctrl Pts',(117.959151451804,-1.22928414712742,330.235878450008));
#55266=CARTESIAN_POINT('Ctrl Pts',(117.951390196878,-1.36160476403147,330.272002859238));
#55267=CARTESIAN_POINT('Ctrl Pts',(117.943628941951,-1.49205241701669,330.313534098345));
#55268=CARTESIAN_POINT('Ctrl Pts',(117.935855271547,-1.62270874373381,330.3551317739));
#55269=CARTESIAN_POINT('Ctrl Pts',(117.928081601142,-1.75148575201679,330.40215342879));
#55270=CARTESIAN_POINT('Ctrl Pts',(117.920307930737,-1.87791468701139,330.454384586131));
#55271=CARTESIAN_POINT('Ctrl Pts',(117.91289612656,-1.9984583246656,330.504184370531));
#55272=CARTESIAN_POINT('Ctrl Pts',(117.905484322383,-2.11686731366726,330.558719447037));
#55273=CARTESIAN_POINT('Ctrl Pts',(117.898072518206,-2.2327578765785,330.617765943371));
#55274=CARTESIAN_POINT('Ctrl Pts',(117.890297439428,-2.35432858119775,330.679706484381));
#55275=CARTESIAN_POINT('Ctrl Pts',(117.882522360649,-2.47351193234357,330.746807606973));
#55276=CARTESIAN_POINT('Ctrl Pts',(117.874747281871,-2.58983888197942,330.818861682761));
#55277=CARTESIAN_POINT('Ctrl Pts',(117.866981770822,-2.706022683898,330.890827091421));
#55278=CARTESIAN_POINT('Ctrl Pts',(117.859216259773,-2.81935674900042,330.967733122267));
#55279=CARTESIAN_POINT('Ctrl Pts',(117.851450748724,-2.92939451705489,331.049325269533));
#55280=CARTESIAN_POINT('Ctrl Pts',(117.843692937201,-3.03932318234206,331.130836517948));
#55281=CARTESIAN_POINT('Ctrl Pts',(117.835935125679,-3.14596174270503,331.217024405074));
#55282=CARTESIAN_POINT('Ctrl Pts',(117.828177314157,-3.24889096056355,331.307590138017));
#55283=CARTESIAN_POINT('Ctrl Pts',(117.820425340634,-3.3517427209215,331.398087717375));
#55284=CARTESIAN_POINT('Ctrl Pts',(117.812673367111,-3.45089040264602,331.492956327909));
#55285=CARTESIAN_POINT('Ctrl Pts',(117.804921393588,-3.54594662000991,331.591855984478));
#55286=CARTESIAN_POINT('Ctrl Pts',(117.79717270303,-3.64096258100934,331.690713756983));
#55287=CARTESIAN_POINT('Ctrl Pts',(117.789424012473,-3.73189025364509,331.793598898897));
#55288=CARTESIAN_POINT('Ctrl Pts',(117.781675321915,-3.81837818158028,331.90013369241));
#55289=CARTESIAN_POINT('Ctrl Pts',(117.773928243537,-3.90484811497968,332.00664632047));
#55290=CARTESIAN_POINT('Ctrl Pts',(117.766181165159,-3.9868798948299,332.116806786475));
#55291=CARTESIAN_POINT('Ctrl Pts',(117.758434086782,-4.06416180535297,332.230203638819));
#55292=CARTESIAN_POINT('Ctrl Pts',(117.750686943476,-4.14144436357289,332.343601441538));
#55293=CARTESIAN_POINT('Ctrl Pts',(117.74293980017,-4.21397675293714,332.460235361701));
#55294=CARTESIAN_POINT('Ctrl Pts',(117.735192656864,-4.28149035151387,332.579664603326));
#55295=CARTESIAN_POINT('Ctrl Pts',(117.727443771836,-4.34901912858079,332.699120695179));
#55296=CARTESIAN_POINT('Ctrl Pts',(117.719694886808,-4.41152667729135,332.821373018834));
#55297=CARTESIAN_POINT('Ctrl Pts',(117.71194600178,-4.46879032565175,332.945956162137));
#55298=CARTESIAN_POINT('Ctrl Pts',(117.704188892005,-4.52611475424024,333.070671539277));
#55299=CARTESIAN_POINT('Ctrl Pts',(117.69643178223,-4.57818400050974,333.19772232231));
#55300=CARTESIAN_POINT('Ctrl Pts',(117.688674672456,-4.62482335785744,333.326622585572));
#55301=CARTESIAN_POINT('Ctrl Pts',(117.680913417529,-4.67148763778646,333.455591729014));
#55302=CARTESIAN_POINT('Ctrl Pts',(117.673152162603,-4.71271612974655,333.586411949358));
#55303=CARTESIAN_POINT('Ctrl Pts',(117.665390907677,-4.74838433486586,333.718583100275));
#55304=CARTESIAN_POINT('Ctrl Pts',(117.657617237272,-4.78410959748912,333.850965681959));
#55305=CARTESIAN_POINT('Ctrl Pts',(117.649843566868,-4.81425671313375,333.984703131125));
#55306=CARTESIAN_POINT('Ctrl Pts',(117.642069896463,-4.83875236983975,334.119285196065));
#55307=CARTESIAN_POINT('Ctrl Pts',(117.634658092286,-4.86210774783247,334.247602433502));
#55308=CARTESIAN_POINT('Ctrl Pts',(117.627246288109,-4.88032593679839,334.376687137616));
#55309=CARTESIAN_POINT('Ctrl Pts',(117.619834483932,-4.89338751171919,334.506095431636));
#55310=CARTESIAN_POINT('Ctrl Pts',(117.610495448124,-4.90984538256678,334.669152720096));
#55311=CARTESIAN_POINT('Ctrl Pts',(117.601156412316,-4.91815503121431,334.833046133824));
#55312=CARTESIAN_POINT('Ctrl Pts',(117.591817376508,-4.91824919068047,334.997178498468));
#55313=CARTESIAN_POINT('',(115.84181737656,-4.91824921532725,334.997221793222));
#55314=CARTESIAN_POINT('Ctrl Pts',(117.59181737647,-4.91824919068085,334.99717849913));
#55315=CARTESIAN_POINT('Ctrl Pts',(117.584144529207,-4.91832655102595,335.132027812359));
#55316=CARTESIAN_POINT('Ctrl Pts',(117.576471681944,-4.91285375398507,335.267100332213));
#55317=CARTESIAN_POINT('Ctrl Pts',(117.56879883468,-4.90180212690904,335.401894228784));
#55318=CARTESIAN_POINT('Ctrl Pts',(117.561134564802,-4.89076285431585,335.536537440856));
#55319=CARTESIAN_POINT('Ctrl Pts',(117.553470294923,-4.87415718779738,335.670902252343));
#55320=CARTESIAN_POINT('Ctrl Pts',(117.545806025045,-4.85200845814346,335.804485540333));
#55321=CARTESIAN_POINT('Ctrl Pts',(117.538148379225,-4.82987887114447,335.937953375255));
#55322=CARTESIAN_POINT('Ctrl Pts',(117.530490733404,-4.80221581649998,336.070640636286));
#55323=CARTESIAN_POINT('Ctrl Pts',(117.522833087584,-4.76909450283843,336.20204853708));
#55324=CARTESIAN_POINT('Ctrl Pts',(117.515179689865,-4.7359915633218,336.333383538959));
#55325=CARTESIAN_POINT('Ctrl Pts',(117.507526292146,-4.69743648457715,336.463440203752));
#55326=CARTESIAN_POINT('Ctrl Pts',(117.499872894427,-4.65355562973359,336.591729582396));
#55327=CARTESIAN_POINT('Ctrl Pts',(117.492221660361,-4.6096871802239,336.719982693001));
#55328=CARTESIAN_POINT('Ctrl Pts',(117.484570426295,-4.5604960777282,336.846469131093));
#55329=CARTESIAN_POINT('Ctrl Pts',(117.476919192229,-4.50615851227743,336.97071523177));
#55330=CARTESIAN_POINT('Ctrl Pts',(117.469268366191,-4.45182384456133,337.094954706603));
#55331=CARTESIAN_POINT('Ctrl Pts',(117.461617540154,-4.39234342062797,337.216953713654));
#55332=CARTESIAN_POINT('Ctrl Pts',(117.453966714116,-4.32794131306079,337.336259200774));
#55333=CARTESIAN_POINT('Ctrl Pts',(117.446314541037,-4.26352786655405,337.455585693383));
#55334=CARTESIAN_POINT('Ctrl Pts',(117.438662367959,-4.1941912043012,337.572217369784));
#55335=CARTESIAN_POINT('Ctrl Pts',(117.43101019488,-4.12020075350308,337.685726868714));
#55336=CARTESIAN_POINT('Ctrl Pts',(117.42335028893,-4.04613553196235,337.799351074197));
#55337=CARTESIAN_POINT('Ctrl Pts',(117.41569038298,-3.96740734910642,337.909846463974));
#55338=CARTESIAN_POINT('Ctrl Pts',(117.40803047703,-3.88432848554171,338.016815420093));
#55339=CARTESIAN_POINT('Ctrl Pts',(117.400366632117,-3.8012069002403,338.123839382977));
#55340=CARTESIAN_POINT('Ctrl Pts',(117.392702787205,-3.71373043828124,338.227332994806));
#55341=CARTESIAN_POINT('Ctrl Pts',(117.385038942293,-3.62225002662831,338.326933694424));
#55342=CARTESIAN_POINT('Ctrl Pts',(117.37736309491,-3.53062634603469,338.426690380295));
#55343=CARTESIAN_POINT('Ctrl Pts',(117.369687247528,-3.43498647310173,338.522541691041));
#55344=CARTESIAN_POINT('Ctrl Pts',(117.362011400145,-3.33571684786384,338.614163274311));
#55345=CARTESIAN_POINT('Ctrl Pts',(117.355206416649,-3.24770986600406,338.695389923424));
#55346=CARTESIAN_POINT('Ctrl Pts',(117.348401433154,-3.15685067194417,338.773292636824));
#55347=CARTESIAN_POINT('Ctrl Pts',(117.341596449658,-3.06342765363515,338.84767385227));
#55348=CARTESIAN_POINT('Ctrl Pts',(117.333821370879,-2.95668656785087,338.932658600595));
#55349=CARTESIAN_POINT('Ctrl Pts',(117.326046292101,-2.84623769652375,339.013332503847));
#55350=CARTESIAN_POINT('Ctrl Pts',(117.318271213323,-2.73246433625197,339.089354681806));
#55351=CARTESIAN_POINT('Ctrl Pts',(117.310505702274,-2.61883098134325,339.165283309636));
#55352=CARTESIAN_POINT('Ctrl Pts',(117.302740191225,-2.50188159928907,339.236571386691));
#55353=CARTESIAN_POINT('Ctrl Pts',(117.294974680176,-2.38203283510247,339.302917921015));
#55354=CARTESIAN_POINT('Ctrl Pts',(117.287216868653,-2.2623029013147,339.369198672557));
#55355=CARTESIAN_POINT('Ctrl Pts',(117.279459057131,-2.13967964606959,339.430547443665));
#55356=CARTESIAN_POINT('Ctrl Pts',(117.271701245609,-2.0146087022326,339.486706457903));
#55357=CARTESIAN_POINT('Ctrl Pts',(117.263949272086,-1.88963187824648,339.542823210702));
#55358=CARTESIAN_POINT('Ctrl Pts',(117.256197298563,-1.76221138714826,339.593757820786));
#55359=CARTESIAN_POINT('Ctrl Pts',(117.24844532504,-1.63281715644165,339.639298567255));
#55360=CARTESIAN_POINT('Ctrl Pts',(117.240696634482,-1.50347772426891,339.68482002719));
#55361=CARTESIAN_POINT('Ctrl Pts',(117.232947943925,-1.3721665829315,339.724952037333));
#55362=CARTESIAN_POINT('Ctrl Pts',(117.225199253367,-1.23937311654837,339.759531210159));
#55363=CARTESIAN_POINT('Ctrl Pts',(117.217452174989,-1.10660727895499,339.7941031885));
#55364=CARTESIAN_POINT('Ctrl Pts',(117.209705096611,-0.972360107788149,
339.823124529089));
#55365=CARTESIAN_POINT('Ctrl Pts',(117.201958018233,-0.837135225290063,
339.846481989761));
#55366=CARTESIAN_POINT('Ctrl Pts',(117.194210874928,-0.701909209477538,
339.869839646191));
#55367=CARTESIAN_POINT('Ctrl Pts',(117.186463731622,-0.565705851160481,
339.887533261494));
#55368=CARTESIAN_POINT('Ctrl Pts',(117.178716588316,-0.429037626449165,
339.899500972302));
#55369=CARTESIAN_POINT('Ctrl Pts',(117.170967703288,-0.292338675819384,
339.911471373706));
#55370=CARTESIAN_POINT('Ctrl Pts',(117.16321881826,-0.155175040136601,339.917713274931));
#55371=CARTESIAN_POINT('Ctrl Pts',(117.155469933232,-0.0180625627713276,
339.918216831975));
#55372=CARTESIAN_POINT('Ctrl Pts',(117.147712823457,0.119195447194198,339.9187209235));
#55373=CARTESIAN_POINT('Ctrl Pts',(117.139955713682,0.256401798883917,339.913474502585));
#55374=CARTESIAN_POINT('Ctrl Pts',(117.132198603908,0.393041850661492,339.902519879218));
#55375=CARTESIAN_POINT('Ctrl Pts',(117.124437348981,0.529754918513928,339.891559402051));
#55376=CARTESIAN_POINT('Ctrl Pts',(117.116676094055,0.66590069569305,339.874884691966));
#55377=CARTESIAN_POINT('Ctrl Pts',(117.108914839129,0.800972398676446,339.852589646679));
#55378=CARTESIAN_POINT('Ctrl Pts',(117.101141168724,0.936260172364942,339.830258936586));
#55379=CARTESIAN_POINT('Ctrl Pts',(117.09336749832,1.07047005559319,339.802290004985));
#55380=CARTESIAN_POINT('Ctrl Pts',(117.085593827915,1.20310727411774,339.76882752356));
#55381=CARTESIAN_POINT('Ctrl Pts',(117.078182023738,1.32957019820814,339.736922728697));
#55382=CARTESIAN_POINT('Ctrl Pts',(117.070770219561,1.45460330167092,339.700024405104));
#55383=CARTESIAN_POINT('Ctrl Pts',(117.063358415384,1.57779454607045,339.658298770248));
#55384=CARTESIAN_POINT('Ctrl Pts',(117.055583336606,1.70702376032662,339.614528037733));
#55385=CARTESIAN_POINT('Ctrl Pts',(117.047808257827,1.83463438850358,339.565306503628));
#55386=CARTESIAN_POINT('Ctrl Pts',(117.040033179049,1.96013235336833,339.510772020373));
#55387=CARTESIAN_POINT('Ctrl Pts',(117.032267668,2.08547588499781,339.456304645271));
#55388=CARTESIAN_POINT('Ctrl Pts',(117.024502156951,2.20871157104214,339.3965374839));
#55389=CARTESIAN_POINT('Ctrl Pts',(117.016736645902,2.32936083041821,339.33165801792));
#55390=CARTESIAN_POINT('Ctrl Pts',(117.008978834379,2.44989046570219,339.26684288012));
#55391=CARTESIAN_POINT('Ctrl Pts',(117.001221022857,2.56783843567985,339.196925708971));
#55392=CARTESIAN_POINT('Ctrl Pts',(116.993463211335,2.68274681313196,339.122141749034));
#55393=CARTESIAN_POINT('Ctrl Pts',(116.985711237812,2.79756871838577,339.047414066399));
#55394=CARTESIAN_POINT('Ctrl Pts',(116.977959264289,2.90935525776649,338.967827097182));
#55395=CARTESIAN_POINT('Ctrl Pts',(116.970207290766,3.01767408591497,338.883661439119));
#55396=CARTESIAN_POINT('Ctrl Pts',(116.962458600209,3.12594704097579,338.799531425261));
#55397=CARTESIAN_POINT('Ctrl Pts',(116.954709909651,3.23075489769328,338.710826818573));
#55398=CARTESIAN_POINT('Ctrl Pts',(116.946961219093,3.33169542618465,338.617870734236));
#55399=CARTESIAN_POINT('Ctrl Pts',(116.939214140716,3.43261495315607,338.524933990189));
#55400=CARTESIAN_POINT('Ctrl Pts',(116.931467062338,3.52966846502012,338.427747792554));
#55401=CARTESIAN_POINT('Ctrl Pts',(116.92371998396,3.62248819513091,338.326674366186));
#55402=CARTESIAN_POINT('Ctrl Pts',(116.915972840654,3.7153087031605,338.225600092725));
#55403=CARTESIAN_POINT('Ctrl Pts',(116.908225697348,3.80389509427798,338.120638813444));
#55404=CARTESIAN_POINT('Ctrl Pts',(116.900478554042,3.88791801602921,338.012188002621));
#55405=CARTESIAN_POINT('Ctrl Pts',(116.892729669014,3.97195982791705,337.903712809753));
#55406=CARTESIAN_POINT('Ctrl Pts',(116.884980783986,4.05143588953866,337.791746833163));
#55407=CARTESIAN_POINT('Ctrl Pts',(116.877231898958,4.12605877041466,337.676718529391));
#55408=CARTESIAN_POINT('Ctrl Pts',(116.869474789183,4.20076085678731,337.561568133389));
#55409=CARTESIAN_POINT('Ctrl Pts',(116.861717679409,4.27059925931053,337.443349245687));
#55410=CARTESIAN_POINT('Ctrl Pts',(116.853960569634,4.33533105523617,337.32251753578));
#55411=CARTESIAN_POINT('Ctrl Pts',(116.846199314708,4.40009744176379,337.20162125727));
#55412=CARTESIAN_POINT('Ctrl Pts',(116.838438059782,4.45975161438901,337.078109726277));
#55413=CARTESIAN_POINT('Ctrl Pts',(116.830676804855,4.51409828406028,336.952459921316));
#55414=CARTESIAN_POINT('Ctrl Pts',(116.822903134451,4.56853189069155,336.826609117616));
#55415=CARTESIAN_POINT('Ctrl Pts',(116.815129464046,4.61764088819396,336.698613569821));
#55416=CARTESIAN_POINT('Ctrl Pts',(116.807355793642,4.66127918333878,336.568967634297));
#55417=CARTESIAN_POINT('Ctrl Pts',(116.799943989464,4.70288610534631,336.445356748262));
#55418=CARTESIAN_POINT('Ctrl Pts',(116.792532185287,4.73952010452823,336.320245943972));
#55419=CARTESIAN_POINT('Ctrl Pts',(116.78512038111,4.77109797905778,336.194071663147));
#55420=CARTESIAN_POINT('Ctrl Pts',(116.777345302332,4.8042235792833,336.061713204967));
#55421=CARTESIAN_POINT('Ctrl Pts',(116.769570223553,4.83188957436215,335.927766108844));
#55422=CARTESIAN_POINT('Ctrl Pts',(116.761795144775,4.85394451381067,335.79272045473));
#55423=CARTESIAN_POINT('Ctrl Pts',(116.754029633726,4.87597231325211,335.657840982891));
#55424=CARTESIAN_POINT('Ctrl Pts',(116.746264122677,4.89240273315953,335.521866024921));
#55425=CARTESIAN_POINT('Ctrl Pts',(116.738498611628,4.90313444317588,335.385299486948));
#55426=CARTESIAN_POINT('Ctrl Pts',(116.730740800105,4.91385551267051,335.248868355095));
#55427=CARTESIAN_POINT('Ctrl Pts',(116.722982988583,4.91888908624141,335.111847197675));
#55428=CARTESIAN_POINT('Ctrl Pts',(116.715225177061,4.91818517536568,334.974748399788));
#55429=CARTESIAN_POINT('Ctrl Pts',(116.707473203538,4.91748179420521,334.837752773094));
#55430=CARTESIAN_POINT('Ctrl Pts',(116.699721230015,4.91104952464625,334.700680011525));
#55431=CARTESIAN_POINT('Ctrl Pts',(116.691969256492,4.89889036042889,334.564045531051));
#55432=CARTESIAN_POINT('Ctrl Pts',(116.684220565934,4.88673634562477,334.42746891536));
#55433=CARTESIAN_POINT('Ctrl Pts',(116.676471875377,4.86886029457421,334.29133060012));
#55434=CARTESIAN_POINT('Ctrl Pts',(116.668723184819,4.84531625205711,334.156143685186));
#55435=CARTESIAN_POINT('Ctrl Pts',(116.660976106441,4.82177710807469,334.020984897019));
#55436=CARTESIAN_POINT('Ctrl Pts',(116.653229028063,4.7925723853058,333.886777500263));
#55437=CARTESIAN_POINT('Ctrl Pts',(116.645481949686,4.75780766672358,333.754026778391));
#55438=CARTESIAN_POINT('Ctrl Pts',(116.63773480638,4.7230426567796,333.62127494394));
#55439=CARTESIAN_POINT('Ctrl Pts',(116.629987663074,4.68271765710167,333.489980186847));
#55440=CARTESIAN_POINT('Ctrl Pts',(116.622240519768,4.63698868077768,333.360634562753));
#55441=CARTESIAN_POINT('Ctrl Pts',(116.61449163474,4.59124942360894,333.231259859017));
#55442=CARTESIAN_POINT('Ctrl Pts',(116.606742749712,4.54010390248369,333.103835528713));
#55443=CARTESIAN_POINT('Ctrl Pts',(116.598993864684,4.48375687052214,332.978835140681));
#55444=CARTESIAN_POINT('Ctrl Pts',(116.591236754909,4.42735003123865,332.853702075946));
#55445=CARTESIAN_POINT('Ctrl Pts',(116.583479645134,4.36573081341286,332.730998449793));
#55446=CARTESIAN_POINT('Ctrl Pts',(116.57572253536,4.29915093980522,332.611175130054));
#55447=CARTESIAN_POINT('Ctrl Pts',(116.567961280433,4.23253548804204,332.491287780564));
#55448=CARTESIAN_POINT('Ctrl Pts',(116.560200025507,4.16095430238943,332.374284137627));
#55449=CARTESIAN_POINT('Ctrl Pts',(116.552438770581,4.08470280214685,332.260586544416));
#55450=CARTESIAN_POINT('Ctrl Pts',(116.544665100176,4.00832932435404,332.14670707211));
#55451=CARTESIAN_POINT('Ctrl Pts',(116.536891429772,3.92727083397016,332.036144533121));
#55452=CARTESIAN_POINT('Ctrl Pts',(116.529117759367,3.84186398638091,331.929289304957));
#55453=CARTESIAN_POINT('Ctrl Pts',(116.52170595519,3.76043284809528,331.827408213373));
#55454=CARTESIAN_POINT('Ctrl Pts',(116.514294151013,3.67504926266306,331.728897266853));
#55455=CARTESIAN_POINT('Ctrl Pts',(116.506882346836,3.58603521795476,331.634062615245));
#55456=CARTESIAN_POINT('Ctrl Pts',(116.499107268058,3.49265832975548,331.534579834864));
#55457=CARTESIAN_POINT('Ctrl Pts',(116.491332189279,3.39499101640154,331.438828449779));
#55458=CARTESIAN_POINT('Ctrl Pts',(116.483557110501,3.29336343803204,331.347201028316));
#55459=CARTESIAN_POINT('Ctrl Pts',(116.475791599452,3.1918609188678,331.255686360229));
#55460=CARTESIAN_POINT('Ctrl Pts',(116.468026088403,3.08640811880186,331.168285817602));
#55461=CARTESIAN_POINT('Ctrl Pts',(116.460260577354,2.97737394757625,331.085357303815));
#55462=CARTESIAN_POINT('Ctrl Pts',(116.452502765831,2.8684478840493,331.002511013891));
#55463=CARTESIAN_POINT('Ctrl Pts',(116.444744954309,2.75594782504317,330.924128163937));
#55464=CARTESIAN_POINT('Ctrl Pts',(116.436987142787,2.64027759446093,330.850528071346));
#55465=CARTESIAN_POINT('Ctrl Pts',(116.429235169264,2.52469440939517,330.776983365159));
#55466=CARTESIAN_POINT('Ctrl Pts',(116.421483195741,2.40594612973061,330.708214461339));
#55467=CARTESIAN_POINT('Ctrl Pts',(116.413731222218,2.2844672586807,330.644498604464));
#55468=CARTESIAN_POINT('Ctrl Pts',(116.405982531661,2.16303983400456,330.580809731293));
#55469=CARTESIAN_POINT('Ctrl Pts',(116.398233841103,2.0388844633851,330.522169829999));
#55470=CARTESIAN_POINT('Ctrl Pts',(116.390485150545,1.91246187016815,330.468811120947));
#55471=CARTESIAN_POINT('Ctrl Pts',(116.382738072168,1.78606558022753,330.415463513621));
#55472=CARTESIAN_POINT('Ctrl Pts',(116.37499099379,1.65740336584989,330.367395064849));
#55473=CARTESIAN_POINT('Ctrl Pts',(116.367243915412,1.52695726769135,330.324790425538));
#55474=CARTESIAN_POINT('Ctrl Pts',(116.359496772106,1.39651007626887,330.282185429158));
#55475=CARTESIAN_POINT('Ctrl Pts',(116.3517496288,1.26427934280408,330.245044454928));
#55476=CARTESIAN_POINT('Ctrl Pts',(116.344002485494,1.13076327501897,330.213502587657));
#55477=CARTESIAN_POINT('Ctrl Pts',(116.336253600466,0.997217189986916,330.181953629104));
#55478=CARTESIAN_POINT('Ctrl Pts',(116.328504715438,0.862385575944641,330.156006372225));
#55479=CARTESIAN_POINT('Ctrl Pts',(116.32075583041,0.726777470695663,330.135744911028));
#55480=CARTESIAN_POINT('Ctrl Pts',(116.312998720635,0.59102542960305,330.115461944107));
#55481=CARTESIAN_POINT('Ctrl Pts',(116.305241610861,0.454495638128982,330.100876886121));
#55482=CARTESIAN_POINT('Ctrl Pts',(116.297484501086,0.317703462280664,330.092022048485));
#55483=CARTESIAN_POINT('Ctrl Pts',(116.28972324616,0.180838189067712,330.083162479108));
#55484=CARTESIAN_POINT('Ctrl Pts',(116.281961991234,0.043710642674533,330.080039240379));
#55485=CARTESIAN_POINT('Ctrl Pts',(116.274200736308,-0.0931641511791335,
330.082632462035));
#55486=CARTESIAN_POINT('Ctrl Pts',(116.266427065903,-0.230257900095948,
330.085229832));
#55487=CARTESIAN_POINT('Ctrl Pts',(116.258653395498,-0.367097698161858,
330.093561911946));
#55488=CARTESIAN_POINT('Ctrl Pts',(116.250879725094,-0.503173085055177,
330.107556856848));
#55489=CARTESIAN_POINT('Ctrl Pts',(116.243467920916,-0.632914129952058,
330.120900333698));
#55490=CARTESIAN_POINT('Ctrl Pts',(116.236056116739,-0.761960043908237,
330.139391286548));
#55491=CARTESIAN_POINT('Ctrl Pts',(116.228644312562,-0.889879132872186,
330.162924624179));
#55492=CARTESIAN_POINT('Ctrl Pts',(116.220869233784,-1.02406791743659,330.187611400789));
#55493=CARTESIAN_POINT('Ctrl Pts',(116.213094155005,-1.15744068732577,330.217925359546));
#55494=CARTESIAN_POINT('Ctrl Pts',(116.205319076227,-1.28948865486437,330.253801302992));
#55495=CARTESIAN_POINT('Ctrl Pts',(116.197553565178,-1.4213741289716,330.289633098806));
#55496=CARTESIAN_POINT('Ctrl Pts',(116.189788054129,-1.55193767087079,330.331013159461));
#55497=CARTESIAN_POINT('Ctrl Pts',(116.18202254308,-1.68067867374598,330.377824942939));
#55498=CARTESIAN_POINT('Ctrl Pts',(116.174264731558,-1.80929202954278,330.424590312398));
#55499=CARTESIAN_POINT('Ctrl Pts',(116.166506920035,-1.9360860774751,330.476776554383));
#55500=CARTESIAN_POINT('Ctrl Pts',(116.158749108513,-2.0605737644493,330.534216885723));
#55501=CARTESIAN_POINT('Ctrl Pts',(116.15099713499,-2.18496777049114,330.591613991392));
#55502=CARTESIAN_POINT('Ctrl Pts',(116.143245161467,-2.3070585167355,330.65425715333));
#55503=CARTESIAN_POINT('Ctrl Pts',(116.135493187944,-2.42637772768128,330.721931021464));
#55504=CARTESIAN_POINT('Ctrl Pts',(116.127744497387,-2.54564640687014,330.789576229675));
#55505=CARTESIAN_POINT('Ctrl Pts',(116.119995806829,-2.66214554597141,330.862247714221));
#55506=CARTESIAN_POINT('Ctrl Pts',(116.112247116271,-2.77543054208758,330.939683710775));
#55507=CARTESIAN_POINT('Ctrl Pts',(116.104500037894,-2.88869196831414,331.017103596123));
#55508=CARTESIAN_POINT('Ctrl Pts',(116.096752959516,-2.99874025921742,331.099285801284));
#55509=CARTESIAN_POINT('Ctrl Pts',(116.089005881138,-3.10515927805352,331.185924893186));
#55510=CARTESIAN_POINT('Ctrl Pts',(116.081258737832,-3.21157918878343,331.272564711207));
#55511=CARTESIAN_POINT('Ctrl Pts',(116.073511594526,-3.31436946365678,331.363661243692));
#55512=CARTESIAN_POINT('Ctrl Pts',(116.065764451221,-3.41314689819048,331.45886863928));
#55513=CARTESIAN_POINT('Ctrl Pts',(116.058015566193,-3.51194653998911,331.554097439513));
#55514=CARTESIAN_POINT('Ctrl Pts',(116.050266681164,-3.60673126485332,331.653438670718));
#55515=CARTESIAN_POINT('Ctrl Pts',(116.042517796136,-3.69715488677519,331.756509780238));
#55516=CARTESIAN_POINT('Ctrl Pts',(116.034760686362,-3.78767448526299,331.859690290497));
#55517=CARTESIAN_POINT('Ctrl Pts',(116.027003576587,-3.87382347592597,331.966608293117));
#55518=CARTESIAN_POINT('Ctrl Pts',(116.019246466812,-3.95529579328814,332.076847891386));
#55519=CARTESIAN_POINT('Ctrl Pts',(116.011485211886,-4.03681164685179,332.187146398171));
#55520=CARTESIAN_POINT('Ctrl Pts',(116.00372395696,-4.11364562866012,332.300769713734));
#55521=CARTESIAN_POINT('Ctrl Pts',(115.995962702034,-4.18553573807435,332.417273989018));
#55522=CARTESIAN_POINT('Ctrl Pts',(115.988189031629,-4.25754084823477,332.533964633174));
#55523=CARTESIAN_POINT('Ctrl Pts',(115.980415361224,-4.32458609104988,332.653545105271));
#55524=CARTESIAN_POINT('Ctrl Pts',(115.97264169082,-4.38645564316487,332.775547268867));
#55525=CARTESIAN_POINT('Ctrl Pts',(115.965229886643,-4.44544515274365,332.891870202394));
#55526=CARTESIAN_POINT('Ctrl Pts',(115.957818082466,-4.49972986469864,333.01039418011));
#55527=CARTESIAN_POINT('Ctrl Pts',(115.950406278289,-4.54916453805657,333.130699310387));
#55528=CARTESIAN_POINT('Ctrl Pts',(115.941357203145,-4.60951935359828,333.277579899523));
#55529=CARTESIAN_POINT('Ctrl Pts',(115.932308128001,-4.66281245506729,333.42752295293));
#55530=CARTESIAN_POINT('Ctrl Pts',(115.923259052857,-4.70875950389444,333.579870781589));
#55531=CARTESIAN_POINT('Ctrl Pts',(115.914584544033,-4.75280467692059,333.725912511031));
#55532=CARTESIAN_POINT('Ctrl Pts',(115.90591003521,-4.79009954401527,333.874163693861));
#55533=CARTESIAN_POINT('Ctrl Pts',(115.897235526387,-4.82044076125398,334.024021552625));
#55534=CARTESIAN_POINT('Ctrl Pts',(115.888587993326,-4.85068762416624,334.173413387326));
#55535=CARTESIAN_POINT('Ctrl Pts',(115.879940460264,-4.87402390341494,334.324401719336));
#55536=CARTESIAN_POINT('Ctrl Pts',(115.871292927202,-4.89029591783363,334.47636950192));
#55537=CARTESIAN_POINT('Ctrl Pts',(115.86268627168,-4.90649101321472,334.627618921351));
#55538=CARTESIAN_POINT('Ctrl Pts',(115.854079616159,-4.91568837694199,334.77983833998));
#55539=CARTESIAN_POINT('Ctrl Pts',(115.845472960637,-4.9177854448456,334.932402803573));
#55540=CARTESIAN_POINT('Ctrl Pts',(115.844254432611,-4.91808234716799,334.954002840213));
#55541=CARTESIAN_POINT('Ctrl Pts',(115.843035904585,-4.91823700718782,334.975609769017));
#55542=CARTESIAN_POINT('Ctrl Pts',(115.84181737656,-4.91824921532725,334.997221793222));
#55543=CARTESIAN_POINT('',(114.09181737646,-4.91824836605016,335.004009032921));
#55544=CARTESIAN_POINT('Ctrl Pts',(115.841817376508,-4.91824921532777,334.997221794137));
#55545=CARTESIAN_POINT('Ctrl Pts',(115.833984682288,-4.91832768918275,335.136143816042));
#55546=CARTESIAN_POINT('Ctrl Pts',(115.826151988068,-4.91251578406707,335.275072939698));
#55547=CARTESIAN_POINT('Ctrl Pts',(115.818319293848,-4.90083827818156,335.413481841935));
#55548=CARTESIAN_POINT('Ctrl Pts',(115.810485101013,-4.88915853806036,335.551917225693));
#55549=CARTESIAN_POINT('Ctrl Pts',(115.802650908177,-4.8716109934746,335.689831812301));
#55550=CARTESIAN_POINT('Ctrl Pts',(115.794816715342,-4.84827231816433,335.826703448294));
#55551=CARTESIAN_POINT('Ctrl Pts',(115.786979472975,-4.82492455805909,335.963628362836));
#55552=CARTESIAN_POINT('Ctrl Pts',(115.779142230608,-4.79578124125216,336.099509144996));
#55553=CARTESIAN_POINT('Ctrl Pts',(115.771304988241,-4.76097011595331,336.233834112634));
#55554=CARTESIAN_POINT('Ctrl Pts',(115.763463143711,-4.72613854896433,336.368237958198));
#55555=CARTESIAN_POINT('Ctrl Pts',(115.755621299181,-4.68563263977677,336.501083803625));
#55556=CARTESIAN_POINT('Ctrl Pts',(115.74777945465,-4.63962983588254,336.631875622861));
#55557=CARTESIAN_POINT('Ctrl Pts',(115.739926779051,-4.59356349342512,336.76284809031));
#55558=CARTESIAN_POINT('Ctrl Pts',(115.732074103452,-4.5419852213524,336.891760509309));
#55559=CARTESIAN_POINT('Ctrl Pts',(115.724221427853,-4.48512066900968,337.018136676968));
#55560=CARTESIAN_POINT('Ctrl Pts',(115.716362315279,-4.42820950379904,337.144616437381));
#55561=CARTESIAN_POINT('Ctrl Pts',(115.708503202704,-4.36600359200974,337.268555466074));
#55562=CARTESIAN_POINT('Ctrl Pts',(115.70064409013,-4.2987739076315,337.38950328595));
#55563=CARTESIAN_POINT('Ctrl Pts',(115.692772760256,-4.23143971206717,337.510639123965));
#55564=CARTESIAN_POINT('Ctrl Pts',(115.684901430382,-4.15906634776463,337.628774147442));
#55565=CARTESIAN_POINT('Ctrl Pts',(115.677030100508,-4.0819676517212,337.743487407079));
#55566=CARTESIAN_POINT('Ctrl Pts',(115.675409481677,-4.06609389205533,337.767105584914));
#55567=CARTESIAN_POINT('Ctrl Pts',(115.673788862845,-4.05001995799648,337.790578828913));
#55568=CARTESIAN_POINT('Ctrl Pts',(115.672168244014,-4.03374879222463,337.813903648622));
#55569=CARTESIAN_POINT('Ctrl Pts',(115.664393165236,-3.95568626866411,337.925806773053));
#55570=CARTESIAN_POINT('Ctrl Pts',(115.656618086457,-3.87284028544115,338.034635881784));
#55571=CARTESIAN_POINT('Ctrl Pts',(115.648843007679,-3.78548097087406,338.139954917137));
#55572=CARTESIAN_POINT('Ctrl Pts',(115.64107749663,-3.69822915750517,338.245144350711));
#55573=CARTESIAN_POINT('Ctrl Pts',(115.633311985581,-3.60647531070338,338.346832007239));
#55574=CARTESIAN_POINT('Ctrl Pts',(115.625546474532,-3.51053290029633,338.4446105467));
#55575=CARTESIAN_POINT('Ctrl Pts',(115.61778866301,-3.41468561706853,338.542292138454));
#55576=CARTESIAN_POINT('Ctrl Pts',(115.610030851487,-3.31465830688097,338.636072049203));
#55577=CARTESIAN_POINT('Ctrl Pts',(115.602273039965,-3.21080455085213,338.72557608951));
#55578=CARTESIAN_POINT('Ctrl Pts',(115.594521066442,-3.1070289480681,338.815012775188));
#55579=CARTESIAN_POINT('Ctrl Pts',(115.586769092919,-2.99943292588546,338.900179741005));
#55580=CARTESIAN_POINT('Ctrl Pts',(115.579017119396,-2.88840648867091,338.980740008931));
#55581=CARTESIAN_POINT('Ctrl Pts',(115.571268428839,-2.77742707121852,339.061266159536));
#55582=CARTESIAN_POINT('Ctrl Pts',(115.563519738281,-2.66302044392482,339.137189263455));
#55583=CARTESIAN_POINT('Ctrl Pts',(115.555771047723,-2.54560904720101,339.208213117382));
#55584=CARTESIAN_POINT('Ctrl Pts',(115.548023969346,-2.42822207889877,339.279222194204));
#55585=CARTESIAN_POINT('Ctrl Pts',(115.540276890968,-2.30783191890321,339.34533384637));
#55586=CARTESIAN_POINT('Ctrl Pts',(115.53252981259,-2.18488895891302,339.406295870651));
#55587=CARTESIAN_POINT('Ctrl Pts',(115.524782669284,-2.06194496854258,339.467258405853));
#55588=CARTESIAN_POINT('Ctrl Pts',(115.517035525978,-1.93644848569086,339.523071053445));
#55589=CARTESIAN_POINT('Ctrl Pts',(115.509288382672,-1.8088730446726,339.573528328409));
#55590=CARTESIAN_POINT('Ctrl Pts',(115.501539497644,-1.68126892198678,339.623996947239));
#55591=CARTESIAN_POINT('Ctrl Pts',(115.493790612616,-1.55158527447946,339.669107653882));
#55592=CARTESIAN_POINT('Ctrl Pts',(115.486041727588,-1.42031370318315,339.708703860623));
#55593=CARTESIAN_POINT('Ctrl Pts',(115.478284617813,-1.28890279888477,339.748342095188));
#55594=CARTESIAN_POINT('Ctrl Pts',(115.470527508039,-1.15590097878726,339.782454024584));
#55595=CARTESIAN_POINT('Ctrl Pts',(115.462770398264,-1.0218135699008,339.810933390816));
#55596=CARTESIAN_POINT('Ctrl Pts',(115.455009143338,-0.887654508990122,
339.83942797551));
#55597=CARTESIAN_POINT('Ctrl Pts',(115.447247888412,-0.752409088595061,
339.86228393452));
#55598=CARTESIAN_POINT('Ctrl Pts',(115.439486633486,-0.616589820371562,
339.879446695673));
#55599=CARTESIAN_POINT('Ctrl Pts',(115.431712963081,-0.480553285582395,
339.896636911651));
#55600=CARTESIAN_POINT('Ctrl Pts',(115.423939292676,-0.343941458296462,
339.908115698022));
#55601=CARTESIAN_POINT('Ctrl Pts',(115.416165622272,-0.207269824000443,
339.91388057268));
#55602=CARTESIAN_POINT('Ctrl Pts',(115.408753818094,-0.0769602871616455,
339.919377091036));
#55603=CARTESIAN_POINT('Ctrl Pts',(115.401342013917,0.0534033261641989,
339.919679690646));
#55604=CARTESIAN_POINT('Ctrl Pts',(115.39393020974,0.183378682197175,339.914830141665));
#55605=CARTESIAN_POINT('Ctrl Pts',(115.386155130962,0.319724517605634,339.909742901842));
#55606=CARTESIAN_POINT('Ctrl Pts',(115.378380052183,0.456073952128501,339.898969622455));
#55607=CARTESIAN_POINT('Ctrl Pts',(115.370604973405,0.591914113628146,339.882501484341));
#55608=CARTESIAN_POINT('Ctrl Pts',(115.362839462356,0.727587115161151,339.866053611318));
#55609=CARTESIAN_POINT('Ctrl Pts',(115.355073951307,0.862751706286306,339.843924869844));
#55610=CARTESIAN_POINT('Ctrl Pts',(115.347308440258,0.99689570957855,339.816158428325));
#55611=CARTESIAN_POINT('Ctrl Pts',(115.339550628736,1.13090670870052,339.788419517313));
#55612=CARTESIAN_POINT('Ctrl Pts',(115.331792817214,1.26389875346427,339.755054108984));
#55613=CARTESIAN_POINT('Ctrl Pts',(115.324035005691,1.39536583695736,339.716157041867));
#55614=CARTESIAN_POINT('Ctrl Pts',(115.316283032168,1.52673398730124,339.677289246027));
#55615=CARTESIAN_POINT('Ctrl Pts',(115.308531058645,1.65657908727584,339.632898187596));
#55616=CARTESIAN_POINT('Ctrl Pts',(115.300779085122,1.78440671112553,339.583129471419));
#55617=CARTESIAN_POINT('Ctrl Pts',(115.293030394565,1.91218019990054,339.533381832323));
#55618=CARTESIAN_POINT('Ctrl Pts',(115.285281704007,2.03793754841391,339.478261206671));
#55619=CARTESIAN_POINT('Ctrl Pts',(115.27753301345,2.16120106624084,339.417962541011));
#55620=CARTESIAN_POINT('Ctrl Pts',(115.269785935072,2.28443893806337,339.357676420993));
#55621=CARTESIAN_POINT('Ctrl Pts',(115.262038856694,2.40518366035942,339.292214575514));
#55622=CARTESIAN_POINT('Ctrl Pts',(115.254291778316,2.52297941726174,339.221819266924));
#55623=CARTESIAN_POINT('Ctrl Pts',(115.24654463501,2.64077616140572,339.151423368354));
#55624=CARTESIAN_POINT('Ctrl Pts',(115.238797491705,2.75562355533375,339.076094124715));
#55625=CARTESIAN_POINT('Ctrl Pts',(115.231050348399,2.86709254572145,338.996118541381));
#55626=CARTESIAN_POINT('Ctrl Pts',(115.223301463371,2.97858659670474,338.916124977838));
#55627=CARTESIAN_POINT('Ctrl Pts',(115.215552578343,3.08670041522773,338.831483223786));
#55628=CARTESIAN_POINT('Ctrl Pts',(115.207803693315,3.19103628981436,338.742521938424));
#55629=CARTESIAN_POINT('Ctrl Pts',(115.20004658354,3.29548290757648,338.653466228635));
#55630=CARTESIAN_POINT('Ctrl Pts',(115.192289473765,3.3961432732495,338.560082082984));
#55631=CARTESIAN_POINT('Ctrl Pts',(115.18453236399,3.49265457077679,338.462736939436));
#55632=CARTESIAN_POINT('Ctrl Pts',(115.176771109064,3.58921744085566,338.365339777755));
#55633=CARTESIAN_POINT('Ctrl Pts',(115.169009854138,3.68162656175378,338.263977689305));
#55634=CARTESIAN_POINT('Ctrl Pts',(115.161248599212,3.76955869310252,338.159052123938));
#55635=CARTESIAN_POINT('Ctrl Pts',(115.153474928807,3.85763148720447,338.053958711861));
#55636=CARTESIAN_POINT('Ctrl Pts',(115.145701258403,3.94121274208253,337.945290741769));
#55637=CARTESIAN_POINT('Ctrl Pts',(115.137927587998,4.02002141170511,337.833480353193));
#55638=CARTESIAN_POINT('Ctrl Pts',(115.130515783821,4.09516151879633,337.726874765107));
#55639=CARTESIAN_POINT('Ctrl Pts',(115.123103979644,4.16596321269736,337.617412975488));
#55640=CARTESIAN_POINT('Ctrl Pts',(115.115692175467,4.23222224663177,337.505489556477));
#55641=CARTESIAN_POINT('Ctrl Pts',(115.107917096688,4.30172883319483,337.388080437297));
#55642=CARTESIAN_POINT('Ctrl Pts',(115.10014201791,4.3664558554701,337.267591249273));
#55643=CARTESIAN_POINT('Ctrl Pts',(115.092366939131,4.42611835269136,337.14444850497));
#55644=CARTESIAN_POINT('Ctrl Pts',(115.084601428082,4.48570743141148,337.021457295654));
#55645=CARTESIAN_POINT('Ctrl Pts',(115.076835917033,4.54024421661018,336.895819375608));
#55646=CARTESIAN_POINT('Ctrl Pts',(115.069070405984,4.58948784092821,336.767988806659));
#55647=CARTESIAN_POINT('Ctrl Pts',(115.061312594462,4.63868264004919,336.640284982092));
#55648=CARTESIAN_POINT('Ctrl Pts',(115.05355478294,4.68259458286879,336.510393197436));
#55649=CARTESIAN_POINT('Ctrl Pts',(115.045796971418,4.72102959175553,336.378790287269));
#55650=CARTESIAN_POINT('Ctrl Pts',(115.038044997895,4.75943567707948,336.247286412466));
#55651=CARTESIAN_POINT('Ctrl Pts',(115.030293024372,4.79237292310994,336.114074348898));
#55652=CARTESIAN_POINT('Ctrl Pts',(115.022541050849,4.81969620992057,335.979648664868));
#55653=CARTESIAN_POINT('Ctrl Pts',(115.014792360291,4.84700792530293,335.845279910195));
#55654=CARTESIAN_POINT('Ctrl Pts',(115.007043669733,4.86871033248061,335.709698939554));
#55655=CARTESIAN_POINT('Ctrl Pts',(114.999294979176,4.88470886046739,335.573412949776));
#55656=CARTESIAN_POINT('Ctrl Pts',(114.991547900798,4.90070405982682,335.437155315437));
#55657=CARTESIAN_POINT('Ctrl Pts',(114.98380082242,4.91099769496158,335.300193341694));
#55658=CARTESIAN_POINT('Ctrl Pts',(114.976053744042,4.91554682132943,335.163041435893));
#55659=CARTESIAN_POINT('Ctrl Pts',(114.968306600736,4.92009598582334,335.025888380627));
#55660=CARTESIAN_POINT('Ctrl Pts',(114.960559457431,4.9189005325649,334.888545780787));
#55661=CARTESIAN_POINT('Ctrl Pts',(114.952812314125,4.91196962512306,334.751529751543));
#55662=CARTESIAN_POINT('Ctrl Pts',(114.945063429097,4.9050371594661,334.614482918187));
#55663=CARTESIAN_POINT('Ctrl Pts',(114.937314544069,4.89236669350375,334.477763191824));
#55664=CARTESIAN_POINT('Ctrl Pts',(114.929565659041,4.87401937926774,334.34188287287));
#55665=CARTESIAN_POINT('Ctrl Pts',(114.921808549266,4.85565259100276,334.20585832914));
#55666=CARTESIAN_POINT('Ctrl Pts',(114.914051439491,4.83159697041761,334.070675360558));
#55667=CARTESIAN_POINT('Ctrl Pts',(114.906294329716,4.80196516334924,333.936837908652));
#55668=CARTESIAN_POINT('Ctrl Pts',(114.89853307479,4.77231752199068,333.802928938291));
#55669=CARTESIAN_POINT('Ctrl Pts',(114.890771819864,4.73708785710019,333.67036729485));
#55670=CARTESIAN_POINT('Ctrl Pts',(114.883010564938,4.69643883251175,333.539642045601));
#55671=CARTESIAN_POINT('Ctrl Pts',(114.875236894533,4.65572478273139,333.408707678557));
#55672=CARTESIAN_POINT('Ctrl Pts',(114.867463224128,4.60957418125725,333.279615944218));
#55673=CARTESIAN_POINT('Ctrl Pts',(114.859689553724,4.55819833330779,333.152837035687));
#55674=CARTESIAN_POINT('Ctrl Pts',(114.852277749547,4.50921404344014,333.031959715847));
#55675=CARTESIAN_POINT('Ctrl Pts',(114.844865945369,4.4554801484547,332.913185005678));
#55676=CARTESIAN_POINT('Ctrl Pts',(114.837454141192,4.39721792283059,332.796898186275));
#55677=CARTESIAN_POINT('Ctrl Pts',(114.829679062414,4.33610009197499,332.674911803454));
#55678=CARTESIAN_POINT('Ctrl Pts',(114.821903983635,4.26980566903004,332.555277856224));
#55679=CARTESIAN_POINT('Ctrl Pts',(114.814128904857,4.19853910889006,332.438466784596));
#55680=CARTESIAN_POINT('Ctrl Pts',(114.806363393808,4.12736024678934,332.321799456427));
#55681=CARTESIAN_POINT('Ctrl Pts',(114.798597882759,4.05122162324646,332.207948422623));
#55682=CARTESIAN_POINT('Ctrl Pts',(114.79083237171,3.97037472138839,332.097361952592));
#55683=CARTESIAN_POINT('Ctrl Pts',(114.783074560188,3.88960797946899,331.986885129368));
#55684=CARTESIAN_POINT('Ctrl Pts',(114.775316748666,3.80414247855796,331.879666741964));
#55685=CARTESIAN_POINT('Ctrl Pts',(114.767558937143,3.71427417248259,331.776128036952));
#55686=CARTESIAN_POINT('Ctrl Pts',(114.75980696362,3.62447349515731,331.672667248098));
#55687=CARTESIAN_POINT('Ctrl Pts',(114.752054990097,3.53027686271404,331.572880923922));
#55688=CARTESIAN_POINT('Ctrl Pts',(114.744303016574,3.43202163547017,331.477158738154));
#55689=CARTESIAN_POINT('Ctrl Pts',(114.736554326017,3.33380801937357,331.381477090788));
#55690=CARTESIAN_POINT('Ctrl Pts',(114.728805635459,3.23153950647545,331.289856430743));
#55691=CARTESIAN_POINT('Ctrl Pts',(114.721056944901,3.12559143162631,331.202650758089));
#55692=CARTESIAN_POINT('Ctrl Pts',(114.713309866524,3.01966540015896,331.115463229303));
#55693=CARTESIAN_POINT('Ctrl Pts',(114.705562788146,2.91006163110279,331.032689109044));
#55694=CARTESIAN_POINT('Ctrl Pts',(114.697815709768,2.79718946081311,330.954642885626));
#55695=CARTESIAN_POINT('Ctrl Pts',(114.690068566462,2.68431634454577,330.876596008106));
#55696=CARTESIAN_POINT('Ctrl Pts',(114.682321423156,2.56817509391059,330.803277328764));
#55697=CARTESIAN_POINT('Ctrl Pts',(114.674574279851,2.44920468009787,330.734958441294));
#55698=CARTESIAN_POINT('Ctrl Pts',(114.666825394822,2.33020751921072,330.666624194288));
#55699=CARTESIAN_POINT('Ctrl Pts',(114.659076509794,2.20838026836055,330.603292170517));
#55700=CARTESIAN_POINT('Ctrl Pts',(114.651327624766,2.08418682477,330.545188181084));
#55701=CARTESIAN_POINT('Ctrl Pts',(114.643570514992,1.95986156097518,330.487022519476));
#55702=CARTESIAN_POINT('Ctrl Pts',(114.635813405217,1.83316544208234,330.434096142933));
#55703=CARTESIAN_POINT('Ctrl Pts',(114.628056295442,1.70458320240005,330.386587036846));
#55704=CARTESIAN_POINT('Ctrl Pts',(114.620295040516,1.57593225247996,330.339052543412));
#55705=CARTESIAN_POINT('Ctrl Pts',(114.61253378559,1.44539354528147,330.296941208559));
#55706=CARTESIAN_POINT('Ctrl Pts',(114.604772530664,1.31346637464161,330.260380907163));
#55707=CARTESIAN_POINT('Ctrl Pts',(114.596998860259,1.18132816352396,330.2237621212));
#55708=CARTESIAN_POINT('Ctrl Pts',(114.589225189854,1.04779743148864,330.192712201827));
#55709=CARTESIAN_POINT('Ctrl Pts',(114.58145151945,0.913383923324057,330.167307906445));
#55710=CARTESIAN_POINT('Ctrl Pts',(114.574039715273,0.785227396304288,330.143086187125));
#55711=CARTESIAN_POINT('Ctrl Pts',(114.566627911096,0.656268714751831,330.123996354817));
#55712=CARTESIAN_POINT('Ctrl Pts',(114.559216106919,0.52695161407784,330.1100608328));
#55713=CARTESIAN_POINT('Ctrl Pts',(114.55144102814,0.391296297082119,330.095442289336));
#55714=CARTESIAN_POINT('Ctrl Pts',(114.543665949362,0.254817842349541,330.086449890479));
#55715=CARTESIAN_POINT('Ctrl Pts',(114.535890870584,0.118022495196177,330.08316628783));
#55716=CARTESIAN_POINT('Ctrl Pts',(114.528125359535,-0.0186045165733258,
330.079886725863));
#55717=CARTESIAN_POINT('Ctrl Pts',(114.520359848486,-0.155547257836182,
330.082301991585));
#55718=CARTESIAN_POINT('Ctrl Pts',(114.512594337437,-0.292292677332945,
330.090443191766));
#55719=CARTESIAN_POINT('Ctrl Pts',(114.504836525914,-0.428902513348433,
330.098576319924));
#55720=CARTESIAN_POINT('Ctrl Pts',(114.497078714392,-0.56531502927271,330.112424061352));
#55721=CARTESIAN_POINT('Ctrl Pts',(114.48932090287,-0.701015832278744,330.131965502855));
#55722=CARTESIAN_POINT('Ctrl Pts',(114.481568929347,-0.836614516127381,
330.151492238803));
#55723=CARTESIAN_POINT('Ctrl Pts',(114.473816955824,-0.971502167790937,
330.176704090872));
#55724=CARTESIAN_POINT('Ctrl Pts',(114.466064982301,-1.10516853729211,330.207528240388));
#55725=CARTESIAN_POINT('Ctrl Pts',(114.458316291743,-1.23877829900636,330.238339335858));
#55726=CARTESIAN_POINT('Ctrl Pts',(114.450567601186,-1.37116742717439,330.274757913814));
#55727=CARTESIAN_POINT('Ctrl Pts',(114.442818910628,-1.50183512036135,330.316659916924));
#55728=CARTESIAN_POINT('Ctrl Pts',(114.43507183225,-1.63247562704337,330.358553201972));
#55729=CARTESIAN_POINT('Ctrl Pts',(114.427324753873,-1.76139503917644,330.405927523615));
#55730=CARTESIAN_POINT('Ctrl Pts',(114.419577675495,-1.88810738143914,330.458608849851));
#55731=CARTESIAN_POINT('Ctrl Pts',(114.411830532189,-2.01482078567322,330.511290617607));
#55732=CARTESIAN_POINT('Ctrl Pts',(114.404083388883,-2.13932672221883,330.569279328614));
#55733=CARTESIAN_POINT('Ctrl Pts',(114.396336245577,-2.26115924964645,330.632352817564));
#55734=CARTESIAN_POINT('Ctrl Pts',(114.388587360549,-2.38301916761315,330.695440486774));
#55735=CARTESIAN_POINT('Ctrl Pts',(114.380838475521,-2.50220413341341,330.763615029031));
#55736=CARTESIAN_POINT('Ctrl Pts',(114.373089590493,-2.61827321626783,330.836608542609));
#55737=CARTESIAN_POINT('Ctrl Pts',(114.365332480718,-2.73446549604562,330.909679532256));
#55738=CARTESIAN_POINT('Ctrl Pts',(114.357575370943,-2.84753495496961,330.987579502314));
#55739=CARTESIAN_POINT('Ctrl Pts',(114.349818261169,-2.9570696037799,331.069997147469));
#55740=CARTESIAN_POINT('Ctrl Pts',(114.342057006243,-3.06666278440428,331.152458833978));
#55741=CARTESIAN_POINT('Ctrl Pts',(114.334295751316,-3.17271708906238,331.239442758146));
#55742=CARTESIAN_POINT('Ctrl Pts',(114.32653449639,-3.2748547884988,331.330598253564));
#55743=CARTESIAN_POINT('Ctrl Pts',(114.318760825986,-3.37715587496764,331.421899568068));
#55744=CARTESIAN_POINT('Ctrl Pts',(114.310987155581,-3.47552755568549,331.517385516373));
#55745=CARTESIAN_POINT('Ctrl Pts',(114.303213485176,-3.56962943156249,331.616668981045));
#55746=CARTESIAN_POINT('Ctrl Pts',(114.295801680999,-3.6593508424778,331.711330776551));
#55747=CARTESIAN_POINT('Ctrl Pts',(114.288389876822,-3.74519083196599,331.809444279446));
#55748=CARTESIAN_POINT('Ctrl Pts',(114.280978072645,-3.82689041312112,331.91064847768));
#55749=CARTESIAN_POINT('Ctrl Pts',(114.273096376973,-3.91376956154956,332.018268791464));
#55750=CARTESIAN_POINT('Ctrl Pts',(114.2652146813,-3.99625251524312,332.12973910162));
#55751=CARTESIAN_POINT('Ctrl Pts',(114.257332985628,-4.07397831343783,332.244662676887));
#55752=CARTESIAN_POINT('Ctrl Pts',(114.24959039858,-4.15033228387286,332.357557899221));
#55753=CARTESIAN_POINT('Ctrl Pts',(114.241847811533,-4.22209536857364,332.473785176595));
#55754=CARTESIAN_POINT('Ctrl Pts',(114.234105224486,-4.28896385994519,332.592932890303));
#55755=CARTESIAN_POINT('Ctrl Pts',(114.226370083379,-4.35576804479946,332.711966021278));
#55756=CARTESIAN_POINT('Ctrl Pts',(114.218634942272,-4.41768680853792,332.833913661757));
#55757=CARTESIAN_POINT('Ctrl Pts',(114.210899801165,-4.47445926984854,332.958334673614));
#55758=CARTESIAN_POINT('Ctrl Pts',(114.20317040219,-4.5311895864961,333.082663322352));
#55759=CARTESIAN_POINT('Ctrl Pts',(114.195441003214,-4.58278103946054,333.209461333341));
#55760=CARTESIAN_POINT('Ctrl Pts',(114.187711604238,-4.62901851245242,333.338262754262));
#55761=CARTESIAN_POINT('Ctrl Pts',(114.179720418594,-4.67682200035038,333.471426544751));
#55762=CARTESIAN_POINT('Ctrl Pts',(114.17172923295,-4.71890222308606,333.606731473012));
#55763=CARTESIAN_POINT('Ctrl Pts',(114.163738047306,-4.75507534014221,333.743639553284));
#55764=CARTESIAN_POINT('Ctrl Pts',(114.15601424407,-4.79003811675802,333.875966734822));
#55765=CARTESIAN_POINT('Ctrl Pts',(114.148290440834,-4.81948264477097,334.00979109895));
#55766=CARTESIAN_POINT('Ctrl Pts',(114.140566637598,-4.84329371029037,334.144611726547));
#55767=CARTESIAN_POINT('Ctrl Pts',(114.132441760749,-4.86834121202774,334.286433179316));
#55768=CARTESIAN_POINT('Ctrl Pts',(114.124316883901,-4.88715441838337,334.429356673909));
#55769=CARTESIAN_POINT('Ctrl Pts',(114.116192007053,-4.89966052700142,334.572788363169));
#55770=CARTESIAN_POINT('Ctrl Pts',(114.108067130205,-4.91216663561948,334.716220052429));
#55771=CARTESIAN_POINT('Ctrl Pts',(114.099942253356,-4.91836562276903,334.860159431135));
#55772=CARTESIAN_POINT('Ctrl Pts',(114.091817376508,-4.91824836605085,335.004009032065));
#55773=CARTESIAN_POINT('',(112.341817415646,-4.92215159501353,335.000927415304));
#55774=CARTESIAN_POINT('Ctrl Pts',(114.09181737646,-4.91824836605016,335.004009032921));
#55775=CARTESIAN_POINT('Ctrl Pts',(114.082676714162,-4.91811644967628,335.165842947251));
#55776=CARTESIAN_POINT('Ctrl Pts',(114.073536051864,-4.90999303901002,335.32733713016));
#55777=CARTESIAN_POINT('Ctrl Pts',(114.064395389566,-4.89400164464294,335.487781677323));
#55778=CARTESIAN_POINT('Ctrl Pts',(114.055191910065,-4.87790035291416,335.64932884456));
#55779=CARTESIAN_POINT('Ctrl Pts',(114.045988430563,-4.8538226684699,335.809811838755));
#55780=CARTESIAN_POINT('Ctrl Pts',(114.036784951062,-4.82194352195957,335.96852657864));
#55781=CARTESIAN_POINT('Ctrl Pts',(114.027512341879,-4.78982492305096,336.128433465407));
#55782=CARTESIAN_POINT('Ctrl Pts',(114.018239732696,-4.74978729078376,336.28654537743));
#55783=CARTESIAN_POINT('Ctrl Pts',(114.008967123514,-4.70205766064995,336.442163936043));
#55784=CARTESIAN_POINT('Ctrl Pts',(114.006891428466,-4.69137327236871,336.476999510912));
#55785=CARTESIAN_POINT('Ctrl Pts',(114.004815733418,-4.68030362671436,336.511710231549));
#55786=CARTESIAN_POINT('Ctrl Pts',(114.002740038371,-4.66885159300798,336.546288415842));
#55787=CARTESIAN_POINT('Ctrl Pts',(113.994964959592,-4.62595489469636,336.675810383539));
#55788=CARTESIAN_POINT('Ctrl Pts',(113.987189880814,-4.57759658448115,336.803750626139));
#55789=CARTESIAN_POINT('Ctrl Pts',(113.979414802036,-4.5239111738125,336.929614146392));
#55790=CARTESIAN_POINT('Ctrl Pts',(113.971649290987,-4.47029182645941,337.05532278357));
#55791=CARTESIAN_POINT('Ctrl Pts',(113.963883779938,-4.41135857378103,337.178959427094));
#55792=CARTESIAN_POINT('Ctrl Pts',(113.956118268889,-4.34729566000345,337.30004424023));
#55793=CARTESIAN_POINT('Ctrl Pts',(113.948360457366,-4.2832962647914,337.421008997421));
#55794=CARTESIAN_POINT('Ctrl Pts',(113.940602645844,-4.21417751167162,337.539426616088));
#55795=CARTESIAN_POINT('Ctrl Pts',(113.932844834322,-4.14017154621386,337.654837590215));
#55796=CARTESIAN_POINT('Ctrl Pts',(113.925092860799,-4.06622127259198,337.770161713926));
#55797=CARTESIAN_POINT('Ctrl Pts',(113.917340887276,-3.98739131721963,337.88248336897));
#55798=CARTESIAN_POINT('Ctrl Pts',(113.909588913753,-3.90395935062811,337.991368324219));
#55799=CARTESIAN_POINT('Ctrl Pts',(113.901840223195,-3.82056271752398,338.100207166625));
#55800=CARTESIAN_POINT('Ctrl Pts',(113.894091532638,-3.73256818677585,338.205611894393));
#55801=CARTESIAN_POINT('Ctrl Pts',(113.88634284208,-3.6402961488424,338.307178103947));
#55802=CARTESIAN_POINT('Ctrl Pts',(113.878595763702,-3.54804330887711,338.408723181801));
#55803=CARTESIAN_POINT('Ctrl Pts',(113.870848685324,-3.45151499461248,338.506431040856));
#55804=CARTESIAN_POINT('Ctrl Pts',(113.863101606946,-3.35107093811122,338.599931475771));
#55805=CARTESIAN_POINT('Ctrl Pts',(113.855354463641,-3.25062603979216,338.693432694309));
#55806=CARTESIAN_POINT('Ctrl Pts',(113.847607320335,-3.14626561988103,338.78272615205));
#55807=CARTESIAN_POINT('Ctrl Pts',(113.839860177029,-3.03838491857391,338.867479818833));
#55808=CARTESIAN_POINT('Ctrl Pts',(113.832111292001,-2.93047996339461,338.95225254004));
#55809=CARTESIAN_POINT('Ctrl Pts',(113.824362406973,-2.81905345925911,339.032483197902));
#55810=CARTESIAN_POINT('Ctrl Pts',(113.816613521945,-2.70453191113264,339.107881473967));
#55811=CARTESIAN_POINT('Ctrl Pts',(113.80885641217,-2.58988880865183,339.183359778543));
#55812=CARTESIAN_POINT('Ctrl Pts',(113.801099302395,-2.47214442684781,339.253995240104));
#55813=CARTESIAN_POINT('Ctrl Pts',(113.793342192621,-2.35175278369957,339.319541863075));
#55814=CARTESIAN_POINT('Ctrl Pts',(113.785580937694,-2.23129680710669,339.385123512066));
#55815=CARTESIAN_POINT('Ctrl Pts',(113.777819682768,-2.10819110106501,339.445610731708));
#55816=CARTESIAN_POINT('Ctrl Pts',(113.770058427842,-1.98291131389037,339.500805015077));
#55817=CARTESIAN_POINT('Ctrl Pts',(113.762284757437,-1.85743111988475,339.556087591312));
#55818=CARTESIAN_POINT('Ctrl Pts',(113.754511087033,-1.72977025920189,339.606060169199));
#55819=CARTESIAN_POINT('Ctrl Pts',(113.746737416628,-1.60042208996249,339.650573319115));
#55820=CARTESIAN_POINT('Ctrl Pts',(113.739325612451,-1.47709510912091,339.693014371192));
#55821=CARTESIAN_POINT('Ctrl Pts',(113.731913808274,-1.35223464861885,339.730492746943));
#55822=CARTESIAN_POINT('Ctrl Pts',(113.724502004097,-1.22627657812866,339.762922297963));
#55823=CARTESIAN_POINT('Ctrl Pts',(113.716726925318,-1.09414492739364,339.796941317882));
#55824=CARTESIAN_POINT('Ctrl Pts',(113.70895184654,-0.960387791449329,339.825511589623));
#55825=CARTESIAN_POINT('Ctrl Pts',(113.701176767762,-0.825494215907046,
339.84847835532));
#55826=CARTESIAN_POINT('Ctrl Pts',(113.693411256713,-0.690766635497214,
339.871416858949));
#55827=CARTESIAN_POINT('Ctrl Pts',(113.685645745664,-0.55490577967201,339.888765511566));
#55828=CARTESIAN_POINT('Ctrl Pts',(113.677880234615,-0.418414858500553,
339.900419580881));
#55829=CARTESIAN_POINT('Ctrl Pts',(113.670122423092,-0.282059268474728,
339.912062095153));
#55830=CARTESIAN_POINT('Ctrl Pts',(113.66236461157,-0.145075243262551,339.918021229332));
#55831=CARTESIAN_POINT('Ctrl Pts',(113.654606800048,-0.00797481856245829,
339.918243534512));
#55832=CARTESIAN_POINT('Ctrl Pts',(113.646854826525,0.129022433720157,339.9184656724));
#55833=CARTESIAN_POINT('Ctrl Pts',(113.639102853002,0.26613552183858,339.912959573724));
#55834=CARTESIAN_POINT('Ctrl Pts',(113.631350879479,0.402849028114068,339.901723750177));
#55835=CARTESIAN_POINT('Ctrl Pts',(113.623602188921,0.539504636138481,339.890492685008));
#55836=CARTESIAN_POINT('Ctrl Pts',(113.615853498364,0.675760610142744,339.873536753138));
#55837=CARTESIAN_POINT('Ctrl Pts',(113.608104807806,0.811103496870204,339.850906531759));
#55838=CARTESIAN_POINT('Ctrl Pts',(113.600357729428,0.946418224379767,339.828281018787));
#55839=CARTESIAN_POINT('Ctrl Pts',(113.59261065105,1.08081985720693,339.799983628991));
#55840=CARTESIAN_POINT('Ctrl Pts',(113.584863572673,1.21380241012255,339.766116529385));
#55841=CARTESIAN_POINT('Ctrl Pts',(113.577116429367,1.34678607755987,339.732249145941));
#55842=CARTESIAN_POINT('Ctrl Pts',(113.569369286061,1.47835026258007,339.692812056047));
#55843=CARTESIAN_POINT('Ctrl Pts',(113.561622142755,1.60800186678905,339.647957945045));
#55844=CARTESIAN_POINT('Ctrl Pts',(113.553873257727,1.73768261943124,339.603093749886));
#55845=CARTESIAN_POINT('Ctrl Pts',(113.546124372699,1.86544956631175,339.552810237981));
#55846=CARTESIAN_POINT('Ctrl Pts',(113.538375487671,1.99082776614344,339.497308958483));
#55847=CARTESIAN_POINT('Ctrl Pts',(113.530618377896,2.11633904369191,339.441748769353));
#55848=CARTESIAN_POINT('Ctrl Pts',(113.522861268121,2.23945615142586,339.380959908041));
#55849=CARTESIAN_POINT('Ctrl Pts',(113.515104158347,2.35972653123695,339.315191045629));
#55850=CARTESIAN_POINT('Ctrl Pts',(113.507342903421,2.48006117969343,339.24938703844));
#55851=CARTESIAN_POINT('Ctrl Pts',(113.499581648494,2.59754573447187,339.178597929188));
#55852=CARTESIAN_POINT('Ctrl Pts',(113.491820393568,2.7117558662681,339.103116277204));
#55853=CARTESIAN_POINT('Ctrl Pts',(113.484046723164,2.82614869705421,339.027513879177));
#55854=CARTESIAN_POINT('Ctrl Pts',(113.476273052759,2.93725632081177,338.947204167224));
#55855=CARTESIAN_POINT('Ctrl Pts',(113.468499382354,3.04468609459395,338.862521151772));
#55856=CARTESIAN_POINT('Ctrl Pts',(113.461087578177,3.14711498656046,338.781780151063));
#55857=CARTESIAN_POINT('Ctrl Pts',(113.453675774,3.24620051196466,338.697064025672));
#55858=CARTESIAN_POINT('Ctrl Pts',(113.446263969823,3.34163435268695,338.608692687864));
#55859=CARTESIAN_POINT('Ctrl Pts',(113.438488891045,3.44174569022572,338.515990007545));
#55860=CARTESIAN_POINT('Ctrl Pts',(113.430713812266,3.53815470249504,338.418971791747));
#55861=CARTESIAN_POINT('Ctrl Pts',(113.422938733488,3.63046659966161,338.317965540997));
#55862=CARTESIAN_POINT('Ctrl Pts',(113.415173222439,3.72266490116185,338.217083584868));
#55863=CARTESIAN_POINT('Ctrl Pts',(113.40740771139,3.81077585804598,338.112223644137));
#55864=CARTESIAN_POINT('Ctrl Pts',(113.399642200341,3.89443908285492,338.003752202235));
#55865=CARTESIAN_POINT('Ctrl Pts',(113.391884388819,3.97801935533294,337.895388310083));
#55866=CARTESIAN_POINT('Ctrl Pts',(113.384126577296,4.05716043458111,337.783420350296));
#55867=CARTESIAN_POINT('Ctrl Pts',(113.376368765774,4.13154028237513,337.668249980345));
#55868=CARTESIAN_POINT('Ctrl Pts',(113.368616792251,4.20586415697486,337.55316627975));
#55869=CARTESIAN_POINT('Ctrl Pts',(113.360864818728,4.27543372065897,337.434885292838));
#55870=CARTESIAN_POINT('Ctrl Pts',(113.353112845205,4.3399687997975,337.313839639924));
#55871=CARTESIAN_POINT('Ctrl Pts',(113.345364154648,4.40447654829175,337.192845249916));
#55872=CARTESIAN_POINT('Ctrl Pts',(113.33761546409,4.46395386934341,337.069088866816));
#55873=CARTESIAN_POINT('Ctrl Pts',(113.329866773532,4.51816543537293,336.943029634643));
#55874=CARTESIAN_POINT('Ctrl Pts',(113.322119695154,4.57236572223335,336.816996630146));
#55875=CARTESIAN_POINT('Ctrl Pts',(113.314372616777,4.62130227894242,336.688662088447));
#55876=CARTESIAN_POINT('Ctrl Pts',(113.306625538399,4.66478720228103,336.558506791751));
#55877=CARTESIAN_POINT('Ctrl Pts',(113.298878395093,4.70827249006515,336.428350404229));
#55878=CARTESIAN_POINT('Ctrl Pts',(113.291131251787,4.74630592948563,336.296373602006));
#55879=CARTESIAN_POINT('Ctrl Pts',(113.283384108481,4.77874907306849,336.163073668839));
#55880=CARTESIAN_POINT('Ctrl Pts',(113.275635223453,4.81119951055879,336.029743767018));
#55881=CARTESIAN_POINT('Ctrl Pts',(113.267886338425,4.83805705886931,335.895090522039));
#55882=CARTESIAN_POINT('Ctrl Pts',(113.260137453397,4.8592341870001,335.759622391975));
#55883=CARTESIAN_POINT('Ctrl Pts',(113.252380343622,4.8804337927535,335.624010474638));
#55884=CARTESIAN_POINT('Ctrl Pts',(113.244623233848,4.89594087385555,335.487582331236));
#55885=CARTESIAN_POINT('Ctrl Pts',(113.236866124073,4.90571963796484,335.350853097729));
#55886=CARTESIAN_POINT('Ctrl Pts',(113.229104869147,4.91550362753301,335.214050800492));
#55887=CARTESIAN_POINT('Ctrl Pts',(113.221343614221,4.91955318919733,335.076947483062));
#55888=CARTESIAN_POINT('Ctrl Pts',(113.213582359295,4.91788471340464,334.940058293643));
#55889=CARTESIAN_POINT('Ctrl Pts',(113.20580868889,4.91621356859443,334.802950126134));
#55890=CARTESIAN_POINT('Ctrl Pts',(113.198035018485,4.90880612905042,334.666057161631));
#55891=CARTESIAN_POINT('Ctrl Pts',(113.190261348081,4.89573078963655,334.529890334172));
#55892=CARTESIAN_POINT('Ctrl Pts',(113.182849543903,4.88326411041796,334.40006210529));
#55893=CARTESIAN_POINT('Ctrl Pts',(113.175437739726,4.86564537656034,334.27089421662));
#55894=CARTESIAN_POINT('Ctrl Pts',(113.168025935549,4.84297676048445,334.142819062328));
#55895=CARTESIAN_POINT('Ctrl Pts',(113.160250856771,4.81919708800866,334.008466563211));
#55896=CARTESIAN_POINT('Ctrl Pts',(113.152475777992,4.78978484903819,333.874892044525));
#55897=CARTESIAN_POINT('Ctrl Pts',(113.144700699214,4.7548018023207,333.742604722791));
#55898=CARTESIAN_POINT('Ctrl Pts',(113.136935188165,4.71986180446933,333.610480189028));
#55899=CARTESIAN_POINT('Ctrl Pts',(113.129169677116,4.67936473779544,333.479640074828));
#55900=CARTESIAN_POINT('Ctrl Pts',(113.121404166067,4.63342375970188,333.350585762905));
#55901=CARTESIAN_POINT('Ctrl Pts',(113.113646354544,4.58752833222185,333.221659408709));
#55902=CARTESIAN_POINT('Ctrl Pts',(113.105888543022,4.53619986520041,333.094515699008));
#55903=CARTESIAN_POINT('Ctrl Pts',(113.0981307315,4.47960184761256,332.969642802518));
#55904=CARTESIAN_POINT('Ctrl Pts',(113.090378757977,4.42304642182784,332.844863876843));
#55905=CARTESIAN_POINT('Ctrl Pts',(113.082626784454,4.36122949932981,332.72235271756));
#55906=CARTESIAN_POINT('Ctrl Pts',(113.074874810931,4.29436326174215,332.602579044327));
#55907=CARTESIAN_POINT('Ctrl Pts',(113.067126120373,4.22752534204577,332.482856095316));
#55908=CARTESIAN_POINT('Ctrl Pts',(113.059377429816,4.15564255049942,332.365868667115));
#55909=CARTESIAN_POINT('Ctrl Pts',(113.051628739258,4.07897364184698,332.252063120882));
#55910=CARTESIAN_POINT('Ctrl Pts',(113.04388166088,4.00232068480135,332.138281252843));
#55911=CARTESIAN_POINT('Ctrl Pts',(113.036134582502,3.92088380960276,332.027680273942));
#55912=CARTESIAN_POINT('Ctrl Pts',(113.028387504125,3.83496563105287,331.920678374846));
#55913=CARTESIAN_POINT('Ctrl Pts',(113.020640360819,3.74904673242589,331.81367557897));
#55914=CARTESIAN_POINT('Ctrl Pts',(113.012893217513,3.6586467002629,331.710272227843));
#55915=CARTESIAN_POINT('Ctrl Pts',(113.005146074207,3.56410878921342,331.610853853675));
#55916=CARTESIAN_POINT('Ctrl Pts',(112.997397189179,3.4695496240345,331.511413128146));
#55917=CARTESIAN_POINT('Ctrl Pts',(112.989648304151,3.37085099810707,331.415959445531));
#55918=CARTESIAN_POINT('Ctrl Pts',(112.981899419123,3.26839311662505,331.324841568354));
#55919=CARTESIAN_POINT('Ctrl Pts',(112.974142309348,3.16582648528896,331.233626977721));
#55920=CARTESIAN_POINT('Ctrl Pts',(112.966385199573,3.05949292031569,331.146757645753));
#55921=CARTESIAN_POINT('Ctrl Pts',(112.958628089799,2.94980624123419,331.064542440621));
#55922=CARTESIAN_POINT('Ctrl Pts',(112.950866834872,2.84006094909857,330.982283302311));
#55923=CARTESIAN_POINT('Ctrl Pts',(112.943105579946,2.72695929468062,330.904683467466));
#55924=CARTESIAN_POINT('Ctrl Pts',(112.93534432502,2.61094334690706,330.832007929261));
#55925=CARTESIAN_POINT('Ctrl Pts',(112.927570654616,2.49474181142657,330.75921613388));
#55926=CARTESIAN_POINT('Ctrl Pts',(112.919796984211,2.37561700651664,330.691364569814));
#55927=CARTESIAN_POINT('Ctrl Pts',(112.912023313806,2.25403559989488,330.628672218089));
#55928=CARTESIAN_POINT('Ctrl Pts',(112.904611509629,2.13811383700298,330.56889821042));
#55929=CARTESIAN_POINT('Ctrl Pts',(112.897199705452,2.01995929589355,330.51381402339));
#55930=CARTESIAN_POINT('Ctrl Pts',(112.889787901275,1.89999087740523,330.463567731325));
#55931=CARTESIAN_POINT('Ctrl Pts',(112.882012822497,1.77414244935842,330.410858718809));
#55932=CARTESIAN_POINT('Ctrl Pts',(112.874237743718,1.64590013672735,330.363307261477));
#55933=CARTESIAN_POINT('Ctrl Pts',(112.86646266494,1.51572557174947,330.321136991357));
#55934=CARTESIAN_POINT('Ctrl Pts',(112.858697153891,1.38571119486112,330.27901861444));
#55935=CARTESIAN_POINT('Ctrl Pts',(112.850931642842,1.25376966498008,330.242268368375));
#55936=CARTESIAN_POINT('Ctrl Pts',(112.843166131793,1.12038384149275,330.211062423645));
#55937=CARTESIAN_POINT('Ctrl Pts',(112.835408320271,0.987130270437835,330.179887419701));
#55938=CARTESIAN_POINT('Ctrl Pts',(112.827650508748,0.852435633725583,330.15424586584));
#55939=CARTESIAN_POINT('Ctrl Pts',(112.819892697226,0.716798916111024,330.1342644568));
#55940=CARTESIAN_POINT('Ctrl Pts',(112.812140723703,0.581264269427758,330.114298084403));
#55941=CARTESIAN_POINT('Ctrl Pts',(112.80438875018,0.444789338107743,330.099983435361));
#55942=CARTESIAN_POINT('Ctrl Pts',(112.796636776657,0.307883943084047,330.091396273879));
#55943=CARTESIAN_POINT('Ctrl Pts',(112.7888880861,0.171036527576332,330.082812749064));
#55944=CARTESIAN_POINT('Ctrl Pts',(112.781139395542,0.0337594002458191,
330.079951911891));
#55945=CARTESIAN_POINT('Ctrl Pts',(112.773390704984,-0.103432057249437,
330.082837721609));
#55946=CARTESIAN_POINT('Ctrl Pts',(112.765643626607,-0.240594970916021,
330.08572293091));
#55947=CARTESIAN_POINT('Ctrl Pts',(112.757896548229,-0.377671859658696,
330.094352400678));
#55948=CARTESIAN_POINT('Ctrl Pts',(112.750149469851,-0.51414729579194,330.108697962635));
#55949=CARTESIAN_POINT('Ctrl Pts',(112.742402326545,-0.650623875720788,
330.123043644822));
#55950=CARTESIAN_POINT('Ctrl Pts',(112.734655183239,-0.786498604253429,
330.14310547389));
#55951=CARTESIAN_POINT('Ctrl Pts',(112.726908039934,-0.921261524342264,
330.168803433282));
#55952=CARTESIAN_POINT('Ctrl Pts',(112.719159154905,-1.05605474199663,330.194507170121));
#55953=CARTESIAN_POINT('Ctrl Pts',(112.711410269877,-1.18973526993767,330.225849485512));
#55954=CARTESIAN_POINT('Ctrl Pts',(112.703661384849,-1.3218040754722,330.26269939221));
#55955=CARTESIAN_POINT('Ctrl Pts',(112.695904275075,-1.45401306020146,330.29958841178));
#55956=CARTESIAN_POINT('Ctrl Pts',(112.6881471653,-1.58460652815471,330.341996595004));
#55957=CARTESIAN_POINT('Ctrl Pts',(112.680390055525,-1.71310080400642,330.389743098502));
#55958=CARTESIAN_POINT('Ctrl Pts',(112.672628800599,-1.84166374309061,330.437515116204));
#55959=CARTESIAN_POINT('Ctrl Pts',(112.664867545673,-1.96812489470892,330.49063098701));
#55960=CARTESIAN_POINT('Ctrl Pts',(112.657106290747,-2.09202219158389,330.54886236874));
#55961=CARTESIAN_POINT('Ctrl Pts',(112.649332620342,-2.21611768375592,330.607186901703));
#55962=CARTESIAN_POINT('Ctrl Pts',(112.641558949937,-2.33764077884499,330.67064311693));
#55963=CARTESIAN_POINT('Ctrl Pts',(112.633785279533,-2.45615479035629,330.738957086779));
#55964=CARTESIAN_POINT('Ctrl Pts',(112.626373475356,-2.56915194611876,330.804091024896));
#55965=CARTESIAN_POINT('Ctrl Pts',(112.618961671179,-2.67941361606295,330.8736404849));
#55966=CARTESIAN_POINT('Ctrl Pts',(112.611549867002,-2.78658859004902,330.947333335653));
#55967=CARTESIAN_POINT('Ctrl Pts',(112.603813727223,-2.89845346933367,331.024250936349));
#55968=CARTESIAN_POINT('Ctrl Pts',(112.596077587444,-3.00731676404034,331.105931343334));
#55969=CARTESIAN_POINT('Ctrl Pts',(112.588341447665,-3.11274309098139,331.19211167285));
#55970=CARTESIAN_POINT('Ctrl Pts',(112.580614850363,-3.21803937524821,331.278185699501));
#55971=CARTESIAN_POINT('Ctrl Pts',(112.572888253061,-3.31990682244749,331.368748359051));
#55972=CARTESIAN_POINT('Ctrl Pts',(112.56516165576,-3.41793826010091,331.463493091674));
#55973=CARTESIAN_POINT('Ctrl Pts',(112.557442693122,-3.51587283271895,331.55814420686));
#55974=CARTESIAN_POINT('Ctrl Pts',(112.549723730485,-3.6099786550814,331.656968900253));
#55975=CARTESIAN_POINT('Ctrl Pts',(112.542004767847,-3.69988128146181,331.759620151033));
#55976=CARTESIAN_POINT('Ctrl Pts',(112.534291539137,-3.7897171248876,331.862195148715));
#55977=CARTESIAN_POINT('Ctrl Pts',(112.526578310427,-3.8753557266531,331.968590750737));
#55978=CARTESIAN_POINT('Ctrl Pts',(112.518865081717,-3.95645950875015,332.07842316238));
#55979=CARTESIAN_POINT('Ctrl Pts',(112.511154984209,-4.03753036659233,332.188210987318));
#55980=CARTESIAN_POINT('Ctrl Pts',(112.5034448867,-4.11406983101611,332.301432530293));
#55981=CARTESIAN_POINT('Ctrl Pts',(112.495734789192,-4.18578082841537,332.417671221752));
#55982=CARTESIAN_POINT('Ctrl Pts',(112.4880261404,-4.2574783514216,332.533888072128));
#55983=CARTESIAN_POINT('Ctrl Pts',(112.480317491608,-4.32434900432464,332.653120607296));
#55984=CARTESIAN_POINT('Ctrl Pts',(112.472608842816,-4.38613951426719,332.774923995931));
#55985=CARTESIAN_POINT('Ctrl Pts',(112.464899930553,-4.44793213612624,332.896731547642));
#55986=CARTESIAN_POINT('Ctrl Pts',(112.457191018289,-4.5046440908141,333.021109775104));
#55987=CARTESIAN_POINT('Ctrl Pts',(112.449482106026,-4.55606868309945,333.147590429365));
#55988=CARTESIAN_POINT('Ctrl Pts',(112.441771218253,-4.60750645360872,333.274103495946));
#55989=CARTESIAN_POINT('Ctrl Pts',(112.43406033048,-4.65365401753412,333.402719695066));
#55990=CARTESIAN_POINT('Ctrl Pts',(112.426349442707,-4.69435348447759,333.532952480227));
#55991=CARTESIAN_POINT('Ctrl Pts',(112.418630419675,-4.73509589079766,333.66332266558));
#55992=CARTESIAN_POINT('Ctrl Pts',(112.410911396643,-4.77037860415737,333.795312465115));
#55993=CARTESIAN_POINT('Ctrl Pts',(112.403192373611,-4.80009401809788,333.928421500812));
#55994=CARTESIAN_POINT('Ctrl Pts',(112.395468925079,-4.82982646859386,334.061606851095));
#55995=CARTESIAN_POINT('Ctrl Pts',(112.387745476547,-4.85398519231118,334.195912327251));
#55996=CARTESIAN_POINT('Ctrl Pts',(112.380022028015,-4.87251422816711,334.330830246642));
#55997=CARTESIAN_POINT('Ctrl Pts',(112.372287044735,-4.89107093660431,334.465949662059));
#55998=CARTESIAN_POINT('Ctrl Pts',(112.364552061455,-4.9039811281351,334.601682954669));
#55999=CARTESIAN_POINT('Ctrl Pts',(112.356817078175,-4.91124089480556,334.737519647041));
#56000=CARTESIAN_POINT('Ctrl Pts',(112.351817203424,-4.91593359067253,334.825324161127));
#56001=CARTESIAN_POINT('Ctrl Pts',(112.346817328674,-4.91826643516687,334.913171884236));
#56002=CARTESIAN_POINT('Ctrl Pts',(112.341817453923,-4.91824991282565,335.000926007804));
#56003=CARTESIAN_POINT('',(110.591817843044,-4.91738553598639,334.995487657965));
#56004=CARTESIAN_POINT('Ctrl Pts',(112.341817376508,-4.92614104176129,335.000928854464));
#56005=CARTESIAN_POINT('Ctrl Pts',(112.338982195248,-4.92627011657859,335.050769735367));
#56006=CARTESIAN_POINT('Ctrl Pts',(112.243401002563,-4.90298212628779,336.73090936613));
#56007=CARTESIAN_POINT('Ctrl Pts',(112.055073798454,-2.99650838422388,339.984514657387));
#56008=CARTESIAN_POINT('Ctrl Pts',(111.776835764179,2.57000208903517,340.2172347205));
#56009=CARTESIAN_POINT('Ctrl Pts',(111.498597729906,5.7780595783553,335.662175486868));
#56010=CARTESIAN_POINT('Ctrl Pts',(111.220359695631,3.68367707663835,330.499447582632));
#56011=CARTESIAN_POINT('Ctrl Pts',(110.942121661358,-1.7911615073251,329.466810203769));
#56012=CARTESIAN_POINT('Ctrl Pts',(110.732607789333,-4.6760006404016,332.512771583302));
#56013=CARTESIAN_POINT('Ctrl Pts',(110.615839928733,-4.92075371318481,334.571140323605));
#56014=CARTESIAN_POINT('Ctrl Pts',(110.591818079557,-4.91694833721634,334.995483880473));
#56015=CARTESIAN_POINT('',(108.84181737648,-4.91824982733306,335.001303241486));
#56016=CARTESIAN_POINT('Ctrl Pts',(110.591817376508,-4.91824793686326,334.995495109295));
#56017=CARTESIAN_POINT('Ctrl Pts',(110.584146126918,-4.91837209122975,335.131041562429));
#56018=CARTESIAN_POINT('Ctrl Pts',(110.576474877328,-4.9128885595775,335.266724912895));
#56019=CARTESIAN_POINT('Ctrl Pts',(110.568803627738,-4.90179024276939,335.402039150321));
#56020=CARTESIAN_POINT('Ctrl Pts',(110.561136543147,-4.89069795164023,335.537279920737));
#56021=CARTESIAN_POINT('Ctrl Pts',(110.553469458557,-4.87399697080814,335.672151579091));
#56022=CARTESIAN_POINT('Ctrl Pts',(110.545802373967,-4.85173227595791,335.806149480511));
#56023=CARTESIAN_POINT('Ctrl Pts',(110.538137415738,-4.82947375591737,335.940110219439));
#56024=CARTESIAN_POINT('Ctrl Pts',(110.530472457509,-4.80165465517224,336.073197288958));
#56025=CARTESIAN_POINT('Ctrl Pts',(110.52280749928,-4.7683716047274,336.204912985128));
#56026=CARTESIAN_POINT('Ctrl Pts',(110.515142921812,-4.73509020763609,336.336622138249));
#56027=CARTESIAN_POINT('Ctrl Pts',(110.507478344344,-4.69634549859154,336.466959665636));
#56028=CARTESIAN_POINT('Ctrl Pts',(110.499813766876,-4.65228472135179,336.595440357386));
#56029=CARTESIAN_POINT('Ctrl Pts',(110.492147825117,-4.60821610131729,336.723943918631));
#56030=CARTESIAN_POINT('Ctrl Pts',(110.484481883359,-4.55882966116891,336.850589608606));
#56031=CARTESIAN_POINT('Ctrl Pts',(110.4768159416,-4.50432160298151,336.974910114262));
#56032=CARTESIAN_POINT('Ctrl Pts',(110.469142147348,-4.44975771027771,337.099357965774));
#56033=CARTESIAN_POINT('Ctrl Pts',(110.461468353096,-4.39006188184791,337.221475508781));
#56034=CARTESIAN_POINT('Ctrl Pts',(110.453794558845,-4.32547749756932,337.34081769485));
#56035=CARTESIAN_POINT('Ctrl Pts',(110.446116831348,-4.26086001021524,337.460221050401));
#56036=CARTESIAN_POINT('Ctrl Pts',(110.438439103852,-4.19134918162487,337.576845872649));
#56037=CARTESIAN_POINT('Ctrl Pts',(110.430761376355,-4.11723229695039,337.69027531592));
#56038=CARTESIAN_POINT('Ctrl Pts',(110.423071357589,-4.04299675859383,337.803886348328));
#56039=CARTESIAN_POINT('Ctrl Pts',(110.415381338822,-3.96414066467786,337.914291456165));
#56040=CARTESIAN_POINT('Ctrl Pts',(110.407691320056,-3.88099269015923,338.021105559465));
#56041=CARTESIAN_POINT('Ctrl Pts',(110.400342744307,-3.80153655258109,338.123177030673));
#56042=CARTESIAN_POINT('Ctrl Pts',(110.392994168559,-3.71816169532594,338.221969332601));
#56043=CARTESIAN_POINT('Ctrl Pts',(110.38564559281,-3.63118545644224,338.317178807876));
#56044=CARTESIAN_POINT('Ctrl Pts',(110.377870514032,-3.53916121496859,338.417914133474));
#56045=CARTESIAN_POINT('Ctrl Pts',(110.370095435253,-3.44279652465389,338.514976372805));
#56046=CARTESIAN_POINT('Ctrl Pts',(110.362320356475,-3.34241621146445,338.607968532546));
#56047=CARTESIAN_POINT('Ctrl Pts',(110.354554845426,-3.24215942264098,338.700846259513));
#56048=CARTESIAN_POINT('Ctrl Pts',(110.346789334377,-3.1378971270698,338.789663609256));
#56049=CARTESIAN_POINT('Ctrl Pts',(110.339023823328,-3.02999336514519,338.874057726683));
#56050=CARTESIAN_POINT('Ctrl Pts',(110.331266011805,-2.92219659011453,338.958368167098));
#56051=CARTESIAN_POINT('Ctrl Pts',(110.323508200283,-2.81076583978284,339.038263863628));
#56052=CARTESIAN_POINT('Ctrl Pts',(110.315750388761,-2.69610058685823,339.113420071916));
#56053=CARTESIAN_POINT('Ctrl Pts',(110.307998415238,-2.58152162317276,339.188519722774));
#56054=CARTESIAN_POINT('Ctrl Pts',(110.300246441715,-2.46371332737801,339.258886771156));
#56055=CARTESIAN_POINT('Ctrl Pts',(110.292494468192,-2.34310641714275,339.324238127167));
#56056=CARTESIAN_POINT('Ctrl Pts',(110.284745777634,-2.22255058400558,339.38956180684));
#56057=CARTESIAN_POINT('Ctrl Pts',(110.276997087077,-2.09919883668719,339.449873833094));
#56058=CARTESIAN_POINT('Ctrl Pts',(110.269248396519,-1.97350871892266,339.504935781877));
#56059=CARTESIAN_POINT('Ctrl Pts',(110.261501318141,-1.84784475203692,339.559986274561));
#56060=CARTESIAN_POINT('Ctrl Pts',(110.253754239763,-1.71984374022442,339.609788705735));
#56061=CARTESIAN_POINT('Ctrl Pts',(110.246007161386,-1.58998518530124,339.654151928442));
#56062=CARTESIAN_POINT('Ctrl Pts',(110.23826001808,-1.4601255420383,339.698515522956));
#56063=CARTESIAN_POINT('Ctrl Pts',(110.230512874774,-1.32840869449841,339.737439691714));
#56064=CARTESIAN_POINT('Ctrl Pts',(110.222765731468,-1.19533097978101,339.770782630898));
#56065=CARTESIAN_POINT('Ctrl Pts',(110.21501684644,-1.06222334636803,339.804133066282));
#56066=CARTESIAN_POINT('Ctrl Pts',(110.207267961412,-0.927754616047893,
339.831899680242));
#56067=CARTESIAN_POINT('Ctrl Pts',(110.199519076384,-0.792432643955706,
339.853991508778));
#56068=CARTESIAN_POINT('Ctrl Pts',(110.191761966609,-0.656967039724294,
339.87610678581));
#56069=CARTESIAN_POINT('Ctrl Pts',(110.184004856834,-0.520646770997407,
339.892535182283));
#56070=CARTESIAN_POINT('Ctrl Pts',(110.17624774706,-0.383986720176763,339.903237426561));
#56071=CARTESIAN_POINT('Ctrl Pts',(110.168486492134,-0.247253642594687,
339.913945389776));
#56072=CARTESIAN_POINT('Ctrl Pts',(110.160725237207,-0.110180811545775,
339.918921089554));
#56073=CARTESIAN_POINT('Ctrl Pts',(110.152963982281,0.0267165257919835,
339.918177435773));
#56074=CARTESIAN_POINT('Ctrl Pts',(110.145190311877,0.163832854254837,339.917432592389));
#56075=CARTESIAN_POINT('Ctrl Pts',(110.137416641472,0.300772737376946,339.910950131324));
#56076=CARTESIAN_POINT('Ctrl Pts',(110.129642971067,0.437024790724611,339.898794994158));
#56077=CARTESIAN_POINT('Ctrl Pts',(110.12223116689,0.566934278208219,339.887205681552));
#56078=CARTESIAN_POINT('Ctrl Pts',(110.114819362713,0.696218246345673,339.870459970809));
#56079=CARTESIAN_POINT('Ctrl Pts',(110.107407558536,0.824443620590572,339.848657110888));
#56080=CARTESIAN_POINT('Ctrl Pts',(110.099632479758,0.958953702391189,339.825785627855));
#56081=CARTESIAN_POINT('Ctrl Pts',(110.091857400979,1.09272387351054,339.797276451051));
#56082=CARTESIAN_POINT('Ctrl Pts',(110.084082322201,1.22524451182462,339.763187897695));
#56083=CARTESIAN_POINT('Ctrl Pts',(110.076316811152,1.3576020750564,339.729141292473));
#56084=CARTESIAN_POINT('Ctrl Pts',(110.068551300103,1.48871278999301,339.689529068073));
#56085=CARTESIAN_POINT('Ctrl Pts',(110.060785789054,1.61807452090086,339.644460992119));
#56086=CARTESIAN_POINT('Ctrl Pts',(110.053027977532,1.74730798927606,339.599437601292));
#56087=CARTESIAN_POINT('Ctrl Pts',(110.045270166009,1.87479555788748,339.548969251874));
#56088=CARTESIAN_POINT('Ctrl Pts',(110.037512354487,2.00004796467262,339.493216131181));
#56089=CARTESIAN_POINT('Ctrl Pts',(110.029760380964,2.12520611505045,339.43750496648));
#56090=CARTESIAN_POINT('Ctrl Pts',(110.022008407441,2.24813209594357,339.376517104756));
#56091=CARTESIAN_POINT('Ctrl Pts',(110.014256433918,2.36835476497503,339.3104615495));
#56092=CARTESIAN_POINT('Ctrl Pts',(110.00650774336,2.48852651963404,339.244433968812));
#56093=CARTESIAN_POINT('Ctrl Pts',(109.998759052803,2.60599689760791,339.173343151008));
#56094=CARTESIAN_POINT('Ctrl Pts',(109.991010362245,2.72031779985406,339.097444829439));
#56095=CARTESIAN_POINT('Ctrl Pts',(109.983263283867,2.83461491668183,339.02156229915));
#56096=CARTESIAN_POINT('Ctrl Pts',(109.97551620549,2.94576353573271,338.940874470706));
#56097=CARTESIAN_POINT('Ctrl Pts',(109.967769127112,3.05334343150593,338.855681126828));
#56098=CARTESIAN_POINT('Ctrl Pts',(109.960021983806,3.16092422890206,338.770487068948));
#56099=CARTESIAN_POINT('Ctrl Pts',(109.9522748405,3.26493593693671,338.68078766298));
#56100=CARTESIAN_POINT('Ctrl Pts',(109.944527697194,3.36499071326769,338.586923551196));
#56101=CARTESIAN_POINT('Ctrl Pts',(109.936778812166,3.46506798403668,338.493038336766));
#56102=CARTESIAN_POINT('Ctrl Pts',(109.929029927138,3.56118626788049,338.394986820737));
#56103=CARTESIAN_POINT('Ctrl Pts',(109.92128104211,3.65299424167759,338.293146843487));
#56104=CARTESIAN_POINT('Ctrl Pts',(109.913523932335,3.74489966140663,338.191198772233));
#56105=CARTESIAN_POINT('Ctrl Pts',(109.905766822561,3.83248536994826,338.085454497988));
#56106=CARTESIAN_POINT('Ctrl Pts',(109.898009712786,3.91543971053541,337.976325744213));
#56107=CARTESIAN_POINT('Ctrl Pts',(109.89024845786,3.99843837926987,337.86713867552));
#56108=CARTESIAN_POINT('Ctrl Pts',(109.882487202933,4.07680052548278,337.754563844226));
#56109=CARTESIAN_POINT('Ctrl Pts',(109.874725948007,4.15025817555468,337.63904151895));
#56110=CARTESIAN_POINT('Ctrl Pts',(109.866952277603,4.2238333339269,337.523334395602));
#56111=CARTESIAN_POINT('Ctrl Pts',(109.859178607198,4.29248812248646,337.404670694755));
#56112=CARTESIAN_POINT('Ctrl Pts',(109.851404936793,4.35600041253313,337.283515594103));
#56113=CARTESIAN_POINT('Ctrl Pts',(109.843993132616,4.41655619019804,337.168000292534));
#56114=CARTESIAN_POINT('Ctrl Pts',(109.836581328439,4.4724373382522,337.050220580623));
#56115=CARTESIAN_POINT('Ctrl Pts',(109.829169524262,4.52349295577554,336.9305943493));
#56116=CARTESIAN_POINT('Ctrl Pts',(109.821394445484,4.57705096120053,336.805104880032));
#56117=CARTESIAN_POINT('Ctrl Pts',(109.813619366705,4.62546770153305,336.677186737851));
#56118=CARTESIAN_POINT('Ctrl Pts',(109.805844287927,4.6685164311926,336.547300033667));
#56119=CARTESIAN_POINT('Ctrl Pts',(109.798078776878,4.71151218664973,336.41757316334));
#56120=CARTESIAN_POINT('Ctrl Pts',(109.790313265829,4.74915295304581,336.285882918453));
#56121=CARTESIAN_POINT('Ctrl Pts',(109.78254775478,4.7812593018591,336.152710957216));
#56122=CARTESIAN_POINT('Ctrl Pts',(109.774789943257,4.8133338171341,336.019671036366));
#56123=CARTESIAN_POINT('Ctrl Pts',(109.767032131735,4.83988474402424,335.885152700348));
#56124=CARTESIAN_POINT('Ctrl Pts',(109.759274320213,4.8607820196859,335.749654066619));
#56125=CARTESIAN_POINT('Ctrl Pts',(109.75152234669,4.88166356948478,335.614257399909));
#56126=CARTESIAN_POINT('Ctrl Pts',(109.743770373167,4.8968998771944,335.477882288605));
#56127=CARTESIAN_POINT('Ctrl Pts',(109.736018399644,4.90641173613487,335.341038030164));
#56128=CARTESIAN_POINT('Ctrl Pts',(109.728269709086,4.91591956679747,335.204251725347));
#56129=CARTESIAN_POINT('Ctrl Pts',(109.720521018529,4.91970774342025,335.066997057684));
#56130=CARTESIAN_POINT('Ctrl Pts',(109.712772327971,4.91774882553059,334.929789235209));
#56131=CARTESIAN_POINT('Ctrl Pts',(109.705025249593,4.91579031521016,334.792609959969));
#56132=CARTESIAN_POINT('Ctrl Pts',(109.697278171215,4.90808709434732,334.65547790112));
#56133=CARTESIAN_POINT('Ctrl Pts',(109.689531092838,4.8946638484961,334.518908664882));
#56134=CARTESIAN_POINT('Ctrl Pts',(109.681783949532,4.88124049014515,334.382338284063));
#56135=CARTESIAN_POINT('Ctrl Pts',(109.674036806226,4.86209704942166,334.246331124264));
#56136=CARTESIAN_POINT('Ctrl Pts',(109.66628966292,4.83731009593355,334.111397671464));
#56137=CARTESIAN_POINT('Ctrl Pts',(109.658540777892,4.81251756981203,333.976433882759));
#56138=CARTESIAN_POINT('Ctrl Pts',(109.650791892864,4.7820790767997,333.842544665763));
#56139=CARTESIAN_POINT('Ctrl Pts',(109.643043007836,4.74612222983168,333.710229926693));
#56140=CARTESIAN_POINT('Ctrl Pts',(109.635285898061,4.71012721789476,333.577774747392));
#56141=CARTESIAN_POINT('Ctrl Pts',(109.627528788286,4.66860225428536,333.446897762121));
#56142=CARTESIAN_POINT('Ctrl Pts',(109.619771678512,4.6217249106862,333.318083856893));
#56143=CARTESIAN_POINT('Ctrl Pts',(109.612010423585,4.57482251733343,333.189201117633));
#56144=CARTESIAN_POINT('Ctrl Pts',(109.604249168659,4.52256219375378,333.062384016344));
#56145=CARTESIAN_POINT('Ctrl Pts',(109.596487913733,4.46516915532161,332.938096152372));
#56146=CARTESIAN_POINT('Ctrl Pts',(109.588714243328,4.40768430673237,332.813609468323));
#56147=CARTESIAN_POINT('Ctrl Pts',(109.580940572924,4.3450505146111,332.691660454487));
#56148=CARTESIAN_POINT('Ctrl Pts',(109.573166902519,4.27753875022061,332.572687637971));
#56149=CARTESIAN_POINT('Ctrl Pts',(109.565755098342,4.21316967470548,332.459253034687));
#56150=CARTESIAN_POINT('Ctrl Pts',(109.558343294165,4.14436669791148,332.348524024804));
#56151=CARTESIAN_POINT('Ctrl Pts',(109.550931489988,4.0713995720919,332.240853648885));
#56152=CARTESIAN_POINT('Ctrl Pts',(109.54315641121,3.99485611007735,332.127906027109));
#56153=CARTESIAN_POINT('Ctrl Pts',(109.535381332431,3.91348809164955,332.017967510562));
#56154=CARTESIAN_POINT('Ctrl Pts',(109.527606253653,3.82755972884398,331.911477766855));
#56155=CARTESIAN_POINT('Ctrl Pts',(109.519840742604,3.74173710635947,331.805119065558));
#56156=CARTESIAN_POINT('Ctrl Pts',(109.512075231555,3.65136554846989,331.702200994172));
#56157=CARTESIAN_POINT('Ctrl Pts',(109.504309720506,3.55675299277143,331.603135090865));
#56158=CARTESIAN_POINT('Ctrl Pts',(109.496551908984,3.4622342456972,331.50416741169));
#56159=CARTESIAN_POINT('Ctrl Pts',(109.488794097461,3.36348313714986,331.409044580549));
#56160=CARTESIAN_POINT('Ctrl Pts',(109.481036285939,3.26084816025649,331.318145530001));
#56161=CARTESIAN_POINT('Ctrl Pts',(109.473284312416,3.15829041943749,331.22731488387));
#56162=CARTESIAN_POINT('Ctrl Pts',(109.465532338893,3.05185491926622,331.140701949735));
#56163=CARTESIAN_POINT('Ctrl Pts',(109.45778036537,2.94192707556095,331.05864894426));
#56164=CARTESIAN_POINT('Ctrl Pts',(109.450031674812,2.83204578636343,330.976630688282));
#56165=CARTESIAN_POINT('Ctrl Pts',(109.442282984255,2.71867540786182,330.8991687534));
#56166=CARTESIAN_POINT('Ctrl Pts',(109.434534293697,2.60223433987015,330.826565023521));
#56167=CARTESIAN_POINT('Ctrl Pts',(109.426787215319,2.48581749841538,330.753976399454));
#56168=CARTESIAN_POINT('Ctrl Pts',(109.419040136942,2.36633156972565,330.68624417654));
#56169=CARTESIAN_POINT('Ctrl Pts',(109.411293058564,2.24422349684125,330.62362662028));
#56170=CARTESIAN_POINT('Ctrl Pts',(109.403545915258,2.12211440057376,330.561008539224));
#56171=CARTESIAN_POINT('Ctrl Pts',(109.395798771952,1.99738346408768,330.503505388679));
#56172=CARTESIAN_POINT('Ctrl Pts',(109.388051628646,1.87050140214203,330.451329032884));
#56173=CARTESIAN_POINT('Ctrl Pts',(109.380302743618,1.74359081441508,330.399140946736));
#56174=CARTESIAN_POINT('Ctrl Pts',(109.37255385859,1.61452850031306,330.352282187009));
#56175=CARTESIAN_POINT('Ctrl Pts',(109.364804973562,1.48380390032075,330.310915969201));
#56176=CARTESIAN_POINT('Ctrl Pts',(109.357047863787,1.35294054788719,330.269505844862));
#56177=CARTESIAN_POINT('Ctrl Pts',(109.349290754013,1.220411758324,330.233600026208));
#56178=CARTESIAN_POINT('Ctrl Pts',(109.341533644238,1.08672137685137,330.203311589065));
#56179=CARTESIAN_POINT('Ctrl Pts',(109.333772389312,0.952959555513651,330.173006966751));
#56180=CARTESIAN_POINT('Ctrl Pts',(109.326011134386,0.818035289730003,330.148325777502));
#56181=CARTESIAN_POINT('Ctrl Pts',(109.318249879459,0.68246030704377,330.129329513115));
#56182=CARTESIAN_POINT('Ctrl Pts',(109.310476209055,0.546668448568562,330.110302860896));
#56183=CARTESIAN_POINT('Ctrl Pts',(109.30270253865,0.410224182323015,330.096979344104));
#56184=CARTESIAN_POINT('Ctrl Pts',(109.294928868246,0.273642913204627,330.089368409405));
#56185=CARTESIAN_POINT('Ctrl Pts',(109.287517064068,0.143419535021954,330.082111765546));
#56186=CARTESIAN_POINT('Ctrl Pts',(109.280105259891,0.0130719096515187,
330.080047835702));
#56187=CARTESIAN_POINT('Ctrl Pts',(109.272693455714,-0.116957105141296,
330.083140829955));
#56188=CARTESIAN_POINT('Ctrl Pts',(109.264918376936,-0.253359229284194,
330.086385421069));
#56189=CARTESIAN_POINT('Ctrl Pts',(109.257143298157,-0.389841776951017,
330.095315484102));
#56190=CARTESIAN_POINT('Ctrl Pts',(109.249368219379,-0.525892041975531,
330.109946766886));
#56191=CARTESIAN_POINT('Ctrl Pts',(109.24160270833,-0.661774888487457,330.124560044946));
#56192=CARTESIAN_POINT('Ctrl Pts',(109.233837197281,-0.797226125869462,
330.144860542103));
#56193=CARTESIAN_POINT('Ctrl Pts',(109.226071686232,-0.931733040194316,
330.170812013981));
#56194=CARTESIAN_POINT('Ctrl Pts',(109.218313874709,-1.06610659052192,330.196737754899));
#56195=CARTESIAN_POINT('Ctrl Pts',(109.210556063187,-1.19953729975662,330.228303246762));
#56196=CARTESIAN_POINT('Ctrl Pts',(109.202798251665,-1.33151792579958,330.265420496414));
#56197=CARTESIAN_POINT('Ctrl Pts',(109.195046278142,-1.46339923223611,330.302509814159));
#56198=CARTESIAN_POINT('Ctrl Pts',(109.187294304619,-1.59383225276587,330.345142468445));
#56199=CARTESIAN_POINT('Ctrl Pts',(109.179542331096,-1.72232063948017,330.393179547961));
#56200=CARTESIAN_POINT('Ctrl Pts',(109.171793640538,-1.8507546112865,330.441196283746));
#56201=CARTESIAN_POINT('Ctrl Pts',(109.164044949981,-1.97724522190571,330.494612755949));
#56202=CARTESIAN_POINT('Ctrl Pts',(109.156296259423,-2.1013121905709,330.553240489946));
#56203=CARTESIAN_POINT('Ctrl Pts',(109.148549181045,-2.22535334606703,330.611856025953));
#56204=CARTESIAN_POINT('Ctrl Pts',(109.140802102668,-2.3469715094348,330.675680500215));
#56205=CARTESIAN_POINT('Ctrl Pts',(109.13305502429,-2.46570763317888,330.744477831078));
#56206=CARTESIAN_POINT('Ctrl Pts',(109.125307880984,-2.58444475204605,330.813275738529));
#56207=CARTESIAN_POINT('Ctrl Pts',(109.117560737678,-2.70029944490754,330.887046389749));
#56208=CARTESIAN_POINT('Ctrl Pts',(109.109813594372,-2.81283881983988,330.96550860255));
#56209=CARTESIAN_POINT('Ctrl Pts',(109.102064709344,-2.92540349601252,331.043988455321));
#56210=CARTESIAN_POINT('Ctrl Pts',(109.094315824316,-3.03465105050955,331.12716174503));
#56211=CARTESIAN_POINT('Ctrl Pts',(109.086566939288,-3.14017936760529,331.214705216002));
#56212=CARTESIAN_POINT('Ctrl Pts',(109.078809829513,-3.24581969354754,331.302341606518));
#56213=CARTESIAN_POINT('Ctrl Pts',(109.071052719739,-3.34773259500456,331.39435719429));
#56214=CARTESIAN_POINT('Ctrl Pts',(109.063295609964,-3.44555032454047,331.490389476942));
#56215=CARTESIAN_POINT('Ctrl Pts',(109.055534355038,-3.5434203247435,331.586473076175));
#56216=CARTESIAN_POINT('Ctrl Pts',(109.047773100111,-3.63719052550113,331.686577362048));
#56217=CARTESIAN_POINT('Ctrl Pts',(109.040011845185,-3.72653229191451,331.790305288689));
#56218=CARTESIAN_POINT('Ctrl Pts',(109.032238174781,-3.81601697603767,331.894199146208));
#56219=CARTESIAN_POINT('Ctrl Pts',(109.024464504376,-3.90105882718815,332.001727921166));
#56220=CARTESIAN_POINT('Ctrl Pts',(109.016690833971,-3.98137098630086,332.112463310719));
#56221=CARTESIAN_POINT('Ctrl Pts',(109.009279029794,-4.05794459508521,332.218043941249));
#56222=CARTESIAN_POINT('Ctrl Pts',(109.001867225617,-4.13021877715577,332.3265391294));
#56223=CARTESIAN_POINT('Ctrl Pts',(108.99445542144,-4.1979839732698,332.437557098652));
#56224=CARTESIAN_POINT('Ctrl Pts',(108.98643752161,-4.27129062592677,332.557653492927));
#56225=CARTESIAN_POINT('Ctrl Pts',(108.978419621781,-4.33954024120941,332.681062081186));
#56226=CARTESIAN_POINT('Ctrl Pts',(108.970401721951,-4.40243049178079,332.807332941932));
#56227=CARTESIAN_POINT('Ctrl Pts',(108.962395699245,-4.46522758138862,332.933416754368));
#56228=CARTESIAN_POINT('Ctrl Pts',(108.954389676539,-4.5226809591057,333.062354077842));
#56229=CARTESIAN_POINT('Ctrl Pts',(108.946383653833,-4.57453223890482,333.193667290414));
#56230=CARTESIAN_POINT('Ctrl Pts',(108.9383882249,-4.62631490776866,333.324806745995));
#56231=CARTESIAN_POINT('Ctrl Pts',(108.930392795968,-4.67251011317925,333.458315498203));
#56232=CARTESIAN_POINT('Ctrl Pts',(108.922397367035,-4.71290597159602,333.593692649029));
#56233=CARTESIAN_POINT('Ctrl Pts',(108.91441396919,-4.75324104451714,333.728866091665));
#56234=CARTESIAN_POINT('Ctrl Pts',(108.906430571345,-4.78779406588513,333.865901986915));
#56235=CARTESIAN_POINT('Ctrl Pts',(108.8984471735,-4.816401918241,334.004281352758));
#56236=CARTESIAN_POINT('Ctrl Pts',(108.890470898944,-4.84498424487213,334.14253724783));
#56237=CARTESIAN_POINT('Ctrl Pts',(108.882494624389,-4.86763189451933,334.282133877477));
#56238=CARTESIAN_POINT('Ctrl Pts',(108.874518349833,-4.88423188169256,334.42253832304));
#56239=CARTESIAN_POINT('Ctrl Pts',(108.866549434797,-4.90081655245036,334.562813220742));
#56240=CARTESIAN_POINT('Ctrl Pts',(108.858580519762,-4.91136464155386,334.703894094417));
#56241=CARTESIAN_POINT('Ctrl Pts',(108.850611604726,-4.91581450105162,334.845239366276));
#56242=CARTESIAN_POINT('Ctrl Pts',(108.84768019532,-4.91745140644305,334.897234005135));
#56243=CARTESIAN_POINT('Ctrl Pts',(108.844748785915,-4.91826361663179,334.949264349273));
#56244=CARTESIAN_POINT('Ctrl Pts',(108.841817376509,-4.91824982733319,335.001303240966));
#56245=CARTESIAN_POINT('',(107.091817376565,-4.9182483968572,335.00397105925));
#56246=CARTESIAN_POINT('Ctrl Pts',(108.84181737648,-4.91824982733305,335.001303241486));
#56247=CARTESIAN_POINT('Ctrl Pts',(108.833518067776,-4.91821078751442,335.148634018929));
#56248=CARTESIAN_POINT('Ctrl Pts',(108.825218759072,-4.91154738041952,335.295783482802));
#56249=CARTESIAN_POINT('Ctrl Pts',(108.816919450368,-4.89833361422636,335.442166107068));
#56250=CARTESIAN_POINT('Ctrl Pts',(108.808527611768,-4.88497252631503,335.590180767153));
#56251=CARTESIAN_POINT('Ctrl Pts',(108.800135773168,-4.86491422082103,335.737411076446));
#56252=CARTESIAN_POINT('Ctrl Pts',(108.791743934568,-4.83828747072515,335.88326519977));
#56253=CARTESIAN_POINT('Ctrl Pts',(108.783399897589,-4.81181239202047,336.028288508303));
#56254=CARTESIAN_POINT('Ctrl Pts',(108.775055860611,-4.77884366846353,336.171951004413));
#56255=CARTESIAN_POINT('Ctrl Pts',(108.766711823632,-4.7395575456705,336.313688446237));
#56256=CARTESIAN_POINT('Ctrl Pts',(108.758296084221,-4.69993382722955,336.456643873959));
#56257=CARTESIAN_POINT('Ctrl Pts',(108.74988034481,-4.6538837589856,336.597640722434));
#56258=CARTESIAN_POINT('Ctrl Pts',(108.741464605399,-4.60163695354992,336.736122233664));
#56259=CARTESIAN_POINT('Ctrl Pts',(108.733048865988,-4.54939014811427,336.874603744894));
#56260=CARTESIAN_POINT('Ctrl Pts',(108.724633126577,-4.49094678658842,337.010569666897));
#56261=CARTESIAN_POINT('Ctrl Pts',(108.716217387166,-4.42658291127038,337.143489396323));
#56262=CARTESIAN_POINT('Ctrl Pts',(108.708442308388,-4.36711883133142,337.266290414394));
#56263=CARTESIAN_POINT('Ctrl Pts',(108.700667229609,-4.30244684778947,337.386809153136));
#56264=CARTESIAN_POINT('Ctrl Pts',(108.692892150831,-4.23276504070697,337.504572453068));
#56265=CARTESIAN_POINT('Ctrl Pts',(108.685126639782,-4.16316898152424,337.622190837763));
#56266=CARTESIAN_POINT('Ctrl Pts',(108.677361128733,-4.08857556234406,337.737060197072));
#56267=CARTESIAN_POINT('Ctrl Pts',(108.669595617684,-4.00923018671835,337.848728904688));
#56268=CARTESIAN_POINT('Ctrl Pts',(108.661837806162,-3.92996348226347,337.960286892456));
#56269=CARTESIAN_POINT('Ctrl Pts',(108.654079994639,-3.84595442261319,338.068650227308));
#56270=CARTESIAN_POINT('Ctrl Pts',(108.646322183117,-3.75749324306918,338.173393702456));
#56271=CARTESIAN_POINT('Ctrl Pts',(108.638570209594,-3.66909863336823,338.278058354818));
#56272=CARTESIAN_POINT('Ctrl Pts',(108.630818236071,-3.57625882369179,338.379108272162));
#56273=CARTESIAN_POINT('Ctrl Pts',(108.623066262548,-3.47930587863644,338.476149258215));
#56274=CARTESIAN_POINT('Ctrl Pts',(108.615317571991,-3.38239399321076,338.573149147352));
#56275=CARTESIAN_POINT('Ctrl Pts',(108.607568881433,-3.28137271264234,338.666143206032));
#56276=CARTESIAN_POINT('Ctrl Pts',(108.599820190875,-3.17661255458554,338.754772395306));
#56277=CARTESIAN_POINT('Ctrl Pts',(108.592073112497,-3.0718741927546,338.843383144536));
#56278=CARTESIAN_POINT('Ctrl Pts',(108.58432603412,-2.96339879896313,338.92763057843));
#56279=CARTESIAN_POINT('Ctrl Pts',(108.576578955742,-2.85159142311456,339.007194706789));
#56280=CARTESIAN_POINT('Ctrl Pts',(108.568831812436,-2.73978311021256,339.086759501972));
#56281=CARTESIAN_POINT('Ctrl Pts',(108.56108466913,-2.62464307802337,339.161640686704));
#56282=CARTESIAN_POINT('Ctrl Pts',(108.553337525824,-2.5066065881345,339.231560761093));
#56283=CARTESIAN_POINT('Ctrl Pts',(108.545588640796,-2.38854356113689,339.301496554999));
#56284=CARTESIAN_POINT('Ctrl Pts',(108.537839755768,-2.26758311688829,339.366468819942));
#56285=CARTESIAN_POINT('Ctrl Pts',(108.53009087074,-2.1441860593072,339.426245497662));
#56286=CARTESIAN_POINT('Ctrl Pts',(108.522333760965,-2.0206580268141,339.486085622966));
#56287=CARTESIAN_POINT('Ctrl Pts',(108.514576651191,-1.89468856704656,339.540718974339));
#56288=CARTESIAN_POINT('Ctrl Pts',(108.506819541416,-1.76675996528577,339.589961033338));
#56289=CARTESIAN_POINT('Ctrl Pts',(108.49905828649,-1.63876300257057,339.639229405719));
#56290=CARTESIAN_POINT('Ctrl Pts',(108.491297031563,-1.50880518196739,339.683100620247));
#56291=CARTESIAN_POINT('Ctrl Pts',(108.483535776637,-1.37738402400586,339.721440067703));
#56292=CARTESIAN_POINT('Ctrl Pts',(108.475762106233,-1.24575263502173,339.75984084578));
#56293=CARTESIAN_POINT('Ctrl Pts',(108.467988435828,-1.11265361062778,339.7926920801));
#56294=CARTESIAN_POINT('Ctrl Pts',(108.460214765423,-0.97859561200515,339.819910133049));
#56295=CARTESIAN_POINT('Ctrl Pts',(108.452802961246,-0.85077804547189,339.845861179083));
#56296=CARTESIAN_POINT('Ctrl Pts',(108.445391157069,-0.722089060107164,
339.866691644544));
#56297=CARTESIAN_POINT('Ctrl Pts',(108.437979352892,-0.592972047854779,
339.882373112838));
#56298=CARTESIAN_POINT('Ctrl Pts',(108.430204274114,-0.457526626211204,
339.898823176606));
#56299=CARTESIAN_POINT('Ctrl Pts',(108.422429195335,-0.321182126475817,
339.909658730827));
#56300=CARTESIAN_POINT('Ctrl Pts',(108.414654116557,-0.184443631039657,
339.914790291505));
#56301=CARTESIAN_POINT('Ctrl Pts',(108.406888605508,-0.0478734010273303,
339.919915537471));
#56302=CARTESIAN_POINT('Ctrl Pts',(108.399123094459,0.0890894731342093,
339.919350741426));
#56303=CARTESIAN_POINT('Ctrl Pts',(108.39135758341,0.225932407303675,339.913057867543));
#56304=CARTESIAN_POINT('Ctrl Pts',(108.383599771888,0.362639661305597,339.906771233063));
#56305=CARTESIAN_POINT('Ctrl Pts',(108.375841960365,0.499226824028267,339.894767840924));
#56306=CARTESIAN_POINT('Ctrl Pts',(108.368084148843,0.635179267037453,339.877061652391));
#56307=CARTESIAN_POINT('Ctrl Pts',(108.36033217532,0.771029401521789,339.859368788327));
#56308=CARTESIAN_POINT('Ctrl Pts',(108.352580201797,0.90624538098487,339.835981720238));
#56309=CARTESIAN_POINT('Ctrl Pts',(108.344828228274,1.04031601816314,339.806966366104));
#56310=CARTESIAN_POINT('Ctrl Pts',(108.337079537716,1.17432987634696,339.77796329999));
#56311=CARTESIAN_POINT('Ctrl Pts',(108.329330847159,1.30719897574745,339.743336771115));
#56312=CARTESIAN_POINT('Ctrl Pts',(108.321582156601,1.43842088448955,339.703204059103));
#56313=CARTESIAN_POINT('Ctrl Pts',(108.313835078223,1.56961549141756,339.663079697037));
#56314=CARTESIAN_POINT('Ctrl Pts',(108.306087999846,1.69916321581614,339.617451544774));
#56315=CARTESIAN_POINT('Ctrl Pts',(108.298340921468,1.82657577535686,339.566487052361));
#56316=CARTESIAN_POINT('Ctrl Pts',(108.290593778162,1.95398940273756,339.515522132816));
#56317=CARTESIAN_POINT('Ctrl Pts',(108.282846634856,2.07926746664981,339.459220929084));
#56318=CARTESIAN_POINT('Ctrl Pts',(108.27509949155,2.20194106649374,339.397799290803));
#56319=CARTESIAN_POINT('Ctrl Pts',(108.267350606522,2.32464224596727,339.336363843634));
#56320=CARTESIAN_POINT('Ctrl Pts',(108.259601721494,2.44473744677209,339.269805846156));
#56321=CARTESIAN_POINT('Ctrl Pts',(108.251852836466,2.56178215872544,339.198387218175));
#56322=CARTESIAN_POINT('Ctrl Pts',(108.244095726691,2.67895110314544,339.126892785724));
#56323=CARTESIAN_POINT('Ctrl Pts',(108.236338616917,2.79306275667324,339.050527620855));
#56324=CARTESIAN_POINT('Ctrl Pts',(108.228581507142,2.90370096157295,338.96959743403));
#56325=CARTESIAN_POINT('Ctrl Pts',(108.220820252216,3.01439828799184,338.888624000702));
#56326=CARTESIAN_POINT('Ctrl Pts',(108.21305899729,3.12161816194648,338.803080928339));
#56327=CARTESIAN_POINT('Ctrl Pts',(108.205297742363,3.22497815076592,338.713313747798));
#56328=CARTESIAN_POINT('Ctrl Pts',(108.197524071959,3.32850348188246,338.623402969022));
#56329=CARTESIAN_POINT('Ctrl Pts',(108.189750401554,3.42815630499256,338.52925484776));
#56330=CARTESIAN_POINT('Ctrl Pts',(108.181976731149,3.52359102168934,338.431251866939));
#56331=CARTESIAN_POINT('Ctrl Pts',(108.174564926972,3.61458322936439,338.337810948452));
#56332=CARTESIAN_POINT('Ctrl Pts',(108.167153122795,3.70174100632332,338.24086619531));
#56333=CARTESIAN_POINT('Ctrl Pts',(108.159741318618,3.78480051162477,338.140775087412));
#56334=CARTESIAN_POINT('Ctrl Pts',(108.15196623984,3.87193101070197,338.035778216159));
#56335=CARTESIAN_POINT('Ctrl Pts',(108.144191161061,3.95482669166532,337.926986957682));
#56336=CARTESIAN_POINT('Ctrl Pts',(108.136416082283,4.03313897645041,337.814777621614));
#56337=CARTESIAN_POINT('Ctrl Pts',(108.128650571234,4.11135489298348,337.702706366277));
#56338=CARTESIAN_POINT('Ctrl Pts',(108.120885060185,4.18499841407718,337.587225719872));
#56339=CARTESIAN_POINT('Ctrl Pts',(108.113119549136,4.25376016590161,337.468746141969));
#56340=CARTESIAN_POINT('Ctrl Pts',(108.105361737613,4.32245374024891,337.350384036914));
#56341=CARTESIAN_POINT('Ctrl Pts',(108.097603926091,4.38627498283673,337.22902925358));
#56342=CARTESIAN_POINT('Ctrl Pts',(108.089846114569,4.44495713901647,337.105122109239));
#56343=CARTESIAN_POINT('Ctrl Pts',(108.082094141046,4.50359513501273,336.981308208954));
#56344=CARTESIAN_POINT('Ctrl Pts',(108.074342167523,4.55710157569387,336.854946122624));
#56345=CARTESIAN_POINT('Ctrl Pts',(108.066590194,4.60525526013601,336.726501390526));
#56346=CARTESIAN_POINT('Ctrl Pts',(108.058841503442,4.65338855146419,336.598111054849));
#56347=CARTESIAN_POINT('Ctrl Pts',(108.051092812885,4.69617345832183,336.467640192881));
#56348=CARTESIAN_POINT('Ctrl Pts',(108.043344122327,4.73343670892902,336.335574777039));
#56349=CARTESIAN_POINT('Ctrl Pts',(108.035597043949,4.77069220660572,336.20353683851));
#56350=CARTESIAN_POINT('Ctrl Pts',(108.027849965571,4.80242822705234,336.06990538195));
#56351=CARTESIAN_POINT('Ctrl Pts',(108.020102887194,4.8285213450012,335.935181631218));
#56352=CARTESIAN_POINT('Ctrl Pts',(108.012355743888,4.85461468163549,335.800456751371));
#56353=CARTESIAN_POINT('Ctrl Pts',(108.004608600582,4.87506494711981,335.664639942835));
#56354=CARTESIAN_POINT('Ctrl Pts',(107.996861457276,4.88979990500149,335.528242322753));
#56355=CARTESIAN_POINT('Ctrl Pts',(107.989112572248,4.90453817561453,335.39181403759));
#56356=CARTESIAN_POINT('Ctrl Pts',(107.98136368722,4.91355853979926,335.254805069582));
#56357=CARTESIAN_POINT('Ctrl Pts',(107.973614802192,4.91684070154239,335.11773095666));
#56358=CARTESIAN_POINT('Ctrl Pts',(107.965857692417,4.9201263470059,334.980511351859));
#56359=CARTESIAN_POINT('Ctrl Pts',(107.958100582642,4.91766161413682,334.843226855399));
#56360=CARTESIAN_POINT('Ctrl Pts',(107.950343472868,4.90947837455626,334.706392860672));
#56361=CARTESIAN_POINT('Ctrl Pts',(107.942582217941,4.90129076211412,334.569485746234));
#56362=CARTESIAN_POINT('Ctrl Pts',(107.934820963015,4.88737859365483,334.433030001873));
#56363=CARTESIAN_POINT('Ctrl Pts',(107.927059708089,4.86782547718353,334.297534209955));
#56364=CARTESIAN_POINT('Ctrl Pts',(107.919286037684,4.84824108209825,334.161821668929));
#56365=CARTESIAN_POINT('Ctrl Pts',(107.91151236728,4.82299777902962,334.027072533343));
#56366=CARTESIAN_POINT('Ctrl Pts',(107.903738696875,4.79223018290202,333.893784407729));
#56367=CARTESIAN_POINT('Ctrl Pts',(107.896326892698,4.76289482577666,333.766700876432));
#56368=CARTESIAN_POINT('Ctrl Pts',(107.888915088521,4.7285379888598,333.640945673746));
#56369=CARTESIAN_POINT('Ctrl Pts',(107.881503284344,4.68931750515014,333.516934122032));
#56370=CARTESIAN_POINT('Ctrl Pts',(107.873728205566,4.64817470870175,333.386844394757));
#56371=CARTESIAN_POINT('Ctrl Pts',(107.865953126787,4.60154942801112,333.25826245573));
#56372=CARTESIAN_POINT('Ctrl Pts',(107.858178048009,4.5495694742852,333.131685074418));
#56373=CARTESIAN_POINT('Ctrl Pts',(107.85041253696,4.49765348520154,333.005263454632));
#56374=CARTESIAN_POINT('Ctrl Pts',(107.842647025911,4.44039608089622,332.880841842581));
#56375=CARTESIAN_POINT('Ctrl Pts',(107.834881514862,4.37797500564806,332.758902520545));
#56376=CARTESIAN_POINT('Ctrl Pts',(107.827123703339,4.31561582107774,332.637084101701));
#56377=CARTESIAN_POINT('Ctrl Pts',(107.819365891817,4.2481033312079,332.517743420645));
#56378=CARTESIAN_POINT('Ctrl Pts',(107.811608080295,4.17566345197931,332.401343077991));
#56379=CARTESIAN_POINT('Ctrl Pts',(107.803856106772,4.10327808605705,332.285030330287));
#56380=CARTESIAN_POINT('Ctrl Pts',(107.796104133249,4.02597291709686,332.17165384724));
#56381=CARTESIAN_POINT('Ctrl Pts',(107.788352159726,3.94401972333747,332.061651571984));
#56382=CARTESIAN_POINT('Ctrl Pts',(107.780603469168,3.86210123680435,331.951695882757));
#56383=CARTESIAN_POINT('Ctrl Pts',(107.772854778611,3.77553887360009,331.845111871977));
#56384=CARTESIAN_POINT('Ctrl Pts',(107.765106088053,3.68464753099484,331.74230823514));
#56385=CARTESIAN_POINT('Ctrl Pts',(107.757359009675,3.59377509909251,331.639525987459));
#56386=CARTESIAN_POINT('Ctrl Pts',(107.749611931298,3.49857573804616,331.540522841892));
#56387=CARTESIAN_POINT('Ctrl Pts',(107.74186485292,3.39940414519525,331.445673830368));
#56388=CARTESIAN_POINT('Ctrl Pts',(107.734117709614,3.30023172119101,331.350824023918));
#56389=CARTESIAN_POINT('Ctrl Pts',(107.726370566308,3.19708728145803,331.26012869112));
#56390=CARTESIAN_POINT('Ctrl Pts',(107.718623423002,3.09036154401724,331.17392517196));
#56391=CARTESIAN_POINT('Ctrl Pts',(107.710874537974,2.98361181236482,331.08770227242));
#56392=CARTESIAN_POINT('Ctrl Pts',(107.703125652946,2.8732794848576,331.005973441574));
#56393=CARTESIAN_POINT('Ctrl Pts',(107.695376767918,2.7597871050036,330.929034733929));
#56394=CARTESIAN_POINT('Ctrl Pts',(107.687619658143,2.64617426316494,330.852014362745));
#56395=CARTESIAN_POINT('Ctrl Pts',(107.679862548369,2.52939499287368,330.77979449078));
#56396=CARTESIAN_POINT('Ctrl Pts',(107.672105438594,2.40989994699168,330.712627225446));
#56397=CARTESIAN_POINT('Ctrl Pts',(107.664344183668,2.29034104677787,330.645424068072));
#56398=CARTESIAN_POINT('Ctrl Pts',(107.656582928742,2.16806382755665,330.58327907423));
#56399=CARTESIAN_POINT('Ctrl Pts',(107.648821673815,2.043541212177,330.526397159265));
#56400=CARTESIAN_POINT('Ctrl Pts',(107.641048003411,1.91881940119457,330.469424251773));
#56401=CARTESIAN_POINT('Ctrl Pts',(107.633274333006,1.79184537858289,330.417731394696));
#56402=CARTESIAN_POINT('Ctrl Pts',(107.625500662601,1.66311043846837,330.371474669837));
#56403=CARTESIAN_POINT('Ctrl Pts',(107.618088858424,1.54036814078723,330.327371206649));
#56404=CARTESIAN_POINT('Ctrl Pts',(107.610677054247,1.4160254521268,330.288209247777));
#56405=CARTESIAN_POINT('Ctrl Pts',(107.60326525007,1.29051703841253,330.254080822847));
#56406=CARTESIAN_POINT('Ctrl Pts',(107.595490171292,1.1588570834726,330.218279662148));
#56407=CARTESIAN_POINT('Ctrl Pts',(107.587715092513,1.02549817302981,330.18790479015));
#56408=CARTESIAN_POINT('Ctrl Pts',(107.579940013735,0.890927217104305,330.163117558145));
#56409=CARTESIAN_POINT('Ctrl Pts',(107.572174502686,0.756521859307278,330.138360828408));
#56410=CARTESIAN_POINT('Ctrl Pts',(107.564408991637,0.62090780441603,330.11917812763));
#56411=CARTESIAN_POINT('Ctrl Pts',(107.556643480588,0.484586801516951,330.10568097747));
#56412=CARTESIAN_POINT('Ctrl Pts',(107.548885669066,0.348400961289134,330.092197209775));
#56413=CARTESIAN_POINT('Ctrl Pts',(107.541127857543,0.211509954432455,330.084387812536));
#56414=CARTESIAN_POINT('Ctrl Pts',(107.533370046021,0.074425047752714,330.082313147956));
#56415=CARTESIAN_POINT('Ctrl Pts',(107.525618072498,-0.0625566981874454,
330.080240044627));
#56416=CARTESIAN_POINT('Ctrl Pts',(107.517866098975,-0.199731664256605,
330.083893089921));
#56417=CARTESIAN_POINT('Ctrl Pts',(107.510114125452,-0.336584499931678,
330.093280735878));
#56418=CARTESIAN_POINT('Ctrl Pts',(107.502365434895,-0.473379378349593,
330.102664406161));
#56419=CARTESIAN_POINT('Ctrl Pts',(107.494616744337,-0.609852008561665,
330.117777820084));
#56420=CARTESIAN_POINT('Ctrl Pts',(107.486868053779,-0.745488300824605,
330.138577342399));
#56421=CARTESIAN_POINT('Ctrl Pts',(107.479120975402,-0.881096372824082,
330.1593725372));
#56422=CARTESIAN_POINT('Ctrl Pts',(107.471373897024,-1.01586806687144,330.185851428027));
#56423=CARTESIAN_POINT('Ctrl Pts',(107.463626818646,-1.14929606353317,330.217918693618));
#56424=CARTESIAN_POINT('Ctrl Pts',(107.45587967534,-1.28272517845002,330.249986227963));
#56425=CARTESIAN_POINT('Ctrl Pts',(107.448132532034,-1.414810193467,330.287642139151));
#56426=CARTESIAN_POINT('Ctrl Pts',(107.440385388728,-1.54505599225037,330.330740418084));
#56427=CARTESIAN_POINT('Ctrl Pts',(107.4326365037,-1.67533107305451,330.373848386426));
#56428=CARTESIAN_POINT('Ctrl Pts',(107.424887618672,-1.80376574380302,330.422401034494));
#56429=CARTESIAN_POINT('Ctrl Pts',(107.417138733644,-1.92988238340716,330.476203248518));
#56430=CARTESIAN_POINT('Ctrl Pts',(107.409381623869,-2.0561328845156,330.530062568769));
#56431=CARTESIAN_POINT('Ctrl Pts',(107.401624514095,-2.18006007954213,330.589182431838));
#56432=CARTESIAN_POINT('Ctrl Pts',(107.39386740432,-2.30120809186383,330.653320303905));
#56433=CARTESIAN_POINT('Ctrl Pts',(107.386106149394,-2.42242084180975,330.717492449201));
#56434=CARTESIAN_POINT('Ctrl Pts',(107.378344894468,-2.54085111252258,330.786687749468));
#56435=CARTESIAN_POINT('Ctrl Pts',(107.370583639541,-2.65607066062768,330.860619405243));
#56436=CARTESIAN_POINT('Ctrl Pts',(107.362809969137,-2.77147452245979,330.934669327573));
#56437=CARTESIAN_POINT('Ctrl Pts',(107.355036298732,-2.88365707819748,331.013470520959));
#56438=CARTESIAN_POINT('Ctrl Pts',(107.347262628327,-2.99222120788063,331.096694310509));
#56439=CARTESIAN_POINT('Ctrl Pts',(107.33985082415,-3.09573165120778,331.176044012634));
#56440=CARTESIAN_POINT('Ctrl Pts',(107.332439019973,-3.19595274152198,331.259413649204));
#56441=CARTESIAN_POINT('Ctrl Pts',(107.325027215796,-3.29257186647513,331.346487502882));
#56442=CARTESIAN_POINT('Ctrl Pts',(107.317367950252,-3.39241685927191,331.436468531974));
#56443=CARTESIAN_POINT('Ctrl Pts',(107.309708684708,-3.4887509638778,331.530708390154));
#56444=CARTESIAN_POINT('Ctrl Pts',(107.302049419163,-3.5811807498019,331.628898177191));
#56445=CARTESIAN_POINT('Ctrl Pts',(107.294399665406,-3.67349575025715,331.726966025605));
#56446=CARTESIAN_POINT('Ctrl Pts',(107.286749911648,-3.76191580043934,331.828973757283));
#56447=CARTESIAN_POINT('Ctrl Pts',(107.27910015789,-3.84608082321445,331.934572564258));
#56448=CARTESIAN_POINT('Ctrl Pts',(107.271296708668,-3.93193685234707,332.042293015688));
#56449=CARTESIAN_POINT('Ctrl Pts',(107.263493259446,-4.01336470738464,332.153750130447));
#56450=CARTESIAN_POINT('Ctrl Pts',(107.255689810224,-4.09002141961977,332.268533754638));
#56451=CARTESIAN_POINT('Ctrl Pts',(107.24805347621,-4.16503648570301,332.380859223641));
#56452=CARTESIAN_POINT('Ctrl Pts',(107.240417142196,-4.23548245496336,332.496369811835));
#56453=CARTESIAN_POINT('Ctrl Pts',(107.232780808182,-4.30107893507099,332.614648232065));
#56454=CARTESIAN_POINT('Ctrl Pts',(107.225147462329,-4.36664974672413,332.732880368955));
#56455=CARTESIAN_POINT('Ctrl Pts',(107.217514116477,-4.42737464720835,332.853877831972));
#56456=CARTESIAN_POINT('Ctrl Pts',(107.209880770624,-4.48301770655805,332.977196177286));
#56457=CARTESIAN_POINT('Ctrl Pts',(107.202248645274,-4.53865186909091,333.100494805123));
#56458=CARTESIAN_POINT('Ctrl Pts',(107.194616519924,-4.58920564146773,333.226113209185));
#56459=CARTESIAN_POINT('Ctrl Pts',(107.186984394574,-4.63449026864816,333.35358479954));
#56460=CARTESIAN_POINT('Ctrl Pts',(107.179053809739,-4.68154578215933,333.486041253655));
#56461=CARTESIAN_POINT('Ctrl Pts',(107.171123224905,-4.72291148549212,333.620498350175));
#56462=CARTESIAN_POINT('Ctrl Pts',(107.163192640071,-4.75843206096906,333.756413499735));
#56463=CARTESIAN_POINT('Ctrl Pts',(107.155554518819,-4.79264271101794,333.887316379417));
#56464=CARTESIAN_POINT('Ctrl Pts',(107.147916397567,-4.82143164608762,334.019571264848));
#56465=CARTESIAN_POINT('Ctrl Pts',(107.140278276315,-4.8447121656197,334.152682412081));
#56466=CARTESIAN_POINT('Ctrl Pts',(107.132636775724,-4.86800298516572,334.285852451758));
#56467=CARTESIAN_POINT('Ctrl Pts',(107.124995275133,-4.88578048327286,334.419879108267));
#56468=CARTESIAN_POINT('Ctrl Pts',(107.117353774543,-4.89800980322335,334.554261253616));
#56469=CARTESIAN_POINT('Ctrl Pts',(107.109704288804,-4.91025190246137,334.688783824441));
#56470=CARTESIAN_POINT('Ctrl Pts',(107.102054803065,-4.91693423712501,334.823662223669));
#56471=CARTESIAN_POINT('Ctrl Pts',(107.094405317326,-4.91807402271891,334.958395077725));
#56472=CARTESIAN_POINT('Ctrl Pts',(107.093542670405,-4.91820255848797,334.973589155548));
#56473=CARTESIAN_POINT('Ctrl Pts',(107.092680023485,-4.91826066120041,334.988781387545));
#56474=CARTESIAN_POINT('Ctrl Pts',(107.091817376565,-4.9182483968572,335.00397105925));
#56475=CARTESIAN_POINT('',(105.341817376472,-4.91824882476302,334.996599968063));
#56476=CARTESIAN_POINT('Ctrl Pts',(107.091817376509,-4.91824839685641,335.003971060231));
#56477=CARTESIAN_POINT('Ctrl Pts',(107.079247665722,-4.91806969189428,335.225301219511));
#56478=CARTESIAN_POINT('Ctrl Pts',(107.066677954934,-4.90294797263902,335.446045535405));
#56479=CARTESIAN_POINT('Ctrl Pts',(107.054108244147,-4.87313418658796,335.664639949151));
#56480=CARTESIAN_POINT('Ctrl Pts',(107.051668556606,-4.86734755206395,335.707067501934));
#56481=CARTESIAN_POINT('Ctrl Pts',(107.049228869064,-4.86100754838075,335.749414178383));
#56482=CARTESIAN_POINT('Ctrl Pts',(107.046789181522,-4.85411616778059,335.791668675767));
#56483=CARTESIAN_POINT('Ctrl Pts',(107.039014102744,-4.83215391804811,335.926330201189));
#56484=CARTESIAN_POINT('Ctrl Pts',(107.031239023965,-4.80454910457406,336.060289919449));
#56485=CARTESIAN_POINT('Ctrl Pts',(107.023463945187,-4.77135660038552,336.19303782608));
#56486=CARTESIAN_POINT('Ctrl Pts',(107.015698434138,-4.73820494168652,336.32562237796));
#56487=CARTESIAN_POINT('Ctrl Pts',(107.007932923089,-4.69947936746907,336.456997709719));
#56488=CARTESIAN_POINT('Ctrl Pts',(107.00016741204,-4.65528625056723,336.586660955523));
#56489=CARTESIAN_POINT('Ctrl Pts',(106.992409600518,-4.61113695126951,336.71619563984));
#56490=CARTESIAN_POINT('Ctrl Pts',(106.984651788995,-4.56153102283847,336.844021248808));
#56491=CARTESIAN_POINT('Ctrl Pts',(106.976893977473,-4.50662534362196,336.969647449348));
#56492=CARTESIAN_POINT('Ctrl Pts',(106.96914200395,-4.45176098267015,337.095179112189));
#56493=CARTESIAN_POINT('Ctrl Pts',(106.961390030427,-4.39160496521674,337.218514304329));
#56494=CARTESIAN_POINT('Ctrl Pts',(106.953638056904,-4.32636310708101,337.339180482175));
#56495=CARTESIAN_POINT('Ctrl Pts',(106.945889366347,-4.26114887891098,337.459795557823));
#56496=CARTESIAN_POINT('Ctrl Pts',(106.938140675789,-4.1908532794453,337.577743524203));
#56497=CARTESIAN_POINT('Ctrl Pts',(106.930391985231,-4.11572900897169,337.692574564837));
#56498=CARTESIAN_POINT('Ctrl Pts',(106.922644906853,-4.04062036873001,337.807381713915));
#56499=CARTESIAN_POINT('Ctrl Pts',(106.914897828476,-3.96068526964706,337.919072900274));
#56500=CARTESIAN_POINT('Ctrl Pts',(106.907150750098,-3.87622064867957,338.02722588276));
#56501=CARTESIAN_POINT('Ctrl Pts',(106.899403606792,-3.79175531981721,338.135379771671));
#56502=CARTESIAN_POINT('Ctrl Pts',(106.891656463486,-3.70276063393929,338.239995089502));
#56503=CARTESIAN_POINT('Ctrl Pts',(106.88390932018,-3.60957460539302,338.34068170148));
#56504=CARTESIAN_POINT('Ctrl Pts',(106.876160435152,-3.5163676266492,338.441390949945));
#56505=CARTESIAN_POINT('Ctrl Pts',(106.868411550124,-3.41896769560604,338.538169448164));
#56506=CARTESIAN_POINT('Ctrl Pts',(106.860662665096,-3.31775027058181,338.63066332845));
#56507=CARTESIAN_POINT('Ctrl Pts',(106.852905555321,-3.21642541233688,338.723255382697));
#56508=CARTESIAN_POINT('Ctrl Pts',(106.845148445547,-3.11127525500551,338.811553470386));
#56509=CARTESIAN_POINT('Ctrl Pts',(106.837391335772,-3.00270940718991,338.895243160378));
#56510=CARTESIAN_POINT('Ctrl Pts',(106.829630080846,-2.89408554525651,338.978977571465));
#56511=CARTESIAN_POINT('Ctrl Pts',(106.82186882592,-2.78204267501926,339.058098452584));
#56512=CARTESIAN_POINT('Ctrl Pts',(106.814107570993,-2.66701924469968,339.132334861903));
#56513=CARTESIAN_POINT('Ctrl Pts',(106.806333900589,-2.55181181437772,339.206690025284));
#56514=CARTESIAN_POINT('Ctrl Pts',(106.798560230184,-2.4336146334237,339.276144904922));
#56515=CARTESIAN_POINT('Ctrl Pts',(106.790786559779,-2.31289136828018,339.340474234578));
#56516=CARTESIAN_POINT('Ctrl Pts',(106.783374755602,-2.19778780017286,339.401809018462));
#56517=CARTESIAN_POINT('Ctrl Pts',(106.775962951425,-2.0803882929454,339.458484577115));
#56518=CARTESIAN_POINT('Ctrl Pts',(106.768551147248,-1.96110970855013,339.51034718991));
#56519=CARTESIAN_POINT('Ctrl Pts',(106.76077606847,-1.83598492542161,339.564751743848));
#56520=CARTESIAN_POINT('Ctrl Pts',(106.753000989691,-1.70839679189643,339.614031557433));
#56521=CARTESIAN_POINT('Ctrl Pts',(106.745225910913,-1.57880387655637,339.657956781881));
#56522=CARTESIAN_POINT('Ctrl Pts',(106.737460399864,-1.44937043354892,339.701827953544));
#56523=CARTESIAN_POINT('Ctrl Pts',(106.729694888815,-1.31793748402125,339.74035752234));
#56524=CARTESIAN_POINT('Ctrl Pts',(106.721929377766,-1.18498546302489,339.773362809898));
#56525=CARTESIAN_POINT('Ctrl Pts',(106.714171566244,-1.05216526434435,339.806335372618));
#56526=CARTESIAN_POINT('Ctrl Pts',(106.706413754722,-0.91782936846196,339.833794460748));
#56527=CARTESIAN_POINT('Ctrl Pts',(106.698655943199,-0.782475002798547,
339.855606649276));
#56528=CARTESIAN_POINT('Ctrl Pts',(106.690903969676,-0.64722249558772,339.877402423441));
#56529=CARTESIAN_POINT('Ctrl Pts',(106.683151996153,-0.510953428480875,
339.89355969443));
#56530=CARTESIAN_POINT('Ctrl Pts',(106.67540002263,-0.374176552216034,339.903995816706));
#56531=CARTESIAN_POINT('Ctrl Pts',(106.667651332073,-0.237457601039497,
339.914427519278));
#56532=CARTESIAN_POINT('Ctrl Pts',(106.659902641515,-0.100231657369472,
339.919142862458));
#56533=CARTESIAN_POINT('Ctrl Pts',(106.652153950958,0.0369862678958382,
339.918110925801));
#56534=CARTESIAN_POINT('Ctrl Pts',(106.64440687258,0.174175643825637,339.917079203848));
#56535=CARTESIAN_POINT('Ctrl Pts',(106.636659794202,0.311356614051241,339.910302583467));
#56536=CARTESIAN_POINT('Ctrl Pts',(106.628912715824,0.448013417350148,339.897802266361));
#56537=CARTESIAN_POINT('Ctrl Pts',(106.621165572518,0.58467136596469,339.885301844491));
#56538=CARTESIAN_POINT('Ctrl Pts',(106.613418429213,0.720804749641099,339.867077665822));
#56539=CARTESIAN_POINT('Ctrl Pts',(106.605671285907,0.855902576767339,339.843202849518));
#56540=CARTESIAN_POINT('Ctrl Pts',(106.597922400879,0.991030776753234,339.819322665649));
#56541=CARTESIAN_POINT('Ctrl Pts',(106.590173515851,1.12512257207817,339.789789384234));
#56542=CARTESIAN_POINT('Ctrl Pts',(106.582424630823,1.25767720581652,339.754727238073));
#56543=CARTESIAN_POINT('Ctrl Pts',(106.574667521048,1.39037253441276,339.719627876587));
#56544=CARTESIAN_POINT('Ctrl Pts',(106.566910411273,1.52152706375457,339.678988027799));
#56545=CARTESIAN_POINT('Ctrl Pts',(106.559153301499,1.65065471927012,339.632981983588));
#56546=CARTESIAN_POINT('Ctrl Pts',(106.551392046572,1.77985137647608,339.586951355218));
#56547=CARTESIAN_POINT('Ctrl Pts',(106.543630791646,1.90701863948305,339.535548964035));
#56548=CARTESIAN_POINT('Ctrl Pts',(106.53586953672,2.03169139803317,339.478996888329));
#56549=CARTESIAN_POINT('Ctrl Pts',(106.528095866315,2.15656359236621,339.422354347732));
#56550=CARTESIAN_POINT('Ctrl Pts',(106.520322195911,2.27893295917535,339.360545837333));
#56551=CARTESIAN_POINT('Ctrl Pts',(106.512548525506,2.39835915075817,339.293839359649));
#56552=CARTESIAN_POINT('Ctrl Pts',(106.505136721329,2.51222602439118,339.23023808455));
#56553=CARTESIAN_POINT('Ctrl Pts',(106.497724917152,2.62341732052589,339.162184731144));
#56554=CARTESIAN_POINT('Ctrl Pts',(106.490313112975,2.73157818428538,339.089946660488));
#56555=CARTESIAN_POINT('Ctrl Pts',(106.482538034196,2.84504033417182,339.014167986803));
#56556=CARTESIAN_POINT('Ctrl Pts',(106.474762955418,2.95552604080997,338.933544538154));
#56557=CARTESIAN_POINT('Ctrl Pts',(106.46698787664,3.0625938616824,338.848337550279));
#56558=CARTESIAN_POINT('Ctrl Pts',(106.459222365591,3.16952992878496,338.763235415026));
#56559=CARTESIAN_POINT('Ctrl Pts',(106.451456854542,3.27305617578858,338.673561204271));
#56560=CARTESIAN_POINT('Ctrl Pts',(106.443691343493,3.3727589935798,338.579620068349));
#56561=CARTESIAN_POINT('Ctrl Pts',(106.43593353197,3.47236295573698,338.485772075336));
#56562=CARTESIAN_POINT('Ctrl Pts',(106.428175720448,3.56815075021403,338.387665842748));
#56563=CARTESIAN_POINT('Ctrl Pts',(106.420417908926,3.65974109878217,338.285647295798));
#56564=CARTESIAN_POINT('Ctrl Pts',(106.412665935403,3.7512625227084,338.18370552104));
#56565=CARTESIAN_POINT('Ctrl Pts',(106.40491396188,3.83859252791289,338.077857581773));
#56566=CARTESIAN_POINT('Ctrl Pts',(106.397161988357,3.921386301782,337.968486573104));
#56567=CARTESIAN_POINT('Ctrl Pts',(106.389413297799,4.00414501243878,337.859161883121));
#56568=CARTESIAN_POINT('Ctrl Pts',(106.381664607242,4.0823710772588,337.746317402262));
#56569=CARTESIAN_POINT('Ctrl Pts',(106.373915916684,4.1557597926331,337.630369481353));
#56570=CARTESIAN_POINT('Ctrl Pts',(106.366168838306,4.22913323887222,337.514445684377));
#56571=CARTESIAN_POINT('Ctrl Pts',(106.358421759928,4.29767112865233,337.395420061756));
#56572=CARTESIAN_POINT('Ctrl Pts',(106.350674681551,4.36111218294644,337.273737801563));
#56573=CARTESIAN_POINT('Ctrl Pts',(106.342927538245,4.42455376893765,337.152054521555));
#56574=CARTESIAN_POINT('Ctrl Pts',(106.335180394939,4.48289825353818,337.027714906162));
#56575=CARTESIAN_POINT('Ctrl Pts',(106.327433251633,4.53593059733132,336.901188228107));
#56576=CARTESIAN_POINT('Ctrl Pts',(106.319684366605,4.58897486392122,336.774633104169));
#56577=CARTESIAN_POINT('Ctrl Pts',(106.311935481577,4.6367044621499,336.645890299564));
#56578=CARTESIAN_POINT('Ctrl Pts',(106.304186596549,4.67895287372387,336.515448140971));
#56579=CARTESIAN_POINT('Ctrl Pts',(106.296429486774,4.72124612819842,336.384867529722));
#56580=CARTESIAN_POINT('Ctrl Pts',(106.288672376999,4.75804645381128,336.252584333846));
#56581=CARTESIAN_POINT('Ctrl Pts',(106.280915267225,4.78923737348115,336.119101623156));
#56582=CARTESIAN_POINT('Ctrl Pts',(106.273154012298,4.82044496058119,335.985547583574));
#56583=CARTESIAN_POINT('Ctrl Pts',(106.265392757372,4.846037096082,335.850793135779));
#56584=CARTESIAN_POINT('Ctrl Pts',(106.257631502446,4.86594883250799,335.715349580215));
#56585=CARTESIAN_POINT('Ctrl Pts',(106.249857832041,4.88589242122303,335.579689359104));
#56586=CARTESIAN_POINT('Ctrl Pts',(106.242084161637,4.90013741213522,335.44333821637));
#56587=CARTESIAN_POINT('Ctrl Pts',(106.234310491232,4.90867087686924,335.30681148133));
#56588=CARTESIAN_POINT('Ctrl Pts',(106.226898687055,4.91680710676677,335.176640098654));
#56589=CARTESIAN_POINT('Ctrl Pts',(106.219486882878,4.91975158052645,335.046309391145));
#56590=CARTESIAN_POINT('Ctrl Pts',(106.212075078701,4.91753709542967,334.91626244825));
#56591=CARTESIAN_POINT('Ctrl Pts',(106.204299999923,4.91521407182167,334.779841517292));
#56592=CARTESIAN_POINT('Ctrl Pts',(106.196524921144,4.90720624935718,334.643301755234));
#56593=CARTESIAN_POINT('Ctrl Pts',(106.188749842366,4.89349441686567,334.507155750156));
#56594=CARTESIAN_POINT('Ctrl Pts',(106.180984331317,4.87979945765698,334.371177281404));
#56595=CARTESIAN_POINT('Ctrl Pts',(106.173218820268,4.86041449330612,334.235591990719));
#56596=CARTESIAN_POINT('Ctrl Pts',(106.165453309219,4.83537230361631,334.100912825183));
#56597=CARTESIAN_POINT('Ctrl Pts',(106.157695497697,4.81035494333049,333.966367194432));
#56598=CARTESIAN_POINT('Ctrl Pts',(106.149937686174,4.77969159123611,333.832726282726));
#56599=CARTESIAN_POINT('Ctrl Pts',(106.142179874652,4.74346681169933,333.700497915043));
#56600=CARTESIAN_POINT('Ctrl Pts',(106.134427901129,4.70726929245792,333.568369053401));
#56601=CARTESIAN_POINT('Ctrl Pts',(106.126675927606,4.66551877897275,333.43765099543));
#56602=CARTESIAN_POINT('Ctrl Pts',(106.118923954083,4.61835082620066,333.308841016157));
#56603=CARTESIAN_POINT('Ctrl Pts',(106.111175263526,4.57120284908455,333.180085587988));
#56604=CARTESIAN_POINT('Ctrl Pts',(106.103426572968,4.51864212998409,333.053236997593));
#56605=CARTESIAN_POINT('Ctrl Pts',(106.09567788241,4.46085389458412,332.928776788061));
#56606=CARTESIAN_POINT('Ctrl Pts',(106.087930804032,4.40307768250918,332.804342473516));
#56607=CARTESIAN_POINT('Ctrl Pts',(106.080183725655,4.34007628201017,332.682295905719));
#56608=CARTESIAN_POINT('Ctrl Pts',(106.072436647277,4.27208266816222,332.56309771659));
#56609=CARTESIAN_POINT('Ctrl Pts',(106.064689503971,4.20408848446235,332.443898528466));
#56610=CARTESIAN_POINT('Ctrl Pts',(106.056942360665,4.13110219763241,332.327548106146));
#56611=CARTESIAN_POINT('Ctrl Pts',(106.049195217359,4.05340205894974,332.21448123126));
#56612=CARTESIAN_POINT('Ctrl Pts',(106.041446332331,3.97568445162629,332.10138893654));
#56613=CARTESIAN_POINT('Ctrl Pts',(106.033697447303,3.89325110495208,331.991581980291));
#56614=CARTESIAN_POINT('Ctrl Pts',(106.025948562275,3.8064225506459,331.885464652884));
#56615=CARTESIAN_POINT('Ctrl Pts',(106.0181914525,3.71950183561507,331.779234691449));
#56616=CARTESIAN_POINT('Ctrl Pts',(106.010434342726,3.6281768418562,331.676702484844));
#56617=CARTESIAN_POINT('Ctrl Pts',(106.002677232951,3.53280757907679,331.578238221074));
#56618=CARTESIAN_POINT('Ctrl Pts',(105.994915978025,3.43738735401274,331.47972134115));
#56619=CARTESIAN_POINT('Ctrl Pts',(105.987154723099,3.33791883699792,331.385277004513));
#56620=CARTESIAN_POINT('Ctrl Pts',(105.979393468173,3.23479684467875,331.295236520889));
#56621=CARTESIAN_POINT('Ctrl Pts',(105.971619797768,3.13150989077918,331.205052001835));
#56622=CARTESIAN_POINT('Ctrl Pts',(105.963846127363,3.02455808789032,331.119285657913));
#56623=CARTESIAN_POINT('Ctrl Pts',(105.956072456959,2.91436779114319,331.038227235132));
#56624=CARTESIAN_POINT('Ctrl Pts',(105.948660652781,2.80930687921841,330.960942101432));
#56625=CARTESIAN_POINT('Ctrl Pts',(105.941248848604,2.70130243049351,330.887936606421));
#56626=CARTESIAN_POINT('Ctrl Pts',(105.933837044427,2.59074479682716,330.819422951289));
#56627=CARTESIAN_POINT('Ctrl Pts',(105.926061965649,2.47476840420195,330.747551237827));
#56628=CARTESIAN_POINT('Ctrl Pts',(105.91828688687,2.35561571311514,330.680395686678));
#56629=CARTESIAN_POINT('Ctrl Pts',(105.910511808092,2.23370737355073,330.618249843744));
#56630=CARTESIAN_POINT('Ctrl Pts',(105.902746297043,2.1119490499593,330.556180475228));
#56631=CARTESIAN_POINT('Ctrl Pts',(105.894980785994,1.98744216991709,330.499108724638));
#56632=CARTESIAN_POINT('Ctrl Pts',(105.887215274945,1.86063582060239,330.44728461184));
#56633=CARTESIAN_POINT('Ctrl Pts',(105.879457463422,1.73395520015223,330.3955118828));
#56634=CARTESIAN_POINT('Ctrl Pts',(105.8716996519,1.60498000711307,330.348976584112));
#56635=CARTESIAN_POINT('Ctrl Pts',(105.863941840378,1.47418304497533,330.307882417031));
#56636=CARTESIAN_POINT('Ctrl Pts',(105.856189866855,1.34348451169958,330.266819174614));
#56637=CARTESIAN_POINT('Ctrl Pts',(105.848437893332,1.21096730951346,330.231189030343));
#56638=CARTESIAN_POINT('Ctrl Pts',(105.840685919809,1.07712296416119,330.201147097214));
#56639=CARTESIAN_POINT('Ctrl Pts',(105.832937229251,0.943335301968555,330.171117886861));
#56640=CARTESIAN_POINT('Ctrl Pts',(105.825188538694,0.808221995071072,330.146672266054));
#56641=CARTESIAN_POINT('Ctrl Pts',(105.817439848136,0.672288219570297,330.127915065157));
#56642=CARTESIAN_POINT('Ctrl Pts',(105.809692769758,0.536382726226855,330.109161766852));
#56643=CARTESIAN_POINT('Ctrl Pts',(105.80194569138,0.39965749078738,330.096094587742));
#56644=CARTESIAN_POINT('Ctrl Pts',(105.794198613003,0.262625944641374,330.088766888479));
#56645=CARTESIAN_POINT('Ctrl Pts',(105.786451469697,0.125593250039026,330.081439127803));
#56646=CARTESIAN_POINT('Ctrl Pts',(105.778704326391,-0.0117453700736549,
330.079850963789));
#56647=CARTESIAN_POINT('Ctrl Pts',(105.770957183085,-0.148873720815505,
330.08400369429));
#56648=CARTESIAN_POINT('Ctrl Pts',(105.763208298057,-0.286032900921733,
330.088157358414));
#56649=CARTESIAN_POINT('Ctrl Pts',(105.755459413029,-0.422981326970275,
330.098054473522));
#56650=CARTESIAN_POINT('Ctrl Pts',(105.747710528001,-0.559205564457357,
330.113644282374));
#56651=CARTESIAN_POINT('Ctrl Pts',(105.739953418226,-0.695574391757753,
330.129250638409));
#56652=CARTESIAN_POINT('Ctrl Pts',(105.732196308451,-0.8312171060709,330.150561713703));
#56653=CARTESIAN_POINT('Ctrl Pts',(105.724439198677,-0.965627586495292,
330.177475098385));
#56654=CARTESIAN_POINT('Ctrl Pts',(105.716677943751,-1.10010989158272,330.204402864718));
#56655=CARTESIAN_POINT('Ctrl Pts',(105.708916688824,-1.23335827120195,330.236938812974));
#56656=CARTESIAN_POINT('Ctrl Pts',(105.701155433898,-1.36488046199348,330.274930224116));
#56657=CARTESIAN_POINT('Ctrl Pts',(105.693381763494,-1.4966130454273,330.312982409135));
#56658=CARTESIAN_POINT('Ctrl Pts',(105.685608093089,-1.62661355121246,330.356507371933));
#56659=CARTESIAN_POINT('Ctrl Pts',(105.677834422684,-1.75440760052237,330.405303379577));
#56660=CARTESIAN_POINT('Ctrl Pts',(105.670422618507,-1.87625280609057,330.451827921325));
#56661=CARTESIAN_POINT('Ctrl Pts',(105.66301081433,-1.99609208884605,330.503143704025));
#56662=CARTESIAN_POINT('Ctrl Pts',(105.655599010153,-2.11353576249201,330.559037306713));
#56663=CARTESIAN_POINT('Ctrl Pts',(105.647823931375,-2.23673570043089,330.617670421367));
#56664=CARTESIAN_POINT('Ctrl Pts',(105.640048852596,-2.35768859422035,330.681526739201));
#56665=CARTESIAN_POINT('Ctrl Pts',(105.632273773818,-2.47591995700338,330.750411381203));
#56666=CARTESIAN_POINT('Ctrl Pts',(105.624508262769,-2.59400582856752,330.819211256266));
#56667=CARTESIAN_POINT('Ctrl Pts',(105.61674275172,-2.70937649820478,330.893026948911));
#56668=CARTESIAN_POINT('Ctrl Pts',(105.608977240671,-2.8215786920368,330.971616112243));
#56669=CARTESIAN_POINT('Ctrl Pts',(105.601219429149,-2.93366963706683,331.050127354189));
#56670=CARTESIAN_POINT('Ctrl Pts',(105.593461617626,-3.0425980400692,331.133402425266));
#56671=CARTESIAN_POINT('Ctrl Pts',(105.585703806104,-3.14793674321381,331.221153969368));
#56672=CARTESIAN_POINT('Ctrl Pts',(105.577951832581,-3.2531961756439,331.30883947765));
#56673=CARTESIAN_POINT('Ctrl Pts',(105.570199859058,-3.35487098603542,331.400994504577));
#56674=CARTESIAN_POINT('Ctrl Pts',(105.562447885535,-3.45256474377734,331.497289656205));
#56675=CARTESIAN_POINT('Ctrl Pts',(105.554699194978,-3.55021712815485,331.59354402678));
#56676=CARTESIAN_POINT('Ctrl Pts',(105.54695050442,-3.64389153537855,331.693934760958));
#56677=CARTESIAN_POINT('Ctrl Pts',(105.539201813862,-3.73322643158218,331.798093775103));
#56678=CARTESIAN_POINT('Ctrl Pts',(105.531454735485,-3.82254274091457,331.902231118095));
#56679=CARTESIAN_POINT('Ctrl Pts',(105.523707657107,-3.9075210807928,332.01013488507));
#56680=CARTESIAN_POINT('Ctrl Pts',(105.515960578729,-3.98783873192088,332.121402197129));
#56681=CARTESIAN_POINT('Ctrl Pts',(105.508213435423,-4.06815705618808,332.232670441716));
#56682=CARTESIAN_POINT('Ctrl Pts',(105.500466292117,-4.14381438502051,332.347301970683));
#56683=CARTESIAN_POINT('Ctrl Pts',(105.492719148811,-4.2145302843566,332.464863407084));
#56684=CARTESIAN_POINT('Ctrl Pts',(105.484970263783,-4.28526208212835,332.582451273793));
#56685=CARTESIAN_POINT('Ctrl Pts',(105.477221378755,-4.35105003832197,332.702970023805));
#56686=CARTESIAN_POINT('Ctrl Pts',(105.469472493727,-4.41165898691453,332.825960431437));
#56687=CARTESIAN_POINT('Ctrl Pts',(105.461715383952,-4.47233226647129,332.949081382359));
#56688=CARTESIAN_POINT('Ctrl Pts',(105.453958274178,-4.52781538449648,333.074678880306));
#56689=CARTESIAN_POINT('Ctrl Pts',(105.446201164403,-4.5779205685756,333.202271897557));
#56690=CARTESIAN_POINT('Ctrl Pts',(105.438439909477,-4.628052527263,333.329933096437));
#56691=CARTESIAN_POINT('Ctrl Pts',(105.43067865455,-4.67280069825269,333.459591570102));
#56692=CARTESIAN_POINT('Ctrl Pts',(105.422917399624,-4.7120271142913,333.590750718757));
#56693=CARTESIAN_POINT('Ctrl Pts',(105.41514372922,-4.75131627981175,333.722119679305));
#56694=CARTESIAN_POINT('Ctrl Pts',(105.407370058815,-4.78506594313833,333.854993732891));
#56695=CARTESIAN_POINT('Ctrl Pts',(105.39959638841,-4.81318903219623,333.988864794973));
#56696=CARTESIAN_POINT('Ctrl Pts',(105.392184584233,-4.84000298469279,334.116504126908));
#56697=CARTESIAN_POINT('Ctrl Pts',(105.384772780056,-4.86170236052158,334.245049450957));
#56698=CARTESIAN_POINT('Ctrl Pts',(105.377360975879,-4.87825574831046,334.374057577268));
#56699=CARTESIAN_POINT('Ctrl Pts',(105.365513109422,-4.90471655639987,334.58027876388));
#56700=CARTESIAN_POINT('Ctrl Pts',(105.353665242965,-4.9181047645561,334.788212569106));
#56701=CARTESIAN_POINT('Ctrl Pts',(105.341817376508,-4.91824882476258,334.996599967431));
#56702=CARTESIAN_POINT('',(103.591817376553,-4.91824952580637,334.997840276541));
#56703=CARTESIAN_POINT('Ctrl Pts',(105.341817376472,-4.91824882476302,334.996599968063));
#56704=CARTESIAN_POINT('Ctrl Pts',(105.334158591598,-4.91834194920273,335.13130728099));
#56705=CARTESIAN_POINT('Ctrl Pts',(105.326499806723,-4.91289660595529,335.266230429205));
#56706=CARTESIAN_POINT('Ctrl Pts',(105.318841021849,-4.90188611779449,335.400868495487));
#56707=CARTESIAN_POINT('Ctrl Pts',(105.31119031737,-4.89088724624152,335.535364511971));
#56708=CARTESIAN_POINT('Ctrl Pts',(105.303539612892,-4.87433493981361,335.669575646368));
#56709=CARTESIAN_POINT('Ctrl Pts',(105.295888908413,-4.85225454198551,335.802999951607));
#56710=CARTESIAN_POINT('Ctrl Pts',(105.288244324432,-4.83019180828679,335.936317518543));
#56711=CARTESIAN_POINT('Ctrl Pts',(105.280599740452,-4.80260984610632,336.068849112915));
#56712=CARTESIAN_POINT('Ctrl Pts',(105.272955156471,-4.76958586071718,336.200097404275));
#56713=CARTESIAN_POINT('Ctrl Pts',(105.265314147281,-4.73657731813556,336.331284320786));
#56714=CARTESIAN_POINT('Ctrl Pts',(105.257673138092,-4.69813190983903,336.461188737582));
#56715=CARTESIAN_POINT('Ctrl Pts',(105.250032128902,-4.65437795177756,336.589323423507));
#56716=CARTESIAN_POINT('Ctrl Pts',(105.242392815477,-4.61063370401019,336.717429672565));
#56717=CARTESIAN_POINT('Ctrl Pts',(105.234753502053,-4.56158337873665,336.843766590538));
#56718=CARTESIAN_POINT('Ctrl Pts',(105.227114188628,-4.50740502695809,336.967862542317));
#56719=CARTESIAN_POINT('Ctrl Pts',(105.219474808225,-4.45322620016345,337.091959582124));
#56720=CARTESIAN_POINT('Ctrl Pts',(105.211835427822,-4.39391941889369,337.213815247516));
#56721=CARTESIAN_POINT('Ctrl Pts',(105.204196047419,-4.32971047981391,337.332978830485));
#56722=CARTESIAN_POINT('Ctrl Pts',(105.196554837451,-4.26548616325695,337.452170952086));
#56723=CARTESIAN_POINT('Ctrl Pts',(105.188913627483,-4.19635754581876,337.568669354893));
#56724=CARTESIAN_POINT('Ctrl Pts',(105.181272417516,-4.12259559524014,337.682049332247));
#56725=CARTESIAN_POINT('Ctrl Pts',(105.173623269308,-4.04875701543377,337.795547096889));
#56726=CARTESIAN_POINT('Ctrl Pts',(105.165974121101,-3.97027571268535,337.905919630354));
#56727=CARTESIAN_POINT('Ctrl Pts',(105.158324972894,-3.88746524452945,338.012772317165));
#56728=CARTESIAN_POINT('Ctrl Pts',(105.150671437674,-3.80460728211723,338.119686287157));
#56729=CARTESIAN_POINT('Ctrl Pts',(105.143017902454,-3.71741547073258,338.223076084499));
#56730=CARTESIAN_POINT('Ctrl Pts',(105.135364367234,-3.62624172249859,338.322582434269));
#56731=CARTESIAN_POINT('Ctrl Pts',(105.127699536033,-3.53493340940863,338.42223564712));
#56732=CARTESIAN_POINT('Ctrl Pts',(105.120034704833,-3.43963170969533,338.517993684794));
#56733=CARTESIAN_POINT('Ctrl Pts',(105.112369873632,-3.34072353461826,338.609535888137));
#56734=CARTESIAN_POINT('Ctrl Pts',(105.107954229623,-3.28374337689356,338.662272572247));
#56735=CARTESIAN_POINT('Ctrl Pts',(105.103538585614,-3.22556689088289,338.713610864243));
#56736=CARTESIAN_POINT('Ctrl Pts',(105.099122941605,-3.16627243683877,338.763495970267));
#56737=CARTESIAN_POINT('Ctrl Pts',(105.091347862826,-3.06186659018059,338.85133380964));
#56738=CARTESIAN_POINT('Ctrl Pts',(105.083572784048,-2.95363783367437,338.934962561326));
#56739=CARTESIAN_POINT('Ctrl Pts',(105.07579770527,-2.84196011347315,339.014031112975));
#56740=CARTESIAN_POINT('Ctrl Pts',(105.068032194221,-2.73041981981638,339.093002365737));
#56741=CARTESIAN_POINT('Ctrl Pts',(105.060266683172,-2.61543932310731,339.167424360266));
#56742=CARTESIAN_POINT('Ctrl Pts',(105.052501172122,-2.49742698350977,339.236984956846));
#56743=CARTESIAN_POINT('Ctrl Pts',(105.0447433606,-2.37953165349075,339.306476583891));
#56744=CARTESIAN_POINT('Ctrl Pts',(105.036985549078,-2.25861079741665,339.371116208037));
#56745=CARTESIAN_POINT('Ctrl Pts',(105.029227737556,-2.13510292039348,339.430634106065));
#56746=CARTESIAN_POINT('Ctrl Pts',(105.021475764033,-2.01168798696383,339.490107214988));
#56747=CARTESIAN_POINT('Ctrl Pts',(105.01372379051,-1.88569025832933,339.544466100508));
#56748=CARTESIAN_POINT('Ctrl Pts',(105.005971816987,-1.757573769774,339.593486421696));
#56749=CARTESIAN_POINT('Ctrl Pts',(104.998223126429,-1.62951153862798,339.642485982748));
#56750=CARTESIAN_POINT('Ctrl Pts',(104.990474435872,-1.49933269652401,339.686151336816));
#56751=CARTESIAN_POINT('Ctrl Pts',(104.982725745314,-1.36752203421418,339.724305932985));
#56752=CARTESIAN_POINT('Ctrl Pts',(104.974978666936,-1.23573879621356,339.762452590772));
#56753=CARTESIAN_POINT('Ctrl Pts',(104.967231588558,-1.10232478854908,339.795090662633));
#56754=CARTESIAN_POINT('Ctrl Pts',(104.95948451018,-0.967780389813594,339.822093339992));
#56755=CARTESIAN_POINT('Ctrl Pts',(104.951737366875,-0.833234863466634,
339.849096243659));
#56756=CARTESIAN_POINT('Ctrl Pts',(104.943990223569,-0.697559310384833,
339.870463581708));
#56757=CARTESIAN_POINT('Ctrl Pts',(104.936243080263,-0.56126434803956,339.886119666373));
#56758=CARTESIAN_POINT('Ctrl Pts',(104.928494195235,-0.424938743693313,
339.901779270859));
#56759=CARTESIAN_POINT('Ctrl Pts',(104.920745310207,-0.287993841223883,
339.911725022325));
#56760=CARTESIAN_POINT('Ctrl Pts',(104.912996425179,-0.150945029684462,
339.915933142397));
#56761=CARTESIAN_POINT('Ctrl Pts',(104.905239315404,-0.0137507531200268,
339.92014572901));
#56762=CARTESIAN_POINT('Ctrl Pts',(104.897482205629,0.123547261522099,339.918608506904));
#56763=CARTESIAN_POINT('Ctrl Pts',(104.889725095855,0.260433417295594,339.911349865124));
#56764=CARTESIAN_POINT('Ctrl Pts',(104.881963840928,0.397392720653963,339.904087344558));
#56765=CARTESIAN_POINT('Ctrl Pts',(104.874202586002,0.533939337686005,339.891097349283));
#56766=CARTESIAN_POINT('Ctrl Pts',(104.866441331076,0.669564132802064,339.872460049561));
#56767=CARTESIAN_POINT('Ctrl Pts',(104.858667660671,0.805405883390107,339.853792936233));
#56768=CARTESIAN_POINT('Ctrl Pts',(104.850893990267,0.940322480474719,339.829460535569));
#56769=CARTESIAN_POINT('Ctrl Pts',(104.843120319862,1.07381542145992,339.799594097748));
#56770=CARTESIAN_POINT('Ctrl Pts',(104.835708515685,1.20109423392509,339.771117949793));
#56771=CARTESIAN_POINT('Ctrl Pts',(104.828296711508,1.32707867176214,339.737611462832));
#56772=CARTESIAN_POINT('Ctrl Pts',(104.820884907331,1.45135235581407,339.699229660463));
#56773=CARTESIAN_POINT('Ctrl Pts',(104.813109828553,1.58171706331423,339.658966651626));
#56774=CARTESIAN_POINT('Ctrl Pts',(104.805334749774,1.71061105505814,339.613211097475));
#56775=CARTESIAN_POINT('Ctrl Pts',(104.797559670996,1.8375367094602,339.562087450267));
#56776=CARTESIAN_POINT('Ctrl Pts',(104.789794159947,1.96430617376386,339.511026713963));
#56777=CARTESIAN_POINT('Ctrl Pts',(104.782028648898,2.0891117610358,339.454611172852));
#56778=CARTESIAN_POINT('Ctrl Pts',(104.774263137849,2.21146999921276,339.393015308997));
#56779=CARTESIAN_POINT('Ctrl Pts',(104.766505326326,2.33370691884083,339.33148051762));
#56780=CARTESIAN_POINT('Ctrl Pts',(104.758747514804,2.45350097147044,339.26477579966));
#56781=CARTESIAN_POINT('Ctrl Pts',(104.750989703282,2.57038804081908,339.193123940705));
#56782=CARTESIAN_POINT('Ctrl Pts',(104.743237729759,2.68718714894094,339.121526002046));
#56783=CARTESIAN_POINT('Ctrl Pts',(104.735485756236,2.80108329618332,339.044988536062));
#56784=CARTESIAN_POINT('Ctrl Pts',(104.727733782713,2.91163671335181,338.96378035617));
#56785=CARTESIAN_POINT('Ctrl Pts',(104.719985092155,3.02214331108264,338.882606567991));
#56786=CARTESIAN_POINT('Ctrl Pts',(104.712236401598,3.12930968000112,338.796766231026));
#56787=CARTESIAN_POINT('Ctrl Pts',(104.70448771104,3.23272500658261,338.70657147433));
#56788=CARTESIAN_POINT('Ctrl Pts',(104.696740632662,3.33611881674152,338.616395483406));
#56789=CARTESIAN_POINT('Ctrl Pts',(104.688993554284,3.43576284251314,338.521867131554));
#56790=CARTESIAN_POINT('Ctrl Pts',(104.681246475907,3.53127966429302,338.423338574411));
#56791=CARTESIAN_POINT('Ctrl Pts',(104.673499332601,3.62679728659593,338.324809191504));
#56792=CARTESIAN_POINT('Ctrl Pts',(104.665752189295,3.71818736384754,338.222279817082));
#56793=CARTESIAN_POINT('Ctrl Pts',(104.658005045989,3.80510992417901,338.116138881278));
#56794=CARTESIAN_POINT('Ctrl Pts',(104.650256160961,3.89205202654741,338.009974082739));
#56795=CARTESIAN_POINT('Ctrl Pts',(104.642507275933,3.97452436576206,337.900196409467));
#56796=CARTESIAN_POINT('Ctrl Pts',(104.634758390905,4.05222803948967,337.787226395267));
#56797=CARTESIAN_POINT('Ctrl Pts',(104.62700128113,4.13001418869945,337.674136473527));
#56798=CARTESIAN_POINT('Ctrl Pts',(104.619244171355,4.20302133971685,337.557847764803));
#56799=CARTESIAN_POINT('Ctrl Pts',(104.611487061581,4.27099434640244,337.438809208507));
#56800=CARTESIAN_POINT('Ctrl Pts',(104.603725806654,4.33900367568931,337.319707041813));
#56801=CARTESIAN_POINT('Ctrl Pts',(104.595964551728,4.40197332105235,337.197852446648));
#56802=CARTESIAN_POINT('Ctrl Pts',(104.588203296802,4.45969517689283,337.073716950719));
#56803=CARTESIAN_POINT('Ctrl Pts',(104.580429626398,4.51750936889123,336.949382878452));
#56804=CARTESIAN_POINT('Ctrl Pts',(104.572655955993,4.57005884625894,336.822760975452));
#56805=CARTESIAN_POINT('Ctrl Pts',(104.564882285588,4.61718421171329,336.69434147019));
#56806=CARTESIAN_POINT('Ctrl Pts',(104.557470481411,4.66211588006781,336.571899923794));
#56807=CARTESIAN_POINT('Ctrl Pts',(104.550058677234,4.70211696865175,336.44782463956));
#56808=CARTESIAN_POINT('Ctrl Pts',(104.542646873057,4.73709251346281,336.322549651769));
#56809=CARTESIAN_POINT('Ctrl Pts',(104.534871794279,4.77378231391201,336.191134563651));
#56810=CARTESIAN_POINT('Ctrl Pts',(104.5270967155,4.80505742714246,336.057983900356));
#56811=CARTESIAN_POINT('Ctrl Pts',(104.519321636722,4.83075321612019,335.923583470751));
#56812=CARTESIAN_POINT('Ctrl Pts',(104.511556125673,4.85641738479367,335.789348429431));
#56813=CARTESIAN_POINT('Ctrl Pts',(104.503790614624,4.87651581731665,335.653867062066));
#56814=CARTESIAN_POINT('Ctrl Pts',(104.496025103575,4.89093360490284,335.517640352882));
#56815=CARTESIAN_POINT('Ctrl Pts',(104.488267292052,4.9053370972107,335.381548712877));
#56816=CARTESIAN_POINT('Ctrl Pts',(104.48050948053,4.91407111245435,335.244713587923));
#56817=CARTESIAN_POINT('Ctrl Pts',(104.472751669008,4.91707183583693,335.107645825368));
#56818=CARTESIAN_POINT('Ctrl Pts',(104.464999695485,4.92007030107998,334.970681210653));
#56819=CARTESIAN_POINT('Ctrl Pts',(104.457247721962,4.91734405371076,334.833484696006));
#56820=CARTESIAN_POINT('Ctrl Pts',(104.449495748439,4.90888116032316,334.696571563092));
#56821=CARTESIAN_POINT('Ctrl Pts',(104.441747057881,4.90042185097591,334.559716412971));
#56822=CARTESIAN_POINT('Ctrl Pts',(104.433998367324,4.88623075172543,334.423144795204));
#56823=CARTESIAN_POINT('Ctrl Pts',(104.426249676766,4.86634802378248,334.28737108259));
#56824=CARTESIAN_POINT('Ctrl Pts',(104.418502598388,4.84646943260715,334.151625618832));
#56825=CARTESIAN_POINT('Ctrl Pts',(104.410755520011,4.82090162477888,334.016678116525));
#56826=CARTESIAN_POINT('Ctrl Pts',(104.403008441633,4.78973649208191,333.883036527491));
#56827=CARTESIAN_POINT('Ctrl Pts',(104.395261298327,4.7585710981911,333.749393818412));
#56828=CARTESIAN_POINT('Ctrl Pts',(104.387514155021,4.72180837463398,333.617057425095));
#56829=CARTESIAN_POINT('Ctrl Pts',(104.379767011715,4.67959098231029,333.486523438972));
#56830=CARTESIAN_POINT('Ctrl Pts',(104.372018126687,4.63736409862057,333.355960106038));
#56831=CARTESIAN_POINT('Ctrl Pts',(104.364269241659,4.58968022617278,333.227200358473));
#56832=CARTESIAN_POINT('Ctrl Pts',(104.356520356631,4.53673124761302,333.100723124599));
#56833=CARTESIAN_POINT('Ctrl Pts',(104.348763246856,4.4837260684603,332.974111646483));
#56834=CARTESIAN_POINT('Ctrl Pts',(104.341006137082,4.42544477094841,332.849787882718));
#56835=CARTESIAN_POINT('Ctrl Pts',(104.333249027307,4.36212680359099,332.728209338013));
#56836=CARTESIAN_POINT('Ctrl Pts',(104.325487772381,4.29877500113634,332.606565825621));
#56837=CARTESIAN_POINT('Ctrl Pts',(104.317726517455,4.23038136071163,332.487670793977));
#56838=CARTESIAN_POINT('Ctrl Pts',(104.309965262529,4.1572297821454,332.371954414219));
#56839=CARTESIAN_POINT('Ctrl Pts',(104.302191592124,4.0839611848935,332.256052925965));
#56840=CARTESIAN_POINT('Ctrl Pts',(104.294417921719,4.00591966279319,332.143340572076));
#56841=CARTESIAN_POINT('Ctrl Pts',(104.286644251315,3.92343120040872,332.034216683883));
#56842=CARTESIAN_POINT('Ctrl Pts',(104.279232447137,3.84478259579287,331.930172538937));
#56843=CARTESIAN_POINT('Ctrl Pts',(104.27182064296,3.76209192654405,331.829390514423));
#56844=CARTESIAN_POINT('Ctrl Pts',(104.264408838783,3.67567279087798,331.732185348448));
#56845=CARTESIAN_POINT('Ctrl Pts',(104.256633760005,3.5850179959445,331.63021586773));
#56846=CARTESIAN_POINT('Ctrl Pts',(104.248858681226,3.48997352086974,331.531860493697));
#56847=CARTESIAN_POINT('Ctrl Pts',(104.241083602448,3.39085879814743,331.437520572196));
#56848=CARTESIAN_POINT('Ctrl Pts',(104.233318091399,3.2918660424014,331.343296741974));
#56849=CARTESIAN_POINT('Ctrl Pts',(104.22555258035,3.18881328530124,331.253078799483));
#56850=CARTESIAN_POINT('Ctrl Pts',(104.217787069301,3.08205963143479,331.167234485286));
#56851=CARTESIAN_POINT('Ctrl Pts',(104.210029257778,2.97541182412724,331.081475285976));
#56852=CARTESIAN_POINT('Ctrl Pts',(104.202271446256,2.86507072511024,331.000081328516));
#56853=CARTESIAN_POINT('Ctrl Pts',(104.194513634734,2.75143138296973,330.923382724941));
#56854=CARTESIAN_POINT('Ctrl Pts',(104.186761661211,2.63787755803828,330.846741839498));
#56855=CARTESIAN_POINT('Ctrl Pts',(104.179009687688,2.52103075302939,330.774789492663));
#56856=CARTESIAN_POINT('Ctrl Pts',(104.171257714165,2.40131782143594,330.707814567967));
#56857=CARTESIAN_POINT('Ctrl Pts',(104.163509023608,2.28165558833945,330.640868007191));
#56858=CARTESIAN_POINT('Ctrl Pts',(104.15576033305,2.15912998324193,330.578894866453));
#56859=CARTESIAN_POINT('Ctrl Pts',(104.148011642492,2.03419528673923,330.522139729971));
#56860=CARTESIAN_POINT('Ctrl Pts',(104.140264564115,1.90928658394378,330.465396401868));
#56861=CARTESIAN_POINT('Ctrl Pts',(104.132517485737,1.78197014237945,330.413869080152));
#56862=CARTESIAN_POINT('Ctrl Pts',(104.124770407359,1.65272283748507,330.367755372937));
#56863=CARTESIAN_POINT('Ctrl Pts',(104.117023264053,1.5234744493737,330.321641279244));
#56864=CARTESIAN_POINT('Ctrl Pts',(104.109276120747,1.39229553379929,330.280941021897));
#56865=CARTESIAN_POINT('Ctrl Pts',(104.101528977441,1.25968046662818,330.245803097841));
#56866=CARTESIAN_POINT('Ctrl Pts',(104.093780092413,1.12703558477439,330.210657274034));
#56867=CARTESIAN_POINT('Ctrl Pts',(104.086031207385,0.992954286596443,330.181076372026));
#56868=CARTESIAN_POINT('Ctrl Pts',(104.078282322357,0.857943151847668,330.157158209202));
#56869=CARTESIAN_POINT('Ctrl Pts',(104.070525212582,0.722788714885544,330.133214659394));
#56870=CARTESIAN_POINT('Ctrl Pts',(104.062768102808,0.586702855340249,330.114945923579));
#56871=CARTESIAN_POINT('Ctrl Pts',(104.055010993033,0.450199878011816,330.102398226444));
#56872=CARTESIAN_POINT('Ctrl Pts',(104.047249738107,0.313623957856817,330.089843824221));
#56873=CARTESIAN_POINT('Ctrl Pts',(104.039488483181,0.176630865973257,330.083016571751));
#56874=CARTESIAN_POINT('Ctrl Pts',(104.031727228254,0.0397359769346117,
330.081910521896));
#56875=CARTESIAN_POINT('Ctrl Pts',(104.02395355785,-0.097377899312462,330.080802702722));
#56876=CARTESIAN_POINT('Ctrl Pts',(104.016179887445,-0.234392867940548,
330.085434361476));
#56877=CARTESIAN_POINT('Ctrl Pts',(104.008406217041,-0.370796713761589,
330.095747471881));
#56878=CARTESIAN_POINT('Ctrl Pts',(104.000994412863,-0.500850927742978,
330.105580504515));
#56879=CARTESIAN_POINT('Ctrl Pts',(103.993582608686,-0.630349348166679,
330.120577916078));
#56880=CARTESIAN_POINT('Ctrl Pts',(103.986170804509,-0.758857599052846,
330.14064631799));
#56881=CARTESIAN_POINT('Ctrl Pts',(103.978395725731,-0.893664422121261,
330.161698332061));
#56882=CARTESIAN_POINT('Ctrl Pts',(103.970620646952,-1.02780757357939,330.188397522317));
#56883=CARTESIAN_POINT('Ctrl Pts',(103.962845568174,-1.16077668989048,330.220692462426));
#56884=CARTESIAN_POINT('Ctrl Pts',(103.955080057125,-1.29358217923854,330.252947661556));
#56885=CARTESIAN_POINT('Ctrl Pts',(103.947314546076,-1.42521613182715,330.290784818149));
#56886=CARTESIAN_POINT('Ctrl Pts',(103.939549035027,-1.55517497467427,330.334100959017));
#56887=CARTESIAN_POINT('Ctrl Pts',(103.931791223505,-1.68500496295034,330.377374151805));
#56888=CARTESIAN_POINT('Ctrl Pts',(103.924033411983,-1.81316277829227,330.426115395226));
#56889=CARTESIAN_POINT('Ctrl Pts',(103.91627560046,-1.93915703898772,330.480171127062));
#56890=CARTESIAN_POINT('Ctrl Pts',(103.908523626937,-2.06505648500657,330.534186180245));
#56891=CARTESIAN_POINT('Ctrl Pts',(103.900771653414,-2.18879525935524,330.593507607898));
#56892=CARTESIAN_POINT('Ctrl Pts',(103.893019679891,-2.30989943879194,330.657932791265));
#56893=CARTESIAN_POINT('Ctrl Pts',(103.885270989334,-2.43095233053667,330.722330690529));
#56894=CARTESIAN_POINT('Ctrl Pts',(103.877522298776,-2.54937250215816,330.791827863354));
#56895=CARTESIAN_POINT('Ctrl Pts',(103.869773608219,-2.66470844027314,330.866174654048));
#56896=CARTESIAN_POINT('Ctrl Pts',(103.862026529841,-2.78002038178296,330.940505976271));
#56897=CARTESIAN_POINT('Ctrl Pts',(103.854279451463,-2.89224903784756,331.019684697742));
#56898=CARTESIAN_POINT('Ctrl Pts',(103.846532373085,-3.00097017092505,331.10341674082));
#56899=CARTESIAN_POINT('Ctrl Pts',(103.838785229779,-3.1096922151902,331.187149485654));
#56900=CARTESIAN_POINT('Ctrl Pts',(103.831038086473,-3.2149063681568,331.275435389709));
#56901=CARTESIAN_POINT('Ctrl Pts',(103.823290943168,-3.3162202204275,331.367939081991));
#56902=CARTESIAN_POINT('Ctrl Pts',(103.81554205814,-3.41755685020343,331.460463571067));
#56903=CARTESIAN_POINT('Ctrl Pts',(103.807793173111,-3.51499114581035,331.557207471776));
#56904=CARTESIAN_POINT('Ctrl Pts',(103.800044288083,-3.60816671115022,331.657797724995));
#56905=CARTESIAN_POINT('Ctrl Pts',(103.792287178309,-3.70144117399769,331.758494745748));
#56906=CARTESIAN_POINT('Ctrl Pts',(103.784530068534,-3.79044761089548,331.863045987095));
#56907=CARTESIAN_POINT('Ctrl Pts',(103.776772958759,-3.87486883068108,331.971043973988));
#56908=CARTESIAN_POINT('Ctrl Pts',(103.769011703833,-3.95933516246709,332.079099671551));
#56909=CARTESIAN_POINT('Ctrl Pts',(103.761250448907,-4.03921116740232,332.190605467076));
#56910=CARTESIAN_POINT('Ctrl Pts',(103.753489193981,-4.11422294780748,332.305124752751));
#56911=CARTESIAN_POINT('Ctrl Pts',(103.745715523576,-4.1893547226151,332.419827231962));
#56912=CARTESIAN_POINT('Ctrl Pts',(103.737941853171,-4.25960652339841,332.537552498484));
#56913=CARTESIAN_POINT('Ctrl Pts',(103.730168182767,-4.3247499566633,332.657838418289));
#56914=CARTESIAN_POINT('Ctrl Pts',(103.72275637859,-4.3868609474371,332.772524999589));
#56915=CARTESIAN_POINT('Ctrl Pts',(103.715344574412,-4.44432833000703,332.889538943999));
#56916=CARTESIAN_POINT('Ctrl Pts',(103.707932770235,-4.49699557105443,333.008464437572));
#56917=CARTESIAN_POINT('Ctrl Pts',(103.69938140188,-4.5577603953395,333.145674714325));
#56918=CARTESIAN_POINT('Ctrl Pts',(103.690830033525,-4.6123013316562,333.285802805362));
#56919=CARTESIAN_POINT('Ctrl Pts',(103.682278665169,-4.66035602045924,333.42829238563));
#56920=CARTESIAN_POINT('Ctrl Pts',(103.673760056184,-4.70822661693014,333.570236103677));
#56921=CARTESIAN_POINT('Ctrl Pts',(103.665241447199,-4.74966043838958,333.714523022454));
#56922=CARTESIAN_POINT('Ctrl Pts',(103.656722838214,-4.7844438726408,333.860579141823));
#56923=CARTESIAN_POINT('Ctrl Pts',(103.648225198979,-4.81914168259438,334.006275723586));
#56924=CARTESIAN_POINT('Ctrl Pts',(103.639727559743,-4.84722168144211,334.153732572376));
#56925=CARTESIAN_POINT('Ctrl Pts',(103.631229920508,-4.86851934992104,334.302359403457));
#56926=CARTESIAN_POINT('Ctrl Pts',(103.62276552463,-4.88973370043676,334.450404796019));
#56927=CARTESIAN_POINT('Ctrl Pts',(103.614301128751,-4.90421858397522,334.599610788059));
#56928=CARTESIAN_POINT('Ctrl Pts',(103.605836732873,-4.91186026695796,334.749377214963));
#56929=CARTESIAN_POINT('Ctrl Pts',(103.601163614099,-4.91607917315269,334.83206194654));
#56930=CARTESIAN_POINT('Ctrl Pts',(103.596490495326,-4.91821311226992,334.914917225596));
#56931=CARTESIAN_POINT('Ctrl Pts',(103.591817376553,-4.91824952580637,334.997840276542));
#56932=CARTESIAN_POINT('',(101.841817376472,-4.91824811790539,335.004302699158));
#56933=CARTESIAN_POINT('Ctrl Pts',(103.591817376509,-4.91824952580671,334.997840277318));
#56934=CARTESIAN_POINT('Ctrl Pts',(103.583929525821,-4.91831098892144,335.137807754317));
#56935=CARTESIAN_POINT('Ctrl Pts',(103.576041675134,-4.91239314012991,335.277751606086));
#56936=CARTESIAN_POINT('Ctrl Pts',(103.568153824446,-4.90052846099034,335.417137705708));
#56937=CARTESIAN_POINT('Ctrl Pts',(103.560262823948,-4.88865904399659,335.556579465581));
#56938=CARTESIAN_POINT('Ctrl Pts',(103.552371823451,-4.87083809652471,335.695462660097));
#56939=CARTESIAN_POINT('Ctrl Pts',(103.544480822953,-4.84714990479059,335.833259181161));
#56940=CARTESIAN_POINT('Ctrl Pts',(103.536585223407,-4.82344790705798,335.971136013064));
#56941=CARTESIAN_POINT('Ctrl Pts',(103.528689623861,-4.79387191458711,336.10792454456));
#56942=CARTESIAN_POINT('Ctrl Pts',(103.520794024314,-4.75855712104157,336.243107874758));
#56943=CARTESIAN_POINT('Ctrl Pts',(103.512886603557,-4.72318945454764,336.378493600057));
#56944=CARTESIAN_POINT('Ctrl Pts',(103.5049791828,-4.68206591424285,336.512268963163));
#56945=CARTESIAN_POINT('Ctrl Pts',(103.497071762043,-4.63537159557901,336.643932247205));
#56946=CARTESIAN_POINT('Ctrl Pts',(103.489158134885,-4.58864062733358,336.775698871533));
#56947=CARTESIAN_POINT('Ctrl Pts',(103.481244507727,-4.53633030194542,336.905349768461));
#56948=CARTESIAN_POINT('Ctrl Pts',(103.473330880569,-4.47867326865673,337.032404687832));
#56949=CARTESIAN_POINT('Ctrl Pts',(103.465402634855,-4.42090972762745,337.159694311133));
#56950=CARTESIAN_POINT('Ctrl Pts',(103.457474389141,-4.35777990602733,337.284378041659));
#56951=CARTESIAN_POINT('Ctrl Pts',(103.449546143427,-4.28956225889343,337.406000558931));
#56952=CARTESIAN_POINT('Ctrl Pts',(103.442929007605,-4.23262590085788,337.507510116642));
#56953=CARTESIAN_POINT('Ctrl Pts',(103.436311871783,-4.17214620241084,337.606887630587));
#56954=CARTESIAN_POINT('Ctrl Pts',(103.429694735961,-4.10830708304314,337.703885347776));
#56955=CARTESIAN_POINT('Ctrl Pts',(103.421919657183,-4.03329665624005,337.817856847341));
#56956=CARTESIAN_POINT('Ctrl Pts',(103.414144578404,-3.95342145703706,337.928884701484));
#56957=CARTESIAN_POINT('Ctrl Pts',(103.406369499626,-3.86893973295263,338.036525712929));
#56958=CARTESIAN_POINT('Ctrl Pts',(103.398603988577,-3.78456196900823,338.144034265257));
#56959=CARTESIAN_POINT('Ctrl Pts',(103.390838477528,-3.69558919813373,338.248163962923));
#56960=CARTESIAN_POINT('Ctrl Pts',(103.383072966479,-3.60232376947725,338.348499144745));
#56961=CARTESIAN_POINT('Ctrl Pts',(103.375315154957,-3.50915081376474,338.448734843943));
#56962=CARTESIAN_POINT('Ctrl Pts',(103.367557343434,-3.41169393471967,338.545183229985));
#56963=CARTESIAN_POINT('Ctrl Pts',(103.359799531912,-3.31029647385732,338.637460696374));
#56964=CARTESIAN_POINT('Ctrl Pts',(103.352047558389,-3.20897531779949,338.729668721044));
#56965=CARTESIAN_POINT('Ctrl Pts',(103.344295584866,-3.10371977035404,338.817711811562));
#56966=CARTESIAN_POINT('Ctrl Pts',(103.336543611343,-2.99491058842981,338.901242575105));
#56967=CARTESIAN_POINT('Ctrl Pts',(103.328794920785,-2.88614748725895,338.984737963319));
#56968=CARTESIAN_POINT('Ctrl Pts',(103.321046230228,-2.77383405428439,339.063724587826));
#56969=CARTESIAN_POINT('Ctrl Pts',(103.31329753967,-2.65838457234053,339.137894939222));
#56970=CARTESIAN_POINT('Ctrl Pts',(103.305550461292,-2.54295911062556,339.212049858858));
#56971=CARTESIAN_POINT('Ctrl Pts',(103.297803382915,-2.42439922642217,339.281390287423));
#56972=CARTESIAN_POINT('Ctrl Pts',(103.290056304537,-2.30314833251895,339.34565194429));
#56973=CARTESIAN_POINT('Ctrl Pts',(103.282309161231,-2.18189642241679,339.409914139732));
#56974=CARTESIAN_POINT('Ctrl Pts',(103.274562017925,-2.05795380299812,339.469097295537));
#56975=CARTESIAN_POINT('Ctrl Pts',(103.266814874619,-1.93178828353325,339.522983206923));
#56976=CARTESIAN_POINT('Ctrl Pts',(103.259065989591,-1.80559439938113,339.576881233005));
#56977=CARTESIAN_POINT('Ctrl Pts',(103.251317104563,-1.67717698011644,339.625479491349));
#56978=CARTESIAN_POINT('Ctrl Pts',(103.243568219535,-1.54702321632472,339.668608168464));
#56979=CARTESIAN_POINT('Ctrl Pts',(103.23581110976,-1.41673130598302,339.711782622804));
#56980=CARTESIAN_POINT('Ctrl Pts',(103.228053999986,-1.284699741221,339.749475775802));
#56981=CARTESIAN_POINT('Ctrl Pts',(103.220296890211,-1.15143079348762,339.781567754441));
#56982=CARTESIAN_POINT('Ctrl Pts',(103.212535635285,-1.0180906310896,339.813676882007));
#56983=CARTESIAN_POINT('Ctrl Pts',(103.204774380358,-0.883512151498329,
339.840178795731));
#56984=CARTESIAN_POINT('Ctrl Pts',(103.197013125432,-0.74820620472424,339.861005095421));
#56985=CARTESIAN_POINT('Ctrl Pts',(103.189239455028,-0.612683812531602,
339.881864710404));
#56986=CARTESIAN_POINT('Ctrl Pts',(103.181465784623,-0.476432016397678,
339.897030525293));
#56987=CARTESIAN_POINT('Ctrl Pts',(103.173692114218,-0.339966046539224,
339.906486130593));
#56988=CARTESIAN_POINT('Ctrl Pts',(103.166280310041,-0.20985260041005,339.915501575191));
#56989=CARTESIAN_POINT('Ctrl Pts',(103.158868505864,-0.079544759074796,
339.91932645848));
#56990=CARTESIAN_POINT('Ctrl Pts',(103.151456701687,0.0505141765631969,
339.917990583609));
#56991=CARTESIAN_POINT('Ctrl Pts',(103.143681622909,0.186947688063153,339.916589233531));
#56992=CARTESIAN_POINT('Ctrl Pts',(103.13590654413,0.323538432814568,339.909504017112));
#56993=CARTESIAN_POINT('Ctrl Pts',(103.128131465352,0.459773964221454,339.896712260724));
#56994=CARTESIAN_POINT('Ctrl Pts',(103.120365954303,0.595841849133858,339.883936245406));
#56995=CARTESIAN_POINT('Ctrl Pts',(103.112600443254,0.731555004988187,339.865467698595));
#56996=CARTESIAN_POINT('Ctrl Pts',(103.104834932205,0.866400274955407,339.841335934022));
#56997=CARTESIAN_POINT('Ctrl Pts',(103.097077120682,1.00111184544505,339.817228096165));
#56998=CARTESIAN_POINT('Ctrl Pts',(103.08931930916,1.13495686023082,339.787468283319));
#56999=CARTESIAN_POINT('Ctrl Pts',(103.081561497638,1.26742693462888,339.752137627203));
#57000=CARTESIAN_POINT('Ctrl Pts',(103.073809524115,1.39979732109473,339.716833558526));
#57001=CARTESIAN_POINT('Ctrl Pts',(103.066057550592,1.53079445051333,339.675967091341));
#57002=CARTESIAN_POINT('Ctrl Pts',(103.058305577069,1.65992014343549,339.629670418066));
#57003=CARTESIAN_POINT('Ctrl Pts',(103.050556886511,1.78899115155012,339.58339335146));
#57004=CARTESIAN_POINT('Ctrl Pts',(103.042808195954,1.91619193232941,339.531690784341));
#57005=CARTESIAN_POINT('Ctrl Pts',(103.035059505396,2.04103970234368,339.474744685002));
#57006=CARTESIAN_POINT('Ctrl Pts',(103.027312427018,2.16586149673648,339.417810433775));
#57007=CARTESIAN_POINT('Ctrl Pts',(103.01956534864,2.28833089873702,339.355634982434));
#57008=CARTESIAN_POINT('Ctrl Pts',(103.011818270262,2.40798571302497,339.28844818884));
#57009=CARTESIAN_POINT('Ctrl Pts',(103.004071126957,2.52764153013551,339.221260832157));
#57010=CARTESIAN_POINT('Ctrl Pts',(102.996323983651,2.64448237166226,339.149062240822));
#57011=CARTESIAN_POINT('Ctrl Pts',(102.988576840345,2.75807158611075,339.072127722504));
#57012=CARTESIAN_POINT('Ctrl Pts',(102.980827955317,2.87168633782614,338.995175907674));
#57013=CARTESIAN_POINT('Ctrl Pts',(102.973079070289,2.98204768421959,338.913486266305));
#57014=CARTESIAN_POINT('Ctrl Pts',(102.965330185261,3.08874917872546,338.827376591534));
#57015=CARTESIAN_POINT('Ctrl Pts',(102.957573075486,3.19556392730025,338.741175519064));
#57016=CARTESIAN_POINT('Ctrl Pts',(102.949815965711,3.29871075946694,338.650545287406));
#57017=CARTESIAN_POINT('Ctrl Pts',(102.942058855936,3.39781706354589,338.555843397167));
#57018=CARTESIAN_POINT('Ctrl Pts',(102.93429760101,3.49697632686494,338.461090901266));
#57019=CARTESIAN_POINT('Ctrl Pts',(102.926536346084,3.59209048892746,338.362262692867));
#57020=CARTESIAN_POINT('Ctrl Pts',(102.918775091158,3.6828255802995,338.259751341374));
#57021=CARTESIAN_POINT('Ctrl Pts',(102.911001420753,3.77370581824706,338.157076005127));
#57022=CARTESIAN_POINT('Ctrl Pts',(102.903227750349,3.86019274055043,338.050706055605));
#57023=CARTESIAN_POINT('Ctrl Pts',(102.895454079944,3.94199372747953,337.941065880767));
#57024=CARTESIAN_POINT('Ctrl Pts',(102.888042275767,4.01998685878547,337.836529482448));
#57025=CARTESIAN_POINT('Ctrl Pts',(102.88063047159,4.09372033475148,337.729020702494));
#57026=CARTESIAN_POINT('Ctrl Pts',(102.873218667413,4.16297932192538,337.618928450287));
#57027=CARTESIAN_POINT('Ctrl Pts',(102.865443588635,4.23563289837379,337.503440248849));
#57028=CARTESIAN_POINT('Ctrl Pts',(102.857668509856,4.30359187829115,337.384743960398));
#57029=CARTESIAN_POINT('Ctrl Pts',(102.849893431078,4.36655988068137,337.263258242208));
#57030=CARTESIAN_POINT('Ctrl Pts',(102.842127920029,4.42945039693583,337.141922019929));
#57031=CARTESIAN_POINT('Ctrl Pts',(102.83436240898,4.48736197776486,337.017803541454));
#57032=CARTESIAN_POINT('Ctrl Pts',(102.826596897931,4.54004157510634,336.891350194651));
#57033=CARTESIAN_POINT('Ctrl Pts',(102.818839086409,4.59266894047375,336.765022226709));
#57034=CARTESIAN_POINT('Ctrl Pts',(102.811081274886,4.64007449647996,336.63636435597));
#57035=CARTESIAN_POINT('Ctrl Pts',(102.803323463364,4.68205135239322,336.505847998987));
#57036=CARTESIAN_POINT('Ctrl Pts',(102.795571489841,4.72399661939116,336.375429859702));
#57037=CARTESIAN_POINT('Ctrl Pts',(102.787819516318,4.76052119863007,336.243156388562));
#57038=CARTESIAN_POINT('Ctrl Pts',(102.780067542795,4.79146666004779,336.109518052197));
#57039=CARTESIAN_POINT('Ctrl Pts',(102.772318852238,4.82239901604427,335.975936311746));
#57040=CARTESIAN_POINT('Ctrl Pts',(102.76457016168,4.84775686558752,335.840991235719));
#57041=CARTESIAN_POINT('Ctrl Pts',(102.756821471122,4.86743196788014,335.705187280485));
#57042=CARTESIAN_POINT('Ctrl Pts',(102.749074392745,4.88710297660338,335.569411580399));
#57043=CARTESIAN_POINT('Ctrl Pts',(102.741327314367,4.90109353383086,335.43277774314));
#57044=CARTESIAN_POINT('Ctrl Pts',(102.733580235989,4.90934681153394,335.295798827891));
#57045=CARTESIAN_POINT('Ctrl Pts',(102.725833092683,4.91760015840744,335.158818764627));
#57046=CARTESIAN_POINT('Ctrl Pts',(102.718085949377,4.92011610634116,335.021494007772));
#57047=CARTESIAN_POINT('Ctrl Pts',(102.710338806072,4.91688987024794,334.884340731659));
#57048=CARTESIAN_POINT('Ctrl Pts',(102.702589921043,4.91366290882836,334.747156620578));
#57049=CARTESIAN_POINT('Ctrl Pts',(102.694841036015,4.90469120369609,334.610144457645));
#57050=CARTESIAN_POINT('Ctrl Pts',(102.687092150987,4.89002204231956,334.473818008548));
#57051=CARTESIAN_POINT('Ctrl Pts',(102.679335041213,4.87533731094359,334.337346861149));
#57052=CARTESIAN_POINT('Ctrl Pts',(102.671577931438,4.85494308508052,334.201563270727));
#57053=CARTESIAN_POINT('Ctrl Pts',(102.663820821663,4.82893835305869,334.066974038486));
#57054=CARTESIAN_POINT('Ctrl Pts',(102.656059566737,4.80291972493951,333.932312886062));
#57055=CARTESIAN_POINT('Ctrl Pts',(102.648298311811,4.77128470683159,333.798847743687));
#57056=CARTESIAN_POINT('Ctrl Pts',(102.640537056885,4.73418268869762,333.667071895211));
#57057=CARTESIAN_POINT('Ctrl Pts',(102.63276338648,4.69702131942618,333.535085248324));
#57058=CARTESIAN_POINT('Ctrl Pts',(102.624989716076,4.65437559584653,333.404793667048));
#57059=CARTESIAN_POINT('Ctrl Pts',(102.617216045671,4.60644404152253,333.276672882236));
#57060=CARTESIAN_POINT('Ctrl Pts',(102.609804241494,4.56074371258291,333.154516150778));
#57061=CARTESIAN_POINT('Ctrl Pts',(102.602392437316,4.51023870059003,333.034332928113));
#57062=CARTESIAN_POINT('Ctrl Pts',(102.594980633139,4.455139789031,332.916514333456));
#57063=CARTESIAN_POINT('Ctrl Pts',(102.587205554361,4.39734031568635,332.792921098515));
#57064=CARTESIAN_POINT('Ctrl Pts',(102.579430475582,4.33430257797251,332.671539569988));
#57065=CARTESIAN_POINT('Ctrl Pts',(102.571655396804,4.26621824495883,332.552845540453));
#57066=CARTESIAN_POINT('Ctrl Pts',(102.563889885755,4.19821769405148,332.434297571478));
#57067=CARTESIAN_POINT('Ctrl Pts',(102.556124374706,4.12518309690227,332.318430857049));
#57068=CARTESIAN_POINT('Ctrl Pts',(102.548358863657,4.04735373268759,332.205700297928));
#57069=CARTESIAN_POINT('Ctrl Pts',(102.540601052135,3.96960153651417,332.093081511484));
#57070=CARTESIAN_POINT('Ctrl Pts',(102.532843240613,3.88706425469921,331.983593011841));
#57071=CARTESIAN_POINT('Ctrl Pts',(102.52508542909,3.80002635103384,331.877663888376));
#57072=CARTESIAN_POINT('Ctrl Pts',(102.517333455567,3.71305394615075,331.771814479936));
#57073=CARTESIAN_POINT('Ctrl Pts',(102.509581482044,3.62158790794401,331.669519416952));
#57074=CARTESIAN_POINT('Ctrl Pts',(102.501829508521,3.52595494466814,331.571177346279));
#57075=CARTESIAN_POINT('Ctrl Pts',(102.494080817964,3.43036248200924,331.472876923532));
#57076=CARTESIAN_POINT('Ctrl Pts',(102.486332127406,3.33060687607175,331.37852644308));
#57077=CARTESIAN_POINT('Ctrl Pts',(102.478583436848,3.22705375967267,331.288489917206));
#57078=CARTESIAN_POINT('Ctrl Pts',(102.470836358471,3.12352218836428,331.198472124183));
#57079=CARTESIAN_POINT('Ctrl Pts',(102.463089280093,3.0161949729509,331.112766756746));
#57080=CARTESIAN_POINT('Ctrl Pts',(102.455342201715,2.90547280293872,331.031699248559));
#57081=CARTESIAN_POINT('Ctrl Pts',(102.447595058409,2.79474970496796,330.950631060949));
#57082=CARTESIAN_POINT('Ctrl Pts',(102.439847915103,2.68063191102454,330.874201041029));
#57083=CARTESIAN_POINT('Ctrl Pts',(102.432100771797,2.5635508936325,330.802692544231));
#57084=CARTESIAN_POINT('Ctrl Pts',(102.424351886769,2.44644355394213,330.731167970804));
#57085=CARTESIAN_POINT('Ctrl Pts',(102.416603001741,2.32637199866117,330.664567325933));
#57086=CARTESIAN_POINT('Ctrl Pts',(102.408854116713,2.20379385428027,330.603128872671));
#57087=CARTESIAN_POINT('Ctrl Pts',(102.401097006938,2.0810856041907,330.541625208));
#57088=CARTESIAN_POINT('Ctrl Pts',(102.393339897164,1.95586580035378,330.485294855583));
#57089=CARTESIAN_POINT('Ctrl Pts',(102.385582787389,1.82861419097799,330.434328833232));
#57090=CARTESIAN_POINT('Ctrl Pts',(102.377821532463,1.70129458241061,330.383335576269));
#57091=CARTESIAN_POINT('Ctrl Pts',(102.370060277537,1.57194137331711,330.337712491132));
#57092=CARTESIAN_POINT('Ctrl Pts',(102.36229902261,1.44105022009306,330.297600896811));
#57093=CARTESIAN_POINT('Ctrl Pts',(102.354525352206,1.30994968368136,330.257425137012));
#57094=CARTESIAN_POINT('Ctrl Pts',(102.346751681801,1.17730666529713,330.22277858502));
#57095=CARTESIAN_POINT('Ctrl Pts',(102.338978011396,1.04362864965377,330.193751743395));
#57096=CARTESIAN_POINT('Ctrl Pts',(102.331566207219,0.916173377803752,330.166076108232));
#57097=CARTESIAN_POINT('Ctrl Pts',(102.324154403043,0.787777581908544,330.143508812399));
#57098=CARTESIAN_POINT('Ctrl Pts',(102.316742598866,0.658884229499549,330.126084260616));
#57099=CARTESIAN_POINT('Ctrl Pts',(102.308967520087,0.523673429931368,330.107805679644));
#57100=CARTESIAN_POINT('Ctrl Pts',(102.301192441309,0.387487776050841,330.095128948182));
#57101=CARTESIAN_POINT('Ctrl Pts',(102.29341736253,0.250831095116849,330.088150366285));
#57102=CARTESIAN_POINT('Ctrl Pts',(102.285651851481,0.114342578928736,330.081180371978));
#57103=CARTESIAN_POINT('Ctrl Pts',(102.277886340432,-0.0226154243838896,
330.079894595237));
#57104=CARTESIAN_POINT('Ctrl Pts',(102.270120829383,-0.159530891374533,
330.084337994004));
#57105=CARTESIAN_POINT('Ctrl Pts',(102.262363017861,-0.29631060628113,330.088776987127));
#57106=CARTESIAN_POINT('Ctrl Pts',(102.254605206339,-0.43304748064413,330.098933838655));
#57107=CARTESIAN_POINT('Ctrl Pts',(102.246847394817,-0.569226744371924,
330.114801541801));
#57108=CARTESIAN_POINT('Ctrl Pts',(102.239095421294,-0.705303528885548,
330.130657303997));
#57109=CARTESIAN_POINT('Ctrl Pts',(102.231343447771,-0.840823151312165,
330.152215318597));
#57110=CARTESIAN_POINT('Ctrl Pts',(102.223591474248,-0.975273580423576,
330.179416580348));
#57111=CARTESIAN_POINT('Ctrl Pts',(102.21584278369,-1.10966706969789,330.206606322348));
#57112=CARTESIAN_POINT('Ctrl Pts',(102.208094093132,-1.24299188393726,330.239434480771));
#57113=CARTESIAN_POINT('Ctrl Pts',(102.200345402575,-1.37474405254973,330.277790575114));
#57114=CARTESIAN_POINT('Ctrl Pts',(102.192598324197,-1.506468809023,330.316138689152));
#57115=CARTESIAN_POINT('Ctrl Pts',(102.184851245819,-1.63662119563893,330.360012342225));
#57116=CARTESIAN_POINT('Ctrl Pts',(102.177104167441,-1.76471071220216,330.40925069681));
#57117=CARTESIAN_POINT('Ctrl Pts',(102.169357024135,-1.89280130227917,330.45848946406));
#57118=CARTESIAN_POINT('Ctrl Pts',(102.161609880829,-2.01882862297318,330.51309288225));
#57119=CARTESIAN_POINT('Ctrl Pts',(102.153862737524,-2.14232090011578,330.572851456815));
#57120=CARTESIAN_POINT('Ctrl Pts',(102.146113852495,-2.26584094094325,330.632623466375));
#57121=CARTESIAN_POINT('Ctrl Pts',(102.138364967467,-2.3868244523435,330.697552768341));
#57122=CARTESIAN_POINT('Ctrl Pts',(102.130616082439,-2.50482342587954,330.767383472642));
#57123=CARTESIAN_POINT('Ctrl Pts',(102.122858972665,-2.6229476447459,330.837288295975));
#57124=CARTESIAN_POINT('Ctrl Pts',(102.11510186289,-2.73808066081635,330.91210471454));
#57125=CARTESIAN_POINT('Ctrl Pts',(102.107344753115,-2.84980222385214,330.991532668534));
#57126=CARTESIAN_POINT('Ctrl Pts',(102.099583498189,-2.96158348731882,331.071003066288));
#57127=CARTESIAN_POINT('Ctrl Pts',(102.091822243263,-3.06994935666206,331.155089670224));
#57128=CARTESIAN_POINT('Ctrl Pts',(102.084060988337,-3.17451276561177,331.24345214812));
#57129=CARTESIAN_POINT('Ctrl Pts',(102.076287317932,-3.27924344193879,331.331955977183));
#57130=CARTESIAN_POINT('Ctrl Pts',(102.068513647527,-3.38015921496347,331.424749083855));
#57131=CARTESIAN_POINT('Ctrl Pts',(102.060739977123,-3.47690935005386,331.521453689541));
#57132=CARTESIAN_POINT('Ctrl Pts',(102.053328172945,-3.56915574308011,331.613656672568));
#57133=CARTESIAN_POINT('Ctrl Pts',(102.045916368768,-3.6576153961095,331.709414977858));
#57134=CARTESIAN_POINT('Ctrl Pts',(102.038504564591,-3.74201966233167,331.808374722931));
#57135=CARTESIAN_POINT('Ctrl Pts',(102.03078102222,-3.8299739459106,331.911496684304));
#57136=CARTESIAN_POINT('Ctrl Pts',(102.02305747985,-3.91381268601028,332.018433581657));
#57137=CARTESIAN_POINT('Ctrl Pts',(102.015333937479,-3.99318321602257,332.128820648971));
#57138=CARTESIAN_POINT('Ctrl Pts',(102.007622832742,-4.07242593142545,332.239029954086));
#57139=CARTESIAN_POINT('Ctrl Pts',(101.999911728005,-4.14721453531853,332.352678046835));
#57140=CARTESIAN_POINT('Ctrl Pts',(101.992200623267,-4.21723515906342,332.469365558667));
#57141=CARTESIAN_POINT('Ctrl Pts',(101.984496712,-4.28719046256242,332.585944216043));
#57142=CARTESIAN_POINT('Ctrl Pts',(101.976792800733,-4.35238642900278,332.705556316164));
#57143=CARTESIAN_POINT('Ctrl Pts',(101.969088889465,-4.41255109860553,332.82777168219));
#57144=CARTESIAN_POINT('Ctrl Pts',(101.961390440342,-4.47267311090889,332.949900396407));
#57145=CARTESIAN_POINT('Ctrl Pts',(101.953691991218,-4.52777074797215,333.074628350676));
#57146=CARTESIAN_POINT('Ctrl Pts',(101.945993542094,-4.57761706477003,333.201499215784));
#57147=CARTESIAN_POINT('Ctrl Pts',(101.93829882817,-4.62743919670017,333.328308524586));
#57148=CARTESIAN_POINT('Ctrl Pts',(101.930604114246,-4.67201493381984,333.457258306925));
#57149=CARTESIAN_POINT('Ctrl Pts',(101.922909400323,-4.71116491965499,333.587871053228));
#57150=CARTESIAN_POINT('Ctrl Pts',(101.915215346244,-4.75031154826039,333.718472599092));
#57151=CARTESIAN_POINT('Ctrl Pts',(101.907521292165,-4.78403322919711,333.850736448018));
#57152=CARTESIAN_POINT('Ctrl Pts',(101.899827238087,-4.81220014008847,333.984168875141));
#57153=CARTESIAN_POINT('Ctrl Pts',(101.892133632618,-4.84036540867839,334.117593522346));
#57154=CARTESIAN_POINT('Ctrl Pts',(101.884440027149,-4.86297647519989,334.252186222965));
#57155=CARTESIAN_POINT('Ctrl Pts',(101.876746421681,-4.8799545760377,334.387442738751));
#57156=CARTESIAN_POINT('Ctrl Pts',(101.869049202525,-4.89694065148953,334.522762784523));
#57157=CARTESIAN_POINT('Ctrl Pts',(101.86135198337,-4.90828843265978,334.658746873884));
#57158=CARTESIAN_POINT('Ctrl Pts',(101.853654764215,-4.91397100480007,334.794885333328));
#57159=CARTESIAN_POINT('Ctrl Pts',(101.849708968313,-4.91688403993803,334.864673469087));
#57160=CARTESIAN_POINT('Ctrl Pts',(101.845763172411,-4.91830918249373,334.934502131675));
#57161=CARTESIAN_POINT('Ctrl Pts',(101.841817376509,-4.91824811790597,335.004302698495));
#57162=CARTESIAN_POINT('',(100.091817376546,-4.91824999882167,335.00010765993));
#57163=CARTESIAN_POINT('Ctrl Pts',(101.841817376472,-4.91824811790539,335.004302699159));
#57164=CARTESIAN_POINT('Ctrl Pts',(101.832410613969,-4.91810254013675,335.17070698639));
#57165=CARTESIAN_POINT('Ctrl Pts',(101.823003851466,-4.90950805915332,335.33674024558));
#57166=CARTESIAN_POINT('Ctrl Pts',(101.813597088963,-4.8925997979356,335.501647565269));
#57167=CARTESIAN_POINT('Ctrl Pts',(101.804058433833,-4.87545446525098,335.66886705767));
#57168=CARTESIAN_POINT('Ctrl Pts',(101.794519778704,-4.84976063729519,335.834928835721));
#57169=CARTESIAN_POINT('Ctrl Pts',(101.784981123574,-4.81570820956695,335.999068317388));
#57170=CARTESIAN_POINT('Ctrl Pts',(101.776742925822,-4.78629833681709,336.140829759703));
#57171=CARTESIAN_POINT('Ctrl Pts',(101.76850472807,-4.75065445968432,336.281157717628));
#57172=CARTESIAN_POINT('Ctrl Pts',(101.760266530318,-4.70892734215704,336.419572593701));
#57173=CARTESIAN_POINT('Ctrl Pts',(101.752491451539,-4.66954595854219,336.550206331559));
#57174=CARTESIAN_POINT('Ctrl Pts',(101.744716372761,-4.62466221922097,336.679406493277));
#57175=CARTESIAN_POINT('Ctrl Pts',(101.736941293982,-4.57439721182412,336.806674627861));
#57176=CARTESIAN_POINT('Ctrl Pts',(101.729175782933,-4.52419405871887,336.933786150903));
#57177=CARTESIAN_POINT('Ctrl Pts',(101.721410271884,-4.46862295561675,337.058970017249));
#57178=CARTESIAN_POINT('Ctrl Pts',(101.713644760835,-4.40785511440055,337.181741587116));
#57179=CARTESIAN_POINT('Ctrl Pts',(101.705886949313,-4.34714752467597,337.304391428615));
#57180=CARTESIAN_POINT('Ctrl Pts',(101.698129137791,-4.28125362304016,337.424633385396));
#57181=CARTESIAN_POINT('Ctrl Pts',(101.690371326269,-4.21039305456203,337.542001846694));
#57182=CARTESIAN_POINT('Ctrl Pts',(101.682619352746,-4.13958581090865,337.659281984503));
#57183=CARTESIAN_POINT('Ctrl Pts',(101.674867379223,-4.06381954108214,337.773692597702));
#57184=CARTESIAN_POINT('Ctrl Pts',(101.6671154057,-3.98336008141318,337.884792111107));
#57185=CARTESIAN_POINT('Ctrl Pts',(101.659366715142,-3.90293469637327,337.995844573801));
#57186=CARTESIAN_POINT('Ctrl Pts',(101.651618024585,-3.81782030341457,338.103588409767));
#57187=CARTESIAN_POINT('Ctrl Pts',(101.643869334027,-3.72832624913155,338.207610706201));
#57188=CARTESIAN_POINT('Ctrl Pts',(101.636122255649,-3.63885081483393,338.311611359927));
#57189=CARTESIAN_POINT('Ctrl Pts',(101.628375177271,-3.54499778646565,338.411891718134));
#57190=CARTESIAN_POINT('Ctrl Pts',(101.620628098893,-3.44711676188987,338.508071990766));
#57191=CARTESIAN_POINT('Ctrl Pts',(101.612880955588,-3.34923491697709,338.604253069482));
#57192=CARTESIAN_POINT('Ctrl Pts',(101.605133812282,-3.24732528732444,338.696333720127));
#57193=CARTESIAN_POINT('Ctrl Pts',(101.597386668976,-3.14177399744879,338.783971354471));
#57194=CARTESIAN_POINT('Ctrl Pts',(101.589637783948,-3.03619897740227,338.871628691615));
#57195=CARTESIAN_POINT('Ctrl Pts',(101.58188889892,-2.92698096863593,338.954840775147));
#57196=CARTESIAN_POINT('Ctrl Pts',(101.574140013892,-2.81453847606166,339.033305868549));
#57197=CARTESIAN_POINT('Ctrl Pts',(101.566382904117,-2.70197663586379,339.111854245612));
#57198=CARTESIAN_POINT('Ctrl Pts',(101.558625794342,-2.58618379614258,339.185645343623));
#57199=CARTESIAN_POINT('Ctrl Pts',(101.550868684568,-2.46760716237224,339.25442098936));
#57200=CARTESIAN_POINT('Ctrl Pts',(101.543107429642,-2.34896716504017,339.323233386604));
#57201=CARTESIAN_POINT('Ctrl Pts',(101.535346174715,-2.22754075539452,339.387024809543));
#57202=CARTESIAN_POINT('Ctrl Pts',(101.527584919789,-2.10379804448129,339.445583971824));
#57203=CARTESIAN_POINT('Ctrl Pts',(101.519811249385,-1.97985738555834,339.50423680968));
#57204=CARTESIAN_POINT('Ctrl Pts',(101.51203757898,-1.8535933812147,339.557640508971));
#57205=CARTESIAN_POINT('Ctrl Pts',(101.504263908575,-1.7254951718925,339.605632364212));
#57206=CARTESIAN_POINT('Ctrl Pts',(101.496852104398,-1.60335996503264,339.651390187045));
#57207=CARTESIAN_POINT('Ctrl Pts',(101.489440300221,-1.4795577480398,339.692228579685));
#57208=CARTESIAN_POINT('Ctrl Pts',(101.482028496044,-1.35452190374054,339.728049648088));
#57209=CARTESIAN_POINT('Ctrl Pts',(101.474253417266,-1.2233576802498,339.765626413759));
#57210=CARTESIAN_POINT('Ctrl Pts',(101.466478338487,-1.09042134112152,339.79780034082));
#57211=CARTESIAN_POINT('Ctrl Pts',(101.458703259709,-0.9561975718951,339.824403514011));
#57212=CARTESIAN_POINT('Ctrl Pts',(101.45093774866,-0.822138973561904,339.850973950303));
#57213=CARTESIAN_POINT('Ctrl Pts',(101.443172237611,-0.686796477113662,
339.871987197276));
#57214=CARTESIAN_POINT('Ctrl Pts',(101.435406726562,-0.550670279055428,
339.887324964259));
#57215=CARTESIAN_POINT('Ctrl Pts',(101.427648915039,-0.41467905051889,339.902647523801));
#57216=CARTESIAN_POINT('Ctrl Pts',(101.419891103517,-0.277906052645194,
339.912305758427));
#57217=CARTESIAN_POINT('Ctrl Pts',(101.412133291995,-0.140861690011362,
339.916232403659));
#57218=CARTESIAN_POINT('Ctrl Pts',(101.404381318472,-0.00392045760633933,
339.920156093966));
#57219=CARTESIAN_POINT('Ctrl Pts',(101.396629344949,0.133291343946892,339.918356768948));
#57220=CARTESIAN_POINT('Ctrl Pts',(101.388877371426,0.270258525362551,339.910819014377));
#57221=CARTESIAN_POINT('Ctrl Pts',(101.381128680868,0.407167701095562,339.90328445205));
#57222=CARTESIAN_POINT('Ctrl Pts',(101.373379990311,0.543832073266215,339.890016315156));
#57223=CARTESIAN_POINT('Ctrl Pts',(101.365631299753,0.679737009496073,339.871051289036));
#57224=CARTESIAN_POINT('Ctrl Pts',(101.357884221375,0.815613669568848,339.852090208748));
#57225=CARTESIAN_POINT('Ctrl Pts',(101.350137142998,0.950730821107749,339.827434650838));
#57226=CARTESIAN_POINT('Ctrl Pts',(101.34239006462,1.08457990309042,339.797173073417));
#57227=CARTESIAN_POINT('Ctrl Pts',(101.334642921314,1.21843010685722,339.766911242374));
#57228=CARTESIAN_POINT('Ctrl Pts',(101.326895778008,1.35101183861837,339.731043384303));
#57229=CARTESIAN_POINT('Ctrl Pts',(101.319148634702,1.48182805448822,339.689708805398));
#57230=CARTESIAN_POINT('Ctrl Pts',(101.311399749674,1.61267368062071,339.648364933603));
#57231=CARTESIAN_POINT('Ctrl Pts',(101.303650864646,1.74175262838628,339.601552013074));
#57232=CARTESIAN_POINT('Ctrl Pts',(101.295901979618,1.86858468408841,339.549458686579));
#57233=CARTESIAN_POINT('Ctrl Pts',(101.288144869843,1.99555136064496,339.497310067689));
#57234=CARTESIAN_POINT('Ctrl Pts',(101.280387760069,2.12026601899166,339.439869995702));
#57235=CARTESIAN_POINT('Ctrl Pts',(101.272630650294,2.2422695472152,339.377374822897));
#57236=CARTESIAN_POINT('Ctrl Pts',(101.264869395368,2.36433827022323,339.31484625467));
#57237=CARTESIAN_POINT('Ctrl Pts',(101.257108140441,2.48369263640856,339.247257395584));
#57238=CARTESIAN_POINT('Ctrl Pts',(101.249346885515,2.59990056650561,339.174889232876));
#57239=CARTESIAN_POINT('Ctrl Pts',(101.241573215111,2.71629439141875,339.102405304693));
#57240=CARTESIAN_POINT('Ctrl Pts',(101.233799544706,2.82953139924868,339.025127015706));
#57241=CARTESIAN_POINT('Ctrl Pts',(101.226025874301,2.9392100655196,338.943377645274));
#57242=CARTESIAN_POINT('Ctrl Pts',(101.218614070124,3.04378316348874,338.865433727703));
#57243=CARTESIAN_POINT('Ctrl Pts',(101.211202265947,3.14512152249386,338.783425799794));
#57244=CARTESIAN_POINT('Ctrl Pts',(101.20379046177,3.24290829302842,338.697665326325));
#57245=CARTESIAN_POINT('Ctrl Pts',(101.196015382992,3.34548788447835,338.607701476585));
#57246=CARTESIAN_POINT('Ctrl Pts',(101.188240304213,3.4444831071328,338.513323631012));
#57247=CARTESIAN_POINT('Ctrl Pts',(101.180465225435,3.53949046630928,338.414848503434));
#57248=CARTESIAN_POINT('Ctrl Pts',(101.172699714386,3.63438091288183,338.31649455577));
#57249=CARTESIAN_POINT('Ctrl Pts',(101.164934203337,3.72529299133774,338.214053636778));
#57250=CARTESIAN_POINT('Ctrl Pts',(101.157168692288,3.81185654349949,338.107882358501));
#57251=CARTESIAN_POINT('Ctrl Pts',(101.149410880766,3.8983342676472,338.001816349355));
#57252=CARTESIAN_POINT('Ctrl Pts',(101.141653069243,3.98047180037617,337.892027642465));
#57253=CARTESIAN_POINT('Ctrl Pts',(101.133895257721,4.05793636834805,337.778909047259));
#57254=CARTESIAN_POINT('Ctrl Pts',(101.126143284198,4.13534264177599,337.665875577383));
#57255=CARTESIAN_POINT('Ctrl Pts',(101.118391310675,4.2080827300135,337.549517528159));
#57256=CARTESIAN_POINT('Ctrl Pts',(101.110639337152,4.2758648724231,337.430259791726));
#57257=CARTESIAN_POINT('Ctrl Pts',(101.102890646594,4.34361830905519,337.311052561014));
#57258=CARTESIAN_POINT('Ctrl Pts',(101.095141956037,4.40641778325965,337.188948424651));
#57259=CARTESIAN_POINT('Ctrl Pts',(101.087393265479,4.46401564741182,337.064400000524));
#57260=CARTESIAN_POINT('Ctrl Pts',(101.079646187101,4.52160152784723,336.939877489737));
#57261=CARTESIAN_POINT('Ctrl Pts',(101.071899108724,4.57398778691545,336.812912057289));
#57262=CARTESIAN_POINT('Ctrl Pts',(101.064152030346,4.6209735993788,336.683979232753));
#57263=CARTESIAN_POINT('Ctrl Pts',(101.05640488704,4.6679598056285,336.555045327636));
#57264=CARTESIAN_POINT('Ctrl Pts',(101.048657743734,4.70954534116398,336.424144364792));
#57265=CARTESIAN_POINT('Ctrl Pts',(101.040910600428,4.74557837256834,336.291769705602));
#57266=CARTESIAN_POINT('Ctrl Pts',(101.0331617154,4.78161950496313,336.159365285779));
#57267=CARTESIAN_POINT('Ctrl Pts',(101.025412830372,4.81210554656546,336.025486887402));
#57268=CARTESIAN_POINT('Ctrl Pts',(101.017663945344,4.83693525991552,335.890640417838));
#57269=CARTESIAN_POINT('Ctrl Pts',(101.009906835569,4.86179132777987,335.755650820837));
#57270=CARTESIAN_POINT('Ctrl Pts',(101.002149725795,4.88097900357264,335.6196914851));
#57271=CARTESIAN_POINT('Ctrl Pts',(100.99439261602,4.89444858916778,335.483276391409));
#57272=CARTESIAN_POINT('Ctrl Pts',(100.986631361094,4.90792537247879,335.346788401854));
#57273=CARTESIAN_POINT('Ctrl Pts',(100.978870106168,4.91567795502317,335.209844559115));
#57274=CARTESIAN_POINT('Ctrl Pts',(100.971108851241,4.91770880208033,335.072960266184));
#57275=CARTESIAN_POINT('Ctrl Pts',(100.963335180837,4.91974289783093,334.935857002994));
#57276=CARTESIAN_POINT('Ctrl Pts',(100.955561510432,4.91603697843713,334.798813870906));
#57277=CARTESIAN_POINT('Ctrl Pts',(100.947787840027,4.90664560847443,334.662343465429));
#57278=CARTESIAN_POINT('Ctrl Pts',(100.94037603585,4.89769140904286,334.532225790158));
#57279=CARTESIAN_POINT('Ctrl Pts',(100.932964231673,4.88356919375284,334.402629006706));
#57280=CARTESIAN_POINT('Ctrl Pts',(100.925552427496,4.86436941453331,334.273988112044));
#57281=CARTESIAN_POINT('Ctrl Pts',(100.917777348718,4.84422859694115,334.139042143935));
#57282=CARTESIAN_POINT('Ctrl Pts',(100.910002269939,4.81843624845891,334.004721681595));
#57283=CARTESIAN_POINT('Ctrl Pts',(100.902227191161,4.78704034637554,333.871537424337));
#57284=CARTESIAN_POINT('Ctrl Pts',(100.894461680112,4.75568307894844,333.738517058785));
#57285=CARTESIAN_POINT('Ctrl Pts',(100.886696169063,4.71873606687302,333.606630493162));
#57286=CARTESIAN_POINT('Ctrl Pts',(100.878930658014,4.6762988789953,333.476381984614));
#57287=CARTESIAN_POINT('Ctrl Pts',(100.871172846491,4.63390376771292,333.346262617842));
#57288=CARTESIAN_POINT('Ctrl Pts',(100.863415034969,4.58602943385974,333.21777844527));
#57289=CARTESIAN_POINT('Ctrl Pts',(100.855657223447,4.53282611651697,333.091421874818));
#57290=CARTESIAN_POINT('Ctrl Pts',(100.847905249924,4.47966283635768,332.965160391693));
#57291=CARTESIAN_POINT('Ctrl Pts',(100.840153276401,4.42117870594579,332.841023682594));
#57292=CARTESIAN_POINT('Ctrl Pts',(100.832401302878,4.35757313772273,332.719487028781));
#57293=CARTESIAN_POINT('Ctrl Pts',(100.82465261232,4.29399450649563,332.598001845814));
#57294=CARTESIAN_POINT('Ctrl Pts',(100.816903921763,4.2252989321751,332.479114873667));
#57295=CARTESIAN_POINT('Ctrl Pts',(100.809155231205,4.15173301446012,332.363279302023));
#57296=CARTESIAN_POINT('Ctrl Pts',(100.801408152827,4.0781824027487,332.247467830937));
#57297=CARTESIAN_POINT('Ctrl Pts',(100.793661074449,3.99976367261914,332.134706827302));
#57298=CARTESIAN_POINT('Ctrl Pts',(100.785913996072,3.91676802897488,332.025422505683));
#57299=CARTESIAN_POINT('Ctrl Pts',(100.778166852766,3.8337716897473,331.916137268156));
#57300=CARTESIAN_POINT('Ctrl Pts',(100.77041970946,3.7461985968976,331.810329082045));
#57301=CARTESIAN_POINT('Ctrl Pts',(100.762672566154,3.65438146276325,331.708392613462));
#57302=CARTESIAN_POINT('Ctrl Pts',(100.754923681126,3.56254368618781,331.606433227397));
#57303=CARTESIAN_POINT('Ctrl Pts',(100.747174796098,3.4664602312216,331.508347581319));
#57304=CARTESIAN_POINT('Ctrl Pts',(100.73942591107,3.36650174076411,331.414494583475));
#57305=CARTESIAN_POINT('Ctrl Pts',(100.731668801295,3.26643715333202,331.320541969088));
#57306=CARTESIAN_POINT('Ctrl Pts',(100.72391169152,3.16248959970536,331.230831245251));
#57307=CARTESIAN_POINT('Ctrl Pts',(100.716154581746,3.05506440278209,331.14568234867));
#57308=CARTESIAN_POINT('Ctrl Pts',(100.70839332682,2.94758180126844,331.060487951242));
#57309=CARTESIAN_POINT('Ctrl Pts',(100.700632071893,2.83661816959872,330.979860468044));
#57310=CARTESIAN_POINT('Ctrl Pts',(100.692870816967,2.72260825524676,330.904076740103));
#57311=CARTESIAN_POINT('Ctrl Pts',(100.685097146563,2.60841596218758,330.828171782896));
#57312=CARTESIAN_POINT('Ctrl Pts',(100.677323476158,2.49116798309834,330.75712626727));
#57313=CARTESIAN_POINT('Ctrl Pts',(100.669549805753,2.37132489850027,330.691171703554));
#57314=CARTESIAN_POINT('Ctrl Pts',(100.662138001576,2.2570605383238,330.628287340647));
#57315=CARTESIAN_POINT('Ctrl Pts',(100.654726197399,2.14043749726805,330.570030756982));
#57316=CARTESIAN_POINT('Ctrl Pts',(100.647314393222,2.02187052229731,330.516561291423));
#57317=CARTESIAN_POINT('Ctrl Pts',(100.639539314444,1.89749222668933,330.46047112808));
#57318=CARTESIAN_POINT('Ctrl Pts',(100.631764235665,1.77058156457802,330.409471954696));
#57319=CARTESIAN_POINT('Ctrl Pts',(100.623989156887,1.64159395717388,330.363799794846));
#57320=CARTESIAN_POINT('Ctrl Pts',(100.616223645838,1.51276507723248,330.318183837497));
#57321=CARTESIAN_POINT('Ctrl Pts',(100.608458134789,1.38186470227037,330.277881979872));
#57322=CARTESIAN_POINT('Ctrl Pts',(100.60069262374,1.24937075529673,330.243083374884));
#57323=CARTESIAN_POINT('Ctrl Pts',(100.592934812218,1.11700817645717,330.208319272813));
#57324=CARTESIAN_POINT('Ctrl Pts',(100.585177000696,0.983055545574793,330.179047663305));
#57325=CARTESIAN_POINT('Ctrl Pts',(100.577419189173,0.848008241963068,330.155408677291));
#57326=CARTESIAN_POINT('Ctrl Pts',(100.56966721565,0.713062565729998,330.131787480365));
#57327=CARTESIAN_POINT('Ctrl Pts',(100.561915242127,0.57702423992336,330.113790537076));
#57328=CARTESIAN_POINT('Ctrl Pts',(100.554163268604,0.440400852209341,330.10150735921));
#57329=CARTESIAN_POINT('Ctrl Pts',(100.546414578047,0.303835324581131,330.089229383277));
#57330=CARTESIAN_POINT('Ctrl Pts',(100.538665887489,0.166685616344576,330.082660394918));
#57331=CARTESIAN_POINT('Ctrl Pts',(100.530917196931,0.0294662736183612,
330.081838270124));
#57332=CARTESIAN_POINT('Ctrl Pts',(100.523170118554,-0.107724519477521,
330.08101631638));
#57333=CARTESIAN_POINT('Ctrl Pts',(100.515423040176,-0.244984527623456,
330.085938850244));
#57334=CARTESIAN_POINT('Ctrl Pts',(100.507675961798,-0.381797750216591,
330.096591640458));
#57335=CARTESIAN_POINT('Ctrl Pts',(100.499928818492,-0.518612119436214,
330.107244519952));
#57336=CARTESIAN_POINT('Ctrl Pts',(100.492181675186,-0.654979305939604,
330.123627721242));
#57337=CARTESIAN_POINT('Ctrl Pts',(100.484434531881,-0.79038737683619,330.145675035905));
#57338=CARTESIAN_POINT('Ctrl Pts',(100.476685646852,-0.925825890341909,
330.167727307272));
#57339=CARTESIAN_POINT('Ctrl Pts',(100.468936761824,-1.0603044734436,330.195446163158));
#57340=CARTESIAN_POINT('Ctrl Pts',(100.461187876796,-1.19332073640064,330.228714147887));
#57341=CARTESIAN_POINT('Ctrl Pts',(100.453430767022,-1.3264781841935,330.262017443598));
#57342=CARTESIAN_POINT('Ctrl Pts',(100.445673657247,-1.45816983153963,330.300881538798));
#57343=CARTESIAN_POINT('Ctrl Pts',(100.437916547472,-1.58790729335798,330.345138724924));
#57344=CARTESIAN_POINT('Ctrl Pts',(100.430155292546,-1.71771408272773,330.389419560676));
#57345=CARTESIAN_POINT('Ctrl Pts',(100.42239403762,-1.8455642416487,330.43909908829));
#57346=CARTESIAN_POINT('Ctrl Pts',(100.414632782694,-1.97098970179248,330.493961533905));
#57347=CARTESIAN_POINT('Ctrl Pts',(100.406859112289,-2.09661580179643,330.548911741553));
#57348=CARTESIAN_POINT('Ctrl Pts',(100.399085441884,-2.21980910074816,330.60906126345));
#57349=CARTESIAN_POINT('Ctrl Pts',(100.39131177148,-2.34012567012689,330.674148071129));
#57350=CARTESIAN_POINT('Ctrl Pts',(100.383899967302,-2.45484147425528,330.736205072253));
#57351=CARTESIAN_POINT('Ctrl Pts',(100.376488163125,-2.56694209765501,330.802749895338));
#57352=CARTESIAN_POINT('Ctrl Pts',(100.369076358948,-2.6760691054939,330.873519998216));
#57353=CARTESIAN_POINT('Ctrl Pts',(100.361306196586,-2.79047236666394,330.947711811251));
#57354=CARTESIAN_POINT('Ctrl Pts',(100.353536034224,-2.90196984830229,331.026782815924));
#57355=CARTESIAN_POINT('Ctrl Pts',(100.345765871861,-3.01011694758207,331.110478303907));
#57356=CARTESIAN_POINT('Ctrl Pts',(100.338005274769,-3.1181309149972,331.194070760588));
#57357=CARTESIAN_POINT('Ctrl Pts',(100.330244677677,-3.2228023996505,331.282276136441));
#57358=CARTESIAN_POINT('Ctrl Pts',(100.322484080585,-3.32371400817106,331.374795418961));
#57359=CARTESIAN_POINT('Ctrl Pts',(100.314731175224,-3.42452560054457,331.467223003189));
#57360=CARTESIAN_POINT('Ctrl Pts',(100.306978269863,-3.52158444591892,331.563955722731));
#57361=CARTESIAN_POINT('Ctrl Pts',(100.299225364503,-3.61450490775293,331.664653341206));
#57362=CARTESIAN_POINT('Ctrl Pts',(100.291478284049,-3.70735555666506,331.765275303632));
#57363=CARTESIAN_POINT('Ctrl Pts',(100.283731203594,-3.79607374631849,331.869855949245));
#57364=CARTESIAN_POINT('Ctrl Pts',(100.27598412314,-3.88030978721557,331.978017369716));
#57365=CARTESIAN_POINT('Ctrl Pts',(100.26824030382,-3.96451036893695,332.086133259618));
#57366=CARTESIAN_POINT('Ctrl Pts',(100.260496484501,-4.04423231438862,332.197826618326));
#57367=CARTESIAN_POINT('Ctrl Pts',(100.252752665181,-4.11916558285399,332.312685734133));
#57368=CARTESIAN_POINT('Ctrl Pts',(100.245010436373,-4.19408346069447,332.427521258903));
#57369=CARTESIAN_POINT('Ctrl Pts',(100.237268207565,-4.26421440410984,332.545520919834));
#57370=CARTESIAN_POINT('Ctrl Pts',(100.229525978757,-4.32929140183202,332.666243581579));
#57371=CARTESIAN_POINT('Ctrl Pts',(100.221783658601,-4.39436916737268,332.786967667684));
#57372=CARTESIAN_POINT('Ctrl Pts',(100.214041338445,-4.45439268265099,332.910414474062));
#57373=CARTESIAN_POINT('Ctrl Pts',(100.20629901829,-4.50914084844599,333.036118162573));
#57374=CARTESIAN_POINT('Ctrl Pts',(100.198554925221,-4.56390155101699,333.161850635956));
#57375=CARTESIAN_POINT('Ctrl Pts',(100.190810832152,-4.61338434413656,333.289840661015));
#57376=CARTESIAN_POINT('Ctrl Pts',(100.183066739084,-4.65741639196718,333.419602703642));
#57377=CARTESIAN_POINT('Ctrl Pts',(100.175314421007,-4.70149520627491,333.54950256665));
#57378=CARTESIAN_POINT('Ctrl Pts',(100.16756210293,-4.740111585229,333.681177835431));
#57379=CARTESIAN_POINT('Ctrl Pts',(100.159809784853,-4.77314253692811,333.814127584996));
#57380=CARTESIAN_POINT('Ctrl Pts',(100.152053284464,-4.80619130855539,333.947149059863));
#57381=CARTESIAN_POINT('Ctrl Pts',(100.144296784075,-4.83364857062412,334.081446002232));
#57382=CARTESIAN_POINT('Ctrl Pts',(100.136540283686,-4.85544274728425,334.216508589489));
#57383=CARTESIAN_POINT('Ctrl Pts',(100.128771457292,-4.87727155749343,334.351785807324));
#57384=CARTESIAN_POINT('Ctrl Pts',(100.121002630897,-4.89341925394935,334.487830712417));
#57385=CARTESIAN_POINT('Ctrl Pts',(100.113233804503,-4.90386622104369,334.624128813812));
#57386=CARTESIAN_POINT('Ctrl Pts',(100.106094995184,-4.91346598582958,334.749373748761));
#57387=CARTESIAN_POINT('Ctrl Pts',(100.098956185865,-4.91825274108658,334.874832226572));
#57388=CARTESIAN_POINT('Ctrl Pts',(100.091817376546,-4.91824999882167,335.00010765993));
#57389=CARTESIAN_POINT('',(98.3418173765424,-4.91824806724263,334.99563977476));
#57390=CARTESIAN_POINT('Ctrl Pts',(100.091817376508,-4.91824999882165,335.000107660602));
#57391=CARTESIAN_POINT('Ctrl Pts',(100.091491025897,-4.91824987345825,335.005834626047));
#57392=CARTESIAN_POINT('Ctrl Pts',(100.091164675285,-4.9182397451109,335.011561578566));
#57393=CARTESIAN_POINT('Ctrl Pts',(100.090838324674,-4.91821961388564,335.017288495902));
#57394=CARTESIAN_POINT('Ctrl Pts',(100.083063245895,-4.91774000129503,335.153728361095));
#57395=CARTESIAN_POINT('Ctrl Pts',(100.075288167117,-4.91157771429302,335.290363854516));
#57396=CARTESIAN_POINT('Ctrl Pts',(100.067513088339,-4.89970661782587,335.426682694439));
#57397=CARTESIAN_POINT('Ctrl Pts',(100.05974757729,-4.88785012949866,335.56283378535));
#57398=CARTESIAN_POINT('Ctrl Pts',(100.051982066241,-4.87029884313455,335.698668612402));
#57399=CARTESIAN_POINT('Ctrl Pts',(100.044216555192,-4.84707860505728,335.83367383244));
#57400=CARTESIAN_POINT('Ctrl Pts',(100.036458743669,-4.82388138991367,335.96854519441));
#57401=CARTESIAN_POINT('Ctrl Pts',(100.028700932147,-4.79502647455996,336.102588203565));
#57402=CARTESIAN_POINT('Ctrl Pts',(100.020943120625,-4.7605915543613,336.235293938722));
#57403=CARTESIAN_POINT('Ctrl Pts',(100.013191147102,-4.72618254753208,336.367899808605));
#57404=CARTESIAN_POINT('Ctrl Pts',(100.005439173579,-4.68620199180087,336.499170030741));
#57405=CARTESIAN_POINT('Ctrl Pts',(99.9976872000558,-4.64077871101077,336.628605543994));
#57406=CARTESIAN_POINT('Ctrl Pts',(99.9899385094982,-4.59537466700711,336.757986241231));
#57407=CARTESIAN_POINT('Ctrl Pts',(99.9821898189406,-4.54453261158466,336.885533406931));
#57408=CARTESIAN_POINT('Ctrl Pts',(99.9744411283829,-4.48843124733662,337.010763039354));
#57409=CARTESIAN_POINT('Ctrl Pts',(99.9666940500051,-4.43234155544598,337.135966616707));
#57410=CARTESIAN_POINT('Ctrl Pts',(99.9589469716273,-4.37099489096032,337.258853263387));
#57411=CARTESIAN_POINT('Ctrl Pts',(99.9511998932494,-4.30461798403781,337.378959241769));
#57412=CARTESIAN_POINT('Ctrl Pts',(99.9434527499436,-4.23824052081289,337.499066226755));
#57413=CARTESIAN_POINT('Ctrl Pts',(99.9357056066378,-4.16683292012931,337.616392154853));
#57414=CARTESIAN_POINT('Ctrl Pts',(99.927958463332,-4.09066753348094,337.730498524633));
#57415=CARTESIAN_POINT('Ctrl Pts',(99.9202095783039,-4.01448502323657,337.844630547949));
#57416=CARTESIAN_POINT('Ctrl Pts',(99.9124606932757,-3.93354281550278,337.955541247576));
#57417=CARTESIAN_POINT('Ctrl Pts',(99.9047118082476,-3.84815595032648,338.062822039307));
#57418=CARTESIAN_POINT('Ctrl Pts',(99.8969546984729,-3.76267845464938,338.170216699979));
#57419=CARTESIAN_POINT('Ctrl Pts',(99.8891975886981,-3.67274712147055,338.273973450068));
#57420=CARTESIAN_POINT('Ctrl Pts',(99.8814404789234,-3.57871692598314,338.373717271228));
#57421=CARTESIAN_POINT('Ctrl Pts',(99.8736792239972,-3.48463648376576,338.473514392296));
#57422=CARTESIAN_POINT('Ctrl Pts',(99.8659179690711,-3.38645309451952,338.569294038758));
#57423=CARTESIAN_POINT('Ctrl Pts',(99.8581567141449,-3.28455706248823,338.660719596713));
#57424=CARTESIAN_POINT('Ctrl Pts',(99.8503830437402,-3.18249803001352,338.752291405766));
#57425=CARTESIAN_POINT('Ctrl Pts',(99.8426093733356,-3.07671478859923,338.839494959173));
#57426=CARTESIAN_POINT('Ctrl Pts',(99.8348357029309,-2.96762973966714,338.92203477684));
#57427=CARTESIAN_POINT('Ctrl Pts',(99.8274238987539,-2.86362262600917,339.000732346135));
#57428=CARTESIAN_POINT('Ctrl Pts',(99.820012094577,-2.75661442154201,339.07519043785));
#57429=CARTESIAN_POINT('Ctrl Pts',(99.8126002904,-2.64699257541845,339.145191596076));
#57430=CARTESIAN_POINT('Ctrl Pts',(99.8048252116216,-2.5319978360677,339.21862371959));
#57431=CARTESIAN_POINT('Ctrl Pts',(99.7970501328432,-2.41376336757124,339.287383026617));
#57432=CARTESIAN_POINT('Ctrl Pts',(99.7892750540647,-2.29270581538381,339.351170314594));
#57433=CARTESIAN_POINT('Ctrl Pts',(99.7815095430157,-2.17179723222117,339.414879108253));
#57434=CARTESIAN_POINT('Ctrl Pts',(99.7737440319667,-2.0480728201003,339.473627876228));
#57435=CARTESIAN_POINT('Ctrl Pts',(99.7659785209177,-1.92197824715985,339.527160553807));
#57436=CARTESIAN_POINT('Ctrl Pts',(99.7582207093955,-1.79600869735567,339.58064015358));
#57437=CARTESIAN_POINT('Ctrl Pts',(99.7504628978733,-1.66767402088233,339.628913803307));
#57438=CARTESIAN_POINT('Ctrl Pts',(99.7427050863511,-1.53744422584185,339.671771432222));
#57439=CARTESIAN_POINT('Ctrl Pts',(99.7349531128281,-1.40731243285197,339.714596809412));
#57440=CARTESIAN_POINT('Ctrl Pts',(99.7272011393051,-1.27528872974119,339.752014156631));
#57441=CARTESIAN_POINT('Ctrl Pts',(99.7194491657821,-1.14186250163802,339.783861733982));
#57442=CARTESIAN_POINT('Ctrl Pts',(99.7117004752245,-1.00849277962175,339.815695823864));
#57443=CARTESIAN_POINT('Ctrl Pts',(99.7039517846669,-0.873722093380531,
339.841964744806));
#57444=CARTESIAN_POINT('Ctrl Pts',(99.6962030941093,-0.73805415652861,339.862556850519));
#57445=CARTESIAN_POINT('Ctrl Pts',(99.6884560157314,-0.60241444652398,339.883144671873));
#57446=CARTESIAN_POINT('Ctrl Pts',(99.6807089373536,-0.465878243434824,
339.898057968686));
#57447=CARTESIAN_POINT('Ctrl Pts',(99.6729618589758,-0.328958210823053,
339.907236448148));
#57448=CARTESIAN_POINT('Ctrl Pts',(99.6652147156699,-0.192037030689624,
339.916415004534));
#57449=CARTESIAN_POINT('Ctrl Pts',(99.6574675723642,-0.0547324046163078,
339.919858621559));
#57450=CARTESIAN_POINT('Ctrl Pts',(99.6497204290583,0.0824395371690725,
339.91755902712));
#57451=CARTESIAN_POINT('Ctrl Pts',(99.6419715440303,0.219642318119116,339.915258915683));
#57452=CARTESIAN_POINT('Ctrl Pts',(99.6342226590022,0.356711964679367,339.907213029997));
#57453=CARTESIAN_POINT('Ctrl Pts',(99.6264737739741,0.49313440342502,339.893465185598));
#57454=CARTESIAN_POINT('Ctrl Pts',(99.6187166641994,0.629701642356758,339.879702749095));
#57455=CARTESIAN_POINT('Ctrl Pts',(99.6109595544246,0.765619911701912,339.860226303458));
#57456=CARTESIAN_POINT('Ctrl Pts',(99.6032024446499,0.900381753085704,339.835131410956));
#57457=CARTESIAN_POINT('Ctrl Pts',(99.5954411897237,1.03521560688868,339.810023108545));
#57458=CARTESIAN_POINT('Ctrl Pts',(99.5876799347976,1.16889142064978,339.779290464412));
#57459=CARTESIAN_POINT('Ctrl Pts',(99.5799186798714,1.30091491253837,339.743079532628));
#57460=CARTESIAN_POINT('Ctrl Pts',(99.5721450094668,1.43314959898763,339.706810675154));
#57461=CARTESIAN_POINT('Ctrl Pts',(99.5643713390621,1.56372630922448,339.66504613715));
#57462=CARTESIAN_POINT('Ctrl Pts',(99.5565976686574,1.6921679820863,339.617981223749));
#57463=CARTESIAN_POINT('Ctrl Pts',(99.5491858644803,1.81463066417573,339.57310719339));
#57464=CARTESIAN_POINT('Ctrl Pts',(99.5417740603032,1.93515234156217,339.523415257164));
#57465=CARTESIAN_POINT('Ctrl Pts',(99.5343622561261,2.05334047996373,339.46911355146));
#57466=CARTESIAN_POINT('Ctrl Pts',(99.5265871773476,2.17732137109212,339.412150357403));
#57467=CARTESIAN_POINT('Ctrl Pts',(99.5188120985692,2.29912599448184,339.349934076862));
#57468=CARTESIAN_POINT('Ctrl Pts',(99.5110370197908,2.41827727355382,339.282653160217));
#57469=CARTESIAN_POINT('Ctrl Pts',(99.5032715087417,2.53728192939135,339.215455037022));
#57470=CARTESIAN_POINT('Ctrl Pts',(99.4955059976928,2.65363940043506,339.14320486868));
#57471=CARTESIAN_POINT('Ctrl Pts',(99.4877404866437,2.76689317980419,339.066138855727));
#57472=CARTESIAN_POINT('Ctrl Pts',(99.4799826751215,2.88003466772134,338.98914925395));
#57473=CARTESIAN_POINT('Ctrl Pts',(99.4722248635993,2.99007826693166,338.907353528412));
#57474=CARTESIAN_POINT('Ctrl Pts',(99.4644670520771,3.09659297609416,338.821033237608));
#57475=CARTESIAN_POINT('Ctrl Pts',(99.4567150785541,3.20302752956024,338.73477790556));
#57476=CARTESIAN_POINT('Ctrl Pts',(99.4489631050311,3.30593817637274,338.644005030599));
#57477=CARTESIAN_POINT('Ctrl Pts',(99.4412111315081,3.40492407162688,338.549038620381));
#57478=CARTESIAN_POINT('Ctrl Pts',(99.4334624409505,3.50386804629555,338.454112428494));
#57479=CARTESIAN_POINT('Ctrl Pts',(99.4257137503929,3.59889029380429,338.35499650366));
#57480=CARTESIAN_POINT('Ctrl Pts',(99.4179650598353,3.68962434006682,338.252054011188));
#57481=CARTESIAN_POINT('Ctrl Pts',(99.4102179814574,3.78033950835326,338.149132936762));
#57482=CARTESIAN_POINT('Ctrl Pts',(99.4024709030796,3.86676799174228,338.042387171343));
#57483=CARTESIAN_POINT('Ctrl Pts',(99.3947238247018,3.94858165705209,337.932215196757));
#57484=CARTESIAN_POINT('Ctrl Pts',(99.386976681396,4.03039600803916,337.822042298823));
#57485=CARTESIAN_POINT('Ctrl Pts',(99.3792295380902,4.10759523076798,337.70844344826));
#57486=CARTESIAN_POINT('Ctrl Pts',(99.3714823947844,4.17989306136877,337.591848193475));
#57487=CARTESIAN_POINT('Ctrl Pts',(99.3637335097563,4.25220714605676,337.475226725603));
#57488=CARTESIAN_POINT('Ctrl Pts',(99.3559846247281,4.31961743994021,337.35560784514));
#57489=CARTESIAN_POINT('Ctrl Pts',(99.3482357397,4.38188259381066,337.233447558498));
#57490=CARTESIAN_POINT('Ctrl Pts',(99.3404786299253,4.44421383655879,337.111157609665));
#57491=CARTESIAN_POINT('Ctrl Pts',(99.3327215201506,4.50138885244284,336.986321214992));
#57492=CARTESIAN_POINT('Ctrl Pts',(99.3249644103759,4.55321338696688,336.859416821276));
#57493=CARTESIAN_POINT('Ctrl Pts',(99.3172031554497,4.60506561486511,336.732444613911));
#57494=CARTESIAN_POINT('Ctrl Pts',(99.3094419005235,4.65156153190451,336.603402573092));
#57495=CARTESIAN_POINT('Ctrl Pts',(99.3016806455974,4.69255647380802,336.472785389194));
#57496=CARTESIAN_POINT('Ctrl Pts',(99.2939069751927,4.73361699425838,336.341959260369));
#57497=CARTESIAN_POINT('Ctrl Pts',(99.2861333047881,4.76915885364278,336.209553331037));
#57498=CARTESIAN_POINT('Ctrl Pts',(99.2783596343834,4.79908812304527,336.076074462919));
#57499=CARTESIAN_POINT('Ctrl Pts',(99.2709478302064,4.82762417775645,335.948809068225));
#57500=CARTESIAN_POINT('Ctrl Pts',(99.2635360260293,4.85105836361912,335.82056866048));
#57501=CARTESIAN_POINT('Ctrl Pts',(99.2561242218522,4.86935328413904,335.691795964678));
#57502=CARTESIAN_POINT('Ctrl Pts',(99.2483491430738,4.88854489321143,335.55671173546));
#57503=CARTESIAN_POINT('Ctrl Pts',(99.2405740642953,4.90214136644291,335.420614829694));
#57504=CARTESIAN_POINT('Ctrl Pts',(99.2327989855169,4.91004300226502,335.284008412566));
#57505=CARTESIAN_POINT('Ctrl Pts',(99.2250334744679,4.91793491462121,335.147570098331));
#57506=CARTESIAN_POINT('Ctrl Pts',(99.2172679634189,4.92014591084444,335.010623906749));
#57507=CARTESIAN_POINT('Ctrl Pts',(99.2095024523699,4.91662757493826,334.873681545859));
#57508=CARTESIAN_POINT('Ctrl Pts',(99.2017446408477,4.91311272747239,334.736874963717));
#57509=CARTESIAN_POINT('Ctrl Pts',(99.1939868293255,4.90387986266518,334.600072592938));
#57510=CARTESIAN_POINT('Ctrl Pts',(99.1862290178033,4.88893250950576,334.4637892392));
#57511=CARTESIAN_POINT('Ctrl Pts',(99.1784770442803,4.87399640470359,334.327608443008));
#57512=CARTESIAN_POINT('Ctrl Pts',(99.1707250707573,4.85335441359659,334.191946273413));
#57513=CARTESIAN_POINT('Ctrl Pts',(99.1629730972343,4.82706208095634,334.057315148582));
#57514=CARTESIAN_POINT('Ctrl Pts',(99.1552244066766,4.80078088313457,333.922741040112));
#57515=CARTESIAN_POINT('Ctrl Pts',(99.147475716119,4.76885417789806,333.789197490772));
#57516=CARTESIAN_POINT('Ctrl Pts',(99.1397270255614,4.73138903854832,333.657189206029));
#57517=CARTESIAN_POINT('Ctrl Pts',(99.1319799471835,4.69393169413374,333.525208386712));
#57518=CARTESIAN_POINT('Ctrl Pts',(99.1242328688057,4.65093831429878,333.39476257242));
#57519=CARTESIAN_POINT('Ctrl Pts',(99.1164857904279,4.60256641921949,333.266343338728));
#57520=CARTESIAN_POINT('Ctrl Pts',(99.1087386471221,4.55419411873716,333.137923028759));
#57521=CARTESIAN_POINT('Ctrl Pts',(99.1009915038163,4.50044335088185,333.011529699052));
#57522=CARTESIAN_POINT('Ctrl Pts',(99.0932443605105,4.44152041826989,332.887636528295));
#57523=CARTESIAN_POINT('Ctrl Pts',(99.0854954754823,4.3825842385317,332.763715503724));
#57524=CARTESIAN_POINT('Ctrl Pts',(99.0777465904543,4.31847374801572,332.642296109513));
#57525=CARTESIAN_POINT('Ctrl Pts',(99.0699977054262,4.24944180433612,332.523828072597));
#57526=CARTESIAN_POINT('Ctrl Pts',(99.0622405956514,4.18033658943827,332.405234292482));
#57527=CARTESIAN_POINT('Ctrl Pts',(99.0544834858767,4.10629968368623,332.289598465581));
#57528=CARTESIAN_POINT('Ctrl Pts',(99.046726376102,4.02762830094663,332.17734285966));
#57529=CARTESIAN_POINT('Ctrl Pts',(99.0389651211758,3.94891487873553,332.065027267932));
#57530=CARTESIAN_POINT('Ctrl Pts',(99.0312038662496,3.86556228226477,331.956095806629));
#57531=CARTESIAN_POINT('Ctrl Pts',(99.0234426113235,3.77790822108268,331.850937832374));
#57532=CARTESIAN_POINT('Ctrl Pts',(99.0156689409188,3.69011394196909,331.745611639631));
#57533=CARTESIAN_POINT('Ctrl Pts',(99.0078952705141,3.59800471074091,331.644071286009));
#57534=CARTESIAN_POINT('Ctrl Pts',(99.0001216001095,3.50195592790865,331.546670050301));
#57535=CARTESIAN_POINT('Ctrl Pts',(98.9927097959324,3.41037823902563,331.453802865549));
#57536=CARTESIAN_POINT('Ctrl Pts',(98.9852979917553,3.3152197268874,331.364698315647));
#57537=CARTESIAN_POINT('Ctrl Pts',(98.9778861875783,3.21683245099812,331.279627432003));
#57538=CARTESIAN_POINT('Ctrl Pts',(98.9701111087999,3.11362292163643,331.190386970938));
#57539=CARTESIAN_POINT('Ctrl Pts',(98.9623360300214,3.0065339619087,331.10530356158));
#57540=CARTESIAN_POINT('Ctrl Pts',(98.954560951243,2.89593473991489,331.024733336661));
#57541=CARTESIAN_POINT('Ctrl Pts',(98.946795440194,2.78547161730484,330.944262258533));
#57542=CARTESIAN_POINT('Ctrl Pts',(98.939029929145,2.67150714010772,330.868293542403));
#57543=CARTESIAN_POINT('Ctrl Pts',(98.9312644180959,2.55444541385672,330.797144816898));
#57544=CARTESIAN_POINT('Ctrl Pts',(98.9235066065738,2.43749975464812,330.726066635562));
#57545=CARTESIAN_POINT('Ctrl Pts',(98.9157487950515,2.31746328958002,330.659799136005));
#57546=CARTESIAN_POINT('Ctrl Pts',(98.9079909835293,2.19477083947044,330.59861794152));
#57547=CARTESIAN_POINT('Ctrl Pts',(98.9002390100063,2.07217071932036,330.537482787824));
#57548=CARTESIAN_POINT('Ctrl Pts',(98.8924870364833,1.94691894085738,330.481426494262));
#57549=CARTESIAN_POINT('Ctrl Pts',(98.8847350629603,1.81947646591242,330.430679650923));
#57550=CARTESIAN_POINT('Ctrl Pts',(98.8769863724027,1.69208796293135,330.379954298902));
#57551=CARTESIAN_POINT('Ctrl Pts',(98.869237681845,1.56251097110767,330.334534069187));
#57552=CARTESIAN_POINT('Ctrl Pts',(98.8614889912874,1.43122785154232,330.294602046642));
#57553=CARTESIAN_POINT('Ctrl Pts',(98.8537419129096,1.29997204652649,330.254678332287));
#57554=CARTESIAN_POINT('Ctrl Pts',(98.8459948345317,1.16701119356086,330.220240667521));
#57555=CARTESIAN_POINT('Ctrl Pts',(98.8382477561539,1.03284391223874,330.191422610017));
#57556=CARTESIAN_POINT('Ctrl Pts',(98.8305006128481,0.898675506465665,330.162604310991));
#57557=CARTESIAN_POINT('Ctrl Pts',(98.8227534695423,0.763301034327023,330.139405795251));
#57558=CARTESIAN_POINT('Ctrl Pts',(98.8150063262365,0.627230044059254,330.121909642664));
#57559=CARTESIAN_POINT('Ctrl Pts',(98.8072574412084,0.491128462143912,330.104409556572));
#57560=CARTESIAN_POINT('Ctrl Pts',(98.7995085561803,0.354330438105604,330.092614434533));
#57561=CARTESIAN_POINT('Ctrl Pts',(98.7917596711522,0.217350992680787,330.086555016235));
#57562=CARTESIAN_POINT('Ctrl Pts',(98.7840025613775,0.0802261558574262,
330.080489166408));
#57563=CARTESIAN_POINT('Ctrl Pts',(98.7762454516027,-0.0570800959049829,
330.080171198845));
#57564=CARTESIAN_POINT('Ctrl Pts',(98.768488341828,-0.194051829155775,330.085579693382));
#57565=CARTESIAN_POINT('Ctrl Pts',(98.7607270869018,-0.33109675572131,330.090991078045));
#57566=CARTESIAN_POINT('Ctrl Pts',(98.7529658319757,-0.467806418203325,
330.10213499047));
#57567=CARTESIAN_POINT('Ctrl Pts',(98.7452045770495,-0.603670644296039,
330.118938146703));
#57568=CARTESIAN_POINT('Ctrl Pts',(98.7374309066448,-0.739752208872452,
330.135768182509));
#57569=CARTESIAN_POINT('Ctrl Pts',(98.7296572362401,-0.874985248745111,
330.158275488384));
#57570=CARTESIAN_POINT('Ctrl Pts',(98.7218835658355,-1.00886953348464,330.186335561456));
#57571=CARTESIAN_POINT('Ctrl Pts',(98.7144717616583,-1.1365214725594,330.213089431375));
#57572=CARTESIAN_POINT('Ctrl Pts',(98.7070599574813,-1.26294712064762,330.24489066958));
#57573=CARTESIAN_POINT('Ctrl Pts',(98.6996481533041,-1.38772804205732,330.28158989237));
#57574=CARTESIAN_POINT('Ctrl Pts',(98.6918730745257,-1.5186248481281,330.32008785339));
#57575=CARTESIAN_POINT('Ctrl Pts',(98.6840979957473,-1.64812528310341,330.36409772938));
#57576=CARTESIAN_POINT('Ctrl Pts',(98.6763229169688,-1.77573008933132,330.413501802863));
#57577=CARTESIAN_POINT('Ctrl Pts',(98.6685574059198,-1.90317786972135,330.462845081488));
#57578=CARTESIAN_POINT('Ctrl Pts',(98.6607918948708,-2.0287343017279,330.517569210307));
#57579=CARTESIAN_POINT('Ctrl Pts',(98.6530263838218,-2.15191359997138,330.57750625543));
#57580=CARTESIAN_POINT('Ctrl Pts',(98.6452685722996,-2.27497076558185,330.637383872799));
#57581=CARTESIAN_POINT('Ctrl Pts',(98.6375107607774,-2.39565513865294,330.702463950702));
#57582=CARTESIAN_POINT('Ctrl Pts',(98.6297529492552,-2.5134996351845,330.772529994615));
#57583=CARTESIAN_POINT('Ctrl Pts',(98.6220009757322,-2.63125544999552,330.842543311609));
#57584=CARTESIAN_POINT('Ctrl Pts',(98.6142490022092,-2.74617530743215,330.917534927292));
#57585=CARTESIAN_POINT('Ctrl Pts',(98.6064970286862,-2.85781584647261,330.997241994556));
#57586=CARTESIAN_POINT('Ctrl Pts',(98.5987483381286,-2.9694091056785,331.076915305828));
#57587=CARTESIAN_POINT('Ctrl Pts',(98.5909996475709,-3.07772549124603,331.161299870146));
#57588=CARTESIAN_POINT('Ctrl Pts',(98.5832509570133,-3.18235000993756,331.250089137493));
#57589=CARTESIAN_POINT('Ctrl Pts',(98.5755038786355,-3.28695276062421,331.338859931491));
#57590=CARTESIAN_POINT('Ctrl Pts',(98.5677568002576,-3.387864874453,331.432033352908));
#57591=CARTESIAN_POINT('Ctrl Pts',(98.5600097218798,-3.48470420825454,331.52926237761));
#57592=CARTESIAN_POINT('Ctrl Pts',(98.5522625785739,-3.5815443536629,331.626492217185));
#57593=CARTESIAN_POINT('Ctrl Pts',(98.5445154352681,-3.67431137512724,331.727777450897));
#57594=CARTESIAN_POINT('Ctrl Pts',(98.5367682919623,-3.76266008368666,331.832734277467));
#57595=CARTESIAN_POINT('Ctrl Pts',(98.5290194069342,-3.85102865491146,331.93771470056));
#57596=CARTESIAN_POINT('Ctrl Pts',(98.5212705219061,-3.93497668494761,332.046368060093));
#57597=CARTESIAN_POINT('Ctrl Pts',(98.513521636878,-4.01419961686452,332.158277899149));
#57598=CARTESIAN_POINT('Ctrl Pts',(98.5057645271033,-4.09350663681984,332.270306520464));
#57599=CARTESIAN_POINT('Ctrl Pts',(98.4980074173285,-4.16807831398719,332.385598206378));
#57600=CARTESIAN_POINT('Ctrl Pts',(98.4902503075538,-4.23765345984436,332.503707505766));
#57601=CARTESIAN_POINT('Ctrl Pts',(98.4824890526276,-4.3072657844349,332.621879918987));
#57602=CARTESIAN_POINT('Ctrl Pts',(98.4747277977014,-4.37187607349971,332.742872601191));
#57603=CARTESIAN_POINT('Ctrl Pts',(98.4669665427753,-4.43126986957041,332.866216879452));
#57604=CARTESIAN_POINT('Ctrl Pts',(98.4591928723706,-4.49075867635843,332.989758468359));
#57605=CARTESIAN_POINT('Ctrl Pts',(98.451419201966,-4.54501416022077,333.115658811337));
#57606=CARTESIAN_POINT('Ctrl Pts',(98.4436455315613,-4.59387031489085,333.243429878296));
#57607=CARTESIAN_POINT('Ctrl Pts',(98.4362337273843,-4.6404522038063,333.365253171346));
#57608=CARTESIAN_POINT('Ctrl Pts',(98.4288219232073,-4.68212603663192,333.488776670742));
#57609=CARTESIAN_POINT('Ctrl Pts',(98.4214101190303,-4.71879099374629,333.61356766489));
#57610=CARTESIAN_POINT('Ctrl Pts',(98.4117633154176,-4.76651211971021,333.775988876302));
#57611=CARTESIAN_POINT('Ctrl Pts',(98.4021165118049,-4.80587145811916,333.940970878287));
#57612=CARTESIAN_POINT('Ctrl Pts',(98.3924697081922,-4.83663764127717,334.107744773352));
#57613=CARTESIAN_POINT('Ctrl Pts',(98.3829601260023,-4.86696618938061,334.272146385112));
#57614=CARTESIAN_POINT('Ctrl Pts',(98.3734505438124,-4.88894431319201,334.438289332985));
#57615=CARTESIAN_POINT('Ctrl Pts',(98.3639409616224,-4.90239600787342,334.605416112231));
#57616=CARTESIAN_POINT('Ctrl Pts',(98.3565664332624,-4.9128275811999,334.735020247161));
#57617=CARTESIAN_POINT('Ctrl Pts',(98.3491919049024,-4.91813244098066,334.865215631944));
#57618=CARTESIAN_POINT('Ctrl Pts',(98.3418173765424,-4.91824806724263,334.99563977476));
#57619=CARTESIAN_POINT('',(96.5918173764665,-4.91824959781138,335.001989001811));
#57620=CARTESIAN_POINT('Ctrl Pts',(98.3418173765085,-4.91824806724316,334.995639775358));
#57621=CARTESIAN_POINT('Ctrl Pts',(98.3341262128526,-4.91836865805767,335.131663854203));
#57622=CARTESIAN_POINT('Ctrl Pts',(98.3264350491966,-4.91284197471611,335.267801370545));
#57623=CARTESIAN_POINT('Ctrl Pts',(98.3187438855406,-4.9016666356082,335.403543375445));
#57624=CARTESIAN_POINT('Ctrl Pts',(98.3110556037903,-4.89049548393849,335.539234517346));
#57625=CARTESIAN_POINT('Ctrl Pts',(98.3033673220399,-4.87367991624643,335.674530046989));
#57626=CARTESIAN_POINT('Ctrl Pts',(98.2956790402896,-4.85127061813189,335.808923019916));
#57627=CARTESIAN_POINT('Ctrl Pts',(98.287992039792,-4.82886505452859,335.943293596244));
#57628=CARTESIAN_POINT('Ctrl Pts',(98.2803050392944,-4.80086767947502,336.076761523036));
#57629=CARTESIAN_POINT('Ctrl Pts',(98.2726180387968,-4.7673807476608,336.208827477076));
#57630=CARTESIAN_POINT('Ctrl Pts',(98.2649305918404,-4.73389187093554,336.340901101467));
#57631=CARTESIAN_POINT('Ctrl Pts',(98.2572431448842,-4.69491290094729,336.471572205827));
#57632=CARTESIAN_POINT('Ctrl Pts',(98.2495556979278,-4.65059654726642,336.600354591037));
#57633=CARTESIAN_POINT('Ctrl Pts',(98.2418660767841,-4.60626765989809,336.729173398878));
#57634=CARTESIAN_POINT('Ctrl Pts',(98.2341764556405,-4.55659851553014,336.856102049364));
#57635=CARTESIAN_POINT('Ctrl Pts',(98.2264868344968,-4.50179056263719,336.980672813125));
#57636=CARTESIAN_POINT('Ctrl Pts',(98.2187888072795,-4.44692269525984,337.105379754076));
#57637=CARTESIAN_POINT('Ctrl Pts',(98.2110907800621,-4.38690496302017,337.227723297566));
#57638=CARTESIAN_POINT('Ctrl Pts',(98.2033927528448,-4.32198570563955,337.347258533427));
#57639=CARTESIAN_POINT('Ctrl Pts',(98.1956901004697,-4.25702744322512,337.466865588901));
#57640=CARTESIAN_POINT('Ctrl Pts',(98.1879874480945,-4.18716199483521,337.583660636348));
#57641=CARTESIAN_POINT('Ctrl Pts',(98.1802847957194,-4.11268127752368,337.697227423115));
#57642=CARTESIAN_POINT('Ctrl Pts',(98.172570452277,-4.03808751355848,337.810966581279));
#57643=CARTESIAN_POINT('Ctrl Pts',(98.1648561088346,-3.95886472363139,337.921467372271));
#57644=CARTESIAN_POINT('Ctrl Pts',(98.1571417653922,-3.87534569531122,338.028345885848));
#57645=CARTESIAN_POINT('Ctrl Pts',(98.1524852051803,-3.82493163387864,338.092860285233));
#57646=CARTESIAN_POINT('Ctrl Pts',(98.1478286449683,-3.77295293558199,338.156055549211));
#57647=CARTESIAN_POINT('Ctrl Pts',(98.1431720847564,-3.71948909971673,338.217853927634));
#57648=CARTESIAN_POINT('Ctrl Pts',(98.1353970059779,-3.63022030113384,338.321038948067));
#57649=CARTESIAN_POINT('Ctrl Pts',(98.1276219271995,-3.53651339248321,338.420669501185));
#57650=CARTESIAN_POINT('Ctrl Pts',(98.119846848421,-3.43868235447085,338.516339961885));
#57651=CARTESIAN_POINT('Ctrl Pts',(98.112081337372,-3.34097170377907,338.611892693993));
#57652=CARTESIAN_POINT('Ctrl Pts',(98.104315826323,-3.23914729831483,338.703494759172));
#57653=CARTESIAN_POINT('Ctrl Pts',(98.096550315274,-3.13356324130191,338.790773598523));
#57654=CARTESIAN_POINT('Ctrl Pts',(98.0887925037518,-3.02808387118892,338.877965900651));
#57655=CARTESIAN_POINT('Ctrl Pts',(98.0810346922296,-2.9188525672001,338.960843259878));
#57656=CARTESIAN_POINT('Ctrl Pts',(98.0732768807074,-2.80625988167974,339.039070256752));
#57657=CARTESIAN_POINT('Ctrl Pts',(98.0655249071844,-2.69375192572582,339.117238385329));
#57658=CARTESIAN_POINT('Ctrl Pts',(98.0577729336614,-2.57788794288802,339.190762895099));
#57659=CARTESIAN_POINT('Ctrl Pts',(98.0500209601384,-2.45909084455753,339.259349161634));
#57660=CARTESIAN_POINT('Ctrl Pts',(98.0422722695808,-2.34034405686871,339.327906381844));
#57661=CARTESIAN_POINT('Ctrl Pts',(98.0345235790232,-2.21866696209217,339.391529323337));
#57662=CARTESIAN_POINT('Ctrl Pts',(98.0267748884656,-2.09451049475174,339.449967286383));
#57663=CARTESIAN_POINT('Ctrl Pts',(98.0190278100877,-1.97037985920131,339.508393090922));
#57664=CARTESIAN_POINT('Ctrl Pts',(98.0112807317099,-1.84377123059323,339.561635896425));
#57665=CARTESIAN_POINT('Ctrl Pts',(98.0035336533321,-1.71515877093141,339.609491669696));
#57666=CARTESIAN_POINT('Ctrl Pts',(97.9957865100263,-1.5865452333732,339.657347844045));
#57667=CARTESIAN_POINT('Ctrl Pts',(97.9880393667205,-1.45592819760025,339.699816759798));
#57668=CARTESIAN_POINT('Ctrl Pts',(97.9802922234147,-1.32379998799317,339.736743253997));
#57669=CARTESIAN_POINT('Ctrl Pts',(97.9725433383866,-1.19164207315978,339.773678050056));
#57670=CARTESIAN_POINT('Ctrl Pts',(97.9647944533585,-1.05797268481536,339.805067839865));
#57671=CARTESIAN_POINT('Ctrl Pts',(97.9570455683304,-0.923297034851003,
339.830807970509));
#57672=CARTESIAN_POINT('Ctrl Pts',(97.9492884585557,-0.788478438760129,
339.856575421994));
#57673=CARTESIAN_POINT('Ctrl Pts',(97.9415313487809,-0.652651832037589,
339.876681162036));
#57674=CARTESIAN_POINT('Ctrl Pts',(97.9337742390062,-0.516330847990964,
339.891072021338));
#57675=CARTESIAN_POINT('Ctrl Pts',(97.92601298408,-0.379937018369072,339.905470570654));
#57676=CARTESIAN_POINT('Ctrl Pts',(97.9182517291539,-0.243048674915173,
339.914148129444));
#57677=CARTESIAN_POINT('Ctrl Pts',(97.9104904742277,-0.106181225512197,
339.917103681015));
#57678=CARTESIAN_POINT('Ctrl Pts',(97.902716803823,0.03090516720492,339.920063960505));
#57679=CARTESIAN_POINT('Ctrl Pts',(97.8949431334184,0.16797020808126,339.917283949611));
#57680=CARTESIAN_POINT('Ctrl Pts',(97.8871694630137,0.304500944683629,339.908814748713));
#57681=CARTESIAN_POINT('Ctrl Pts',(97.8797576588366,0.434676142649488,339.900739791156));
#57682=CARTESIAN_POINT('Ctrl Pts',(97.8723458546596,0.564365374310985,339.887493416679));
#57683=CARTESIAN_POINT('Ctrl Pts',(97.8649340504825,0.693133041553943,339.869163136434));
#57684=CARTESIAN_POINT('Ctrl Pts',(97.857158971704,0.828211995747758,339.849934434551));
#57685=CARTESIAN_POINT('Ctrl Pts',(97.8493838929256,0.96270363856121,339.825050105009));
#57686=CARTESIAN_POINT('Ctrl Pts',(97.8416088141472,1.09609695821608,339.794554673866));
#57687=CARTESIAN_POINT('Ctrl Pts',(97.8338433030982,1.22932612889878,339.764096769292));
#57688=CARTESIAN_POINT('Ctrl Pts',(97.8260777920492,1.36145928823187,339.728041588002));
#57689=CARTESIAN_POINT('Ctrl Pts',(97.8183122810002,1.49199151791639,339.686485289955));
#57690=CARTESIAN_POINT('Ctrl Pts',(97.810554469478,1.62239432451515,339.644970195098));
#57691=CARTESIAN_POINT('Ctrl Pts',(97.8027966579558,1.75119899027894,339.597964955806));
#57692=CARTESIAN_POINT('Ctrl Pts',(97.7950388464336,1.8779121035515,339.545616481165));
#57693=CARTESIAN_POINT('Ctrl Pts',(97.7872868729105,2.00452986118854,339.49330740041));
#57694=CARTESIAN_POINT('Ctrl Pts',(97.7795348993875,2.12905883941901,339.435663236464));
#57695=CARTESIAN_POINT('Ctrl Pts',(97.7717829258645,2.25102242065511,339.372880186354));
#57696=CARTESIAN_POINT('Ctrl Pts',(97.7640342353068,2.37293435024156,339.310123724903));
#57697=CARTESIAN_POINT('Ctrl Pts',(97.7562855447492,2.49228269689234,339.242232884364));
#57698=CARTESIAN_POINT('Ctrl Pts',(97.7485368541916,2.60861261531108,339.169451197189));
#57699=CARTESIAN_POINT('Ctrl Pts',(97.7407897758138,2.72491833031869,339.096684652852));
#57700=CARTESIAN_POINT('Ctrl Pts',(97.733042697436,2.83820653509296,339.019029493108));
#57701=CARTESIAN_POINT('Ctrl Pts',(97.7252956190581,2.9480490574991,338.936774036833));
#57702=CARTESIAN_POINT('Ctrl Pts',(97.7175484757523,3.05789250049152,338.854517891177));
#57703=CARTESIAN_POINT('Ctrl Pts',(97.7098013324465,3.16428989064397,338.767661606384));
#57704=CARTESIAN_POINT('Ctrl Pts',(97.7020541891407,3.26684432314165,338.676535220946));
#57705=CARTESIAN_POINT('Ctrl Pts',(97.6943053041126,3.36942181205292,338.585388348363));
#57706=CARTESIAN_POINT('Ctrl Pts',(97.6865564190845,3.46815433195597,338.489969724404));
#57707=CARTESIAN_POINT('Ctrl Pts',(97.6788075340564,3.56268047883941,338.39064755883));
#57708=CARTESIAN_POINT('Ctrl Pts',(97.6710504242817,3.65730695675178,338.291219971683));
#57709=CARTESIAN_POINT('Ctrl Pts',(97.663293314507,3.74771787311701,338.18788084996));
#57710=CARTESIAN_POINT('Ctrl Pts',(97.6555362047322,3.83359056028304,338.08103334591));
#57711=CARTESIAN_POINT('Ctrl Pts',(97.647774949806,3.91950913506754,337.97412874597));
#57712=CARTESIAN_POINT('Ctrl Pts',(97.6400136948799,4.00088441667551,337.863712342554));
#57713=CARTESIAN_POINT('Ctrl Pts',(97.6322524399537,4.07743663337025,337.750217002956));
#57714=CARTESIAN_POINT('Ctrl Pts',(97.624478769549,4.15411130866329,337.636540107804));
#57715=CARTESIAN_POINT('Ctrl Pts',(97.6167050991444,4.22594729660149,337.519774767365));
#57716=CARTESIAN_POINT('Ctrl Pts',(97.6089314287397,4.29270998059204,337.400379987632));
#57717=CARTESIAN_POINT('Ctrl Pts',(97.6015196245627,4.35636484558052,337.286543063621));
#57718=CARTESIAN_POINT('Ctrl Pts',(97.5941078203856,4.41540797150253,337.170316248613));
#57719=CARTESIAN_POINT('Ctrl Pts',(97.5866960162085,4.46967722121733,337.052113203659));
#57720=CARTESIAN_POINT('Ctrl Pts',(97.5789209374301,4.5266063685206,336.928116675363));
#57721=CARTESIAN_POINT('Ctrl Pts',(97.5711458586516,4.57846174998048,336.80155344509));
#57722=CARTESIAN_POINT('Ctrl Pts',(97.5633707798732,4.62500427071286,336.672877329151));
#57723=CARTESIAN_POINT('Ctrl Pts',(97.5556052688242,4.67148951791053,336.544359557365));
#57724=CARTESIAN_POINT('Ctrl Pts',(97.5478397577751,4.71267478107494,336.413734437302));
#57725=CARTESIAN_POINT('Ctrl Pts',(97.5400742467261,4.7483676829023,336.281478603204));
#57726=CARTESIAN_POINT('Ctrl Pts',(97.5323164352039,4.7840251951135,336.14935390115));
#57727=CARTESIAN_POINT('Ctrl Pts',(97.5245586236817,4.81420108203467,336.015602077641));
#57728=CARTESIAN_POINT('Ctrl Pts',(97.5168008121595,4.83875186929176,335.880717554001));
#57729=CARTESIAN_POINT('Ctrl Pts',(97.5090488386364,4.86328418130292,335.745934535242));
#57730=CARTESIAN_POINT('Ctrl Pts',(97.5012968651134,4.88219974964813,335.610020896007));
#57731=CARTESIAN_POINT('Ctrl Pts',(97.4935448915904,4.89540563546843,335.473483607661));
#57732=CARTESIAN_POINT('Ctrl Pts',(97.4857962010328,4.90860592858823,335.337004142939));
#57733=CARTESIAN_POINT('Ctrl Pts',(97.4780475104752,4.91610131097061,335.199901942663));
#57734=CARTESIAN_POINT('Ctrl Pts',(97.4702988199175,4.9178504313616,335.062691285332));
#57735=CARTESIAN_POINT('Ctrl Pts',(97.4625517415397,4.91959918783348,334.925509175824));
#57736=CARTESIAN_POINT('Ctrl Pts',(97.4548046631618,4.91560405538378,334.788219044742));
#57737=CARTESIAN_POINT('Ctrl Pts',(97.447057584784,4.90587577899509,334.651336977055));
#57738=CARTESIAN_POINT('Ctrl Pts',(97.4393104414782,4.89614742107409,334.514453762165));
#57739=CARTESIAN_POINT('Ctrl Pts',(97.4315632981724,4.88068585108596,334.377979007382));
#57740=CARTESIAN_POINT('Ctrl Pts',(97.4238161548666,4.85955381747202,334.242425081201));
#57741=CARTESIAN_POINT('Ctrl Pts',(97.4160672698385,4.83841703292822,334.106840679619));
#57742=CARTESIAN_POINT('Ctrl Pts',(97.4083183848103,4.81160730816411,333.972177904722));
#57743=CARTESIAN_POINT('Ctrl Pts',(97.4005694997822,4.77923870217493,333.838939928284));
#57744=CARTESIAN_POINT('Ctrl Pts',(97.3928123900074,4.746835739813,333.705560531681));
#57745=CARTESIAN_POINT('Ctrl Pts',(97.3850552802327,4.70886220233535,333.573609334915));
#57746=CARTESIAN_POINT('Ctrl Pts',(97.377298170458,4.66548249508715,333.443575844914));
#57747=CARTESIAN_POINT('Ctrl Pts',(97.3695369155318,4.62207960711038,333.313472869173));
#57748=CARTESIAN_POINT('Ctrl Pts',(97.3617756606056,4.57326493203777,333.185290007223));
#57749=CARTESIAN_POINT('Ctrl Pts',(97.3540144056795,4.51925107667216,333.059496774417));
#57750=CARTESIAN_POINT('Ctrl Pts',(97.3462407352748,4.46515081674115,332.933502313435));
#57751=CARTESIAN_POINT('Ctrl Pts',(97.3384670648701,4.40583492590786,332.809905472919));
#57752=CARTESIAN_POINT('Ctrl Pts',(97.3306933944655,4.34156242760417,332.689151941448));
#57753=CARTESIAN_POINT('Ctrl Pts',(97.3232815902885,4.28028182956064,332.57401951592));
#57754=CARTESIAN_POINT('Ctrl Pts',(97.3158697861116,4.2144958445608,332.46147189301));
#57755=CARTESIAN_POINT('Ctrl Pts',(97.3084579819346,4.14446458729827,332.351869273029));
#57756=CARTESIAN_POINT('Ctrl Pts',(97.3006829031562,4.07100088950344,332.23689470215));
#57757=CARTESIAN_POINT('Ctrl Pts',(97.2929078243777,3.99263309142799,332.124797779497));
#57758=CARTESIAN_POINT('Ctrl Pts',(97.2851327455993,3.90961342892804,332.016025151104));
#57759=CARTESIAN_POINT('Ctrl Pts',(97.2773672345502,3.82669592740815,331.907386374354));
#57760=CARTESIAN_POINT('Ctrl Pts',(97.2696017235012,3.73913818629106,331.802064060177));
#57761=CARTESIAN_POINT('Ctrl Pts',(97.2618362124522,3.64723691108034,331.700477916887));
#57762=CARTESIAN_POINT('Ctrl Pts',(97.25407840093,3.55542675625205,331.598992496554));
#57763=CARTESIAN_POINT('Ctrl Pts',(97.2463205894079,3.45928189829871,331.501236163089));
#57764=CARTESIAN_POINT('Ctrl Pts',(97.2385627778857,3.35914046444386,331.407597126903));
#57765=CARTESIAN_POINT('Ctrl Pts',(97.2308108043627,3.25907439019338,331.314028557061));
#57766=CARTESIAN_POINT('Ctrl Pts',(97.2230588308397,3.15501801077683,331.22457138318));
#57767=CARTESIAN_POINT('Ctrl Pts',(97.2153068573167,3.04734735468317,331.139578110827));
#57768=CARTESIAN_POINT('Ctrl Pts',(97.2075581667591,2.93972229717629,331.054620833175));
#57769=CARTESIAN_POINT('Ctrl Pts',(97.1998094762015,2.82848631350964,330.974123938731));
#57770=CARTESIAN_POINT('Ctrl Pts',(97.1920607856438,2.71404949390709,330.898400506251));
#57771=CARTESIAN_POINT('Ctrl Pts',(97.184313707266,2.59963648384064,330.822692828663));
#57772=CARTESIAN_POINT('Ctrl Pts',(97.1765666288882,2.48202428824806,330.751756853138));
#57773=CARTESIAN_POINT('Ctrl Pts',(97.1688195505104,2.3616527087174,330.68586282718));
#57774=CARTESIAN_POINT('Ctrl Pts',(97.1610724072045,2.2412801203568,330.619968248967));
#57775=CARTESIAN_POINT('Ctrl Pts',(97.1533252638987,2.11814844479384,330.559115892295));
#57776=CARTESIAN_POINT('Ctrl Pts',(97.1455781205929,1.99272250040752,330.503530262654));
#57777=CARTESIAN_POINT('Ctrl Pts',(97.1378292355648,1.86726835760628,330.447932136183));
#57778=CARTESIAN_POINT('Ctrl Pts',(97.1300803505367,1.7395192768804,330.397603251253));
#57779=CARTESIAN_POINT('Ctrl Pts',(97.1223314655087,1.60996010997533,330.352719988339));
#57780=CARTESIAN_POINT('Ctrl Pts',(97.1145743557339,1.48026342763182,330.307789085865));
#57781=CARTESIAN_POINT('Ctrl Pts',(97.1068172459592,1.34875319116615,330.268315479732));
#57782=CARTESIAN_POINT('Ctrl Pts',(97.0990601361845,1.21593000656208,330.234425818263));
#57783=CARTESIAN_POINT('Ctrl Pts',(97.0912988812583,1.08303584549521,330.200518047242));
#57784=CARTESIAN_POINT('Ctrl Pts',(97.0835376263321,0.948827720553178,330.172200247193));
#57785=CARTESIAN_POINT('Ctrl Pts',(97.075776371406,0.813815510953494,330.14954771422));
#57786=CARTESIAN_POINT('Ctrl Pts',(97.0680027010013,0.678587325818643,330.126858944576));
#57787=CARTESIAN_POINT('Ctrl Pts',(97.0602290305967,0.542552873730515,330.109853600238));
#57788=CARTESIAN_POINT('Ctrl Pts',(97.052455360192,0.406227116165392,330.09855505054));
#57789=CARTESIAN_POINT('Ctrl Pts',(97.0450435560149,0.276247355411802,330.087782451048));
#57790=CARTESIAN_POINT('Ctrl Pts',(97.0376317518377,0.146003086922303,330.082197312579));
#57791=CARTESIAN_POINT('Ctrl Pts',(97.0302199476605,0.0159379738098615,
330.081775824193));
#57792=CARTESIAN_POINT('Ctrl Pts',(97.0224448688821,-0.120502017939399,
330.081333677407));
#57793=CARTESIAN_POINT('Ctrl Pts',(97.0146697901036,-0.257176023963366,
330.086572753744));
#57794=CARTESIAN_POINT('Ctrl Pts',(97.0068947113252,-0.393571950787843,
330.097522648492));
#57795=CARTESIAN_POINT('Ctrl Pts',(96.9991292002761,-0.529800033741066,
330.108459068696));
#57796=CARTESIAN_POINT('Ctrl Pts',(96.9913636892271,-0.665750332466889,
330.12509229357));
#57797=CARTESIAN_POINT('Ctrl Pts',(96.983598178178,-0.800909340915666,330.147399945376));
#57798=CARTESIAN_POINT('Ctrl Pts',(96.9758403666559,-0.935934338813051,
330.169685479081));
#57799=CARTESIAN_POINT('Ctrl Pts',(96.9680825551337,-1.07016922459281,330.19763418));
#57800=CARTESIAN_POINT('Ctrl Pts',(96.9603247436115,-1.20310456379608,330.231171792665));
#57801=CARTESIAN_POINT('Ctrl Pts',(96.9525727700885,-1.33593986494134,330.264684167213));
#57802=CARTESIAN_POINT('Ctrl Pts',(96.9448207965655,-1.46747718859873,330.303776986772));
#57803=CARTESIAN_POINT('Ctrl Pts',(96.9370688230425,-1.59721661472551,330.348324801951));
#57804=CARTESIAN_POINT('Ctrl Pts',(96.9293201324849,-1.72690109612829,330.392853751104));
#57805=CARTESIAN_POINT('Ctrl Pts',(96.9215714419272,-1.85478882547357,330.44283297439));
#57806=CARTESIAN_POINT('Ctrl Pts',(96.9138227513696,-1.98039460480516,330.498087043072));
#57807=CARTESIAN_POINT('Ctrl Pts',(96.9060756729918,-2.10597425080545,330.553329615683));
#57808=CARTESIAN_POINT('Ctrl Pts',(96.898328594614,-2.22927253359901,330.613844693441));
#57809=CARTESIAN_POINT('Ctrl Pts',(96.8905815162361,-2.34982419441821,330.679408684239));
#57810=CARTESIAN_POINT('Ctrl Pts',(96.8828343729303,-2.4703768655766,330.744973224527));
#57811=CARTESIAN_POINT('Ctrl Pts',(96.8750872296244,-2.58818252547101,330.815586575505));
#57812=CARTESIAN_POINT('Ctrl Pts',(96.8673400863186,-2.70280084275048,330.890979354283));
#57813=CARTESIAN_POINT('Ctrl Pts',(96.8595912012905,-2.81744492866101,330.966389082959));
#57814=CARTESIAN_POINT('Ctrl Pts',(96.8518423162624,-2.92889991954033,331.046580162842));
#57815=CARTESIAN_POINT('Ctrl Pts',(96.8440934312342,-3.03675511218316,331.131240321352));
#57816=CARTESIAN_POINT('Ctrl Pts',(96.8363363214595,-3.14472478344174,331.21599033903));
#57817=CARTESIAN_POINT('Ctrl Pts',(96.8285792116848,-3.249086715979,331.305218669248));
#57818=CARTESIAN_POINT('Ctrl Pts',(96.82082210191,-3.34946350189497,331.398572878431));
#57819=CARTESIAN_POINT('Ctrl Pts',(96.8130608469839,-3.44989392595577,331.491976973118));
#57820=CARTESIAN_POINT('Ctrl Pts',(96.8052995920577,-3.5463346854169,331.589511062106));
#57821=CARTESIAN_POINT('Ctrl Pts',(96.7975383371315,-3.63844653727828,331.690787124123));
#57822=CARTESIAN_POINT('Ctrl Pts',(96.7897646667269,-3.73070573808358,331.792225194835));
#57823=CARTESIAN_POINT('Ctrl Pts',(96.7819909963222,-3.81862194261059,331.897416900176));
#57824=CARTESIAN_POINT('Ctrl Pts',(96.7742173259175,-3.90189682388459,332.005941844543));
#57825=CARTESIAN_POINT('Ctrl Pts',(96.7668055217405,-3.98129523939921,332.109414926638));
#57826=CARTESIAN_POINT('Ctrl Pts',(96.7593937175635,-4.05647454858417,332.215917671747));
#57827=CARTESIAN_POINT('Ctrl Pts',(96.7519819133866,-4.1272146829975,332.325064108628));
#57828=CARTESIAN_POINT('Ctrl Pts',(96.7440360237955,-4.20305226373831,332.442075502346));
#57829=CARTESIAN_POINT('Ctrl Pts',(96.7360901342044,-4.27401918672239,332.562482642817));
#57830=CARTESIAN_POINT('Ctrl Pts',(96.7281442446133,-4.33980458986947,332.685852384949));
#57831=CARTESIAN_POINT('Ctrl Pts',(96.7202093851187,-4.40549867292804,332.809050871221));
#57832=CARTESIAN_POINT('Ctrl Pts',(96.7122745256241,-4.46602538477777,332.935203449713));
#57833=CARTESIAN_POINT('Ctrl Pts',(96.7043396661294,-4.52111690709878,333.063847894703));
#57834=CARTESIAN_POINT('Ctrl Pts',(96.6964143958491,-4.57614185175478,333.192336873909));
#57835=CARTESIAN_POINT('Ctrl Pts',(96.6884891255689,-4.62574454215312,333.323311387149));
#57836=CARTESIAN_POINT('Ctrl Pts',(96.6805638552886,-4.6697029614376,333.456284574657));
#57837=CARTESIAN_POINT('Ctrl Pts',(96.6726487998849,-4.71360472273898,333.589086373095));
#57838=CARTESIAN_POINT('Ctrl Pts',(96.6647337444813,-4.75187659762769,333.723881363622));
#57839=CARTESIAN_POINT('Ctrl Pts',(96.6568186890776,-4.78434478643938,333.860163157741));
#57840=CARTESIAN_POINT('Ctrl Pts',(96.6489096294969,-4.81678837990684,333.9963417155));
#57841=CARTESIAN_POINT('Ctrl Pts',(96.6410005699162,-4.84343695578189,334.134004477713));
#57842=CARTESIAN_POINT('Ctrl Pts',(96.6330915103355,-4.86416650873616,334.2726299169));
#57843=CARTESIAN_POINT('Ctrl Pts',(96.6251876881894,-4.88488233443557,334.411163557352));
#57844=CARTESIAN_POINT('Ctrl Pts',(96.6172838660432,-4.89968689245801,334.55065824144));
#57845=CARTESIAN_POINT('Ctrl Pts',(96.6093800438971,-4.90850729581909,334.690582499863));
#57846=CARTESIAN_POINT('Ctrl Pts',(96.6035258214342,-4.91504041391476,334.794221944377));
#57847=CARTESIAN_POINT('Ctrl Pts',(96.5976715989714,-4.91829161310381,334.898096802524));
#57848=CARTESIAN_POINT('Ctrl Pts',(96.5918173765085,-4.91824959781168,335.001989001065));
#57849=CARTESIAN_POINT('',(94.8418173765432,-4.91824873103481,335.0035330121));
#57850=CARTESIAN_POINT('Ctrl Pts',(96.5918173764665,-4.91824959781138,335.001989001811));
#57851=CARTESIAN_POINT('Ctrl Pts',(96.5833945245865,-4.91818914764619,335.151465487433));
#57852=CARTESIAN_POINT('Ctrl Pts',(96.5749716727065,-4.91131016362299,335.300727750483));
#57853=CARTESIAN_POINT('Ctrl Pts',(96.5665488208265,-4.89769596485386,335.449174017898));
#57854=CARTESIAN_POINT('Ctrl Pts',(96.5580887459079,-4.88402160097038,335.598276312655));
#57855=CARTESIAN_POINT('Ctrl Pts',(96.5496286709893,-4.86355244556594,335.746555118912));
#57856=CARTESIAN_POINT('Ctrl Pts',(96.5411685960706,-4.83642350062271,335.893415236676));
#57857=CARTESIAN_POINT('Ctrl Pts',(96.5326895812262,-4.80923382096836,336.040604136368));
#57858=CARTESIAN_POINT('Ctrl Pts',(96.5242105663816,-4.77535461917704,336.186367738042));
#57859=CARTESIAN_POINT('Ctrl Pts',(96.5157315515371,-4.73497092739557,336.330125324629));
#57860=CARTESIAN_POINT('Ctrl Pts',(96.507224131049,-4.69445194575082,336.474364515134));
#57861=CARTESIAN_POINT('Ctrl Pts',(96.4987167105608,-4.64738494710277,336.616583982642));
#57862=CARTESIAN_POINT('Ctrl Pts',(96.4902092900727,-4.59400437601776,336.756219478206));
#57863=CARTESIAN_POINT('Ctrl Pts',(96.4847208197527,-4.55956647789453,336.846303808008));
#57864=CARTESIAN_POINT('Ctrl Pts',(96.4792323494327,-4.52250180143257,336.935313140221));
#57865=CARTESIAN_POINT('Ctrl Pts',(96.4737438791128,-4.4828833428076,337.023101578586));
#57866=CARTESIAN_POINT('Ctrl Pts',(96.4659688003343,-4.42675902784707,337.147464467393));
#57867=CARTESIAN_POINT('Ctrl Pts',(96.4581937215558,-4.36536704404127,337.269686626464));
#57868=CARTESIAN_POINT('Ctrl Pts',(96.4504186427774,-4.29889261447564,337.389289716988));
#57869=CARTESIAN_POINT('Ctrl Pts',(96.4426531317284,-4.23249998592756,337.508745628296));
#57870=CARTESIAN_POINT('Ctrl Pts',(96.4348876206794,-4.16103754390154,337.625588545381));
#57871=CARTESIAN_POINT('Ctrl Pts',(96.4271221096304,-4.08473839951597,337.739360376077));
#57872=CARTESIAN_POINT('Ctrl Pts',(96.4193642981082,-4.00851490595414,337.853019401671));
#57873=CARTESIAN_POINT('Ctrl Pts',(96.4116064865859,-3.92746446986302,337.963613078041));
#57874=CARTESIAN_POINT('Ctrl Pts',(96.4038486750637,-3.84186573159191,338.070708511552));
#57875=CARTESIAN_POINT('Ctrl Pts',(96.3960967015407,-3.75633140908602,338.177723352353));
#57876=CARTESIAN_POINT('Ctrl Pts',(96.3883447280177,-3.66625584025968,338.281244886136));
#57877=CARTESIAN_POINT('Ctrl Pts',(96.3805927544947,-3.57196031738197,338.380870088239));
#57878=CARTESIAN_POINT('Ctrl Pts',(96.3728440639371,-3.47770472871405,338.48045309901));
#57879=CARTESIAN_POINT('Ctrl Pts',(96.3650953733794,-3.3792330086492,338.576142776745));
#57880=CARTESIAN_POINT('Ctrl Pts',(96.3573466828218,-3.27690583841765,338.667570202279));
#57881=CARTESIAN_POINT('Ctrl Pts',(96.349599604444,-3.17459995820858,338.758978605574));
#57882=CARTESIAN_POINT('Ctrl Pts',(96.3418525260661,-3.06844051467748,338.846126260304));
#57883=CARTESIAN_POINT('Ctrl Pts',(96.3341054476883,-2.95882376378397,338.928682348748));
#57884=CARTESIAN_POINT('Ctrl Pts',(96.3263583043825,-2.84920609419659,339.011239129092));
#57885=CARTESIAN_POINT('Ctrl Pts',(96.3186111610767,-2.736131371682,339.089204031244));
#57886=CARTESIAN_POINT('Ctrl Pts',(96.3108640177709,-2.62002720093174,339.162287895963));
#57887=CARTESIAN_POINT('Ctrl Pts',(96.3031151327427,-2.50389692749893,339.235388191485));
#57888=CARTESIAN_POINT('Ctrl Pts',(96.2953662477147,-2.38473618127892,339.303605057765));
#57889=CARTESIAN_POINT('Ctrl Pts',(96.2876173626865,-2.26299932779089,339.366694070452));
#57890=CARTESIAN_POINT('Ctrl Pts',(96.2798602529118,-2.1411332615488,339.429850046469));
#57891=CARTESIAN_POINT('Ctrl Pts',(96.2721031431371,-2.01668597359211,339.487867116342));
#57892=CARTESIAN_POINT('Ctrl Pts',(96.2643460333624,-1.89013458747446,339.540547797759));
#57893=CARTESIAN_POINT('Ctrl Pts',(96.2565847784362,-1.76351557634231,339.593256630048));
#57894=CARTESIAN_POINT('Ctrl Pts',(96.24882352351,-1.63479059329713,339.640623256908));
#57895=CARTESIAN_POINT('Ctrl Pts',(96.2410622685838,-1.50445334011409,339.682499675378));
#57896=CARTESIAN_POINT('Ctrl Pts',(96.2332885981792,-1.37390758980286,339.724443082471));
#57897=CARTESIAN_POINT('Ctrl Pts',(96.2255149277745,-1.24174479254969,339.76087862711));
#57898=CARTESIAN_POINT('Ctrl Pts',(96.2177412573698,-1.10847116395459,339.791708958313));
#57899=CARTESIAN_POINT('Ctrl Pts',(96.2103294531928,-0.981401454835365,
339.821104130181));
#57900=CARTESIAN_POINT('Ctrl Pts',(96.2029176490158,-0.853322288157855,
339.845404136533));
#57901=CARTESIAN_POINT('Ctrl Pts',(96.1955058448387,-0.724676126173611,
339.864568590806));
#57902=CARTESIAN_POINT('Ctrl Pts',(96.1877307660603,-0.589724632572411,
339.88467235207));
#57903=CARTESIAN_POINT('Ctrl Pts',(96.1799556872819,-0.453722686406367,
339.899187946526));
#57904=CARTESIAN_POINT('Ctrl Pts',(96.1721806085035,-0.31717276782418,339.908012275642));
#57905=CARTESIAN_POINT('Ctrl Pts',(96.1644150974544,-0.18079088260991,339.916825745858));
#57906=CARTESIAN_POINT('Ctrl Pts',(96.1566495864054,-0.0438627530047198,
339.919961860654));
#57907=CARTESIAN_POINT('Ctrl Pts',(96.1488840753564,0.0931002517139404,
339.917368748185));
#57908=CARTESIAN_POINT('Ctrl Pts',(96.1411262638342,0.229927457214479,339.914778206795));
#57909=CARTESIAN_POINT('Ctrl Pts',(96.133368452312,0.366789080727974,339.906469750098));
#57910=CARTESIAN_POINT('Ctrl Pts',(96.1256106407898,0.503170304481162,339.892443429125));
#57911=CARTESIAN_POINT('Ctrl Pts',(96.1178586672668,0.639448897038578,339.878427663403));
#57912=CARTESIAN_POINT('Ctrl Pts',(96.1101066937438,0.775247422157984,339.858702637893));
#57913=CARTESIAN_POINT('Ctrl Pts',(96.1023547202208,0.91005309812221,339.833320434349));
#57914=CARTESIAN_POINT('Ctrl Pts',(96.0946060296632,1.04480168380263,339.807948980184));
#57915=CARTESIAN_POINT('Ctrl Pts',(96.0868573391056,1.17855787329232,339.776925185274));
#57916=CARTESIAN_POINT('Ctrl Pts',(96.079108648548,1.31081624928653,339.740352710833));
#57917=CARTESIAN_POINT('Ctrl Pts',(96.0713615701702,1.44304710782097,339.703787845601));
#57918=CARTESIAN_POINT('Ctrl Pts',(96.0636144917924,1.57378039621972,339.66167670123));
#57919=CARTESIAN_POINT('Ctrl Pts',(96.0558674134145,1.70252348596556,339.614173473357));
#57920=CARTESIAN_POINT('Ctrl Pts',(96.0481202701087,1.83126765470251,339.566669847362));
#57921=CARTESIAN_POINT('Ctrl Pts',(96.0403731268029,1.95802122480944,339.513774183036));
#57922=CARTESIAN_POINT('Ctrl Pts',(96.0326259834971,2.08230963467583,339.455689581629));
#57923=CARTESIAN_POINT('Ctrl Pts',(96.024877098469,2.20662598721531,339.39759192157));
#57924=CARTESIAN_POINT('Ctrl Pts',(96.0171282134409,2.32847572263421,339.334303168518));
#57925=CARTESIAN_POINT('Ctrl Pts',(96.0093793284129,2.44740741602913,339.26607313609));
#57926=CARTESIAN_POINT('Ctrl Pts',(96.0016222186381,2.56646534475237,339.1977706836));
#57927=CARTESIAN_POINT('Ctrl Pts',(95.9938651088634,2.68259870484572,339.124516669718));
#57928=CARTESIAN_POINT('Ctrl Pts',(95.9861079990887,2.79538323028787,339.046605448808));
#57929=CARTESIAN_POINT('Ctrl Pts',(95.9783467441626,2.90822802417418,338.968652594633));
#57930=CARTESIAN_POINT('Ctrl Pts',(95.9705854892364,3.01772010578734,338.886037809854));
#57931=CARTESIAN_POINT('Ctrl Pts',(95.9628242343102,3.12346784592035,338.799096165932));
#57932=CARTESIAN_POINT('Ctrl Pts',(95.9550505639056,3.22938474797446,338.712015443714));
#57933=CARTESIAN_POINT('Ctrl Pts',(95.9472768935009,3.33154504787365,338.62059429181));
#57934=CARTESIAN_POINT('Ctrl Pts',(95.9395032230963,3.42959293879054,338.525205715515));
#57935=CARTESIAN_POINT('Ctrl Pts',(95.9320914189191,3.52307667679721,338.434257500394));
#57936=CARTESIAN_POINT('Ctrl Pts',(95.924679614742,3.6128220568282,338.339703124455));
#57937=CARTESIAN_POINT('Ctrl Pts',(95.9172678105648,3.69855567524792,338.241892808159));
#57938=CARTESIAN_POINT('Ctrl Pts',(95.9094927317864,3.78849135369295,338.139288516899));
#57939=CARTESIAN_POINT('Ctrl Pts',(95.9017176530079,3.87429628360831,338.032776799959));
#57940=CARTESIAN_POINT('Ctrl Pts',(95.8939425742295,3.95561184639788,337.922724411082));
#57941=CARTESIAN_POINT('Ctrl Pts',(95.8861770631805,4.03682734521063,337.812807448677));
#57942=CARTESIAN_POINT('Ctrl Pts',(95.8784115521315,4.11356423891229,337.699358794924));
#57943=CARTESIAN_POINT('Ctrl Pts',(95.8706460410825,4.18550217610446,337.582780400329));
#57944=CARTESIAN_POINT('Ctrl Pts',(95.8628882295603,4.25736878662246,337.466317593552));
#57945=CARTESIAN_POINT('Ctrl Pts',(95.8551304180381,4.3244457057346,337.346731551867));
#57946=CARTESIAN_POINT('Ctrl Pts',(95.8473726065159,4.38645437891549,337.224455224138));
#57947=CARTESIAN_POINT('Ctrl Pts',(95.8396206329929,4.4484163886034,337.102270913223));
#57948=CARTESIAN_POINT('Ctrl Pts',(95.8318686594699,4.50531756789691,336.97740069319));
#57949=CARTESIAN_POINT('Ctrl Pts',(95.8241166859468,4.55692421784395,336.850303957551));
#57950=CARTESIAN_POINT('Ctrl Pts',(95.8163679953892,4.60850901234409,336.723261047454));
#57951=CARTESIAN_POINT('Ctrl Pts',(95.8086193048316,4.65480359040232,336.593993858578));
#57952=CARTESIAN_POINT('Ctrl Pts',(95.800870614274,4.69562161263999,336.462983504148));
#57953=CARTESIAN_POINT('Ctrl Pts',(95.7931235358961,4.73643114234722,336.332000407516));
#57954=CARTESIAN_POINT('Ctrl Pts',(95.7853764575183,4.77176626647043,336.199275239672));
#57955=CARTESIAN_POINT('Ctrl Pts',(95.7776293791405,4.80149006185392,336.065305706555));
#57956=CARTESIAN_POINT('Ctrl Pts',(95.7698822358347,4.83121410635141,335.931335050644));
#57957=CARTESIAN_POINT('Ctrl Pts',(95.7621350925289,4.85532664364326,335.796120390252));
#57958=CARTESIAN_POINT('Ctrl Pts',(95.754387949223,4.87374165338536,335.660170704104));
#57959=CARTESIAN_POINT('Ctrl Pts',(95.7466390641949,4.89216080321262,335.524190453579));
#57960=CARTESIAN_POINT('Ctrl Pts',(95.7388901791668,4.90487982413585,335.38747523573));
#57961=CARTESIAN_POINT('Ctrl Pts',(95.7311412941387,4.91186449783825,335.250539851872));
#57962=CARTESIAN_POINT('Ctrl Pts',(95.723384184364,4.91885658514548,335.113459123383));
#57963=CARTESIAN_POINT('Ctrl Pts',(95.7156270745892,4.92010214694343,334.976158153058));
#57964=CARTESIAN_POINT('Ctrl Pts',(95.7078699648145,4.91561911740867,334.839153007282));
#57965=CARTESIAN_POINT('Ctrl Pts',(95.7001087098884,4.91113369228627,334.702074650337));
#57966=CARTESIAN_POINT('Ctrl Pts',(95.6923474549622,4.90091360527163,334.565292822518));
#57967=CARTESIAN_POINT('Ctrl Pts',(95.684586200036,4.88502869206876,334.429318179574));
#57968=CARTESIAN_POINT('Ctrl Pts',(95.6768125296313,4.86911836818165,334.293126021515));
#57969=CARTESIAN_POINT('Ctrl Pts',(95.6690388592267,4.84752517139296,334.157744014796));
#57970=CARTESIAN_POINT('Ctrl Pts',(95.661265188822,4.8203702223217,334.023673219534));
#57971=CARTESIAN_POINT('Ctrl Pts',(95.653853384645,4.79447934266315,333.89584345205));
#57972=CARTESIAN_POINT('Ctrl Pts',(95.646441580468,4.76353292543133,333.769205849001));
#57973=CARTESIAN_POINT('Ctrl Pts',(95.639029776291,4.72767752408759,333.644179845725));
#57974=CARTESIAN_POINT('Ctrl Pts',(95.6312546975126,4.6900647427158,333.513025945594));
#57975=CARTESIAN_POINT('Ctrl Pts',(95.6234796187342,4.64693073867575,333.383231147783));
#57976=CARTESIAN_POINT('Ctrl Pts',(95.6157045399557,4.59838985391638,333.255295493816));
#57977=CARTESIAN_POINT('Ctrl Pts',(95.6079390289067,4.54990870180596,333.127517272816));
#57978=CARTESIAN_POINT('Ctrl Pts',(95.6001735178577,4.4960340448888,333.001594005565));
#57979=CARTESIAN_POINT('Ctrl Pts',(95.5924080068087,4.43693053139547,332.878012600869));
#57980=CARTESIAN_POINT('Ctrl Pts',(95.5846501952865,4.37788561920789,332.754553727496));
#57981=CARTESIAN_POINT('Ctrl Pts',(95.5768923837643,4.31362233530307,332.63343244619));
#57982=CARTESIAN_POINT('Ctrl Pts',(95.5691345722421,4.24435401377999,332.515117292867));
#57983=CARTESIAN_POINT('Ctrl Pts',(95.5613825987191,4.17513781886548,332.396891175449));
#57984=CARTESIAN_POINT('Ctrl Pts',(95.5536306251961,4.1009242799554,332.281467318736));
#57985=CARTESIAN_POINT('Ctrl Pts',(95.5458786516731,4.0219732429417,332.169290849352));
#57986=CARTESIAN_POINT('Ctrl Pts',(95.5381299611155,3.94305564173905,332.05716188677));
#57987=CARTESIAN_POINT('Ctrl Pts',(95.5303812705579,3.8594047573886,331.948277895179));
#57988=CARTESIAN_POINT('Ctrl Pts',(95.5226325800003,3.77132432933522,331.84305592931));
#57989=CARTESIAN_POINT('Ctrl Pts',(95.5148855016224,3.68326222715057,331.73785585575));
#57990=CARTESIAN_POINT('Ctrl Pts',(95.5071384232446,3.59077266513595,331.636316591944));
#57991=CARTESIAN_POINT('Ctrl Pts',(95.4993913448668,3.49420007785615,331.538822616737));
#57992=CARTESIAN_POINT('Ctrl Pts',(95.4916442015609,3.39762668120513,331.441327824437));
#57993=CARTESIAN_POINT('Ctrl Pts',(95.4838970582552,3.29697046610974,331.347878666056));
#57994=CARTESIAN_POINT('Ctrl Pts',(95.4761499149494,3.19261289309245,331.25882291553));
#57995=CARTESIAN_POINT('Ctrl Pts',(95.4684010299213,3.08823185827717,331.169747143381));
#57996=CARTESIAN_POINT('Ctrl Pts',(95.4606521448932,2.98014810693591,331.085066998243));
#57997=CARTESIAN_POINT('Ctrl Pts',(95.4529032598651,2.86877602898271,331.005089843559));
#57998=CARTESIAN_POINT('Ctrl Pts',(95.4451461500904,2.75728573955521,330.925027800297));
#57999=CARTESIAN_POINT('Ctrl Pts',(95.4373890403156,2.64250046938033,330.849678947437));
#58000=CARTESIAN_POINT('Ctrl Pts',(95.4296319305409,2.52486389490342,330.779307476881));
#58001=CARTESIAN_POINT('Ctrl Pts',(95.4218706756147,2.40716445920239,330.708898402061));
#58002=CARTESIAN_POINT('Ctrl Pts',(95.4141094206885,2.28661102656509,330.643472195695));
#58003=CARTESIAN_POINT('Ctrl Pts',(95.4063481657624,2.16367081041174,330.583246476577));
#58004=CARTESIAN_POINT('Ctrl Pts',(95.3985744953577,2.04053392997867,330.522924415935));
#58005=CARTESIAN_POINT('Ctrl Pts',(95.3908008249531,1.91500299448009,330.467819623731));
#58006=CARTESIAN_POINT('Ctrl Pts',(95.3830271545484,1.78756490137708,330.418101399434));
#58007=CARTESIAN_POINT('Ctrl Pts',(95.3756153503712,1.66605908216638,330.370697570439));
#58008=CARTESIAN_POINT('Ctrl Pts',(95.3682035461941,1.54281993799597,330.328190199428));
#58009=CARTESIAN_POINT('Ctrl Pts',(95.3607917420169,1.41827948947577,330.290683026995));
#58010=CARTESIAN_POINT('Ctrl Pts',(95.3530166632384,1.28763494258823,330.251337516314));
#58011=CARTESIAN_POINT('Ctrl Pts',(95.34524158446,1.1551454434434,330.217370407815));
#58012=CARTESIAN_POINT('Ctrl Pts',(95.3374665056816,1.0212933646164,330.188956150076));
#58013=CARTESIAN_POINT('Ctrl Pts',(95.3297009946325,0.887605999293833,330.16057685789));
#58014=CARTESIAN_POINT('Ctrl Pts',(95.3219354835835,0.752559769222005,330.137736900872));
#58015=CARTESIAN_POINT('Ctrl Pts',(95.3141699725345,0.616653227009483,330.120561317106));
#58016=CARTESIAN_POINT('Ctrl Pts',(95.3064121610123,0.480881436529245,330.103402762982));
#58017=CARTESIAN_POINT('Ctrl Pts',(95.2986543494901,0.344251416722254,330.091897454162));
#58018=CARTESIAN_POINT('Ctrl Pts',(95.2908965379679,0.207272616758024,330.086119545121));
#58019=CARTESIAN_POINT('Ctrl Pts',(95.2831445644449,0.0703968976847071,
330.080345984139));
#58020=CARTESIAN_POINT('Ctrl Pts',(95.2753925909219,-0.0668266901612984,
330.080291260399));
#58021=CARTESIAN_POINT('Ctrl Pts',(95.2676406173989,-0.203883212783746,
330.085977747502));
#58022=CARTESIAN_POINT('Ctrl Pts',(95.2598919268413,-0.340881691887493,
330.091661826375));
#58023=CARTESIAN_POINT('Ctrl Pts',(95.2521432362837,-0.477712856763349,
330.103082264027));
#58024=CARTESIAN_POINT('Ctrl Pts',(95.2443945457261,-0.613861626348289,
330.120209331724));
#58025=CARTESIAN_POINT('Ctrl Pts',(95.2366474673482,-0.74998206904458,330.137332835991));
#58026=CARTESIAN_POINT('Ctrl Pts',(95.2289003889704,-0.885420011280039,
330.160160559901));
#58027=CARTESIAN_POINT('Ctrl Pts',(95.2211533105925,-1.01966574328563,330.188610924642));
#58028=CARTESIAN_POINT('Ctrl Pts',(95.2134061672867,-1.15391260039966,330.217061527826));
#58029=CARTESIAN_POINT('Ctrl Pts',(95.2056590239809,-1.28696684497268,330.251134784794));
#58030=CARTESIAN_POINT('Ctrl Pts',(95.1979118806751,-1.4183295963068,330.290698117689));
#58031=CARTESIAN_POINT('Ctrl Pts',(95.1901629956471,-1.54972188077615,330.33027034526));
#58032=CARTESIAN_POINT('Ctrl Pts',(95.182414110619,-1.67942154108957,330.375334992149));
#58033=CARTESIAN_POINT('Ctrl Pts',(95.1746652255909,-1.80694585860989,330.425709921031));
#58034=CARTESIAN_POINT('Ctrl Pts',(95.1669081158161,-1.93460553175857,330.476138318384));
#58035=CARTESIAN_POINT('Ctrl Pts',(95.1591510060414,-2.0600848856947,330.531888113111));
#58036=CARTESIAN_POINT('Ctrl Pts',(95.1513938962667,-2.1829216570294,330.592729177623));
#58037=CARTESIAN_POINT('Ctrl Pts',(95.1436326413405,-2.30582406840723,330.653602753655));
#58038=CARTESIAN_POINT('Ctrl Pts',(95.1358713864144,-2.42608074090186,330.719572832635));
#58039=CARTESIAN_POINT('Ctrl Pts',(95.1281101314882,-2.54325583823656,330.790364290847));
#58040=CARTESIAN_POINT('Ctrl Pts',(95.1203364610835,-2.66061837753965,330.861268992321));
#58041=CARTESIAN_POINT('Ctrl Pts',(95.1125627906789,-2.77488916507475,330.937010269093));
#58042=CARTESIAN_POINT('Ctrl Pts',(95.1047891202742,-2.88566234515216,331.017270296358));
#58043=CARTESIAN_POINT('Ctrl Pts',(95.0973773160972,-2.99127900704595,331.093794200044));
#58044=CARTESIAN_POINT('Ctrl Pts',(95.0899655119201,-3.09371613455408,331.17442544804));
#58045=CARTESIAN_POINT('Ctrl Pts',(95.0825537077431,-3.19265269885515,331.258856884989));
#58046=CARTESIAN_POINT('Ctrl Pts',(95.0748901037727,-3.29495041596678,331.346156694856));
#58047=CARTESIAN_POINT('Ctrl Pts',(95.0672264998024,-3.39384881934144,331.437812771077));
#58048=CARTESIAN_POINT('Ctrl Pts',(95.059562895832,-3.48894604651845,331.533526497003));
#58049=CARTESIAN_POINT('Ctrl Pts',(95.0519087841593,-3.58392548431247,331.629121669937));
#58050=CARTESIAN_POINT('Ctrl Pts',(95.0442546724865,-3.67511282771166,331.728764214921));
#58051=CARTESIAN_POINT('Ctrl Pts',(95.0366005608138,-3.7621384884469,331.832114734362));
#58052=CARTESIAN_POINT('Ctrl Pts',(95.0289539735891,-3.8490785977698,331.935363654082));
#58053=CARTESIAN_POINT('Ctrl Pts',(95.0213073863645,-3.93186490413887,332.042312991526));
#58054=CARTESIAN_POINT('Ctrl Pts',(95.0136607991398,-4.01016435594877,332.152586278607));
#58055=CARTESIAN_POINT('Ctrl Pts',(95.0060199106811,-4.08840545358838,332.262777382403));
#58056=CARTESIAN_POINT('Ctrl Pts',(94.9983790222224,-4.16216611803201,332.376287179157));
#58057=CARTESIAN_POINT('Ctrl Pts',(94.9907381337637,-4.23115367591782,332.492706312921));
#58058=CARTESIAN_POINT('Ctrl Pts',(94.9831002448847,-4.30011415139341,332.609079744085));
#58059=CARTESIAN_POINT('Ctrl Pts',(94.9754623560057,-4.36430504078019,332.728359895267));
#58060=CARTESIAN_POINT('Ctrl Pts',(94.9678244671267,-4.42347731560101,332.850108956048));
#58061=CARTESIAN_POINT('Ctrl Pts',(94.9601878128149,-4.48264002597855,332.971838337647));
#58062=CARTESIAN_POINT('Ctrl Pts',(94.9525511585032,-4.53678555946599,333.096035472577));
#58063=CARTESIAN_POINT('Ctrl Pts',(94.9449145041915,-4.58571139008812,333.222239017945));
#58064=CARTESIAN_POINT('Ctrl Pts',(94.9372773207062,-4.63464061097224,333.348451308451));
#58065=CARTESIAN_POINT('Ctrl Pts',(94.9296401372208,-4.67834926551093,333.476669909567));
#58066=CARTESIAN_POINT('Ctrl Pts',(94.9220029537354,-4.7166836177908,333.606415157888));
#58067=CARTESIAN_POINT('Ctrl Pts',(94.914359929218,-4.75504728875635,333.736259637315));
#58068=CARTESIAN_POINT('Ctrl Pts',(94.9067169047005,-4.78802833608416,333.867632708348));
#58069=CARTESIAN_POINT('Ctrl Pts',(94.8990738801831,-4.81552337000894,334.000041133147));
#58070=CARTESIAN_POINT('Ctrl Pts',(94.891427580026,-4.84303018772731,334.132506305414));
#58071=CARTESIAN_POINT('Ctrl Pts',(94.8837812798689,-4.86504624396026,334.266007317853));
#58072=CARTESIAN_POINT('Ctrl Pts',(94.8761349797118,-4.88151980372615,334.400043777989));
#58073=CARTESIAN_POINT('Ctrl Pts',(94.8684794165725,-4.89801332011002,334.53424261435));
#58074=CARTESIAN_POINT('Ctrl Pts',(94.8608238534331,-4.90895090241172,334.668977792443));
#58075=CARTESIAN_POINT('Ctrl Pts',(94.8531682902938,-4.9143328816872,334.803746616671));
#58076=CARTESIAN_POINT('Ctrl Pts',(94.849384652377,-4.91699283765438,334.870353922246));
#58077=CARTESIAN_POINT('Ctrl Pts',(94.8456010144601,-4.91829654678943,334.936969477117));
#58078=CARTESIAN_POINT('Ctrl Pts',(94.8418173765432,-4.91824873103481,335.0035330121));
#58079=CARTESIAN_POINT('',(93.0918173764785,-4.91824847853219,334.996131419409));
#58080=CARTESIAN_POINT('Ctrl Pts',(94.8418173765085,-4.91824873103437,335.00353301271));
#58081=CARTESIAN_POINT('Ctrl Pts',(94.8293168088287,-4.91809075498242,335.223448869443));
#58082=CARTESIAN_POINT('Ctrl Pts',(94.8168162411489,-4.90318214465297,335.442842262135));
#58083=CARTESIAN_POINT('Ctrl Pts',(94.8043156734691,-4.87373462892463,335.660222560445));
#58084=CARTESIAN_POINT('Ctrl Pts',(94.7965405946907,-4.85541892035186,335.795428335698));
#58085=CARTESIAN_POINT('Ctrl Pts',(94.7887655159123,-4.83144374547594,335.930085020765));
#58086=CARTESIAN_POINT('Ctrl Pts',(94.7809904371338,-4.80185017708903,336.063681314723));
#58087=CARTESIAN_POINT('Ctrl Pts',(94.7732249260848,-4.77229302547203,336.197113209936));
#58088=CARTESIAN_POINT('Ctrl Pts',(94.7654594150358,-4.73713132053269,336.3294869324));
#58089=CARTESIAN_POINT('Ctrl Pts',(94.7576939039868,-4.69645780895182,336.460296925709));
#58090=CARTESIAN_POINT('Ctrl Pts',(94.7499360924646,-4.6558246252761,336.590977220529));
#58091=CARTESIAN_POINT('Ctrl Pts',(94.7421782809424,-4.6096906258712,336.720096500818));
#58092=CARTESIAN_POINT('Ctrl Pts',(94.7344204694202,-4.55819938312424,336.847160373705));
#58093=CARTESIAN_POINT('Ctrl Pts',(94.7266684958972,-4.50674688917036,336.974128626998));
#58094=CARTESIAN_POINT('Ctrl Pts',(94.7189165223742,-4.44994532257975,337.099044190835));
#58095=CARTESIAN_POINT('Ctrl Pts',(94.7111645488512,-4.38798765601154,337.221429133056));
#58096=CARTESIAN_POINT('Ctrl Pts',(94.7034158582935,-4.32605622855186,337.343762245181));
#58097=CARTESIAN_POINT('Ctrl Pts',(94.6956671677359,-4.25897322034282,337.463566519258));
#58098=CARTESIAN_POINT('Ctrl Pts',(94.6879184771782,-4.18697908547576,337.580385475135));
#58099=CARTESIAN_POINT('Ctrl Pts',(94.6801713988004,-4.11499992958977,337.697180125853));
#58100=CARTESIAN_POINT('Ctrl Pts',(94.6724243204226,-4.03811188442553,337.810990361274));
#58101=CARTESIAN_POINT('Ctrl Pts',(94.6646772420447,-3.95660036967125,337.921386071237));
#58102=CARTESIAN_POINT('Ctrl Pts',(94.6569300987389,-3.87508817177203,338.031782706422));
#58103=CARTESIAN_POINT('Ctrl Pts',(94.6491829554331,-3.78895265916973,338.138764444621));
#58104=CARTESIAN_POINT('Ctrl Pts',(94.6414358121273,-3.69852118145261,338.241932160432));
#58105=CARTESIAN_POINT('Ctrl Pts',(94.6336869270992,-3.60806937281932,338.345123070537));
#58106=CARTESIAN_POINT('Ctrl Pts',(94.6259380420711,-3.51331993478883,338.444497958097));
#58107=CARTESIAN_POINT('Ctrl Pts',(94.618189157043,-3.41463862717781,338.53969293983));
#58108=CARTESIAN_POINT('Ctrl Pts',(94.6104320472682,-3.31585257820739,338.634988962501));
#58109=CARTESIAN_POINT('Ctrl Pts',(94.6026749374935,-3.21312660480307,338.726095945025));
#58110=CARTESIAN_POINT('Ctrl Pts',(94.5949178277188,-3.10686167016336,338.812688503533));
#58111=CARTESIAN_POINT('Ctrl Pts',(94.5871565727926,-3.00053995094027,338.899327334335));
#58112=CARTESIAN_POINT('Ctrl Pts',(94.5793953178664,-2.89067581520077,338.981446700372));
#58113=CARTESIAN_POINT('Ctrl Pts',(94.5716340629402,-2.77770023030416,339.058763911965));
#58114=CARTESIAN_POINT('Ctrl Pts',(94.5638603925356,-2.66454392129045,339.136204805898));
#58115=CARTESIAN_POINT('Ctrl Pts',(94.5560867221309,-2.54826654869037,339.208827987543));
#58116=CARTESIAN_POINT('Ctrl Pts',(94.5483130517262,-2.42932552302091,339.276395744748));
#58117=CARTESIAN_POINT('Ctrl Pts',(94.5409012475492,-2.31592123071321,339.340818206598));
#58118=CARTESIAN_POINT('Ctrl Pts',(94.5334894433722,-2.20009594636449,339.400645180038));
#58119=CARTESIAN_POINT('Ctrl Pts',(94.5260776391952,-2.08226222623539,339.455711737051));
#58120=CARTESIAN_POINT('Ctrl Pts',(94.5183025604168,-1.95865312447281,339.513477270059));
#58121=CARTESIAN_POINT('Ctrl Pts',(94.5105274816384,-1.83244310240549,339.566186492906));
#58122=CARTESIAN_POINT('Ctrl Pts',(94.5027524028599,-1.70408435073156,339.613597250313));
#58123=CARTESIAN_POINT('Ctrl Pts',(94.4949868918109,-1.57588355267328,339.660949665764));
#58124=CARTESIAN_POINT('Ctrl Pts',(94.4872213807619,-1.44553964926298,339.703016454766));
#58125=CARTESIAN_POINT('Ctrl Pts',(94.4794558697129,-1.31352796421854,339.739602024402));
#58126=CARTESIAN_POINT('Ctrl Pts',(94.4716980581907,-1.18164716914417,339.776151319339));
#58127=CARTESIAN_POINT('Ctrl Pts',(94.4639402466685,-1.04810225746365,339.807230106441));
#58128=CARTESIAN_POINT('Ctrl Pts',(94.4561824351463,-0.913386669947358,
339.83269157444));
#58129=CARTESIAN_POINT('Ctrl Pts',(94.4484304616233,-0.778772460182841,
339.858133881877));
#58130=CARTESIAN_POINT('Ctrl Pts',(94.4406784881003,-0.642989710639765,
339.877967211969));
#58131=CARTESIAN_POINT('Ctrl Pts',(94.4329265145773,-0.50654475324799,339.892095203025));
#58132=CARTESIAN_POINT('Ctrl Pts',(94.4251778240196,-0.370157580376678,
339.906217210868));
#58133=CARTESIAN_POINT('Ctrl Pts',(94.417429133462,-0.233109145429348,339.914638645183));
#58134=CARTESIAN_POINT('Ctrl Pts',(94.4096804429044,-0.0959134358103597,
339.917314681341));
#58135=CARTESIAN_POINT('Ctrl Pts',(94.4019333645266,0.0412537290953617,
339.919990160727));
#58136=CARTESIAN_POINT('Ctrl Pts',(94.3941862861487,0.178567717169585,339.916922612031));
#58137=CARTESIAN_POINT('Ctrl Pts',(94.3864392077709,0.315512382629436,339.908119293467));
#58138=CARTESIAN_POINT('Ctrl Pts',(94.3786920644651,0.452458195817486,339.899315901124));
#58139=CARTESIAN_POINT('Ctrl Pts',(94.3709449211593,0.589034290148235,339.884776668106));
#58140=CARTESIAN_POINT('Ctrl Pts',(94.3631977778535,0.724727884910329,339.864560880011));
#58141=CARTESIAN_POINT('Ctrl Pts',(94.3554488928254,0.860451986473198,339.844340546977));
#58142=CARTESIAN_POINT('Ctrl Pts',(94.3477000077973,0.995292807132512,339.818441176936));
#58143=CARTESIAN_POINT('Ctrl Pts',(94.3399511227692,1.12874641604819,339.786973426995));
#58144=CARTESIAN_POINT('Ctrl Pts',(94.3321940129945,1.26234167400339,339.75547227686));
#58145=CARTESIAN_POINT('Ctrl Pts',(94.3244369032197,1.39454639791398,339.718391030223));
#58146=CARTESIAN_POINT('Ctrl Pts',(94.316679793445,1.52486998134862,339.67589078171));
#58147=CARTESIAN_POINT('Ctrl Pts',(94.3089185385189,1.65526320553931,339.633367822424));
#58148=CARTESIAN_POINT('Ctrl Pts',(94.3011572835927,1.78377292023109,339.585420227803));
#58149=CARTESIAN_POINT('Ctrl Pts',(94.2933960286665,1.90992818447491,339.532257427888));
#58150=CARTESIAN_POINT('Ctrl Pts',(94.2856223582618,2.03628525602753,339.47900958482));
#58151=CARTESIAN_POINT('Ctrl Pts',(94.2778486878572,2.16027999712832,339.420530032237));
#58152=CARTESIAN_POINT('Ctrl Pts',(94.2700750174526,2.28146497948108,339.357074776717));
#58153=CARTESIAN_POINT('Ctrl Pts',(94.2626632132755,2.39700877174998,339.296573378607));
#58154=CARTESIAN_POINT('Ctrl Pts',(94.2552514090984,2.50999825748356,339.231549234173));
#58155=CARTESIAN_POINT('Ctrl Pts',(94.2478396049213,2.62007148732974,339.162260018762));
#58156=CARTESIAN_POINT('Ctrl Pts',(94.2400645261428,2.73553973406183,339.089574732501));
#58157=CARTESIAN_POINT('Ctrl Pts',(94.2322894473644,2.84816352892613,339.011966017309));
#58158=CARTESIAN_POINT('Ctrl Pts',(94.224514368586,2.95749453204789,338.929683085874));
#58159=CARTESIAN_POINT('Ctrl Pts',(94.216748857537,3.06669099641003,338.847501408825));
#58160=CARTESIAN_POINT('Ctrl Pts',(94.2089833464879,3.17260242200452,338.760657193003));
#58161=CARTESIAN_POINT('Ctrl Pts',(94.2012178354389,3.27480710563654,338.669444301713));
#58162=CARTESIAN_POINT('Ctrl Pts',(94.1934600239167,3.3769104530271,338.57832184827));
#58163=CARTESIAN_POINT('Ctrl Pts',(94.1857022123945,3.47531408265366,338.482839597984));
#58164=CARTESIAN_POINT('Ctrl Pts',(94.1779444008723,3.56962750867437,338.383333047723));
#58165=CARTESIAN_POINT('Ctrl Pts',(94.1701924273493,3.66386996085115,338.283901379297));
#58166=CARTESIAN_POINT('Ctrl Pts',(94.1624404538264,3.75402806824117,338.180451721358));
#58167=CARTESIAN_POINT('Ctrl Pts',(94.1546884803033,3.83974679298242,338.073357712386));
#58168=CARTESIAN_POINT('Ctrl Pts',(94.1469397897457,3.92542921579286,337.96630905779));
#58169=CARTESIAN_POINT('Ctrl Pts',(94.1391910991881,4.00667575155903,337.855619426373));
#58170=CARTESIAN_POINT('Ctrl Pts',(94.1314424086305,4.08317055821811,337.741696783928));
#58171=CARTESIAN_POINT('Ctrl Pts',(94.1236953302526,4.15964944949376,337.627797844041));
#58172=CARTESIAN_POINT('Ctrl Pts',(94.1159482518748,4.23137836037357,337.510667555388));
#58173=CARTESIAN_POINT('Ctrl Pts',(94.108201173497,4.29808407834662,337.390743883808));
#58174=CARTESIAN_POINT('Ctrl Pts',(94.1004540301912,4.3647903553778,337.270819207151));
#58175=CARTESIAN_POINT('Ctrl Pts',(94.0927068868854,4.42647316552963,337.148101442459));
#58176=CARTESIAN_POINT('Ctrl Pts',(94.0849597435796,4.48290486825782,337.023053880808));
#58177=CARTESIAN_POINT('Ctrl Pts',(94.0772108585515,4.53934925803082,336.89797820581));
#58178=CARTESIAN_POINT('Ctrl Pts',(94.0694619735234,4.59054003044752,336.770572047779));
#58179=CARTESIAN_POINT('Ctrl Pts',(94.0617130884953,4.63629753353837,336.641319055822));
#58180=CARTESIAN_POINT('Ctrl Pts',(94.0539559787206,4.6821036041158,336.511928873404));
#58181=CARTESIAN_POINT('Ctrl Pts',(94.0461988689459,4.72246475473862,336.380688310327));
#58182=CARTESIAN_POINT('Ctrl Pts',(94.0384417591711,4.75725095802335,336.248097105551));
#58183=CARTESIAN_POINT('Ctrl Pts',(94.030680504245,4.79205574994286,336.115435048275));
#58184=CARTESIAN_POINT('Ctrl Pts',(94.0229192493188,4.82127957521477,335.981421292875));
#58185=CARTESIAN_POINT('Ctrl Pts',(94.0151579943927,4.84484369485811,335.846565198253));
#58186=CARTESIAN_POINT('Ctrl Pts',(94.007384323988,4.86844550941335,335.71149337783));
#58187=CARTESIAN_POINT('Ctrl Pts',(93.9996106535833,4.88636947526628,335.575576913268));
#58188=CARTESIAN_POINT('Ctrl Pts',(93.9918369831787,4.89858874468487,335.439330596415));
#58189=CARTESIAN_POINT('Ctrl Pts',(93.9844251790016,4.91023920417228,335.309426578391));
#58190=CARTESIAN_POINT('Ctrl Pts',(93.9770133748245,4.9167041079539,335.179223013674));
#58191=CARTESIAN_POINT('Ctrl Pts',(93.9696015706473,4.91800426916427,335.049163716113));
#58192=CARTESIAN_POINT('Ctrl Pts',(93.9618264918689,4.91936815514853,334.912729824952));
#58193=CARTESIAN_POINT('Ctrl Pts',(93.9540514130905,4.91505252858747,334.77602354415));
#58194=CARTESIAN_POINT('Ctrl Pts',(93.946276334312,4.90502433531529,334.639556755557));
#58195=CARTESIAN_POINT('Ctrl Pts',(93.938510823263,4.89500848237336,334.503257898035));
#58196=CARTESIAN_POINT('Ctrl Pts',(93.930745312214,4.87929407813407,334.36719833243));
#58197=CARTESIAN_POINT('Ctrl Pts',(93.922979801165,4.8579000307232,334.23189170425));
#58198=CARTESIAN_POINT('Ctrl Pts',(93.9152219896427,4.83652719557265,334.096719232987));
#58199=CARTESIAN_POINT('Ctrl Pts',(93.9074641781205,4.80948598467219,333.962298597084));
#58200=CARTESIAN_POINT('Ctrl Pts',(93.8997063665983,4.77684721020204,333.829139721023));
#58201=CARTESIAN_POINT('Ctrl Pts',(93.8919543930753,4.74423299744472,333.69608105124));
#58202=CARTESIAN_POINT('Ctrl Pts',(93.8842024195523,4.70602969826126,333.564282629445));
#58203=CARTESIAN_POINT('Ctrl Pts',(93.8764504460292,4.66235938186314,333.434245211774));
#58204=CARTESIAN_POINT('Ctrl Pts',(93.8687017554716,4.61870755986995,333.304262865026));
#58205=CARTESIAN_POINT('Ctrl Pts',(93.860953064914,4.56959344977913,333.176040408851));
#58206=CARTESIAN_POINT('Ctrl Pts',(93.8532043743564,4.51518919846861,333.05006421528));
#58207=CARTESIAN_POINT('Ctrl Pts',(93.8454572959785,4.46079626641697,332.924114232108));
#58208=CARTESIAN_POINT('Ctrl Pts',(93.8377102176007,4.40111553730479,332.800409940555));
#58209=CARTESIAN_POINT('Ctrl Pts',(93.8299631392229,4.33636745498178,332.679418099296));
#58210=CARTESIAN_POINT('Ctrl Pts',(93.822215995917,4.27161883000751,332.558425244009));
#58211=CARTESIAN_POINT('Ctrl Pts',(93.8144688526112,4.20180295154076,332.440145228988));
#58212=CARTESIAN_POINT('Ctrl Pts',(93.8067217093054,4.12718622157182,332.325020195409));
#58213=CARTESIAN_POINT('Ctrl Pts',(93.7989728242773,4.05255271617787,332.209869279279));
#58214=CARTESIAN_POINT('Ctrl Pts',(93.7912239392492,3.97311642407947,332.097875083972));
#58215=CARTESIAN_POINT('Ctrl Pts',(93.7834750542211,3.8891868361384,331.989450412947));
#58216=CARTESIAN_POINT('Ctrl Pts',(93.7757179444464,3.80516816446548,331.880910658855));
#58217=CARTESIAN_POINT('Ctrl Pts',(93.7679608346716,3.71664690960338,331.775948306966));
#58218=CARTESIAN_POINT('Ctrl Pts',(93.7602037248969,3.62397294742711,331.674943137506));
#58219=CARTESIAN_POINT('Ctrl Pts',(93.7524424699707,3.53124946324859,331.573883994114));
#58220=CARTESIAN_POINT('Ctrl Pts',(93.7446812150445,3.43436912599131,331.476786523225));
#58221=CARTESIAN_POINT('Ctrl Pts',(93.7369199601184,3.33371765624306,331.383992581458));
#58222=CARTESIAN_POINT('Ctrl Pts',(93.7291462897137,3.23290517694546,331.291050199625));
#58223=CARTESIAN_POINT('Ctrl Pts',(93.721372619309,3.12830980864425,331.202425356489));
#58224=CARTESIAN_POINT('Ctrl Pts',(93.7135989489044,3.02034992193897,331.118419212287));
#58225=CARTESIAN_POINT('Ctrl Pts',(93.7061871447273,2.9174155939345,331.038323574309));
#58226=CARTESIAN_POINT('Ctrl Pts',(93.6987753405503,2.81142316898638,330.962426478851));
#58227=CARTESIAN_POINT('Ctrl Pts',(93.6913635363733,2.70275712280939,330.890950596841));
#58228=CARTESIAN_POINT('Ctrl Pts',(93.6835884575949,2.58876503000877,330.815971468937));
#58229=CARTESIAN_POINT('Ctrl Pts',(93.6758133788164,2.4714703688187,330.745620958636));
#58230=CARTESIAN_POINT('Ctrl Pts',(93.668038300038,2.3512857041024,330.68020387053));
#58231=CARTESIAN_POINT('Ctrl Pts',(93.660272788989,2.23124893426737,330.614867282316));
#58232=CARTESIAN_POINT('Ctrl Pts',(93.6525072779399,2.1083295770204,330.554452222048));
#58233=CARTESIAN_POINT('Ctrl Pts',(93.6447417668909,1.98296980009994,330.499220752537));
#58234=CARTESIAN_POINT('Ctrl Pts',(93.6369839553687,1.85773431776327,330.444044045189));
#58235=CARTESIAN_POINT('Ctrl Pts',(93.6292261438465,1.73006358645143,330.394040857193));
#58236=CARTESIAN_POINT('Ctrl Pts',(93.6214683323243,1.60042473307406,330.349427590472));
#58237=CARTESIAN_POINT('Ctrl Pts',(93.6137163588013,1.47088343704494,330.304847896649));
#58238=CARTESIAN_POINT('Ctrl Pts',(93.6059643852783,1.33937733506883,330.265650177339));
#58239=CARTESIAN_POINT('Ctrl Pts',(93.5982124117553,1.20639358231703,330.232002769816));
#58240=CARTESIAN_POINT('Ctrl Pts',(93.5904637211977,1.07346614826357,330.19836961199));
#58241=CARTESIAN_POINT('Ctrl Pts',(93.58271503064,0.939062686223085,330.17028218653));
#58242=CARTESIAN_POINT('Ctrl Pts',(93.5749663400824,0.803685355365287,330.147858935267));
#58243=CARTESIAN_POINT('Ctrl Pts',(93.5672192617046,0.668336190891868,330.125440349348));
#58244=CARTESIAN_POINT('Ctrl Pts',(93.5594721833268,0.532013946007936,330.108683657381));
#58245=CARTESIAN_POINT('Ctrl Pts',(93.5517251049489,0.395230422856683,330.097656073331));
#58246=CARTESIAN_POINT('Ctrl Pts',(93.5439779616431,0.258445753327946,330.086628396859));
#58247=CARTESIAN_POINT('Ctrl Pts',(93.5362308183373,0.121200187431118,330.081329955484));
#58248=CARTESIAN_POINT('Ctrl Pts',(93.5284836750315,-0.0159903034833192,
330.081775994051));
#58249=CARTESIAN_POINT('Ctrl Pts',(93.5207347900034,-0.153211637732751,
330.082222132896));
#58250=CARTESIAN_POINT('Ctrl Pts',(93.5129859049753,-0.290377481565105,
330.088415320315));
#58251=CARTESIAN_POINT('Ctrl Pts',(93.5052370199472,-0.426973216483055,
330.100318690475));
#58252=CARTESIAN_POINT('Ctrl Pts',(93.4974799101725,-0.563713935525438,
330.112234694996));
#58253=CARTESIAN_POINT('Ctrl Pts',(93.4897228003977,-0.699882946856863,
330.129872955382));
#58254=CARTESIAN_POINT('Ctrl Pts',(93.481965690623,-0.834971547270154,330.153144774418));
#58255=CARTESIAN_POINT('Ctrl Pts',(93.4742044356968,-0.970132334712393,
330.176429029171));
#58256=CARTESIAN_POINT('Ctrl Pts',(93.4664431807707,-1.1042111789492,330.205352758672));
#58257=CARTESIAN_POINT('Ctrl Pts',(93.4586819258445,-1.23671186991421,330.239776600483));
#58258=CARTESIAN_POINT('Ctrl Pts',(93.4509082554399,-1.36942451880271,330.274255509221));
#58259=CARTESIAN_POINT('Ctrl Pts',(93.4431345850352,-1.50055359559283,330.314251997957));
#58260=CARTESIAN_POINT('Ctrl Pts',(93.4353609146305,-1.62961944387752,330.359577225011));
#58261=CARTESIAN_POINT('Ctrl Pts',(93.4279491104535,-1.75267724587232,330.402792551841));
#58262=CARTESIAN_POINT('Ctrl Pts',(93.4205373062764,-1.87385931562098,330.450851569902));
#58263=CARTESIAN_POINT('Ctrl Pts',(93.4131255020994,-1.99277034251709,330.50355146538));
#58264=CARTESIAN_POINT('Ctrl Pts',(93.4053504233209,-2.11750955305984,330.558834339721));
#58265=CARTESIAN_POINT('Ctrl Pts',(93.3975753445425,-2.24014366957103,330.619399224852));
#58266=CARTESIAN_POINT('Ctrl Pts',(93.3898002657641,-2.36019311284394,330.685064133433));
#58267=CARTESIAN_POINT('Ctrl Pts',(93.3820347547151,-2.4800948276341,330.750648237164));
#58268=CARTESIAN_POINT('Ctrl Pts',(93.3742692436661,-2.59741785802978,330.821319691316));
#58269=CARTESIAN_POINT('Ctrl Pts',(93.3665037326171,-2.71170254748708,330.896848484829));
#58270=CARTESIAN_POINT('Ctrl Pts',(93.3587459210949,-2.82587392334213,330.972302391323));
#58271=CARTESIAN_POINT('Ctrl Pts',(93.3509881095727,-2.93701262935733,331.052603838811));
#58272=CARTESIAN_POINT('Ctrl Pts',(93.3432302980505,-3.04468389936381,331.137477117808));
#58273=CARTESIAN_POINT('Ctrl Pts',(93.3354783245275,-3.15227414332494,331.222286526971));
#58274=CARTESIAN_POINT('Ctrl Pts',(93.3277263510045,-3.25640183933689,331.311660678599));
#58275=CARTESIAN_POINT('Ctrl Pts',(93.3199743774815,-3.35666180137882,331.405281010473));
#58276=CARTESIAN_POINT('Ctrl Pts',(93.3122256869239,-3.45687930326736,331.498861694081));
#58277=CARTESIAN_POINT('Ctrl Pts',(93.3044769963663,-3.5532320439348,331.596684715111));
#58278=CARTESIAN_POINT('Ctrl Pts',(93.2967283058087,-3.64534867597783,331.698391892873));
#58279=CARTESIAN_POINT('Ctrl Pts',(93.2889812274308,-3.73744614238625,331.800077909608));
#58280=CARTESIAN_POINT('Ctrl Pts',(93.281234149053,-3.82530899102509,331.905646186116));
#58281=CARTESIAN_POINT('Ctrl Pts',(93.2734870706751,-3.90860373473029,332.01470271039));
#58282=CARTESIAN_POINT('Ctrl Pts',(93.2657399273693,-3.99189917652562,332.123760148663));
#58283=CARTESIAN_POINT('Ctrl Pts',(93.2579927840635,-4.07062619977048,332.236305582379));
#58284=CARTESIAN_POINT('Ctrl Pts',(93.2502456407577,-4.14449276304682,332.351913370082));
#58285=CARTESIAN_POINT('Ctrl Pts',(93.2424967557296,-4.21837593309477,332.467547148869));
#58286=CARTESIAN_POINT('Ctrl Pts',(93.2347478707016,-4.28739625834084,332.58624432233));
#58287=CARTESIAN_POINT('Ctrl Pts',(93.2269989856735,-4.3513062504514,332.707552186574));
#58288=CARTESIAN_POINT('Ctrl Pts',(93.2192418758988,-4.4152840772879,332.828988808238));
#58289=CARTESIAN_POINT('Ctrl Pts',(93.211484766124,-4.47414055324128,332.953041309683));
#58290=CARTESIAN_POINT('Ctrl Pts',(93.2037276563493,-4.52767497719698,333.079233912377));
#58291=CARTESIAN_POINT('Ctrl Pts',(93.1959664014232,-4.58123800823714,333.205493948362));
#58292=CARTESIAN_POINT('Ctrl Pts',(93.188205146497,-4.62947318309786,333.333895998604));
#58293=CARTESIAN_POINT('Ctrl Pts',(93.1804438915708,-4.67222916688808,333.463947372457));
#58294=CARTESIAN_POINT('Ctrl Pts',(93.1726702211662,-4.71505354631822,333.594206786126));
#58295=CARTESIAN_POINT('Ctrl Pts',(93.1648965507615,-4.75238111328922,333.726120419367));
#58296=CARTESIAN_POINT('Ctrl Pts',(93.1571228803569,-4.78411109919153,333.859182725809));
#58297=CARTESIAN_POINT('Ctrl Pts',(93.1497110761798,-4.81436404661656,333.986050949874));
#58298=CARTESIAN_POINT('Ctrl Pts',(93.1422992720026,-4.83952876440203,334.113963029932));
#58299=CARTESIAN_POINT('Ctrl Pts',(93.1348874678254,-4.85956187775862,334.242476786669));
#58300=CARTESIAN_POINT('Ctrl Pts',(93.121960343435,-4.89450216248528,334.466621040822));
#58301=CARTESIAN_POINT('Ctrl Pts',(93.1090332190446,-4.91394075435093,334.693242051901));
#58302=CARTESIAN_POINT('Ctrl Pts',(93.0961060946542,-4.91760996652478,334.920657201737));
#58303=CARTESIAN_POINT('Ctrl Pts',(93.0946765219389,-4.91801573392143,334.945806375166));
#58304=CARTESIAN_POINT('Ctrl Pts',(93.0932469492237,-4.91822868337733,334.970965218337));
#58305=CARTESIAN_POINT('Ctrl Pts',(93.0918173765085,-4.91824847853178,334.996131418882));
#58306=CARTESIAN_POINT('',(91.3418173765403,-4.91824977563263,334.998514405971));
#58307=CARTESIAN_POINT('Ctrl Pts',(93.0918173764786,-4.91824847853219,334.996131419409));
#58308=CARTESIAN_POINT('Ctrl Pts',(93.0841670405432,-4.91835441197591,335.130807946413));
#58309=CARTESIAN_POINT('Ctrl Pts',(93.0765167046078,-4.91292441288391,335.265689551054));
#58310=CARTESIAN_POINT('Ctrl Pts',(93.0688663686724,-4.9019345736358,335.400275527973));
#58311=CARTESIAN_POINT('Ctrl Pts',(93.0612235414835,-4.89095552083125,335.53472940978));
#58312=CARTESIAN_POINT('Ctrl Pts',(93.0535807142946,-4.87442751375331,335.668887841591));
#58313=CARTESIAN_POINT('Ctrl Pts',(93.0459378871057,-4.85237868326861,335.802249447903));
#58314=CARTESIAN_POINT('Ctrl Pts',(93.0380508682076,-4.82962538289751,335.939872016523));
#58315=CARTESIAN_POINT('Ctrl Pts',(93.0301638493095,-4.80099256063041,336.076645554702));
#58316=CARTESIAN_POINT('Ctrl Pts',(93.0222768304114,-4.76656921628651,336.212023501773));
#58317=CARTESIAN_POINT('Ctrl Pts',(93.0146424450639,-4.73324850550022,336.343065081467));
#58318=CARTESIAN_POINT('Ctrl Pts',(93.0070080597165,-4.6945026516089,336.472798683477));
#58319=CARTESIAN_POINT('Ctrl Pts',(92.999373674369,-4.65046431971374,336.600738789925));
#58320=CARTESIAN_POINT('Ctrl Pts',(92.9917404031036,-4.60643241431026,336.728660226137));
#58321=CARTESIAN_POINT('Ctrl Pts',(92.9841071318382,-4.5571096977126,336.854788305704));
#58322=CARTESIAN_POINT('Ctrl Pts',(92.9764738605728,-4.50267839643901,336.978653663667));
#58323=CARTESIAN_POINT('Ctrl Pts',(92.9688399372556,-4.44824244551771,337.102529602495));
#58324=CARTESIAN_POINT('Ctrl Pts',(92.9612060139385,-4.38869720493128,337.224142066119));
#58325=CARTESIAN_POINT('Ctrl Pts',(92.9535720906214,-4.32427240432899,337.34304315702));
#58326=CARTESIAN_POINT('Ctrl Pts',(92.9459357487757,-4.25982719309214,337.46198191737));
#58327=CARTESIAN_POINT('Ctrl Pts',(92.9382994069301,-4.19049954043573,337.578207242644));
#58328=CARTESIAN_POINT('Ctrl Pts',(92.9306630650844,-4.11656403727938,337.691297751918));
#58329=CARTESIAN_POINT('Ctrl Pts',(92.9230185230526,-4.04254913944699,337.80450970196));
#58330=CARTESIAN_POINT('Ctrl Pts',(92.9153739810208,-3.96391673735568,337.914579780392));
#58331=CARTESIAN_POINT('Ctrl Pts',(92.907729438989,-3.88098360102912,338.021117235567));
#58332=CARTESIAN_POINT('Ctrl Pts',(92.9000799730801,-3.79799704717011,338.127723311903));
#58333=CARTESIAN_POINT('Ctrl Pts',(92.8924305071712,-3.71070450560542,338.230791929636));
#58334=CARTESIAN_POINT('Ctrl Pts',(92.8847810412623,-3.61946064865998,338.329968119262));
#58335=CARTESIAN_POINT('Ctrl Pts',(92.8771210068183,-3.52809072880846,338.42928133114));
#58336=CARTESIAN_POINT('Ctrl Pts',(92.8694609723744,-3.43275888576777,338.524691102134));
#58337=CARTESIAN_POINT('Ctrl Pts',(92.8618009379304,-3.33385409106862,338.615881629971));
#58338=CARTESIAN_POINT('Ctrl Pts',(92.8600837698041,-3.31168236818159,338.636324027322));
#58339=CARTESIAN_POINT('Ctrl Pts',(92.8583666016778,-3.28933121214617,338.656554563683));
#58340=CARTESIAN_POINT('Ctrl Pts',(92.8566494335515,-3.26680520479631,338.676569979807));
#58341=CARTESIAN_POINT('Ctrl Pts',(92.848874354773,-3.16481083451602,338.767196770952));
#58342=CARTESIAN_POINT('Ctrl Pts',(92.8410992759946,-3.05888122157502,338.853719305274));
#58343=CARTESIAN_POINT('Ctrl Pts',(92.8333241972162,-2.94938068862535,338.935776494679));
#58344=CARTESIAN_POINT('Ctrl Pts',(92.8255586861672,-2.84001490305284,339.017732707487));
#58345=CARTESIAN_POINT('Ctrl Pts',(92.8177931751182,-2.72708725056083,339.095234276476));
#58346=CARTESIAN_POINT('Ctrl Pts',(92.8100276640692,-2.61099750827896,339.167958142096));
#58347=CARTESIAN_POINT('Ctrl Pts',(92.802269852547,-2.49502286931439,339.240609901791));
#58348=CARTESIAN_POINT('Ctrl Pts',(92.7945120410248,-2.37589270893908,339.308493179057));
#58349=CARTESIAN_POINT('Ctrl Pts',(92.7867542295026,-2.25403808430272,339.371326500848));
#58350=CARTESIAN_POINT('Ctrl Pts',(92.7790022559797,-2.13227515913579,339.434112538571));
#58351=CARTESIAN_POINT('Ctrl Pts',(92.7712502824566,-2.00779219663088,339.491856006617));
#58352=CARTESIAN_POINT('Ctrl Pts',(92.7634983089337,-1.88104700101329,339.544320107836));
#58353=CARTESIAN_POINT('Ctrl Pts',(92.7557496183761,-1.75435548206121,339.596761990477));
#58354=CARTESIAN_POINT('Ctrl Pts',(92.7480009278185,-1.62540399590929,339.643928803986));
#58355=CARTESIAN_POINT('Ctrl Pts',(92.7402522372609,-1.49467238594812,339.685630962974));
#58356=CARTESIAN_POINT('Ctrl Pts',(92.732505158883,-1.36396797579029,339.72732444548));
#58357=CARTESIAN_POINT('Ctrl Pts',(92.7247580805052,-1.23148455066784,339.76355541626));
#58358=CARTESIAN_POINT('Ctrl Pts',(92.7170110021274,-1.09771888014727,339.794183592925));
#58359=CARTESIAN_POINT('Ctrl Pts',(92.7092638588216,-0.963952088541721,
339.824812026283));
#58360=CARTESIAN_POINT('Ctrl Pts',(92.7015167155159,-0.828903411117643,
339.849837484626));
#58361=CARTESIAN_POINT('Ctrl Pts',(92.6937695722101,-0.693081233854145,
339.86917051106));
#58362=CARTESIAN_POINT('Ctrl Pts',(92.686020687182,-0.557228520881242,339.888507883969));
#58363=CARTESIAN_POINT('Ctrl Pts',(92.6782718021538,-0.420602348927069,
339.902150223279));
#58364=CARTESIAN_POINT('Ctrl Pts',(92.6705229171257,-0.283717276389902,
339.910059833605));
#58365=CARTESIAN_POINT('Ctrl Pts',(92.662765807351,-0.14668691262255,339.917977839272));
#58366=CARTESIAN_POINT('Ctrl Pts',(92.6550086975763,-0.0093974901736511,
339.920150938457));
#58367=CARTESIAN_POINT('Ctrl Pts',(92.6472515878016,0.127634815189879,339.916593578531));
#58368=CARTESIAN_POINT('Ctrl Pts',(92.6394903328754,0.26474034623586,339.913034317665));
#58369=CARTESIAN_POINT('Ctrl Pts',(92.6317290779493,0.401588096646474,339.903738522507));
#58370=CARTESIAN_POINT('Ctrl Pts',(92.6239678230231,0.537666950536118,339.888772577325));
#58371=CARTESIAN_POINT('Ctrl Pts',(92.6161941526184,0.67396348624399,339.873782691507));
#58372=CARTESIAN_POINT('Ctrl Pts',(92.6084204822138,0.809488280953241,339.853104589322));
#58373=CARTESIAN_POINT('Ctrl Pts',(92.6006468118091,0.943739467722467,339.826856003608));
#58374=CARTESIAN_POINT('Ctrl Pts',(92.593235007632,1.07174122944952,339.801829295873));
#58375=CARTESIAN_POINT('Ctrl Pts',(92.5858232034549,1.1985850077016,339.771739112013));
#58376=CARTESIAN_POINT('Ctrl Pts',(92.5784113992777,1.32385038664073,339.73672916856));
#58377=CARTESIAN_POINT('Ctrl Pts',(92.5706363204993,1.4552553949473,339.70000328349));
#58378=CARTESIAN_POINT('Ctrl Pts',(92.5628612417208,1.5853386317387,339.657747120043));
#58379=CARTESIAN_POINT('Ctrl Pts',(92.5550861629424,1.71359929444044,339.610071639421));
#58380=CARTESIAN_POINT('Ctrl Pts',(92.5473206518934,1.84170212423134,339.562454826513));
#58381=CARTESIAN_POINT('Ctrl Pts',(92.5395551408444,1.96798647956887,339.509432100346));
#58382=CARTESIAN_POINT('Ctrl Pts',(92.5317896297953,2.0919643504414,339.451164815976));
#58383=CARTESIAN_POINT('Ctrl Pts',(92.5240318182731,2.21581929689341,339.392955303789));
#58384=CARTESIAN_POINT('Ctrl Pts',(92.516274006751,2.33737195843876,339.329511746869));
#58385=CARTESIAN_POINT('Ctrl Pts',(92.5085161952288,2.45615236862982,339.261044309154));
#58386=CARTESIAN_POINT('Ctrl Pts',(92.5007642217058,2.57484339279587,339.192628395357));
#58387=CARTESIAN_POINT('Ctrl Pts',(92.4930122481827,2.69076598082098,339.119196320338));
#58388=CARTESIAN_POINT('Ctrl Pts',(92.4852602746597,2.80347326079535,339.041004916912));
#58389=CARTESIAN_POINT('Ctrl Pts',(92.4775115841021,2.91613280916965,338.962846627592));
#58390=CARTESIAN_POINT('Ctrl Pts',(92.4697628935445,3.02557943730098,338.879933241048));
#58391=CARTESIAN_POINT('Ctrl Pts',(92.4620142029868,3.13139404799926,338.792565672293));
#58392=CARTESIAN_POINT('Ctrl Pts',(92.454267124609,3.23718664308401,338.70521628109));
#58393=CARTESIAN_POINT('Ctrl Pts',(92.4465200462312,3.33934842259777,338.613414799716));
#58394=CARTESIAN_POINT('Ctrl Pts',(92.4387729678533,3.43749258956973,338.517503057448));
#58395=CARTESIAN_POINT('Ctrl Pts',(92.4310258245475,3.53563757908407,338.421590511346));
#58396=CARTESIAN_POINT('Ctrl Pts',(92.4232786812417,3.6297646093454,338.321567908833));
#58397=CARTESIAN_POINT('Ctrl Pts',(92.4155315379359,3.71952333731798,338.217814352266));
#58398=CARTESIAN_POINT('Ctrl Pts',(92.4077826529079,3.80930224495782,338.114037469696));
#58399=CARTESIAN_POINT('Ctrl Pts',(92.4000337678799,3.89471064038191,338.006528259507));
#58400=CARTESIAN_POINT('Ctrl Pts',(92.3922848828518,3.97543836766182,337.895699025697));
#58401=CARTESIAN_POINT('Ctrl Pts',(92.3845277730771,4.0562517801861,337.784752156592));
#58402=CARTESIAN_POINT('Ctrl Pts',(92.3767706633023,4.13237436980426,337.670478540975));
#58403=CARTESIAN_POINT('Ctrl Pts',(92.3690135535276,4.20353895329355,337.553320060361));
#58404=CARTESIAN_POINT('Ctrl Pts',(92.3612522986014,4.27474156486085,337.436098974002));
#58405=CARTESIAN_POINT('Ctrl Pts',(92.3534910436753,4.34098070246503,337.31599029301));
#58406=CARTESIAN_POINT('Ctrl Pts',(92.3457297887491,4.40203559591913,337.193459749975));
#58407=CARTESIAN_POINT('Ctrl Pts',(92.3379561183444,4.46318815730497,337.070733198004));
#58408=CARTESIAN_POINT('Ctrl Pts',(92.3301824479398,4.51913974285814,336.945577399237));
#58409=CARTESIAN_POINT('Ctrl Pts',(92.3224087775351,4.56971776763404,336.818478096285));
#58410=CARTESIAN_POINT('Ctrl Pts',(92.314996973358,4.61794137318849,336.697295296464));
#58411=CARTESIAN_POINT('Ctrl Pts',(92.3075851691809,4.66128034234134,336.574346132178));
#58412=CARTESIAN_POINT('Ctrl Pts',(92.3001733650038,4.69962801825756,336.450061913336));
#58413=CARTESIAN_POINT('Ctrl Pts',(92.2923982862253,4.73985522800213,336.319686154706));
#58414=CARTESIAN_POINT('Ctrl Pts',(92.2846232074469,4.77471662226578,336.187429150985));
#58415=CARTESIAN_POINT('Ctrl Pts',(92.2768481286685,4.80403449768238,336.053772085215));
#58416=CARTESIAN_POINT('Ctrl Pts',(92.2690826176194,4.83331629558679,335.920279492973));
#58417=CARTESIAN_POINT('Ctrl Pts',(92.2613171065704,4.85706806483019,335.785390644839));
#58418=CARTESIAN_POINT('Ctrl Pts',(92.2535515955214,4.87516140210359,335.649603237322));
#58419=CARTESIAN_POINT('Ctrl Pts',(92.2457937839992,4.89323679978045,335.513950463415));
#58420=CARTESIAN_POINT('Ctrl Pts',(92.238035972477,4.90566487911035,335.377401288069));
#58421=CARTESIAN_POINT('Ctrl Pts',(92.2302781609548,4.91236804562007,335.240464647861));
#58422=CARTESIAN_POINT('Ctrl Pts',(92.2225261874318,4.91906616778437,335.103631056818));
#58423=CARTESIAN_POINT('Ctrl Pts',(92.2147742139088,4.92004793331333,334.966410970124));
#58424=CARTESIAN_POINT('Ctrl Pts',(92.2070222403858,4.91528749036846,334.829319158874));
#58425=CARTESIAN_POINT('Ctrl Pts',(92.1992735498282,4.91052906347398,334.692285406087));
#58426=CARTESIAN_POINT('Ctrl Pts',(92.1915248592706,4.90003327837805,334.555380210522));
#58427=CARTESIAN_POINT('Ctrl Pts',(92.1837761687129,4.88382638339658,334.419118842327));
#58428=CARTESIAN_POINT('Ctrl Pts',(92.1760290903351,4.86762286039498,334.282885824447));
#58429=CARTESIAN_POINT('Ctrl Pts',(92.1682820119573,4.84571063714553,334.147296755389));
#58430=CARTESIAN_POINT('Ctrl Pts',(92.1605349335794,4.81816784714409,334.012861884412));
#58431=CARTESIAN_POINT('Ctrl Pts',(92.1527877902736,4.79062482630755,333.878425886741));
#58432=CARTESIAN_POINT('Ctrl Pts',(92.1450406469678,4.75745122304795,333.745144489367));
#58433=CARTESIAN_POINT('Ctrl Pts',(92.137293503662,4.71877624190575,333.613517457259));
#58434=CARTESIAN_POINT('Ctrl Pts',(92.1295446186339,4.6800925658068,333.4818608326));
#58435=CARTESIAN_POINT('Ctrl Pts',(92.1217957336059,4.63590516084678,333.351859688269));
#58436=CARTESIAN_POINT('Ctrl Pts',(92.1140468485778,4.58639289908473,333.223997962353));
#58437=CARTESIAN_POINT('Ctrl Pts',(92.106289738803,4.5368280844964,333.096000522681));
#58438=CARTESIAN_POINT('Ctrl Pts',(92.0985326290283,4.48192726435879,332.970147402637));
#58439=CARTESIAN_POINT('Ctrl Pts',(92.0907755192536,4.42191743809321,332.846902409739));
#58440=CARTESIAN_POINT('Ctrl Pts',(92.0830142643274,4.36187554449522,332.723591558657));
#58441=CARTESIAN_POINT('Ctrl Pts',(92.0752530094013,4.29671939040158,332.602891955577));
#58442=CARTESIAN_POINT('Ctrl Pts',(92.0674917544751,4.22672114886593,332.485241285485));
#58443=CARTESIAN_POINT('Ctrl Pts',(92.0597180840704,4.1566109329562,332.367402412663));
#58444=CARTESIAN_POINT('Ctrl Pts',(92.0519444136658,4.08164336513511,332.252622546546));
#58445=CARTESIAN_POINT('Ctrl Pts',(92.0441707432611,4.00213352111117,332.141309680693));
#58446=CARTESIAN_POINT('Ctrl Pts',(92.036758939084,3.9263248794549,332.035178455526));
#58447=CARTESIAN_POINT('Ctrl Pts',(92.0293471349068,3.84638750719902,331.932198944152));
#58448=CARTESIAN_POINT('Ctrl Pts',(92.0219353307297,3.76262638391469,331.832694243119));
#58449=CARTESIAN_POINT('Ctrl Pts',(92.0141602519513,3.67475987846731,331.728312520281));
#58450=CARTESIAN_POINT('Ctrl Pts',(92.0063851731728,3.5824076432408,331.627424976491));
#58451=CARTESIAN_POINT('Ctrl Pts',(91.9986100943944,3.48587814983359,331.530441442054));
#58452=CARTESIAN_POINT('Ctrl Pts',(91.9908445833453,3.38946744211318,331.433577252032));
#58453=CARTESIAN_POINT('Ctrl Pts',(91.9830790722963,3.2888899772032,331.340607786907));
#58454=CARTESIAN_POINT('Ctrl Pts',(91.9753135612472,3.18449479231876,331.251910355902));
#58455=CARTESIAN_POINT('Ctrl Pts',(91.967555749725,3.08020311556399,331.163300868658));
#58456=CARTESIAN_POINT('Ctrl Pts',(91.9597979382028,2.97210154771474,331.078955237638));
#58457=CARTESIAN_POINT('Ctrl Pts',(91.9520401266806,2.86057607357491,330.999214128475));
#58458=CARTESIAN_POINT('Ctrl Pts',(91.9442881531576,2.74913452589151,330.919533027026));
#58459=CARTESIAN_POINT('Ctrl Pts',(91.9365361796346,2.6342745171893,330.844449776851));
#58460=CARTESIAN_POINT('Ctrl Pts',(91.9287842061116,2.5164149395517,330.774264689489));
#58461=CARTESIAN_POINT('Ctrl Pts',(91.921035515554,2.39860527551512,330.704109325553));
#58462=CARTESIAN_POINT('Ctrl Pts',(91.9132868249963,2.27779890425685,330.638848198219));
#58463=CARTESIAN_POINT('Ctrl Pts',(91.9055381344387,2.15444333190666,330.578738076962));
#58464=CARTESIAN_POINT('Ctrl Pts',(91.8977910560608,2.03111342471351,330.518640462118));
#58465=CARTESIAN_POINT('Ctrl Pts',(91.890043977683,1.90523572255281,330.463691892759));
#58466=CARTESIAN_POINT('Ctrl Pts',(91.8822968993051,1.77728158743122,330.414102789914));
#58467=CARTESIAN_POINT('Ctrl Pts',(91.8745497559993,1.64932637993065,330.364513271464));
#58468=CARTESIAN_POINT('Ctrl Pts',(91.8668026126935,1.51929506921937,330.320283450369));
#58469=CARTESIAN_POINT('Ctrl Pts',(91.8590554693877,1.38767783831432,330.281575127275));
#58470=CARTESIAN_POINT('Ctrl Pts',(91.8513065843596,1.25603101706171,330.242858101728));
#58471=CARTESIAN_POINT('Ctrl Pts',(91.8435576993315,1.12279794104366,330.209665154594));
#58472=CARTESIAN_POINT('Ctrl Pts',(91.8358088143034,0.988482362058231,330.182107755211));
#58473=CARTESIAN_POINT('Ctrl Pts',(91.8280517045287,0.85402421912962,330.154521106119));
#58474=CARTESIAN_POINT('Ctrl Pts',(91.820294594754,0.718481661541847,330.132582032324));
#58475=CARTESIAN_POINT('Ctrl Pts',(91.8125374849792,0.582367557341854,330.116350638031));
#58476=CARTESIAN_POINT('Ctrl Pts',(91.8047762300531,0.446180718116847,330.1001105702));
#58477=CARTESIAN_POINT('Ctrl Pts',(91.7970149751269,0.309422113234143,330.089584289255));
#58478=CARTESIAN_POINT('Ctrl Pts',(91.7892537202008,0.172607089793971,330.084779775529));
#58479=CARTESIAN_POINT('Ctrl Pts',(91.7814800497961,0.035573206903927,330.079967576146));
#58480=CARTESIAN_POINT('Ctrl Pts',(91.7737063793914,-0.101516883821502,
330.080895431666));
#58481=CARTESIAN_POINT('Ctrl Pts',(91.7659327089868,-0.238149586347875,
330.087519176931));
#58482=CARTESIAN_POINT('Ctrl Pts',(91.7585209048098,-0.368422003698419,
330.09383458526));
#58483=CARTESIAN_POINT('Ctrl Pts',(91.7511091006327,-0.498278370715269,
330.105327504411));
#58484=CARTESIAN_POINT('Ctrl Pts',(91.7436972964557,-0.627281946672058,
330.121916316638));
#58485=CARTESIAN_POINT('Ctrl Pts',(91.7359222176773,-0.762608372169753,
330.139318195969));
#58486=CARTESIAN_POINT('Ctrl Pts',(91.7281471388988,-0.897423953735751,
330.162383121948));
#58487=CARTESIAN_POINT('Ctrl Pts',(91.7203720601204,-1.03121712463991,330.191073476923));
#58488=CARTESIAN_POINT('Ctrl Pts',(91.7126065490714,-1.16484565452921,330.21972852659));
#58489=CARTESIAN_POINT('Ctrl Pts',(91.7048410380224,-1.297453898565,330.253995150393));
#58490=CARTESIAN_POINT('Ctrl Pts',(91.6970755269734,-1.42853568530859,330.293784019161));
#58491=CARTESIAN_POINT('Ctrl Pts',(91.6893177154513,-1.55948750407908,330.333533437151));
#58492=CARTESIAN_POINT('Ctrl Pts',(91.6815599039291,-1.68891550586809,330.378794091105));
#58493=CARTESIAN_POINT('Ctrl Pts',(91.6738020924069,-1.81632433915199,330.429425751888));
#58494=CARTESIAN_POINT('Ctrl Pts',(91.6660501188839,-1.94363729324847,330.480019310741));
#58495=CARTESIAN_POINT('Ctrl Pts',(91.6582981453609,-2.06893374152666,330.535975687544));
#58496=CARTESIAN_POINT('Ctrl Pts',(91.6505461718379,-2.19173445906332,330.597105142812));
#58497=CARTESIAN_POINT('Ctrl Pts',(91.6427974812803,-2.31448317042335,330.658208709719));
#58498=CARTESIAN_POINT('Ctrl Pts',(91.6350487907227,-2.43473790403931,330.724480823918));
#58499=CARTESIAN_POINT('Ctrl Pts',(91.627300100165,-2.55204056573768,330.795684120653));
#58500=CARTESIAN_POINT('Ctrl Pts',(91.6195530217872,-2.66931882163763,330.866872602947));
#58501=CARTESIAN_POINT('Ctrl Pts',(91.6118059434094,-2.78364589338849,330.942990024348));
#58502=CARTESIAN_POINT('Ctrl Pts',(91.6040588650315,-2.89458975242904,331.023753877382));
#58503=CARTESIAN_POINT('Ctrl Pts',(91.5963117217258,-3.00553454128576,331.104518407295));
#58504=CARTESIAN_POINT('Ctrl Pts',(91.58856457842,-3.11309574486761,331.189929216467));
#58505=CARTESIAN_POINT('Ctrl Pts',(91.5808174351142,-3.21687203540074,331.279661659156));
#58506=CARTESIAN_POINT('Ctrl Pts',(91.5730685500861,-3.32067165704671,331.369414275602));
#58507=CARTESIAN_POINT('Ctrl Pts',(91.5653196650581,-3.42068437677736,331.463490203323));
#58508=CARTESIAN_POINT('Ctrl Pts',(91.55757078003,-3.51654384864533,331.561526149139));
#58509=CARTESIAN_POINT('Ctrl Pts',(91.5498136702553,-3.61250506674748,331.659666151321));
#58510=CARTESIAN_POINT('Ctrl Pts',(91.5420565604806,-3.70430395729192,331.761774287976));
#58511=CARTESIAN_POINT('Ctrl Pts',(91.5342994507059,-3.79161243504285,331.867451803255));
#58512=CARTESIAN_POINT('Ctrl Pts',(91.5265381957797,-3.87896756765288,331.97318578922));
#58513=CARTESIAN_POINT('Ctrl Pts',(91.5187769408536,-3.96182727017782,332.082492643066));
#58514=CARTESIAN_POINT('Ctrl Pts',(91.5110156859274,-4.03990594789826,332.194943317037));
#58515=CARTESIAN_POINT('Ctrl Pts',(91.5032420155228,-4.11810952605717,332.307573875439));
#58516=CARTESIAN_POINT('Ctrl Pts',(91.4954683451181,-4.1915165868746,332.423357973281));
#58517=CARTESIAN_POINT('Ctrl Pts',(91.4876946747134,-4.25988633349031,332.541839816399));
#58518=CARTESIAN_POINT('Ctrl Pts',(91.4802828705363,-4.32507345195294,332.654806301216));
#58519=CARTESIAN_POINT('Ctrl Pts',(91.4728710663591,-4.38568154239888,332.770224768623));
#58520=CARTESIAN_POINT('Ctrl Pts',(91.465459262182,-4.44154289346483,332.88768378598));
#58521=CARTESIAN_POINT('Ctrl Pts',(91.4570490574045,-4.50492899897717,333.020965017556));
#58522=CARTESIAN_POINT('Ctrl Pts',(91.448638852627,-4.56237957711634,333.157243344602));
#58523=CARTESIAN_POINT('Ctrl Pts',(91.4402286478496,-4.61362440268593,333.295989162757));
#58524=CARTESIAN_POINT('Ctrl Pts',(91.4318462779367,-4.66469962563346,333.434275780315));
#58525=CARTESIAN_POINT('Ctrl Pts',(91.4234639080239,-4.70960995933787,333.575013330719));
#58526=CARTESIAN_POINT('Ctrl Pts',(91.4150815381111,-4.74813305682816,333.717652333743));
#58527=CARTESIAN_POINT('Ctrl Pts',(91.4067160565243,-4.78657854015439,333.860003955748));
#58528=CARTESIAN_POINT('Ctrl Pts',(91.3983505749376,-4.81866236243912,334.004249117229));
#58529=CARTESIAN_POINT('Ctrl Pts',(91.3899850933509,-4.84421074358203,334.149820410581));
#58530=CARTESIAN_POINT('Ctrl Pts',(91.3816465856593,-4.86967674580334,334.294922319745));
#58531=CARTESIAN_POINT('Ctrl Pts',(91.3733080779676,-4.88864928004082,334.441341549971));
#58532=CARTESIAN_POINT('Ctrl Pts',(91.3649695702759,-4.90100499951194,334.588499019128));
#58533=CARTESIAN_POINT('Ctrl Pts',(91.3572521723641,-4.91244037945907,334.72469518122));
#58534=CARTESIAN_POINT('Ctrl Pts',(91.3495347744523,-4.91820839646373,334.861523354464));
#58535=CARTESIAN_POINT('Ctrl Pts',(91.3418173765404,-4.91824977563263,334.998514405971));
#58536=CARTESIAN_POINT('',(89.5918173764638,-4.91824796037091,335.004479152525));
#58537=CARTESIAN_POINT('Ctrl Pts',(91.3418173765086,-4.9182497756328,334.998514406535));
#58538=CARTESIAN_POINT('Ctrl Pts',(91.333865556607,-4.91829241171009,335.139666668237));
#58539=CARTESIAN_POINT('Ctrl Pts',(91.3259137367055,-4.9122541569799,335.280763706402));
#58540=CARTESIAN_POINT('Ctrl Pts',(91.317961916804,-4.90017551578669,335.421263548132));
#58541=CARTESIAN_POINT('Ctrl Pts',(91.310004976711,-4.88808909713424,335.561853857967));
#58542=CARTESIAN_POINT('Ctrl Pts',(91.302048036618,-4.86995457012187,335.701845845342));
#58543=CARTESIAN_POINT('Ctrl Pts',(91.294091096525,-4.84586413341891,335.840704384992));
#58544=CARTESIAN_POINT('Ctrl Pts',(91.2861277333872,-4.82175425030143,335.979675014794));
#58545=CARTESIAN_POINT('Ctrl Pts',(91.2781643702494,-4.7916789355462,336.117510017953));
#58546=CARTESIAN_POINT('Ctrl Pts',(91.2702010071115,-4.75578111746013,336.25368617497));
#58547=CARTESIAN_POINT('Ctrl Pts',(91.2622241741035,-4.71982257892921,336.390092671245));
#58548=CARTESIAN_POINT('Ctrl Pts',(91.2542473410954,-4.67802195195456,336.524834365975));
#58549=CARTESIAN_POINT('Ctrl Pts',(91.2462705080873,-4.63057185807171,336.657403792));
#58550=CARTESIAN_POINT('Ctrl Pts',(91.238286142611,-4.58307695739393,336.790098402415));
#58551=CARTESIAN_POINT('Ctrl Pts',(91.2303017771348,-4.52992208698784,336.920616320105));
#58552=CARTESIAN_POINT('Ctrl Pts',(91.2223174116586,-4.47134716387251,337.04847201656));
#58553=CARTESIAN_POINT('Ctrl Pts',(91.214318496306,-4.41266549991637,337.176560703923));
#58554=CARTESIAN_POINT('Ctrl Pts',(91.2063195809536,-4.34854421160031,337.301977155514));
#58555=CARTESIAN_POINT('Ctrl Pts',(91.198320665601,-4.27926864095019,337.42426132277));
#58556=CARTESIAN_POINT('Ctrl Pts',(91.1946208530367,-4.247225968238,337.480822553699));
#58557=CARTESIAN_POINT('Ctrl Pts',(91.1909210404723,-4.21408117395572,337.536714077698));
#58558=CARTESIAN_POINT('Ctrl Pts',(91.187221227908,-4.17986548399099,337.591892667191));
#58559=CARTESIAN_POINT('Ctrl Pts',(91.1794461491296,-4.10796192663283,337.707849319788));
#58560=CARTESIAN_POINT('Ctrl Pts',(91.1716710703512,-4.03111583639892,337.820994846696));
#58561=CARTESIAN_POINT('Ctrl Pts',(91.1638959915727,-3.94957339143528,337.930879234661));
#58562=CARTESIAN_POINT('Ctrl Pts',(91.1561304805237,-3.86813128964135,338.040628402891));
#58563=CARTESIAN_POINT('Ctrl Pts',(91.1483649694746,-3.78200456269868,338.147124106088));
#58564=CARTESIAN_POINT('Ctrl Pts',(91.1405994584256,-3.69148421830019,338.249942665424));
#58565=CARTESIAN_POINT('Ctrl Pts',(91.1328416469034,-3.60105362508691,338.352659279858));
#58566=CARTESIAN_POINT('Ctrl Pts',(91.1250838353813,-3.50623834029327,338.451705714488));
#58567=CARTESIAN_POINT('Ctrl Pts',(91.1173260238591,-3.40737121512308,338.546689225863));
#58568=CARTESIAN_POINT('Ctrl Pts',(91.1095740503361,-3.30857849060003,338.641601259133));
#58569=CARTESIAN_POINT('Ctrl Pts',(91.1018220768131,-3.20574027559687,338.732456185201));
#58570=CARTESIAN_POINT('Ctrl Pts',(91.0940701032901,-3.0992278015355,338.818896450113));
#58571=CARTESIAN_POINT('Ctrl Pts',(91.0863214127324,-2.99276043556985,338.905300107523));
#58572=CARTESIAN_POINT('Ctrl Pts',(91.0785727221748,-2.88262220829389,338.987292576506));
#58573=CARTESIAN_POINT('Ctrl Pts',(91.0708240316172,-2.76921894245547,339.064555266108));
#58574=CARTESIAN_POINT('Ctrl Pts',(91.0630769532394,-2.65583927111367,339.141801880562));
#58575=CARTESIAN_POINT('Ctrl Pts',(91.0553298748615,-2.53919623524676,339.214320453077));
#58576=CARTESIAN_POINT('Ctrl Pts',(91.0475827964837,-2.41972594495273,339.281834818606));
#58577=CARTESIAN_POINT('Ctrl Pts',(91.0398356531779,-2.30025465338267,339.349349749969));
#58578=CARTESIAN_POINT('Ctrl Pts',(91.0320885098721,-2.17795640041949,339.411860198388));
#58579=CARTESIAN_POINT('Ctrl Pts',(91.0243413665663,-2.05329292869422,339.469135398651));
#58580=CARTESIAN_POINT('Ctrl Pts',(91.0165924815383,-1.92860142997425,339.526423475595));
#58581=CARTESIAN_POINT('Ctrl Pts',(91.0088435965102,-1.80154400947818,339.578473799142));
#58582=CARTESIAN_POINT('Ctrl Pts',(91.0010947114821,-1.67260309159753,339.62510345403));
#58583=CARTESIAN_POINT('Ctrl Pts',(90.9933376017074,-1.543525314494,339.671782602115));
#58584=CARTESIAN_POINT('Ctrl Pts',(90.9855804919326,-1.41256041464631,339.713029455138));
#58585=CARTESIAN_POINT('Ctrl Pts',(90.9778233821579,-1.28020724118315,339.74871061259));
#58586=CARTESIAN_POINT('Ctrl Pts',(90.9700621272317,-1.14778334241584,339.784410836911));
#58587=CARTESIAN_POINT('Ctrl Pts',(90.9623008723055,-1.01397007296683,339.814539353627));
#58588=CARTESIAN_POINT('Ctrl Pts',(90.9545396173794,-0.879276248177881,
339.839013984469));
#58589=CARTESIAN_POINT('Ctrl Pts',(90.9467659469747,-0.744366957165977,
339.863527766745));
#58590=CARTESIAN_POINT('Ctrl Pts',(90.9389922765701,-0.608574683379752,
339.88236953606));
#58591=CARTESIAN_POINT('Ctrl Pts',(90.9312186061654,-0.472414025544393,
339.89550896751));
#58592=CARTESIAN_POINT('Ctrl Pts',(90.9238068019883,-0.342591679088524,
339.908036755264));
#58593=CARTESIAN_POINT('Ctrl Pts',(90.9163949978111,-0.212434760655099,
339.915381129299));
#58594=CARTESIAN_POINT('Ctrl Pts',(90.908983193634,-0.0823872145721554,
339.917559903995));
#58595=CARTESIAN_POINT('Ctrl Pts',(90.9012081148555,0.0540343491349865,
339.919845466928));
#58596=CARTESIAN_POINT('Ctrl Pts',(90.8934330360771,0.190766665418773,339.91645348711));
#58597=CARTESIAN_POINT('Ctrl Pts',(90.8856579572987,0.327298087413861,339.907347453001));
#58598=CARTESIAN_POINT('Ctrl Pts',(90.8778924462496,0.463661498802075,339.898252624447));
#58599=CARTESIAN_POINT('Ctrl Pts',(90.8701269352007,0.599824121505498,339.88345775805));
#58600=CARTESIAN_POINT('Ctrl Pts',(90.8623614241516,0.735272193998754,339.862978291462));
#58601=CARTESIAN_POINT('Ctrl Pts',(90.8546036126294,0.870585969333695,339.842519130326));
#58602=CARTESIAN_POINT('Ctrl Pts',(90.8468458011073,1.00518622037897,339.816386643609));
#58603=CARTESIAN_POINT('Ctrl Pts',(90.8390879895851,1.13856255590235,339.784648196973));
#58604=CARTESIAN_POINT('Ctrl Pts',(90.8313360160621,1.27183852150355,339.752933634525));
#58605=CARTESIAN_POINT('Ctrl Pts',(90.823584042539,1.4038920261332,339.715621599322));
#58606=CARTESIAN_POINT('Ctrl Pts',(90.815832069016,1.53422150041965,339.672830774825));
#58607=CARTESIAN_POINT('Ctrl Pts',(90.8080833784584,1.66449578009646,339.630058072268));
#58608=CARTESIAN_POINT('Ctrl Pts',(90.8003346879008,1.79304711100607,339.581811316949));
#58609=CARTESIAN_POINT('Ctrl Pts',(90.7925859973432,1.91938796924289,339.528259366029));
#58610=CARTESIAN_POINT('Ctrl Pts',(90.7848389189654,2.04570254120884,339.474718557039));
#58611=CARTESIAN_POINT('Ctrl Pts',(90.7770918405876,2.16980719563602,339.415874900411));
#58612=CARTESIAN_POINT('Ctrl Pts',(90.7693447622098,2.29123369524647,339.351945681677));
#58613=CARTESIAN_POINT('Ctrl Pts',(90.761597618904,2.41266121252795,339.288015927154));
#58614=CARTESIAN_POINT('Ctrl Pts',(90.7538504755982,2.53141018435577,339.219000707607));
#58615=CARTESIAN_POINT('Ctrl Pts',(90.7461033322924,2.64703667990872,339.145163431967));
#58616=CARTESIAN_POINT('Ctrl Pts',(90.7383544472643,2.76268917075269,339.07130955614));
#58617=CARTESIAN_POINT('Ctrl Pts',(90.7306055622362,2.87521745905286,338.992631677312));
#58618=CARTESIAN_POINT('Ctrl Pts',(90.7228566772081,2.98420665994171,338.909436490501));
#58619=CARTESIAN_POINT('Ctrl Pts',(90.7150995674334,3.09331154309453,338.826152999459));
#58620=CARTESIAN_POINT('Ctrl Pts',(90.7073424576587,3.19886952383646,338.738342860078));
#58621=CARTESIAN_POINT('Ctrl Pts',(90.6995853478839,3.30049846694625,338.646353374563));
#58622=CARTESIAN_POINT('Ctrl Pts',(90.6918240929578,3.40218171731364,338.554314732808));
#58623=CARTESIAN_POINT('Ctrl Pts',(90.6840628380316,3.49993146808569,338.458092568916));
#58624=CARTESIAN_POINT('Ctrl Pts',(90.6763015831054,3.59340326462794,338.358070285188));
#58625=CARTESIAN_POINT('Ctrl Pts',(90.6685279127008,3.68702458558233,338.257887998402));
#58626=CARTESIAN_POINT('Ctrl Pts',(90.6607542422962,3.7763540224756,338.153893740891));
#58627=CARTESIAN_POINT('Ctrl Pts',(90.6529805718915,3.86108759555049,338.046503839155));
#58628=CARTESIAN_POINT('Ctrl Pts',(90.6455687677144,3.9418768004133,337.944112963181));
#58629=CARTESIAN_POINT('Ctrl Pts',(90.6381569635373,4.01848821819065,337.838635695905));
#58630=CARTESIAN_POINT('Ctrl Pts',(90.6307451593602,4.09069658562617,337.730454999967));
#58631=CARTESIAN_POINT('Ctrl Pts',(90.6229700805817,4.16644410024723,337.616972045869));
#58632=CARTESIAN_POINT('Ctrl Pts',(90.6151950018033,4.23758541409293,337.500155329138));
#58633=CARTESIAN_POINT('Ctrl Pts',(90.6074199230248,4.30381294235502,337.380415346052));
#58634=CARTESIAN_POINT('Ctrl Pts',(90.5996544119758,4.36995897342737,337.260822710637));
#58635=CARTESIAN_POINT('Ctrl Pts',(90.5918889009268,4.43120306279379,337.138314305167));
#58636=CARTESIAN_POINT('Ctrl Pts',(90.5841233898777,4.48728016646518,337.013330516867));
#58637=CARTESIAN_POINT('Ctrl Pts',(90.5763655783556,4.54330166952482,336.888470650358));
#58638=CARTESIAN_POINT('Ctrl Pts',(90.5686077668334,4.5941662231338,336.761140639639));
#58639=CARTESIAN_POINT('Ctrl Pts',(90.5608499553112,4.63965427453192,336.631806139012));
#58640=CARTESIAN_POINT('Ctrl Pts',(90.5530979817882,4.68510809472885,336.502568966698));
#58641=CARTESIAN_POINT('Ctrl Pts',(90.5453460082652,4.72519333689264,336.371330674205));
#58642=CARTESIAN_POINT('Ctrl Pts',(90.5375940347422,4.75973837651114,336.238577268348));
#58643=CARTESIAN_POINT('Ctrl Pts',(90.5298453441846,4.79426878628487,336.105880083637));
#58644=CARTESIAN_POINT('Ctrl Pts',(90.5220966536269,4.82326356186689,335.971669439251));
#58645=CARTESIAN_POINT('Ctrl Pts',(90.5143479630693,4.84660087168616,335.836446682743));
#58646=CARTESIAN_POINT('Ctrl Pts',(90.5066008846915,4.8699333259832,335.701252060458));
#58647=CARTESIAN_POINT('Ctrl Pts',(90.4988538063137,4.88761058938459,335.565046129844));
#58648=CARTESIAN_POINT('Ctrl Pts',(90.4911067279359,4.89956199187121,335.428340227286));
#58649=CARTESIAN_POINT('Ctrl Pts',(90.4833595846301,4.91151349452211,335.291633179));
#58650=CARTESIAN_POINT('Ctrl Pts',(90.4756124413242,4.91773900650009,335.154426539802));
#58651=CARTESIAN_POINT('Ctrl Pts',(90.4678652980184,4.91821979755603,335.017236166278));
#58652=CARTESIAN_POINT('Ctrl Pts',(90.4601164129903,4.918700696704,334.880014949445));
#58653=CARTESIAN_POINT('Ctrl Pts',(90.4523675279622,4.91343430354956,334.742810396358));
#58654=CARTESIAN_POINT('Ctrl Pts',(90.4446186429342,4.90245400646844,334.606137362826));
#58655=CARTESIAN_POINT('Ctrl Pts',(90.4368615331594,4.89146205478653,334.469319263124));
#58656=CARTESIAN_POINT('Ctrl Pts',(90.4291044233847,4.87474411552898,334.333034200173));
#58657=CARTESIAN_POINT('Ctrl Pts',(90.42134731361,4.8523854472342,334.197791464786));
#58658=CARTESIAN_POINT('Ctrl Pts',(90.4135860586838,4.83001483118199,334.062476460006));
#58659=CARTESIAN_POINT('Ctrl Pts',(90.4058248037576,4.80199755977768,333.928205275074));
#58660=CARTESIAN_POINT('Ctrl Pts',(90.3980635488315,4.76846964002803,333.795475050225));
#58661=CARTESIAN_POINT('Ctrl Pts',(90.3902898784268,4.73488808653347,333.662532500273));
#58662=CARTESIAN_POINT('Ctrl Pts',(90.3825162080221,4.69577838079714,333.531136211101));
#58663=CARTESIAN_POINT('Ctrl Pts',(90.3747425376175,4.6513261197662,333.40176710393));
#58664=CARTESIAN_POINT('Ctrl Pts',(90.3673307334404,4.6089431221809,333.278420159822));
#58665=CARTESIAN_POINT('Ctrl Pts',(90.3599189292633,4.56170387199145,333.156916182574));
#58666=CARTESIAN_POINT('Ctrl Pts',(90.3525071250863,4.50980850777866,333.037651843921));
#58667=CARTESIAN_POINT('Ctrl Pts',(90.3447320463078,4.45536959717738,332.91254200476));
#58668=CARTESIAN_POINT('Ctrl Pts',(90.3369569675294,4.39563457491288,332.789501527849));
#58669=CARTESIAN_POINT('Ctrl Pts',(90.3291818887509,4.33078218427259,332.669011210905));
#58670=CARTESIAN_POINT('Ctrl Pts',(90.3214163777019,4.26600959862779,332.548669164966));
#58671=CARTESIAN_POINT('Ctrl Pts',(90.3136508666529,4.19613235780692,332.430871375902));
#58672=CARTESIAN_POINT('Ctrl Pts',(90.3058853556039,4.12137736231394,332.316079043655));
#58673=CARTESIAN_POINT('Ctrl Pts',(90.2981275440818,4.04669648661663,332.20140052834));
#58674=CARTESIAN_POINT('Ctrl Pts',(90.2903697325596,3.96714769270209,332.089721865068));
#58675=CARTESIAN_POINT('Ctrl Pts',(90.2826119210374,3.88300374660957,331.981479672701));
#58676=CARTESIAN_POINT('Ctrl Pts',(90.2748599475143,3.79892312150439,331.873318936016));
#58677=CARTESIAN_POINT('Ctrl Pts',(90.2671079739912,3.71025446612536,331.768589830178));
#58678=CARTESIAN_POINT('Ctrl Pts',(90.2593560004682,3.61731359810144,331.667699684079));
#58679=CARTESIAN_POINT('Ctrl Pts',(90.2516073099106,3.52441209059057,331.566852265016));
#58680=CARTESIAN_POINT('Ctrl Pts',(90.243858619353,3.42724223325535,331.46984085897));
#58681=CARTESIAN_POINT('Ctrl Pts',(90.2361099287953,3.32615968989382,331.377039224636));
#58682=CARTESIAN_POINT('Ctrl Pts',(90.2283628504175,3.2250981775999,331.284256898458));
#58683=CARTESIAN_POINT('Ctrl Pts',(90.2206157720397,3.1201258862679,331.195682865985));
#58684=CARTESIAN_POINT('Ctrl Pts',(90.2128686936619,3.01163456597101,331.111653268605));
#58685=CARTESIAN_POINT('Ctrl Pts',(90.2051215503561,2.90314233641259,331.027622966976));
#58686=CARTESIAN_POINT('Ctrl Pts',(90.1973744070502,2.79113132808707,330.948137415753));
#58687=CARTESIAN_POINT('Ctrl Pts',(90.1896272637445,2.67602519979056,330.873491525201));
#58688=CARTESIAN_POINT('Ctrl Pts',(90.1818783787163,2.5608931931924,330.798828852668));
#58689=CARTESIAN_POINT('Ctrl Pts',(90.1741294936882,2.44266500984922,330.729008218554));
#58690=CARTESIAN_POINT('Ctrl Pts',(90.1663806086601,2.3217916713604,330.664280163883));
#58691=CARTESIAN_POINT('Ctrl Pts',(90.1586234988854,2.20079003666118,330.599483406185));
#58692=CARTESIAN_POINT('Ctrl Pts',(90.1508663891107,2.07713798350429,330.53979021037));
#58693=CARTESIAN_POINT('Ctrl Pts',(90.1431092793359,1.95130992368549,330.485404487196));
#58694=CARTESIAN_POINT('Ctrl Pts',(90.1353480244098,1.82541462537499,330.430989702031));
#58695=CARTESIAN_POINT('Ctrl Pts',(90.1275867694836,1.69734136822776,330.381888180631));
#58696=CARTESIAN_POINT('Ctrl Pts',(90.1198255145574,1.56758180926913,330.338254582911));
#58697=CARTESIAN_POINT('Ctrl Pts',(90.1120518441528,1.43761467730453,330.294551185655));
#58698=CARTESIAN_POINT('Ctrl Pts',(90.1042781737481,1.30595622863437,330.256333299989));
#58699=CARTESIAN_POINT('Ctrl Pts',(90.0965045033434,1.17311131733125,330.223705107549));
#58700=CARTESIAN_POINT('Ctrl Pts',(90.0890926991663,1.04645036860984,330.192595765318));
#58701=CARTESIAN_POINT('Ctrl Pts',(90.0816808949892,0.918711213102214,330.166567484621));
#58702=CARTESIAN_POINT('Ctrl Pts',(90.0742690908122,0.790335727004762,330.145666626495));
#58703=CARTESIAN_POINT('Ctrl Pts',(90.0664940120337,0.655668175922929,330.123741355053));
#58704=CARTESIAN_POINT('Ctrl Pts',(90.0587189332553,0.519874765792876,330.107389547548));
#58705=CARTESIAN_POINT('Ctrl Pts',(90.0509438544768,0.383456537921072,330.096721082171));
#58706=CARTESIAN_POINT('Ctrl Pts',(90.0431783434278,0.247206181363659,330.08606574502));
#58707=CARTESIAN_POINT('Ctrl Pts',(90.0354128323788,0.110332922870522,330.081079864693));
#58708=CARTESIAN_POINT('Ctrl Pts',(90.0276473213298,-0.0266526158047855,
330.08182221747));
#58709=CARTESIAN_POINT('Ctrl Pts',(90.0198895098076,-0.163502332919209,
330.082563834202));
#58710=CARTESIAN_POINT('Ctrl Pts',(90.0121316982855,-0.300463720319841,
330.089022379287));
#58711=CARTESIAN_POINT('Ctrl Pts',(90.0043738867633,-0.437022006536157,
330.101204757463));
#58712=CARTESIAN_POINT('Ctrl Pts',(89.9966219132403,-0.573477528311397,
330.113377968013));
#58713=CARTESIAN_POINT('Ctrl Pts',(89.9888699397173,-0.709530164938046,
330.131266403461));
#58714=CARTESIAN_POINT('Ctrl Pts',(89.9811179661944,-0.844666477822673,
330.154824915058));
#58715=CARTESIAN_POINT('Ctrl Pts',(89.9733692756367,-0.97974556039939,330.178373449612));
#58716=CARTESIAN_POINT('Ctrl Pts',(89.9656205850791,-1.1139087068,330.207587217348));
#58717=CARTESIAN_POINT('Ctrl Pts',(89.9578718945215,-1.24664914527527,330.242369395268));
#58718=CARTESIAN_POINT('Ctrl Pts',(89.9501248161437,-1.37936196599346,330.277144336465));
#58719=CARTESIAN_POINT('Ctrl Pts',(89.9423777377659,-1.5106522896919,330.317485284384));
#58720=CARTESIAN_POINT('Ctrl Pts',(89.934630659388,-1.64002544946506,330.363244713422));
#58721=CARTESIAN_POINT('Ctrl Pts',(89.9268835160823,-1.76939969350948,330.409004525969));
#58722=CARTESIAN_POINT('Ctrl Pts',(89.9191363727764,-1.89685637307775,330.460182779873));
#58723=CARTESIAN_POINT('Ctrl Pts',(89.9113892294706,-2.02191822575249,330.516582804281));
#58724=CARTESIAN_POINT('Ctrl Pts',(89.9036403444425,-2.14700819498795,330.572995508612));
#58725=CARTESIAN_POINT('Ctrl Pts',(89.8958914594144,-2.26970190971158,330.634632158847));
#58726=CARTESIAN_POINT('Ctrl Pts',(89.8881425743862,-2.38954461096502,330.701249063425));
#58727=CARTESIAN_POINT('Ctrl Pts',(89.8803854646115,-2.50951451449913,330.767936675872));
#58728=CARTESIAN_POINT('Ctrl Pts',(89.8726283548368,-2.62662701747445,330.839614911923));
#58729=CARTESIAN_POINT('Ctrl Pts',(89.864871245062,-2.7404539155405,330.915995176386));
#58730=CARTESIAN_POINT('Ctrl Pts',(89.8571099901359,-2.8543416390614,330.992416256021));
#58731=CARTESIAN_POINT('Ctrl Pts',(89.8493487352097,-2.9649399442258,331.073544139606));
#58732=CARTESIAN_POINT('Ctrl Pts',(89.8415874802835,-3.0718527103851,331.159049077611));
#58733=CARTESIAN_POINT('Ctrl Pts',(89.8338138098789,-3.17893650212739,331.244690795651));
#58734=CARTESIAN_POINT('Ctrl Pts',(89.8260401394742,-3.28232267866212,331.334723303072));
#58735=CARTESIAN_POINT('Ctrl Pts',(89.8182664690696,-3.38165042592205,331.428778435974));
#58736=CARTESIAN_POINT('Ctrl Pts',(89.8108546648924,-3.47635444265063,331.518455279812));
#58737=CARTESIAN_POINT('Ctrl Pts',(89.8034428607153,-3.56736916589403,331.611788464687));
#58738=CARTESIAN_POINT('Ctrl Pts',(89.7960310565382,-3.65441648510363,331.708431496094));
#58739=CARTESIAN_POINT('Ctrl Pts',(89.7883327731203,-3.74482833598726,331.808809950295));
#58740=CARTESIAN_POINT('Ctrl Pts',(89.7806344897024,-3.83125922718602,331.91309179026));
#58741=CARTESIAN_POINT('Ctrl Pts',(89.7729362062846,-3.91334805919744,332.020924635046));
#58742=CARTESIAN_POINT('Ctrl Pts',(89.7652500608121,-3.99530746108672,332.128587458917));
#58743=CARTESIAN_POINT('Ctrl Pts',(89.7575639153397,-4.07293819487718,332.239789825614));
#58744=CARTESIAN_POINT('Ctrl Pts',(89.7498777698673,-4.14591691548458,332.354143618335));
#58745=CARTESIAN_POINT('Ctrl Pts',(89.742198603955,-4.21882936628581,332.468393569776));
#58746=CARTESIAN_POINT('Ctrl Pts',(89.7345194380427,-4.28709799008229,332.585788923023));
#58747=CARTESIAN_POINT('Ctrl Pts',(89.7268402721304,-4.35044045679348,332.705909571443));
#58748=CARTESIAN_POINT('Ctrl Pts',(89.7191663354651,-4.41373978947113,332.825948421848));
#58749=CARTESIAN_POINT('Ctrl Pts',(89.7114923987997,-4.47211945116495,332.948708524726));
#58750=CARTESIAN_POINT('Ctrl Pts',(89.7038184621344,-4.52534138480801,333.07374238134));
#58751=CARTESIAN_POINT('Ctrl Pts',(89.6961480088085,-4.57853916004745,333.198719482814));
#58752=CARTESIAN_POINT('Ctrl Pts',(89.6884775554825,-4.62658370907463,333.325967917878));
#58753=CARTESIAN_POINT('Ctrl Pts',(89.6808071021566,-4.66928397564227,333.455017729128));
#58754=CARTESIAN_POINT('Ctrl Pts',(89.6731365065765,-4.71198503411787,333.584069933701));
#58755=CARTESIAN_POINT('Ctrl Pts',(89.6654659109963,-4.74934147416188,333.714923206294));
#58756=CARTESIAN_POINT('Ctrl Pts',(89.6577953154162,-4.78121130484941,333.84708997711));
#58757=CARTESIAN_POINT('Ctrl Pts',(89.6501249457811,-4.81308019677933,333.979252854822));
#58758=CARTESIAN_POINT('Ctrl Pts',(89.642454576146,-4.83946271293504,334.112728763981));
#58759=CARTESIAN_POINT('Ctrl Pts',(89.6347842065108,-4.86026765416642,334.247018331987));
#58760=CARTESIAN_POINT('Ctrl Pts',(89.6271087563662,-4.88108637565981,334.381396847393));
#58761=CARTESIAN_POINT('Ctrl Pts',(89.6194333062215,-4.89632008458264,334.516589702478));
#58762=CARTESIAN_POINT('Ctrl Pts',(89.6117578560768,-4.90592927962572,334.652090578151));
#58763=CARTESIAN_POINT('Ctrl Pts',(89.6051110295541,-4.91425070068513,334.769432336263));
#58764=CARTESIAN_POINT('Ctrl Pts',(89.5984642030313,-4.91835494669348,334.88700484173));
#58765=CARTESIAN_POINT('Ctrl Pts',(89.5918173765086,-4.91824796037164,335.004479151733));
#58766=CARTESIAN_POINT('',(87.8418168890551,-4.92245083146177,334.999291596085));
#58767=CARTESIAN_POINT('Ctrl Pts',(89.5918173764638,-4.91824796037091,335.004479152525));
#58768=CARTESIAN_POINT('Ctrl Pts',(89.5820887354747,-4.91809136959837,335.176420662286));
#58769=CARTESIAN_POINT('Ctrl Pts',(89.5723600944857,-4.90891462743897,335.347960022259));
#58770=CARTESIAN_POINT('Ctrl Pts',(89.5626314534967,-4.89086547025376,335.518283719964));
#58771=CARTESIAN_POINT('Ctrl Pts',(89.5527221300621,-4.8724811001787,335.691770706587));
#58772=CARTESIAN_POINT('Ctrl Pts',(89.5428128066276,-4.844891715429,335.863996613599));
#58773=CARTESIAN_POINT('Ctrl Pts',(89.532903483193,-4.80830183373595,336.034125977912));
#58774=CARTESIAN_POINT('Ctrl Pts',(89.5278666628834,-4.78970352473403,336.120601209352));
#58775=CARTESIAN_POINT('Ctrl Pts',(89.5228298425739,-4.76878061185351,336.206535146784));
#58776=CARTESIAN_POINT('Ctrl Pts',(89.5177930222643,-4.74556462793198,336.291820198255));
#58777=CARTESIAN_POINT('Ctrl Pts',(89.5100179434858,-4.70972731533896,336.423470317391));
#58778=CARTESIAN_POINT('Ctrl Pts',(89.5022428647075,-4.66835092106235,336.553836056142));
#58779=CARTESIAN_POINT('Ctrl Pts',(89.494467785929,-4.62154302049518,336.68241587374));
#58780=CARTESIAN_POINT('Ctrl Pts',(89.48670227488,-4.57479272002955,336.810837465687));
#58781=CARTESIAN_POINT('Ctrl Pts',(89.478936763831,-4.52262434457786,336.937477145472));
#58782=CARTESIAN_POINT('Ctrl Pts',(89.4711712527819,-4.4651959486605,337.06184582415));
#58783=CARTESIAN_POINT('Ctrl Pts',(89.4634134412598,-4.40782449316502,337.186091190921));
#58784=CARTESIAN_POINT('Ctrl Pts',(89.4556556297376,-4.34520355880484,337.308069685023));
#58785=CARTESIAN_POINT('Ctrl Pts',(89.4478978182154,-4.277540129763,337.427309930925));
#58786=CARTESIAN_POINT('Ctrl Pts',(89.4401458446924,-4.20992761959716,337.546460444761));
#58787=CARTESIAN_POINT('Ctrl Pts',(89.4323938711694,-4.13728035992132,337.662876473372));
#58788=CARTESIAN_POINT('Ctrl Pts',(89.4246418976464,-4.05985215875158,337.776109419958));
#58789=CARTESIAN_POINT('Ctrl Pts',(89.4168932070887,-3.98245674847101,337.889294412324));
#58790=CARTESIAN_POINT('Ctrl Pts',(89.4091445165311,-3.90028464391505,337.999298681833));
#58791=CARTESIAN_POINT('Ctrl Pts',(89.4013958259735,-3.81363392192876,338.105701107965));
#58792=CARTESIAN_POINT('Ctrl Pts',(89.3936487475957,-3.72700122834885,338.212081396183));
#58793=CARTESIAN_POINT('Ctrl Pts',(89.3859016692178,-3.63589201745043,338.314861028724));
#58794=CARTESIAN_POINT('Ctrl Pts',(89.37815459084,-3.54064549762043,338.413650908145));
#58795=CARTESIAN_POINT('Ctrl Pts',(89.3704074475342,-3.44539817953299,338.51244161552));
#58796=CARTESIAN_POINT('Ctrl Pts',(89.3626603042284,-3.34601375465022,338.607242221689));
#58797=CARTESIAN_POINT('Ctrl Pts',(89.3549131609226,-3.2428689498613,338.697699830506));
#58798=CARTESIAN_POINT('Ctrl Pts',(89.3471642758945,-3.13970095593051,338.788177776114));
#58799=CARTESIAN_POINT('Ctrl Pts',(89.3394153908663,-3.03277119363023,338.874310523771));
#58800=CARTESIAN_POINT('Ctrl Pts',(89.3316665058383,-2.92248986222626,338.955785139221));
#58801=CARTESIAN_POINT('Ctrl Pts',(89.3239093960635,-2.81209147707757,339.03734623267));
#58802=CARTESIAN_POINT('Ctrl Pts',(89.3161522862888,-2.69833473148445,339.114239084799));
#58803=CARTESIAN_POINT('Ctrl Pts',(89.3083951765141,-2.58165969186645,339.186193533258));
#58804=CARTESIAN_POINT('Ctrl Pts',(89.3006339215879,-2.46492230483782,339.258186431874));
#58805=CARTESIAN_POINT('Ctrl Pts',(89.2928726666617,-2.34526385727184,339.325235477551));
#58806=CARTESIAN_POINT('Ctrl Pts',(89.2851114117355,-2.22314857966914,339.387116758785));
#58807=CARTESIAN_POINT('Ctrl Pts',(89.2773377413308,-2.10083795741956,339.449097029903));
#58808=CARTESIAN_POINT('Ctrl Pts',(89.2695640709262,-1.97606300751493,339.505892855166));
#58809=CARTESIAN_POINT('Ctrl Pts',(89.2617904005215,-1.849308295548,339.557328372031));
#58810=CARTESIAN_POINT('Ctrl Pts',(89.2543785963445,-1.72845404591932,339.606369553211));
#58811=CARTESIAN_POINT('Ctrl Pts',(89.2469667921674,-1.60580047293763,339.650538142507));
#58812=CARTESIAN_POINT('Ctrl Pts',(89.2395549879904,-1.48177815612713,339.689724571713));
#58813=CARTESIAN_POINT('Ctrl Pts',(89.2317799092119,-1.35167713612559,339.730831644544));
#58814=CARTESIAN_POINT('Ctrl Pts',(89.2240048304335,-1.21965866405884,339.766585733493));
#58815=CARTESIAN_POINT('Ctrl Pts',(89.2162297516551,-1.08620271147651,339.796805888514));
#58816=CARTESIAN_POINT('Ctrl Pts',(89.2084642406061,-0.952910984940047,
339.82698885571));
#58817=CARTESIAN_POINT('Ctrl Pts',(89.200698729557,-0.818185675092528,339.851651353144));
#58818=CARTESIAN_POINT('Ctrl Pts',(89.192933218508,-0.682523599630967,339.870661618143));
#58819=CARTESIAN_POINT('Ctrl Pts',(89.1851754069858,-0.546996033512196,
339.889653034408));
#58820=CARTESIAN_POINT('Ctrl Pts',(89.1774175954637,-0.410533934754198,
339.903003317028));
#58821=CARTESIAN_POINT('Ctrl Pts',(89.1696597839415,-0.273645704114665,
339.910631435072));
#58822=CARTESIAN_POINT('Ctrl Pts',(89.1619078104184,-0.136860486209756,
339.918253812716));
#58823=CARTESIAN_POINT('Ctrl Pts',(89.1541558368954,0.000349836585899654,
339.920162575225));
#58824=CARTESIAN_POINT('Ctrl Pts',(89.1464038633724,0.137470679571206,339.916328393706));
#58825=CARTESIAN_POINT('Ctrl Pts',(89.1386551728148,0.274533451798099,339.912495835965));
#58826=CARTESIAN_POINT('Ctrl Pts',(89.1309064822572,0.411506429676223,339.902925182454));
#58827=CARTESIAN_POINT('Ctrl Pts',(89.1231577916996,0.547874177490426,339.887639199873));
#58828=CARTESIAN_POINT('Ctrl Pts',(89.1154107133217,0.68421355285573,339.872356397669));
#58829=CARTESIAN_POINT('Ctrl Pts',(89.1076636349439,0.819947560429564,339.851360675157));
#58830=CARTESIAN_POINT('Ctrl Pts',(89.0999165565661,0.954565434748096,339.824726716953));
#58831=CARTESIAN_POINT('Ctrl Pts',(89.0921694132603,1.08918443729398,339.798092535532));
#58832=CARTESIAN_POINT('Ctrl Pts',(89.0844222699545,1.22268690448518,339.76582010003));
#58833=CARTESIAN_POINT('Ctrl Pts',(89.0766751266487,1.35457220988645,339.728035235772));
#58834=CARTESIAN_POINT('Ctrl Pts',(89.0689262416206,1.48648716590429,339.690241876675));
#58835=CARTESIAN_POINT('Ctrl Pts',(89.0611773565925,1.61678386098025,339.646933730364));
#58836=CARTESIAN_POINT('Ctrl Pts',(89.0534284715644,1.74497715966093,339.59828639547));
#58837=CARTESIAN_POINT('Ctrl Pts',(89.0456713617896,1.87330652403341,339.549587425792));
#58838=CARTESIAN_POINT('Ctrl Pts',(89.037914252015,1.99952766622661,339.495538085927));
#58839=CARTESIAN_POINT('Ctrl Pts',(89.0301571422402,2.12317525576623,339.436362236766));
#58840=CARTESIAN_POINT('Ctrl Pts',(89.0223958873141,2.24688891862431,339.377154765923));
#58841=CARTESIAN_POINT('Ctrl Pts',(89.0146346323879,2.36802594354105,339.312815510453));
#58842=CARTESIAN_POINT('Ctrl Pts',(89.0068733774617,2.48614681679418,339.243613680325));
#58843=CARTESIAN_POINT('Ctrl Pts',(88.9990997070571,2.60445664494892,339.174301149822));
#58844=CARTESIAN_POINT('Ctrl Pts',(88.9913260366524,2.71974035107673,339.100110712484));
#58845=CARTESIAN_POINT('Ctrl Pts',(88.9835523662477,2.83158782236641,339.021354680543));
#58846=CARTESIAN_POINT('Ctrl Pts',(88.9761405620707,2.93822876695884,338.946264760837));
#58847=CARTESIAN_POINT('Ctrl Pts',(88.9687287578935,3.04174596219514,338.867024912678));
#58848=CARTESIAN_POINT('Ctrl Pts',(88.9613169537164,3.14181425854564,338.783937925931));
#58849=CARTESIAN_POINT('Ctrl Pts',(88.953541874938,3.2467872001882,338.696778598461));
#58850=CARTESIAN_POINT('Ctrl Pts',(88.9457667961596,3.34829634681888,338.605110037908));
#58851=CARTESIAN_POINT('Ctrl Pts',(88.9379917173812,3.4459297935382,338.509237940138));
#58852=CARTESIAN_POINT('Ctrl Pts',(88.9302262063322,3.54344309608568,338.413483819088));
#58853=CARTESIAN_POINT('Ctrl Pts',(88.9224606952831,3.63708991202431,338.313536724294));
#58854=CARTESIAN_POINT('Ctrl Pts',(88.9146951842341,3.72649058274801,338.209743136014));
#58855=CARTESIAN_POINT('Ctrl Pts',(88.9069373727119,3.8158026124464,338.106052459379));
#58856=CARTESIAN_POINT('Ctrl Pts',(88.8991795611897,3.9008766217492,337.998523173208));
#58857=CARTESIAN_POINT('Ctrl Pts',(88.8914217496675,3.98136934519541,337.887538952056));
#58858=CARTESIAN_POINT('Ctrl Pts',(88.8836697761445,4.0618014953146,337.77663825005));
#58859=CARTESIAN_POINT('Ctrl Pts',(88.8759178026215,4.1376589932216,337.662288103275));
#58860=CARTESIAN_POINT('Ctrl Pts',(88.8681658290985,4.20863870431525,337.544905365439));
#58861=CARTESIAN_POINT('Ctrl Pts',(88.8604171385409,4.27958835545911,337.427572339262));
#58862=CARTESIAN_POINT('Ctrl Pts',(88.8526684479833,4.34566412657855,337.307209610195));
#58863=CARTESIAN_POINT('Ctrl Pts',(88.8449197574257,4.40660623083631,337.184262939496));
#58864=CARTESIAN_POINT('Ctrl Pts',(88.8371726790478,4.46753565558028,337.061341848878));
#58865=CARTESIAN_POINT('Ctrl Pts',(88.82942560067,4.52333336450984,336.935838235966));
#58866=CARTESIAN_POINT('Ctrl Pts',(88.8216785222922,4.57378575701152,336.808222030465));
#58867=CARTESIAN_POINT('Ctrl Pts',(88.8139313789864,4.62423857235285,336.680604755417));
#58868=CARTESIAN_POINT('Ctrl Pts',(88.8061842356805,4.66934583820442,336.550875215964));
#58869=CARTESIAN_POINT('Ctrl Pts',(88.7984370923747,4.70894244607535,336.419522490857));
#58870=CARTESIAN_POINT('Ctrl Pts',(88.7906882073466,4.74854795610436,336.28814023487));
#58871=CARTESIAN_POINT('Ctrl Pts',(88.7829393223186,4.78264023006099,336.155134441232));
#58872=CARTESIAN_POINT('Ctrl Pts',(88.7751904372905,4.81110439794924,336.021008097193));
#58873=CARTESIAN_POINT('Ctrl Pts',(88.7674333275158,4.8395987779994,335.886739390066));
#58874=CARTESIAN_POINT('Ctrl Pts',(88.759676217741,4.86245303762319,335.751348139634));
#58875=CARTESIAN_POINT('Ctrl Pts',(88.7519191079663,4.87960360919957,335.615346796194));
#58876=CARTESIAN_POINT('Ctrl Pts',(88.7441578530401,4.89676334549302,335.479272777985));
#58877=CARTESIAN_POINT('Ctrl Pts',(88.736396598114,4.9082132879741,335.342588406467));
#58878=CARTESIAN_POINT('Ctrl Pts',(88.7286353431878,4.91394197495463,335.205808963068));
#58879=CARTESIAN_POINT('Ctrl Pts',(88.7208616727831,4.91967982596735,335.068810717135));
#58880=CARTESIAN_POINT('Ctrl Pts',(88.7130880023785,4.91967813278979,334.931717486493));
#58881=CARTESIAN_POINT('Ctrl Pts',(88.7053143319738,4.91397758986589,334.795043153821));
#58882=CARTESIAN_POINT('Ctrl Pts',(88.6979025277968,4.90854240858656,334.664731044216));
#58883=CARTESIAN_POINT('Ctrl Pts',(88.6904907236196,4.89792702391962,334.53479999768));
#58884=CARTESIAN_POINT('Ctrl Pts',(88.6830789194426,4.8822101012541,334.405687296356));
#58885=CARTESIAN_POINT('Ctrl Pts',(88.6753038406641,4.86572284539043,334.270246396934));
#58886=CARTESIAN_POINT('Ctrl Pts',(88.6675287618857,4.84356922099467,334.135278071874));
#58887=CARTESIAN_POINT('Ctrl Pts',(88.6597536831073,4.815783388864,334.001294130366));
#58888=CARTESIAN_POINT('Ctrl Pts',(88.6519881720583,4.78803174896869,333.867475064628));
#58889=CARTESIAN_POINT('Ctrl Pts',(88.6442226610092,4.75466177023629,333.734638351282));
#58890=CARTESIAN_POINT('Ctrl Pts',(88.6364571499602,4.71575936025072,333.603290753697));
#58891=CARTESIAN_POINT('Ctrl Pts',(88.628699338438,4.67689552211791,333.472073387638));
#58892=CARTESIAN_POINT('Ctrl Pts',(88.6209415269157,4.63251027931863,333.342342571464));
#58893=CARTESIAN_POINT('Ctrl Pts',(88.6131837153935,4.58274051133555,333.214594592743));
#58894=CARTESIAN_POINT('Ctrl Pts',(88.6054317418705,4.53300819668123,333.086942748426));
#58895=CARTESIAN_POINT('Ctrl Pts',(88.5976797683475,4.47789956352514,332.961271134258));
#58896=CARTESIAN_POINT('Ctrl Pts',(88.5899277948245,4.4176011095153,332.83806024605));
#58897=CARTESIAN_POINT('Ctrl Pts',(88.5821791042669,4.35732819193649,332.714901537726));
#58898=CARTESIAN_POINT('Ctrl Pts',(88.5744304137093,4.29186999641765,332.594201833017));
#58899=CARTESIAN_POINT('Ctrl Pts',(88.5666817231517,4.22146078754553,332.47642081921));
#58900=CARTESIAN_POINT('Ctrl Pts',(88.5589346447738,4.15106622789738,332.358664310727));
#58901=CARTESIAN_POINT('Ctrl Pts',(88.551187566396,4.07572290427074,332.243825620553));
#58902=CARTESIAN_POINT('Ctrl Pts',(88.5434404880181,3.99571039903277,332.132338675931));
#58903=CARTESIAN_POINT('Ctrl Pts',(88.5356933447123,3.91569722321299,332.020850796941));
#58904=CARTESIAN_POINT('Ctrl Pts',(88.5279462014065,3.83101501563496,331.912715037087));
#58905=CARTESIAN_POINT('Ctrl Pts',(88.5201990581007,3.74198570337721,331.808334908199));
#58906=CARTESIAN_POINT('Ctrl Pts',(88.5124501730726,3.65293637543993,331.703931312442));
#58907=CARTESIAN_POINT('Ctrl Pts',(88.5047012880445,3.55953825166814,331.603285325137));
#58908=CARTESIAN_POINT('Ctrl Pts',(88.4969524030164,3.46215214202312,331.506765738175));
#58909=CARTESIAN_POINT('Ctrl Pts',(88.4891952932417,3.36466266575506,331.410143704327));
#58910=CARTESIAN_POINT('Ctrl Pts',(88.4814381834669,3.26317702608077,331.317657095478));
#58911=CARTESIAN_POINT('Ctrl Pts',(88.4736810736922,3.15809175330003,331.229636683257));
#58912=CARTESIAN_POINT('Ctrl Pts',(88.465919818766,3.0529503263095,331.141569235743));
#58913=CARTESIAN_POINT('Ctrl Pts',(88.4581585638398,2.94420574314074,331.05797297846));
#58914=CARTESIAN_POINT('Ctrl Pts',(88.4503973089137,2.83228511236174,330.979136398136));
#58915=CARTESIAN_POINT('Ctrl Pts',(88.442623638509,2.72018544504841,330.900173704976));
#58916=CARTESIAN_POINT('Ctrl Pts',(88.4348499681043,2.60489990636934,330.825986115296));
#58917=CARTESIAN_POINT('Ctrl Pts',(88.4270762976996,2.48688265333304,330.756817499677));
#58918=CARTESIAN_POINT('Ctrl Pts',(88.4196644935225,2.37435913181912,330.690868699755));
#58919=CARTESIAN_POINT('Ctrl Pts',(88.4122526893455,2.25935274907523,330.629482258468));
#58920=CARTESIAN_POINT('Ctrl Pts',(88.4048408851684,2.1422737953427,330.572828662872));
#58921=CARTESIAN_POINT('Ctrl Pts',(88.39706580639,2.01945645332735,330.513398305793));
#58922=CARTESIAN_POINT('Ctrl Pts',(88.3892907276116,1.89397011202614,330.458988656004));
#58923=CARTESIAN_POINT('Ctrl Pts',(88.3815156488331,1.76626364907357,330.409847956281));
#58924=CARTESIAN_POINT('Ctrl Pts',(88.3737501377841,1.63871433705385,330.360767727317));
#58925=CARTESIAN_POINT('Ctrl Pts',(88.3659846267351,1.50895070059308,330.31694368659));
#58926=CARTESIAN_POINT('Ctrl Pts',(88.3582191156861,1.3774453773434,330.278577831317));
#58927=CARTESIAN_POINT('Ctrl Pts',(88.3504613041639,1.24607044200467,330.240250015901));
#58928=CARTESIAN_POINT('Ctrl Pts',(88.3427034926417,1.11295762929524,330.207369724904));
#58929=CARTESIAN_POINT('Ctrl Pts',(88.3349456811195,0.978598351360524,330.180090423129));
#58930=CARTESIAN_POINT('Ctrl Pts',(88.3271937075965,0.844340183043319,330.152831649893));
#58931=CARTESIAN_POINT('Ctrl Pts',(88.3194417340735,0.708837798069523,330.131165553743));
#58932=CARTESIAN_POINT('Ctrl Pts',(88.3116897605505,0.572596180197431,330.115195328683));
#58933=CARTESIAN_POINT('Ctrl Pts',(88.3039410699929,0.436412260731209,330.099231867022));
#58934=CARTESIAN_POINT('Ctrl Pts',(88.2961923794353,0.299490118440352,330.088959524157));
#58935=CARTESIAN_POINT('Ctrl Pts',(88.2884436888777,0.162343088182089,330.084430065168));
#58936=CARTESIAN_POINT('Ctrl Pts',(88.2806966104998,0.0252245925090398,
330.079901548571));
#58937=CARTESIAN_POINT('Ctrl Pts',(88.272949532122,-0.112118307647133,330.081113552093));
#58938=CARTESIAN_POINT('Ctrl Pts',(88.2652024537442,-0.24916941555038,330.088065791885));
#58939=CARTESIAN_POINT('Ctrl Pts',(88.2574553104384,-0.386221672073916,
330.095018089943));
#58940=CARTESIAN_POINT('Ctrl Pts',(88.2497081671326,-0.522981741094443,
330.107710700426));
#58941=CARTESIAN_POINT('Ctrl Pts',(88.2419610238268,-0.658936087692332,
330.126091271388));
#58942=CARTESIAN_POINT('Ctrl Pts',(88.2342121387987,-0.794920999713729,
330.144475974694));
#58943=CARTESIAN_POINT('Ctrl Pts',(88.2264632537706,-0.930099441582536,
330.168551130739));
#58944=CARTESIAN_POINT('Ctrl Pts',(88.2187143687425,-1.06396603335614,330.198212901183));
#58945=CARTESIAN_POINT('Ctrl Pts',(88.2109572589678,-1.19797471251335,330.227906154937));
#58946=CARTESIAN_POINT('Ctrl Pts',(88.203200149193,-1.33066837788202,330.263197783512));
#58947=CARTESIAN_POINT('Ctrl Pts',(88.1954430394183,-1.46155429124487,330.303933335626));
#58948=CARTESIAN_POINT('Ctrl Pts',(88.1876817844921,-1.59251014585482,330.344690655517));
#58949=CARTESIAN_POINT('Ctrl Pts',(88.1799205295659,-1.72165595576657,330.3908975639));
#58950=CARTESIAN_POINT('Ctrl Pts',(88.1721592746398,-1.84851799338471,330.442351012788));
#58951=CARTESIAN_POINT('Ctrl Pts',(88.1643856042351,-1.97558296891889,330.493886770426));
#58952=CARTESIAN_POINT('Ctrl Pts',(88.1566119338305,-2.1003565158653,330.550685677752));
#58953=CARTESIAN_POINT('Ctrl Pts',(88.1488382634258,-2.22238778783423,330.612497796811));
#58954=CARTESIAN_POINT('Ctrl Pts',(88.1414264592487,-2.33873847473389,330.671432546857));
#58955=CARTESIAN_POINT('Ctrl Pts',(88.1340146550717,-2.45259619560212,330.734924141927));
#58956=CARTESIAN_POINT('Ctrl Pts',(88.1266028508946,-2.56359555264389,330.802719820531));
#58957=CARTESIAN_POINT('Ctrl Pts',(88.1188277721161,-2.68003531882461,330.873838367296));
#58958=CARTESIAN_POINT('Ctrl Pts',(88.1110526933377,-2.79369741379469,330.949918325304));
#58959=CARTESIAN_POINT('Ctrl Pts',(88.1032776145592,-2.90413017146207,331.030716562186));
#58960=CARTESIAN_POINT('Ctrl Pts',(88.0955121035102,-3.0144270345905,331.111415371694));
#58961=CARTESIAN_POINT('Ctrl Pts',(88.0877465924612,-3.12150215490779,331.196820678919));
#58962=CARTESIAN_POINT('Ctrl Pts',(88.0799810814122,-3.2249298972908,331.286644345062));
#58963=CARTESIAN_POINT('Ctrl Pts',(88.07222326989,-3.32825509076612,331.376378950779));
#58964=CARTESIAN_POINT('Ctrl Pts',(88.0644654583678,-3.42793980990432,331.470522942695));
#58965=CARTESIAN_POINT('Ctrl Pts',(88.0567076468456,-3.52358907156986,331.568746130463));
#58966=CARTESIAN_POINT('Ctrl Pts',(88.0489556733226,-3.61916635413291,331.666895402168));
#58967=CARTESIAN_POINT('Ctrl Pts',(88.0412036997996,-3.71071395224622,331.769117480682));
#58968=CARTESIAN_POINT('Ctrl Pts',(88.0334517262765,-3.79787181218263,331.875043558587));
#58969=CARTESIAN_POINT('Ctrl Pts',(88.0257030357189,-3.8849927607135,331.980924776735));
#58970=CARTESIAN_POINT('Ctrl Pts',(88.0179543451613,-3.96772742076359,332.090506573142));
#58971=CARTESIAN_POINT('Ctrl Pts',(88.0102056546037,-4.04575446702686,332.203385286631));
#58972=CARTESIAN_POINT('Ctrl Pts',(88.0024585762258,-4.12376527911147,332.316240514761));
#58973=CARTESIAN_POINT('Ctrl Pts',(87.994711497848,-4.19707020350187,332.432390974235));
#58974=CARTESIAN_POINT('Ctrl Pts',(87.9869644194701,-4.26539013521873,332.551402430599));
#58975=CARTESIAN_POINT('Ctrl Pts',(87.9792172761643,-4.33371063952243,332.670414884393));
#58976=CARTESIAN_POINT('Ctrl Pts',(87.9714701328585,-4.39704587322069,332.792288043915));
#58977=CARTESIAN_POINT('Ctrl Pts',(87.9637229895527,-4.45516195696875,332.916561736053));
#58978=CARTESIAN_POINT('Ctrl Pts',(87.9559741045245,-4.5132911064464,333.040863367556));
#58979=CARTESIAN_POINT('Ctrl Pts',(87.9482252194964,-4.56619860553989,333.167566251597));
#58980=CARTESIAN_POINT('Ctrl Pts',(87.9404763344683,-4.61369828403918,333.296189210518));
#58981=CARTESIAN_POINT('Ctrl Pts',(87.9327192246935,-4.66124837918786,333.424948691176));
#58982=CARTESIAN_POINT('Ctrl Pts',(87.9249621149188,-4.7033790520974,333.555631950535));
#58983=CARTESIAN_POINT('Ctrl Pts',(87.9172050051441,-4.73995353522223,333.687741052065));
#58984=CARTESIAN_POINT('Ctrl Pts',(87.9094437502179,-4.77654756258143,333.819920748475));
#58985=CARTESIAN_POINT('Ctrl Pts',(87.9016824952917,-4.80757939566933,333.953527424713));
#58986=CARTESIAN_POINT('Ctrl Pts',(87.8939212403656,-4.83296342068516,334.088052832222));
#58987=CARTESIAN_POINT('Ctrl Pts',(87.8861475699609,-4.85838805186836,334.22279343654));
#58988=CARTESIAN_POINT('Ctrl Pts',(87.8783738995562,-4.87814676470385,334.358455321969));
#58989=CARTESIAN_POINT('Ctrl Pts',(87.8706002291515,-4.89220575849805,334.494524106392));
#58990=CARTESIAN_POINT('Ctrl Pts',(87.8631884249746,-4.90561030274846,334.624258856162));
#58991=CARTESIAN_POINT('Ctrl Pts',(87.8557766207976,-4.91383381183715,334.754363187925));
#58992=CARTESIAN_POINT('Ctrl Pts',(87.8483648166207,-4.91689110057861,334.884393047134));
#58993=CARTESIAN_POINT('Ctrl Pts',(87.8461823365833,-4.91779134989543,334.922681642625));
#58994=CARTESIAN_POINT('Ctrl Pts',(87.8439998565459,-4.91824436888267,334.960980794805));
#58995=CARTESIAN_POINT('Ctrl Pts',(87.8418173765086,-4.91824994782974,334.999283639204));
#58996=CARTESIAN_POINT('',(86.0918183737958,-4.91614223044281,334.995887905754));
#58997=CARTESIAN_POINT('Ctrl Pts',(87.8418164509476,-4.92622645040437,334.999298747474));
#58998=CARTESIAN_POINT('Ctrl Pts',(87.7512532280806,-4.92298212659158,336.591274825728));
#58999=CARTESIAN_POINT('Ctrl Pts',(87.5679439937889,-3.21788844791034,339.819547858999));
#59000=CARTESIAN_POINT('Ctrl Pts',(87.2918887480729,2.28441556428547,340.348447849244));
#59001=CARTESIAN_POINT('Ctrl Pts',(87.0136507137988,5.73385224213235,335.973338241222));
#59002=CARTESIAN_POINT('Ctrl Pts',(86.735412679525,3.92141734889474,330.70501049568));
#59003=CARTESIAN_POINT('Ctrl Pts',(86.4571746452509,-1.48964436539838,329.378131224311));
#59004=CARTESIAN_POINT('Ctrl Pts',(86.2426434753134,-4.60773713649915,332.332910879143));
#59005=CARTESIAN_POINT('Ctrl Pts',(86.1208583168005,-4.9184828895762,334.482243502733));
#59006=CARTESIAN_POINT('Ctrl Pts',(86.0918191697123,-4.91446141997587,334.995875227902));
#59007=CARTESIAN_POINT('',(84.3418173764577,-4.91824930023121,335.002623599657));
#59008=CARTESIAN_POINT('Ctrl Pts',(86.0918173765086,-4.91824829421748,334.995903791165));
#59009=CARTESIAN_POINT('Ctrl Pts',(86.0838540931834,-4.91836569290393,335.136862397669));
#59010=CARTESIAN_POINT('Ctrl Pts',(86.0758908098582,-4.91241836281413,335.277914761862));
#59011=CARTESIAN_POINT('Ctrl Pts',(86.0679275265329,-4.90041250066869,335.418497772742));
#59012=CARTESIAN_POINT('Ctrl Pts',(86.0602115756372,-4.88877952982098,335.554714401539));
#59013=CARTESIAN_POINT('Ctrl Pts',(86.0524956247415,-4.87145882520636,335.690489980585));
#59014=CARTESIAN_POINT('Ctrl Pts',(86.0447796738458,-4.84850889564337,335.825314819549));
#59015=CARTESIAN_POINT('Ctrl Pts',(86.0370640114249,-4.82555982410478,335.960134617844));
#59016=CARTESIAN_POINT('Ctrl Pts',(86.0293483490039,-4.79698201203871,336.094003358224));
#59017=CARTESIAN_POINT('Ctrl Pts',(86.0216326865829,-4.76288540529612,336.226419862248));
#59018=CARTESIAN_POINT('Ctrl Pts',(86.0139156105548,-4.72878255162301,336.358860626654));
#59019=CARTESIAN_POINT('Ctrl Pts',(86.0061985345267,-4.68915898980021,336.489848243718));
#59020=CARTESIAN_POINT('Ctrl Pts',(85.9984814584986,-4.6441748975198,336.618895482651));
#59021=CARTESIAN_POINT('Ctrl Pts',(85.9907612661606,-4.59917263976184,336.747994833443));
#59022=CARTESIAN_POINT('Ctrl Pts',(85.9830410738225,-4.54880567413809,336.875151875321));
#59023=CARTESIAN_POINT('Ctrl Pts',(85.9753208814845,-4.49328261641219,336.999898595316));
#59024=CARTESIAN_POINT('Ctrl Pts',(85.9675916533351,-4.4376945737923,337.124791320462));
#59025=CARTESIAN_POINT('Ctrl Pts',(85.9598624251856,-4.37693855331885,337.247267732583));
#59026=CARTESIAN_POINT('Ctrl Pts',(85.9521331970362,-4.31126967778069,337.366883357487));
#59027=CARTESIAN_POINT('Ctrl Pts',(85.9443985497762,-4.24555476053018,337.486582847208));
#59028=CARTESIAN_POINT('Ctrl Pts',(85.9366639025161,-4.17492033197678,337.603417219478));
#59029=CARTESIAN_POINT('Ctrl Pts',(85.9289292552561,-4.0996646559619,337.716971249601));
#59030=CARTESIAN_POINT('Ctrl Pts',(85.9211835131052,-4.02430103016177,337.830688166216));
#59031=CARTESIAN_POINT('Ctrl Pts',(85.9134377709543,-3.9443031574284,337.94111503249));
#59032=CARTESIAN_POINT('Ctrl Pts',(85.9056920288034,-3.86000952431726,338.047869671538));
#59033=CARTESIAN_POINT('Ctrl Pts',(85.9040275447699,-3.8418956491454,338.070810196633));
#59034=CARTESIAN_POINT('Ctrl Pts',(85.9023630607365,-3.82358353923497,338.093581283071));
#59035=CARTESIAN_POINT('Ctrl Pts',(85.900698576703,-3.80507676839332,338.116179367292));
#59036=CARTESIAN_POINT('Ctrl Pts',(85.8929234979246,-3.71862859686583,338.221738736756));
#59037=CARTESIAN_POINT('Ctrl Pts',(85.8851484191462,-3.62764789475629,338.323864853333));
#59038=CARTESIAN_POINT('Ctrl Pts',(85.8773733403678,-3.53243756824137,338.422143756328));
#59039=CARTESIAN_POINT('Ctrl Pts',(85.8696078293188,-3.43734440409467,338.520301720877));
#59040=CARTESIAN_POINT('Ctrl Pts',(85.8618423182698,-3.33803224101858,338.614621613574));
#59041=CARTESIAN_POINT('Ctrl Pts',(85.8540768072208,-3.23484498649983,338.704721443755));
#59042=CARTESIAN_POINT('Ctrl Pts',(85.8463189956986,-3.13176004244429,338.794731939692));
#59043=CARTESIAN_POINT('Ctrl Pts',(85.8385611841764,-3.02480794560392,338.880530444486));
#59044=CARTESIAN_POINT('Ctrl Pts',(85.8308033726542,-2.91437004277748,338.961771108515));
#59045=CARTESIAN_POINT('Ctrl Pts',(85.8230513991312,-2.80401524797518,339.042950636367));
#59046=CARTESIAN_POINT('Ctrl Pts',(85.8152994256082,-2.69018018208852,339.119578919857));
#59047=CARTESIAN_POINT('Ctrl Pts',(85.8075474520852,-2.57327964142081,339.191350015156));
#59048=CARTESIAN_POINT('Ctrl Pts',(85.7997987615276,-2.4564286082014,339.263090715354));
#59049=CARTESIAN_POINT('Ctrl Pts',(85.79205007097,-2.3365150147009,339.32997811455));
#59050=CARTESIAN_POINT('Ctrl Pts',(85.7843013804124,-2.21398285695901,339.391749420401));
#59051=CARTESIAN_POINT('Ctrl Pts',(85.7765543020345,-2.09147619305594,339.453507874215));
#59052=CARTESIAN_POINT('Ctrl Pts',(85.7688072236567,-1.9663523973973,339.510152176098));
#59053=CARTESIAN_POINT('Ctrl Pts',(85.7610601452789,-1.83907994594124,339.561465555601));
#59054=CARTESIAN_POINT('Ctrl Pts',(85.7533130019731,-1.71180642781954,339.61277936516));
#59055=CARTESIAN_POINT('Ctrl Pts',(85.7455658586673,-1.58238458050164,339.658762017064));
#59056=CARTESIAN_POINT('Ctrl Pts',(85.7378187153615,-1.45130235615365,339.699245102516));
#59057=CARTESIAN_POINT('Ctrl Pts',(85.7300698303334,-1.32019066173875,339.739737289425));
#59058=CARTESIAN_POINT('Ctrl Pts',(85.7223209453053,-1.1874182208884,339.774727334228));
#59059=CARTESIAN_POINT('Ctrl Pts',(85.7145720602772,-1.05348723334344,339.804096971511));
#59060=CARTESIAN_POINT('Ctrl Pts',(85.7068149505025,-0.919414090064437,
339.833497782031));
#59061=CARTESIAN_POINT('Ctrl Pts',(85.6990578407278,-0.784180326067946,
339.857266184412));
#59062=CARTESIAN_POINT('Ctrl Pts',(85.691300730953,-0.648297950511844,339.875335150517));
#59063=CARTESIAN_POINT('Ctrl Pts',(85.6835394760269,-0.512342963759013,
339.893413772099));
#59064=CARTESIAN_POINT('Ctrl Pts',(85.6757782211007,-0.375739063903513,
339.905786853538));
#59065=CARTESIAN_POINT('Ctrl Pts',(85.6680169661746,-0.239001443181835,
339.912439452315));
#59066=CARTESIAN_POINT('Ctrl Pts',(85.6602432957699,-0.102045086829596,
339.919102693081));
#59067=CARTESIAN_POINT('Ctrl Pts',(85.6524696253652,0.0350450267729754,
339.920027162323));
#59068=CARTESIAN_POINT('Ctrl Pts',(85.6446959549606,0.171754751751551,339.915250081913));
#59069=CARTESIAN_POINT('Ctrl Pts',(85.6372841507834,0.30210060614284,339.910695375746));
#59070=CARTESIAN_POINT('Ctrl Pts',(85.6298723466063,0.432100402124639,339.900958010051));
#59071=CARTESIAN_POINT('Ctrl Pts',(85.6224605424292,0.561316336089136,339.886113694271));
#59072=CARTESIAN_POINT('Ctrl Pts',(85.6146854636507,0.696865527890769,339.870541814355));
#59073=CARTESIAN_POINT('Ctrl Pts',(85.6069103848723,0.831980436468299,339.849300502638));
#59074=CARTESIAN_POINT('Ctrl Pts',(85.5991353060939,0.966149033530582,339.822420461501));
#59075=CARTESIAN_POINT('Ctrl Pts',(85.5913697950449,1.10015252759268,339.795573497967));
#59076=CARTESIAN_POINT('Ctrl Pts',(85.5836042839959,1.23321164755928,339.763101687317));
#59077=CARTESIAN_POINT('Ctrl Pts',(85.5758387729468,1.36481906125792,339.725087511626));
#59078=CARTESIAN_POINT('Ctrl Pts',(85.5680809614246,1.49629598582279,339.687111027102));
#59079=CARTESIAN_POINT('Ctrl Pts',(85.5603231499024,1.62632369544553,339.643603221207));
#59080=CARTESIAN_POINT('Ctrl Pts',(85.5525653383802,1.75440498916578,339.594697617525));
#59081=CARTESIAN_POINT('Ctrl Pts',(85.5448133648572,1.8823898976501,339.545828816861));
#59082=CARTESIAN_POINT('Ctrl Pts',(85.5370613913343,2.0084309420348,339.491570442518));
#59083=CARTESIAN_POINT('Ctrl Pts',(85.5293094178113,2.13204637754787,339.432105741799));
#59084=CARTESIAN_POINT('Ctrl Pts',(85.5215607272537,2.25560946185111,339.372666224415));
#59085=CARTESIAN_POINT('Ctrl Pts',(85.513812036696,2.37674862889893,339.308024935099));
#59086=CARTESIAN_POINT('Ctrl Pts',(85.5060633461384,2.49500261926964,339.238413027577));
#59087=CARTESIAN_POINT('Ctrl Pts',(85.4983162677606,2.61323200591006,339.168815603395));
#59088=CARTESIAN_POINT('Ctrl Pts',(85.4905691893828,2.72857707324962,339.094249816224));
#59089=CARTESIAN_POINT('Ctrl Pts',(85.4828221110049,2.84060201517121,339.014992310566));
#59090=CARTESIAN_POINT('Ctrl Pts',(85.4750749676991,2.95262789596941,338.935734140654));
#59091=CARTESIAN_POINT('Ctrl Pts',(85.4673278243933,3.06133327676036,338.85178439958));
#59092=CARTESIAN_POINT('Ctrl Pts',(85.4595806810875,3.16631248007696,338.763462281066));
#59093=CARTESIAN_POINT('Ctrl Pts',(85.4518317960594,3.27131528494751,338.675120305865));
#59094=CARTESIAN_POINT('Ctrl Pts',(85.4440829110313,3.37258994632697,338.582404248749));
#59095=CARTESIAN_POINT('Ctrl Pts',(85.4363340260032,3.4697652432116,338.485672419993));
#59096=CARTESIAN_POINT('Ctrl Pts',(85.4285769162284,3.56704368296036,338.388837919075));
#59097=CARTESIAN_POINT('Ctrl Pts',(85.4208198064537,3.66021378900941,338.287979408203));
#59098=CARTESIAN_POINT('Ctrl Pts',(85.413062696679,3.74894211843394,338.183491174031));
#59099=CARTESIAN_POINT('Ctrl Pts',(85.4053014417528,3.83771786144074,338.078947104687));
#59100=CARTESIAN_POINT('Ctrl Pts',(85.3975401868266,3.9220468581332,337.970769755316));
#59101=CARTESIAN_POINT('Ctrl Pts',(85.3897789319004,4.00163774294694,337.859384275805));
#59102=CARTESIAN_POINT('Ctrl Pts',(85.3820052614958,4.08135594723767,337.747820615828));
#59103=CARTESIAN_POINT('Ctrl Pts',(85.3742315910911,4.15632067984563,337.633038897963));
#59104=CARTESIAN_POINT('Ctrl Pts',(85.3664579206864,4.22628500760272,337.515491621336));
#59105=CARTESIAN_POINT('Ctrl Pts',(85.3590461165093,4.29299247906989,337.403416198717));
#59106=CARTESIAN_POINT('Ctrl Pts',(85.3516343123323,4.35515446951123,337.288827149546));
#59107=CARTESIAN_POINT('Ctrl Pts',(85.3442225081553,4.41259772395807,337.17213360294));
#59108=CARTESIAN_POINT('Ctrl Pts',(85.3364474293769,4.47285644342027,337.049720558002));
#59109=CARTESIAN_POINT('Ctrl Pts',(85.3286723505985,4.52811260115697,336.924604656233));
#59110=CARTESIAN_POINT('Ctrl Pts',(85.32089727182,4.57811492756779,336.797233087966));
#59111=CARTESIAN_POINT('Ctrl Pts',(85.313131760771,4.62805572293273,336.670018258523));
#59112=CARTESIAN_POINT('Ctrl Pts',(85.305366249722,4.67275540934577,336.540553645877));
#59113=CARTESIAN_POINT('Ctrl Pts',(85.297600738673,4.71200880119516,336.409310512257));
#59114=CARTESIAN_POINT('Ctrl Pts',(85.2898429271508,4.75122327319227,336.278197506587));
#59115=CARTESIAN_POINT('Ctrl Pts',(85.2820851156286,4.7850020856823,336.145309861299));
#59116=CARTESIAN_POINT('Ctrl Pts',(85.2743273041064,4.81318845752591,336.01113794056));
#59117=CARTESIAN_POINT('Ctrl Pts',(85.2665753305834,4.84135361823079,335.877066988446));
#59118=CARTESIAN_POINT('Ctrl Pts',(85.2588233570604,4.86393463504489,335.741714065553));
#59119=CARTESIAN_POINT('Ctrl Pts',(85.2510713835374,4.88082490479422,335.605583446967));
#59120=CARTESIAN_POINT('Ctrl Pts',(85.2433226929797,4.89770802150431,335.469510479778));
#59121=CARTESIAN_POINT('Ctrl Pts',(85.2355740024221,4.90890513651081,335.332660859052));
#59122=CARTESIAN_POINT('Ctrl Pts',(85.2278253118645,4.91436101797314,335.195547558221));
#59123=CARTESIAN_POINT('Ctrl Pts',(85.2200782334867,4.91981576429376,335.058462784957));
#59124=CARTESIAN_POINT('Ctrl Pts',(85.2123311551088,4.91953163750699,334.92111483103));
#59125=CARTESIAN_POINT('Ctrl Pts',(85.204584076731,4.91350543417797,334.784019883314));
#59126=CARTESIAN_POINT('Ctrl Pts',(85.1968369334252,4.90747918034357,334.646923786611));
#59127=CARTESIAN_POINT('Ctrl Pts',(85.1890897901194,4.8957107711446,334.510081090846));
#59128=CARTESIAN_POINT('Ctrl Pts',(85.1813426468136,4.87824908803674,334.374005672894));
#59129=CARTESIAN_POINT('Ctrl Pts',(85.1735937617855,4.86078347917178,334.237899662299));
#59130=CARTESIAN_POINT('Ctrl Pts',(85.1658448767574,4.83762209914363,334.102561660393));
#59131=CARTESIAN_POINT('Ctrl Pts',(85.1580959917293,4.8088653697216,333.968497737088));
#59132=CARTESIAN_POINT('Ctrl Pts',(85.1503388819545,4.78007811760985,333.83429151695));
#59133=CARTESIAN_POINT('Ctrl Pts',(85.1425817721798,4.74568373457853,333.701362459583));
#59134=CARTESIAN_POINT('Ctrl Pts',(85.1348246624051,4.70583333958636,333.57020433539));
#59135=CARTESIAN_POINT('Ctrl Pts',(85.1270634074789,4.66596164981726,333.438976124489));
#59136=CARTESIAN_POINT('Ctrl Pts',(85.1193021525527,4.62062826777559,333.30952110113));
#59137=CARTESIAN_POINT('Ctrl Pts',(85.1115408976266,4.570033036447,333.182314353833));
#59138=CARTESIAN_POINT('Ctrl Pts',(85.1037672272219,4.51935686923727,333.054904117196));
#59139=CARTESIAN_POINT('Ctrl Pts',(85.0959935568172,4.46340219221381,332.929749700533));
#59140=CARTESIAN_POINT('Ctrl Pts',(85.0882198864126,4.40241589183839,332.807303628455));
#59141=CARTESIAN_POINT('Ctrl Pts',(85.0808080822355,4.34426851841768,332.690557450489));
#59142=CARTESIAN_POINT('Ctrl Pts',(85.0733962780583,4.28154756220092,332.576273396933));
#59143=CARTESIAN_POINT('Ctrl Pts',(85.0659844738812,4.21450331038607,332.464818564827));
#59144=CARTESIAN_POINT('Ctrl Pts',(85.0582093951028,4.14417302007551,332.347900999393));
#59145=CARTESIAN_POINT('Ctrl Pts',(85.0504343163243,4.06886266659583,332.233727523917));
#59146=CARTESIAN_POINT('Ctrl Pts',(85.0426592375459,3.98881232544097,332.122751436718));
#59147=CARTESIAN_POINT('Ctrl Pts',(85.0348937264969,3.90886049132738,332.011911912659));
#59148=CARTESIAN_POINT('Ctrl Pts',(85.0271282154479,3.82418050173203,331.904262262147));
#59149=CARTESIAN_POINT('Ctrl Pts',(85.0193627043989,3.73505761341126,331.800230057176));
#59150=CARTESIAN_POINT('Ctrl Pts',(85.0116048928767,3.64602309069343,331.696301000439));
#59151=CARTESIAN_POINT('Ctrl Pts',(85.0038470813545,3.55255468840301,331.59598254642));
#59152=CARTESIAN_POINT('Ctrl Pts',(84.9960892698323,3.45497992095919,331.499671899912));
#59153=CARTESIAN_POINT('Ctrl Pts',(84.9883372963093,3.35747858162235,331.403433730219));
#59154=CARTESIAN_POINT('Ctrl Pts',(84.9805853227863,3.25587730503031,331.311197638309));
#59155=CARTESIAN_POINT('Ctrl Pts',(84.9728333492633,3.15054245776644,331.223326161248));
#59156=CARTESIAN_POINT('Ctrl Pts',(84.9650846587056,3.04525221987286,331.13549189781));
#59157=CARTESIAN_POINT('Ctrl Pts',(84.9573359681481,2.93623185566565,331.052018822717));
#59158=CARTESIAN_POINT('Ctrl Pts',(84.9495872775904,2.82388284633023,330.97323098096));
#59159=CARTESIAN_POINT('Ctrl Pts',(84.9418401992126,2.71155721214464,330.894459531671));
#59160=CARTESIAN_POINT('Ctrl Pts',(84.9340931208348,2.59590463019016,330.820371601054));
#59161=CARTESIAN_POINT('Ctrl Pts',(84.9263460424569,2.47735743945906,330.751249221282));
#59162=CARTESIAN_POINT('Ctrl Pts',(84.9185988991511,2.35880925518849,330.682126262198));
#59163=CARTESIAN_POINT('Ctrl Pts',(84.9108517558453,2.23736675142004,330.61796913385));
#59164=CARTESIAN_POINT('Ctrl Pts',(84.9031046125395,2.11348851074179,330.559014819045));
#59165=CARTESIAN_POINT('Ctrl Pts',(84.8953557275114,1.98958241960477,330.500047250058));
#59166=CARTESIAN_POINT('Ctrl Pts',(84.8876068424833,1.86323985475948,330.446284990126));
#59167=CARTESIAN_POINT('Ctrl Pts',(84.8798579574552,1.7349407251728,330.397917455908));
#59168=CARTESIAN_POINT('Ctrl Pts',(84.8721008476805,1.60650541756431,330.34949858389));
#59169=CARTESIAN_POINT('Ctrl Pts',(84.8643437379057,1.47610976310014,330.306486013944));
#59170=CARTESIAN_POINT('Ctrl Pts',(84.856586628131,1.34425076298466,330.269019874411));
#59171=CARTESIAN_POINT('Ctrl Pts',(84.8488253732048,1.21232130163528,330.231533714172));
#59172=CARTESIAN_POINT('Ctrl Pts',(84.8410641182786,1.07892731643922,330.199599981009));
#59173=CARTESIAN_POINT('Ctrl Pts',(84.8333028633524,0.94457646597386,330.17330772035));
#59174=CARTESIAN_POINT('Ctrl Pts',(84.8255291929477,0.810010697933139,330.146973400644));
#59175=CARTESIAN_POINT('Ctrl Pts',(84.8177555225431,0.67448539249313,330.126298646079));
#59176=CARTESIAN_POINT('Ctrl Pts',(84.8099818521384,0.53851469168353,330.111320731594));
#59177=CARTESIAN_POINT('Ctrl Pts',(84.8025700479614,0.408873459710019,330.097040042632));
#59178=CARTESIAN_POINT('Ctrl Pts',(84.7951582437844,0.278827652596291,330.087937773811));
#59179=CARTESIAN_POINT('Ctrl Pts',(84.7877464396073,0.148821414839618,330.084002110559));
#59180=CARTESIAN_POINT('Ctrl Pts',(84.7799713608289,0.012443184101203,330.079873548727));
#59181=CARTESIAN_POINT('Ctrl Pts',(84.7721962820505,-0.124322480785245,
330.081417812792));
#59182=CARTESIAN_POINT('Ctrl Pts',(84.764421203272,-0.26096447296876,330.088678323878));
#59183=CARTESIAN_POINT('Ctrl Pts',(84.756655692223,-0.39743831848221,330.095929900443));
#59184=CARTESIAN_POINT('Ctrl Pts',(84.748890181174,-0.533788407509145,330.108883707434));
#59185=CARTESIAN_POINT('Ctrl Pts',(84.741124670125,-0.669500816840078,330.1275312501));
#59186=CARTESIAN_POINT('Ctrl Pts',(84.7333668586029,-0.805078666920661,
330.146160303673));
#59187=CARTESIAN_POINT('Ctrl Pts',(84.7256090470807,-0.940019710799557,
330.170471805478));
#59188=CARTESIAN_POINT('Ctrl Pts',(84.7178512355586,-1.07381269364743,330.200405291958));
#59189=CARTESIAN_POINT('Ctrl Pts',(84.7100992620356,-1.20750499303416,330.230316252541));
#59190=CARTESIAN_POINT('Ctrl Pts',(84.7023472885126,-1.34005057113636,330.265840691757));
#59191=CARTESIAN_POINT('Ctrl Pts',(84.6945953149896,-1.47094630081934,330.30686671374));
#59192=CARTESIAN_POINT('Ctrl Pts',(84.686846624432,-1.60178659608265,330.347875361178));
#59193=CARTESIAN_POINT('Ctrl Pts',(84.6790979338744,-1.7309780604082,330.394380840669));
#59194=CARTESIAN_POINT('Ctrl Pts',(84.6713492433168,-1.85803093294256,330.44622089746));
#59195=CARTESIAN_POINT('Ctrl Pts',(84.6636021649389,-1.98505737106589,330.498050168494));
#59196=CARTESIAN_POINT('Ctrl Pts',(84.6558550865611,-2.10994574075779,330.555211661578));
#59197=CARTESIAN_POINT('Ctrl Pts',(84.6481080081833,-2.23222491171074,330.617494437421));
#59198=CARTESIAN_POINT('Ctrl Pts',(84.6403608648775,-2.35450510748066,330.679777735253));
#59199=CARTESIAN_POINT('Ctrl Pts',(84.6326137215717,-2.47417571259869,330.74718222405));
#59200=CARTESIAN_POINT('Ctrl Pts',(84.6248665782659,-2.59078927781674,330.819450516924));
#59201=CARTESIAN_POINT('Ctrl Pts',(84.6171176932378,-2.70742906024019,330.891735057244));
#59202=CARTESIAN_POINT('Ctrl Pts',(84.6093688082097,-2.82101010295721,330.968885371695));
#59203=CARTESIAN_POINT('Ctrl Pts',(84.6016199231816,-2.93111341517882,331.050600398813));
#59204=CARTESIAN_POINT('Ctrl Pts',(84.5938628134069,-3.04133359219369,331.132402159104));
#59205=CARTESIAN_POINT('Ctrl Pts',(84.5861057036322,-3.14806835062554,331.218778077154));
#59206=CARTESIAN_POINT('Ctrl Pts',(84.5783485938575,-3.25093089769393,331.309386045531));
#59207=CARTESIAN_POINT('Ctrl Pts',(84.5705873389313,-3.35384841121836,331.40004243191));
#59208=CARTESIAN_POINT('Ctrl Pts',(84.5628260840052,-3.45288930824588,331.494935104525));
#59209=CARTESIAN_POINT('Ctrl Pts',(84.555064829079,-3.54770398539075,331.593685350038));
#59210=CARTESIAN_POINT('Ctrl Pts',(84.5472911586743,-3.64267033511916,331.692593563762));
#59211=CARTESIAN_POINT('Ctrl Pts',(84.5395174882697,-3.73339669652386,331.7953713884));
#59212=CARTESIAN_POINT('Ctrl Pts',(84.531743817865,-3.81957349255914,331.901606642558));
#59213=CARTESIAN_POINT('Ctrl Pts',(84.5243320136879,-3.90173873800721,332.002896620078));
#59214=CARTESIAN_POINT('Ctrl Pts',(84.5169202095106,-3.97976827830493,332.107329153741));
#59215=CARTESIAN_POINT('Ctrl Pts',(84.5095084053335,-4.0534316965053,332.21452435942));
#59216=CARTESIAN_POINT('Ctrl Pts',(84.5016248252933,-4.13178393565423,332.328542750043));
#59217=CARTESIAN_POINT('Ctrl Pts',(84.4937412452531,-4.20543972543899,332.446041085973));
#59218=CARTESIAN_POINT('Ctrl Pts',(84.4858576652129,-4.27407965357783,332.566601927885));
#59219=CARTESIAN_POINT('Ctrl Pts',(84.4779844568314,-4.34262927884607,332.687004159635));
#59220=CARTESIAN_POINT('Ctrl Pts',(84.47011124845,-4.40617599182058,332.810460554398));
#59221=CARTESIAN_POINT('Ctrl Pts',(84.4622380400685,-4.46444249803971,332.936523262986));
#59222=CARTESIAN_POINT('Ctrl Pts',(84.454373654175,-4.52264371250896,333.062444709375));
#59223=CARTESIAN_POINT('Ctrl Pts',(84.4465092682815,-4.57557634175535,333.190966316337));
#59224=CARTESIAN_POINT('Ctrl Pts',(84.4386448823881,-4.62300815605339,333.321614272116));
#59225=CARTESIAN_POINT('Ctrl Pts',(84.4305759235648,-4.67167379398992,333.455660717675));
#59226=CARTESIAN_POINT('Ctrl Pts',(84.4225069647415,-4.71454830376636,333.591945312942));
#59227=CARTESIAN_POINT('Ctrl Pts',(84.4144380059182,-4.75143234417331,333.729931599778));
#59228=CARTESIAN_POINT('Ctrl Pts',(84.4065875903808,-4.78731740075063,333.86418060437));
#59229=CARTESIAN_POINT('Ctrl Pts',(84.3987371748433,-4.81753218104775,334.000039923139));
#59230=CARTESIAN_POINT('Ctrl Pts',(84.3908867593059,-4.84194286277766,334.136998043979));
#59231=CARTESIAN_POINT('Ctrl Pts',(84.3827085288397,-4.86737287728747,334.279675214519));
#59232=CARTESIAN_POINT('Ctrl Pts',(84.3745302983735,-4.88650344351115,334.423544538267));
#59233=CARTESIAN_POINT('Ctrl Pts',(84.3663520679073,-4.89924191044213,334.568014160571));
#59234=CARTESIAN_POINT('Ctrl Pts',(84.358173837441,-4.91198037737311,334.712483782875));
#59235=CARTESIAN_POINT('Ctrl Pts',(84.3499956069748,-4.91832668679319,334.857553244037));
#59236=CARTESIAN_POINT('Ctrl Pts',(84.3418173765086,-4.9182493002317,335.002623598754));
#59237=CARTESIAN_POINT('',(82.5918173765463,-4.91824909607723,335.002981851016));
#59238=CARTESIAN_POINT('Ctrl Pts',(84.3418173764577,-4.91824930023122,335.002623599657));
#59239=CARTESIAN_POINT('Ctrl Pts',(84.3332528523107,-4.91816825833526,335.15454626326));
#59240=CARTESIAN_POINT('Ctrl Pts',(84.3246883281636,-4.91104390444931,335.306222086739));
#59241=CARTESIAN_POINT('Ctrl Pts',(84.3161238040166,-4.89696912524936,335.457030030583));
#59242=CARTESIAN_POINT('Ctrl Pts',(84.3075123360255,-4.88281719941171,335.608664582477));
#59243=CARTESIAN_POINT('Ctrl Pts',(84.2989008680343,-4.86163853326073,335.759421483946));
#59244=CARTESIAN_POINT('Ctrl Pts',(84.2902894000431,-4.83357773483632,335.908685503238));
#59245=CARTESIAN_POINT('Ctrl Pts',(84.2816536082752,-4.80543767645363,336.058371130631));
#59246=CARTESIAN_POINT('Ctrl Pts',(84.2730178165074,-4.77037667053886,336.206555215299));
#59247=CARTESIAN_POINT('Ctrl Pts',(84.2643820247396,-4.72858930711563,336.352636768365));
#59248=CARTESIAN_POINT('Ctrl Pts',(84.2557148909255,-4.68665028400532,336.499248498038));
#59249=CARTESIAN_POINT('Ctrl Pts',(84.2470477571114,-4.63793611011578,336.643742196788));
#59250=CARTESIAN_POINT('Ctrl Pts',(84.2383806232973,-4.5826907614107,336.785533099044));
#59251=CARTESIAN_POINT('Ctrl Pts',(84.236010539218,-4.56758356170332,336.82430674293));
#59252=CARTESIAN_POINT('Ctrl Pts',(84.2336404551387,-4.55198823657263,336.862878416919));
#59253=CARTESIAN_POINT('Ctrl Pts',(84.2312703710595,-4.53591036852141,336.901236490087));
#59254=CARTESIAN_POINT('Ctrl Pts',(84.223495292281,-4.48316680056935,337.027070439727));
#59255=CARTESIAN_POINT('Ctrl Pts',(84.2157202135026,-4.42509964498674,337.150906772384));
#59256=CARTESIAN_POINT('Ctrl Pts',(84.2079451347242,-4.3618811326319,337.272262319207));
#59257=CARTESIAN_POINT('Ctrl Pts',(84.2001796236752,-4.29874041468121,337.393468530305));
#59258=CARTESIAN_POINT('Ctrl Pts',(84.1924141126262,-4.23046113175489,337.512199686352));
#59259=CARTESIAN_POINT('Ctrl Pts',(84.1846486015771,-4.15726393231983,337.627991563824));
#59260=CARTESIAN_POINT('Ctrl Pts',(84.1768907900549,-4.08413930812106,337.743668633314));
#59261=CARTESIAN_POINT('Ctrl Pts',(84.1691329785327,-4.0061066786973,337.85641189559));
#59262=CARTESIAN_POINT('Ctrl Pts',(84.1613751670105,-3.923432885982,337.965781086273));
#59263=CARTESIAN_POINT('Ctrl Pts',(84.1536231934875,-3.8408213079174,338.075067973172));
#59264=CARTESIAN_POINT('Ctrl Pts',(84.1458712199645,-3.75357575320992,338.180985531866));
#59265=CARTESIAN_POINT('Ctrl Pts',(84.1381192464415,-3.66200650719316,338.283122203601));
#59266=CARTESIAN_POINT('Ctrl Pts',(84.1303705558839,-3.57047604080659,338.385215620393));
#59267=CARTESIAN_POINT('Ctrl Pts',(84.1226218653262,-3.47462578539216,338.483531044486));
#59268=CARTESIAN_POINT('Ctrl Pts',(84.1148731747686,-3.37480632238623,338.577689945884));
#59269=CARTESIAN_POINT('Ctrl Pts',(84.1071260963908,-3.27500762765328,338.671829256737));
#59270=CARTESIAN_POINT('Ctrl Pts',(84.0993790180129,-3.17124165211249,338.761813497001));
#59271=CARTESIAN_POINT('Ctrl Pts',(84.0916319396351,-3.06389556843324,338.847301262994));
#59272=CARTESIAN_POINT('Ctrl Pts',(84.0838847963293,-2.95654858509048,338.932789745456));
#59273=CARTESIAN_POINT('Ctrl Pts',(84.0761376530235,-2.84562173952397,339.013781434981));
#59274=CARTESIAN_POINT('Ctrl Pts',(84.0683905097177,-2.73153466729184,339.089975724119));
#59275=CARTESIAN_POINT('Ctrl Pts',(84.0606416246896,-2.61742194586382,339.166187143351));
#59276=CARTESIAN_POINT('Ctrl Pts',(84.0528927396615,-2.50014790896661,339.237598798944));
#59277=CARTESIAN_POINT('Ctrl Pts',(84.0451438546334,-2.3801601519419,339.303954078938));
#59278=CARTESIAN_POINT('Ctrl Pts',(84.0373867448587,-2.2600450386721,339.370379789112));
#59279=CARTESIAN_POINT('Ctrl Pts',(84.0296296350839,-2.13721079405819,339.431738213363));
#59280=CARTESIAN_POINT('Ctrl Pts',(84.0218725253092,-2.01212903153014,339.487819049714));
#59281=CARTESIAN_POINT('Ctrl Pts',(84.014111270383,-1.88698042930755,339.54392985387));
#59282=CARTESIAN_POINT('Ctrl Pts',(84.0063500154569,-1.75958227892961,339.594757305905));
#59283=CARTESIAN_POINT('Ctrl Pts',(83.9985887605307,-1.63042410291557,339.640140117187));
#59284=CARTESIAN_POINT('Ctrl Pts',(83.990815090126,-1.50105931591254,339.685595526178));
#59285=CARTESIAN_POINT('Ctrl Pts',(83.9830414197214,-1.36992925120473,339.725588775866));
#59286=CARTESIAN_POINT('Ctrl Pts',(83.9752677493167,-1.23753730917189,339.760008872986));
#59287=CARTESIAN_POINT('Ctrl Pts',(83.9678559451397,-1.11130824389287,339.792826706304));
#59288=CARTESIAN_POINT('Ctrl Pts',(83.9604441409626,-0.983932419435646,
339.820578509659));
#59289=CARTESIAN_POINT('Ctrl Pts',(83.9530323367856,-0.855851045273139,
339.843211956007));
#59290=CARTESIAN_POINT('Ctrl Pts',(83.9452572580071,-0.721492021427351,
339.866954734982));
#59291=CARTESIAN_POINT('Ctrl Pts',(83.9374821792287,-0.58593193758518,339.885139770372));
#59292=CARTESIAN_POINT('Ctrl Pts',(83.9297071004502,-0.449670304741494,
339.897650424391));
#59293=CARTESIAN_POINT('Ctrl Pts',(83.9219415894012,-0.313576350512047,
339.910145683253));
#59294=CARTESIAN_POINT('Ctrl Pts',(83.9141760783522,-0.176782950518166,
339.916980418895));
#59295=CARTESIAN_POINT('Ctrl Pts',(83.9064105673032,-0.0397998857711188,
339.918088961334));
#59296=CARTESIAN_POINT('Ctrl Pts',(83.898652755781,0.0970473598686024,339.919196404649));
#59297=CARTESIAN_POINT('Ctrl Pts',(83.8908949442588,0.234083507681419,339.914588950238));
#59298=CARTESIAN_POINT('Ctrl Pts',(83.8831371327366,0.370793926475477,339.904252738857));
#59299=CARTESIAN_POINT('Ctrl Pts',(83.8753851592136,0.507401466343871,339.893924305803));
#59300=CARTESIAN_POINT('Ctrl Pts',(83.8676331856906,0.643683376903208,339.877875726105));
#59301=CARTESIAN_POINT('Ctrl Pts',(83.8598812121676,0.779125656416427,339.856145207262));
#59302=CARTESIAN_POINT('Ctrl Pts',(83.8521325216099,0.914510576043951,339.834423891306));
#59303=CARTESIAN_POINT('Ctrl Pts',(83.8443838310523,1.04905618672202,339.807025483967));
#59304=CARTESIAN_POINT('Ctrl Pts',(83.8366351404947,1.18225445477238,339.774039952354));
#59305=CARTESIAN_POINT('Ctrl Pts',(83.8288880621168,1.31542500981058,339.741061283656));
#59306=CARTESIAN_POINT('Ctrl Pts',(83.821140983739,1.44724840063401,339.702497896775));
#59307=CARTESIAN_POINT('Ctrl Pts',(83.8133939053612,1.57722801225449,339.658490620347));
#59308=CARTESIAN_POINT('Ctrl Pts',(83.8056467620553,1.70720871322922,339.614482975095));
#59309=CARTESIAN_POINT('Ctrl Pts',(83.7978996187495,1.83534523394945,339.565031474641));
#59310=CARTESIAN_POINT('Ctrl Pts',(83.7901524754437,1.96115769831933,339.510326323541));
#59311=CARTESIAN_POINT('Ctrl Pts',(83.7824035904156,2.0869984480022,339.45560887356));
#59312=CARTESIAN_POINT('Ctrl Pts',(83.7746547053875,2.21051374323885,339.395635578443));
#59313=CARTESIAN_POINT('Ctrl Pts',(83.7669058203594,2.33124557403613,339.330643963204));
#59314=CARTESIAN_POINT('Ctrl Pts',(83.7591487105847,2.45210555084611,339.265583365194));
#59315=CARTESIAN_POINT('Ctrl Pts',(83.75139160081,2.57017581681137,339.195493992452));
#59316=CARTESIAN_POINT('Ctrl Pts',(83.7436344910352,2.68502430742466,339.120658628307));
#59317=CARTESIAN_POINT('Ctrl Pts',(83.7358732361091,2.79993416939919,339.045783274536));
#59318=CARTESIAN_POINT('Ctrl Pts',(83.7281119811829,2.91161850744542,338.966157102737));
#59319=CARTESIAN_POINT('Ctrl Pts',(83.7203507262567,3.01967678178837,338.882104480308));
#59320=CARTESIAN_POINT('Ctrl Pts',(83.712577055852,3.12790791415415,338.797917401076));
#59321=CARTESIAN_POINT('Ctrl Pts',(83.7048033854474,3.23250109329111,338.709289974345));
#59322=CARTESIAN_POINT('Ctrl Pts',(83.6970297150427,3.33309056376183,338.616585455407));
#59323=CARTESIAN_POINT('Ctrl Pts',(83.6896179108657,3.42899757018056,338.528196354131));
#59324=CARTESIAN_POINT('Ctrl Pts',(83.6822061066887,3.52126502111687,338.436101399095));
#59325=CARTESIAN_POINT('Ctrl Pts',(83.6747943025117,3.60961014988057,338.340643295591));
#59326=CARTESIAN_POINT('Ctrl Pts',(83.6670192237332,3.70228533657253,338.240506506079));
#59327=CARTESIAN_POINT('Ctrl Pts',(83.6592441449548,3.79093686059564,338.136352105636));
#59328=CARTESIAN_POINT('Ctrl Pts',(83.6514690661764,3.87519632468573,338.028537024314));
#59329=CARTESIAN_POINT('Ctrl Pts',(83.6437035551274,3.95935210214103,337.920854616314));
#59330=CARTESIAN_POINT('Ctrl Pts',(83.6359380440784,4.03912633509538,337.809520795533));
#59331=CARTESIAN_POINT('Ctrl Pts',(83.6281725330294,4.1141879285028,337.694928709903));
#59332=CARTESIAN_POINT('Ctrl Pts',(83.6204147215072,4.18917509812181,337.58045024266));
#59333=CARTESIAN_POINT('Ctrl Pts',(83.612656909985,4.25945871412599,337.462720264469));
#59334=CARTESIAN_POINT('Ctrl Pts',(83.6048990984628,4.3247486255139,337.342164039647));
#59335=CARTESIAN_POINT('Ctrl Pts',(83.5971471249398,4.38998940417298,337.221698537207));
#59336=CARTESIAN_POINT('Ctrl Pts',(83.5893951514168,4.45024377278173,337.098411363829));
#59337=CARTESIAN_POINT('Ctrl Pts',(83.5816431778938,4.5052657050071,336.972755430809));
#59338=CARTESIAN_POINT('Ctrl Pts',(83.5738944873362,4.56026433541155,336.847152713151));
#59339=CARTESIAN_POINT('Ctrl Pts',(83.5661457967786,4.61003478032397,336.719183588396));
#59340=CARTESIAN_POINT('Ctrl Pts',(83.558397106221,4.6543777688322,336.589323959267));
#59341=CARTESIAN_POINT('Ctrl Pts',(83.5506500278431,4.69871153141132,336.459491348519));
#59342=CARTESIAN_POINT('Ctrl Pts',(83.5429029494653,4.73761995746883,336.327769385439));
#59343=CARTESIAN_POINT('Ctrl Pts',(83.5351558710875,4.77095272594241,336.194651894621));
#59344=CARTESIAN_POINT('Ctrl Pts',(83.5274087277816,4.80428577377668,336.061533288151));
#59345=CARTESIAN_POINT('Ctrl Pts',(83.5196615844759,4.83204297587769,335.927019509783));
#59346=CARTESIAN_POINT('Ctrl Pts',(83.5119144411701,4.85412459082211,335.791617028162));
#59347=CARTESIAN_POINT('Ctrl Pts',(83.504165556142,4.87621117018238,335.656184105188));
#59348=CARTESIAN_POINT('Ctrl Pts',(83.4964166711139,4.89261956040267,335.519862467085));
#59349=CARTESIAN_POINT('Ctrl Pts',(83.4886677860858,4.90330164584888,335.383165802644));
#59350=CARTESIAN_POINT('Ctrl Pts',(83.4809106763111,4.91399506937095,335.24632404695));
#59351=CARTESIAN_POINT('Ctrl Pts',(83.4731535665364,4.91895001632563,335.109106860064));
#59352=CARTESIAN_POINT('Ctrl Pts',(83.4653964567616,4.91817047034942,334.972030604531));
#59353=CARTESIAN_POINT('Ctrl Pts',(83.4576352018355,4.91739050780877,334.83488109983));
#59354=CARTESIAN_POINT('Ctrl Pts',(83.4498739469093,4.91086996495655,334.697873066777));
#59355=CARTESIAN_POINT('Ctrl Pts',(83.4421126919831,4.89866485420154,334.561518861625));
#59356=CARTESIAN_POINT('Ctrl Pts',(83.4343390215785,4.88644021924696,334.424946534183));
#59357=CARTESIAN_POINT('Ctrl Pts',(83.4265653511738,4.86851289611195,334.289030512404));
#59358=CARTESIAN_POINT('Ctrl Pts',(83.4187916807692,4.84499042266779,334.154274946122));
#59359=CARTESIAN_POINT('Ctrl Pts',(83.411379876592,4.82256292602124,334.025792283868));
#59360=CARTESIAN_POINT('Ctrl Pts',(83.4039680724147,4.79504952557784,333.898364751355));
#59361=CARTESIAN_POINT('Ctrl Pts',(83.3965562682375,4.76258538824808,333.772415590623));
#59362=CARTESIAN_POINT('Ctrl Pts',(83.3887811894591,4.72853008684265,333.640293286342));
#59363=CARTESIAN_POINT('Ctrl Pts',(83.3810061106806,4.68891885594517,333.509380406035));
#59364=CARTESIAN_POINT('Ctrl Pts',(83.3732310319022,4.64385248475392,333.380179898154));
#59365=CARTESIAN_POINT('Ctrl Pts',(83.3654655208532,4.5988415706015,333.251138379723));
#59366=CARTESIAN_POINT('Ctrl Pts',(83.3577000098042,4.54838900039974,333.123805406565));
#59367=CARTESIAN_POINT('Ctrl Pts',(83.3499344987552,4.4926462061047,332.998672158473));
#59368=CARTESIAN_POINT('Ctrl Pts',(83.3421766872329,4.43695868095249,332.87366298036));
#59369=CARTESIAN_POINT('Ctrl Pts',(83.3344188757107,4.37599152812549,332.750849541683));
#59370=CARTESIAN_POINT('Ctrl Pts',(83.3266610641885,4.30994534410407,332.630705971532));
#59371=CARTESIAN_POINT('Ctrl Pts',(83.3189090906655,4.24394886193057,332.510652813227));
#59372=CARTESIAN_POINT('Ctrl Pts',(83.3111571171425,4.17288114386934,332.393265865461));
#59373=CARTESIAN_POINT('Ctrl Pts',(83.3034051436195,4.09698991372582,332.278997113319));
#59374=CARTESIAN_POINT('Ctrl Pts',(83.2956564530618,4.02113082356338,332.16477675406));
#59375=CARTESIAN_POINT('Ctrl Pts',(83.2879077625042,3.94045250002448,332.053672288855));
#59376=CARTESIAN_POINT('Ctrl Pts',(83.2801590719466,3.85524730293788,331.946108827137));
#59377=CARTESIAN_POINT('Ctrl Pts',(83.2724119935687,3.77005983350412,331.838567744895));
#59378=CARTESIAN_POINT('Ctrl Pts',(83.2646649151909,3.68034760648996,331.734566506921));
#59379=CARTESIAN_POINT('Ctrl Pts',(83.2569178368131,3.58644454217906,331.634498758227));
#59380=CARTESIAN_POINT('Ctrl Pts',(83.2491706935072,3.4925406908701,331.534430170869));
#59381=CARTESIAN_POINT('Ctrl Pts',(83.2414235502014,3.39444619967918,331.438295423574));
#59382=CARTESIAN_POINT('Ctrl Pts',(83.2336764068956,3.29253299308747,331.346452470279));
#59383=CARTESIAN_POINT('Ctrl Pts',(83.2259275218675,3.19059687424331,331.254588868738));
#59384=CARTESIAN_POINT('Ctrl Pts',(83.2181786368394,3.08484062192922,331.167019242833));
#59385=CARTESIAN_POINT('Ctrl Pts',(83.2104297518113,2.97567016987738,331.084062040507));
#59386=CARTESIAN_POINT('Ctrl Pts',(83.2026726420365,2.86638384317972,331.001016786549));
#59387=CARTESIAN_POINT('Ctrl Pts',(83.1949155322618,2.75367638943808,330.9225939726));
#59388=CARTESIAN_POINT('Ctrl Pts',(83.1871584224871,2.63798418470832,330.84906968214));
#59389=CARTESIAN_POINT('Ctrl Pts',(83.1793971675609,2.52223015776348,330.77550610265));
#59390=CARTESIAN_POINT('Ctrl Pts',(83.1716359126347,2.40348853994487,330.70684645804));
#59391=CARTESIAN_POINT('Ctrl Pts',(83.1638746577085,2.28222049408427,330.643320911648));
#59392=CARTESIAN_POINT('Ctrl Pts',(83.1561009873039,2.16075845887154,330.579693745085));
#59393=CARTESIAN_POINT('Ctrl Pts',(83.1483273168992,2.03676227329839,330.521217255328));
#59394=CARTESIAN_POINT('Ctrl Pts',(83.1405536464946,1.91071408262761,330.46807383589));
#59395=CARTESIAN_POINT('Ctrl Pts',(83.1331418423176,1.79053346556021,330.417404255412));
#59396=CARTESIAN_POINT('Ctrl Pts',(83.1257300381407,1.66848785522842,330.371582511186));
#59397=CARTESIAN_POINT('Ctrl Pts',(83.1183182339637,1.5450063114647,330.330723979027));
#59398=CARTESIAN_POINT('Ctrl Pts',(83.1105431551853,1.41547256940628,330.287862848494));
#59399=CARTESIAN_POINT('Ctrl Pts',(83.1027680764069,1.28394922552208,330.250328306311));
#59400=CARTESIAN_POINT('Ctrl Pts',(83.0949929976284,1.15091376271326,330.218307770956));
#59401=CARTESIAN_POINT('Ctrl Pts',(83.0872274865794,1.01804200851096,330.186326638909));
#59402=CARTESIAN_POINT('Ctrl Pts',(83.0794619755304,0.883662214148742,330.15984610341));
#59403=CARTESIAN_POINT('Ctrl Pts',(83.0716964644814,0.748269371713734,330.139004627666));
#59404=CARTESIAN_POINT('Ctrl Pts',(83.0639386529592,0.613010771676187,330.118183816306));
#59405=CARTESIAN_POINT('Ctrl Pts',(83.056180841437,0.476741506293891,330.102990997093));
#59406=CARTESIAN_POINT('Ctrl Pts',(83.0484230299148,0.33996883509979,330.093514062625));
#59407=CARTESIAN_POINT('Ctrl Pts',(83.0406710563918,0.203299089678165,330.08404425985));
#59408=CARTESIAN_POINT('Ctrl Pts',(83.0329190828688,0.0661270808542804,
330.080281807033));
#59409=CARTESIAN_POINT('Ctrl Pts',(83.0251671093458,-0.0710330499077727,
330.082262983005));
#59410=CARTESIAN_POINT('Ctrl Pts',(83.0174184187882,-0.208135093273016,
330.084243319948));
#59411=CARTESIAN_POINT('Ctrl Pts',(83.0096697282306,-0.345224878561342,
330.091962442113));
#59412=CARTESIAN_POINT('Ctrl Pts',(83.001921037673,-0.481786709502685,330.10540454899));
#59413=CARTESIAN_POINT('Ctrl Pts',(82.9941739592951,-0.618320127614607,
330.118843859125));
#59414=CARTESIAN_POINT('Ctrl Pts',(82.9864268809173,-0.754325421119501,
330.13800374729));
#59415=CARTESIAN_POINT('Ctrl Pts',(82.9786798025395,-0.889290862103369,
330.162816436698));
#59416=CARTESIAN_POINT('Ctrl Pts',(82.9709326592337,-1.02425743422744,330.18762933406));
#59417=CARTESIAN_POINT('Ctrl Pts',(82.9631855159279,-1.15818375201624,330.218095056485));
#59418=CARTESIAN_POINT('Ctrl Pts',(82.9554383726221,-1.29056753469086,330.254094554155));
#59419=CARTESIAN_POINT('Ctrl Pts',(82.947689487594,-1.42298108005033,330.290102145276));
#59420=CARTESIAN_POINT('Ctrl Pts',(82.939940602566,-1.55385102310939,330.331645884736));
#59421=CARTESIAN_POINT('Ctrl Pts',(82.9321917175379,-1.68268990016405,330.378556744654));
#59422=CARTESIAN_POINT('Ctrl Pts',(82.9244346077631,-1.81166552813415,330.425517396243));
#59423=CARTESIAN_POINT('Ctrl Pts',(82.9166774979884,-1.9386054158323,330.477856414074));
#59424=CARTESIAN_POINT('Ctrl Pts',(82.9089203882137,-2.06304125064884,330.535356244825));
#59425=CARTESIAN_POINT('Ctrl Pts',(82.9011591332875,-2.18754357999674,330.592886801647));
#59426=CARTESIAN_POINT('Ctrl Pts',(82.8933978783614,-2.30953884273251,330.655583487924));
#59427=CARTESIAN_POINT('Ctrl Pts',(82.8856366234352,-2.42858392792535,330.72318305658));
#59428=CARTESIAN_POINT('Ctrl Pts',(82.8778629530306,-2.54781944645781,330.790890762516));
#59429=CARTESIAN_POINT('Ctrl Pts',(82.8700892826259,-2.6640950251489,330.863516816319));
#59430=CARTESIAN_POINT('Ctrl Pts',(82.8623156122213,-2.77699636893558,330.940754475347));
#59431=CARTESIAN_POINT('Ctrl Pts',(82.8549038080441,-2.88464212800749,331.014396702765));
#59432=CARTESIAN_POINT('Ctrl Pts',(82.847492003867,-2.98922049302006,331.092230685172));
#59433=CARTESIAN_POINT('Ctrl Pts',(82.8400801996898,-3.09040225309415,331.173958053475));
#59434=CARTESIAN_POINT('Ctrl Pts',(82.8324063694531,-3.19516104478746,331.258574691349));
#59435=CARTESIAN_POINT('Ctrl Pts',(82.8247325392163,-3.29662844556156,331.347647886257));
#59436=CARTESIAN_POINT('Ctrl Pts',(82.8170587089795,-3.39439409141408,331.440888901049));
#59437=CARTESIAN_POINT('Ctrl Pts',(82.8093943689736,-3.49203883042911,331.534014604619));
#59438=CARTESIAN_POINT('Ctrl Pts',(82.8017300289677,-3.58599063092221,331.631297602963));
#59439=CARTESIAN_POINT('Ctrl Pts',(82.7940656889617,-3.67587032862144,331.732407554535));
#59440=CARTESIAN_POINT('Ctrl Pts',(82.7864088789718,-3.76566172183942,331.833418168191));
#59441=CARTESIAN_POINT('Ctrl Pts',(82.7787520689819,-3.85138870493917,331.938247957744));
#59442=CARTESIAN_POINT('Ctrl Pts',(82.7710952589921,-3.9327076603401,332.046528564417));
#59443=CARTESIAN_POINT('Ctrl Pts',(82.7634440899739,-4.01396670594483,332.154729397942));
#59444=CARTESIAN_POINT('Ctrl Pts',(82.7557929209558,-4.09082394509794,332.266375669851));
#59445=CARTESIAN_POINT('Ctrl Pts',(82.7481417519376,-4.16297523965459,332.381065060655));
#59446=CARTESIAN_POINT('Ctrl Pts',(82.740493585754,-4.23509821717846,332.495709439609));
#59447=CARTESIAN_POINT('Ctrl Pts',(82.7328454195705,-4.30251870852421,332.613394223232));
#59448=CARTESIAN_POINT('Ctrl Pts',(82.7251972533869,-4.36497543862418,332.733687470205));
#59449=CARTESIAN_POINT('Ctrl Pts',(82.7175503313811,-4.4274220084746,332.853961148278));
#59450=CARTESIAN_POINT('Ctrl Pts',(82.7099034093753,-4.48490623804694,332.976842089059));
#59451=CARTESIAN_POINT('Ctrl Pts',(82.7022564873696,-4.53721269882533,333.101873558448));
#59452=CARTESIAN_POINT('Ctrl Pts',(82.6946090521321,-4.58952267021037,333.226913419465));
#59453=CARTESIAN_POINT('Ctrl Pts',(82.6869616168946,-4.63665402759163,333.354103724897));
#59454=CARTESIAN_POINT('Ctrl Pts',(82.6793141816571,-4.67843961371987,333.482968080996));
#59455=CARTESIAN_POINT('Ctrl Pts',(82.6716604408377,-4.7202596535479,333.611938690334));
#59456=CARTESIAN_POINT('Ctrl Pts',(82.6640067000182,-4.75672499409276,333.742585724375));
#59457=CARTESIAN_POINT('Ctrl Pts',(82.6563529591987,-4.78771841246239,333.874417721591));
#59458=CARTESIAN_POINT('Ctrl Pts',(82.6486959875867,-4.81872491375561,334.006305367652));
#59459=CARTESIAN_POINT('Ctrl Pts',(82.6410390159747,-4.84425481630877,334.139378578565));
#59460=CARTESIAN_POINT('Ctrl Pts',(82.6333820443626,-4.86424235210448,334.273137287727));
#59461=CARTESIAN_POINT('Ctrl Pts',(82.6257145787911,-4.88425728102653,334.407079314595));
#59462=CARTESIAN_POINT('Ctrl Pts',(82.6180471132196,-4.89871462721325,334.54170831678));
#59463=CARTESIAN_POINT('Ctrl Pts',(82.6103796476481,-4.90760062330737,334.676520194428));
#59464=CARTESIAN_POINT('Ctrl Pts',(82.6041922239475,-4.91477136601546,334.785309493721));
#59465=CARTESIAN_POINT('Ctrl Pts',(82.5980048002468,-4.91831503790099,334.894217760072));
#59466=CARTESIAN_POINT('Ctrl Pts',(82.5918173765462,-4.91824909607723,335.002981851016));
#59467=CARTESIAN_POINT('',(80.8418173764668,-4.91824819243925,334.995783358204));
#59468=CARTESIAN_POINT('Ctrl Pts',(82.5918173765086,-4.91824909607683,335.002981851677));
#59469=CARTESIAN_POINT('Ctrl Pts',(82.5818256394777,-4.9181426101563,335.178619119737));
#59470=CARTESIAN_POINT('Ctrl Pts',(82.5718339024468,-4.9086284126831,335.353969158787));
#59471=CARTESIAN_POINT('Ctrl Pts',(82.561842165416,-4.8897942842515,335.528294349962));
#59472=CARTESIAN_POINT('Ctrl Pts',(82.5540670866375,-4.87513849098686,335.663945647655));
#59473=CARTESIAN_POINT('Ctrl Pts',(82.5462920078591,-4.85481046140537,335.799200973084));
#59474=CARTESIAN_POINT('Ctrl Pts',(82.5385169290807,-4.82883743807289,335.933548102224));
#59475=CARTESIAN_POINT('Ctrl Pts',(82.5307514180316,-4.80289637619914,336.067729908668));
#59476=CARTESIAN_POINT('Ctrl Pts',(82.5229859069826,-4.77132421564953,336.201005362415));
#59477=CARTESIAN_POINT('Ctrl Pts',(82.5152203959336,-4.73420000922789,336.332866585644));
#59478=CARTESIAN_POINT('Ctrl Pts',(82.5074625844114,-4.69711261156494,336.464597068086));
#59479=CARTESIAN_POINT('Ctrl Pts',(82.4997047728891,-4.65448422827802,336.594915736672));
#59480=CARTESIAN_POINT('Ctrl Pts',(82.4919469613669,-4.6064450209568,336.723324499739));
#59481=CARTESIAN_POINT('Ctrl Pts',(82.4841949878439,-4.55844196466258,336.851636631141));
#59482=CARTESIAN_POINT('Ctrl Pts',(82.4764430143209,-4.50503632549459,336.978041353209));
#59483=CARTESIAN_POINT('Ctrl Pts',(82.4686910407979,-4.44640809204299,337.102055694199));
#59484=CARTESIAN_POINT('Ctrl Pts',(82.4609423502403,-4.3878046876831,337.226017515042));
#59485=CARTESIAN_POINT('Ctrl Pts',(82.4531936596826,-4.3239832548095,337.347590615617));
#59486=CARTESIAN_POINT('Ctrl Pts',(82.445444969125,-4.25517182573731,337.46631218542));
#59487=CARTESIAN_POINT('Ctrl Pts',(82.4376978907472,-4.18637471345766,337.585009054209));
#59488=CARTESIAN_POINT('Ctrl Pts',(82.4299508123693,-4.1125898659386,337.700855234346));
#59489=CARTESIAN_POINT('Ctrl Pts',(82.4222037339915,-4.03409097718606,337.81341306073));
#59490=CARTESIAN_POINT('Ctrl Pts',(82.4144565906857,-3.95559143053722,337.925971830457));
#59491=CARTESIAN_POINT('Ctrl Pts',(82.4067094473799,-3.87237798744675,338.035241870854));
#59492=CARTESIAN_POINT('Ctrl Pts',(82.3989623040741,-3.78476709371294,338.140815357331));
#59493=CARTESIAN_POINT('Ctrl Pts',(82.391213419046,-3.69713650319018,338.24641257897));
#59494=CARTESIAN_POINT('Ctrl Pts',(82.3834645340179,-3.60510674430559,338.348311292231));
#59495=CARTESIAN_POINT('Ctrl Pts',(82.3757156489898,-3.50903361129608,338.446137863942));
#59496=CARTESIAN_POINT('Ctrl Pts',(82.3679585392151,-3.41285850527058,338.544068269787));
#59497=CARTESIAN_POINT('Ctrl Pts',(82.3602014294403,-3.31263172640043,338.637917620737));
#59498=CARTESIAN_POINT('Ctrl Pts',(82.3524443196656,-3.20874529969669,338.727349817789));
#59499=CARTESIAN_POINT('Ctrl Pts',(82.3446830647394,-3.10480335940817,338.816829804548));
#59500=CARTESIAN_POINT('Ctrl Pts',(82.3369218098133,-2.99719818106671,338.901887691862));
#59501=CARTESIAN_POINT('Ctrl Pts',(82.3291605548871,-2.8863529364766,338.982229248624));
#59502=CARTESIAN_POINT('Ctrl Pts',(82.3213868844824,-2.7753303756196,339.062699325693));
#59503=CARTESIAN_POINT('Ctrl Pts',(82.3136132140778,-2.66105771722564,339.138437779826));
#59504=CARTESIAN_POINT('Ctrl Pts',(82.3058395436731,-2.5439857818845,339.209194626537));
#59505=CARTESIAN_POINT('Ctrl Pts',(82.298427739496,-2.43236357329969,339.27665772501));
#59506=CARTESIAN_POINT('Ctrl Pts',(82.291015935319,-2.31819708756365,339.339592427523));
#59507=CARTESIAN_POINT('Ctrl Pts',(82.2836041311419,-2.20189427399635,339.397822719101));
#59508=CARTESIAN_POINT('Ctrl Pts',(82.2758290523635,-2.07989111308739,339.458907050729));
#59509=CARTESIAN_POINT('Ctrl Pts',(82.2680539735851,-1.95515136116017,339.515007194513));
#59510=CARTESIAN_POINT('Ctrl Pts',(82.2602788948066,-1.82812050083908,339.565868865497));
#59511=CARTESIAN_POINT('Ctrl Pts',(82.2525133837576,-1.70124596007879,339.616667947956));
#59512=CARTESIAN_POINT('Ctrl Pts',(82.2447478727086,-1.57208628003232,339.662241239954));
#59513=CARTESIAN_POINT('Ctrl Pts',(82.2369823616596,-1.44111132600204,339.702380376848));
#59514=CARTESIAN_POINT('Ctrl Pts',(82.2292245501373,-1.31026623401991,339.742479715672));
#59515=CARTESIAN_POINT('Ctrl Pts',(82.2214667386152,-1.17760982116692,339.777155507984));
#59516=CARTESIAN_POINT('Ctrl Pts',(82.213708927093,-1.04363138125204,339.806247663465));
#59517=CARTESIAN_POINT('Ctrl Pts',(82.20595695357,-0.909753764362079,339.835317926177));
#59518=CARTESIAN_POINT('Ctrl Pts',(82.1982049800469,-0.774556481079916,
339.858812833054));
#59519=CARTESIAN_POINT('Ctrl Pts',(82.1904530065239,-0.638543074803164,
339.876622376617));
#59520=CARTESIAN_POINT('Ctrl Pts',(82.1827043159663,-0.50258727028472,339.894424377828));
#59521=CARTESIAN_POINT('Ctrl Pts',(82.1749556254087,-0.365816416961941,
339.906545753938));
#59522=CARTESIAN_POINT('Ctrl Pts',(82.1672069348511,-0.228743103431238,
339.912927808866));
#59523=CARTESIAN_POINT('Ctrl Pts',(82.1594598564732,-0.0916983091482738,
339.919308535955));
#59524=CARTESIAN_POINT('Ctrl Pts',(82.1517127780954,0.0456484299654675,
339.91995229887));
#59525=CARTESIAN_POINT('Ctrl Pts',(82.1439656997175,0.182780960456905,339.914852407041));
#59526=CARTESIAN_POINT('Ctrl Pts',(82.1362185564117,0.319914640250844,339.909752472469));
#59527=CARTESIAN_POINT('Ctrl Pts',(82.128471413106,0.456833717237402,339.898908801666));
#59528=CARTESIAN_POINT('Ctrl Pts',(82.1207242698002,0.593023996038871,339.882366803367));
#59529=CARTESIAN_POINT('Ctrl Pts',(82.1129753847721,0.729244893306509,339.865821086076));
#59530=CARTESIAN_POINT('Ctrl Pts',(82.1052264997439,0.864736278400571,339.843574539154));
#59531=CARTESIAN_POINT('Ctrl Pts',(82.0974776147159,0.998991414537339,339.815724163216));
#59532=CARTESIAN_POINT('Ctrl Pts',(82.0897205049411,1.13338905046272,339.787844226601));
#59533=CARTESIAN_POINT('Ctrl Pts',(82.0819633951664,1.26654743292266,339.754348658879));
#59534=CARTESIAN_POINT('Ctrl Pts',(82.0742062853917,1.39797178186756,339.715385239787));
#59535=CARTESIAN_POINT('Ctrl Pts',(82.0664450304655,1.5294663597825,339.67640099989));
#59536=CARTESIAN_POINT('Ctrl Pts',(82.0586837755393,1.65922468823911,339.631943213213));
#59537=CARTESIAN_POINT('Ctrl Pts',(82.0509225206132,1.78677033947869,339.582208508619));
#59538=CARTESIAN_POINT('Ctrl Pts',(82.0431488502085,1.91452002219312,339.532394244706));
#59539=CARTESIAN_POINT('Ctrl Pts',(82.0353751798038,2.04004959650382,339.477286351766));
#59540=CARTESIAN_POINT('Ctrl Pts',(82.0276015093992,2.16290488023338,339.417128653499));
#59541=CARTESIAN_POINT('Ctrl Pts',(82.0201897052221,2.28004122094723,339.359771310561));
#59542=CARTESIAN_POINT('Ctrl Pts',(82.0127779010451,2.39474639124589,339.297823855792));
#59543=CARTESIAN_POINT('Ctrl Pts',(82.0053660968681,2.50665161159788,339.231534090678));
#59544=CARTESIAN_POINT('Ctrl Pts',(81.9975910180896,2.62404164014878,339.161995266709));
#59545=CARTESIAN_POINT('Ctrl Pts',(81.9898159393112,2.7387212852339,339.087457954934));
#59546=CARTESIAN_POINT('Ctrl Pts',(81.9820408605327,2.85023563699942,339.008159163017));
#59547=CARTESIAN_POINT('Ctrl Pts',(81.9742753494837,2.96161276325573,338.928957953312));
#59548=CARTESIAN_POINT('Ctrl Pts',(81.9665098384347,3.06983203081421,338.845007146155));
#59549=CARTESIAN_POINT('Ctrl Pts',(81.9587443273857,3.17446395032673,338.756589103239));
#59550=CARTESIAN_POINT('Ctrl Pts',(81.9509865158635,3.27899212698643,338.668258727071));
#59551=CARTESIAN_POINT('Ctrl Pts',(81.9432287043413,3.37993973733575,338.575470180319));
#59552=CARTESIAN_POINT('Ctrl Pts',(81.9354708928191,3.47690737305295,338.478548286528));
#59553=CARTESIAN_POINT('Ctrl Pts',(81.927718919296,3.57380203754919,338.381699329537));
#59554=CARTESIAN_POINT('Ctrl Pts',(81.919966945773,3.6667224135862,338.280723491965));
#59555=CARTESIAN_POINT('Ctrl Pts',(81.91221497225,3.75530349730259,338.175984682842));
#59556=CARTESIAN_POINT('Ctrl Pts',(81.9044662816924,3.84384706687744,338.071290230666));
#59557=CARTESIAN_POINT('Ctrl Pts',(81.8967175911348,3.9280547472896,337.962836274367));
#59558=CARTESIAN_POINT('Ctrl Pts',(81.8889689005771,4.0075997886505,337.851022096812));
#59559=CARTESIAN_POINT('Ctrl Pts',(81.8812218221993,4.08712828000118,337.73923118313));
#59560=CARTESIAN_POINT('Ctrl Pts',(81.8734747438215,4.16199583545949,337.624081757098));
#59561=CARTESIAN_POINT('Ctrl Pts',(81.8657276654436,4.23191750853067,337.506004242513));
#59562=CARTESIAN_POINT('Ctrl Pts',(81.8579805221378,4.30183976761282,337.387925738324));
#59563=CARTESIAN_POINT('Ctrl Pts',(81.850233378832,4.36681586246736,337.266919432964));
#59564=CARTESIAN_POINT('Ctrl Pts',(81.8424862355262,4.42660571764579,337.143442297568));
#59565=CARTESIAN_POINT('Ctrl Pts',(81.8347373504981,4.48640901485295,337.019937401891));
#59566=CARTESIAN_POINT('Ctrl Pts',(81.82698846547,4.54102358190525,336.893960922538));
#59567=CARTESIAN_POINT('Ctrl Pts',(81.8192395804419,4.59025676433914,336.765991477878));
#59568=CARTESIAN_POINT('Ctrl Pts',(81.8114824706671,4.6395422033816,336.637886205128));
#59569=CARTESIAN_POINT('Ctrl Pts',(81.8037253608924,4.68343470726242,336.507784106838));
#59570=CARTESIAN_POINT('Ctrl Pts',(81.7959682511177,4.72179079324202,336.376181226203));
#59571=CARTESIAN_POINT('Ctrl Pts',(81.7882069961915,4.76016737548755,336.244508021198));
#59572=CARTESIAN_POINT('Ctrl Pts',(81.7804457412653,4.7930015512644,336.111332815168));
#59573=CARTESIAN_POINT('Ctrl Pts',(81.7726844863391,4.82020084758153,335.97716265354));
#59574=CARTESIAN_POINT('Ctrl Pts',(81.7649108159345,4.84744365390854,335.842777863381));
#59575=CARTESIAN_POINT('Ctrl Pts',(81.7571371455298,4.86903350660446,335.707395323326));
#59576=CARTESIAN_POINT('Ctrl Pts',(81.7493634751252,4.88492965818476,335.571528911856));
#59577=CARTESIAN_POINT('Ctrl Pts',(81.7419516709481,4.90008584008457,335.441987114527));
#59578=CARTESIAN_POINT('Ctrl Pts',(81.734539866771,4.91006645320872,335.312005767375));
#59579=CARTESIAN_POINT('Ctrl Pts',(81.7271280625939,4.91488031134712,335.182029084578));
#59580=CARTESIAN_POINT('Ctrl Pts',(81.7193529838155,4.91993011101263,335.045681857377));
#59581=CARTESIAN_POINT('Ctrl Pts',(81.7115779050371,4.9193098316297,334.908908880891));
#59582=CARTESIAN_POINT('Ctrl Pts',(81.7038028262587,4.91297260017343,334.772220956967));
#59583=CARTESIAN_POINT('Ctrl Pts',(81.6960373152097,4.90664316708393,334.635701236235));
#59584=CARTESIAN_POINT('Ctrl Pts',(81.6882718041606,4.89461079762967,334.49926674654));
#59585=CARTESIAN_POINT('Ctrl Pts',(81.6805062931116,4.87688051445229,334.36343145675));
#59586=CARTESIAN_POINT('Ctrl Pts',(81.6727484815894,4.85916781090232,334.227730848045));
#59587=CARTESIAN_POINT('Ctrl Pts',(81.6649906700672,4.83576848671471,334.092628642027));
#59588=CARTESIAN_POINT('Ctrl Pts',(81.6572328585451,4.80673955017657,333.958636490332));
#59589=CARTESIAN_POINT('Ctrl Pts',(81.6494808850221,4.77773245883373,333.82474517198));
#59590=CARTESIAN_POINT('Ctrl Pts',(81.641728911499,4.74310427003886,333.691962625699));
#59591=CARTESIAN_POINT('Ctrl Pts',(81.633976937976,4.70296347812297,333.560792723079));
#59592=CARTESIAN_POINT('Ctrl Pts',(81.6262282474184,4.66283968585629,333.429678370991));
#59593=CARTESIAN_POINT('Ctrl Pts',(81.6184795568608,4.61720804794689,333.3001756772));
#59594=CARTESIAN_POINT('Ctrl Pts',(81.6107308663032,4.56622750676396,333.17277548753));
#59595=CARTESIAN_POINT('Ctrl Pts',(81.6029837879254,4.51525757250842,333.045401804533));
#59596=CARTESIAN_POINT('Ctrl Pts',(81.5952367095475,4.4589410937105,332.92013011822));
#59597=CARTESIAN_POINT('Ctrl Pts',(81.5874896311697,4.39748582202621,332.797432973193));
#59598=CARTESIAN_POINT('Ctrl Pts',(81.5797424878639,4.33603003528759,332.674734799845));
#59599=CARTESIAN_POINT('Ctrl Pts',(81.5719953445581,4.26943554480757,332.554611560308));
#59600=CARTESIAN_POINT('Ctrl Pts',(81.5642482012523,4.19795670876241,332.437512432448));
#59601=CARTESIAN_POINT('Ctrl Pts',(81.5564993162242,4.12646180275742,332.320386978219));
#59602=CARTESIAN_POINT('Ctrl Pts',(81.5487504311962,4.05008056969389,332.206287322127));
#59603=CARTESIAN_POINT('Ctrl Pts',(81.5410015461681,3.96911123358604,332.095634479284));
#59604=CARTESIAN_POINT('Ctrl Pts',(81.5332444363934,3.88805595578816,331.984864188371));
#59605=CARTESIAN_POINT('Ctrl Pts',(81.5254873266186,3.80240307813069,331.87754833481));
#59606=CARTESIAN_POINT('Ctrl Pts',(81.5177302168439,3.7124920871764,331.774076013736));
#59607=CARTESIAN_POINT('Ctrl Pts',(81.5099689619178,3.62253305066339,331.670548400362));
#59608=CARTESIAN_POINT('Ctrl Pts',(81.5022077069916,3.52831163528186,331.57086869589));
#59609=CARTESIAN_POINT('Ctrl Pts',(81.4944464520654,3.43020418390745,331.475389054207));
#59610=CARTESIAN_POINT('Ctrl Pts',(81.4866727816608,3.33193979258399,331.379756676214));
#59611=CARTESIAN_POINT('Ctrl Pts',(81.4788991112561,3.22977723451189,331.288338047811));
#59612=CARTESIAN_POINT('Ctrl Pts',(81.4711254408515,3.12412659026461,331.201445523557));
#59613=CARTESIAN_POINT('Ctrl Pts',(81.4637136366744,3.02339400892483,331.118597867213));
#59614=CARTESIAN_POINT('Ctrl Pts',(81.4563018324972,2.91949100352308,331.039864591438));
#59615=CARTESIAN_POINT('Ctrl Pts',(81.4488900283201,2.81279589288573,330.965478674308));
#59616=CARTESIAN_POINT('Ctrl Pts',(81.4411149495417,2.70087133704788,330.887446881795));
#59617=CARTESIAN_POINT('Ctrl Pts',(81.4333398707633,2.58552035443142,330.813952782353));
#59618=CARTESIAN_POINT('Ctrl Pts',(81.4255647919848,2.46714712352351,330.745312216697));
#59619=CARTESIAN_POINT('Ctrl Pts',(81.4177992809358,2.34891955841233,330.676756117626));
#59620=CARTESIAN_POINT('Ctrl Pts',(81.4100337698868,2.2276774797962,330.613041862816));
#59621=CARTESIAN_POINT('Ctrl Pts',(81.4022682588378,2.10385581310242,330.554443366667));
#59622=CARTESIAN_POINT('Ctrl Pts',(81.3945104473156,1.98015691595166,330.495902971096));
#59623=CARTESIAN_POINT('Ctrl Pts',(81.3867526357934,1.85388387166077,330.442468406169));
#59624=CARTESIAN_POINT('Ctrl Pts',(81.3789948242712,1.72549778946204,330.394368616459));
#59625=CARTESIAN_POINT('Ctrl Pts',(81.3712428507482,1.59720832186153,330.346305023365));
#59626=CARTESIAN_POINT('Ctrl Pts',(81.3634908772251,1.46680934598065,330.30356835123));
#59627=CARTESIAN_POINT('Ctrl Pts',(81.3557389037021,1.3347832906966,330.266340038683));
#59628=CARTESIAN_POINT('Ctrl Pts',(81.3479902131445,1.20281314852534,330.229127492349));
#59629=CARTESIAN_POINT('Ctrl Pts',(81.3402415225869,1.06921767288196,330.197418771702));
#59630=CARTESIAN_POINT('Ctrl Pts',(81.3324928320293,0.934495639327215,330.171345843552));
#59631=CARTESIAN_POINT('Ctrl Pts',(81.3247457536514,0.799801635816768,330.145278340094));
#59632=CARTESIAN_POINT('Ctrl Pts',(81.3169986752736,0.663981924125593,330.124844371023));
#59633=CARTESIAN_POINT('Ctrl Pts',(81.3092515968957,0.527546303432146,330.110124954538));
#59634=CARTESIAN_POINT('Ctrl Pts',(81.3015044535899,0.391109539276879,330.09540541469));
#59635=CARTESIAN_POINT('Ctrl Pts',(81.2937573102841,0.254057244442737,330.086400564882));
#59636=CARTESIAN_POINT('Ctrl Pts',(81.2860101669783,0.116904789986733,330.083139585815));
#59637=CARTESIAN_POINT('Ctrl Pts',(81.2782612819502,-0.0202784992528622,
330.079877873611));
#59638=CARTESIAN_POINT('Ctrl Pts',(81.2705123969221,-0.157561602235148,
330.082362611068));
#59639=CARTESIAN_POINT('Ctrl Pts',(81.262763511894,-0.294429092244181,330.090570850685));
#59640=CARTESIAN_POINT('Ctrl Pts',(81.2550064021193,-0.431441854821215,
330.098787802613));
#59641=CARTESIAN_POINT('Ctrl Pts',(81.2472492923446,-0.568037732425112,
330.112740368615));
#59642=CARTESIAN_POINT('Ctrl Pts',(81.2394921825698,-0.703705810998619,
330.132353628902));
#59643=CARTESIAN_POINT('Ctrl Pts',(81.2317309276437,-0.839446386255491,
330.151977369887));
#59644=CARTESIAN_POINT('Ctrl Pts',(81.2239696727174,-0.974257790605692,
330.177267760498));
#59645=CARTESIAN_POINT('Ctrl Pts',(81.2162084177913,-1.10764022960908,330.208098896654));
#59646=CARTESIAN_POINT('Ctrl Pts',(81.2084347473866,-1.24123603704555,330.23897935258));
#59647=CARTESIAN_POINT('Ctrl Pts',(81.200661076982,-1.37339793425984,330.275418161776));
#59648=CARTESIAN_POINT('Ctrl Pts',(81.1928874065773,-1.50364133750999,330.317239511716));
#59649=CARTESIAN_POINT('Ctrl Pts',(81.1854756024003,-1.62782187900365,330.357114067755));
#59650=CARTESIAN_POINT('Ctrl Pts',(81.1780637982232,-1.75025824847928,330.401881228434));
#59651=CARTESIAN_POINT('Ctrl Pts',(81.1706519940461,-1.87054979967704,330.451348935187));
#59652=CARTESIAN_POINT('Ctrl Pts',(81.1628769152677,-1.99673719812966,330.503241201605));
#59653=CARTESIAN_POINT('Ctrl Pts',(81.1551018364893,-2.12096298981029,330.560470429493));
#59654=CARTESIAN_POINT('Ctrl Pts',(81.1473267577108,-2.24274285335172,330.622867656074));
#59655=CARTESIAN_POINT('Ctrl Pts',(81.1395612466618,-2.36437285901802,330.685188098896));
#59656=CARTESIAN_POINT('Ctrl Pts',(81.1317957356128,-2.4835625807801,330.752663710189));
#59657=CARTESIAN_POINT('Ctrl Pts',(81.1240302245638,-2.59984631507018,330.825076982684));
#59658=CARTESIAN_POINT('Ctrl Pts',(81.1162724130417,-2.71601475369908,330.897418457208));
#59659=CARTESIAN_POINT('Ctrl Pts',(81.1085146015194,-2.82928260913446,330.974687644912));
#59660=CARTESIAN_POINT('Ctrl Pts',(81.1007567899973,-2.93920782433534,331.056620684252));
#59661=CARTESIAN_POINT('Ctrl Pts',(81.0930048164743,-3.04905031732592,331.138492066382));
#59662=CARTESIAN_POINT('Ctrl Pts',(81.0852528429512,-3.15555486481261,331.225020081618));
#59663=CARTESIAN_POINT('Ctrl Pts',(81.0775008694282,-3.25830782123197,331.31589723208));
#59664=CARTESIAN_POINT('Ctrl Pts',(81.0697521788706,-3.36101726171337,331.406735896014));
#59665=CARTESIAN_POINT('Ctrl Pts',(81.062003488313,-3.45997797895877,331.501919773429));
#59666=CARTESIAN_POINT('Ctrl Pts',(81.0542547977554,-3.5548090831861,331.601100848128));
#59667=CARTESIAN_POINT('Ctrl Pts',(81.0465077193775,-3.64962045701014,331.700261287376));
#59668=CARTESIAN_POINT('Ctrl Pts',(81.0387606409997,-3.74030365687123,331.803416987358));
#59669=CARTESIAN_POINT('Ctrl Pts',(81.0310135626219,-3.82651467124989,331.910183090665));
#59670=CARTESIAN_POINT('Ctrl Pts',(81.0232664193161,-3.91272640815977,332.016950088776));
#59671=CARTESIAN_POINT('Ctrl Pts',(81.0155192760103,-3.99446563926721,332.127327246455));
#59672=CARTESIAN_POINT('Ctrl Pts',(81.0077721327045,-4.07142892904662,332.240896968538));
#59673=CARTESIAN_POINT('Ctrl Pts',(81.0000232476764,-4.14840952180764,332.354492223506));
#59674=CARTESIAN_POINT('Ctrl Pts',(80.9922743626483,-4.22061181739706,332.471281147623));
#59675=CARTESIAN_POINT('Ctrl Pts',(80.9845254776202,-4.28777618588676,332.590817889357));
#59676=CARTESIAN_POINT('Ctrl Pts',(80.9767683678455,-4.35501184333107,332.710481508624));
#59677=CARTESIAN_POINT('Ctrl Pts',(80.9690112580707,-4.41719870015613,332.832898430308));
#59678=CARTESIAN_POINT('Ctrl Pts',(80.961254148296,-4.47412327309949,332.957598472482));
#59679=CARTESIAN_POINT('Ctrl Pts',(80.9534928933698,-4.53107826471449,333.082365150371));
#59680=CARTESIAN_POINT('Ctrl Pts',(80.9457316384437,-4.58276522207415,333.209417017885));
#59681=CARTESIAN_POINT('Ctrl Pts',(80.9379703835175,-4.62901955315457,333.338265653297));
#59682=CARTESIAN_POINT('Ctrl Pts',(80.9301967131129,-4.67534787609051,333.467320404534));
#59683=CARTESIAN_POINT('Ctrl Pts',(80.9224230427082,-4.71622609007985,333.598177293966));
#59684=CARTESIAN_POINT('Ctrl Pts',(80.9146493723035,-4.75153980355969,333.730333682542));
#59685=CARTESIAN_POINT('Ctrl Pts',(80.9072375681264,-4.78520965518101,333.856338159434));
#59686=CARTESIAN_POINT('Ctrl Pts',(80.8998257639494,-4.81382133962133,333.983523593974));
#59687=CARTESIAN_POINT('Ctrl Pts',(80.8924139597723,-4.83731955034643,334.111449140265));
#59688=CARTESIAN_POINT('Ctrl Pts',(80.8806823481055,-4.87451317776904,334.313933285217));
#59689=CARTESIAN_POINT('Ctrl Pts',(80.8689507364387,-4.89900138445584,334.518817720643));
#59690=CARTESIAN_POINT('Ctrl Pts',(80.8572191247719,-4.91054538093032,334.724814382055));
#59691=CARTESIAN_POINT('Ctrl Pts',(80.8520852086841,-4.91559719400601,334.814961380104));
#59692=CARTESIAN_POINT('Ctrl Pts',(80.8469512925964,-4.91817063490177,334.905321049511));
#59693=CARTESIAN_POINT('Ctrl Pts',(80.8418173765086,-4.91824819243862,334.995783357466));
#59694=CARTESIAN_POINT('',(79.0918173765422,-4.91824993919102,334.999226600024));
#59695=CARTESIAN_POINT('Ctrl Pts',(80.8418173764667,-4.91824819243925,334.995783358204));
#59696=CARTESIAN_POINT('Ctrl Pts',(80.8341698505714,-4.91836372279806,335.13053679609));
#59697=CARTESIAN_POINT('Ctrl Pts',(80.8265223246761,-4.91293699669705,335.265481447406));
#59698=CARTESIAN_POINT('Ctrl Pts',(80.8188747987808,-4.90194758541068,335.40011614862));
#59699=CARTESIAN_POINT('Ctrl Pts',(80.8112341391248,-4.89096804083545,335.534629969682));
#59700=CARTESIAN_POINT('Ctrl Pts',(80.8035934794689,-4.87443577773073,335.668833994355));
#59701=CARTESIAN_POINT('Ctrl Pts',(80.795952819813,-4.85238242166092,335.802226836036));
#59702=CARTESIAN_POINT('Ctrl Pts',(80.7883167226616,-4.83034223441963,335.935540024196));
#59703=CARTESIAN_POINT('Ctrl Pts',(80.7806806255102,-4.80278757642534,336.068042595841));
#59704=CARTESIAN_POINT('Ctrl Pts',(80.7730445283588,-4.7698018844825,336.199238527269));
#59705=CARTESIAN_POINT('Ctrl Pts',(80.7654107919207,-4.736826390126,336.330393899238));
#59706=CARTESIAN_POINT('Ctrl Pts',(80.7577770554825,-4.69842329769821,336.460243043088));
#59707=CARTESIAN_POINT('Ctrl Pts',(80.7501433190444,-4.65472700459329,336.588300845309));
#59708=CARTESIAN_POINT('Ctrl Pts',(80.742510176465,-4.61103411079685,336.716348685404));
#59709=CARTESIAN_POINT('Ctrl Pts',(80.7348770338855,-4.56204896545517,336.842605079102));
#59710=CARTESIAN_POINT('Ctrl Pts',(80.7272438913061,-4.50795544427893,336.966601325865));
#59711=CARTESIAN_POINT('Ctrl Pts',(80.719609576422,-4.4538536153722,337.090616616081));
#59712=CARTESIAN_POINT('Ctrl Pts',(80.7119752615378,-4.39464201242001,337.21237069951));
#59713=CARTESIAN_POINT('Ctrl Pts',(80.7043409466537,-4.33055189833831,337.331416590466));
#59714=CARTESIAN_POINT('Ctrl Pts',(80.6966990581132,-4.26639820337179,337.450580581431));
#59715=CARTESIAN_POINT('Ctrl Pts',(80.6890571695728,-4.19735652282173,337.56703065818));
#59716=CARTESIAN_POINT('Ctrl Pts',(80.6814152810324,-4.12370334954556,337.680345826092));
#59717=CARTESIAN_POINT('Ctrl Pts',(80.6737695893461,-4.05001352122601,337.793717387668));
#59718=CARTESIAN_POINT('Ctrl Pts',(80.6661238976599,-3.97170786410445,337.903950605303));
#59719=CARTESIAN_POINT('Ctrl Pts',(80.6584782059736,-3.88910434817903,338.010656146337));
#59720=CARTESIAN_POINT('Ctrl Pts',(80.6508204953826,-3.80637098085045,338.11752942677));
#59721=CARTESIAN_POINT('Ctrl Pts',(80.6431627847916,-3.71932651827659,338.220863644361));
#59722=CARTESIAN_POINT('Ctrl Pts',(80.6355050742006,-3.62832755438684,338.320304537324));
#59723=CARTESIAN_POINT('Ctrl Pts',(80.6283953579665,-3.54384057839536,338.412629328479));
#59724=CARTESIAN_POINT('Ctrl Pts',(80.6212856417323,-3.45594540280672,338.501598298593));
#59725=CARTESIAN_POINT('Ctrl Pts',(80.6141759254982,-3.36495254838263,338.586959354332));
#59726=CARTESIAN_POINT('Ctrl Pts',(80.6064008467198,-3.26544413086962,338.680308921478));
#59727=CARTESIAN_POINT('Ctrl Pts',(80.5986257679414,-3.16189101140127,338.769662059598));
#59728=CARTESIAN_POINT('Ctrl Pts',(80.5908506891629,-3.05464762309989,338.854647968517));
#59729=CARTESIAN_POINT('Ctrl Pts',(80.5830851781139,-2.94753620461541,338.939529296864));
#59730=CARTESIAN_POINT('Ctrl Pts',(80.5753196670649,-2.83674385622295,339.020053848591));
#59731=CARTESIAN_POINT('Ctrl Pts',(80.5675541560159,-2.7226614801003,339.095887880213));
#59732=CARTESIAN_POINT('Ctrl Pts',(80.5597963444937,-2.60869221698587,339.171646722172));
#59733=CARTESIAN_POINT('Ctrl Pts',(80.5520385329716,-2.49143974126989,339.242724084123));
#59734=CARTESIAN_POINT('Ctrl Pts',(80.5442807214494,-2.37132734738739,339.308826948722));
#59735=CARTESIAN_POINT('Ctrl Pts',(80.5365287479264,-2.25130534188994,339.37488006882));
#59736=CARTESIAN_POINT('Ctrl Pts',(80.5287767744033,-2.12842804309528,339.435965955054));
#59737=CARTESIAN_POINT('Ctrl Pts',(80.5210248008803,-2.0031466898809,339.491835526967));
#59738=CARTESIAN_POINT('Ctrl Pts',(80.5132761103227,-1.87791839339408,339.547681438083));
#59739=CARTESIAN_POINT('Ctrl Pts',(80.5055274197651,-1.75028842369582,339.598315269779));
#59740=CARTESIAN_POINT('Ctrl Pts',(80.4977787292075,-1.62073132643303,339.643534540629));
#59741=CARTESIAN_POINT('Ctrl Pts',(80.4900316508297,-1.49120118460641,339.688744403233));
#59742=CARTESIAN_POINT('Ctrl Pts',(80.4822845724519,-1.35974508155288,339.728541817041));
#59743=CARTESIAN_POINT('Ctrl Pts',(80.474537494074,-1.22685581507096,339.762773128286));
#59744=CARTESIAN_POINT('Ctrl Pts',(80.4667903507682,-1.09396543484927,339.797004726423));
#59745=CARTESIAN_POINT('Ctrl Pts',(80.4590432074624,-0.959642245759653,
339.825670031447));
#59746=CARTESIAN_POINT('Ctrl Pts',(80.4512960641566,-0.824392031065007,
339.848665882654));
#59747=CARTESIAN_POINT('Ctrl Pts',(80.4435471791285,-0.68911140925047,339.871666903818));
#59748=CARTESIAN_POINT('Ctrl Pts',(80.4357982941005,-0.552903732377097,
339.888995869321));
#59749=CARTESIAN_POINT('Ctrl Pts',(80.4280494090724,-0.416282352457188,
339.900601194296));
#59750=CARTESIAN_POINT('Ctrl Pts',(80.4202922992977,-0.279515961193069,
339.912218837282));
#59751=CARTESIAN_POINT('Ctrl Pts',(80.4125351895229,-0.14233537980844,339.918100670958));
#59752=CARTESIAN_POINT('Ctrl Pts',(80.4047780797482,-0.00525698597878473,
339.918247190473));
#59753=CARTESIAN_POINT('Ctrl Pts',(80.397016824822,0.131894658161522,339.918393788284));
#59754=CARTESIAN_POINT('Ctrl Pts',(80.3892555698958,0.268943615589085,339.912798981042));
#59755=CARTESIAN_POINT('Ctrl Pts',(80.3814943149697,0.405377163339688,339.901515318546));
#59756=CARTESIAN_POINT('Ctrl Pts',(80.373720644565,0.542028960303195,339.890213605868));
#59757=CARTESIAN_POINT('Ctrl Pts',(80.3659469741604,0.678062992298923,339.873204901333));
#59758=CARTESIAN_POINT('Ctrl Pts',(80.3581733037557,0.812974394503769,339.850593334468));
#59759=CARTESIAN_POINT('Ctrl Pts',(80.3507614995787,0.941605638478082,339.82903434148));
#59760=CARTESIAN_POINT('Ctrl Pts',(80.3433496954016,1.06921613569124,339.802382432603));
#59761=CARTESIAN_POINT('Ctrl Pts',(80.3359378912245,1.19538174061244,339.770769912363));
#59762=CARTESIAN_POINT('Ctrl Pts',(80.3281628124461,1.32773109765877,339.737607968337));
#59763=CARTESIAN_POINT('Ctrl Pts',(80.3203877336676,1.45890859258986,339.698882051086));
#59764=CARTESIAN_POINT('Ctrl Pts',(80.3126126548892,1.5884106075289,339.654689549733));
#59765=CARTESIAN_POINT('Ctrl Pts',(80.3048471438402,1.71775326199432,339.610551430066));
#59766=CARTESIAN_POINT('Ctrl Pts',(80.2970816327911,1.84542417243659,339.560960236089));
#59767=CARTESIAN_POINT('Ctrl Pts',(80.2893161217421,1.97093114724105,339.506064078033));
#59768=CARTESIAN_POINT('Ctrl Pts',(80.2815583102199,2.09631368151451,339.451222349677));
#59769=CARTESIAN_POINT('Ctrl Pts',(80.2738004986978,2.21953619410375,339.391086280345));
#59770=CARTESIAN_POINT('Ctrl Pts',(80.2660426871756,2.34012321156602,339.32585325886));
#59771=CARTESIAN_POINT('Ctrl Pts',(80.2582907136526,2.4606194834732,339.260669327292));
#59772=CARTESIAN_POINT('Ctrl Pts',(80.2505387401296,2.57848386549279,339.190396263413));
#59773=CARTESIAN_POINT('Ctrl Pts',(80.2427867666066,2.69326270930591,339.115278731892));
#59774=CARTESIAN_POINT('Ctrl Pts',(80.2350380760489,2.80799294421092,339.04019301269));
#59775=CARTESIAN_POINT('Ctrl Pts',(80.2272893854913,2.91963991351983,338.960267120005));
#59776=CARTESIAN_POINT('Ctrl Pts',(80.2195406949337,3.02777654240234,338.875790535075));
#59777=CARTESIAN_POINT('Ctrl Pts',(80.2117936165558,3.13589067255604,338.791331526205));
#59778=CARTESIAN_POINT('Ctrl Pts',(80.204046538178,3.24049560718018,338.702323948841));
#59779=CARTESIAN_POINT('Ctrl Pts',(80.1962994598002,3.34119545437707,338.609099056295));
#59780=CARTESIAN_POINT('Ctrl Pts',(80.1885523164944,3.44189614553567,338.515873382435));
#59781=CARTESIAN_POINT('Ctrl Pts',(80.1808051731885,3.5386913971573,338.418430588433));
#59782=CARTESIAN_POINT('Ctrl Pts',(80.1730580298827,3.63122075086015,338.317140172049));
#59783=CARTESIAN_POINT('Ctrl Pts',(80.1653091448545,3.72377090712654,338.215826983429));
#59784=CARTESIAN_POINT('Ctrl Pts',(80.1575602598264,3.81205299346731,338.110664739652));
#59785=CARTESIAN_POINT('Ctrl Pts',(80.1498113747983,3.89574582683509,338.002057213845));
#59786=CARTESIAN_POINT('Ctrl Pts',(80.1420542650236,3.97952749264052,337.893334410888));
#59787=CARTESIAN_POINT('Ctrl Pts',(80.1342971552488,4.05870993606958,337.781159331084));
#59788=CARTESIAN_POINT('Ctrl Pts',(80.126540045474,4.13301413191363,337.66596647539));
#59789=CARTESIAN_POINT('Ctrl Pts',(80.1187787905479,4.20735803354424,337.550712064317));
#59790=CARTESIAN_POINT('Ctrl Pts',(80.1110175356217,4.27681829550603,337.432437000976));
#59791=CARTESIAN_POINT('Ctrl Pts',(80.1032562806955,4.34116164423035,337.311600882757));
#59792=CARTESIAN_POINT('Ctrl Pts',(80.0954826102908,4.40560792134309,337.19057146613));
#59793=CARTESIAN_POINT('Ctrl Pts',(80.0877089398862,4.46492075917881,337.066973160483));
#59794=CARTESIAN_POINT('Ctrl Pts',(80.0799352694815,4.51891451115269,336.941286867878));
#59795=CARTESIAN_POINT('Ctrl Pts',(80.0725234653044,4.57039484098189,336.821451302432));
#59796=CARTESIAN_POINT('Ctrl Pts',(80.0651116611273,4.61704004454493,336.699718035696));
#59797=CARTESIAN_POINT('Ctrl Pts',(80.0576998569503,4.65873185005497,336.576515338265));
#59798=CARTESIAN_POINT('Ctrl Pts',(80.0499247781718,4.70246709514666,336.44727410963));
#59799=CARTESIAN_POINT('Ctrl Pts',(80.0421496993934,4.74088931461903,336.316007339676));
#59800=CARTESIAN_POINT('Ctrl Pts',(80.0343746206149,4.77380786853292,336.183191234261));
#59801=CARTESIAN_POINT('Ctrl Pts',(80.0266091095659,4.80668591407045,336.050538567521));
#59802=CARTESIAN_POINT('Ctrl Pts',(80.018843598517,4.83407367646886,335.916340734588));
#59803=CARTESIAN_POINT('Ctrl Pts',(80.011078087468,4.85582935165667,335.781091780836));
#59804=CARTESIAN_POINT('Ctrl Pts',(80.0033202759458,4.8775634560292,335.645976926816));
#59805=CARTESIAN_POINT('Ctrl Pts',(79.9955624644236,4.89367652444947,335.50981340942));
#59806=CARTESIAN_POINT('Ctrl Pts',(79.9878046529014,4.90407723942746,335.37310788283));
#59807=CARTESIAN_POINT('Ctrl Pts',(79.9800526793784,4.9144701275376,335.236505231483));
#59808=CARTESIAN_POINT('Ctrl Pts',(79.9723007058554,4.91915918907855,335.099361770983));
#59809=CARTESIAN_POINT('Ctrl Pts',(79.9645487323324,4.91810467265646,334.962191385972));
#59810=CARTESIAN_POINT('Ctrl Pts',(79.9568000417748,4.9170506028227,334.825079092701));
#59811=CARTESIAN_POINT('Ctrl Pts',(79.9490513512172,4.91025779591392,334.687940287647));
#59812=CARTESIAN_POINT('Ctrl Pts',(79.9413026606595,4.8977385681846,334.551290762055));
#59813=CARTESIAN_POINT('Ctrl Pts',(79.9335555822817,4.88522194518518,334.414669667539));
#59814=CARTESIAN_POINT('Ctrl Pts',(79.9258085039039,4.86698130684158,334.278538039));
#59815=CARTESIAN_POINT('Ctrl Pts',(79.9180614255261,4.8430809713081,334.143408050555));
#59816=CARTESIAN_POINT('Ctrl Pts',(79.9103142822203,4.81918043546678,334.008276929591));
#59817=CARTESIAN_POINT('Ctrl Pts',(79.9025671389144,4.78962017590249,333.874147850366));
#59818=CARTESIAN_POINT('Ctrl Pts',(79.8948199956086,4.75451584645112,333.741523886462));
#59819=CARTESIAN_POINT('Ctrl Pts',(79.8870711105805,4.71940362480125,333.608870105876));
#59820=CARTESIAN_POINT('Ctrl Pts',(79.8793222255525,4.6787449530155,333.477722491741));
#59821=CARTESIAN_POINT('Ctrl Pts',(79.8715733405244,4.63270556195336,333.348569638542));
#59822=CARTESIAN_POINT('Ctrl Pts',(79.8638162307497,4.58661730420578,333.219279701169));
#59823=CARTESIAN_POINT('Ctrl Pts',(79.856059120975,4.53513705007532,333.09198912292));
#59824=CARTESIAN_POINT('Ctrl Pts',(79.8483020112002,4.47847918413576,332.967167675443));
#59825=CARTESIAN_POINT('Ctrl Pts',(79.8405407562741,4.42179104204433,332.842279527377));
#59826=CARTESIAN_POINT('Ctrl Pts',(79.8327795013479,4.3599199513697,332.719863487828));
#59827=CARTESIAN_POINT('Ctrl Pts',(79.8250182464218,4.29312615964964,332.600364436038));
#59828=CARTESIAN_POINT('Ctrl Pts',(79.8172445760171,4.22622551963082,332.480674224709));
#59829=CARTESIAN_POINT('Ctrl Pts',(79.8094709056124,4.15438664748084,332.363910658734));
#59830=CARTESIAN_POINT('Ctrl Pts',(79.8016972352078,4.0779134799839,332.250490095987));
#59831=CARTESIAN_POINT('Ctrl Pts',(79.7942854310307,4.00500015683201,332.142349287722));
#59832=CARTESIAN_POINT('Ctrl Pts',(79.7868736268535,3.927874451917,332.037247485229));
#59833=CARTESIAN_POINT('Ctrl Pts',(79.7794618226764,3.84683250346912,331.935515907571));
#59834=CARTESIAN_POINT('Ctrl Pts',(79.771686743898,3.76181844771666,331.828798162248));
#59835=CARTESIAN_POINT('Ctrl Pts',(79.7639116651196,3.67222588803154,331.725452116884));
#59836=CARTESIAN_POINT('Ctrl Pts',(79.7561365863412,3.57835210987057,331.625895786985));
#59837=CARTESIAN_POINT('Ctrl Pts',(79.7483710752922,3.48459384936992,331.526461967488));
#59838=CARTESIAN_POINT('Ctrl Pts',(79.7406055642432,3.38656511841448,331.430808866125));
#59839=CARTESIAN_POINT('Ctrl Pts',(79.7328400531942,3.28460463197932,331.339323085264));
#59840=CARTESIAN_POINT('Ctrl Pts',(79.7250822416719,3.18274523966296,331.247928012821));
#59841=CARTESIAN_POINT('Ctrl Pts',(79.7173244301497,3.07696213885331,331.160692297505));
#59842=CARTESIAN_POINT('Ctrl Pts',(79.7095666186275,2.96763196872582,331.077966909791));
#59843=CARTESIAN_POINT('Ctrl Pts',(79.7018146451045,2.85838407301878,330.995303775554));
#59844=CARTESIAN_POINT('Ctrl Pts',(79.6940626715815,2.74559473151516,330.917144447901));
#59845=CARTESIAN_POINT('Ctrl Pts',(79.6863106980585,2.62967456901354,330.843800447093));
#59846=CARTESIAN_POINT('Ctrl Pts',(79.6785620075008,2.5138034987694,330.770487507513));
#59847=CARTESIAN_POINT('Ctrl Pts',(79.6708133169432,2.39480457428145,330.701986047323));
#59848=CARTESIAN_POINT('Ctrl Pts',(79.6630646263856,2.27311820044396,330.638564833761));
#59849=CARTESIAN_POINT('Ctrl Pts',(79.6553175480078,2.15145714447315,330.575156815512));
#59850=CARTESIAN_POINT('Ctrl Pts',(79.6475704696299,2.02711009773855,330.516827122008));
#59851=CARTESIAN_POINT('Ctrl Pts',(79.6398233912521,1.90054256462559,330.463798833545));
#59852=CARTESIAN_POINT('Ctrl Pts',(79.6320762479463,1.77397397075462,330.410770100654));
#59853=CARTESIAN_POINT('Ctrl Pts',(79.6243291046405,1.64518521389786,330.363043012468));
#59854=CARTESIAN_POINT('Ctrl Pts',(79.6165819613347,1.51466192629075,330.320792555192));
#59855=CARTESIAN_POINT('Ctrl Pts',(79.6088330763065,1.38410929427714,330.278532599116));
#59856=CARTESIAN_POINT('Ctrl Pts',(79.6010841912784,1.25182172734155,330.241751844379));
#59857=CARTESIAN_POINT('Ctrl Pts',(79.5933353062503,1.11829978148675,330.210575330875));
#59858=CARTESIAN_POINT('Ctrl Pts',(79.5855781964755,0.984636114059443,330.179365726297));
#59859=CARTESIAN_POINT('Ctrl Pts',(79.5778210867008,0.849735831737591,330.153772334456));
#59860=CARTESIAN_POINT('Ctrl Pts',(79.5700639769261,0.714109991318342,330.133869095185));
#59861=CARTESIAN_POINT('Ctrl Pts',(79.5623027219999,0.578411676786446,330.113955220259));
#59862=CARTESIAN_POINT('Ctrl Pts',(79.5545414670737,0.44198742017157,330.099737597138));
#59863=CARTESIAN_POINT('Ctrl Pts',(79.5467802121476,0.305352164793701,330.091238127801));
#59864=CARTESIAN_POINT('Ctrl Pts',(79.5390065417429,0.168498337536831,330.082725062083));
#59865=CARTESIAN_POINT('Ctrl Pts',(79.5312328713382,0.0314332280332238,
330.079948436848));
#59866=CARTESIAN_POINT('Ctrl Pts',(79.5234592009336,-0.105328561864645,
330.082877980306));
#59867=CARTESIAN_POINT('Ctrl Pts',(79.5160473967565,-0.235724057538847,
330.085671152812));
#59868=CARTESIAN_POINT('Ctrl Pts',(79.5086355925795,-0.36584354990371,330.093651187411));
#59869=CARTESIAN_POINT('Ctrl Pts',(79.5012237884025,-0.495248252394823,
330.106748296787));
#59870=CARTESIAN_POINT('Ctrl Pts',(79.4934487096241,-0.630995464833271,
330.120487334507));
#59871=CARTESIAN_POINT('Ctrl Pts',(79.4856736308456,-0.766385034037335,
330.139901154179));
#59872=CARTESIAN_POINT('Ctrl Pts',(79.4778985520672,-0.900904563630016,
330.164965974294));
#59873=CARTESIAN_POINT('Ctrl Pts',(79.4701330410182,-1.03525855837696,330.189999950553));
#59874=CARTESIAN_POINT('Ctrl Pts',(79.4623675299692,-1.16874426319003,330.220671020043));
#59875=CARTESIAN_POINT('Ctrl Pts',(79.4546020189202,-1.30085327778081,330.256903562841));
#59876=CARTESIAN_POINT('Ctrl Pts',(79.446844207398,-1.43283130589927,330.293100180968));
#59877=CARTESIAN_POINT('Ctrl Pts',(79.4390863958758,-1.56343498568158,330.33484719608));
#59878=CARTESIAN_POINT('Ctrl Pts',(79.4313285843536,-1.69216535749892,330.382017814523));
#59879=CARTESIAN_POINT('Ctrl Pts',(79.4235766108306,-1.82079885562928,330.42915293558));
#59880=CARTESIAN_POINT('Ctrl Pts',(79.4158246373075,-1.94756148624772,330.481703402131));
#59881=CARTESIAN_POINT('Ctrl Pts',(79.4080726637845,-2.07196907268009,330.539492492512));
#59882=CARTESIAN_POINT('Ctrl Pts',(79.4003239732269,-2.19632397242574,330.597257109179));
#59883=CARTESIAN_POINT('Ctrl Pts',(79.3925752826693,-2.3183254579115,330.66025577279));
#59884=CARTESIAN_POINT('Ctrl Pts',(79.3848265921117,-2.43750918867437,330.728263582847));
#59885=CARTESIAN_POINT('Ctrl Pts',(79.3770795137338,-2.55666812226654,330.796257243312));
#59886=CARTESIAN_POINT('Ctrl Pts',(79.3693324353559,-2.67301012796333,330.869257783628));
#59887=CARTESIAN_POINT('Ctrl Pts',(79.3615853569781,-2.78609570165184,330.946994472772));
#59888=CARTESIAN_POINT('Ctrl Pts',(79.3538382136723,-2.89918222310654,331.024731813426));
#59889=CARTESIAN_POINT('Ctrl Pts',(79.3460910703665,-3.00901193600733,331.107205160657));
#59890=CARTESIAN_POINT('Ctrl Pts',(79.3383439270607,-3.11517488725376,331.194100831036));
#59891=CARTESIAN_POINT('Ctrl Pts',(79.3305950420326,-3.22136170618538,331.281016037405));
#59892=CARTESIAN_POINT('Ctrl Pts',(79.3228461570044,-3.32387982065475,331.372355297805));
#59893=CARTESIAN_POINT('Ctrl Pts',(79.3150972719763,-3.42235320237136,331.467765350275));
#59894=CARTESIAN_POINT('Ctrl Pts',(79.3073401622016,-3.52093110475275,331.56327667196));
#59895=CARTESIAN_POINT('Ctrl Pts',(79.2995830524269,-3.61545541730402,331.662867144462));
#59896=CARTESIAN_POINT('Ctrl Pts',(79.2918259426521,-3.70558740028424,331.766147022304));
#59897=CARTESIAN_POINT('Ctrl Pts',(79.284064687726,-3.79576754691411,331.86948208961));
#59898=CARTESIAN_POINT('Ctrl Pts',(79.2763034327998,-3.88155044279209,331.976510185803));
#59899=CARTESIAN_POINT('Ctrl Pts',(79.2685421778737,-3.96263900470015,332.086810136478));
#59900=CARTESIAN_POINT('Ctrl Pts',(79.260768507469,-4.04385728188062,332.197286531127));
#59901=CARTESIAN_POINT('Ctrl Pts',(79.2529948370643,-4.12036600082409,332.311044914627));
#59902=CARTESIAN_POINT('Ctrl Pts',(79.2452211666597,-4.19191213713433,332.4276361655));
#59903=CARTESIAN_POINT('Ctrl Pts',(79.2378093624827,-4.26012778358583,332.538800065593));
#59904=CARTESIAN_POINT('Ctrl Pts',(79.2303975583057,-4.32383232581881,332.652538777316));
#59905=CARTESIAN_POINT('Ctrl Pts',(79.2229857541286,-4.38284699688836,332.768445549764));
#59906=CARTESIAN_POINT('Ctrl Pts',(79.2146981126954,-4.44883530708127,332.898048780879));
#59907=CARTESIAN_POINT('Ctrl Pts',(79.2064104712622,-4.50914684226371,333.030729653124));
#59908=CARTESIAN_POINT('Ctrl Pts',(79.198122829829,-4.56350325100782,333.165982240942));
#59909=CARTESIAN_POINT('Ctrl Pts',(79.1898511790019,-4.61775478167207,333.300973865388));
#59910=CARTESIAN_POINT('Ctrl Pts',(79.1815795281748,-4.6660739725485,333.438527026137));
#59911=CARTESIAN_POINT('Ctrl Pts',(79.1733078773477,-4.70822882432829,333.578112381282));
#59912=CARTESIAN_POINT('Ctrl Pts',(79.1650582852519,-4.75027125809499,333.717325492008));
#59913=CARTESIAN_POINT('Ctrl Pts',(79.1568086931562,-4.78618204660611,333.858559690968));
#59914=CARTESIAN_POINT('Ctrl Pts',(79.1485591010604,-4.81577791388594,334.001267730256));
#59915=CARTESIAN_POINT('Ctrl Pts',(79.1403231428154,-4.84532486897333,334.143739920294));
#59916=CARTESIAN_POINT('Ctrl Pts',(79.1320871845703,-4.86857763647147,334.287680792508));
#59917=CARTESIAN_POINT('Ctrl Pts',(79.1238512263252,-4.8854026029074,334.432528000686));
#59918=CARTESIAN_POINT('Ctrl Pts',(79.1156335154431,-4.90219029240967,334.577054289367));
#59919=CARTESIAN_POINT('Ctrl Pts',(79.1074158045611,-4.91257854173931,334.722482600472));
#59920=CARTESIAN_POINT('Ctrl Pts',(79.099198093679,-4.91648478403175,334.868241012131));
#59921=CARTESIAN_POINT('Ctrl Pts',(79.0967378546334,-4.91765424471822,334.911878533666));
#59922=CARTESIAN_POINT('Ctrl Pts',(79.0942776155878,-4.91824307030285,334.955545568417));
#59923=CARTESIAN_POINT('Ctrl Pts',(79.0918173765422,-4.91824993919102,334.999226600024));
#59924=CARTESIAN_POINT('',(77.341817376473,-4.91824791270454,335.004531189402));
#59925=CARTESIAN_POINT('Ctrl Pts',(79.0918173765086,-4.91824993919111,334.99922660062));
#59926=CARTESIAN_POINT('Ctrl Pts',(79.083791910814,-4.91827234595029,335.141717071739));
#59927=CARTESIAN_POINT('Ctrl Pts',(79.0757664451194,-4.91209811143813,335.284120059493));
#59928=CARTESIAN_POINT('Ctrl Pts',(79.0677409794247,-4.89977605790234,335.425884544104));
#59929=CARTESIAN_POINT('Ctrl Pts',(79.0597080005508,-4.88744246886179,335.567781744004));
#59930=CARTESIAN_POINT('Ctrl Pts',(79.0516750216769,-4.86894961308294,335.709038901325));
#59931=CARTESIAN_POINT('Ctrl Pts',(79.0436420428029,-4.84439787917671,335.849112625467));
#59932=CARTESIAN_POINT('Ctrl Pts',(79.0354008492239,-4.81920976465569,335.992817058668));
#59933=CARTESIAN_POINT('Ctrl Pts',(79.0271596556449,-4.78764450194056,336.135275487138));
#59934=CARTESIAN_POINT('Ctrl Pts',(79.0189184620659,-4.74986520391124,336.275916771256));
#59935=CARTESIAN_POINT('Ctrl Pts',(79.0108612637775,-4.71292937750462,336.41341805706));
#59936=CARTESIAN_POINT('Ctrl Pts',(79.0028040654891,-4.67005423227963,336.549182177083));
#59937=CARTESIAN_POINT('Ctrl Pts',(78.9947468672007,-4.62144139096944,336.682695020595));
#59938=CARTESIAN_POINT('Ctrl Pts',(78.9864136759764,-4.57116335534254,336.820781240652));
#59939=CARTESIAN_POINT('Ctrl Pts',(78.9780804847521,-4.51474772886055,336.95645882447));
#59940=CARTESIAN_POINT('Ctrl Pts',(78.9697472935277,-4.45246946170217,337.089186146591));
#59941=CARTESIAN_POINT('Ctrl Pts',(78.9614141023034,-4.39019119454378,337.221913468713));
#59942=CARTESIAN_POINT('Ctrl Pts',(78.9530809110791,-4.32205053731824,337.351690202885));
#59943=CARTESIAN_POINT('Ctrl Pts',(78.9447477198547,-4.2483717430536,337.478007384033));
#59944=CARTESIAN_POINT('Ctrl Pts',(78.9369726410763,-4.17962755918848,337.595864518001));
#59945=CARTESIAN_POINT('Ctrl Pts',(78.9291975622979,-4.10586669101411,337.711045098697));
#59946=CARTESIAN_POINT('Ctrl Pts',(78.9214224835194,-4.02732306754453,337.823092625495));
#59947=CARTESIAN_POINT('Ctrl Pts',(78.9136569724704,-3.9488760970039,337.935002270678));
#59948=CARTESIAN_POINT('Ctrl Pts',(78.9058914614213,-3.86565830381378,338.043786216138));
#59949=CARTESIAN_POINT('Ctrl Pts',(78.8981259503723,-3.77794914171783,338.149013074773));
#59950=CARTESIAN_POINT('Ctrl Pts',(78.8903681388501,-3.69032694351157,338.254135600672));
#59951=CARTESIAN_POINT('Ctrl Pts',(78.8826103273279,-3.59822248718326,338.355707760086));
#59952=CARTESIAN_POINT('Ctrl Pts',(78.8748525158057,-3.50195789057692,338.453327959393));
#59953=CARTESIAN_POINT('Ctrl Pts',(78.8671005422826,-3.40576573613206,338.550874696405));
#59954=CARTESIAN_POINT('Ctrl Pts',(78.8593485687596,-3.30541994613564,338.644475115667));
#59955=CARTESIAN_POINT('Ctrl Pts',(78.8515965952366,-3.20128195544908,338.733761763184));
#59956=CARTESIAN_POINT('Ctrl Pts',(78.843847904679,-3.09718806726361,338.823010597753));
#59957=CARTESIAN_POINT('Ctrl Pts',(78.8360992141213,-2.98930546872777,338.907949040231));
#59958=CARTESIAN_POINT('Ctrl Pts',(78.8283505235637,-2.87803122617068,338.988247650747));
#59959=CARTESIAN_POINT('Ctrl Pts',(78.8206034451858,-2.76678013514905,339.068529554466));
#59960=CARTESIAN_POINT('Ctrl Pts',(78.812856366808,-2.6521391204776,339.144173317798));
#59961=CARTESIAN_POINT('Ctrl Pts',(78.8051092884302,-2.53453667111569,339.214891092931));
#59962=CARTESIAN_POINT('Ctrl Pts',(78.7973621451244,-2.41693323613239,339.285609460747));
#59963=CARTESIAN_POINT('Ctrl Pts',(78.7896150018186,-2.29636865192931,339.351401556589));
#59964=CARTESIAN_POINT('Ctrl Pts',(78.7818678585128,-2.17329825733337,339.412024223321));
#59965=CARTESIAN_POINT('Ctrl Pts',(78.7741189734847,-2.05020019389978,339.472660519316));
#59966=CARTESIAN_POINT('Ctrl Pts',(78.7663700884565,-1.92459554962494,339.52812490087));
#59967=CARTESIAN_POINT('Ctrl Pts',(78.7586212034284,-1.79696163043961,339.57822148451));
#59968=CARTESIAN_POINT('Ctrl Pts',(78.7508640936537,-1.66919223929349,339.628371241181));
#59969=CARTESIAN_POINT('Ctrl Pts',(78.743106983879,-1.53938963505829,339.673141675736));
#59970=CARTESIAN_POINT('Ctrl Pts',(78.7353498741042,-1.40804888028225,339.712385957584));
#59971=CARTESIAN_POINT('Ctrl Pts',(78.7275886191781,-1.27663794120632,339.751651210322));
#59972=CARTESIAN_POINT('Ctrl Pts',(78.7198273642519,-1.14368759248009,339.785384330156));
#59973=CARTESIAN_POINT('Ctrl Pts',(78.7120661093257,-1.00970424323918,339.813489420751));
#59974=CARTESIAN_POINT('Ctrl Pts',(78.704292438921,-0.875506564304655,339.841639470333));
#59975=CARTESIAN_POINT('Ctrl Pts',(78.6965187685164,-0.740272968517659,
339.864143435795));
#59976=CARTESIAN_POINT('Ctrl Pts',(78.6887450981117,-0.604517047351342,
339.880957098968));
#59977=CARTESIAN_POINT('Ctrl Pts',(78.6813332939347,-0.475080596978326,
339.896988082074));
#59978=CARTESIAN_POINT('Ctrl Pts',(78.6739214897578,-0.345169642161097,
339.907846583985));
#59979=CARTESIAN_POINT('Ctrl Pts',(78.6665096855808,-0.215228446483766,
339.913538417304));
#59980=CARTESIAN_POINT('Ctrl Pts',(78.6587346068023,-0.0789184457292216,
339.91950922433));
#59981=CARTESIAN_POINT('Ctrl Pts',(78.6509595280239,0.0578556000153201,
339.919812957938));
#59982=CARTESIAN_POINT('Ctrl Pts',(78.6431844492455,0.194583217220188,339.914399295344));
#59983=CARTESIAN_POINT('Ctrl Pts',(78.6354189381964,0.331142582387951,339.908992294606));
#59984=CARTESIAN_POINT('Ctrl Pts',(78.6276534271474,0.467655245860287,339.897881911849));
#59985=CARTESIAN_POINT('Ctrl Pts',(78.6198879160983,0.603607216564659,339.881069697373));
#59986=CARTESIAN_POINT('Ctrl Pts',(78.6121301045761,0.73942439049408,339.864274152257));
#59987=CARTESIAN_POINT('Ctrl Pts',(78.6043722930539,0.874681592564173,339.841788073636));
#59988=CARTESIAN_POINT('Ctrl Pts',(78.5966144815317,1.00886679768246,339.813665011925));
#59989=CARTESIAN_POINT('Ctrl Pts',(78.5888625080087,1.14295102417854,339.785563113711));
#59990=CARTESIAN_POINT('Ctrl Pts',(78.5811105344857,1.27596447842093,339.751832755773));
#59991=CARTESIAN_POINT('Ctrl Pts',(78.5733585609626,1.40740256736202,339.712579025956));
#59992=CARTESIAN_POINT('Ctrl Pts',(78.565609870405,1.53878499219414,339.673341920117));
#59993=CARTESIAN_POINT('Ctrl Pts',(78.5578611798474,1.66859300492612,339.628586206426));
#59994=CARTESIAN_POINT('Ctrl Pts',(78.5501124892898,1.79633469716679,339.578467507612));
#59995=CARTESIAN_POINT('Ctrl Pts',(78.5423654109119,1.92404981168165,339.528359236411));
#59996=CARTESIAN_POINT('Ctrl Pts',(78.5346183325341,2.04969909719514,339.472890342192));
#59997=CARTESIAN_POINT('Ctrl Pts',(78.5268712541563,2.17280861637904,339.412265379495));
#59998=CARTESIAN_POINT('Ctrl Pts',(78.5191241108505,2.29591916733903,339.351639908702));
#59999=CARTESIAN_POINT('Ctrl Pts',(78.5113769675446,2.41648955885201,339.285858455923));
#60000=CARTESIAN_POINT('Ctrl Pts',(78.5036298242388,2.53406890492873,339.215172339012));
#60001=CARTESIAN_POINT('Ctrl Pts',(78.4958809392107,2.65167468533881,339.144470330361));
#60002=CARTESIAN_POINT('Ctrl Pts',(78.4881320541826,2.76628774727898,339.068861664738));
#60003=CARTESIAN_POINT('Ctrl Pts',(78.4803831691545,2.87748507052918,338.988641715093));
#60004=CARTESIAN_POINT('Ctrl Pts',(78.4726260593798,2.98880041976724,338.908336619165));
#60005=CARTESIAN_POINT('Ctrl Pts',(78.464868949605,3.09669247054324,338.823410691111));
#60006=CARTESIAN_POINT('Ctrl Pts',(78.4571118398303,3.2007698431298,338.734200781133));
#60007=CARTESIAN_POINT('Ctrl Pts',(78.4493505849041,3.3049028313366,338.64494320023));
#60008=CARTESIAN_POINT('Ctrl Pts',(78.441589329978,3.40521679385444,338.551397342363));
#60009=CARTESIAN_POINT('Ctrl Pts',(78.4338280750518,3.50135704236948,338.453937162768));
#60010=CARTESIAN_POINT('Ctrl Pts',(78.4260544046471,3.59765108394991,338.356321078648));
#60011=CARTESIAN_POINT('Ctrl Pts',(78.4182807342425,3.68975780699028,338.254778449857));
#60012=CARTESIAN_POINT('Ctrl Pts',(78.4105070638378,3.77736209367237,338.149717237434));
#60013=CARTESIAN_POINT('Ctrl Pts',(78.4030952596608,3.86088837973238,338.049546649726));
#60014=CARTESIAN_POINT('Ctrl Pts',(78.3956834554837,3.94032179758588,337.946177914735));
#60015=CARTESIAN_POINT('Ctrl Pts',(78.3882716513067,4.01542681865982,337.839987768721));
#60016=CARTESIAN_POINT('Ctrl Pts',(78.3804965725283,4.09421296054358,337.728592927327));
#60017=CARTESIAN_POINT('Ctrl Pts',(78.3727214937498,4.16848466086005,337.613741081998));
#60018=CARTESIAN_POINT('Ctrl Pts',(78.3649464149714,4.23792335558755,337.495834268269));
#60019=CARTESIAN_POINT('Ctrl Pts',(78.3571809039224,4.30727660158032,337.378072546381));
#60020=CARTESIAN_POINT('Ctrl Pts',(78.3494153928734,4.37180847898937,337.257263669674));
#60021=CARTESIAN_POINT('Ctrl Pts',(78.3416498818244,4.43124214143404,337.133840703164));
#60022=CARTESIAN_POINT('Ctrl Pts',(78.3338920703022,4.49061687522965,337.010540110884));
#60023=CARTESIAN_POINT('Ctrl Pts',(78.3261342587799,4.54490328509466,336.884630936685));
#60024=CARTESIAN_POINT('Ctrl Pts',(78.3183764472577,4.59386931655804,336.756572732592));
#60025=CARTESIAN_POINT('Ctrl Pts',(78.3106244737347,4.64279849952977,336.62861089636));
#60026=CARTESIAN_POINT('Ctrl Pts',(78.3028725002117,4.68641513433524,336.498503612843));
#60027=CARTESIAN_POINT('Ctrl Pts',(78.2951205266887,4.72453452733265,336.366732074161));
#60028=CARTESIAN_POINT('Ctrl Pts',(78.2873718361311,4.7626377767445,336.235016340805));
#60029=CARTESIAN_POINT('Ctrl Pts',(78.2796231455735,4.79524830635171,336.101638128806));
#60030=CARTESIAN_POINT('Ctrl Pts',(78.2718744550159,4.8222307827711,335.967095310812));
#60031=CARTESIAN_POINT('Ctrl Pts',(78.264127376638,4.84920764526094,335.832580485575));
#60032=CARTESIAN_POINT('Ctrl Pts',(78.2563802982602,4.87055870688119,335.696901919311));
#60033=CARTESIAN_POINT('Ctrl Pts',(78.2486332198824,4.88619950722559,335.560568852228));
#60034=CARTESIAN_POINT('Ctrl Pts',(78.2408860765765,4.90184043865498,335.424234642543));
#60035=CARTESIAN_POINT('Ctrl Pts',(78.2331389332707,4.91177096880236,335.287246309425));
#60036=CARTESIAN_POINT('Ctrl Pts',(78.2253917899649,4.91595843593344,335.150119015034));
#60037=CARTESIAN_POINT('Ctrl Pts',(78.2176429049368,4.92014684449602,335.012960891517));
#60038=CARTESIAN_POINT('Ctrl Pts',(78.2098940199087,4.91858960884494,334.875664135176));
#60039=CARTESIAN_POINT('Ctrl Pts',(78.2021451348806,4.91130619388297,334.738744315991));
#60040=CARTESIAN_POINT('Ctrl Pts',(78.1943880251059,4.90401504822911,334.601679168696));
#60041=CARTESIAN_POINT('Ctrl Pts',(78.1866309153311,4.89098560303289,334.464992148704));
#60042=CARTESIAN_POINT('Ctrl Pts',(78.1788738055564,4.87228932478686,334.32919466455));
#60043=CARTESIAN_POINT('Ctrl Pts',(78.1711125506303,4.85358305584756,334.193324614563));
#60044=CARTESIAN_POINT('Ctrl Pts',(78.1633512957041,4.82920398938614,334.058345432025));
#60045=CARTESIAN_POINT('Ctrl Pts',(78.1555900407779,4.79927465014092,333.924757750544));
#60046=CARTESIAN_POINT('Ctrl Pts',(78.1478163703733,4.76929743370681,333.790956372309));
#60047=CARTESIAN_POINT('Ctrl Pts',(78.1400426999686,4.7337523037596,333.65855132094));
#60048=CARTESIAN_POINT('Ctrl Pts',(78.132269029564,4.69281179510666,333.52802835686));
#60049=CARTESIAN_POINT('Ctrl Pts',(78.1248572253869,4.65377707698132,333.40358126816));
#60050=CARTESIAN_POINT('Ctrl Pts',(78.1174454212098,4.60983808274117,333.280845258649));
#60051=CARTESIAN_POINT('Ctrl Pts',(78.1100336170328,4.56118415991932,333.160222262935));
#60052=CARTESIAN_POINT('Ctrl Pts',(78.1022585382543,4.51014556340726,333.033687174883));
#60053=CARTESIAN_POINT('Ctrl Pts',(78.0944834594759,4.4537568751639,332.909077593865));
#60054=CARTESIAN_POINT('Ctrl Pts',(78.0867083806975,4.39218378217622,332.786878971658));
#60055=CARTESIAN_POINT('Ctrl Pts',(78.0789428696485,4.33068645879943,332.664830722636));
#60056=CARTESIAN_POINT('Ctrl Pts',(78.0711773585994,4.26401759873661,332.545187874998));
#60057=CARTESIAN_POINT('Ctrl Pts',(78.0634118475504,4.19239155813625,332.428417591099));
#60058=CARTESIAN_POINT('Ctrl Pts',(78.0556540360282,4.12083653496359,332.311763085277));
#60059=CARTESIAN_POINT('Ctrl Pts',(78.0478962245061,4.04433431555666,332.197975806246));
#60060=CARTESIAN_POINT('Ctrl Pts',(78.0401384129839,3.9631457690288,332.087499583531));
#60061=CARTESIAN_POINT('Ctrl Pts',(78.0323864394609,3.88201831945728,331.977106497679));
#60062=CARTESIAN_POINT('Ctrl Pts',(78.0246344659379,3.79621179284604,331.870019822286));
#60063=CARTESIAN_POINT('Ctrl Pts',(78.016882492415,3.70603088558811,331.766655270843));
#60064=CARTESIAN_POINT('Ctrl Pts',(78.0091338018573,3.61588816999759,331.663334494349));
#60065=CARTESIAN_POINT('Ctrl Pts',(78.0013851112997,3.52137501479023,331.563733000534));
#60066=CARTESIAN_POINT('Ctrl Pts',(77.9936364207421,3.42283685503905,331.468234021585));
#60067=CARTESIAN_POINT('Ctrl Pts',(77.9858893423643,3.32431919697509,331.372754911997));
#60068=CARTESIAN_POINT('Ctrl Pts',(77.9781422639865,3.22177848059466,331.281376891336));
#60069=CARTESIAN_POINT('Ctrl Pts',(77.9703951856087,3.11559723048165,331.194446563256));
#60070=CARTESIAN_POINT('Ctrl Pts',(77.9626480423028,3.00941509046734,331.107515506616));
#60071=CARTESIAN_POINT('Ctrl Pts',(77.954900898997,2.89959265830718,331.025032464518));
#60072=CARTESIAN_POINT('Ctrl Pts',(77.9471537556912,2.78654546971325,330.947303686714));
#60073=CARTESIAN_POINT('Ctrl Pts',(77.9394048706632,2.67347286571204,330.869557433832));
#60074=CARTESIAN_POINT('Ctrl Pts',(77.9316559856351,2.55717438464273,330.796567793571));
#60075=CARTESIAN_POINT('Ctrl Pts',(77.9239071006071,2.43809411387698,330.728597401979));
#60076=CARTESIAN_POINT('Ctrl Pts',(77.9161499908323,2.31888745008079,330.660554865911));
#60077=CARTESIAN_POINT('Ctrl Pts',(77.9083928810576,2.19689343845477,330.59754241473));
#60078=CARTESIAN_POINT('Ctrl Pts',(77.9006357712829,2.07258080796605,330.539776703241));
#60079=CARTESIAN_POINT('Ctrl Pts',(77.8928745163567,1.94820174878226,330.481980123602));
#60080=CARTESIAN_POINT('Ctrl Pts',(77.8851132614305,1.82150196279881,330.429436019919));
#60081=CARTESIAN_POINT('Ctrl Pts',(77.8773520065044,1.69296874866233,330.382312280096));
#60082=CARTESIAN_POINT('Ctrl Pts',(77.8695783360997,1.56422992327228,330.335113157647));
#60083=CARTESIAN_POINT('Ctrl Pts',(77.861804665695,1.43365218144478,330.293351845045));
#60084=CARTESIAN_POINT('Ctrl Pts',(77.8540309952904,1.30173737796668,330.257146126929));
#60085=CARTESIAN_POINT('Ctrl Pts',(77.8466191911132,1.1759632403262,330.222625793701));
#60086=CARTESIAN_POINT('Ctrl Pts',(77.8392073869361,1.04897400046618,330.193155534017));
#60087=CARTESIAN_POINT('Ctrl Pts',(77.8317955827589,0.921210120589533,330.168793631377));
#60088=CARTESIAN_POINT('Ctrl Pts',(77.8240205039805,0.787184152372231,330.143237679318));
#60089=CARTESIAN_POINT('Ctrl Pts',(77.8162454252021,0.651882142474197,330.123222735876));
#60090=CARTESIAN_POINT('Ctrl Pts',(77.8084703464236,0.515801980388661,330.108872177143));
#60091=CARTESIAN_POINT('Ctrl Pts',(77.8007048353746,0.379889273606136,330.094539277685));
#60092=CARTESIAN_POINT('Ctrl Pts',(77.7929393243256,0.243200704920283,330.085856934468));
#60093=CARTESIAN_POINT('Ctrl Pts',(77.7851738132766,0.106245121535196,330.082897699188));
#60094=CARTESIAN_POINT('Ctrl Pts',(77.7774160017544,-0.0305746699905079,
330.079941397999));
#60095=CARTESIAN_POINT('Ctrl Pts',(77.7696581902322,-0.167660561090477,
330.082696920605));
#60096=CARTESIAN_POINT('Ctrl Pts',(77.76190037871,-0.304498154801893,330.091185078227));
#60097=CARTESIAN_POINT('Ctrl Pts',(77.754148405187,-0.441232773885044,330.099666848241));
#60098=CARTESIAN_POINT('Ctrl Pts',(77.7463964316639,-0.577719078945123,
330.113872642383));
#60099=CARTESIAN_POINT('Ctrl Pts',(77.7386444581408,-0.713442598936831,
330.13377120138));
#60100=CARTESIAN_POINT('Ctrl Pts',(77.7308957675832,-0.849108639936781,
330.153661333324));
#60101=CARTESIAN_POINT('Ctrl Pts',(77.7231470770256,-0.984012152436957,
330.179239378452));
#60102=CARTESIAN_POINT('Ctrl Pts',(77.715398386468,-1.11764393357606,330.210422241967));
#60103=CARTESIAN_POINT('Ctrl Pts',(77.7076513080902,-1.25124791150698,330.241598617627));
#60104=CARTESIAN_POINT('Ctrl Pts',(77.6999042297123,-1.38358030396448,330.278377403392));
#60105=CARTESIAN_POINT('Ctrl Pts',(77.6921571513345,-1.51414263853909,330.320624493305));
#60106=CARTESIAN_POINT('Ctrl Pts',(77.6844100080287,-1.64470606735174,330.362871937289));
#60107=CARTESIAN_POINT('Ctrl Pts',(77.6766628647228,-1.77349903680248,330.410587656496));
#60108=CARTESIAN_POINT('Ctrl Pts',(77.668915721417,-1.90003914472251,330.463587947395));
#60109=CARTESIAN_POINT('Ctrl Pts',(77.6611668363889,-2.0266077015454,330.516600153884));
#60110=CARTESIAN_POINT('Ctrl Pts',(77.6534179513608,-2.15092202851932,330.574899145245));
#60111=CARTESIAN_POINT('Ctrl Pts',(77.6456690663327,-2.27252094822998,330.638253606369));
#60112=CARTESIAN_POINT('Ctrl Pts',(77.637911956558,-2.3942489342903,330.701675312571));
#60113=CARTESIAN_POINT('Ctrl Pts',(77.6301548467833,-2.51325540850563,330.770163026588));
#60114=CARTESIAN_POINT('Ctrl Pts',(77.6223977370085,-2.62910452508903,330.843439828577));
#60115=CARTESIAN_POINT('Ctrl Pts',(77.6146364820824,-2.74501554773595,330.916755787346));
#60116=CARTESIAN_POINT('Ctrl Pts',(77.6068752271562,-2.85776552972986,330.994865710918));
#60117=CARTESIAN_POINT('Ctrl Pts',(77.5991139722301,-2.96694958529134,331.077450673243));
#60118=CARTESIAN_POINT('Ctrl Pts',(77.5913403018254,-3.07630829975895,331.160167744594));
#60119=CARTESIAN_POINT('Ctrl Pts',(77.5835666314207,-3.18208938711603,331.247373910939));
#60120=CARTESIAN_POINT('Ctrl Pts',(77.5757929610161,-3.28392221732683,331.338710891906));
#60121=CARTESIAN_POINT('Ctrl Pts',(77.568381156839,-3.38101470479113,331.425796114435));
#60122=CARTESIAN_POINT('Ctrl Pts',(77.560969352662,-3.47451803920769,331.51663602691));
#60123=CARTESIAN_POINT('Ctrl Pts',(77.5535575484849,-3.56414484936622,331.610891775815));
#60124=CARTESIAN_POINT('Ctrl Pts',(77.5458780966147,-3.6570081736601,331.708551194483));
#60125=CARTESIAN_POINT('Ctrl Pts',(77.5381986447444,-3.74601944247178,331.81020378446));
#60126=CARTESIAN_POINT('Ctrl Pts',(77.5305191928742,-3.83080915142889,331.915509068286));
#60127=CARTESIAN_POINT('Ctrl Pts',(77.5226566171923,-3.91762075139546,332.023325456456));
#60128=CARTESIAN_POINT('Ctrl Pts',(77.5147940415104,-4.00000657169024,332.134970702031));
#60129=CARTESIAN_POINT('Ctrl Pts',(77.5069314658285,-4.07760827444734,332.250037487045));
#60130=CARTESIAN_POINT('Ctrl Pts',(77.4992708826123,-4.15321636087354,332.362148163963));
#60131=CARTESIAN_POINT('Ctrl Pts',(77.4916102993961,-4.22428287453687,332.477506381221));
#60132=CARTESIAN_POINT('Ctrl Pts',(77.4839497161799,-4.29051616916872,332.595700920309));
#60133=CARTESIAN_POINT('Ctrl Pts',(77.4762941438879,-4.35670613942,332.71381814624));
#60134=CARTESIAN_POINT('Ctrl Pts',(77.468638571596,-4.41806898185686,332.834767656018));
#60135=CARTESIAN_POINT('Ctrl Pts',(77.460982999304,-4.47435662834311,332.958109742199));
#60136=CARTESIAN_POINT('Ctrl Pts',(77.4533306794578,-4.53062036119993,333.081399426883));
#60137=CARTESIAN_POINT('Ctrl Pts',(77.4456783596117,-4.58181302090117,333.207079301473));
#60138=CARTESIAN_POINT('Ctrl Pts',(77.4380260397656,-4.62773298058989,333.334686058768));
#60139=CARTESIAN_POINT('Ctrl Pts',(77.4300086511608,-4.6758436410093,333.468380543891));
#60140=CARTESIAN_POINT('Ctrl Pts',(77.4219912625561,-4.71816590548938,333.604189874275));
#60141=CARTESIAN_POINT('Ctrl Pts',(77.4139738739513,-4.7545252176284,333.741559291251));
#60142=CARTESIAN_POINT('Ctrl Pts',(77.4063206178141,-4.78923316837023,333.872689686118));
#60143=CARTESIAN_POINT('Ctrl Pts',(77.3986673616769,-4.81850782164082,334.005241152015));
#60144=CARTESIAN_POINT('Ctrl Pts',(77.3910141055398,-4.8422491117242,334.138718047033));
#60145=CARTESIAN_POINT('Ctrl Pts',(77.3833592324799,-4.8659954176897,334.272223142051));
#60146=CARTESIAN_POINT('Ctrl Pts',(77.37570435942,-4.88420597349974,334.406653658603));
#60147=CARTESIAN_POINT('Ctrl Pts',(77.3680494863601,-4.89683235347569,334.541506854518));
#60148=CARTESIAN_POINT('Ctrl Pts',(77.3603889927685,-4.90946800427409,334.676459065356));
#60149=CARTESIAN_POINT('Ctrl Pts',(77.3527284991769,-4.91651127301378,334.811834174747));
#60150=CARTESIAN_POINT('Ctrl Pts',(77.3450680055853,-4.91796579558135,334.947127549784));
#60151=CARTESIAN_POINT('Ctrl Pts',(77.3439844625598,-4.91817153138216,334.966264200859));
#60152=CARTESIAN_POINT('Ctrl Pts',(77.3429009195342,-4.91826553901394,334.985399221222));
#60153=CARTESIAN_POINT('Ctrl Pts',(77.3418173765086,-4.91824791270512,335.004531188772));
#60154=CARTESIAN_POINT('',(75.5918173764532,-4.91824976747205,334.998487630632));
#60155=CARTESIAN_POINT('Ctrl Pts',(77.3418173764729,-4.91824791270454,335.004531189402));
#60156=CARTESIAN_POINT('Ctrl Pts',(77.3316909005339,-4.91808318235906,335.183332957754));
#60157=CARTESIAN_POINT('Ctrl Pts',(77.3215644245949,-4.9081646217589,335.361701101329));
#60158=CARTESIAN_POINT('Ctrl Pts',(77.3114379486558,-4.88865408756588,335.538743236269));
#60159=CARTESIAN_POINT('Ctrl Pts',(77.3010502676183,-4.86864029330125,335.720352044608));
#60160=CARTESIAN_POINT('Ctrl Pts',(77.2906625865807,-4.83853326650481,335.900565920531));
#60161=CARTESIAN_POINT('Ctrl Pts',(77.2802749055432,-4.79855541263399,336.078447501912));
#60162=CARTESIAN_POINT('Ctrl Pts',(77.2786231084325,-4.7921983341602,336.106733341756));
#60163=CARTESIAN_POINT('Ctrl Pts',(77.2769713113217,-4.78559176117621,336.13496025278));
#60164=CARTESIAN_POINT('Ctrl Pts',(77.275319514211,-4.77873669775026,336.163124514433));
#60165=CARTESIAN_POINT('Ctrl Pts',(77.2675444354326,-4.74646962461989,336.295694883799));
#60166=CARTESIAN_POINT('Ctrl Pts',(77.2597693566541,-4.70863078847159,336.427131006392));
#60167=CARTESIAN_POINT('Ctrl Pts',(77.2519942778757,-4.66531417390901,336.556928617896));
#60168=CARTESIAN_POINT('Ctrl Pts',(77.2442287668267,-4.62205086319838,336.686566505175));
#60169=CARTESIAN_POINT('Ctrl Pts',(77.2364632557777,-4.57332330879617,336.81456952598));
#60170=CARTESIAN_POINT('Ctrl Pts',(77.2286977447287,-4.51927629244884,336.940444499338));
#60171=CARTESIAN_POINT('Ctrl Pts',(77.2209399332065,-4.46528286387542,337.066194667293));
#60172=CARTESIAN_POINT('Ctrl Pts',(77.2131821216842,-4.40598062265845,337.189820629899));
#60173=CARTESIAN_POINT('Ctrl Pts',(77.205424310162,-4.34156374095501,337.310845591061));
#60174=CARTESIAN_POINT('Ctrl Pts',(77.197672336639,-4.27719533499791,337.431779477101));
#60175=CARTESIAN_POINT('Ctrl Pts',(77.189920363116,-4.20772013257298,337.550115914026));
#60176=CARTESIAN_POINT('Ctrl Pts',(77.1821683895929,-4.13337972805088,337.665399610985));
#60177=CARTESIAN_POINT('Ctrl Pts',(77.1744196990353,-4.05907080673423,337.780634485229));
#60178=CARTESIAN_POINT('Ctrl Pts',(77.1666710084777,-3.97990099273244,337.892818863056));
#60179=CARTESIAN_POINT('Ctrl Pts',(77.1589223179201,-3.89615687548517,338.001523723729));
#60180=CARTESIAN_POINT('Ctrl Pts',(77.1511752395422,-3.812430181901,338.110205967448));
#60181=CARTESIAN_POINT('Ctrl Pts',(77.1434281611644,-3.72413131650783,338.215409824536));
#60182=CARTESIAN_POINT('Ctrl Pts',(77.1356810827865,-3.63158885052608,338.316737174278));
#60183=CARTESIAN_POINT('Ctrl Pts',(77.1279339394807,-3.53904560894933,338.41806537324));
#60184=CARTESIAN_POINT('Ctrl Pts',(77.1201867961749,-3.44225895944124,338.515516711437));
#60185=CARTESIAN_POINT('Ctrl Pts',(77.1124396528691,-3.34159595617698,338.608728242492));
#60186=CARTESIAN_POINT('Ctrl Pts',(77.104690767841,-3.24091032173253,338.701960729478));
#60187=CARTESIAN_POINT('Ctrl Pts',(77.0969418828128,-3.13634688611585,338.790951247045));
#60188=CARTESIAN_POINT('Ctrl Pts',(77.0891929977847,-3.02830724341881,338.875375891698));
#60189=CARTESIAN_POINT('Ctrl Pts',(77.08143588801,-2.92015292632868,338.959890145542));
#60190=CARTESIAN_POINT('Ctrl Pts',(77.0736787782353,-2.80851534015112,339.039828604552));
#60191=CARTESIAN_POINT('Ctrl Pts',(77.0659216684606,-2.6938270909141,339.114909314524));
#60192=CARTESIAN_POINT('Ctrl Pts',(77.0581604135344,-2.57907755594371,339.190030145227));
#60193=CARTESIAN_POINT('Ctrl Pts',(77.0503991586082,-2.46127444517347,339.260287854362));
#60194=CARTESIAN_POINT('Ctrl Pts',(77.042637903682,-2.34087576957709,339.325446068778));
#60195=CARTESIAN_POINT('Ctrl Pts',(77.0348642332773,-2.22028449533759,339.390708515102));
#60196=CARTESIAN_POINT('Ctrl Pts',(77.0270905628726,-2.09708971066319,339.450854993968));
#60197=CARTESIAN_POINT('Ctrl Pts',(77.019316892468,-1.97177105246695,339.505696614193));
#60198=CARTESIAN_POINT('Ctrl Pts',(77.011905088291,-1.85228600796204,339.557985343802));
#60199=CARTESIAN_POINT('Ctrl Pts',(77.0044932841141,-1.73087064075181,339.605451877806));
#60200=CARTESIAN_POINT('Ctrl Pts',(76.9970814799371,-1.60795241264849,339.647975053844));
#60201=CARTESIAN_POINT('Ctrl Pts',(76.9893064011587,-1.47900959602892,339.692582417411));
#60202=CARTESIAN_POINT('Ctrl Pts',(76.9815313223802,-1.34800539104188,339.731890560576));
#60203=CARTESIAN_POINT('Ctrl Pts',(76.9737562436018,-1.21541470477148,339.765705630641));
#60204=CARTESIAN_POINT('Ctrl Pts',(76.9659907325528,-1.08298717978167,339.79947908911));
#60205=CARTESIAN_POINT('Ctrl Pts',(76.9582252215038,-0.948977433088734,
339.827772828425));
#60206=CARTESIAN_POINT('Ctrl Pts',(76.9504597104548,-0.813878540804875,
339.850441710125));
#60207=CARTESIAN_POINT('Ctrl Pts',(76.9427018989326,-0.678913599465953,
339.873088115562));
#60208=CARTESIAN_POINT('Ctrl Pts',(76.9349440874104,-0.542862044582386,
339.890120697787));
#60209=CARTESIAN_POINT('Ctrl Pts',(76.9271862758882,-0.406229901857792,
339.901444718584));
#60210=CARTESIAN_POINT('Ctrl Pts',(76.9194343023652,-0.269700579153639,
339.912760217697));
#60211=CARTESIAN_POINT('Ctrl Pts',(76.9116823288422,-0.132591926228203,
339.918375673953));
#60212=CARTESIAN_POINT('Ctrl Pts',(76.9039303553192,0.00458245255235774,
339.918247865209));
#60213=CARTESIAN_POINT('Ctrl Pts',(76.8961816647616,0.141698737902157,339.918120110592));
#60214=CARTESIAN_POINT('Ctrl Pts',(76.888432974204,0.278880303684706,339.912253928964));
#60215=CARTESIAN_POINT('Ctrl Pts',(76.8806842836463,0.415611287219802,339.900658151762));
#60216=CARTESIAN_POINT('Ctrl Pts',(76.8729372052685,0.55231382273168,339.889064787159));
#60217=CARTESIAN_POINT('Ctrl Pts',(76.8651901268907,0.688565573234652,339.871744231143));
#60218=CARTESIAN_POINT('Ctrl Pts',(76.8574430485128,0.823853941784865,339.848757340299));
#60219=CARTESIAN_POINT('Ctrl Pts',(76.849695905207,0.959143444181912,339.825770256804));
#60220=CARTESIAN_POINT('Ctrl Pts',(76.8419487619013,1.09346916317045,339.797116809235));
#60221=CARTESIAN_POINT('Ctrl Pts',(76.8342016185955,1.22632725532357,339.76290925017));
#60222=CARTESIAN_POINT('Ctrl Pts',(76.8264527335674,1.35921521679645,339.728694000519));
#60223=CARTESIAN_POINT('Ctrl Pts',(76.8187038485393,1.49063451640824,339.688922252076));
#60224=CARTESIAN_POINT('Ctrl Pts',(76.8109549635112,1.62009545119503,339.643756431114));
#60225=CARTESIAN_POINT('Ctrl Pts',(76.8031978537365,1.74969379715558,339.598542670684));
#60226=CARTESIAN_POINT('Ctrl Pts',(76.7954407439617,1.87732925639334,339.547923529822));
#60227=CARTESIAN_POINT('Ctrl Pts',(76.787683634187,2.00253061965779,339.492110214569));
#60228=CARTESIAN_POINT('Ctrl Pts',(76.7799223792608,2.1277988865277,339.436267074464));
#60229=CARTESIAN_POINT('Ctrl Pts',(76.7721611243347,2.25063011580118,339.375224403198));
#60230=CARTESIAN_POINT('Ctrl Pts',(76.7643998694085,2.37057768023263,339.309239436894));
#60231=CARTESIAN_POINT('Ctrl Pts',(76.7566261990038,2.49071712167627,339.243148916148));
#60232=CARTESIAN_POINT('Ctrl Pts',(76.7488525285992,2.60796334582652,339.172100504389));
#60233=CARTESIAN_POINT('Ctrl Pts',(76.7410788581945,2.72189795100158,339.096395318671));
#60234=CARTESIAN_POINT('Ctrl Pts',(76.7336670540174,2.83052887289558,339.024214227562));
#60235=CARTESIAN_POINT('Ctrl Pts',(76.7262552498402,2.93614931600617,338.947800320168));
#60236=CARTESIAN_POINT('Ctrl Pts',(76.7188434456631,3.03842606820501,338.867447490342));
#60237=CARTESIAN_POINT('Ctrl Pts',(76.7110683668846,3.145715708695,338.783156328968));
#60238=CARTESIAN_POINT('Ctrl Pts',(76.7032932881062,3.24966465722322,338.69426398991));
#60239=CARTESIAN_POINT('Ctrl Pts',(76.6955182093278,3.34985289944657,338.601064927847));
#60240=CARTESIAN_POINT('Ctrl Pts',(76.6877526982787,3.44991785365957,338.507980553163));
#60241=CARTESIAN_POINT('Ctrl Pts',(76.6799871872297,3.54623102608384,338.410600264035));
#60242=CARTESIAN_POINT('Ctrl Pts',(76.6722216761807,3.63840353491179,338.309260155932));
#60243=CARTESIAN_POINT('Ctrl Pts',(76.6644638646585,3.73048465442894,338.208020526842));
#60244=CARTESIAN_POINT('Ctrl Pts',(76.6567060531363,3.8184330191803,338.102829179379));
#60245=CARTESIAN_POINT('Ctrl Pts',(76.6489482416141,3.90189512223501,337.994060373068));
#60246=CARTESIAN_POINT('Ctrl Pts',(76.6411962680911,3.98529441741033,337.885373418734));
#60247=CARTESIAN_POINT('Ctrl Pts',(76.6334442945681,4.0642139337672,337.773114672999));
#60248=CARTESIAN_POINT('Ctrl Pts',(76.6256923210451,4.13833938409002,337.65769264675));
#60249=CARTESIAN_POINT('Ctrl Pts',(76.6179436304874,4.21243344224068,337.542319501798));
#60250=CARTESIAN_POINT('Ctrl Pts',(76.6101949399298,4.28173726168209,337.423786069011));
#60251=CARTESIAN_POINT('Ctrl Pts',(76.6024462493722,4.34597910606102,337.302530927519));
#60252=CARTESIAN_POINT('Ctrl Pts',(76.5946991709943,4.41020758438767,337.181301014172));
#60253=CARTESIAN_POINT('Ctrl Pts',(76.5869520926165,4.4693759996366,337.057350863656));
#60254=CARTESIAN_POINT('Ctrl Pts',(76.5792050142387,4.52325813178996,336.931144462669));
#60255=CARTESIAN_POINT('Ctrl Pts',(76.5714578709329,4.57714071552746,336.80493700395));
#60256=CARTESIAN_POINT('Ctrl Pts',(76.563710727627,4.62573677432516,336.676473616525));
#60257=CARTESIAN_POINT('Ctrl Pts',(76.5559635843212,4.66886804518057,336.54623873939));
#60258=CARTESIAN_POINT('Ctrl Pts',(76.5482146992931,4.71200901286134,336.415974582691));
#60259=CARTESIAN_POINT('Ctrl Pts',(76.540465814265,4.74968262496021,336.283938514755));
#60260=CARTESIAN_POINT('Ctrl Pts',(76.5327169292369,4.78176046282318,336.150630235428));
#60261=CARTESIAN_POINT('Ctrl Pts',(76.5249598194622,4.81387234843471,336.017180461316));
#60262=CARTESIAN_POINT('Ctrl Pts',(76.5172027096875,4.84037650368658,335.882456159014));
#60263=CARTESIAN_POINT('Ctrl Pts',(76.5094455999127,4.86119553787986,335.74696787414));
#60264=CARTESIAN_POINT('Ctrl Pts',(76.5016843449866,4.88202569709936,335.611407188658));
#60265=CARTESIAN_POINT('Ctrl Pts',(76.4939230900604,4.89716463875778,335.475082095423));
#60266=CARTESIAN_POINT('Ctrl Pts',(76.4861618351342,4.90658698256869,335.33850737804));
#60267=CARTESIAN_POINT('Ctrl Pts',(76.4783881647296,4.91602439905897,335.201714185619));
#60268=CARTESIAN_POINT('Ctrl Pts',(76.4706144943249,4.91972693333389,335.064670962032));
#60269=CARTESIAN_POINT('Ctrl Pts',(76.4628408239202,4.91772137999068,334.927892501898));
#60270=CARTESIAN_POINT('Ctrl Pts',(76.4554290197432,4.91580918563812,334.797481111991));
#60271=CARTESIAN_POINT('Ctrl Pts',(76.4480172155662,4.90870838295846,334.667310678148));
#60272=CARTESIAN_POINT('Ctrl Pts',(76.4406054113892,4.89648579335925,334.537820448385));
#60273=CARTESIAN_POINT('Ctrl Pts',(76.4328303326108,4.88366413823442,334.401983516728));
#60274=CARTESIAN_POINT('Ctrl Pts',(76.4250552538323,4.86516541452339,334.266465882951));
#60275=CARTESIAN_POINT('Ctrl Pts',(76.4172801750539,4.84100994158732,334.1317800924));
#60276=CARTESIAN_POINT('Ctrl Pts',(76.4095146640049,4.8168841934985,333.997260041289));
#60277=CARTESIAN_POINT('Ctrl Pts',(76.4017491529559,4.78711561490042,333.863570177719));
#60278=CARTESIAN_POINT('Ctrl Pts',(76.3939836419069,4.75177638938504,333.731219401243));
#60279=CARTESIAN_POINT('Ctrl Pts',(76.3862258303847,4.71647220281465,333.598999850947));
#60280=CARTESIAN_POINT('Ctrl Pts',(76.3784680188625,4.67560846121725,333.468117120741));
#60281=CARTESIAN_POINT('Ctrl Pts',(76.3707102073403,4.62930858452745,333.339071015449));
#60282=CARTESIAN_POINT('Ctrl Pts',(76.3629582338173,4.58304354996315,333.210122021444));
#60283=CARTESIAN_POINT('Ctrl Pts',(76.3552062602943,4.53135065444095,333.083007267743));
#60284=CARTESIAN_POINT('Ctrl Pts',(76.3474542867713,4.4744033446347,332.958212113852));
#60285=CARTESIAN_POINT('Ctrl Pts',(76.3397055962137,4.41748015204792,332.833469810782));
#60286=CARTESIAN_POINT('Ctrl Pts',(76.3319569056561,4.35530713296958,332.711045508554));
#60287=CARTESIAN_POINT('Ctrl Pts',(76.3242082150985,4.28810604581396,332.591405056396));
#60288=CARTESIAN_POINT('Ctrl Pts',(76.3164611367206,4.22091894040584,332.471789496434));
#60289=CARTESIAN_POINT('Ctrl Pts',(76.3087140583428,4.14870603905123,332.354956975046));
#60290=CARTESIAN_POINT('Ctrl Pts',(76.300966979965,4.07173509742965,332.241348815298));
#60291=CARTESIAN_POINT('Ctrl Pts',(76.2932198366592,3.99476351071744,332.127739703403));
#60292=CARTESIAN_POINT('Ctrl Pts',(76.2854726933534,3.91303402344244,332.017355330645));
#60293=CARTESIAN_POINT('Ctrl Pts',(76.2777255500476,3.8268575423528,331.910607759925));
#60294=CARTESIAN_POINT('Ctrl Pts',(76.2699766650195,3.74066168696069,331.803836190084));
#60295=CARTESIAN_POINT('Ctrl Pts',(76.2622277799914,3.65001709378535,331.70070335335));
#60296=CARTESIAN_POINT('Ctrl Pts',(76.2544788949634,3.55527447638604,331.60158765597));
#60297=CARTESIAN_POINT('Ctrl Pts',(76.2467217851886,3.46043129819367,331.502366756164));
#60298=CARTESIAN_POINT('Ctrl Pts',(76.2389646754139,3.36148167738588,331.407171796116));
#60299=CARTESIAN_POINT('Ctrl Pts',(76.2312075656392,3.25881306211745,331.316344140847));
#60300=CARTESIAN_POINT('Ctrl Pts',(76.223446310713,3.15608958402373,331.225467950183));
#60301=CARTESIAN_POINT('Ctrl Pts',(76.2156850557868,3.04964345475786,331.138963960885));
#60302=CARTESIAN_POINT('Ctrl Pts',(76.2079238008606,2.93989383210682,331.057132094726));
#60303=CARTESIAN_POINT('Ctrl Pts',(76.200150130456,2.82996864582694,330.97516932425));
#60304=CARTESIAN_POINT('Ctrl Pts',(76.1923764600514,2.71672972917205,330.897893832367));
#60305=CARTESIAN_POINT('Ctrl Pts',(76.1846027896467,2.60062448401203,330.825561671835));
#60306=CARTESIAN_POINT('Ctrl Pts',(76.1771909854696,2.48992396594666,330.756596590776));
#60307=CARTESIAN_POINT('Ctrl Pts',(76.1697791812924,2.37661821928833,330.692125116308));
#60308=CARTESIAN_POINT('Ctrl Pts',(76.1623673771153,2.26111277796105,330.632328759185));
#60309=CARTESIAN_POINT('Ctrl Pts',(76.1545922983369,2.13994607088214,330.569601604476));
#60310=CARTESIAN_POINT('Ctrl Pts',(76.1468172195584,2.01597568064073,330.511821208261));
#60311=CARTESIAN_POINT('Ctrl Pts',(76.13904214078,1.88964361352443,330.459247851251));
#60312=CARTESIAN_POINT('Ctrl Pts',(76.131276629731,1.76346700605941,330.406739189104));
#60313=CARTESIAN_POINT('Ctrl Pts',(76.123511118682,1.63493486163489,330.359424965631));
#60314=CARTESIAN_POINT('Ctrl Pts',(76.115745607633,1.50451418742548,330.31751987486));
#60315=CARTESIAN_POINT('Ctrl Pts',(76.1079877961108,1.37422282569433,330.275656333107));
#60316=CARTESIAN_POINT('Ctrl Pts',(76.1002299845886,1.24204703026435,330.239191369842));
#60317=CARTESIAN_POINT('Ctrl Pts',(76.0924721730664,1.10847388728327,330.208291671678));
#60318=CARTESIAN_POINT('Ctrl Pts',(76.0847201995433,0.97500126232804,330.177415226516));
#60319=CARTESIAN_POINT('Ctrl Pts',(76.0769682260204,0.840133762161413,330.15209579811));
#60320=CARTESIAN_POINT('Ctrl Pts',(76.0692162524973,0.704373397894159,330.132450187328));
#60321=CARTESIAN_POINT('Ctrl Pts',(76.0614675619397,0.568670528221865,330.112812896475));
#60322=CARTESIAN_POINT('Ctrl Pts',(76.0537188713821,0.432075932559683,330.09884469998));
#60323=CARTESIAN_POINT('Ctrl Pts',(76.0459701808245,0.295101359665762,330.090611214212));
#60324=CARTESIAN_POINT('Ctrl Pts',(76.0382231024466,0.158155285475765,330.082379441489));
#60325=CARTESIAN_POINT('Ctrl Pts',(76.0304760240688,0.0208297812299513,
330.079880029661));
#60326=CARTESIAN_POINT('Ctrl Pts',(76.022728945691,-0.116359137129804,330.083126642499));
#60327=CARTESIAN_POINT('Ctrl Pts',(76.0149818023852,-0.253549205264831,
330.086373282546));
#60328=CARTESIAN_POINT('Ctrl Pts',(76.0072346590793,-0.390602294465687,
330.095366034065));
#60329=CARTESIAN_POINT('Ctrl Pts',(75.9994875157735,-0.527003642767366,
330.110066439816));
#60330=CARTESIAN_POINT('Ctrl Pts',(75.9917386307454,-0.663435656987934,
330.124770150531));
#60331=CARTESIAN_POINT('Ctrl Pts',(75.9839897457174,-0.799215250192649,
330.145184027033));
#60332=CARTESIAN_POINT('Ctrl Pts',(75.9762408606893,-0.933834421265835,
330.171217924139));
#60333=CARTESIAN_POINT('Ctrl Pts',(75.9684837509146,-1.06859647851817,330.197279453892));
#60334=CARTESIAN_POINT('Ctrl Pts',(75.9607266411398,-1.20219526886451,330.22897284586));
#60335=CARTESIAN_POINT('Ctrl Pts',(75.9529695313651,-1.3341340607493,330.266157018822));
#60336=CARTESIAN_POINT('Ctrl Pts',(75.9452082764389,-1.46614335650588,330.303361061817));
#60337=CARTESIAN_POINT('Ctrl Pts',(75.9374470215127,-1.59649051501126,330.346061610639));
#60338=CARTESIAN_POINT('Ctrl Pts',(75.9296857665866,-1.72469649531938,330.394068491441));
#60339=CARTESIAN_POINT('Ctrl Pts',(75.9219120961819,-1.85310756341376,330.442152167608));
#60340=CARTESIAN_POINT('Ctrl Pts',(75.9141384257772,-1.97937024858825,330.495558985745));
#60341=CARTESIAN_POINT('Ctrl Pts',(75.9063647553725,-2.10302711579265,330.554051280914));
#60342=CARTESIAN_POINT('Ctrl Pts',(75.8989529511955,-2.2209277260784,330.609820745671));
#60343=CARTESIAN_POINT('Ctrl Pts',(75.8915411470184,-2.33645940539615,330.6702127511));
#60344=CARTESIAN_POINT('Ctrl Pts',(75.8841293428413,-2.44925005980186,330.734984500959));
#60345=CARTESIAN_POINT('Ctrl Pts',(75.8763542640629,-2.56756892016618,330.802930907224));
#60346=CARTESIAN_POINT('Ctrl Pts',(75.8685791852845,-2.68324517961335,330.875911965339));
#60347=CARTESIAN_POINT('Ctrl Pts',(75.8608041065061,-2.79582076757547,330.953696835617));
#60348=CARTESIAN_POINT('Ctrl Pts',(75.8530385954571,-2.9082578241096,331.03138598666));
#60349=CARTESIAN_POINT('Ctrl Pts',(75.845273084408,-3.01760148255341,331.113866967809));
#60350=CARTESIAN_POINT('Ctrl Pts',(75.837507573359,-3.12341847774077,331.200863246024));
#60351=CARTESIAN_POINT('Ctrl Pts',(75.8297497618368,-3.22913055506932,331.287773267177));
#60352=CARTESIAN_POINT('Ctrl Pts',(75.8219919503146,-3.33132262777733,331.379189429419));
#60353=CARTESIAN_POINT('Ctrl Pts',(75.8142341387924,-3.4295909352723,331.474792335309));
#60354=CARTESIAN_POINT('Ctrl Pts',(75.8064821652694,-3.52778529274962,331.57032329698));
#60355=CARTESIAN_POINT('Ctrl Pts',(75.7987301917464,-3.62206148329866,331.670034459603));
#60356=CARTESIAN_POINT('Ctrl Pts',(75.7909782182234,-3.71204961955839,331.773566878977));
#60357=CARTESIAN_POINT('Ctrl Pts',(75.7832295276658,-3.80199964578894,331.877055452309));
#60358=CARTESIAN_POINT('Ctrl Pts',(75.7754808371082,-3.88766497372865,331.984361769301));
#60359=CARTESIAN_POINT('Ctrl Pts',(75.7677321465506,-3.96871348855744,332.095090998285));
#60360=CARTESIAN_POINT('Ctrl Pts',(75.7599850681728,-4.04974514056586,332.205797189129));
#60361=CARTESIAN_POINT('Ctrl Pts',(75.752237989795,-4.12616165937756,332.319924560204));
#60362=CARTESIAN_POINT('Ctrl Pts',(75.7444909114171,-4.19767230900181,332.437046576947));
#60363=CARTESIAN_POINT('Ctrl Pts',(75.7367437681113,-4.26918355795408,332.554169575285));
#60364=CARTESIAN_POINT('Ctrl Pts',(75.7289966248056,-4.33578865202132,332.674286935744));
#60365=CARTESIAN_POINT('Ctrl Pts',(75.7212494814998,-4.39724136347907,332.796944972587));
#60366=CARTESIAN_POINT('Ctrl Pts',(75.7135005964717,-4.45870789081106,332.919630585561));
#60367=CARTESIAN_POINT('Ctrl Pts',(75.7057517114436,-4.51501955546467,333.044857662141));
#60368=CARTESIAN_POINT('Ctrl Pts',(75.6980028264155,-4.56597725389353,333.172150230619));
#60369=CARTESIAN_POINT('Ctrl Pts',(75.6902457166408,-4.61698903934999,333.299577908744));
#60370=CARTESIAN_POINT('Ctrl Pts',(75.682488606866,-4.66263536124889,333.429075094712));
#60371=CARTESIAN_POINT('Ctrl Pts',(75.6747314970913,-4.70276604785067,333.560147729216));
#60372=CARTESIAN_POINT('Ctrl Pts',(75.6669702421651,-4.74291817900828,333.691290404744));
#60373=CARTESIAN_POINT('Ctrl Pts',(75.659208987239,-4.77754870331365,333.824009828291));
#60374=CARTESIAN_POINT('Ctrl Pts',(75.6514477323128,-4.80655830546722,333.957800250123));
#60375=CARTESIAN_POINT('Ctrl Pts',(75.6436740619082,-4.83561431353001,334.091804693028));
#60376=CARTESIAN_POINT('Ctrl Pts',(75.6359003915035,-4.85903136467351,334.226883172464));
#60377=CARTESIAN_POINT('Ctrl Pts',(75.6281267210988,-4.87676177206106,334.362522407403));
#60378=CARTESIAN_POINT('Ctrl Pts',(75.6207149169217,-4.89366682471911,334.491847603323));
#60379=CARTESIAN_POINT('Ctrl Pts',(75.6133031127446,-4.90540271983216,334.621682236652));
#60380=CARTESIAN_POINT('Ctrl Pts',(75.6058913085675,-4.91197226855648,334.751582014677));
#60381=CARTESIAN_POINT('Ctrl Pts',(75.6011999978812,-4.91613047260478,334.833802240985));
#60382=CARTESIAN_POINT('Ctrl Pts',(75.5965086871949,-4.91822444166389,334.916127743892));
#60383=CARTESIAN_POINT('Ctrl Pts',(75.5918173765086,-4.91824976747175,334.998487629658));
#60384=CARTESIAN_POINT('',(73.8418173765086,-4.91570827891568,334.996279922712));
#60385=CARTESIAN_POINT('Ctrl Pts',(75.5918173764531,-4.91824976747205,334.998487630632));
#60386=CARTESIAN_POINT('Ctrl Pts',(75.5841035836817,-4.9182914099726,335.133909719248));
#60387=CARTESIAN_POINT('Ctrl Pts',(75.5763897909102,-4.9127356297837,335.269558694198));
#60388=CARTESIAN_POINT('Ctrl Pts',(75.5686759981387,-4.90155235995752,335.40492903711));
#60389=CARTESIAN_POINT('Ctrl Pts',(75.5609714749913,-4.89038252900765,335.540136706195));
#60390=CARTESIAN_POINT('Ctrl Pts',(75.5532669518439,-4.87359869244814,335.675066016892));
#60391=CARTESIAN_POINT('Ctrl Pts',(75.5455624286965,-4.85122276368811,335.80920996013));
#60392=CARTESIAN_POINT('Ctrl Pts',(75.537865249435,-4.82886816347314,335.943226038502));
#60393=CARTESIAN_POINT('Ctrl Pts',(75.5301680701736,-4.80093214085618,336.076457849102));
#60394=CARTESIAN_POINT('Ctrl Pts',(75.5224708909121,-4.76748849417152,336.208402466251));
#60395=CARTESIAN_POINT('Ctrl Pts',(75.5147791369368,-4.73406841993406,336.340254083449));
#60396=CARTESIAN_POINT('Ctrl Pts',(75.5070873829615,-4.69514854401216,336.47081992869));
#60397=CARTESIAN_POINT('Ctrl Pts',(75.4993956289861,-4.65085384591263,336.599606691177));
#60398=CARTESIAN_POINT('Ctrl Pts',(75.4917065716272,-4.60657467688655,336.728348302909));
#60399=CARTESIAN_POINT('Ctrl Pts',(75.4840175142683,-4.5569245600251,336.855311696267));
#60400=CARTESIAN_POINT('Ctrl Pts',(75.4763284569095,-4.50207841063051,336.980018446135));
#60401=CARTESIAN_POINT('Ctrl Pts',(75.4686405336803,-4.44724035099847,337.104706801858));
#60402=CARTESIAN_POINT('Ctrl Pts',(75.4609526104512,-4.38720794289566,337.227138812183));
#60403=CARTESIAN_POINT('Ctrl Pts',(75.453264687222,-4.32220415378727,337.346856262212));
#60404=CARTESIAN_POINT('Ctrl Pts',(75.4455761693606,-4.25719533687747,337.466582971941));
#60405=CARTESIAN_POINT('Ctrl Pts',(75.4378876514992,-4.18721456394206,337.583594354393));
#60406=CARTESIAN_POINT('Ctrl Pts',(75.4301991336378,-4.11253040421546,337.697457457849));
#60407=CARTESIAN_POINT('Ctrl Pts',(75.4225082922612,-4.03782367449748,337.811354971402));
#60408=CARTESIAN_POINT('Ctrl Pts',(75.4148174508845,-3.95841094874331,337.922101981285));
#60409=CARTESIAN_POINT('Ctrl Pts',(75.4071266095078,-3.87460340375593,338.029295549481));
#60410=CARTESIAN_POINT('Ctrl Pts',(75.3994274343602,-3.79070504518257,338.136605272282));
#60411=CARTESIAN_POINT('Ctrl Pts',(75.3917282592126,-3.7024026052751,338.240353553016));
#60412=CARTESIAN_POINT('Ctrl Pts',(75.384029084065,-3.61004696285084,338.340171251375));
#60413=CARTESIAN_POINT('Ctrl Pts',(75.3763251424456,-3.51763414409775,338.440050745736));
#60414=CARTESIAN_POINT('Ctrl Pts',(75.3686212008261,-3.42116340737893,338.535994532661));
#60415=CARTESIAN_POINT('Ctrl Pts',(75.3609172592066,-3.32102069540787,338.627672063896));
#60416=CARTESIAN_POINT('Ctrl Pts',(75.3532021529419,-3.22073285540919,338.719482455317));
#60417=CARTESIAN_POINT('Ctrl Pts',(75.3454870466773,-3.1167627199582,338.807013993407));
#60418=CARTESIAN_POINT('Ctrl Pts',(75.3377719404126,-3.00952764492679,338.889977688486));
#60419=CARTESIAN_POINT('Ctrl Pts',(75.3343990517063,-2.96264663498534,338.926247741103));
#60420=CARTESIAN_POINT('Ctrl Pts',(75.3310261629999,-2.91514196248135,338.96164533264));
#60421=CARTESIAN_POINT('Ctrl Pts',(75.3276532742936,-2.86705002705022,338.996149046881));
#60422=CARTESIAN_POINT('Ctrl Pts',(75.3198781955152,-2.75618998417827,339.075685942324));
#60423=CARTESIAN_POINT('Ctrl Pts',(75.3121031167368,-2.6418425179937,339.150731853742));
#60424=CARTESIAN_POINT('Ctrl Pts',(75.3043280379583,-2.52440750273015,339.220965508348));
#60425=CARTESIAN_POINT('Ctrl Pts',(75.2965625269093,-2.40711699872915,339.29111273597));
#60426=CARTESIAN_POINT('Ctrl Pts',(75.2887970158603,-2.28674683766816,339.356459290732));
#60427=CARTESIAN_POINT('Ctrl Pts',(75.2810315048113,-2.16372820438564,339.41672540691));
#60428=CARTESIAN_POINT('Ctrl Pts',(75.2732736932891,-2.04083154443618,339.476931769058));
#60429=CARTESIAN_POINT('Ctrl Pts',(75.2655158817669,-1.91529198684467,339.53206754622));
#60430=CARTESIAN_POINT('Ctrl Pts',(75.2577580702447,-1.78756750545706,339.581897584619));
#60431=CARTESIAN_POINT('Ctrl Pts',(75.2500060967217,-1.65993914079234,339.631690124333));
#60432=CARTESIAN_POINT('Ctrl Pts',(75.2422541231987,-1.53012948775663,339.676184731138));
#60433=CARTESIAN_POINT('Ctrl Pts',(75.2345021496757,-1.39861847975301,339.715193464811));
#60434=CARTESIAN_POINT('Ctrl Pts',(75.2267534591181,-1.26716316673918,339.754185678262));
#60435=CARTESIAN_POINT('Ctrl Pts',(75.2190047685604,-1.13400830578722,339.787696528479));
#60436=CARTESIAN_POINT('Ctrl Pts',(75.2112560780028,-0.999650843911134,
339.815587321684));
#60437=CARTESIAN_POINT('Ctrl Pts',(75.203508999625,-0.865321336227263,339.843472311977));
#60438=CARTESIAN_POINT('Ctrl Pts',(75.1957619212471,-0.729790107781947,
339.865739491681));
#60439=CARTESIAN_POINT('Ctrl Pts',(75.1880148428693,-0.59356581657329,339.882300962036));
#60440=CARTESIAN_POINT('Ctrl Pts',(75.1802676995635,-0.457340383673773,
339.898862571192));
#60441=CARTESIAN_POINT('Ctrl Pts',(75.1725205562577,-0.320422264442621,
339.909718328448));
#60442=CARTESIAN_POINT('Ctrl Pts',(75.1647734129519,-0.183326388630315,
339.914832092527));
#60443=CARTESIAN_POINT('Ctrl Pts',(75.1570245279238,-0.046199690754497,
339.919947006289));
#60444=CARTESIAN_POINT('Ctrl Pts',(75.1492756428957,0.0911044526989541,
339.919317343516));
#60445=CARTESIAN_POINT('Ctrl Pts',(75.1415267578676,0.228070352015549,339.912959085626));
#60446=CARTESIAN_POINT('Ctrl Pts',(75.1337696480928,0.365181628352708,339.906594079015));
#60447=CARTESIAN_POINT('Ctrl Pts',(75.1260125383181,0.501953552314713,339.894488349291));
#60448=CARTESIAN_POINT('Ctrl Pts',(75.1182554285434,0.637874244230223,339.876709906386));
#60449=CARTESIAN_POINT('Ctrl Pts',(75.1104941736172,0.773867567817685,339.858921963251));
#60450=CARTESIAN_POINT('Ctrl Pts',(75.102732918691,0.909008368070891,339.835455333603));
#60451=CARTESIAN_POINT('Ctrl Pts',(75.0949716637648,1.04279519506601,339.806429157248));
#60452=CARTESIAN_POINT('Ctrl Pts',(75.0871979933601,1.1767960373833,339.777356548471));
#60453=CARTESIAN_POINT('Ctrl Pts',(75.0794243229555,1.30943819991849,339.742706720059));
#60454=CARTESIAN_POINT('Ctrl Pts',(75.0716506525508,1.44023476773872,339.702648921225));
#60455=CARTESIAN_POINT('Ctrl Pts',(75.0642388483737,1.56494272385971,339.664455822563));
#60456=CARTESIAN_POINT('Ctrl Pts',(75.0568270441966,1.68797277171648,339.621347000145));
#60457=CARTESIAN_POINT('Ctrl Pts',(75.0494152400194,1.80892170669439,339.573509081827));
#60458=CARTESIAN_POINT('Ctrl Pts',(75.041640161241,1.9357987092633,339.52332648463));
#60459=CARTESIAN_POINT('Ctrl Pts',(75.0338650824626,2.06078639241786,339.467780909621));
#60460=CARTESIAN_POINT('Ctrl Pts',(75.0260900036841,2.18339819612375,339.407034760433));
#60461=CARTESIAN_POINT('Ctrl Pts',(75.0183244926351,2.30585911819908,339.346363363249));
#60462=CARTESIAN_POINT('Ctrl Pts',(75.0105589815861,2.42594963119493,339.280504297194));
#60463=CARTESIAN_POINT('Ctrl Pts',(75.0027934705371,2.54320113528671,339.209668757512));
#60464=CARTESIAN_POINT('Ctrl Pts',(74.9950356590149,2.66033638417081,339.138903451474));
#60465=CARTESIAN_POINT('Ctrl Pts',(74.9872778474927,2.77463789352716,339.063171691939));
#60466=CARTESIAN_POINT('Ctrl Pts',(74.9795200359705,2.88566008160159,338.982731343683));
#60467=CARTESIAN_POINT('Ctrl Pts',(74.9717680624475,2.99659872195855,338.902351529339));
#60468=CARTESIAN_POINT('Ctrl Pts',(74.9640160889245,3.1042626378053,338.817270407576));
#60469=CARTESIAN_POINT('Ctrl Pts',(74.9562641154015,3.20823406669626,338.727789859392));
#60470=CARTESIAN_POINT('Ctrl Pts',(74.9485154248439,3.31216146362564,338.638347206274));
#60471=CARTESIAN_POINT('Ctrl Pts',(74.9407667342863,3.41239918818163,338.54450908687));
#60472=CARTESIAN_POINT('Ctrl Pts',(74.9330180437287,3.50856168326241,338.446618339364));
#60473=CARTESIAN_POINT('Ctrl Pts',(74.9252709653508,3.60470417093292,338.348747958846));
#60474=CARTESIAN_POINT('Ctrl Pts',(74.9175238869729,3.69677284188704,338.246826906043));
#60475=CARTESIAN_POINT('Ctrl Pts',(74.9097768085951,3.78441851615346,338.141235355254));
#60476=CARTESIAN_POINT('Ctrl Pts',(74.9020296652893,3.872064924975,338.035642919506));
#60477=CARTESIAN_POINT('Ctrl Pts',(74.8942825219835,3.95528801352465,337.926380225179));
#60478=CARTESIAN_POINT('Ctrl Pts',(74.8865353786777,4.03377873179762,337.813860729567));
#60479=CARTESIAN_POINT('Ctrl Pts',(74.8787864936496,4.11228709645053,337.701315937183));
#60480=CARTESIAN_POINT('Ctrl Pts',(74.8710376086215,4.18606075012456,337.585513207041));
#60481=CARTESIAN_POINT('Ctrl Pts',(74.8632887235934,4.25483406263886,337.466894842086));
#60482=CARTESIAN_POINT('Ctrl Pts',(74.8555316138187,4.32368037185762,337.348150574372));
#60483=CARTESIAN_POINT('Ctrl Pts',(74.8477745040439,4.38751554149542,337.22658504063));
#60484=CARTESIAN_POINT('Ctrl Pts',(74.8400173942692,4.44611975509398,337.102665495475));
#60485=CARTESIAN_POINT('Ctrl Pts',(74.832256139343,4.50475528491052,336.978679731678));
#60486=CARTESIAN_POINT('Ctrl Pts',(74.8244948844169,4.55815413679541,336.852337809825));
#60487=CARTESIAN_POINT('Ctrl Pts',(74.8167336294907,4.60614513462613,336.724125883241));
#60488=CARTESIAN_POINT('Ctrl Pts',(74.808959959086,4.65421290241309,336.595708859358));
#60489=CARTESIAN_POINT('Ctrl Pts',(74.8011862886813,4.6968554076331,336.465416224725));
#60490=CARTESIAN_POINT('Ctrl Pts',(74.7934126182767,4.73395147795044,336.333749026958));
#60491=CARTESIAN_POINT('Ctrl Pts',(74.7860008140996,4.76932071726955,336.208210968924));
#60492=CARTESIAN_POINT('Ctrl Pts',(74.7785890099226,4.79964820716896,336.081423719557));
#60493=CARTESIAN_POINT('Ctrl Pts',(74.7711772057455,4.82487268984287,335.953827337262));
#60494=CARTESIAN_POINT('Ctrl Pts',(74.7634021269671,4.85133349955259,335.81997707618));
#60495=CARTESIAN_POINT('Ctrl Pts',(74.7556270481887,4.87226204766127,335.684813369079));
#60496=CARTESIAN_POINT('Ctrl Pts',(74.7478519694102,4.88753159729575,335.548833260595));
#60497=CARTESIAN_POINT('Ctrl Pts',(74.7400864583612,4.90278235677729,335.413020484292));
#60498=CARTESIAN_POINT('Ctrl Pts',(74.7323209473122,4.91238793046495,335.276393690261));
#60499=CARTESIAN_POINT('Ctrl Pts',(74.7245554362632,4.91627233069051,335.139461223955));
#60500=CARTESIAN_POINT('Ctrl Pts',(74.716797624741,4.92015287952192,335.002664526588));
#60501=CARTESIAN_POINT('Ctrl Pts',(74.7090398132189,4.91832353259448,334.865563148282));
#60502=CARTESIAN_POINT('Ctrl Pts',(74.7012820016967,4.91076000404486,334.728671333668));
#60503=CARTESIAN_POINT('Ctrl Pts',(74.6935300281737,4.90320216729032,334.591882534486));
#60504=CARTESIAN_POINT('Ctrl Pts',(74.6857780546507,4.88991875949252,334.455303373801));
#60505=CARTESIAN_POINT('Ctrl Pts',(74.6780260811277,4.87093756359354,334.319448522099));
#60506=CARTESIAN_POINT('Ctrl Pts',(74.67027739057,4.85196440624227,334.183651205006));
#60507=CARTESIAN_POINT('Ctrl Pts',(74.6625287000124,4.82729831408367,334.04857797311));
#60508=CARTESIAN_POINT('Ctrl Pts',(74.6547800094548,4.79701893998964,333.914738579014));
#60509=CARTESIAN_POINT('Ctrl Pts',(74.647032931077,4.76674586577233,333.780927031322));
#60510=CARTESIAN_POINT('Ctrl Pts',(74.6392858526991,4.730861918832,333.648349191817));
#60511=CARTESIAN_POINT('Ctrl Pts',(74.6315387743213,4.68949783452994,333.517504427514));
#60512=CARTESIAN_POINT('Ctrl Pts',(74.6237916310155,4.64813340355697,333.386658566606));
#60513=CARTESIAN_POINT('Ctrl Pts',(74.6160444877097,4.60128886143401,333.257546182566));
#60514=CARTESIAN_POINT('Ctrl Pts',(74.6082973444039,4.54914464852978,333.130650907601));
#60515=CARTESIAN_POINT('Ctrl Pts',(74.6005484593758,4.49698871249951,333.003727103885));
#60516=CARTESIAN_POINT('Ctrl Pts',(74.5927995743478,4.43953088331497,332.879021762579));
#60517=CARTESIAN_POINT('Ctrl Pts',(74.5850506893197,4.37699935522521,332.756997613274));
#60518=CARTESIAN_POINT('Ctrl Pts',(74.5772935795449,4.31440145552538,332.634843946276));
#60519=CARTESIAN_POINT('Ctrl Pts',(74.5695364697702,4.24671927786793,332.515377504528));
#60520=CARTESIAN_POINT('Ctrl Pts',(74.5617793599955,4.17422679132692,332.399035994661));
#60521=CARTESIAN_POINT('Ctrl Pts',(74.5540181050693,4.10169556711892,332.282632315612));
#60522=CARTESIAN_POINT('Ctrl Pts',(74.5462568501431,4.02434913242652,332.169357218434));
#60523=CARTESIAN_POINT('Ctrl Pts',(74.538495595217,3.94250367072959,332.059617734242));
#60524=CARTESIAN_POINT('Ctrl Pts',(74.5307219248123,3.86052728296742,331.949702702639));
#60525=CARTESIAN_POINT('Ctrl Pts',(74.5229482544076,3.77403773323438,331.843334889472));
#60526=CARTESIAN_POINT('Ctrl Pts',(74.515174584003,3.68339078985592,331.740887336758));
#60527=CARTESIAN_POINT('Ctrl Pts',(74.5077627798259,3.59696348349987,331.64320874227));
#60528=CARTESIAN_POINT('Ctrl Pts',(74.5003509756488,3.5067573255949,331.549093853321));
#60529=CARTESIAN_POINT('Ctrl Pts',(74.4929391714717,3.41310922052829,331.45883232376));
#60530=CARTESIAN_POINT('Ctrl Pts',(74.4851640926932,3.31487114286913,331.364146807761));
#60531=CARTESIAN_POINT('Ctrl Pts',(74.4773890139148,3.21253473623743,331.273402707561));
#60532=CARTESIAN_POINT('Ctrl Pts',(74.4696139351363,3.10644939147907,331.186975578274));
#60533=CARTESIAN_POINT('Ctrl Pts',(74.4618484240873,3.00049459149102,331.100654803072));
#60534=CARTESIAN_POINT('Ctrl Pts',(74.4540829130383,2.89080033267491,331.018640673338));
#60535=CARTESIAN_POINT('Ctrl Pts',(74.4463174019892,2.77775297228042,330.941272183616));
#60536=CARTESIAN_POINT('Ctrl Pts',(74.4385595904671,2.66481769867343,330.863980404978));
#60537=CARTESIAN_POINT('Ctrl Pts',(74.4308017789449,2.54853626013645,330.79132531916));
#60538=CARTESIAN_POINT('Ctrl Pts',(74.4230439674227,2.42932795347532,330.72360563594));
#60539=CARTESIAN_POINT('Ctrl Pts',(74.4152919938997,2.31020935484501,330.655936913929));
#60540=CARTESIAN_POINT('Ctrl Pts',(74.4075400203767,2.18816861067551,330.593196394178));
#60541=CARTESIAN_POINT('Ctrl Pts',(74.3997880468537,2.06365355330069,330.53563923115));
#60542=CARTESIAN_POINT('Ctrl Pts',(74.392039356296,1.93919122812675,330.478106443614));
#60543=CARTESIAN_POINT('Ctrl Pts',(74.3842906657384,1.81225702795665,330.425752810458));
#60544=CARTESIAN_POINT('Ctrl Pts',(74.3765419751808,1.68332271937117,330.378787206268));
#60545=CARTESIAN_POINT('Ctrl Pts',(74.368794896803,1.55441523664511,330.331831373664));
#60546=CARTESIAN_POINT('Ctrl Pts',(74.3610478184251,1.42350884027096,330.290261473926));
#60547=CARTESIAN_POINT('Ctrl Pts',(74.3533007400472,1.29109420703118,330.254237805044));
#60548=CARTESIAN_POINT('Ctrl Pts',(74.3455535967414,1.15867846402932,330.21821383425));
#60549=CARTESIAN_POINT('Ctrl Pts',(74.3378064534356,1.02475483611541,330.187736289634));
#60550=CARTESIAN_POINT('Ctrl Pts',(74.3300593101298,0.889827666568586,330.16291515618));
#60551=CARTESIAN_POINT('Ctrl Pts',(74.3223104251017,0.754870162529831,330.138088442409));
#60552=CARTESIAN_POINT('Ctrl Pts',(74.3145615400736,0.618909052253251,330.118920741008));
#60553=CARTESIAN_POINT('Ctrl Pts',(74.3068126550455,0.482456943923607,330.105470568097));
#60554=CARTESIAN_POINT('Ctrl Pts',(74.2990555452708,0.345860003916089,330.092006119034));
#60555=CARTESIAN_POINT('Ctrl Pts',(74.2912984354961,0.208771414412195,330.084271359549));
#60556=CARTESIAN_POINT('Ctrl Pts',(74.2835413257213,0.0717075126428193,
330.082272771378));
#60557=CARTESIAN_POINT('Ctrl Pts',(74.2757800707952,-0.0654296316929282,
330.080273115225));
#60558=CARTESIAN_POINT('Ctrl Pts',(74.268018815869,-0.202541671476678,330.084015727465));
#60559=CARTESIAN_POINT('Ctrl Pts',(74.2602575609429,-0.339115220538798,
330.093454990556));
#60560=CARTESIAN_POINT('Ctrl Pts',(74.2524838905382,-0.475907242770296,
330.102909353391));
#60561=CARTESIAN_POINT('Ctrl Pts',(74.2447102201335,-0.612158664250082,
330.118078533847));
#60562=CARTESIAN_POINT('Ctrl Pts',(74.2369365497289,-0.747363259332668,
330.138865233189));
#60563=CARTESIAN_POINT('Ctrl Pts',(74.2295247455518,-0.87627404798526,330.158684306675));
#60564=CARTESIAN_POINT('Ctrl Pts',(74.2221129413748,-1.00423299402524,330.1836096226));
#60565=CARTESIAN_POINT('Ctrl Pts',(74.2147011371977,-1.13081420305578,330.213514619194));
#60566=CARTESIAN_POINT('Ctrl Pts',(74.2069260584193,-1.26359953420734,330.244885348754));
#60567=CARTESIAN_POINT('Ctrl Pts',(74.1991509796408,-1.39528828569607,330.281835376828));
#60568=CARTESIAN_POINT('Ctrl Pts',(74.1913759008624,-1.5253755697793,330.324274127622));
#60569=CARTESIAN_POINT('Ctrl Pts',(74.1836103898134,-1.65530277317832,330.366660654832));
#60570=CARTESIAN_POINT('Ctrl Pts',(74.1758448787644,-1.78363206226736,330.414522345726));
#60571=CARTESIAN_POINT('Ctrl Pts',(74.1680793677153,-1.90986928922423,330.46771775365));
#60572=CARTESIAN_POINT('Ctrl Pts',(74.1603215561931,-2.03598135160243,330.520860418172));
#60573=CARTESIAN_POINT('Ctrl Pts',(74.1525637446709,-2.16000512191483,330.57932612471));
#60574=CARTESIAN_POINT('Ctrl Pts',(74.1448059331488,-2.28146250317631,330.642923926634));
#60575=CARTESIAN_POINT('Ctrl Pts',(74.1370539596258,-2.40282848390676,330.706473869195));
#60576=CARTESIAN_POINT('Ctrl Pts',(74.1293019861027,-2.52163157484181,330.775148039305));
#60577=CARTESIAN_POINT('Ctrl Pts',(74.1215500125797,-2.6374148633786,330.848707923919));
#60578=CARTESIAN_POINT('Ctrl Pts',(74.1138013220221,-2.75314911762404,330.922236655879));
#60579=CARTESIAN_POINT('Ctrl Pts',(74.1060526314645,-2.86586578385532,331.000646777873));
#60580=CARTESIAN_POINT('Ctrl Pts',(74.0983039409069,-2.97513391501071,331.083654605343));
#60581=CARTESIAN_POINT('Ctrl Pts',(74.0905568625291,-3.08437931201887,331.16664516234));
#60582=CARTESIAN_POINT('Ctrl Pts',(74.0828097841512,-3.19017729004924,331.254231285788));
#60583=CARTESIAN_POINT('Ctrl Pts',(74.0750627057734,-3.29212751773907,331.346087101552));
#60584=CARTESIAN_POINT('Ctrl Pts',(74.0673155624676,-3.39407859986993,331.437943687156));
#60585=CARTESIAN_POINT('Ctrl Pts',(74.0595684191617,-3.49218157694745,331.534069774811));
#60586=CARTESIAN_POINT('Ctrl Pts',(74.0518212758559,-3.58607103116525,331.63410077068));
#60587=CARTESIAN_POINT('Ctrl Pts',(74.0440723908279,-3.67998159372544,331.73415425564));
#60588=CARTESIAN_POINT('Ctrl Pts',(74.0363235057998,-3.76967648097578,331.838114110804));
#60589=CARTESIAN_POINT('Ctrl Pts',(74.0285746207717,-3.85482908376087,331.945580939443));
#60590=CARTESIAN_POINT('Ctrl Pts',(74.020817510997,-3.94007206839863,332.053161834485));
#60591=CARTESIAN_POINT('Ctrl Pts',(74.0130604012223,-4.02076289458544,332.164256831879));
#60592=CARTESIAN_POINT('Ctrl Pts',(74.0053032914475,-4.09661669198922,332.278435240268));
#60593=CARTESIAN_POINT('Ctrl Pts',(73.9975420365214,-4.17251102323696,332.392674661948));
#60594=CARTESIAN_POINT('Ctrl Pts',(73.9897807815952,-4.24356297297313,332.510000443594));
#60595=CARTESIAN_POINT('Ctrl Pts',(73.982019526669,-4.30953307924865,332.629956181552));
#60596=CARTESIAN_POINT('Ctrl Pts',(73.9742458562643,-4.37560871619465,332.750103809598));
#60597=CARTESIAN_POINT('Ctrl Pts',(73.9664721858597,-4.43658609099692,332.872889450669));
#60598=CARTESIAN_POINT('Ctrl Pts',(73.958698515455,-4.49227307649294,332.997834754892));
#60599=CARTESIAN_POINT('Ctrl Pts',(73.9512867112779,-4.5453678194165,333.116963825144));
#60600=CARTESIAN_POINT('Ctrl Pts',(73.9438749071008,-4.59365351748236,333.238055751415));
#60601=CARTESIAN_POINT('Ctrl Pts',(73.9364631029238,-4.63700612328589,333.360683900186));
#60602=CARTESIAN_POINT('Ctrl Pts',(73.9273880990653,-4.69008700016011,333.510829653725));
#60603=CARTESIAN_POINT('Ctrl Pts',(73.9183130952069,-4.73591098356173,333.663667231865));
#60604=CARTESIAN_POINT('Ctrl Pts',(73.9092380913485,-4.77423708957649,333.818541886053));
#60605=CARTESIAN_POINT('Ctrl Pts',(73.9002022728023,-4.81239770580721,333.972747800946));
#60606=CARTESIAN_POINT('Ctrl Pts',(73.891166454256,-4.8431249669467,334.128973136046));
#60607=CARTESIAN_POINT('Ctrl Pts',(73.8821306357098,-4.86622770248834,334.286549924637));
#60608=CARTESIAN_POINT('Ctrl Pts',(73.873167972811,-4.88914339403743,334.44285094259));
#60609=CARTESIAN_POINT('Ctrl Pts',(73.8642053099122,-4.90455744254433,334.600481501425));
#60610=CARTESIAN_POINT('Ctrl Pts',(73.8552426470135,-4.91233052211994,334.758770018553));
#60611=CARTESIAN_POINT('Ctrl Pts',(73.8507675568452,-4.91621164901036,334.837804050599));
#60612=CARTESIAN_POINT('Ctrl Pts',(73.8462924666769,-4.91818859753757,334.917001816555));
#60613=CARTESIAN_POINT('Ctrl Pts',(73.8418173765086,-4.918248591645,334.996278000271));
#60614=CARTESIAN_POINT('',(72.0918173765086,-4.91544128743151,335.003188401032));
#60615=CARTESIAN_POINT('Ctrl Pts',(73.8418173765086,-4.91336535392688,334.996281695775));
#60616=CARTESIAN_POINT('Ctrl Pts',(73.7806199405557,-4.90577526826458,336.079323715111));
#60617=CARTESIAN_POINT('Ctrl Pts',(73.626676493178,-4.01863795453471,338.81503798128));
#60618=CARTESIAN_POINT('Ctrl Pts',(73.3799870343759,0.507402860391596,340.793702719651));
#60619=CARTESIAN_POINT('Ctrl Pts',(73.101749000102,5.14663302270979,337.708619093927));
#60620=CARTESIAN_POINT('Ctrl Pts',(72.823510965828,5.0628740242661,332.137875704857));
#60621=CARTESIAN_POINT('Ctrl Pts',(72.5452729315541,0.332990261651519,329.193661536556));
#60622=CARTESIAN_POINT('Ctrl Pts',(72.3013750684476,-4.0809961841249,331.283583074452));
#60623=CARTESIAN_POINT('Ctrl Pts',(72.1502232167658,-4.90617808429904,333.968985933903));
#60624=CARTESIAN_POINT('Ctrl Pts',(72.0918173765086,-4.91230093438665,335.003186364042));
#60625=CARTESIAN_POINT('',(70.3418173765448,-4.9182494475218,335.002331191005));
#60626=CARTESIAN_POINT('Ctrl Pts',(72.0918173765086,-4.91824896533127,335.003190222232));
#60627=CARTESIAN_POINT('Ctrl Pts',(72.0830646580099,-4.91814831260998,335.158362842285));
#60628=CARTESIAN_POINT('Ctrl Pts',(72.0743119395114,-4.91070000482826,335.3132548513));
#60629=CARTESIAN_POINT('Ctrl Pts',(72.0655592210127,-4.89600773382934,335.467216580167));
#60630=CARTESIAN_POINT('Ctrl Pts',(72.0567713434352,-4.88125644497047,335.621796762898));
#60631=CARTESIAN_POINT('Ctrl Pts',(72.0479834658578,-4.85920298955882,335.775438996226));
#60632=CARTESIAN_POINT('Ctrl Pts',(72.0391955882803,-4.8300021260178,335.927503382831));
#60633=CARTESIAN_POINT('Ctrl Pts',(72.0303584999139,-4.80063774204547,336.080419307065));
#60634=CARTESIAN_POINT('Ctrl Pts',(72.0215214115475,-4.76404577311296,336.231739484791));
#60635=CARTESIAN_POINT('Ctrl Pts',(72.0126843231812,-4.72043232127063,336.380833720186));
#60636=CARTESIAN_POINT('Ctrl Pts',(72.0047218364562,-4.68113526810929,336.515172183364));
#60637=CARTESIAN_POINT('Ctrl Pts',(71.9967593497312,-4.63613847248084,336.647703686998));
#60638=CARTESIAN_POINT('Ctrl Pts',(71.9887968630062,-4.58562526802528,336.777983116834));
#60639=CARTESIAN_POINT('Ctrl Pts',(71.9810217842278,-4.53630096048684,336.905196243233));
#60640=CARTESIAN_POINT('Ctrl Pts',(71.9732467054494,-4.48160103382147,337.030556324065));
#60641=CARTESIAN_POINT('Ctrl Pts',(71.9654716266709,-4.42168460089725,337.153575713247));
#60642=CARTESIAN_POINT('Ctrl Pts',(71.9577061156219,-4.36184189895817,337.276443719239));
#60643=CARTESIAN_POINT('Ctrl Pts',(71.9499406045729,-4.29679563273098,337.396976416642));
#60644=CARTESIAN_POINT('Ctrl Pts',(71.9421750935239,-4.22675382691329,337.514703789549));
#60645=CARTESIAN_POINT('Ctrl Pts',(71.9344172820017,-4.15678146774989,337.632314435424));
#60646=CARTESIAN_POINT('Ctrl Pts',(71.9266594704795,-4.08182362449603,337.747124958366));
#60647=CARTESIAN_POINT('Ctrl Pts',(71.9189016589573,-4.00213514582106,337.85868804473));
#60648=CARTESIAN_POINT('Ctrl Pts',(71.9111496854342,-3.9225066352533,337.970167176334));
#60649=CARTESIAN_POINT('Ctrl Pts',(71.9033977119112,-3.83815480145451,338.078403418836));
#60650=CARTESIAN_POINT('Ctrl Pts',(71.8956457383882,-3.74937869625221,338.182976979903));
#60651=CARTESIAN_POINT('Ctrl Pts',(71.8878970478306,-3.66064018778348,338.287506254004));
#60652=CARTESIAN_POINT('Ctrl Pts',(71.8801483572729,-3.56748138697016,338.388375634434));
#60653=CARTESIAN_POINT('Ctrl Pts',(71.8723996667153,-3.47024251945983,338.485197256775));
#60654=CARTESIAN_POINT('Ctrl Pts',(71.8646525883375,-3.3730238833081,338.581998734569));
#60655=CARTESIAN_POINT('Ctrl Pts',(71.8569055099596,-3.27172714577507,338.674753853786));
#60656=CARTESIAN_POINT('Ctrl Pts',(71.8491584315818,-3.16673011352601,338.763110874076));
#60657=CARTESIAN_POINT('Ctrl Pts',(71.841411288276,-3.06173220130083,338.851468634883));
#60658=CARTESIAN_POINT('Ctrl Pts',(71.8336641449702,-2.95303423157426,338.935427971568));
#60659=CARTESIAN_POINT('Ctrl Pts',(71.8259170016644,-2.84104756435277,339.014677047981));
#60660=CARTESIAN_POINT('Ctrl Pts',(71.8181681166363,-2.72903572015086,339.093943941269));
#60661=CARTESIAN_POINT('Ctrl Pts',(71.8104192316083,-2.61373402619343,339.168498241314));
#60662=CARTESIAN_POINT('Ctrl Pts',(71.8026703465802,-2.49558298081014,339.238071335925));
#60663=CARTESIAN_POINT('Ctrl Pts',(71.7949132368054,-2.37730652868638,339.307718276138));
#60664=CARTESIAN_POINT('Ctrl Pts',(71.7871561270307,-2.25617502110136,339.372373250785));
#60665=CARTESIAN_POINT('Ctrl Pts',(71.779399017256,-2.13265421698883,339.431813291787));
#60666=CARTESIAN_POINT('Ctrl Pts',(71.7716377623298,-2.0090674073081,339.491285095646));
#60667=CARTESIAN_POINT('Ctrl Pts',(71.7638765074036,-1.883089115852,339.5455362586));
#60668=CARTESIAN_POINT('Ctrl Pts',(71.7561152524775,-1.75520432843398,339.594392324121));
#60669=CARTESIAN_POINT('Ctrl Pts',(71.7483415820728,-1.62711496703365,339.643326543425));
#60670=CARTESIAN_POINT('Ctrl Pts',(71.7405679116682,-1.49711338617319,339.686848295053));
#60671=CARTESIAN_POINT('Ctrl Pts',(71.7327942412635,-1.36569980342865,339.724833024501));
#60672=CARTESIAN_POINT('Ctrl Pts',(71.7253824370864,-1.24040355457688,339.761049555655));
#60673=CARTESIAN_POINT('Ctrl Pts',(71.7179706329093,-1.11382408229163,339.792232891618));
#60674=CARTESIAN_POINT('Ctrl Pts',(71.7105588287322,-0.986401021095636,
339.818318803077));
#60675=CARTESIAN_POINT('Ctrl Pts',(71.7027837499537,-0.852732576096907,
339.845683262761));
#60676=CARTESIAN_POINT('Ctrl Pts',(71.6950086711753,-0.717713340685445,
339.867524460355));
#60677=CARTESIAN_POINT('Ctrl Pts',(71.6872335923969,-0.581839491958865,
339.883712303985));
#60678=CARTESIAN_POINT('Ctrl Pts',(71.6794680813478,-0.446132844653388,
339.899880227444));
#60679=CARTESIAN_POINT('Ctrl Pts',(71.6717025702988,-0.309574060945946,
339.910408593201));
#60680=CARTESIAN_POINT('Ctrl Pts',(71.6639370592498,-0.172670961339019,
339.915217981088));
#60681=CARTESIAN_POINT('Ctrl Pts',(71.6561792477276,-0.0359036015540283,
339.920022600453));
#60682=CARTESIAN_POINT('Ctrl Pts',(71.6484214362055,0.101207006627649,339.919119512695));
#60683=CARTESIAN_POINT('Ctrl Pts',(71.6406636246833,0.238146794379776,339.912480958419));
#60684=CARTESIAN_POINT('Ctrl Pts',(71.6329116511603,0.374983530599102,339.905847399865));
#60685=CARTESIAN_POINT('Ctrl Pts',(71.6251596776372,0.511649313413178,339.893486984668));
#60686=CARTESIAN_POINT('Ctrl Pts',(71.6174077041142,0.647629296389616,339.875424018171));
#60687=CARTESIAN_POINT('Ctrl Pts',(71.6096590135566,0.783551691762532,339.857368701351));
#60688=CARTESIAN_POINT('Ctrl Pts',(71.601910322999,0.918788478291488,339.833615687926));
#60689=CARTESIAN_POINT('Ctrl Pts',(71.5941616324414,1.05282937689145,339.804241185209));
#60690=CARTESIAN_POINT('Ctrl Pts',(71.5864145540635,1.18684238716293,339.774872794102));
#60691=CARTESIAN_POINT('Ctrl Pts',(71.5786674756857,1.31965962284119,339.739885323735));
#60692=CARTESIAN_POINT('Ctrl Pts',(71.5709203973079,1.45078084509586,339.699406132907));
#60693=CARTESIAN_POINT('Ctrl Pts',(71.5631732540021,1.58190316627257,339.658926602824));
#60694=CARTESIAN_POINT('Ctrl Pts',(71.5554261106962,1.71132907219253,339.612955375778));
#60695=CARTESIAN_POINT('Ctrl Pts',(71.5476789673904,1.8385737226806,339.561669620738));
#60696=CARTESIAN_POINT('Ctrl Pts',(71.5399300823623,1.96584698046749,339.510372335573));
#60697=CARTESIAN_POINT('Ctrl Pts',(71.5321811973343,2.09093764453166,339.453758290949));
#60698=CARTESIAN_POINT('Ctrl Pts',(71.5244323123062,2.21338145422958,339.392052549842));
#60699=CARTESIAN_POINT('Ctrl Pts',(71.5166752025314,2.33595522705236,339.330281313623));
#60700=CARTESIAN_POINT('Ctrl Pts',(71.5089180927567,2.45587618386523,339.263407761351));
#60701=CARTESIAN_POINT('Ctrl Pts',(71.501160982982,2.57270477716889,339.191702898827));
#60702=CARTESIAN_POINT('Ctrl Pts',(71.4933997280558,2.68959579993728,339.119959719517));
#60703=CARTESIAN_POINT('Ctrl Pts',(71.4856384731296,2.80339084240301,339.043380303808));
#60704=CARTESIAN_POINT('Ctrl Pts',(71.4778772182035,2.91368074669759,338.96227807818));
#60705=CARTESIAN_POINT('Ctrl Pts',(71.4701035477988,3.02414707889566,338.881046115422));
#60706=CARTESIAN_POINT('Ctrl Pts',(71.4623298773941,3.13109676322804,338.795277129697));
#60707=CARTESIAN_POINT('Ctrl Pts',(71.4545562069895,3.23415436272227,338.705324361049));
#60708=CARTESIAN_POINT('Ctrl Pts',(71.4471444028124,3.33241460616541,338.619558915423));
#60709=CARTESIAN_POINT('Ctrl Pts',(71.4397325986354,3.42713675422618,338.529990629114));
#60710=CARTESIAN_POINT('Ctrl Pts',(71.4323207944583,3.51802888363629,338.436954442003));
#60711=CARTESIAN_POINT('Ctrl Pts',(71.4245457156799,3.61337590706287,338.33935827422));
#60712=CARTESIAN_POINT('Ctrl Pts',(71.4167706369015,3.70480929176386,338.237637243919));
#60713=CARTESIAN_POINT('Ctrl Pts',(71.408995558123,3.79195113081103,338.13213819683));
#60714=CARTESIAN_POINT('Ctrl Pts',(71.401230047074,3.87898573627754,338.026768973035));
#60715=CARTESIAN_POINT('Ctrl Pts',(71.393464536025,3.96173905726131,337.91763128129));
#60716=CARTESIAN_POINT('Ctrl Pts',(71.385699024976,4.03986949683469,337.80510917988));
#60717=CARTESIAN_POINT('Ctrl Pts',(71.3779412134538,4.11792246984977,337.69269864446));
#60718=CARTESIAN_POINT('Ctrl Pts',(71.3701834019316,4.19136146158048,337.576910696309));
#60719=CARTESIAN_POINT('Ctrl Pts',(71.3624255904094,4.2598849364179,337.458162604666));
#60720=CARTESIAN_POINT('Ctrl Pts',(71.3546736168864,4.3283568451675,337.339503874729));
#60721=CARTESIAN_POINT('Ctrl Pts',(71.3469216433634,4.39192040529233,337.21788977242));
#60722=CARTESIAN_POINT('Ctrl Pts',(71.3391696698403,4.45031744272701,337.093766396105));
#60723=CARTESIAN_POINT('Ctrl Pts',(71.3314209792827,4.50868974898163,336.969695586114));
#60724=CARTESIAN_POINT('Ctrl Pts',(71.3236722887251,4.56189971832029,336.84311796866));
#60725=CARTESIAN_POINT('Ctrl Pts',(71.3159235981675,4.60973529380511,336.714503888461));
#60726=CARTESIAN_POINT('Ctrl Pts',(71.3081765197897,4.65756091669892,336.585916567496));
#60727=CARTESIAN_POINT('Ctrl Pts',(71.3004294414118,4.70001423371958,336.455293992686));
#60728=CARTESIAN_POINT('Ctrl Pts',(71.292682363034,4.73693163566275,336.323125746691));
#60729=CARTESIAN_POINT('Ctrl Pts',(71.2849352197282,4.7738493470093,336.190956392999));
#60730=CARTESIAN_POINT('Ctrl Pts',(71.2771880764224,4.80523094558301,336.057241718747));
#60731=CARTESIAN_POINT('Ctrl Pts',(71.2694409331166,4.83096304171257,335.922485312678));
#60732=CARTESIAN_POINT('Ctrl Pts',(71.2616920480885,4.85670092296364,335.787698610509));
#60733=CARTESIAN_POINT('Ctrl Pts',(71.2539431630604,4.87678670105804,335.651870094346));
#60734=CARTESIAN_POINT('Ctrl Pts',(71.2461942780323,4.89115839817848,335.515511965359));
#60735=CARTESIAN_POINT('Ctrl Pts',(71.2384371682576,4.90554534956675,335.379009104445));
#60736=CARTESIAN_POINT('Ctrl Pts',(71.2306800584828,4.91420606357072,335.241975897121));
#60737=CARTESIAN_POINT('Ctrl Pts',(71.2229229487081,4.91713057037797,335.104928625048));
#60738=CARTESIAN_POINT('Ctrl Pts',(71.215161693782,4.92005663994815,334.967808119294));
#60739=CARTESIAN_POINT('Ctrl Pts',(71.2074004388558,4.91724040256479,334.830673924407));
#60740=CARTESIAN_POINT('Ctrl Pts',(71.1996391839296,4.90872400644114,334.694039723022));
#60741=CARTESIAN_POINT('Ctrl Pts',(71.1918655135249,4.90019398685918,334.557186951443));
#60742=CARTESIAN_POINT('Ctrl Pts',(71.1840918431203,4.88594562792644,334.420836160618));
#60743=CARTESIAN_POINT('Ctrl Pts',(71.1763181727156,4.86607280624221,334.285494221962));
#60744=CARTESIAN_POINT('Ctrl Pts',(71.1689063685385,4.84712506918852,334.156452483111));
#60745=CARTESIAN_POINT('Ctrl Pts',(71.1614945643615,4.82306477584683,334.028328068849));
#60746=CARTESIAN_POINT('Ctrl Pts',(71.1540827601844,4.79401560787775,333.901547718868));
#60747=CARTESIAN_POINT('Ctrl Pts',(71.146307681406,4.76354265365348,333.768553486275));
#60748=CARTESIAN_POINT('Ctrl Pts',(71.1385326026275,4.72748312005856,333.636618116187));
#60749=CARTESIAN_POINT('Ctrl Pts',(71.1307575238491,4.68592416994429,333.506247096729));
#60750=CARTESIAN_POINT('Ctrl Pts',(71.1229920128001,4.6444163607639,333.37603650711));
#60751=CARTESIAN_POINT('Ctrl Pts',(71.1152265017511,4.59742271779424,333.247386806707));
#60752=CARTESIAN_POINT('Ctrl Pts',(71.1074609907021,4.54508134614102,333.12079308764));
#60753=CARTESIAN_POINT('Ctrl Pts',(71.0997031791799,4.49279187111018,332.994324886614));
#60754=CARTESIAN_POINT('Ctrl Pts',(71.0919453676577,4.43516536763633,332.86990896906));
#60755=CARTESIAN_POINT('Ctrl Pts',(71.0841875561355,4.37238954810552,332.748024711033));
#60756=CARTESIAN_POINT('Ctrl Pts',(71.0764355826125,4.30966096936963,332.626232174776));
#60757=CARTESIAN_POINT('Ctrl Pts',(71.0686836090895,4.24179096587531,332.506967852023));
#60758=CARTESIAN_POINT('Ctrl Pts',(71.0609316355665,4.16901495845334,332.390690256276));
#60759=CARTESIAN_POINT('Ctrl Pts',(71.0531829450089,4.09626977171376,332.27446190416));
#60760=CARTESIAN_POINT('Ctrl Pts',(71.0454342544513,4.01862292037803,332.161218093932));
#60761=CARTESIAN_POINT('Ctrl Pts',(71.0376855638936,3.93635517117736,332.05139167931));
#60762=CARTESIAN_POINT('Ctrl Pts',(71.0299384855158,3.85410453846898,331.94158811499));
#60763=CARTESIAN_POINT('Ctrl Pts',(71.022191407138,3.7672351544122,331.835200844654));
#60764=CARTESIAN_POINT('Ctrl Pts',(71.0144443287601,3.67607018118065,331.732632392042));
#60765=CARTESIAN_POINT('Ctrl Pts',(71.0066971854543,3.58490444389888,331.630063079807));
#60766=CARTESIAN_POINT('Ctrl Pts',(70.9989500421485,3.48944330530694,331.531312941285));
#60767=CARTESIAN_POINT('Ctrl Pts',(70.9912028988427,3.39004888226507,331.436749849035));
#60768=CARTESIAN_POINT('Ctrl Pts',(70.9834540138146,3.29063211324677,331.342165496994));
#60769=CARTESIAN_POINT('Ctrl Pts',(70.9757051287865,3.18728058327983,331.251770333749));
#60770=CARTESIAN_POINT('Ctrl Pts',(70.9679562437584,3.08039147350133,331.165893659211));
#60771=CARTESIAN_POINT('Ctrl Pts',(70.9601991339837,2.97338891051727,331.079925834283));
#60772=CARTESIAN_POINT('Ctrl Pts',(70.952442024209,2.86284157230298,330.998486323662));
#60773=CARTESIAN_POINT('Ctrl Pts',(70.9446849144343,2.7491782158826,330.921862900807));
#60774=CARTESIAN_POINT('Ctrl Pts',(70.9369236595081,2.63545412139888,330.845198532844));
#60775=CARTESIAN_POINT('Ctrl Pts',(70.9291624045819,2.5186110236457,330.77335558533));
#60776=CARTESIAN_POINT('Ctrl Pts',(70.9214011496558,2.39910369812485,330.706576598081));
#60777=CARTESIAN_POINT('Ctrl Pts',(70.9136274792511,2.27940519983042,330.639690786216));
#60778=CARTESIAN_POINT('Ctrl Pts',(70.9058538088465,2.15703430631976,330.577885298496));
#60779=CARTESIAN_POINT('Ctrl Pts',(70.8980801384418,2.03246805859439,330.521355489292));
#60780=CARTESIAN_POINT('Ctrl Pts',(70.8906683342647,1.91370039966878,330.467457156307));
#60781=CARTESIAN_POINT('Ctrl Pts',(70.8832565300876,1.7929374409938,330.418354497947));
#60782=CARTESIAN_POINT('Ctrl Pts',(70.8758447259104,1.67060496832461,330.374174440999));
#60783=CARTESIAN_POINT('Ctrl Pts',(70.868069647132,1.54227661676101,330.327828987854));
#60784=CARTESIAN_POINT('Ctrl Pts',(70.8602945683536,1.41181546661236,330.286754419746));
#60785=CARTESIAN_POINT('Ctrl Pts',(70.8525194895751,1.27969376244737,330.251150988202));
#60786=CARTESIAN_POINT('Ctrl Pts',(70.8447539785261,1.14773464245056,330.215591368947));
#60787=CARTESIAN_POINT('Ctrl Pts',(70.8369884674771,1.01411940805555,330.18548959108));
#60788=CARTESIAN_POINT('Ctrl Pts',(70.8292229564281,0.879339129384364,330.160997441824));
#60789=CARTESIAN_POINT('Ctrl Pts',(70.8214651449059,0.744692485751883,330.136529576605));
#60790=CARTESIAN_POINT('Ctrl Pts',(70.8137073333836,0.608883478745489,330.117660340812));
#60791=CARTESIAN_POINT('Ctrl Pts',(70.8059495218615,0.472416807860145,330.104491300983));
#60792=CARTESIAN_POINT('Ctrl Pts',(70.7981975483385,0.336052832472621,330.091332171274));
#60793=CARTESIAN_POINT('Ctrl Pts',(70.7904455748155,0.199032565806501,330.083864736729));
#60794=CARTESIAN_POINT('Ctrl Pts',(70.7826936012925,0.0618689813671218,
330.082139154913));
#60795=CARTESIAN_POINT('Ctrl Pts',(70.7749449107349,-0.0752365142130927,
330.080414303881));
#60796=CARTESIAN_POINT('Ctrl Pts',(70.7671962201772,-0.212484816818216,
330.084426474049));
#60797=CARTESIAN_POINT('Ctrl Pts',(70.7594475296196,-0.349359991533065,
330.094173804667));
#60798=CARTESIAN_POINT('Ctrl Pts',(70.7517004512418,-0.486206688224612,
330.103919107271));
#60799=CARTESIAN_POINT('Ctrl Pts',(70.743953372864,-0.622680021800037,330.119397169123));
#60800=CARTESIAN_POINT('Ctrl Pts',(70.7362062944861,-0.758266619864602,
330.140554064947));
#60801=CARTESIAN_POINT('Ctrl Pts',(70.7284591511803,-0.893854354275453,
330.161711138087));
#60802=CARTESIAN_POINT('Ctrl Pts',(70.7207120078745,-1.02855495215148,330.188547079867));
#60803=CARTESIAN_POINT('Ctrl Pts',(70.7129648645687,-1.16186309939871,330.220956455445));
#60804=CARTESIAN_POINT('Ctrl Pts',(70.7052159795406,-1.29520121714737,330.253373117338));
#60805=CARTESIAN_POINT('Ctrl Pts',(70.6974670945125,-1.42714588159107,330.29136561409));
#60806=CARTESIAN_POINT('Ctrl Pts',(70.6897182094844,-1.55720523990546,330.334778150687));
#60807=CARTESIAN_POINT('Ctrl Pts',(70.6819610997097,-1.68740264456679,330.378236765798));
#60808=CARTESIAN_POINT('Ctrl Pts',(70.6742039899349,-1.8157103743963,330.427126788732));
#60809=CARTESIAN_POINT('Ctrl Pts',(70.6664468801602,-1.9416544095259,330.481243399289));
#60810=CARTESIAN_POINT('Ctrl Pts',(70.658685625234,-2.06766574512087,330.535388928032));
#60811=CARTESIAN_POINT('Ctrl Pts',(70.6509243703079,-2.19131051703725,330.594766440424));
#60812=CARTESIAN_POINT('Ctrl Pts',(70.6431631153817,-2.31213866325025,330.659124758254));
#60813=CARTESIAN_POINT('Ctrl Pts',(70.6353894449771,-2.43316009511939,330.723586028418));
#60814=CARTESIAN_POINT('Ctrl Pts',(70.6276157745724,-2.55135556042475,330.793043827636));
#60815=CARTESIAN_POINT('Ctrl Pts',(70.6198421041677,-2.6663026272486,330.867202719413));
#60816=CARTESIAN_POINT('Ctrl Pts',(70.6124302999907,-2.77589888045674,330.937909496936));
#60817=CARTESIAN_POINT('Ctrl Pts',(70.6050184958136,-2.88254211974617,331.012889379301));
#60818=CARTESIAN_POINT('Ctrl Pts',(70.5976066916365,-2.98589519257014,331.091853001551));
#60819=CARTESIAN_POINT('Ctrl Pts',(70.5899166867489,-3.09312760402905,331.173780508881));
#60820=CARTESIAN_POINT('Ctrl Pts',(70.5822266818613,-3.19717314114697,331.260268186912));
#60821=CARTESIAN_POINT('Ctrl Pts',(70.5745366769736,-3.2976128294936,331.351036765154));
#60822=CARTESIAN_POINT('Ctrl Pts',(70.5668561735593,-3.39792841843745,331.441693193243));
#60823=CARTESIAN_POINT('Ctrl Pts',(70.5591756701449,-3.49464672559058,331.536619736192));
#60824=CARTESIAN_POINT('Ctrl Pts',(70.5514951667306,-3.58737891189596,331.635494745883));
#60825=CARTESIAN_POINT('Ctrl Pts',(70.543822217071,-3.68001989634226,331.734272512264));
#60826=CARTESIAN_POINT('Ctrl Pts',(70.5361492674113,-3.76868228651825,331.836990730473));
#60827=CARTESIAN_POINT('Ctrl Pts',(70.5284763177517,-3.8530117975947,331.943288834369));
#60828=CARTESIAN_POINT('Ctrl Pts',(70.5206988618681,-3.93848988375168,332.051034727439));
#60829=CARTESIAN_POINT('Ctrl Pts',(70.5129214059844,-4.01951587272606,332.162458473482));
#60830=CARTESIAN_POINT('Ctrl Pts',(70.5051439501008,-4.09576054886704,332.277146976268));
#60831=CARTESIAN_POINT('Ctrl Pts',(70.4974796881985,-4.17089555128226,332.390166289485));
#60832=CARTESIAN_POINT('Ctrl Pts',(70.4898154262962,-4.24138725690919,332.506355619135));
#60833=CARTESIAN_POINT('Ctrl Pts',(70.4821511643939,-4.30696263371713,332.625288241857));
#60834=CARTESIAN_POINT('Ctrl Pts',(70.474488162776,-4.37252722754007,332.744201307715));
#60835=CARTESIAN_POINT('Ctrl Pts',(70.466825161158,-4.43317690716215,332.865856419115));
#60836=CARTESIAN_POINT('Ctrl Pts',(70.4591621595401,-4.48868383873161,332.989800890854));
#60837=CARTESIAN_POINT('Ctrl Pts',(70.4514986713872,-4.54419429451574,333.113753232006));
#60838=CARTESIAN_POINT('Ctrl Pts',(70.4438351832342,-4.59456118986911,333.239994857008));
#60839=CARTESIAN_POINT('Ctrl Pts',(70.4361716950813,-4.63960443655404,333.368052165415));
#60840=CARTESIAN_POINT('Ctrl Pts',(70.4283088352033,-4.68581951904256,333.49944098631));
#60841=CARTESIAN_POINT('Ctrl Pts',(70.4204459753253,-4.72642999964435,333.632740842062));
#60842=CARTESIAN_POINT('Ctrl Pts',(70.4125831154472,-4.76129589053794,333.767423631069));
#60843=CARTESIAN_POINT('Ctrl Pts',(70.4049096326925,-4.79532203581451,333.898862582651));
#60844=CARTESIAN_POINT('Ctrl Pts',(70.3972361499377,-4.82387712552781,334.031618203507));
#60845=CARTESIAN_POINT('Ctrl Pts',(70.389562667183,-4.84688309399061,334.165190239822));
#60846=CARTESIAN_POINT('Ctrl Pts',(70.3816051187433,-4.87074072347867,334.303706997226));
#60847=CARTESIAN_POINT('Ctrl Pts',(70.3736475703036,-4.88863041568758,334.443101301983));
#60848=CARTESIAN_POINT('Ctrl Pts',(70.3656900218639,-4.90052414871174,334.582811636796));
#60849=CARTESIAN_POINT('Ctrl Pts',(70.3577324734242,-4.91241788173591,334.722521971608));
#60850=CARTESIAN_POINT('Ctrl Pts',(70.3497749249845,-4.91831570313657,334.862547861314));
#60851=CARTESIAN_POINT('Ctrl Pts',(70.3418173765448,-4.9182494475218,335.002331191005));
#60852=CARTESIAN_POINT('',(68.5918173764684,-4.91824799793877,334.995562289857));
#60853=CARTESIAN_POINT('Ctrl Pts',(70.3418173765086,-4.9182494475215,335.00233119164));
#60854=CARTESIAN_POINT('Ctrl Pts',(70.3343344701266,-4.91818714382313,335.13377689728));
#60855=CARTESIAN_POINT('Ctrl Pts',(70.3268515637447,-4.91285578162596,335.265093143607));
#60856=CARTESIAN_POINT('Ctrl Pts',(70.3193686573627,-4.90228340698534,335.395980378423));
#60857=CARTESIAN_POINT('Ctrl Pts',(70.3115935785843,-4.89129823070352,335.531978145847));
#60858=CARTESIAN_POINT('Ctrl Pts',(70.3038184998059,-4.87463218996368,335.667733348066));
#60859=CARTESIAN_POINT('Ctrl Pts',(70.2960434210274,-4.85229867721284,335.802733211982));
#60860=CARTESIAN_POINT('Ctrl Pts',(70.2882779099784,-4.82999264727127,335.937566949971));
#60861=CARTESIAN_POINT('Ctrl Pts',(70.2805123989294,-4.80203308513411,336.071646817133));
#60862=CARTESIAN_POINT('Ctrl Pts',(70.2727468878804,-4.76848529200378,336.204462985087));
#60863=CARTESIAN_POINT('Ctrl Pts',(70.2649890763582,-4.73497076160801,336.337147465423));
#60864=CARTESIAN_POINT('Ctrl Pts',(70.2572312648361,-4.69587912172664,336.468570363484));
#60865=CARTESIAN_POINT('Ctrl Pts',(70.2494734533139,-4.65132702810783,336.598230252527));
#60866=CARTESIAN_POINT('Ctrl Pts',(70.2417214797909,-4.60680846135241,336.727792568392));
#60867=CARTESIAN_POINT('Ctrl Pts',(70.2339695062679,-4.55683774645756,336.855594147837));
#60868=CARTESIAN_POINT('Ctrl Pts',(70.2262175327449,-4.50158175651661,336.981147332203));
#60869=CARTESIAN_POINT('Ctrl Pts',(70.2184688421873,-4.44634916752002,337.106647344722));
#60870=CARTESIAN_POINT('Ctrl Pts',(70.2107201516297,-4.38583591245488,337.229900498997));
#60871=CARTESIAN_POINT('Ctrl Pts',(70.202971461072,-4.3202574353507,337.350437992119));
#60872=CARTESIAN_POINT('Ctrl Pts',(70.1952243826942,-4.25469260239645,337.470950406409));
#60873=CARTESIAN_POINT('Ctrl Pts',(70.1874773043164,-4.18406483029078,337.588747940268));
#60874=CARTESIAN_POINT('Ctrl Pts',(70.1797302259385,-4.10863588750571,337.703385693237));
#60875=CARTESIAN_POINT('Ctrl Pts',(70.1719830826327,-4.0332063125535,337.818024406982));
#60876=CARTESIAN_POINT('Ctrl Pts',(70.1642359393269,-3.9529757015129,337.929502960486));
#60877=CARTESIAN_POINT('Ctrl Pts',(70.1564887960212,-3.86824936532322,338.037405127766));
#60878=CARTESIAN_POINT('Ctrl Pts',(70.1487399109931,-3.78350398085437,338.145331553743));
#60879=CARTESIAN_POINT('Ctrl Pts',(70.1409910259649,-3.69426110133613,338.249679686165));
#60880=CARTESIAN_POINT('Ctrl Pts',(70.1332421409368,-3.60086629562431,338.350066414795));
#60881=CARTESIAN_POINT('Ctrl Pts',(70.1254850311621,-3.5073723597007,338.450559694936));
#60882=CARTESIAN_POINT('Ctrl Pts',(70.1177279213874,-3.40971796105718,338.547082885424));
#60883=CARTESIAN_POINT('Ctrl Pts',(70.1099708116127,-3.30828590026031,338.639289417543));
#60884=CARTESIAN_POINT('Ctrl Pts',(70.1022095566865,-3.20679963741346,338.731545221884));
#60885=CARTESIAN_POINT('Ctrl Pts',(70.0944483017604,-3.10153198987717,338.819479521121));
#60886=CARTESIAN_POINT('Ctrl Pts',(70.0866870468342,-2.99289802490024,338.902786757568));
#60887=CARTESIAN_POINT('Ctrl Pts',(70.0789133764296,-2.884090280983,338.986227258444));
#60888=CARTESIAN_POINT('Ctrl Pts',(70.0711397060249,-2.77190577880261,339.065025680773));
#60889=CARTESIAN_POINT('Ctrl Pts',(70.0633660356202,-2.656788419832,339.13891995027));
#60890=CARTESIAN_POINT('Ctrl Pts',(70.055954231443,-2.54702980161509,339.209374423746));
#60891=CARTESIAN_POINT('Ctrl Pts',(70.0485424272658,-2.4346054789703,339.275370900351));
#60892=CARTESIAN_POINT('Ctrl Pts',(70.0411306230886,-2.319918496392,339.33672240668));
#60893=CARTESIAN_POINT('Ctrl Pts',(70.0333555443101,-2.1996103631647,339.401080933089));
#60894=CARTESIAN_POINT('Ctrl Pts',(70.0255804655317,-2.07643196646708,339.460531033429));
#60895=CARTESIAN_POINT('Ctrl Pts',(70.0178053867533,-1.95082175555792,339.514806478748));
#60896=CARTESIAN_POINT('Ctrl Pts',(70.0100398757042,-1.82536611601003,339.569015134676));
#60897=CARTESIAN_POINT('Ctrl Pts',(70.0022743646552,-1.69748497185276,339.618061652006));
#60898=CARTESIAN_POINT('Ctrl Pts',(69.9945088536062,-1.56764238687685,339.661725046522));
#60899=CARTESIAN_POINT('Ctrl Pts',(69.986751042084,-1.43792854120187,339.705345148655));
#60900=CARTESIAN_POINT('Ctrl Pts',(69.9789932305618,-1.3062574930196,339.74359262588));
#60901=CARTESIAN_POINT('Ctrl Pts',(69.9712354190396,-1.17311403189479,339.776294225723));
#60902=CARTESIAN_POINT('Ctrl Pts',(69.9634834455166,-1.04007076544689,339.808971216574));
#60903=CARTESIAN_POINT('Ctrl Pts',(69.9557314719936,-0.905557669614834,
339.836110544232));
#60904=CARTESIAN_POINT('Ctrl Pts',(69.9479794984706,-0.770075131576116,
339.857588635756));
#60905=CARTESIAN_POINT('Ctrl Pts',(69.9402308079129,-0.634649970472694,
339.879057631296));
#60906=CARTESIAN_POINT('Ctrl Pts',(69.9324821173553,-0.49825656898606,339.894870098161));
#60907=CARTESIAN_POINT('Ctrl Pts',(69.9247334267977,-0.36140574261198,339.904953511676));
#60908=CARTESIAN_POINT('Ctrl Pts',(69.9169863484199,-0.224583389195327,
339.915034827254));
#60909=CARTESIAN_POINT('Ctrl Pts',(69.909239270042,-0.0873041897660356,
339.919389431704));
#60910=CARTESIAN_POINT('Ctrl Pts',(69.9014921916642,0.0499160714483651,
339.917996690555));
#60911=CARTESIAN_POINT('Ctrl Pts',(69.8937450483584,0.187137482700722,339.916603937733));
#60912=CARTESIAN_POINT('Ctrl Pts',(69.8859979050526,0.324299563898789,339.909463747203));
#60913=CARTESIAN_POINT('Ctrl Pts',(69.8782507617468,0.460887080464483,339.896607617684));
#60914=CARTESIAN_POINT('Ctrl Pts',(69.8705018767187,0.59750530480355,339.883748597834));
#60915=CARTESIAN_POINT('Ctrl Pts',(69.8627529916906,0.733548318389533,339.865171118482));
#60916=CARTESIAN_POINT('Ctrl Pts',(69.8550041066625,0.868506948514763,339.840958452918));
#60917=CARTESIAN_POINT('Ctrl Pts',(69.8472469968877,1.00360882512458,339.816720087782));
#60918=CARTESIAN_POINT('Ctrl Pts',(69.839489887113,1.1376236337522,339.78683465747));
#60919=CARTESIAN_POINT('Ctrl Pts',(69.8317327773383,1.27005278201869,339.751436518926));
#60920=CARTESIAN_POINT('Ctrl Pts',(69.8239715224121,1.40255269618767,339.71601946475));
#60921=CARTESIAN_POINT('Ctrl Pts',(69.816210267486,1.53346488874996,339.675083949135));
#60922=CARTESIAN_POINT('Ctrl Pts',(69.8084490125598,1.66230779302521,339.628813656192));
#60923=CARTESIAN_POINT('Ctrl Pts',(69.8006753421551,1.7913568039575,339.582469345859));
#60924=CARTESIAN_POINT('Ctrl Pts',(69.7929016717505,1.91832954965948,339.530773352398));
#60925=CARTESIAN_POINT('Ctrl Pts',(69.7851280013458,2.04276542571683,339.473957138596));
#60926=CARTESIAN_POINT('Ctrl Pts',(69.7777161971688,2.16140878180525,339.419785733216));
#60927=CARTESIAN_POINT('Ctrl Pts',(69.7703043929917,2.27774587884159,339.360960202206));
#60928=CARTESIAN_POINT('Ctrl Pts',(69.7628925888147,2.39140137639818,339.297718292241));
#60929=CARTESIAN_POINT('Ctrl Pts',(69.7551175100363,2.5106274684532,339.23137670788));
#60930=CARTESIAN_POINT('Ctrl Pts',(69.7473424312578,2.62727922456917,339.159965226741));
#60931=CARTESIAN_POINT('Ctrl Pts',(69.7395673524794,2.74089549708878,339.083708478398));
#60932=CARTESIAN_POINT('Ctrl Pts',(69.7318018414304,2.85437195755189,339.007545568838));
#60933=CARTESIAN_POINT('Ctrl Pts',(69.7240363303814,2.96482004525852,338.926549471308));
#60934=CARTESIAN_POINT('Ctrl Pts',(69.7162708193324,3.0718027983208,338.840990839709));
#60935=CARTESIAN_POINT('Ctrl Pts',(69.7085130078102,3.17867947767189,338.755517039743));
#60936=CARTESIAN_POINT('Ctrl Pts',(69.700755196288,3.28209735669928,338.665489950814));
#60937=CARTESIAN_POINT('Ctrl Pts',(69.6929973847658,3.38164839624971,338.571223485956));
#60938=CARTESIAN_POINT('Ctrl Pts',(69.6852454112428,3.48112452048593,338.477027959601));
#60939=CARTESIAN_POINT('Ctrl Pts',(69.6774934377198,3.5767393146198,338.378599675055));
#60940=CARTESIAN_POINT('Ctrl Pts',(69.6697414641967,3.66811807531676,338.276292546162));
#60941=CARTESIAN_POINT('Ctrl Pts',(69.6619927736391,3.75945813705432,338.174028744398));
#60942=CARTESIAN_POINT('Ctrl Pts',(69.6542440830815,3.8465654735813,338.067889656402));
#60943=CARTESIAN_POINT('Ctrl Pts',(69.6464953925239,3.92910266577651,337.958265590559));
#60944=CARTESIAN_POINT('Ctrl Pts',(69.6387483141461,4.01162268541953,337.848664332919));
#60945=CARTESIAN_POINT('Ctrl Pts',(69.6310012357682,4.08957421709364,337.735579851731));
#60946=CARTESIAN_POINT('Ctrl Pts',(69.6232541573904,4.16266078838846,337.619434714459));
#60947=CARTESIAN_POINT('Ctrl Pts',(69.6155070140846,4.2357479722191,337.503288603779));
#60948=CARTESIAN_POINT('Ctrl Pts',(69.6077598707788,4.30396990616789,337.384082116675));
#60949=CARTESIAN_POINT('Ctrl Pts',(69.600012727473,4.36707425518542,337.262265570661));
#60950=CARTESIAN_POINT('Ctrl Pts',(69.5922638424449,4.43019279140031,337.140421637701));
#60951=CARTESIAN_POINT('Ctrl Pts',(69.5845149574168,4.48819127347767,337.015966825173));
#60952=CARTESIAN_POINT('Ctrl Pts',(69.5767660723887,4.54086418513642,336.889374371226));
#60953=CARTESIAN_POINT('Ctrl Pts',(69.569008962614,4.59359300436785,336.76264755074));
#60954=CARTESIAN_POINT('Ctrl Pts',(69.5612518528393,4.64098481115718,336.633778917917));
#60955=CARTESIAN_POINT('Ctrl Pts',(69.5534947430645,4.68288277218002,336.503260457978));
#60956=CARTESIAN_POINT('Ctrl Pts',(69.5457334881384,4.72480312213359,336.372672253146));
#60957=CARTESIAN_POINT('Ctrl Pts',(69.5379722332122,4.76122367286807,336.240432841153));
#60958=CARTESIAN_POINT('Ctrl Pts',(69.530210978286,4.79203828490623,336.107046583705));
#60959=CARTESIAN_POINT('Ctrl Pts',(69.5224373078814,4.82290219028119,335.973446951715));
#60960=CARTESIAN_POINT('Ctrl Pts',(69.5146636374767,4.84814216488861,335.838697192633));
#60961=CARTESIAN_POINT('Ctrl Pts',(69.5068899670721,4.86770359124532,335.703309896331));
#60962=CARTESIAN_POINT('Ctrl Pts',(69.499478162895,4.88635442849899,335.574224911244));
#60963=CARTESIAN_POINT('Ctrl Pts',(69.4920663587178,4.89984346311244,335.444560694164));
#60964=CARTESIAN_POINT('Ctrl Pts',(69.4846545545407,4.9081675030951,335.314761535231));
#60965=CARTESIAN_POINT('Ctrl Pts',(69.4768794757623,4.91689952907331,335.178600532868));
#60966=CARTESIAN_POINT('Ctrl Pts',(69.4691043969839,4.91997504979721,335.04186073246));
#60967=CARTESIAN_POINT('Ctrl Pts',(69.4613293182054,4.91733340760958,334.905051482862));
#60968=CARTESIAN_POINT('Ctrl Pts',(69.4535638071564,4.91469501613083,334.768410585754));
#60969=CARTESIAN_POINT('Ctrl Pts',(69.4457982961074,4.90635346750967,334.631700796567));
#60970=CARTESIAN_POINT('Ctrl Pts',(69.4380327850584,4.89229989523602,334.495436032228));
#60971=CARTESIAN_POINT('Ctrl Pts',(69.4302749735362,4.8782602571202,334.3593063748));
#60972=CARTESIAN_POINT('Ctrl Pts',(69.422517162014,4.85851990585494,334.22362125043));
#60973=CARTESIAN_POINT('Ctrl Pts',(69.4147593504918,4.83312200420676,334.0888936643));
#60974=CARTESIAN_POINT('Ctrl Pts',(69.4070073769688,4.80774321528501,333.954267464951));
#60975=CARTESIAN_POINT('Ctrl Pts',(69.3992554034458,4.77671542241618,333.82059775213));
#60976=CARTESIAN_POINT('Ctrl Pts',(69.3915034299228,4.74013346582818,333.688391144954));
#60977=CARTESIAN_POINT('Ctrl Pts',(69.3837547393651,4.7035670017205,333.556240527354));
#60978=CARTESIAN_POINT('Ctrl Pts',(69.3760060488075,4.66145115625928,333.425552158941));
#60979=CARTESIAN_POINT('Ctrl Pts',(69.3682573582499,4.61393155124512,333.296821000915));
#60980=CARTESIAN_POINT('Ctrl Pts',(69.3605102798721,4.56642183308168,333.168116626482));
#60981=CARTESIAN_POINT('Ctrl Pts',(69.3527632014942,4.51351072694607,333.041369018917));
#60982=CARTESIAN_POINT('Ctrl Pts',(69.3450161231164,4.45539314060015,332.917056163697));
#60983=CARTESIAN_POINT('Ctrl Pts',(69.3372689798106,4.39727506717287,332.792742266615));
#60984=CARTESIAN_POINT('Ctrl Pts',(69.3295218365048,4.33395059204179,332.670863516668));
#60985=CARTESIAN_POINT('Ctrl Pts',(69.321774693199,4.26566184383653,332.551875800427));
#60986=CARTESIAN_POINT('Ctrl Pts',(69.3140258081709,4.19735774287091,332.43286133322));
#60987=CARTESIAN_POINT('Ctrl Pts',(69.3062769231428,4.12408734249344,332.316739532024));
#60988=CARTESIAN_POINT('Ctrl Pts',(69.2985280381147,4.04613738210735,332.203939316178));
#60989=CARTESIAN_POINT('Ctrl Pts',(69.29077092834,3.96810468482788,332.091019373018));
#60990=CARTESIAN_POINT('Ctrl Pts',(69.2830138185653,3.88538272819031,331.981428379928));
#60991=CARTESIAN_POINT('Ctrl Pts',(69.2752567087905,3.79830036155177,331.875564462829));
#60992=CARTESIAN_POINT('Ctrl Pts',(69.2674954538644,3.71117146088084,331.769643975438));
#60993=CARTESIAN_POINT('Ctrl Pts',(69.2597341989382,3.61967776794487,331.667454823602));
#60994=CARTESIAN_POINT('Ctrl Pts',(69.251972944012,3.52418597310136,331.569359201331));
#60995=CARTESIAN_POINT('Ctrl Pts',(69.2441992736074,3.42854142250688,331.471106658033));
#60996=CARTESIAN_POINT('Ctrl Pts',(69.2364256032027,3.32888627386391,331.376960998336));
#60997=CARTESIAN_POINT('Ctrl Pts',(69.228651932798,3.22562201827858,331.287245543037));
#60998=CARTESIAN_POINT('Ctrl Pts',(69.2212401286209,3.12716473863469,331.201706363767));
#60999=CARTESIAN_POINT('Ctrl Pts',(69.2138283244439,3.02542702285736,331.120194398792));
#61000=CARTESIAN_POINT('Ctrl Pts',(69.2064165202668,2.92078075663575,331.042952763213));
#61001=CARTESIAN_POINT('Ctrl Pts',(69.1986414414883,2.8110054651814,330.961925284983));
#61002=CARTESIAN_POINT('Ctrl Pts',(69.1908663627099,2.69768239053949,330.885341261864));
#61003=CARTESIAN_POINT('Ctrl Pts',(69.1830912839315,2.5812070296896,330.813527340065));
#61004=CARTESIAN_POINT('Ctrl Pts',(69.1753257728825,2.46487499918649,330.74180178987));
#61005=CARTESIAN_POINT('Ctrl Pts',(69.1675602618335,2.34539873028618,330.674834864729));
#61006=CARTESIAN_POINT('Ctrl Pts',(69.1597947507845,2.22320558852179,330.61291213062));
#61007=CARTESIAN_POINT('Ctrl Pts',(69.1520369392623,2.10113360161322,330.551050793081));
#61008=CARTESIAN_POINT('Ctrl Pts',(69.14427912774,1.97635044904432,330.494223869195));
#61009=CARTESIAN_POINT('Ctrl Pts',(69.1365213162179,1.84931088566766,330.442672679009));
#61010=CARTESIAN_POINT('Ctrl Pts',(69.1287693426949,1.72236692359109,330.391160282729));
#61011=CARTESIAN_POINT('Ctrl Pts',(69.1210173691719,1.59317029126581,330.344915864127));
#61012=CARTESIAN_POINT('Ctrl Pts',(69.1132653956489,1.46219833900484,330.304133830707));
#61013=CARTESIAN_POINT('Ctrl Pts',(69.1055167050913,1.33128185344349,330.263369068502));
#61014=CARTESIAN_POINT('Ctrl Pts',(69.0977680145337,1.19859191574505,330.228062206407));
#61015=CARTESIAN_POINT('Ctrl Pts',(69.090019323976,1.06462355365488,330.19835863985));
#61016=CARTESIAN_POINT('Ctrl Pts',(69.0822722455982,0.930683064801266,330.168661253368));
#61017=CARTESIAN_POINT('Ctrl Pts',(69.0745251672204,0.795465061989936,330.144564928097));
#61018=CARTESIAN_POINT('Ctrl Pts',(69.0667780888426,0.659476969178747,330.12616442731));
#61019=CARTESIAN_POINT('Ctrl Pts',(69.0590309455368,0.523487736656453,330.107763772309));
#61020=CARTESIAN_POINT('Ctrl Pts',(69.051283802231,0.386728788605607,330.095059089417));
#61021=CARTESIAN_POINT('Ctrl Pts',(69.0435366589251,0.249714519465306,330.088093473887));
#61022=CARTESIAN_POINT('Ctrl Pts',(69.0357877738971,0.112669446608407,330.081126292339));
#61023=CARTESIAN_POINT('Ctrl Pts',(69.028038888869,-0.0246306712668604,
330.079900765477));
#61024=CARTESIAN_POINT('Ctrl Pts',(69.0202900038409,-0.161669975591024,
330.084407880886));
#61025=CARTESIAN_POINT('Ctrl Pts',(69.0125328940661,-0.298854734848679,
330.088919780194));
#61026=CARTESIAN_POINT('Ctrl Pts',(69.0047757842914,-0.43577773628084,330.099176463635));
#61027=CARTESIAN_POINT('Ctrl Pts',(68.9970186745167,-0.571926228050113,
330.11511684355));
#61028=CARTESIAN_POINT('Ctrl Pts',(68.9892574195905,-0.708147473220204,
330.131065741494));
#61029=CARTESIAN_POINT('Ctrl Pts',(68.9814961646644,-0.84359299826389,330.152704326145));
#61030=CARTESIAN_POINT('Ctrl Pts',(68.9737349097382,-0.977759789317654,
330.179920243721));
#61031=CARTESIAN_POINT('Ctrl Pts',(68.9659612393335,-1.11214120351225,330.207179697895));
#61032=CARTESIAN_POINT('Ctrl Pts',(68.9581875689289,-1.2452394164035,330.240034219899));
#61033=CARTESIAN_POINT('Ctrl Pts',(68.9504138985242,-1.37656527075809,330.278321154733));
#61034=CARTESIAN_POINT('Ctrl Pts',(68.9430020943471,-1.50177787499784,330.31482582354));
#61035=CARTESIAN_POINT('Ctrl Pts',(68.93559029017,-1.62537914104378,330.356268437812));
#61036=CARTESIAN_POINT('Ctrl Pts',(68.9281784859929,-1.74696337953491,330.402467834472));
#61037=CARTESIAN_POINT('Ctrl Pts',(68.9204034072145,-1.87450682373488,330.450931601183));
#61038=CARTESIAN_POINT('Ctrl Pts',(68.912628328436,-2.00023358078962,330.504783382991));
#61039=CARTESIAN_POINT('Ctrl Pts',(68.9048532496576,-2.1236549408234,330.563867365056));
#61040=CARTESIAN_POINT('Ctrl Pts',(68.8970877386086,-2.24692442301627,330.622878640519));
#61041=CARTESIAN_POINT('Ctrl Pts',(68.8893222275596,-2.3678938036929,330.687109138197));
#61042=CARTESIAN_POINT('Ctrl Pts',(68.8815567165105,-2.48609167231881,330.756354013431));
#61043=CARTESIAN_POINT('Ctrl Pts',(68.8737989049883,-2.60417234741377,330.825530232169));
#61044=CARTESIAN_POINT('Ctrl Pts',(68.8660410934661,-2.71948664397022,330.899710738053));
#61045=CARTESIAN_POINT('Ctrl Pts',(68.8582832819439,-2.83158553686556,330.97864371015));
#61046=CARTESIAN_POINT('Ctrl Pts',(68.8505313084209,-2.94360007178898,331.057517282683));
#61047=CARTESIAN_POINT('Ctrl Pts',(68.8427793348979,-3.05240370102488,331.141135978685));
#61048=CARTESIAN_POINT('Ctrl Pts',(68.8350273613749,-3.15757462151169,331.229203589149));
#61049=CARTESIAN_POINT('Ctrl Pts',(68.8272786708173,-3.26270100205136,331.317233902928));
#61050=CARTESIAN_POINT('Ctrl Pts',(68.8195299802597,-3.36419743466158,331.409709133368));
#61051=CARTESIAN_POINT('Ctrl Pts',(68.811781289702,-3.46167376530756,331.506291682885));
#61052=CARTESIAN_POINT('Ctrl Pts',(68.8040342113242,-3.55912981518887,331.602854137596));
#61053=CARTESIAN_POINT('Ctrl Pts',(68.7962871329463,-3.65256714931052,331.703521936658));
#61054=CARTESIAN_POINT('Ctrl Pts',(68.7885400545685,-3.7416314829952,331.807919658286));
#61055=CARTESIAN_POINT('Ctrl Pts',(68.7807929112627,-3.83069656312466,331.912318254866));
#61056=CARTESIAN_POINT('Ctrl Pts',(68.7730457679569,-3.91538831602784,332.020446538999));
#61057=CARTESIAN_POINT('Ctrl Pts',(68.7652986246511,-3.9953921336405,332.131895266741));
#61058=CARTESIAN_POINT('Ctrl Pts',(68.757549739623,-4.07541393780995,332.243369050522));
#61059=CARTESIAN_POINT('Ctrl Pts',(68.7498008545949,-4.15074548155537,332.358164445908));
#61060=CARTESIAN_POINT('Ctrl Pts',(68.7420519695668,-4.2211151829362,332.475842779285));
#61061=CARTESIAN_POINT('Ctrl Pts',(68.734294859792,-4.29155957544508,332.593646017662));
#61062=CARTESIAN_POINT('Ctrl Pts',(68.7265377500173,-4.35703140423779,332.714337970629));
#61063=CARTESIAN_POINT('Ctrl Pts',(68.7187806402426,-4.41730455978964,332.837454396189));
#61064=CARTESIAN_POINT('Ctrl Pts',(68.7110193853164,-4.47760992338861,332.960636611231));
#61065=CARTESIAN_POINT('Ctrl Pts',(68.7032581303902,-4.53271092138012,333.08624552262));
#61066=CARTESIAN_POINT('Ctrl Pts',(68.6954968754641,-4.58242982479273,333.213797334189));
#61067=CARTESIAN_POINT('Ctrl Pts',(68.6877232050594,-4.63222826224748,333.341553187088));
#61068=CARTESIAN_POINT('Ctrl Pts',(68.6799495346548,-4.67662727394311,333.471257780882));
#61069=CARTESIAN_POINT('Ctrl Pts',(68.6721758642501,-4.71549892889219,333.602411750866));
#61070=CARTESIAN_POINT('Ctrl Pts',(68.664764060073,-4.75256109895122,333.727460471993));
#61071=CARTESIAN_POINT('Ctrl Pts',(68.657352255896,-4.78459885776639,333.853826390087));
#61072=CARTESIAN_POINT('Ctrl Pts',(68.6499404517189,-4.81154500744351,333.981070314572));
#61073=CARTESIAN_POINT('Ctrl Pts',(68.639026225491,-4.85122446557838,334.168442908989));
#61074=CARTESIAN_POINT('Ctrl Pts',(68.6281119992631,-4.87997008721691,334.35820527783));
#61075=CARTESIAN_POINT('Ctrl Pts',(68.6171977730352,-4.89755553794552,334.549297420421));
#61076=CARTESIAN_POINT('Ctrl Pts',(68.6087376408596,-4.91118685128135,334.697421964504));
#61077=CARTESIAN_POINT('Ctrl Pts',(68.6002775086841,-4.91811336021633,334.846345332992));
#61078=CARTESIAN_POINT('Ctrl Pts',(68.5918173765086,-4.91824799793813,334.995562289148));
#61079=CARTESIAN_POINT('',(66.8418173765624,-4.91824999982528,334.99995854384));
#61080=CARTESIAN_POINT('Ctrl Pts',(68.5918173764684,-4.91824799793877,334.995562289857));
#61081=CARTESIAN_POINT('Ctrl Pts',(68.5841669567107,-4.91836974957348,335.130497811652));
#61082=CARTESIAN_POINT('Ctrl Pts',(68.5765165369531,-4.91293425515066,335.265607840655));
#61083=CARTESIAN_POINT('Ctrl Pts',(68.5688661171954,-4.90192521624238,335.400390105856));
#61084=CARTESIAN_POINT('Ctrl Pts',(68.5612218503107,-4.89092503138647,335.535063972017));
#61085=CARTESIAN_POINT('Ctrl Pts',(68.553577583426,-4.87436025167078,335.669410199118));
#61086=CARTESIAN_POINT('Ctrl Pts',(68.5459333165412,-4.85226664415567,335.802926818903));
#61087=CARTESIAN_POINT('Ctrl Pts',(68.5382926658293,-4.83018348817305,335.936380277736));
#61088=CARTESIAN_POINT('Ctrl Pts',(68.5306520151174,-4.80257676992838,336.069004512944));
#61089=CARTESIAN_POINT('Ctrl Pts',(68.5230113644055,-4.76953402762972,336.200303387391));
#61090=CARTESIAN_POINT('Ctrl Pts',(68.5153724381459,-4.73649874289362,336.331572628415));
#61091=CARTESIAN_POINT('Ctrl Pts',(68.5077335118862,-4.69802997143603,336.461516712868));
#61092=CARTESIAN_POINT('Ctrl Pts',(68.5000945856265,-4.65426610759358,336.589650924639));
#61093=CARTESIAN_POINT('Ctrl Pts',(68.4924556208709,-4.61050202320521,336.717785782136));
#61094=CARTESIAN_POINT('Ctrl Pts',(68.4848166561152,-4.56144292382961,336.844110367576));
#61095=CARTESIAN_POINT('Ctrl Pts',(68.4771776913595,-4.50727651927473,336.968156863996));
#61096=CARTESIAN_POINT('Ctrl Pts',(68.4695369253401,-4.45309734231094,337.092232610513));
#61097=CARTESIAN_POINT('Ctrl Pts',(68.4618961593207,-4.39380862705637,337.214028830905));
#61098=CARTESIAN_POINT('Ctrl Pts',(68.4542553933013,-4.32964525353834,337.333099878062));
#61099=CARTESIAN_POINT('Ctrl Pts',(68.4466066995075,-4.26541530649257,337.452294468905));
#61100=CARTESIAN_POINT('Ctrl Pts',(68.4389580057136,-4.19630079483433,337.568757886408));
#61101=CARTESIAN_POINT('Ctrl Pts',(68.4313093119198,-4.12258153727244,337.682070940717));
#61102=CARTESIAN_POINT('Ctrl Pts',(68.4236562563777,-4.0488202405258,337.795448612992));
#61103=CARTESIAN_POINT('Ctrl Pts',(68.4160032008355,-3.97044920342802,337.905672018035));
#61104=CARTESIAN_POINT('Ctrl Pts',(68.4083501452933,-3.88778939609991,338.012354008757));
#61105=CARTESIAN_POINT('Ctrl Pts',(68.4006857519601,-3.80500713054283,338.119194045911));
#61106=CARTESIAN_POINT('Ctrl Pts',(68.3930213586268,-3.71792366853709,338.222481886915));
#61107=CARTESIAN_POINT('Ctrl Pts',(68.3853569652935,-3.6268980684741,338.321865961083));
#61108=CARTESIAN_POINT('Ctrl Pts',(68.3808054493441,-3.57284232622804,338.38088540059));
#61109=CARTESIAN_POINT('Ctrl Pts',(68.3762539333946,-3.51739702621145,338.43852886839));
#61110=CARTESIAN_POINT('Ctrl Pts',(68.3717024174451,-3.46064280031056,338.494729527611));
#61111=CARTESIAN_POINT('Ctrl Pts',(68.3639273386667,-3.36369299670928,338.590733706811));
#61112=CARTESIAN_POINT('Ctrl Pts',(68.3561522598883,-3.26259198530339,338.682852202978));
#61113=CARTESIAN_POINT('Ctrl Pts',(68.3483771811098,-3.15768405087805,338.770704774618));
#61114=CARTESIAN_POINT('Ctrl Pts',(68.3406116700608,-3.05290521234471,338.858449238076));
#61115=CARTESIAN_POINT('Ctrl Pts',(68.3328461590118,-2.94432906873354,338.941937973434));
#61116=CARTESIAN_POINT('Ctrl Pts',(68.3250806479628,-2.83233736183333,339.020826796974));
#61117=CARTESIAN_POINT('Ctrl Pts',(68.3173228364406,-2.72045669503679,339.099637402015));
#61118=CARTESIAN_POINT('Ctrl Pts',(68.3095650249184,-2.60516752185295,339.173856947891));
#61119=CARTESIAN_POINT('Ctrl Pts',(68.3018072133962,-2.48688506491217,339.243181086923));
#61120=CARTESIAN_POINT('Ctrl Pts',(68.2940552398732,-2.3686916192711,339.312453057341));
#61121=CARTESIAN_POINT('Ctrl Pts',(68.2863032663502,-2.24750970931159,339.376836756789));
#61122=CARTESIAN_POINT('Ctrl Pts',(68.2785512928272,-2.12378367906824,339.436071003379));
#61123=CARTESIAN_POINT('Ctrl Pts',(68.2708026022696,-2.00011004687207,339.495280164231));
#61124=CARTESIAN_POINT('Ctrl Pts',(68.263053911712,-1.87389478915699,339.549344041241));
#61125=CARTESIAN_POINT('Ctrl Pts',(68.2553052211544,-1.74560680731257,339.598047404797));
#61126=CARTESIAN_POINT('Ctrl Pts',(68.2475581427765,-1.61734551685426,339.646740635212));
#61127=CARTESIAN_POINT('Ctrl Pts',(68.2398110643987,-1.48701272524551,339.690075431939));
#61128=CARTESIAN_POINT('Ctrl Pts',(68.2320639860209,-1.35509689867547,339.727884882027));
#61129=CARTESIAN_POINT('Ctrl Pts',(68.2243168427151,-1.22317996652401,339.765694648995));
#61130=CARTESIAN_POINT('Ctrl Pts',(68.2165696994093,-1.08968034869367,339.797978869266));
#61131=CARTESIAN_POINT('Ctrl Pts',(68.2088225561035,-0.955100856407698,
339.824620753654));
#61132=CARTESIAN_POINT('Ctrl Pts',(68.2010736710754,-0.820491107794473,
339.851268627704));
#61133=CARTESIAN_POINT('Ctrl Pts',(68.1933247860473,-0.684801384981352,
339.872271565774));
#61134=CARTESIAN_POINT('Ctrl Pts',(68.1855759010192,-0.548543458744524,
339.887564131177));
#61135=CARTESIAN_POINT('Ctrl Pts',(68.1778187912445,-0.41214090693698,339.902872928267));
#61136=CARTESIAN_POINT('Ctrl Pts',(68.1700616814697,-0.275169336012001,
339.912459201514));
#61137=CARTESIAN_POINT('Ctrl Pts',(68.162304571695,-0.138144948494133,339.916309493482));
#61138=CARTESIAN_POINT('Ctrl Pts',(68.1545433167688,-0.00104733952457867,
339.920161842924));
#61139=CARTESIAN_POINT('Ctrl Pts',(68.1467820618427,0.136102751636794,339.918272108931));
#61140=CARTESIAN_POINT('Ctrl Pts',(68.1390208069165,0.272791369337971,339.910678968464));
#61141=CARTESIAN_POINT('Ctrl Pts',(68.1312471365118,0.409698644280568,339.903073681447));
#61142=CARTESIAN_POINT('Ctrl Pts',(68.1234734661072,0.546142581378811,339.889746794335));
#61143=CARTESIAN_POINT('Ctrl Pts',(68.1156997957025,0.681615686580704,339.870788757307));
#61144=CARTESIAN_POINT('Ctrl Pts',(68.1082879915253,0.810782486143793,339.852713221464));
#61145=CARTESIAN_POINT('Ctrl Pts',(68.1008761873482,0.939066521009833,339.82951904882));
#61146=CARTESIAN_POINT('Ctrl Pts',(68.093464383171,1.0660402256666,339.801327035285));
#61147=CARTESIAN_POINT('Ctrl Pts',(68.0856893043926,1.1992372898225,339.771753247187));
#61148=CARTESIAN_POINT('Ctrl Pts',(68.0779142256141,1.33141325695796,339.736585853835));
#61149=CARTESIAN_POINT('Ctrl Pts',(68.0701391468357,1.46206206163609,339.695908601157));
#61150=CARTESIAN_POINT('Ctrl Pts',(68.0623736357867,1.59255009464246,339.655281404429));
#61151=CARTESIAN_POINT('Ctrl Pts',(68.0546081247376,1.72151433476501,339.609157954181));
#61152=CARTESIAN_POINT('Ctrl Pts',(68.0468426136886,1.8484587681849,339.557673007667));
#61153=CARTESIAN_POINT('Ctrl Pts',(68.0390848021664,1.97527733582913,339.506239108628));
#61154=CARTESIAN_POINT('Ctrl Pts',(68.0313269906443,2.10007972226158,339.449454438301));
#61155=CARTESIAN_POINT('Ctrl Pts',(68.0235691791221,2.22238529423551,339.387503466263));
#61156=CARTESIAN_POINT('Ctrl Pts',(68.0158172055991,2.34459882738826,339.325599114295));
#61157=CARTESIAN_POINT('Ctrl Pts',(68.0080652320761,2.4643189387153,339.258536375014));
#61158=CARTESIAN_POINT('Ctrl Pts',(68.0003132585531,2.58108553474316,339.186547566294));
#61159=CARTESIAN_POINT('Ctrl Pts',(67.9925645679955,2.69780268004835,339.114589244877));
#61160=CARTESIAN_POINT('Ctrl Pts',(67.9848158774378,2.81156846580788,339.037709208014));
#61161=CARTESIAN_POINT('Ctrl Pts',(67.9770671868802,2.9219481514017,338.956185291796));
#61162=CARTESIAN_POINT('Ctrl Pts',(67.9693201085024,3.03230487158003,338.874678337309));
#61163=CARTESIAN_POINT('Ctrl Pts',(67.9615730301245,3.13927657868824,338.788529657376));
#61164=CARTESIAN_POINT('Ctrl Pts',(67.9538259517467,3.24245857498245,338.698059687461));
#61165=CARTESIAN_POINT('Ctrl Pts',(67.9460788084408,3.34564143604117,338.60758895932));
#61166=CARTESIAN_POINT('Ctrl Pts',(67.938331665135,3.44503422903476,338.512797126654));
#61167=CARTESIAN_POINT('Ctrl Pts',(67.9305845218292,3.54026664344243,338.414043812816));
#61168=CARTESIAN_POINT('Ctrl Pts',(67.9228356368011,3.63552046811895,338.315268297137));
#61169=CARTESIAN_POINT('Ctrl Pts',(67.915086751773,3.72661178170897,338.212529809348));
#61170=CARTESIAN_POINT('Ctrl Pts',(67.9073378667448,3.81320860857434,338.106223296866));
#61171=CARTESIAN_POINT('Ctrl Pts',(67.8995807569701,3.89989735020622,337.999803949554));
#61172=CARTESIAN_POINT('Ctrl Pts',(67.8918236471954,3.98208182834817,337.889809315917));
#61173=CARTESIAN_POINT('Ctrl Pts',(67.8840665374206,4.05947137955017,337.77666619908));
#61174=CARTESIAN_POINT('Ctrl Pts',(67.8763052824944,4.13690228525394,337.663462622179));
#61175=CARTESIAN_POINT('Ctrl Pts',(67.8685440275683,4.20953295162168,337.547107541056));
#61176=CARTESIAN_POINT('Ctrl Pts',(67.8607827726421,4.27711777203967,337.428054082306));
#61177=CARTESIAN_POINT('Ctrl Pts',(67.8530091022375,4.34481070614445,337.308810176822));
#61178=CARTESIAN_POINT('Ctrl Pts',(67.8452354318327,4.40744148597028,337.186859615899));
#61179=CARTESIAN_POINT('Ctrl Pts',(67.8374617614281,4.46481153885143,337.062678109895));
#61180=CARTESIAN_POINT('Ctrl Pts',(67.830049957251,4.51951100196802,336.944277282873));
#61181=CARTESIAN_POINT('Ctrl Pts',(67.8226381530741,4.56942837956783,336.823848803438));
#61182=CARTESIAN_POINT('Ctrl Pts',(67.815226348897,4.6144338712744,336.701817590148));
#61183=CARTESIAN_POINT('Ctrl Pts',(67.8074512701186,4.66164521619439,336.573805263581));
#61184=CARTESIAN_POINT('Ctrl Pts',(67.7996761913402,4.70360020493318,336.443624578518));
#61185=CARTESIAN_POINT('Ctrl Pts',(67.7919011125617,4.74009540018406,336.31174641591));
#61186=CARTESIAN_POINT('Ctrl Pts',(67.7841356015127,4.77654568577369,336.180030537778));
#61187=CARTESIAN_POINT('Ctrl Pts',(67.7763700904637,4.80754944275621,336.046621711435));
#61188=CARTESIAN_POINT('Ctrl Pts',(67.7686045794148,4.83295156984315,335.912009970368));
#61189=CARTESIAN_POINT('Ctrl Pts',(67.7608467678926,4.8583285106471,335.777531697234));
#61190=CARTESIAN_POINT('Ctrl Pts',(67.7530889563704,4.87811480237946,335.641853264523));
#61191=CARTESIAN_POINT('Ctrl Pts',(67.7453311448482,4.89220547121353,335.505478674059));
#61192=CARTESIAN_POINT('Ctrl Pts',(67.7375791713252,4.90628553637245,335.369206709799));
#61193=CARTESIAN_POINT('Ctrl Pts',(67.7298271978023,4.91467846996816,335.232240017784));
#61194=CARTESIAN_POINT('Ctrl Pts',(67.7220752242793,4.91733065007793,335.095091220963));
#61195=CARTESIAN_POINT('Ctrl Pts',(67.7143265337216,4.91998170698785,334.958000506738));
#61196=CARTESIAN_POINT('Ctrl Pts',(67.706577843164,4.91689683838061,334.820728231084));
#61197=CARTESIAN_POINT('Ctrl Pts',(67.6988291526064,4.90807441945593,334.683790329714));
#61198=CARTESIAN_POINT('Ctrl Pts',(67.6910820742286,4.8992538361092,334.546880919418));
#61199=CARTESIAN_POINT('Ctrl Pts',(67.6833349958508,4.88469810200353,334.410306134847));
#61200=CARTESIAN_POINT('Ctrl Pts',(67.675587917473,4.86445767298652,334.274579700985));
#61201=CARTESIAN_POINT('Ctrl Pts',(67.6678407741671,4.84421707433522,334.138852129605));
#61202=CARTESIAN_POINT('Ctrl Pts',(67.6600936308613,4.81829174339686,334.003973309714));
#61203=CARTESIAN_POINT('Ctrl Pts',(67.6523464875555,4.78678369885221,333.870449256163));
#61204=CARTESIAN_POINT('Ctrl Pts',(67.6445976025274,4.75526857063036,333.73689518357));
#61205=CARTESIAN_POINT('Ctrl Pts',(67.6368487174994,4.7181683210212,333.604696863749));
#61206=CARTESIAN_POINT('Ctrl Pts',(67.6290998324713,4.67563541866781,333.474347190807));
#61207=CARTESIAN_POINT('Ctrl Pts',(67.6213427226966,4.63305737145227,333.343859163374));
#61208=CARTESIAN_POINT('Ctrl Pts',(67.6135856129219,4.58503527426134,333.215224074624));
#61209=CARTESIAN_POINT('Ctrl Pts',(67.6058285031472,4.53177074027741,333.088917317313));
#61210=CARTESIAN_POINT('Ctrl Pts',(67.598067248221,4.47847774342953,332.96254306571));
#61211=CARTESIAN_POINT('Ctrl Pts',(67.5903059932948,4.41993689450501,332.838499978005));
#61212=CARTESIAN_POINT('Ctrl Pts',(67.5825447383686,4.35639632549274,332.717239802841));
#61213=CARTESIAN_POINT('Ctrl Pts',(67.574771067964,4.29275411227796,332.595785650916));
#61214=CARTESIAN_POINT('Ctrl Pts',(67.5669973975593,4.22409639261416,332.477123645954));
#61215=CARTESIAN_POINT('Ctrl Pts',(67.5592237271547,4.15071574242629,332.361678206118));
#61216=CARTESIAN_POINT('Ctrl Pts',(67.5518119229775,4.08075097915844,332.251606779279));
#61217=CARTESIAN_POINT('Ctrl Pts',(67.5444001188004,4.0064932588492,332.144459431106));
#61218=CARTESIAN_POINT('Ctrl Pts',(67.5369883146232,3.92822966214747,332.040575261318));
#61219=CARTESIAN_POINT('Ctrl Pts',(67.5292132358448,3.84613013343676,331.931599418913));
#61220=CARTESIAN_POINT('Ctrl Pts',(67.5214381570663,3.75936266986788,331.825870335359));
#61221=CARTESIAN_POINT('Ctrl Pts',(67.5136630782879,3.66821315367794,331.723813906127));
#61222=CARTESIAN_POINT('Ctrl Pts',(67.5058975672389,3.5771758027706,331.621883063829));
#61223=CARTESIAN_POINT('Ctrl Pts',(67.4981320561899,3.48176738644495,331.523616172215));
#61224=CARTESIAN_POINT('Ctrl Pts',(67.4903665451409,3.38231605010601,331.429408844506));
#61225=CARTESIAN_POINT('Ctrl Pts',(67.4826087336187,3.28296332005659,331.335294923635));
#61226=CARTESIAN_POINT('Ctrl Pts',(67.4748509220965,3.1795759292109,331.245232823629));
#61227=CARTESIAN_POINT('Ctrl Pts',(67.4670931105743,3.07252089609362,331.159583563522));
#61228=CARTESIAN_POINT('Ctrl Pts',(67.4593411370513,2.96554642528396,331.0739987572));
#61229=CARTESIAN_POINT('Ctrl Pts',(67.4515891635283,2.85491010986719,330.992820424088));
#61230=CARTESIAN_POINT('Ctrl Pts',(67.4438371900053,2.74101400751839,330.916371065696));
#61231=CARTESIAN_POINT('Ctrl Pts',(67.4360884994476,2.62716614023639,330.839954083652));
#61232=CARTESIAN_POINT('Ctrl Pts',(67.4283398088901,2.51006155565071,330.768262310439));
#61233=CARTESIAN_POINT('Ctrl Pts',(67.4205911183325,2.39013323583607,330.701576314804));
#61234=CARTESIAN_POINT('Ctrl Pts',(67.4128440399546,2.27022986810987,330.634904193748));
#61235=CARTESIAN_POINT('Ctrl Pts',(67.4050969615767,2.1475042751367,330.5732359685));
#61236=CARTESIAN_POINT('Ctrl Pts',(67.3973498831989,2.02241576376905,330.516807215727));
#61237=CARTESIAN_POINT('Ctrl Pts',(67.3896027398931,1.89732620403919,330.460377990027));
#61238=CARTESIAN_POINT('Ctrl Pts',(67.3818555965873,1.76987404271365,330.409188485118));
#61239=CARTESIAN_POINT('Ctrl Pts',(67.3741084532814,1.64054000663724,330.363426744985));
#61240=CARTESIAN_POINT('Ctrl Pts',(67.3663595682533,1.51117689352342,330.317654716641));
#61241=CARTESIAN_POINT('Ctrl Pts',(67.3586106832252,1.37993143218229,330.277313011643));
#61242=CARTESIAN_POINT('Ctrl Pts',(67.3508617981971,1.24730061731481,330.24254014914));
#61243=CARTESIAN_POINT('Ctrl Pts',(67.3431046884224,1.11452902673065,330.207730378361));
#61244=CARTESIAN_POINT('Ctrl Pts',(67.3353475786476,0.980369523993994,330.178501356793));
#61245=CARTESIAN_POINT('Ctrl Pts',(67.3275904688729,0.845330981477995,330.154940805908));
#61246=CARTESIAN_POINT('Ctrl Pts',(67.3198292139467,0.710220278682479,330.131367665018));
#61247=CARTESIAN_POINT('Ctrl Pts',(67.3120679590206,0.574229987462297,330.113469081445));
#61248=CARTESIAN_POINT('Ctrl Pts',(67.3043067040944,0.437874271345128,330.101280862818));
#61249=CARTESIAN_POINT('Ctrl Pts',(67.2965330336897,0.301300430520302,330.089073147013));
#61250=CARTESIAN_POINT('Ctrl Pts',(67.2887593632851,0.164360387315896,330.082594068517));
#61251=CARTESIAN_POINT('Ctrl Pts',(67.2809856928804,0.0275693736396244,
330.081827271014));
#61252=CARTESIAN_POINT('Ctrl Pts',(67.2735738887033,-0.102853985439723,
330.08109616812));
#61253=CARTESIAN_POINT('Ctrl Pts',(67.2661620845263,-0.233141589771978,
330.085557491137));
#61254=CARTESIAN_POINT('Ctrl Pts',(67.2587502803492,-0.362852927357058,
330.095153334139));
#61255=CARTESIAN_POINT('Ctrl Pts',(67.2509752015708,-0.498921803987518,
330.105219497991));
#61256=CARTESIAN_POINT('Ctrl Pts',(67.2432001227923,-0.634786499232371,
330.120968035364));
#61257=CARTESIAN_POINT('Ctrl Pts',(67.2354250440139,-0.769934161220083,
330.142389018264));
#61258=CARTESIAN_POINT('Ctrl Pts',(67.2276595329649,-0.90491551540598,330.16378364128));
#61259=CARTESIAN_POINT('Ctrl Pts',(67.2198940219159,-1.03918120960381,330.190836760412));
#61260=CARTESIAN_POINT('Ctrl Pts',(67.2121285108669,-1.17222098590981,330.223486520202));
#61261=CARTESIAN_POINT('Ctrl Pts',(67.2043706993447,-1.30512885289008,330.25610390766));
#61262=CARTESIAN_POINT('Ctrl Pts',(67.1966128878225,-1.43681284373003,330.294306800219));
#61263=CARTESIAN_POINT('Ctrl Pts',(67.1888550763003,-1.56677075503651,330.337981932289));
#61264=CARTESIAN_POINT('Ctrl Pts',(67.1811031027773,-1.69663086889336,330.381624197437));
#61265=CARTESIAN_POINT('Ctrl Pts',(67.1733511292543,-1.82476711965399,330.430730381335));
#61266=CARTESIAN_POINT('Ctrl Pts',(67.1655991557313,-1.95069073243961,330.485136909177));
#61267=CARTESIAN_POINT('Ctrl Pts',(67.1578504651737,-2.0765610165007,330.539520395823));
#61268=CARTESIAN_POINT('Ctrl Pts',(67.1501017746161,-2.2002201682515,330.599199607159));
#61269=CARTESIAN_POINT('Ctrl Pts',(67.1423530840585,-2.32119794000141,330.66396227117));
#61270=CARTESIAN_POINT('Ctrl Pts',(67.1346060056806,-2.44215054131556,330.728711460769));
#61271=CARTESIAN_POINT('Ctrl Pts',(67.1268589273028,-2.56042252791154,330.798541814932));
#61272=CARTESIAN_POINT('Ctrl Pts',(67.119111848925,-2.67556724105116,330.873194576781));
#61273=CARTESIAN_POINT('Ctrl Pts',(67.1113647056192,-2.79071291921383,330.947847964291));
#61274=CARTESIAN_POINT('Ctrl Pts',(67.1036175623134,-2.90273094366841,331.027323627463));
#61275=CARTESIAN_POINT('Ctrl Pts',(67.0958704190076,-3.01120303533603,331.111319074225));
#61276=CARTESIAN_POINT('Ctrl Pts',(67.0881215339795,-3.11969951383285,331.195333404948));
#61277=CARTESIAN_POINT('Ctrl Pts',(67.0803726489515,-3.22464816421217,331.283869302008));
#61278=CARTESIAN_POINT('Ctrl Pts',(67.0726237639234,-3.32566355041658,331.376583792616));
#61279=CARTESIAN_POINT('Ctrl Pts',(67.0648666541487,-3.42678615539579,331.469396691344));
#61280=CARTESIAN_POINT('Ctrl Pts',(67.057109544374,-3.52396686820781,331.566396778631));
#61281=CARTESIAN_POINT('Ctrl Pts',(67.0493524345993,-3.61685654195464,331.667203603966));
#61282=CARTESIAN_POINT('Ctrl Pts',(67.0415911796731,-3.70979585297302,331.768064297245));
#61283=CARTESIAN_POINT('Ctrl Pts',(67.033829924747,-3.79843930344952,331.872735483765));
#61284=CARTESIAN_POINT('Ctrl Pts',(67.0260686698208,-3.88247853859796,331.98080417001));
#61285=CARTESIAN_POINT('Ctrl Pts',(67.0182949994162,-3.96665220913432,332.089045730934));
#61286=CARTESIAN_POINT('Ctrl Pts',(67.0105213290115,-4.04620671946224,332.200695333609));
#61287=CARTESIAN_POINT('Ctrl Pts',(67.0027476586069,-4.12087700240813,332.31531085719));
#61288=CARTESIAN_POINT('Ctrl Pts',(66.9953358544297,-4.19207136571891,332.424591000574));
#61289=CARTESIAN_POINT('Ctrl Pts',(66.9879240502525,-4.25882584262179,332.536566904497));
#61290=CARTESIAN_POINT('Ctrl Pts',(66.9805122460754,-4.32095074112603,332.650836796801));
#61291=CARTESIAN_POINT('Ctrl Pts',(66.9723313631025,-4.38952197050791,332.776963795562));
#61292=CARTESIAN_POINT('Ctrl Pts',(66.9641504801296,-4.45265114831385,332.906249954941));
#61293=CARTESIAN_POINT('Ctrl Pts',(66.9559695971568,-4.51005161674404,333.03821064413));
#61294=CARTESIAN_POINT('Ctrl Pts',(66.9478028851898,-4.56735265551854,333.169942749717));
#61295=CARTESIAN_POINT('Ctrl Pts',(66.9396361732229,-4.61894462767693,333.304339851162));
#61296=CARTESIAN_POINT('Ctrl Pts',(66.9314694612559,-4.66458640569054,333.440892330098));
#61297=CARTESIAN_POINT('Ctrl Pts',(66.9233215262709,-4.71012324369306,333.577130846273));
#61298=CARTESIAN_POINT('Ctrl Pts',(66.915173591286,-4.74973706429885,333.715514544774));
#61299=CARTESIAN_POINT('Ctrl Pts',(66.9070256563011,-4.78323481655576,333.855514197472));
#61300=CARTESIAN_POINT('Ctrl Pts',(66.8988889033995,-4.81668659708359,333.995321717096));
#61301=CARTESIAN_POINT('Ctrl Pts',(66.8907521504979,-4.84403895453746,334.136740452318));
#61302=CARTESIAN_POINT('Ctrl Pts',(66.8826153975964,-4.8651481098123,334.279224770064));
#61303=CARTESIAN_POINT('Ctrl Pts',(66.8744933613299,-4.88621908576203,334.42145138185));
#61304=CARTESIAN_POINT('Ctrl Pts',(66.8663713250634,-4.90106932749512,334.564739406573));
#61305=CARTESIAN_POINT('Ctrl Pts',(66.8582492887969,-4.90960585533241,334.708532321199));
#61306=CARTESIAN_POINT('Ctrl Pts',(66.8527719847366,-4.91536268244443,334.805502771623));
#61307=CARTESIAN_POINT('Ctrl Pts',(66.8472946806764,-4.91824918003111,334.902702554081));
#61308=CARTESIAN_POINT('Ctrl Pts',(66.8418173766161,-4.91824999982527,334.999958542886));
#61309=CARTESIAN_POINT('',(65.0918173765437,-4.91824798275492,335.004454506388));
#61310=CARTESIAN_POINT('Ctrl Pts',(66.8418173765086,-4.91824999982529,334.999958544795));
#61311=CARTESIAN_POINT('Ctrl Pts',(66.8337075228607,-4.91825121358016,335.143958554091));
#61312=CARTESIAN_POINT('Ctrl Pts',(66.8255976692128,-4.91192391682476,335.287838366001));
#61313=CARTESIAN_POINT('Ctrl Pts',(66.8174878155649,-4.89932552419494,335.431036507122));
#61314=CARTESIAN_POINT('Ctrl Pts',(66.8093674890112,-4.88671086224822,335.574419571511));
#61315=CARTESIAN_POINT('Ctrl Pts',(66.8012471624575,-4.8678089743011,335.717118876131));
#61316=CARTESIAN_POINT('Ctrl Pts',(66.7931268359039,-4.84272869959005,335.858581274351));
#61317=CARTESIAN_POINT('Ctrl Pts',(66.7849875446338,-4.81758985084326,336.000374052668));
#61318=CARTESIAN_POINT('Ctrl Pts',(66.7768482533637,-4.78624382425322,336.140923818903));
#61319=CARTESIAN_POINT('Ctrl Pts',(66.7687089620936,-4.7488503026307,336.279688972252));
#61320=CARTESIAN_POINT('Ctrl Pts',(66.7605596816537,-4.71141088877714,336.418624428964));
#61321=CARTESIAN_POINT('Ctrl Pts',(66.7524104012138,-4.66790926918605,336.555770583816));
#61322=CARTESIAN_POINT('Ctrl Pts',(66.744261120774,-4.61855401257615,336.690604003135));
#61323=CARTESIAN_POINT('Ctrl Pts',(66.7360932410512,-4.56908611137316,336.825745155748));
#61324=CARTESIAN_POINT('Ctrl Pts',(66.7279253613285,-4.51373798764962,336.958562709231));
#61325=CARTESIAN_POINT('Ctrl Pts',(66.7197574816058,-4.45276583261537,337.08855440494));
#61326=CARTESIAN_POINT('Ctrl Pts',(66.7139297250043,-4.40926239095552,337.18130307271));
#61327=CARTESIAN_POINT('Ctrl Pts',(66.7081019684029,-4.36289685369238,337.272613669177));
#61328=CARTESIAN_POINT('Ctrl Pts',(66.7022742118015,-4.31377583689369,337.362312657447));
#61329=CARTESIAN_POINT('Ctrl Pts',(66.6944991330231,-4.24824122359254,337.481984213389));
#61330=CARTESIAN_POINT('Ctrl Pts',(66.6867240542447,-4.17761943773648,337.599115742901));
#61331=CARTESIAN_POINT('Ctrl Pts',(66.6789489754663,-4.10213198839238,337.713244591316));
#61332=CARTESIAN_POINT('Ctrl Pts',(66.6711834644173,-4.02673743116046,337.827232996918));
#61333=CARTESIAN_POINT('Ctrl Pts',(66.6634179533682,-3.94648933743772,337.938225750497));
#61334=CARTESIAN_POINT('Ctrl Pts',(66.6556524423192,-3.86165540296115,338.045784071677));
#61335=CARTESIAN_POINT('Ctrl Pts',(66.647894630797,-3.77690558157742,338.153235748468));
#61336=CARTESIAN_POINT('Ctrl Pts',(66.6401368192748,-3.68757920847924,338.257259464575));
#61337=CARTESIAN_POINT('Ctrl Pts',(66.6323790077526,-3.59398743294007,338.357445069449));
#61338=CARTESIAN_POINT('Ctrl Pts',(66.6246270342296,-3.5004660881799,338.457555281479));
#61339=CARTESIAN_POINT('Ctrl Pts',(66.6168750607065,-3.40268599578553,338.553832846817));
#61340=CARTESIAN_POINT('Ctrl Pts',(66.6091230871835,-3.3009985301378,338.64590067974));
#61341=CARTESIAN_POINT('Ctrl Pts',(66.6013743966259,-3.19935412919243,338.737929521881));
#61342=CARTESIAN_POINT('Ctrl Pts',(66.5936257060683,-3.09380593537663,338.82575191572));
#61343=CARTESIAN_POINT('Ctrl Pts',(66.5858770155107,-2.9847419686626,338.909027813025));
#61344=CARTESIAN_POINT('Ctrl Pts',(66.5781299371328,-2.87570069361768,338.992286384084));
#61345=CARTESIAN_POINT('Ctrl Pts',(66.570382858755,-2.7631454111238,339.071000103083));
#61346=CARTESIAN_POINT('Ctrl Pts',(66.5626357803772,-2.64749667611866,339.144869649632));
#61347=CARTESIAN_POINT('Ctrl Pts',(66.5548886370714,-2.53184697186582,339.218739815279));
#61348=CARTESIAN_POINT('Ctrl Pts',(66.5471414937655,-2.41310409280062,339.287765517091));
#61349=CARTESIAN_POINT('Ctrl Pts',(66.5393943504597,-2.29171664145694,339.351691383562));
#61350=CARTESIAN_POINT('Ctrl Pts',(66.5316454654316,-2.17030189963691,339.415631621925));
#61351=CARTESIAN_POINT('Ctrl Pts',(66.5238965804035,-2.04624174821828,339.474469561341));
#61352=CARTESIAN_POINT('Ctrl Pts',(66.5161476953754,-1.92000802614176,339.527996493158));
#61353=CARTESIAN_POINT('Ctrl Pts',(66.5083905856007,-1.79364031828855,339.581580239013));
#61354=CARTESIAN_POINT('Ctrl Pts',(66.500633475826,-1.66509479165551,339.629841563685));
#61355=CARTESIAN_POINT('Ctrl Pts',(66.4928763660512,-1.53486236071531,339.672620313717));
#61356=CARTESIAN_POINT('Ctrl Pts',(66.4851151111251,-1.40456033772804,339.715421923345));
#61357=CARTESIAN_POINT('Ctrl Pts',(66.4773538561989,-1.27256999020031,339.75273501434));
#61358=CARTESIAN_POINT('Ctrl Pts',(66.4695926012727,-1.13939495128114,339.784450042324));
#61359=CARTESIAN_POINT('Ctrl Pts',(66.461818930868,-1.00600687570125,339.816215804017));
#61360=CARTESIAN_POINT('Ctrl Pts',(66.4540452604634,-0.871430705618236,
339.842365533209));
#61361=CARTESIAN_POINT('Ctrl Pts',(66.4462715900587,-0.736178650228208,
339.862841150752));
#61362=CARTESIAN_POINT('Ctrl Pts',(66.4388597858816,-0.607222610555794,
339.882363623373));
#61363=CARTESIAN_POINT('Ctrl Pts',(66.4314479817045,-0.477652480456083,
339.896728324271));
#61364=CARTESIAN_POINT('Ctrl Pts',(66.4240361775274,-0.347912518367584,
339.905929060032));
#61365=CARTESIAN_POINT('Ctrl Pts',(66.4162610987489,-0.211813614262213,
339.91558075126));
#61366=CARTESIAN_POINT('Ctrl Pts',(66.4084860199704,-0.0750977115996171,
339.919579976508));
#61367=CARTESIAN_POINT('Ctrl Pts',(66.400710941192,0.061726262174502,339.91786263849));
#61368=CARTESIAN_POINT('Ctrl Pts',(66.392945430143,0.198381865338344,339.916147413766));
#61369=CARTESIAN_POINT('Ctrl Pts',(66.385179919094,0.335144887897763,339.908729627461));
#61370=CARTESIAN_POINT('Ctrl Pts',(66.3774144080449,0.471501484549826,339.895596941392));
#61371=CARTESIAN_POINT('Ctrl Pts',(66.3696565965227,0.607722883239224,339.88247727642));
#61372=CARTESIAN_POINT('Ctrl Pts',(66.3618987850005,0.743538271391627,339.863654025252));
#61373=CARTESIAN_POINT('Ctrl Pts',(66.3541409734783,0.878434363935561,339.839166883954));
#61374=CARTESIAN_POINT('Ctrl Pts',(66.3463889999553,1.01322894289169,339.814698170007));
#61375=CARTESIAN_POINT('Ctrl Pts',(66.3386370264323,1.14710522019096,339.784574119275));
#61376=CARTESIAN_POINT('Ctrl Pts',(66.3308850529093,1.27955594756414,339.748886147251));
#61377=CARTESIAN_POINT('Ctrl Pts',(66.3231363623517,1.41195058197591,339.713213289104));
#61378=CARTESIAN_POINT('Ctrl Pts',(66.3153876717941,1.54292049059182,339.671981297707));
#61379=CARTESIAN_POINT('Ctrl Pts',(66.3076389812364,1.6719697397272,339.625332447721));
#61380=CARTESIAN_POINT('Ctrl Pts',(66.2998919028586,1.80099213908838,339.578693303417));
#61381=CARTESIAN_POINT('Ctrl Pts',(66.2921448244808,1.928094306456,339.526639675049));
#61382=CARTESIAN_POINT('Ctrl Pts',(66.2843977461029,2.05279695052103,339.469363236797));
#61383=CARTESIAN_POINT('Ctrl Pts',(66.2766506027971,2.1775006397145,339.412086318513));
#61384=CARTESIAN_POINT('Ctrl Pts',(66.2689034594913,2.2998044102945,339.349586666183));
#61385=CARTESIAN_POINT('Ctrl Pts',(66.2611563161855,2.41925075034118,339.282103323073));
#61386=CARTESIAN_POINT('Ctrl Pts',(66.2534074311574,2.53872394446045,339.214604808275));
#61387=CARTESIAN_POINT('Ctrl Pts',(66.2456585461293,2.65533808946972,339.142120565378));
#61388=CARTESIAN_POINT('Ctrl Pts',(66.2379096611012,2.76866233868613,339.064934429587));
#61389=CARTESIAN_POINT('Ctrl Pts',(66.2301525513265,2.8821068714319,338.987666367633));
#61390=CARTESIAN_POINT('Ctrl Pts',(66.2223954415518,2.99225420936034,338.905686663903));
#61391=CARTESIAN_POINT('Ctrl Pts',(66.2146383317771,3.09870401402384,338.819321470624));
#61392=CARTESIAN_POINT('Ctrl Pts',(66.2068770768509,3.20521070205928,338.732910126548));
#61393=CARTESIAN_POINT('Ctrl Pts',(66.1991158219247,3.30801562696851,338.642108881984));
#61394=CARTESIAN_POINT('Ctrl Pts',(66.1913545669986,3.40675412575205,338.547281972042));
#61395=CARTESIAN_POINT('Ctrl Pts',(66.1835808965939,3.50565057395484,338.452303369948));
#61396=CARTESIAN_POINT('Ctrl Pts',(66.1758072261892,3.60046732672272,338.353286516405));
#61397=CARTESIAN_POINT('Ctrl Pts',(66.1680335557845,3.69087835827589,338.250630709095));
#61398=CARTESIAN_POINT('Ctrl Pts',(66.1606217516075,3.77708073455789,338.152753554314));
#61399=CARTESIAN_POINT('Ctrl Pts',(66.1532099474305,3.85927815012865,338.051568831559));
#61400=CARTESIAN_POINT('Ctrl Pts',(66.1457981432535,3.9372249830816,337.947446775617));
#61401=CARTESIAN_POINT('Ctrl Pts',(66.138023064475,4.01899222250997,337.83822138755));
#61402=CARTESIAN_POINT('Ctrl Pts',(66.1302479856966,4.09634007602878,337.725418278553));
#61403=CARTESIAN_POINT('Ctrl Pts',(66.1224729069182,4.16893923301867,337.609430729852));
#61404=CARTESIAN_POINT('Ctrl Pts',(66.1147073958692,4.2414490521239,337.493585911215));
#61405=CARTESIAN_POINT('Ctrl Pts',(66.1069418848202,4.30922159633566,337.374564778032));
#61406=CARTESIAN_POINT('Ctrl Pts',(66.0991763737712,4.37196841903521,337.252792756882));
#61407=CARTESIAN_POINT('Ctrl Pts',(66.091418562249,4.43465302807729,337.131141473046));
#61408=CARTESIAN_POINT('Ctrl Pts',(66.0836607507268,4.49232165420805,337.006745074369));
#61409=CARTESIAN_POINT('Ctrl Pts',(66.0759029392046,4.54472991069206,336.88005667504));
#61410=CARTESIAN_POINT('Ctrl Pts',(66.0681509656816,4.59709872830131,336.753463612747));
#61411=CARTESIAN_POINT('Ctrl Pts',(66.0603989921586,4.64421490683903,336.624582342672));
#61412=CARTESIAN_POINT('Ctrl Pts',(66.0526470186356,4.6858808183973,336.493888890874));
#61413=CARTESIAN_POINT('Ctrl Pts',(66.0448983280779,4.72752908441718,336.36325078783));
#61414=CARTESIAN_POINT('Ctrl Pts',(66.0371496375203,4.76373155580886,336.230802401118));
#61415=CARTESIAN_POINT('Ctrl Pts',(66.0294009469627,4.79433949619766,336.097037764938));
#61416=CARTESIAN_POINT('Ctrl Pts',(66.0216538685849,4.82494106834879,335.963300959607));
#61417=CARTESIAN_POINT('Ctrl Pts',(66.013906790207,4.84995033762177,335.828248830315));
#61418=CARTESIAN_POINT('Ctrl Pts',(66.0061597118292,4.86926911489622,335.692388149247));
#61419=CARTESIAN_POINT('Ctrl Pts',(65.9984125685234,4.88858805408062,335.556526329536));
#61420=CARTESIAN_POINT('Ctrl Pts',(65.9906654252176,4.90221635111459,335.419856331514));
#61421=CARTESIAN_POINT('Ctrl Pts',(65.9829182819119,4.91010743662831,335.282892246743));
#61422=CARTESIAN_POINT('Ctrl Pts',(65.9751693968838,4.91800029622556,335.145897369538));
#61423=CARTESIAN_POINT('Ctrl Pts',(65.9674205118557,4.92015335517299,335.00860866417));
#61424=CARTESIAN_POINT('Ctrl Pts',(65.9596716268276,4.91657214068717,334.871542038321));
#61425=CARTESIAN_POINT('Ctrl Pts',(65.9519145170529,4.91298712506329,334.734329928539));
#61426=CARTESIAN_POINT('Ctrl Pts',(65.9441574072782,4.90365568804226,334.597340760501));
#61427=CARTESIAN_POINT('Ctrl Pts',(65.9364002975035,4.88863545188595,334.461087687036));
#61428=CARTESIAN_POINT('Ctrl Pts',(65.9286390425773,4.87360718939566,334.324761804285));
#61429=CARTESIAN_POINT('Ctrl Pts',(65.9208777876511,4.85288412949549,334.189173186074));
#61430=CARTESIAN_POINT('Ctrl Pts',(65.9131165327249,4.82657522518768,334.054825593816));
#61431=CARTESIAN_POINT('Ctrl Pts',(65.9053428623202,4.80022423520704,333.920263089195));
#61432=CARTESIAN_POINT('Ctrl Pts',(65.8975691919156,4.76826963613787,333.786945957928));
#61433=CARTESIAN_POINT('Ctrl Pts',(65.8897955215109,4.73087077466268,333.655364444936));
#61434=CARTESIAN_POINT('Ctrl Pts',(65.8823837173338,4.6952128391867,333.52990808303));
#61435=CARTESIAN_POINT('Ctrl Pts',(65.8749719131567,4.65460618519243,333.406029663209));
#61436=CARTESIAN_POINT('Ctrl Pts',(65.8675601089796,4.60922923090351,333.284136089463));
#61437=CARTESIAN_POINT('Ctrl Pts',(65.8597850302011,4.56162821691407,333.156268148565));
#61438=CARTESIAN_POINT('Ctrl Pts',(65.8520099514227,4.50862703776745,333.030180453478));
#61439=CARTESIAN_POINT('Ctrl Pts',(65.8442348726443,4.45037820316542,332.906362755564));
#61440=CARTESIAN_POINT('Ctrl Pts',(65.8364693615953,4.39220104746271,332.78269742321));
#61441=CARTESIAN_POINT('Ctrl Pts',(65.8287038505462,4.32878924982514,332.661296880322));
#61442=CARTESIAN_POINT('Ctrl Pts',(65.8209383394972,4.26034446552274,332.542633910548));
#61443=CARTESIAN_POINT('Ctrl Pts',(65.813180527975,4.19196754442321,332.424088595454));
#61444=CARTESIAN_POINT('Ctrl Pts',(65.8054227164528,4.11856776151994,332.308275788246));
#61445=CARTESIAN_POINT('Ctrl Pts',(65.7976649049306,4.04039389851348,332.195646205031));
#61446=CARTESIAN_POINT('Ctrl Pts',(65.7899129314077,3.96227886381819,332.08310137915));
#61447=CARTESIAN_POINT('Ctrl Pts',(65.7821609578847,3.87939712198385,331.973735328995));
#61448=CARTESIAN_POINT('Ctrl Pts',(65.7744089843617,3.79204202567799,331.867971849106));
#61449=CARTESIAN_POINT('Ctrl Pts',(65.7666602938041,3.70472392430709,331.762253160113));
#61450=CARTESIAN_POINT('Ctrl Pts',(65.7589116032464,3.61293648482616,331.660134307638));
#61451=CARTESIAN_POINT('Ctrl Pts',(65.7511629126888,3.51701466134618,331.562007717522));
#61452=CARTESIAN_POINT('Ctrl Pts',(65.743415834311,3.42111279520265,331.463901543464));
#61453=CARTESIAN_POINT('Ctrl Pts',(65.7356687559332,3.32107852910539,331.369786258933));
#61454=CARTESIAN_POINT('Ctrl Pts',(65.7279216775553,3.21728488282916,331.280018676765));
#61455=CARTESIAN_POINT('Ctrl Pts',(65.7201745342495,3.11349036666256,331.190250342258));
#61456=CARTESIAN_POINT('Ctrl Pts',(65.7124273909438,3.00593670311625,331.104830038483));
#61457=CARTESIAN_POINT('Ctrl Pts',(65.704680247638,2.89503100139379,331.024075131058));
#61458=CARTESIAN_POINT('Ctrl Pts',(65.6969313626099,2.7841003657146,330.943302068216));
#61459=CARTESIAN_POINT('Ctrl Pts',(65.6891824775817,2.66981650818277,330.867196718914));
#61460=CARTESIAN_POINT('Ctrl Pts',(65.6814335925536,2.5526162576692,330.796033622449));
#61461=CARTESIAN_POINT('Ctrl Pts',(65.6736764827789,2.43529160959892,330.724794992737));
#61462=CARTESIAN_POINT('Ctrl Pts',(65.6659193730042,2.3150447196508,330.658509297944));
#61463=CARTESIAN_POINT('Ctrl Pts',(65.6581622632294,2.19233829169693,330.597405778719));
#61464=CARTESIAN_POINT('Ctrl Pts',(65.6504010083033,2.06956629335136,330.536269607727));
#61465=CARTESIAN_POINT('Ctrl Pts',(65.6426397533771,1.9443324948402,330.480321289516));
#61466=CARTESIAN_POINT('Ctrl Pts',(65.6348784984509,1.81711948060543,330.429741817391));
#61467=CARTESIAN_POINT('Ctrl Pts',(65.6271048280462,1.68970296700651,330.379081434594));
#61468=CARTESIAN_POINT('Ctrl Pts',(65.6193311576416,1.56030128001685,330.333807189209));
#61469=CARTESIAN_POINT('Ctrl Pts',(65.6115574872369,1.42941290868267,330.294050382867));
#61470=CARTESIAN_POINT('Ctrl Pts',(65.6041456830598,1.30461742252375,330.256144265426));
#61471=CARTESIAN_POINT('Ctrl Pts',(65.5967338788827,1.17847082598085,330.223253545967));
#61472=CARTESIAN_POINT('Ctrl Pts',(65.5893220747056,1.05141184563745,330.195448387898));
#61473=CARTESIAN_POINT('Ctrl Pts',(65.5815469959272,0.918125326178437,330.166280416204));
#61474=CARTESIAN_POINT('Ctrl Pts',(65.5737719171487,0.783413514173073,330.142616951757));
#61475=CARTESIAN_POINT('Ctrl Pts',(65.5659968383703,0.647770783741957,330.124594778459));
#61476=CARTESIAN_POINT('Ctrl Pts',(65.5582313273213,0.512294970326168,330.106594782593));
#61477=CARTESIAN_POINT('Ctrl Pts',(65.5504658162723,0.375890901574579,330.094222316339));
#61478=CARTESIAN_POINT('Ctrl Pts',(65.5427003052233,0.239065278581079,330.08756365384));
#61479=CARTESIAN_POINT('Ctrl Pts',(65.5349424937011,0.102375318590763,330.080911593424));
#61480=CARTESIAN_POINT('Ctrl Pts',(65.5271846821788,-0.0347349759557258,
330.079962081465));
#61481=CARTESIAN_POINT('Ctrl Pts',(65.5194268706566,-0.171751958216401,
330.084749820472));
#61482=CARTESIAN_POINT('Ctrl Pts',(65.5116748971336,-0.308665830852681,
330.089533956553));
#61483=CARTESIAN_POINT('Ctrl Pts',(65.5039229236106,-0.445486141910531,
330.100046736305));
#61484=CARTESIAN_POINT('Ctrl Pts',(65.4961709500876,-0.581697763560121,
330.116270812753));
#61485=CARTESIAN_POINT('Ctrl Pts',(65.4884222595299,-0.717851699506703,
330.132488018295));
#61486=CARTESIAN_POINT('Ctrl Pts',(65.4806735689723,-0.853397071428923,
330.1544116637));
#61487=CARTESIAN_POINT('Ctrl Pts',(65.4729248784147,-0.987822617173819,
330.181972443053));
#61488=CARTESIAN_POINT('Ctrl Pts',(65.4651778000368,-1.12222019456155,330.209527488156));
#61489=CARTESIAN_POINT('Ctrl Pts',(65.457430721659,-1.25549802653516,330.242717255861));
#61490=CARTESIAN_POINT('Ctrl Pts',(65.4496836432811,-1.38715419916627,330.281421157781));
#61491=CARTESIAN_POINT('Ctrl Pts',(65.4419364999753,-1.51881147520283,330.320125384077));
#61492=CARTESIAN_POINT('Ctrl Pts',(65.4341893566695,-1.64884668978292,330.364343726522));
#61493=CARTESIAN_POINT('Ctrl Pts',(65.4264422133637,-1.77677265323683,330.413905583047));
#61494=CARTESIAN_POINT('Ctrl Pts',(65.4186933283356,-1.90472737716292,330.463478582129));
#61495=CARTESIAN_POINT('Ctrl Pts',(65.4109444433075,-2.03057154194372,330.518397344636));
#61496=CARTESIAN_POINT('Ctrl Pts',(65.4031955582794,-2.15383788846126,330.578443100815));
#61497=CARTESIAN_POINT('Ctrl Pts',(65.3954384485047,-2.27723507115273,330.638552590181));
#61498=CARTESIAN_POINT('Ctrl Pts',(65.38768133873,-2.39804861796368,330.703799772368));
#61499=CARTESIAN_POINT('Ctrl Pts',(65.3799242289552,-2.51583535992565,330.773919605089));
#61500=CARTESIAN_POINT('Ctrl Pts',(65.3721629740291,-2.63368504335643,330.844076907607));
#61501=CARTESIAN_POINT('Ctrl Pts',(65.3644017191029,-2.74850437203266,330.919111835224));
#61502=CARTESIAN_POINT('Ctrl Pts',(65.3566404641767,-2.85987999069209,330.998716518248));
#61503=CARTESIAN_POINT('Ctrl Pts',(65.3488667937721,-2.97143377404422,331.078448542822));
#61504=CARTESIAN_POINT('Ctrl Pts',(65.3410931233674,-3.07953253076973,331.162764690062));
#61505=CARTESIAN_POINT('Ctrl Pts',(65.3333194529628,-3.18379608549871,331.251316824742));
#61506=CARTESIAN_POINT('Ctrl Pts',(65.3259076487857,-3.28320614666963,331.335746836247));
#61507=CARTESIAN_POINT('Ctrl Pts',(65.3184958446087,-3.37912981603328,331.42402714493));
#61508=CARTESIAN_POINT('Ctrl Pts',(65.3110840404317,-3.47127067155644,331.515826785693));
#61509=CARTESIAN_POINT('Ctrl Pts',(65.3034172238383,-3.56658174874906,331.610784908204));
#61510=CARTESIAN_POINT('Ctrl Pts',(65.295750407245,-3.65816456085217,331.709827552767));
#61511=CARTESIAN_POINT('Ctrl Pts',(65.2880835906516,-3.7456412172627,331.812625699099));
#61512=CARTESIAN_POINT('Ctrl Pts',(65.2804263833121,-3.83300823424355,331.915295002714));
#61513=CARTESIAN_POINT('Ctrl Pts',(65.2727691759726,-3.91627907234102,332.021710143298));
#61514=CARTESIAN_POINT('Ctrl Pts',(65.2651119686331,-3.99511118947942,332.131503940007));
#61515=CARTESIAN_POINT('Ctrl Pts',(65.2574635671177,-4.07385264931564,332.241171473337));
#61516=CARTESIAN_POINT('Ctrl Pts',(65.2498151656024,-4.14816531583106,332.354209603464));
#61517=CARTESIAN_POINT('Ctrl Pts',(65.242166764087,-4.2177460886557,332.47021720416));
#61518=CARTESIAN_POINT('Ctrl Pts',(65.2345232922065,-4.28728201448842,332.586150034316));
#61519=CARTESIAN_POINT('Ctrl Pts',(65.2268798203259,-4.35209190408787,332.705048185819));
#61520=CARTESIAN_POINT('Ctrl Pts',(65.2192363484454,-4.41191535082616,332.826480734007));
#61521=CARTESIAN_POINT('Ctrl Pts',(65.2115960398435,-4.47171403941285,332.947863026891));
#61522=CARTESIAN_POINT('Ctrl Pts',(65.2039557312417,-4.5265302118481,333.071777269771));
#61523=CARTESIAN_POINT('Ctrl Pts',(65.1963154226399,-4.57614917568522,333.197767555398));
#61524=CARTESIAN_POINT('Ctrl Pts',(65.1886765138843,-4.62575904840789,333.323734757268));
#61525=CARTESIAN_POINT('Ctrl Pts',(65.1810376051287,-4.67017346056786,333.451776870211));
#61526=CARTESIAN_POINT('Ctrl Pts',(65.1733986963731,-4.7092258960529,333.581418129805));
#61527=CARTESIAN_POINT('Ctrl Pts',(65.1657567665039,-4.7482937763937,333.711110661248));
#61528=CARTESIAN_POINT('Ctrl Pts',(65.1581148366347,-4.78199532455701,333.842403217695));
#61529=CARTESIAN_POINT('Ctrl Pts',(65.1504729067655,-4.81021396004182,333.974805032631));
#61530=CARTESIAN_POINT('Ctrl Pts',(65.1428293646065,-4.83843854907786,334.107234781624));
#61531=CARTESIAN_POINT('Ctrl Pts',(65.1351858224473,-4.8611778491727,334.240773858928));
#61532=CARTESIAN_POINT('Ctrl Pts',(65.1275422802883,-4.87836666943963,334.374922643987));
#61533=CARTESIAN_POINT('Ctrl Pts',(65.1198917627945,-4.89557117585986,334.509193850386));
#61534=CARTESIAN_POINT('Ctrl Pts',(65.1122412453008,-4.90721504923341,334.64407547474));
#61535=CARTESIAN_POINT('Ctrl Pts',(65.104590727807,-4.91328508657738,334.779063989996));
#61536=CARTESIAN_POINT('Ctrl Pts',(65.1003329440526,-4.91666327719168,334.854189876286));
#61537=CARTESIAN_POINT('Ctrl Pts',(65.0960751602982,-4.9183160066904,334.929348859592));
#61538=CARTESIAN_POINT('Ctrl Pts',(65.0918173765437,-4.91824798275492,335.004454506388));
#61539=CARTESIAN_POINT('',(63.341817376473,-4.91824948425114,334.997747631595));
#61540=CARTESIAN_POINT('Ctrl Pts',(65.0918173765086,-4.91824798275436,335.004454507007));
#61541=CARTESIAN_POINT('Ctrl Pts',(65.0809789349072,-4.91807482375963,335.195640394707));
#61542=CARTESIAN_POINT('Ctrl Pts',(65.0701404933059,-4.90675037086299,335.386341402681));
#61543=CARTESIAN_POINT('Ctrl Pts',(65.0593020517045,-4.88446398368072,335.575495138664));
#61544=CARTESIAN_POINT('Ctrl Pts',(65.0504833698556,-4.86633069797861,335.72939979392));
#61545=CARTESIAN_POINT('Ctrl Pts',(65.0416646880067,-4.84094124615037,335.882281032344));
#61546=CARTESIAN_POINT('Ctrl Pts',(65.0328460061578,-4.80841932933467,336.033579515945));
#61547=CARTESIAN_POINT('Ctrl Pts',(65.0250709273793,-4.77974605711561,336.166973332527));
#61548=CARTESIAN_POINT('Ctrl Pts',(65.0172958486009,-4.74547240905112,336.299383864177));
#61549=CARTESIAN_POINT('Ctrl Pts',(65.0095207698225,-4.70567871032785,336.430304491242));
#61550=CARTESIAN_POINT('Ctrl Pts',(65.0017552587735,-4.66593398028416,336.561064012141));
#61551=CARTESIAN_POINT('Ctrl Pts',(64.9939897477244,-4.62068282783947,336.690336906035));
#61552=CARTESIAN_POINT('Ctrl Pts',(64.9862242366754,-4.57005665624649,336.817626260043));
#61553=CARTESIAN_POINT('Ctrl Pts',(64.9784664251532,-4.51948068065022,336.944789406285));
#61554=CARTESIAN_POINT('Ctrl Pts',(64.970708613631,-4.46354043513179,337.069972565595));
#61555=CARTESIAN_POINT('Ctrl Pts',(64.9629508021088,-4.40241713803768,337.19269386947));
#61556=CARTESIAN_POINT('Ctrl Pts',(64.9551988285858,-4.34133983816296,337.315322821673));
#61557=CARTESIAN_POINT('Ctrl Pts',(64.9474468550628,-4.27508742385039,337.435493257528));
#61558=CARTESIAN_POINT('Ctrl Pts',(64.9396948815398,-4.20388909941276,337.55274352459));
#61559=CARTESIAN_POINT('Ctrl Pts',(64.9319461909822,-4.13272092750776,337.669944136095));
#61560=CARTESIAN_POINT('Ctrl Pts',(64.9241975004246,-4.05661121393649,337.784226705096));
#61561=CARTESIAN_POINT('Ctrl Pts',(64.916448809867,-3.97583485146533,337.895154623915));
#61562=CARTESIAN_POINT('Ctrl Pts',(64.9087017314891,-3.89507529519104,338.006059463253));
#61563=CARTESIAN_POINT('Ctrl Pts',(64.9009546531113,-3.80965125122163,338.113610724927));
#61564=CARTESIAN_POINT('Ctrl Pts',(64.8932075747335,-3.71988041368792,338.21740155566));
#61565=CARTESIAN_POINT('Ctrl Pts',(64.8854604314277,-3.63010882378819,338.321193256259));
#61566=CARTESIAN_POINT('Ctrl Pts',(64.8777132881219,-3.53599062336178,338.421224167421));
#61567=CARTESIAN_POINT('Ctrl Pts',(64.869966144816,-3.4378829258465,338.517121557563));
#61568=CARTESIAN_POINT('Ctrl Pts',(64.862217259788,-3.33975317163807,338.613040507474));
#61569=CARTESIAN_POINT('Ctrl Pts',(64.8544683747599,-3.23763241502894,338.704823813985));
#61570=CARTESIAN_POINT('Ctrl Pts',(64.8467194897318,-3.13191335169259,338.792136840884));
#61571=CARTESIAN_POINT('Ctrl Pts',(64.8389623799571,-3.02608207704992,338.879542542732));
#61572=CARTESIAN_POINT('Ctrl Pts',(64.8312052701824,-2.91664516816334,338.962468237482));
#61573=CARTESIAN_POINT('Ctrl Pts',(64.8234481604076,-2.80402745477987,339.040620384958));
#61574=CARTESIAN_POINT('Ctrl Pts',(64.8156869054815,-2.69134956209119,339.118814294444));
#61575=CARTESIAN_POINT('Ctrl Pts',(64.8079256505552,-2.57548780806422,339.19222936479));
#61576=CARTESIAN_POINT('Ctrl Pts',(64.8001643956291,-2.45689364970565,339.260616933794));
#61577=CARTESIAN_POINT('Ctrl Pts',(64.7923907252244,-2.33810977934354,339.329113900622));
#61578=CARTESIAN_POINT('Ctrl Pts',(64.7846170548198,-2.21658511685253,339.392567114074));
#61579=CARTESIAN_POINT('Ctrl Pts',(64.7768433844151,-2.09279402023467,339.450774792255));
#61580=CARTESIAN_POINT('Ctrl Pts',(64.769431580238,-1.97476542894603,339.506272889012));
#61581=CARTESIAN_POINT('Ctrl Pts',(64.7620197760609,-1.85467692512314,339.557002707616));
#61582=CARTESIAN_POINT('Ctrl Pts',(64.7546079718837,-1.73295254073325,339.602831580024));
#61583=CARTESIAN_POINT('Ctrl Pts',(64.7468328931053,-1.605262081667,339.650906661986));
#61584=CARTESIAN_POINT('Ctrl Pts',(64.7390578143269,-1.47536780315882,339.693740156522));
#61585=CARTESIAN_POINT('Ctrl Pts',(64.7312827355484,-1.3437392010497,339.731125449833));
#61586=CARTESIAN_POINT('Ctrl Pts',(64.7235172244994,-1.21227257631528,339.768464738161));
#61587=CARTESIAN_POINT('Ctrl Pts',(64.7157517134504,-1.0790762468255,339.800369059242));
#61588=CARTESIAN_POINT('Ctrl Pts',(64.7079862024014,-0.944639187063109,
339.826680004803));
#61589=CARTESIAN_POINT('Ctrl Pts',(64.7002283908792,-0.810335422036691,
339.852964862984));
#61590=CARTESIAN_POINT('Ctrl Pts',(64.692470579357,-0.674793756006488,339.873667307606));
#61591=CARTESIAN_POINT('Ctrl Pts',(64.6847127678348,-0.538517470121591,
339.888678962345));
#61592=CARTESIAN_POINT('Ctrl Pts',(64.6769607943118,-0.402343736463855,
339.903679320338));
#61593=CARTESIAN_POINT('Ctrl Pts',(64.6692088207887,-0.265436870281805,
339.912997369928));
#61594=CARTESIAN_POINT('Ctrl Pts',(64.6614568472657,-0.128309120572251,
339.916576027285));
#61595=CARTESIAN_POINT('Ctrl Pts',(64.6537081567081,0.00876055545407584,
339.920153169079));
#61596=CARTESIAN_POINT('Ctrl Pts',(64.6459594661505,0.146050539026823,339.917995742826));
#61597=CARTESIAN_POINT('Ctrl Pts',(64.6382107755929,0.283044917184179,339.910098638251));
#61598=CARTESIAN_POINT('Ctrl Pts',(64.6304636972151,0.42001079251696,339.902203176735));
#61599=CARTESIAN_POINT('Ctrl Pts',(64.6227166188372,0.556680794787046,339.888570434701));
#61600=CARTESIAN_POINT('Ctrl Pts',(64.6149695404594,0.692540869869353,339.869247396268));
#61601=CARTESIAN_POINT('Ctrl Pts',(64.6072223971536,0.828402083589853,339.849924195889));
#61602=CARTESIAN_POINT('Ctrl Pts',(64.5994752538478,0.963452969603614,339.824910659029));
#61603=CARTESIAN_POINT('Ctrl Pts',(64.591728110542,1.097186835399,339.794305383549));
#61604=CARTESIAN_POINT('Ctrl Pts',(64.5839792255139,1.23095076740658,339.763693227354));
#61605=CARTESIAN_POINT('Ctrl Pts',(64.5762303404858,1.36339670905216,339.727486918148));
#61606=CARTESIAN_POINT('Ctrl Pts',(64.5684814554577,1.49403074744294,339.685835591247));
#61607=CARTESIAN_POINT('Ctrl Pts',(64.5607243456829,1.62480344215194,339.644140055196));
#61608=CARTESIAN_POINT('Ctrl Pts',(64.5529672359082,1.75376001889645,339.596988075484));
#61609=CARTESIAN_POINT('Ctrl Pts',(64.5452101261335,1.88042373372718,339.544578049075));
#61610=CARTESIAN_POINT('Ctrl Pts',(64.5374488712073,2.00715513359711,339.492140016424));
#61611=CARTESIAN_POINT('Ctrl Pts',(64.5296876162812,2.13159087574279,339.43443850278));
#61612=CARTESIAN_POINT('Ctrl Pts',(64.521926361355,2.2532775455229,339.371718582588));
#61613=CARTESIAN_POINT('Ctrl Pts',(64.5141526909504,2.37515887431708,339.308898330963));
#61614=CARTESIAN_POINT('Ctrl Pts',(64.5063790205457,2.49428200318152,339.241043824403));
#61615=CARTESIAN_POINT('Ctrl Pts',(64.498605350141,2.61022054708114,339.168444764909));
#61616=CARTESIAN_POINT('Ctrl Pts',(64.491193545964,2.72076212386839,339.099225209101));
#61617=CARTESIAN_POINT('Ctrl Pts',(64.4837817417869,2.82840869069962,339.025693039984));
#61618=CARTESIAN_POINT('Ctrl Pts',(64.4763699376099,2.93281921615969,338.948133040796));
#61619=CARTESIAN_POINT('Ctrl Pts',(64.4685948588315,3.04234721249602,338.866771595008));
#61620=CARTESIAN_POINT('Ctrl Pts',(64.460819780053,3.14866005929728,338.780720386717));
#61621=CARTESIAN_POINT('Ctrl Pts',(64.4530447012746,3.25132993947161,338.690262414408));
#61622=CARTESIAN_POINT('Ctrl Pts',(64.4452791902256,3.35387347782218,338.599915756394));
#61623=CARTESIAN_POINT('Ctrl Pts',(64.4375136791766,3.45278267875889,338.505173380113));
#61624=CARTESIAN_POINT('Ctrl Pts',(64.4297481681276,3.54765972123455,338.406360750835));
#61625=CARTESIAN_POINT('Ctrl Pts',(64.4219903566054,3.6424426928463,338.307646094566));
#61626=CARTESIAN_POINT('Ctrl Pts',(64.4142325450832,3.73320119306368,338.204869496638));
#61627=CARTESIAN_POINT('Ctrl Pts',(64.406474733561,3.81957173161708,338.098395528258));
#61628=CARTESIAN_POINT('Ctrl Pts',(64.398722760038,3.90587727360119,337.992001684917));
#61629=CARTESIAN_POINT('Ctrl Pts',(64.3909707865151,3.98780118129954,337.881916311667));
#61630=CARTESIAN_POINT('Ctrl Pts',(64.3832188129921,4.06501824437489,337.768539278284));
#61631=CARTESIAN_POINT('Ctrl Pts',(64.3754701224344,4.14220260597819,337.655210260141));
#61632=CARTESIAN_POINT('Ctrl Pts',(64.3677214318768,4.21468386802446,337.538592676863));
#61633=CARTESIAN_POINT('Ctrl Pts',(64.3599727413192,4.28217854306664,337.419117605202));
#61634=CARTESIAN_POINT('Ctrl Pts',(64.3522256629414,4.34965917527796,337.299667391328));
#61635=CARTESIAN_POINT('Ctrl Pts',(64.3444785845635,4.41215509201134,337.177361211732));
#61636=CARTESIAN_POINT('Ctrl Pts',(64.3367315061857,4.46942761903059,337.052656771296));
#61637=CARTESIAN_POINT('Ctrl Pts',(64.3289843628799,4.52670062604878,336.927951285717));
#61638=CARTESIAN_POINT('Ctrl Pts',(64.3212372195741,4.57874999290288,336.800847854412));
#61639=CARTESIAN_POINT('Ctrl Pts',(64.3134900762683,4.62538443224659,336.671825922885));
#61640=CARTESIAN_POINT('Ctrl Pts',(64.3057411912402,4.67202935600233,336.542774984489));
#61641=CARTESIAN_POINT('Ctrl Pts',(64.2979923062121,4.71325679693508,336.411805055121));
#61642=CARTESIAN_POINT('Ctrl Pts',(64.290243421184,4.74892488150428,336.279412182344));
#61643=CARTESIAN_POINT('Ctrl Pts',(64.2824863114093,4.78463082454697,336.146878786404));
#61644=CARTESIAN_POINT('Ctrl Pts',(64.2747292016346,4.81476552206692,336.012919808049));
#61645=CARTESIAN_POINT('Ctrl Pts',(64.2669720918599,4.83923781679814,335.87804351542));
#61646=CARTESIAN_POINT('Ctrl Pts',(64.2592108369337,4.86372318874118,335.743095149212));
#61647=CARTESIAN_POINT('Ctrl Pts',(64.2514495820075,4.88254007510712,335.607228878977));
#61648=CARTESIAN_POINT('Ctrl Pts',(64.2436883270814,4.89564919554401,335.470958614604));
#61649=CARTESIAN_POINT('Ctrl Pts',(64.2359146566767,4.90877928630135,335.334470362217));
#61650=CARTESIAN_POINT('Ctrl Pts',(64.2281409862721,4.9161833444349,335.197577214784));
#61651=CARTESIAN_POINT('Ctrl Pts',(64.2203673158674,4.91787424512977,335.060794502953));
#61652=CARTESIAN_POINT('Ctrl Pts',(64.2129555116903,4.91948643399049,334.930379059265));
#61653=CARTESIAN_POINT('Ctrl Pts',(64.2055437075131,4.9159053983112,334.800064288692));
#61654=CARTESIAN_POINT('Ctrl Pts',(64.198131903336,4.90718606672495,334.670291084378));
#61655=CARTESIAN_POINT('Ctrl Pts',(64.1903568245576,4.89803937472416,334.534157308747));
#61656=CARTESIAN_POINT('Ctrl Pts',(64.1825817457791,4.88320905948407,334.398189321363));
#61657=CARTESIAN_POINT('Ctrl Pts',(64.1748066670007,4.86270158409264,334.262900029465));
#61658=CARTESIAN_POINT('Ctrl Pts',(64.1670411559517,4.84221934445524,334.127777219654));
#61659=CARTESIAN_POINT('Ctrl Pts',(64.1592756449027,4.81607390303674,333.993331826329));
#61660=CARTESIAN_POINT('Ctrl Pts',(64.1515101338537,4.78432366672865,333.860074513628));
#61661=CARTESIAN_POINT('Ctrl Pts',(64.1437523223315,4.75260491087231,333.726949325941));
#61662=CARTESIAN_POINT('Ctrl Pts',(64.1359945108093,4.71529250922094,333.595010252401));
#61663=CARTESIAN_POINT('Ctrl Pts',(64.1282366992871,4.67249633203974,333.464760250132));
#61664=CARTESIAN_POINT('Ctrl Pts',(64.1204847257641,4.62973236033901,333.33460826512));
#61665=CARTESIAN_POINT('Ctrl Pts',(64.1127327522411,4.58149294865365,333.206143191203));
#61666=CARTESIAN_POINT('Ctrl Pts',(64.104980778718,4.52793836603238,333.079854897173));
#61667=CARTESIAN_POINT('Ctrl Pts',(64.0972320881604,4.47440646380866,332.953620086309));
#61668=CARTESIAN_POINT('Ctrl Pts',(64.0894833976028,4.41556401997028,332.829560580907));
#61669=CARTESIAN_POINT('Ctrl Pts',(64.0817347070451,4.35162012483087,332.708148051975));
#61670=CARTESIAN_POINT('Ctrl Pts',(64.0739876286673,4.2876895337529,332.586760783933));
#61671=CARTESIAN_POINT('Ctrl Pts',(64.0662405502894,4.21865978460155,332.468019742553));
#61672=CARTESIAN_POINT('Ctrl Pts',(64.0584934719116,4.14478661085327,332.352373324467));
#61673=CARTESIAN_POINT('Ctrl Pts',(64.0507463286058,4.07091281797669,332.236725937154));
#61674=CARTESIAN_POINT('Ctrl Pts',(64.0429991853,3.99219572995644,332.124173554269));
#61675=CARTESIAN_POINT('Ctrl Pts',(64.0352520419942,3.90893500618586,332.015136488897));
#61676=CARTESIAN_POINT('Ctrl Pts',(64.0275031569661,3.82565556363695,331.906074909678));
#61677=CARTESIAN_POINT('Ctrl Pts',(64.019754271938,3.73783068982879,331.800530531214));
#61678=CARTESIAN_POINT('Ctrl Pts',(64.0120053869099,3.64580074582721,331.698891097794));
#61679=CARTESIAN_POINT('Ctrl Pts',(64.0042482771352,3.55367312029216,331.597143783228));
#61680=CARTESIAN_POINT('Ctrl Pts',(63.9964911673604,3.45733177146089,331.499309983436));
#61681=CARTESIAN_POINT('Ctrl Pts',(63.9887340575857,3.35715478242821,331.405741407561));
#61682=CARTESIAN_POINT('Ctrl Pts',(63.9809728026595,3.25692426201564,331.312122831631));
#61683=CARTESIAN_POINT('Ctrl Pts',(63.9732115477333,3.15285431372051,331.222774275616));
#61684=CARTESIAN_POINT('Ctrl Pts',(63.9654502928072,3.04535583847942,331.138006877331));
#61685=CARTESIAN_POINT('Ctrl Pts',(63.9576766224025,2.93768540071161,331.053103878835));
#61686=CARTESIAN_POINT('Ctrl Pts',(63.9499029519979,2.82657579324869,330.972796911389));
#61687=CARTESIAN_POINT('Ctrl Pts',(63.9421292815932,2.71246733612865,330.897354022958));
#61688=CARTESIAN_POINT('Ctrl Pts',(63.9347174774161,2.60367065514083,330.825423019136));
#61689=CARTESIAN_POINT('Ctrl Pts',(63.9273056732391,2.49214828053765,330.75791358862));
#61690=CARTESIAN_POINT('Ctrl Pts',(63.919893869062,2.3783006938045,330.695018133331));
#61691=CARTESIAN_POINT('Ctrl Pts',(63.9121187902836,2.25887309771076,330.629039984422));
#61692=CARTESIAN_POINT('Ctrl Pts',(63.9043437115051,2.13650918183008,330.567931033083));
#61693=CARTESIAN_POINT('Ctrl Pts',(63.8965686327267,2.01164375834977,330.511963407904));
#61694=CARTESIAN_POINT('Ctrl Pts',(63.8888031216777,1.88693198972237,330.45606465445));
#61695=CARTESIAN_POINT('Ctrl Pts',(63.8810376106287,1.75972519163242,330.405294797125));
#61696=CARTESIAN_POINT('Ctrl Pts',(63.8732720995797,1.6304843997679,330.359881069993));
#61697=CARTESIAN_POINT('Ctrl Pts',(63.8655142880575,1.5013717505247,330.314512370703));
#61698=CARTESIAN_POINT('Ctrl Pts',(63.8577564765353,1.37022948726986,330.274489361922));
#61699=CARTESIAN_POINT('Ctrl Pts',(63.8499986650131,1.23754001448266,330.239991830358));
#61700=CARTESIAN_POINT('Ctrl Pts',(63.8422466914901,1.10495039473156,330.205520259281));
#61701=CARTESIAN_POINT('Ctrl Pts',(63.834494717967,0.970816259753514,330.17656598689));
#61702=CARTESIAN_POINT('Ctrl Pts',(63.826742744444,0.835636281442749,330.153259335632));
#61703=CARTESIAN_POINT('Ctrl Pts',(63.8189940538864,0.700513551933149,330.129962554755));
#61704=CARTESIAN_POINT('Ctrl Pts',(63.8112453633288,0.564346244407593,330.112308704221));
#61705=CARTESIAN_POINT('Ctrl Pts',(63.8034966727712,0.427644147845715,330.100377203772));
#61706=CARTESIAN_POINT('Ctrl Pts',(63.7957495943933,0.290970493296784,330.088448185772));
#61707=CARTESIAN_POINT('Ctrl Pts',(63.7880025160155,0.153762660179541,330.082239183668));
#61708=CARTESIAN_POINT('Ctrl Pts',(63.7802554376377,0.0165361068463397,
330.081777798872));
#61709=CARTESIAN_POINT('Ctrl Pts',(63.7725082943319,-0.120691596577458,
330.081316410209));
#61710=CARTESIAN_POINT('Ctrl Pts',(63.7647611510261,-0.257937629658066,
330.086602736247));
#61711=CARTESIAN_POINT('Ctrl Pts',(63.7570140077203,-0.394686379264815,
330.097612242537));
#61712=CARTESIAN_POINT('Ctrl Pts',(63.7492651226922,-0.531465872893734,
330.108624223998));
#61713=CARTESIAN_POINT('Ctrl Pts',(63.7415162376641,-0.667747471042004,
330.125361914723));
#61714=CARTESIAN_POINT('Ctrl Pts',(63.733767352636,-0.803020922363803,330.147748928513));
#61715=CARTESIAN_POINT('Ctrl Pts',(63.7260102428612,-0.938437954324471,
330.170159704111));
#61716=CARTESIAN_POINT('Ctrl Pts',(63.7182531330866,-1.07284431568034,330.198231716926));
#61717=CARTESIAN_POINT('Ctrl Pts',(63.7104960233118,-1.20573964425143,330.231837358816));
#61718=CARTESIAN_POINT('Ctrl Pts',(63.7027347683857,-1.33870598783684,330.265460958487));
#61719=CARTESIAN_POINT('Ctrl Pts',(63.6949735134595,-1.4701593153123,330.304623967764));
#61720=CARTESIAN_POINT('Ctrl Pts',(63.6872122585333,-1.59961562217729,330.34914922581));
#61721=CARTESIAN_POINT('Ctrl Pts',(63.6794385881287,-1.72927901694363,330.393745709757));
#61722=CARTESIAN_POINT('Ctrl Pts',(63.671664917724,-1.85693864320926,330.443721440994));
#61723=CARTESIAN_POINT('Ctrl Pts',(63.6638912473194,-1.98213081128307,330.498851201142));
#61724=CARTESIAN_POINT('Ctrl Pts',(63.6564794431423,-2.10149525381397,330.551414657691));
#61725=CARTESIAN_POINT('Ctrl Pts',(63.6490676389651,-2.21861653023601,330.608662975179));
#61726=CARTESIAN_POINT('Ctrl Pts',(63.641655834788,-2.33311612215949,330.670363499898));
#61727=CARTESIAN_POINT('Ctrl Pts',(63.6338807560096,-2.45322768015955,330.735088151129));
#61728=CARTESIAN_POINT('Ctrl Pts',(63.6261056772312,-2.57083363716574,330.804917018512));
#61729=CARTESIAN_POINT('Ctrl Pts',(63.6183305984527,-2.68546985261784,330.879631723598));
#61730=CARTESIAN_POINT('Ctrl Pts',(63.6105650874037,-2.79996500090858,330.954254487482));
#61731=CARTESIAN_POINT('Ctrl Pts',(63.6027995763547,-2.9114973546321,331.033750914861));
#61732=CARTESIAN_POINT('Ctrl Pts',(63.5950340653057,-3.01962633494997,331.117856280381));
#61733=CARTESIAN_POINT('Ctrl Pts',(63.5872762537835,-3.12764810506897,331.201878255186));
#61734=CARTESIAN_POINT('Ctrl Pts',(63.5795184422613,-3.23227291059481,331.290499835583));
#61735=CARTESIAN_POINT('Ctrl Pts',(63.5717606307391,-3.33308850830447,331.383412650259));
#61736=CARTESIAN_POINT('Ctrl Pts',(63.5640086572161,-3.43382823907994,331.476255545095));
#61737=CARTESIAN_POINT('Ctrl Pts',(63.5562566836931,-3.53076418149791,331.573382982637));
#61738=CARTESIAN_POINT('Ctrl Pts',(63.5485047101701,-3.6235168846556,331.674446144006));
#61739=CARTESIAN_POINT('Ctrl Pts',(63.5407560196125,-3.71623030698837,331.775466505066));
#61740=CARTESIAN_POINT('Ctrl Pts',(63.5330073290549,-3.80476374991112,331.880418987465));
#61741=CARTESIAN_POINT('Ctrl Pts',(63.5252586384972,-3.88877455160031,331.988917877353));
#61742=CARTESIAN_POINT('Ctrl Pts',(63.5175115601194,-3.97276787414055,332.09739419314));
#61743=CARTESIAN_POINT('Ctrl Pts',(63.5097644817416,-4.05224018795635,332.209415139899));
#61744=CARTESIAN_POINT('Ctrl Pts',(63.5020174033638,-4.12688933834126,332.324562194409));
#61745=CARTESIAN_POINT('Ctrl Pts',(63.494270260058,-4.20153911435796,332.439710213963));
#61746=CARTESIAN_POINT('Ctrl Pts',(63.4865231167522,-4.27136543368911,332.557984065545));
#61747=CARTESIAN_POINT('Ctrl Pts',(63.4787759734464,-4.33610990002626,332.678936882074));
#61748=CARTESIAN_POINT('Ctrl Pts',(63.4710270884183,-4.40086892229406,332.799916891365));
#61749=CARTESIAN_POINT('Ctrl Pts',(63.4632782033902,-4.46054363367496,332.923576719549));
#61750=CARTESIAN_POINT('Ctrl Pts',(63.4555293183621,-4.51492214267191,333.049445948426));
#61751=CARTESIAN_POINT('Ctrl Pts',(63.4477722085874,-4.56935836958011,333.175448776204));
#61752=CARTESIAN_POINT('Ctrl Pts',(63.4400150988127,-4.61848700947907,333.303665329808));
#61753=CARTESIAN_POINT('Ctrl Pts',(63.432257989038,-4.66214459609082,333.433605787919));
#61754=CARTESIAN_POINT('Ctrl Pts',(63.4244967341118,-4.70582551192089,333.563615682056));
#61755=CARTESIAN_POINT('Ctrl Pts',(63.4167354791856,-4.74402944020056,333.695350941057));
#61756=CARTESIAN_POINT('Ctrl Pts',(63.4089742242594,-4.77664343665158,333.828308683316));
#61757=CARTESIAN_POINT('Ctrl Pts',(63.4012005538548,-4.80930960486808,333.961479114632));
#61758=CARTESIAN_POINT('Ctrl Pts',(63.3934268834501,-4.83636789516558,334.095875553636));
#61759=CARTESIAN_POINT('Ctrl Pts',(63.3856532130455,-4.85775676938531,334.230986195188));
#61760=CARTESIAN_POINT('Ctrl Pts',(63.3782414088684,-4.87814998636424,334.35980740387));
#61761=CARTESIAN_POINT('Ctrl Pts',(63.3708296046913,-4.89338969793911,334.489277533386));
#61762=CARTESIAN_POINT('Ctrl Pts',(63.3634178005142,-4.90346670955524,334.618952377276));
#61763=CARTESIAN_POINT('Ctrl Pts',(63.356217659179,-4.91325594658029,334.744924027542));
#61764=CARTESIAN_POINT('Ctrl Pts',(63.3490175178438,-4.91819156589539,334.871277715051));
#61765=CARTESIAN_POINT('Ctrl Pts',(63.3418173765086,-4.91824948425085,334.99774763097));
#61766=CARTESIAN_POINT('',(61.5918173765632,-4.91824892677099,334.996750874583));
#61767=CARTESIAN_POINT('Ctrl Pts',(63.341817376473,-4.91824948425114,334.997747631595));
#61768=CARTESIAN_POINT('Ctrl Pts',(63.3341280999864,-4.91831133722102,335.132809167956));
#61769=CARTESIAN_POINT('Ctrl Pts',(63.3264388234998,-4.91280554215197,335.268097297782));
#61770=CARTESIAN_POINT('Ctrl Pts',(63.3187495470132,-4.90170239144568,335.403108829221));
#61771=CARTESIAN_POINT('Ctrl Pts',(63.3110692067358,-4.89061214443433,335.537963454961));
#61772=CARTESIAN_POINT('Ctrl Pts',(63.3033888664584,-4.87393751253565,335.672541726678));
#61773=CARTESIAN_POINT('Ctrl Pts',(63.2957085261811,-4.85170077901492,335.806339018903));
#61774=CARTESIAN_POINT('Ctrl Pts',(63.2880351786687,-4.8294842915049,335.940014491915));
#61775=CARTESIAN_POINT('Ctrl Pts',(63.2803618311564,-4.80171584198153,336.072910007686));
#61776=CARTESIAN_POINT('Ctrl Pts',(63.272688483644,-4.76846959825874,336.204525115131));
#61777=CARTESIAN_POINT('Ctrl Pts',(63.2648756204188,-4.73461887606246,336.338533229735));
#61778=CARTESIAN_POINT('Ctrl Pts',(63.2570627571937,-4.69508925483987,336.471213502174));
#61779=CARTESIAN_POINT('Ctrl Pts',(63.2492498939685,-4.65001379314808,336.602047061117));
#61780=CARTESIAN_POINT('Ctrl Pts',(63.2415838477446,-4.60578537612114,336.730422034746));
#61781=CARTESIAN_POINT('Ctrl Pts',(63.2339178015206,-4.55621786312987,336.857018699575));
#61782=CARTESIAN_POINT('Ctrl Pts',(63.2262517552966,-4.50148740739158,336.981361699336));
#61783=CARTESIAN_POINT('Ctrl Pts',(63.2185864449777,-4.44676220552495,337.105692762742));
#61784=CARTESIAN_POINT('Ctrl Pts',(63.2109211346588,-4.38687520759319,337.227770225173));
#61785=CARTESIAN_POINT('Ctrl Pts',(63.2032558243399,-4.32205049997778,337.347139224277));
#61786=CARTESIAN_POINT('Ctrl Pts',(63.1955895046714,-4.25721725640083,337.466523941604));
#61787=CARTESIAN_POINT('Ctrl Pts',(63.187923185003,-4.18744520120901,337.583199134887));
#61788=CARTESIAN_POINT('Ctrl Pts',(63.1802568653345,-4.11300385274006,337.696735502389));
#61789=CARTESIAN_POINT('Ctrl Pts',(63.1723337737433,-4.0360692025302,337.814074600881));
#61790=CARTESIAN_POINT('Ctrl Pts',(63.1644106821521,-3.95414725526153,337.928060547587));
#61791=CARTESIAN_POINT('Ctrl Pts',(63.1564875905609,-3.8675826693192,338.038253998349));
#61792=CARTESIAN_POINT('Ctrl Pts',(63.1488099080652,-3.78369932673884,338.145034327506));
#61793=CARTESIAN_POINT('Ctrl Pts',(63.1411322255695,-3.69545699440657,338.248253350771));
#61794=CARTESIAN_POINT('Ctrl Pts',(63.1334545430737,-3.60320816603082,338.347547456684));
#61795=CARTESIAN_POINT('Ctrl Pts',(63.1254087469348,-3.50653638159864,338.45160231105));
#61796=CARTESIAN_POINT('Ctrl Pts',(63.1173629507959,-3.40546476805529,338.551346208977));
#61797=CARTESIAN_POINT('Ctrl Pts',(63.1093171546569,-3.30043869652034,338.646407474901));
#61798=CARTESIAN_POINT('Ctrl Pts',(63.101271358518,-3.19541262498533,338.741468740824));
#61799=CARTESIAN_POINT('Ctrl Pts',(63.0932255623791,-3.08643252695116,338.83184711668));
#61800=CARTESIAN_POINT('Ctrl Pts',(63.0851797662401,-2.97397827264193,338.917223033777));
#61801=CARTESIAN_POINT('Ctrl Pts',(63.0774046874617,-2.86530777302618,338.999726302533));
#61802=CARTESIAN_POINT('Ctrl Pts',(63.0696296086832,-2.75302977802615,339.077834456283));
#61803=CARTESIAN_POINT('Ctrl Pts',(63.0618545299048,-2.63753533516603,339.151215535027));
#61804=CARTESIAN_POINT('Ctrl Pts',(63.0540890188558,-2.5221830155706,339.224506313682));
#61805=CARTESIAN_POINT('Ctrl Pts',(63.0463235078068,-2.4036224502484,339.293081383815));
#61806=CARTESIAN_POINT('Ctrl Pts',(63.0385579967578,-2.28227710740803,339.356649431329));
#61807=CARTESIAN_POINT('Ctrl Pts',(63.0308001852356,-2.16105207882837,339.42015445094));
#61808=CARTESIAN_POINT('Ctrl Pts',(63.0230423737133,-2.03704811151664,339.478662147309));
#61809=CARTESIAN_POINT('Ctrl Pts',(63.0152845621911,-1.91071665831261,339.53192507817));
#61810=CARTESIAN_POINT('Ctrl Pts',(63.0075325886681,-1.78448027353341,339.585147926986));
#61811=CARTESIAN_POINT('Ctrl Pts',(62.9997806151451,-1.65592024787204,339.63313371507));
#61812=CARTESIAN_POINT('Ctrl Pts',(62.9920286416221,-1.52551126140707,339.675681603127));
#61813=CARTESIAN_POINT('Ctrl Pts',(62.9842799510645,-1.39515750322539,339.718211472128));
#61814=CARTESIAN_POINT('Ctrl Pts',(62.9765312605069,-1.26295671246653,339.75530790053));
#61815=CARTESIAN_POINT('Ctrl Pts',(62.9687825699493,-1.12940190723566,339.786818817799));
#61816=CARTESIAN_POINT('Ctrl Pts',(62.9610354915714,-0.9958748891974,339.818323178958));
#61817=CARTESIAN_POINT('Ctrl Pts',(62.9532884131936,-0.860994797226269,
339.844244250806));
#61818=CARTESIAN_POINT('Ctrl Pts',(62.9455413348157,-0.725267728605298,
339.864480422855));
#61819=CARTESIAN_POINT('Ctrl Pts',(62.9377941915099,-0.589539522460763,
339.884716764504));
#61820=CARTESIAN_POINT('Ctrl Pts',(62.9300470482041,-0.452964712108936,
339.899268053682));
#61821=CARTESIAN_POINT('Ctrl Pts',(62.9222999048983,-0.316057062770399,
339.90808424903));
#61822=CARTESIAN_POINT('Ctrl Pts',(62.9145510198703,-0.179118633685938,
339.916902426445));
#61823=CARTESIAN_POINT('Ctrl Pts',(62.9068021348421,-0.041847606703032,
339.919982919211));
#61824=CARTESIAN_POINT('Ctrl Pts',(62.899053249814,0.0952400849282741,339.917327769096));
#61825=CARTESIAN_POINT('Ctrl Pts',(62.8912961400393,0.232473282852045,339.914669800777));
#61826=CARTESIAN_POINT('Ctrl Pts',(62.8835390302646,0.369522365286114,339.906264036064));
#61827=CARTESIAN_POINT('Ctrl Pts',(62.8757819204898,0.505873801834289,339.892164629192));
#61828=CARTESIAN_POINT('Ctrl Pts',(62.8680206655637,0.642298100230388,339.878057688048));
#61829=CARTESIAN_POINT('Ctrl Pts',(62.8602594106375,0.778023623322308,339.858251098702));
#61830=CARTESIAN_POINT('Ctrl Pts',(62.8524981557114,0.912545885136313,339.832850408405));
#61831=CARTESIAN_POINT('Ctrl Pts',(62.8447244853067,1.04728333872861,339.807409085281));
#61832=CARTESIAN_POINT('Ctrl Pts',(62.836950814902,1.18081330375572,339.77635586756));
#61833=CARTESIAN_POINT('Ctrl Pts',(62.8291771444974,1.31264446998372,339.739846786334));
#61834=CARTESIAN_POINT('Ctrl Pts',(62.8217653403203,1.43833886370653,339.705037211623));
#61835=CARTESIAN_POINT('Ctrl Pts',(62.8143535361432,1.56248878346954,339.665268371201));
#61836=CARTESIAN_POINT('Ctrl Pts',(62.8069417319662,1.68468612922753,339.620715930296));
#61837=CARTESIAN_POINT('Ctrl Pts',(62.7991666531877,1.81287273090878,339.573979841546));
#61838=CARTESIAN_POINT('Ctrl Pts',(62.7913915744093,1.93931560936574,339.521831684043));
#61839=CARTESIAN_POINT('Ctrl Pts',(62.7836164956309,2.06352399409944,339.46442065539));
#61840=CARTESIAN_POINT('Ctrl Pts',(62.7758509845819,2.18757953250806,339.407080274663));
#61841=CARTESIAN_POINT('Ctrl Pts',(62.7680854735329,2.30940569686697,339.34449007119));
#61842=CARTESIAN_POINT('Ctrl Pts',(62.7603199624839,2.42852835199182,339.276848501651));
#61843=CARTESIAN_POINT('Ctrl Pts',(62.7525621509617,2.54753289665754,339.209273998924));
#61844=CARTESIAN_POINT('Ctrl Pts',(62.7448043394394,2.66383892880011,339.136658288979));
#61845=CARTESIAN_POINT('Ctrl Pts',(62.7370465279172,2.7769940619019,339.059247102932));
#61846=CARTESIAN_POINT('Ctrl Pts',(62.7292945543942,2.89006404217744,338.981894171257));
#61847=CARTESIAN_POINT('Ctrl Pts',(62.7215425808713,2.99998752176656,338.899753166327));
#61848=CARTESIAN_POINT('Ctrl Pts',(62.7137906073483,3.1063387339954,338.81311457108));
#61849=CARTESIAN_POINT('Ctrl Pts',(62.7060419167907,3.21264490642279,338.726512667329));
#61850=CARTESIAN_POINT('Ctrl Pts',(62.698293226233,3.31538151804279,338.635417208001));
#61851=CARTESIAN_POINT('Ctrl Pts',(62.6905445356754,3.41415388911361,338.540160488445));
#61852=CARTESIAN_POINT('Ctrl Pts',(62.6827974572975,3.5129057097676,338.444923587846));
#61853=CARTESIAN_POINT('Ctrl Pts',(62.6750503789197,3.60769464926973,338.345527420295));
#61854=CARTESIAN_POINT('Ctrl Pts',(62.6673033005419,3.69816138291436,338.242342586529));
#61855=CARTESIAN_POINT('Ctrl Pts',(62.6595561572361,3.78862887475735,338.139156887975));
#61856=CARTESIAN_POINT('Ctrl Pts',(62.6518090139303,3.87477383080808,338.032182753782));
#61857=CARTESIAN_POINT('Ctrl Pts',(62.6440618706245,3.95627614237726,337.921825139832));
#61858=CARTESIAN_POINT('Ctrl Pts',(62.6363129855964,4.03779677739658,337.811442715148));
#61859=CARTESIAN_POINT('Ctrl Pts',(62.6285641005683,4.11467245879398,337.697675611404));
#61860=CARTESIAN_POINT('Ctrl Pts',(62.6208152155402,4.18662570244882,337.580958792793));
#61861=CARTESIAN_POINT('Ctrl Pts',(62.6130581057654,4.25865531801975,337.464118089745));
#61862=CARTESIAN_POINT('Ctrl Pts',(62.6053009959907,4.32575185352346,337.344321750904));
#61863=CARTESIAN_POINT('Ctrl Pts',(62.597543886216,4.38768294764708,337.222030920898));
#61864=CARTESIAN_POINT('Ctrl Pts',(62.5897826312898,4.44964713576718,337.099674742583));
#61865=CARTESIAN_POINT('Ctrl Pts',(62.5820213763637,4.50644022070559,336.974821772641));
#61866=CARTESIAN_POINT('Ctrl Pts',(62.5742601214375,4.55787795308787,336.847953361764));
#61867=CARTESIAN_POINT('Ctrl Pts',(62.5664864510329,4.60939796907848,336.720882002776));
#61868=CARTESIAN_POINT('Ctrl Pts',(62.5587127806282,4.65554538182932,336.591789128506));
#61869=CARTESIAN_POINT('Ctrl Pts',(62.5509391102236,4.69618552505608,336.461172329588));
#61870=CARTESIAN_POINT('Ctrl Pts',(62.5435273060464,4.7349338598383,336.336635774084));
#61871=CARTESIAN_POINT('Ctrl Pts',(62.5361155018693,4.76867603880182,336.210714256445));
#61872=CARTESIAN_POINT('Ctrl Pts',(62.5287036976922,4.79733893623155,336.083846019237));
#61873=CARTESIAN_POINT('Ctrl Pts',(62.5209286189138,4.82740668764666,335.950759591804));
#61874=CARTESIAN_POINT('Ctrl Pts',(62.5131535401353,4.85197968629453,335.816210717483));
#61875=CARTESIAN_POINT('Ctrl Pts',(62.5053784613569,4.87091781154455,335.680692835042));
#61876=CARTESIAN_POINT('Ctrl Pts',(62.4976129503079,4.88983263222578,335.545341715983));
#61877=CARTESIAN_POINT('Ctrl Pts',(62.4898474392589,4.90312632274071,335.409024344802));
#61878=CARTESIAN_POINT('Ctrl Pts',(62.4820819282098,4.91070918778971,335.272246828187));
#61879=CARTESIAN_POINT('Ctrl Pts',(62.4743241166877,4.91828453440588,335.135604926878));
#61880=CARTESIAN_POINT('Ctrl Pts',(62.4665663051655,4.92016030235625,334.99850417583));
#61881=CARTESIAN_POINT('Ctrl Pts',(62.4588084936434,4.91629831987537,334.861457975723));
#61882=CARTESIAN_POINT('Ctrl Pts',(62.4510565201203,4.91243924365874,334.724514907228));
#61883=CARTESIAN_POINT('Ctrl Pts',(62.4433045465973,4.90285102242474,334.587626697109));
#61884=CARTESIAN_POINT('Ctrl Pts',(62.4355525730743,4.88754752269653,334.451308578632));
#61885=CARTESIAN_POINT('Ctrl Pts',(62.4278038825167,4.87225050400953,334.315048190959));
#61886=CARTESIAN_POINT('Ctrl Pts',(62.4200551919591,4.85124306439688,334.179357802359));
#61887=CARTESIAN_POINT('Ctrl Pts',(62.4123065014014,4.82459105425371,334.044749131529));
#61888=CARTESIAN_POINT('Ctrl Pts',(62.4045594230236,4.79794458928388,333.910168467157));
#61889=CARTESIAN_POINT('Ctrl Pts',(62.3968123446458,4.76565596561848,333.776669456083));
#61890=CARTESIAN_POINT('Ctrl Pts',(62.3890652662679,4.72784237810801,333.644754815443));
#61891=CARTESIAN_POINT('Ctrl Pts',(62.3813181229621,4.69002847368325,333.512839069231));
#61892=CARTESIAN_POINT('Ctrl Pts',(62.3735709796563,4.64668962076268,333.382508095679));
#61893=CARTESIAN_POINT('Ctrl Pts',(62.3658238363505,4.59799312620769,333.254250225878));
#61894=CARTESIAN_POINT('Ctrl Pts',(62.3580749513224,4.54928568364693,333.125963520985));
#61895=CARTESIAN_POINT('Ctrl Pts',(62.3503260662943,4.49521834132334,332.999751212637));
#61896=CARTESIAN_POINT('Ctrl Pts',(62.3425771812662,4.43600670732754,332.876082027232));
#61897=CARTESIAN_POINT('Ctrl Pts',(62.3348200714915,4.37673222549155,332.752281578077));
#61898=CARTESIAN_POINT('Ctrl Pts',(62.3270629617168,4.31230271377637,332.63102999707));
#61899=CARTESIAN_POINT('Ctrl Pts',(62.319305851942,4.2429802144996,332.512772233617));
#61900=CARTESIAN_POINT('Ctrl Pts',(62.3115445970159,4.17362067149572,332.394451276997));
#61901=CARTESIAN_POINT('Ctrl Pts',(62.3037833420897,4.0993631424971,332.279127654147));
#61902=CARTESIAN_POINT('Ctrl Pts',(62.2960220871635,4.02051269766,332.167216790777));
#61903=CARTESIAN_POINT('Ctrl Pts',(62.2882484167588,3.94153611780852,332.055126906498));
#61904=CARTESIAN_POINT('Ctrl Pts',(62.2804747463542,3.85795217873632,331.946461000988));
#61905=CARTESIAN_POINT('Ctrl Pts',(62.2727010759495,3.77010643937014,331.841601592845));
#61906=CARTESIAN_POINT('Ctrl Pts',(62.2652892717725,3.68634994030634,331.741623415379));
#61907=CARTESIAN_POINT('Ctrl Pts',(62.2578774675954,3.59871967886907,331.645105538661));
#61908=CARTESIAN_POINT('Ctrl Pts',(62.2504656634184,3.50754461006283,331.552346613866));
#61909=CARTESIAN_POINT('Ctrl Pts',(62.2426905846399,3.41190077953747,331.455041297852));
#61910=CARTESIAN_POINT('Ctrl Pts',(62.2349155058615,3.31205362021402,331.36156522274));
#61911=CARTESIAN_POINT('Ctrl Pts',(62.2271404270831,3.20834224796475,331.272303246987));
#61912=CARTESIAN_POINT('Ctrl Pts',(62.2193749160341,3.10475849916148,331.183151113778));
#61913=CARTESIAN_POINT('Ctrl Pts',(62.2116094049851,2.99732029226123,331.09820301438));
#61914=CARTESIAN_POINT('Ctrl Pts',(62.2038438939361,2.8864046839016,331.017808258854));
#61915=CARTESIAN_POINT('Ctrl Pts',(62.1960860824139,2.77559904869134,330.937493214963));
#61916=CARTESIAN_POINT('Ctrl Pts',(62.1883282708917,2.66132318788856,330.861722758444));
#61917=CARTESIAN_POINT('Ctrl Pts',(62.1805704593696,2.54398817414573,330.790806819317));
#61918=CARTESIAN_POINT('Ctrl Pts',(62.1728184858466,2.42674145872108,330.719944246683));
#61919=CARTESIAN_POINT('Ctrl Pts',(62.1650665123236,2.30644050576853,330.653929121335));
#61920=CARTESIAN_POINT('Ctrl Pts',(62.1573145388006,2.18352608990462,330.593028604903));
#61921=CARTESIAN_POINT('Ctrl Pts',(62.149565848243,2.06066372836879,330.532153879875));
#61922=CARTESIAN_POINT('Ctrl Pts',(62.1418171576854,1.93519045478687,330.476389628835));
#61923=CARTESIAN_POINT('Ctrl Pts',(62.1340684671277,1.80757221975524,330.42595739713));
#61924=CARTESIAN_POINT('Ctrl Pts',(62.1263213887499,1.67998053676338,330.375535658272));
#61925=CARTESIAN_POINT('Ctrl Pts',(62.1185743103721,1.55024514328905,330.330443875696));
#61926=CARTESIAN_POINT('Ctrl Pts',(62.1108272319943,1.41885220575438,330.29085554684));
#61927=CARTESIAN_POINT('Ctrl Pts',(62.1030800886884,1.28745816701971,330.251266886196));
#61928=CARTESIAN_POINT('Ctrl Pts',(62.0953329453826,1.15440693077219,330.217181884032));
#61929=CARTESIAN_POINT('Ctrl Pts',(62.0875858020767,1.02019968438663,330.188724112413));
#61930=CARTESIAN_POINT('Ctrl Pts',(62.0798369170487,0.88596226536342,330.160259942883));
#61931=CARTESIAN_POINT('Ctrl Pts',(62.0720880320206,0.750568701336808,330.137425602411));
#61932=CARTESIAN_POINT('Ctrl Pts',(62.0643391469925,0.614529832246269,330.120293436304));
#61933=CARTESIAN_POINT('Ctrl Pts',(62.0565820372177,0.47834657009444,330.103143085939));
#61934=CARTESIAN_POINT('Ctrl Pts',(62.048824927443,0.34151702308346,330.091707048987));
#61935=CARTESIAN_POINT('Ctrl Pts',(62.0410678176683,0.204557164794303,330.086005756126));
#61936=CARTESIAN_POINT('Ctrl Pts',(62.0333065627421,0.0675241195359115,
330.080301416676));
#61937=CARTESIAN_POINT('Ctrl Pts',(62.025545307816,-0.0696389850770303,
330.080337927434));
#61938=CARTESIAN_POINT('Ctrl Pts',(62.0177840528898,-0.206417717737142,
330.086083559084));
#61939=CARTESIAN_POINT('Ctrl Pts',(62.0100103824852,-0.343415251793332,
330.091838381873));
#61940=CARTESIAN_POINT('Ctrl Pts',(62.0022367120805,-0.480026795498825,
330.103320542704));
#61941=CARTESIAN_POINT('Ctrl Pts',(61.9944630416758,-0.615743679042492,
330.120446456466));
#61942=CARTESIAN_POINT('Ctrl Pts',(61.9870512374987,-0.745142909006524,
330.136775154821));
#61943=CARTESIAN_POINT('Ctrl Pts',(61.9796394333216,-0.873728613345349,
330.158233949887));
#61944=CARTESIAN_POINT('Ctrl Pts',(61.9722276291444,-1.00107163348714,330.184707833669));
#61945=CARTESIAN_POINT('Ctrl Pts',(61.964452550366,-1.1346561143806,330.212479281356));
#61946=CARTESIAN_POINT('Ctrl Pts',(61.9566774715876,-1.26729516730605,330.245857619878));
#61947=CARTESIAN_POINT('Ctrl Pts',(61.9489023928091,-1.39848164151895,330.284765948457));
#61948=CARTESIAN_POINT('Ctrl Pts',(61.9411368817601,-1.52950668242314,330.32362639786));
#61949=CARTESIAN_POINT('Ctrl Pts',(61.9333713707111,-1.65908233005115,330.368003187231));
#61950=CARTESIAN_POINT('Ctrl Pts',(61.9256058596622,-1.78671079513906,330.417768273316));
#61951=CARTESIAN_POINT('Ctrl Pts',(61.91784804814,-1.91421271623269,330.467484017173));
#61952=CARTESIAN_POINT('Ctrl Pts',(61.9100902366177,-2.03977093503971,330.522577284761));
#61953=CARTESIAN_POINT('Ctrl Pts',(61.9023324250955,-2.16290236979551,330.582870117233));
#61954=CARTESIAN_POINT('Ctrl Pts',(61.8945804515725,-2.28594114424235,330.643117577437));
#61955=CARTESIAN_POINT('Ctrl Pts',(61.8868284780495,-2.40655642002873,330.708556643011));
#61956=CARTESIAN_POINT('Ctrl Pts',(61.8790765045264,-2.52428500680449,330.778961233663));
#61957=CARTESIAN_POINT('Ctrl Pts',(61.8713278139688,-2.6419637354533,330.849336007929));
#61958=CARTESIAN_POINT('Ctrl Pts',(61.8635791234112,-2.75675787182096,330.924671924549));
#61959=CARTESIAN_POINT('Ctrl Pts',(61.8558304328536,-2.86822896109472,331.004697046626));
#61960=CARTESIAN_POINT('Ctrl Pts',(61.8480833544758,-2.97967685787717,331.084705518808));
#61961=CARTESIAN_POINT('Ctrl Pts',(61.8403362760979,-3.08780276546037,331.169401028047));
#61962=CARTESIAN_POINT('Ctrl Pts',(61.8325891977201,-3.19219769360033,331.258468636043));
#61963=CARTESIAN_POINT('Ctrl Pts',(61.8248420544143,-3.29659349667041,331.347536990512));
#61964=CARTESIAN_POINT('Ctrl Pts',(61.8170949111085,-3.39725796057302,331.440977263128));
#61965=CARTESIAN_POINT('Ctrl Pts',(61.8093477678027,-3.4938159496763,331.53843486667));
#61966=CARTESIAN_POINT('Ctrl Pts',(61.8015988827747,-3.59039564706519,331.635914380749));
#61967=CARTESIAN_POINT('Ctrl Pts',(61.7938499977466,-3.68286675749314,331.73741274537));
#61968=CARTESIAN_POINT('Ctrl Pts',(61.7861011127185,-3.77089199944426,331.842539534527));
#61969=CARTESIAN_POINT('Ctrl Pts',(61.7783440029438,-3.85901067229702,331.947777906343));
#61970=CARTESIAN_POINT('Ctrl Pts',(61.7705868931691,-3.94267379891279,332.056652095761));
#61971=CARTESIAN_POINT('Ctrl Pts',(61.7628297833944,-4.02158497578674,332.168739265799));
#61972=CARTESIAN_POINT('Ctrl Pts',(61.7550685284682,-4.10053832027053,332.280886331638));
#61973=CARTESIAN_POINT('Ctrl Pts',(61.747307273542,-4.17473444391868,332.396249470619));
#61974=CARTESIAN_POINT('Ctrl Pts',(61.7395460186159,-4.24392164029049,332.51437891593));
#61975=CARTESIAN_POINT('Ctrl Pts',(61.7317723482112,-4.31321951362839,332.632697329855));
#61976=CARTESIAN_POINT('Ctrl Pts',(61.7239986778065,-4.37749226469182,332.753790547508));
#61977=CARTESIAN_POINT('Ctrl Pts',(61.7162250074019,-4.43653491156297,332.877185584894));
#61978=CARTESIAN_POINT('Ctrl Pts',(61.7088132032248,-4.49282910901754,332.994836553602));
#61979=CARTESIAN_POINT('Ctrl Pts',(61.7014013990477,-4.54436905330684,333.114579600951));
#61980=CARTESIAN_POINT('Ctrl Pts',(61.6939895948706,-4.59101921477869,333.235991600918));
#61981=CARTESIAN_POINT('Ctrl Pts',(61.6851310443183,-4.64677524985418,333.381102604077));
#61982=CARTESIAN_POINT('Ctrl Pts',(61.676272493766,-4.69569362969611,333.528978980461));
#61983=CARTESIAN_POINT('Ctrl Pts',(61.6674139432137,-4.73752685456457,333.679007053471));
#61984=CARTESIAN_POINT('Ctrl Pts',(61.6585852460574,-4.77921910108445,333.828529530509));
#61985=CARTESIAN_POINT('Ctrl Pts',(61.6497565489011,-4.81387375886097,333.980189069039));
#61986=CARTESIAN_POINT('Ctrl Pts',(61.6409278517448,-4.84129228426136,334.133355851083));
#61987=CARTESIAN_POINT('Ctrl Pts',(61.6321565567288,-4.86853254077153,334.28552677825));
#61988=CARTESIAN_POINT('Ctrl Pts',(61.623385261713,-4.88863036829126,334.439185241312));
#61989=CARTESIAN_POINT('Ctrl Pts',(61.6146139666971,-4.90143841270151,334.59369402048));
#61990=CARTESIAN_POINT('Ctrl Pts',(61.6070151033191,-4.91253444577709,334.727550093209));
#61991=CARTESIAN_POINT('Ctrl Pts',(61.5994162399411,-4.91815993583621,334.862043987869));
#61992=CARTESIAN_POINT('Ctrl Pts',(61.5918173765632,-4.91824892677099,334.996750874583));
#61993=CARTESIAN_POINT('',(59.841817376455,-4.9182486281821,335.003673402358));
#61994=CARTESIAN_POINT('Ctrl Pts',(61.5918173765087,-4.91824892677163,334.996750875548));
#61995=CARTESIAN_POINT('Ctrl Pts',(61.5840252789637,-4.91834018066105,335.134883271021));
#61996=CARTESIAN_POINT('Ctrl Pts',(61.5762331814186,-4.91260779228916,335.273048117306));
#61997=CARTESIAN_POINT('Ctrl Pts',(61.5684410838736,-4.90107024508939,335.410723161265));
#61998=CARTESIAN_POINT('Ctrl Pts',(61.5606487003074,-4.88953227438594,335.548403258801));
#61999=CARTESIAN_POINT('Ctrl Pts',(61.5528563167414,-4.87218875192799,335.685593135114));
#62000=CARTESIAN_POINT('Ctrl Pts',(61.5450639331752,-4.84911011845927,335.821774982313));
#62001=CARTESIAN_POINT('Ctrl Pts',(61.5372696505982,-4.82602586070693,335.95799001715));
#62002=CARTESIAN_POINT('Ctrl Pts',(61.5294753680212,-4.79720377335317,336.093196154834));
#62003=CARTESIAN_POINT('Ctrl Pts',(61.5216810854442,-4.76276550273706,336.226885417811));
#62004=CARTESIAN_POINT('Ctrl Pts',(61.5138832899863,-4.72831171080222,336.360634934501));
#62005=CARTESIAN_POINT('Ctrl Pts',(61.5060854945284,-4.68823679188107,336.492865843505));
#62006=CARTESIAN_POINT('Ctrl Pts',(61.4982876990705,-4.64271227470297,336.623085270965));
#62007=CARTESIAN_POINT('Ctrl Pts',(61.4904799396305,-4.59712958653596,336.753471092124));
#62008=CARTESIAN_POINT('Ctrl Pts',(61.4826721801905,-4.54608352075104,336.881839935816));
#62009=CARTESIAN_POINT('Ctrl Pts',(61.4748644207505,-4.48979403191505,337.007718260484));
#62010=CARTESIAN_POINT('Ctrl Pts',(61.4670510735764,-4.43346425870533,337.133686671766));
#62011=CARTESIAN_POINT('Ctrl Pts',(61.4592377264023,-4.37188375645724,337.2571606695));
#62012=CARTESIAN_POINT('Ctrl Pts',(61.4514243792281,-4.30531805861462,337.377692048325));
#62013=CARTESIAN_POINT('Ctrl Pts',(61.4435985258357,-4.2386458142272,337.498416352371));
#62014=CARTESIAN_POINT('Ctrl Pts',(61.4357726724433,-4.16697263647571,337.616188302863));
#62015=CARTESIAN_POINT('Ctrl Pts',(61.427946819051,-4.09060730540156,337.73058875254));
#62016=CARTESIAN_POINT('Ctrl Pts',(61.4238817328995,-4.0509398551901,337.790013285608));
#62017=CARTESIAN_POINT('Ctrl Pts',(61.4198166467479,-4.01000702988523,337.848528657322));
#62018=CARTESIAN_POINT('Ctrl Pts',(61.4157515605964,-3.96785622599952,337.906079839285));
#62019=CARTESIAN_POINT('Ctrl Pts',(61.407976481818,-3.88723657648375,338.016154990678));
#62020=CARTESIAN_POINT('Ctrl Pts',(61.4002014030395,-3.80190555086133,338.12304674859));
#62021=CARTESIAN_POINT('Ctrl Pts',(61.3924263242611,-3.71214325095125,338.226325393837));
#62022=CARTESIAN_POINT('Ctrl Pts',(61.3846608132121,-3.62249140926588,338.329476948136));
#62023=CARTESIAN_POINT('Ctrl Pts',(61.3768953021631,-3.52841939708857,338.429023944163));
#62024=CARTESIAN_POINT('Ctrl Pts',(61.3691297911141,-3.4302499846955,338.5245663712));
#62025=CARTESIAN_POINT('Ctrl Pts',(61.361371979592,-3.33217790756069,338.620014067643));
#62026=CARTESIAN_POINT('Ctrl Pts',(61.3536141680697,-3.23001679329037,338.711464825838));
#62027=CARTESIAN_POINT('Ctrl Pts',(61.3458563565476,-3.12412874913807,338.798552700873));
#62028=CARTESIAN_POINT('Ctrl Pts',(61.3381043830245,-3.01832038909653,338.88557503952));
#62029=CARTESIAN_POINT('Ctrl Pts',(61.3303524095015,-2.90879098232934,338.968240782784));
#62030=CARTESIAN_POINT('Ctrl Pts',(61.3226004359785,-2.79593819245683,339.046222026343));
#62031=CARTESIAN_POINT('Ctrl Pts',(61.3148517454209,-2.68313319580806,339.124170244799));
#62032=CARTESIAN_POINT('Ctrl Pts',(61.3071030548632,-2.56700793628352,339.197437687621));
#62033=CARTESIAN_POINT('Ctrl Pts',(61.2993543643056,-2.44799156563884,339.265737961603));
#62034=CARTESIAN_POINT('Ctrl Pts',(61.2916072859278,-2.32899995734421,339.334024025142));
#62035=CARTESIAN_POINT('Ctrl Pts',(61.28386020755,-2.20711877319843,339.397344781037));
#62036=CARTESIAN_POINT('Ctrl Pts',(61.2761131291721,-2.08280409522519,339.455458468375));
#62037=CARTESIAN_POINT('Ctrl Pts',(61.2683659858663,-1.95848837537512,339.513572642762));
#62038=CARTESIAN_POINT('Ctrl Pts',(61.2606188425605,-1.83173947511246,339.566479496019));
#62039=CARTESIAN_POINT('Ctrl Pts',(61.2528716992547,-1.70303553671758,339.61398450617));
#62040=CARTESIAN_POINT('Ctrl Pts',(61.2451228142266,-1.57430266294463,339.661500196456));
#62041=CARTESIAN_POINT('Ctrl Pts',(61.2373739291985,-1.44361424303709,339.703611491697));
#62042=CARTESIAN_POINT('Ctrl Pts',(61.2296250441704,-1.3114653547824,339.740173170434));
#62043=CARTESIAN_POINT('Ctrl Pts',(61.2218679343956,-1.17917620233272,339.776773656116));
#62044=CARTESIAN_POINT('Ctrl Pts',(61.2141108246209,-1.04542386227026,339.807812654235));
#62045=CARTESIAN_POINT('Ctrl Pts',(61.2063537148462,-0.910715975303693,
339.833195575892));
#62046=CARTESIAN_POINT('Ctrl Pts',(61.19859245992,-0.77593610474936,339.858592061372));
#62047=CARTESIAN_POINT('Ctrl Pts',(61.1908312049939,-0.640200056458475,
339.878326391725));
#62048=CARTESIAN_POINT('Ctrl Pts',(61.1830699500677,-0.504021463225214,
339.892355815669));
#62049=CARTESIAN_POINT('Ctrl Pts',(61.175296279663,-0.367625028623465,339.906407682119));
#62050=CARTESIAN_POINT('Ctrl Pts',(61.1675226092584,-0.230785024787696,
339.914736381967));
#62051=CARTESIAN_POINT('Ctrl Pts',(61.1597489388537,-0.0940168575877119,
339.917351308681));
#62052=CARTESIAN_POINT('Ctrl Pts',(61.1523371346767,0.0363847185236617,
339.919844509927));
#62053=CARTESIAN_POINT('Ctrl Pts',(61.1449253304996,0.166720707746468,339.917143925025));
#62054=CARTESIAN_POINT('Ctrl Pts',(61.1375135263226,0.29654985591658,339.909301502806));
#62055=CARTESIAN_POINT('Ctrl Pts',(61.1297384475442,0.432742317380743,339.901074700113));
#62056=CARTESIAN_POINT('Ctrl Pts',(61.1219633687657,0.568807391302568,339.887163283864));
#62057=CARTESIAN_POINT('Ctrl Pts',(61.1141882899873,0.704232138484992,339.867570251945));
#62058=CARTESIAN_POINT('Ctrl Pts',(61.1064227789383,0.839490236894263,339.8480013305));
#62059=CARTESIAN_POINT('Ctrl Pts',(61.0986572678893,0.974109193235749,339.822764760078));
#62060=CARTESIAN_POINT('Ctrl Pts',(61.0908917568403,1.10757796044543,339.791915496337));
#62061=CARTESIAN_POINT('Ctrl Pts',(61.0831339453181,1.24091439298383,339.761096819731));
#62062=CARTESIAN_POINT('Ctrl Pts',(61.0753761337959,1.37310252750178,339.724676611932));
#62063=CARTESIAN_POINT('Ctrl Pts',(61.0676183222737,1.5036386761024,339.682761342865));
#62064=CARTESIAN_POINT('Ctrl Pts',(61.0598663487507,1.63407659211166,339.640877616366));
#62065=CARTESIAN_POINT('Ctrl Pts',(61.0521143752277,1.76286462601576,339.593507178548));
#62066=CARTESIAN_POINT('Ctrl Pts',(61.0443624017047,1.8895118374728,339.540806985388));
#62067=CARTESIAN_POINT('Ctrl Pts',(61.036613711147,2.01610541376061,339.488129110792));
#62068=CARTESIAN_POINT('Ctrl Pts',(61.0288650205894,2.14055961071737,339.43012612003));
#62069=CARTESIAN_POINT('Ctrl Pts',(61.0211163300318,2.26240135554464,339.367003912172));
#62070=CARTESIAN_POINT('Ctrl Pts',(61.013369251654,2.38421775017934,339.303894837417));
#62071=CARTESIAN_POINT('Ctrl Pts',(61.0056221732762,2.50342242698248,339.235668843807));
#62072=CARTESIAN_POINT('Ctrl Pts',(60.9978750948983,2.61956527189246,339.162578629743));
#62073=CARTESIAN_POINT('Ctrl Pts',(60.9901279515925,2.73570909019103,339.089487803113));
#62074=CARTESIAN_POINT('Ctrl Pts',(60.9823808082867,2.84879069459559,339.011532882906));
#62075=CARTESIAN_POINT('Ctrl Pts',(60.9746336649809,2.95838775720216,338.929010682161));
#62076=CARTESIAN_POINT('Ctrl Pts',(60.9668847799529,3.06800945955507,338.846469928674));
#62077=CARTESIAN_POINT('Ctrl Pts',(60.9591358949248,3.17414474903934,338.759360086459));
#62078=CARTESIAN_POINT('Ctrl Pts',(60.9513870098967,3.27640359083491,338.668018889328));
#62079=CARTESIAN_POINT('Ctrl Pts',(60.943629900122,3.37877097122196,338.576580741705));
#62080=CARTESIAN_POINT('Ctrl Pts',(60.9358727903473,3.47725339284377,338.480902528365));
#62081=CARTESIAN_POINT('Ctrl Pts',(60.9281156805725,3.57149660036133,338.381359947729));
#62082=CARTESIAN_POINT('Ctrl Pts',(60.9203544256464,3.66579016843575,338.281764174721));
#62083=CARTESIAN_POINT('Ctrl Pts',(60.9125931707202,3.75583975210618,338.178300214421));
#62084=CARTESIAN_POINT('Ctrl Pts',(60.904831915794,3.8413314447297,338.071376856433));
#62085=CARTESIAN_POINT('Ctrl Pts',(60.8970582453894,3.92695989619969,337.964282455918));
#62086=CARTESIAN_POINT('Ctrl Pts',(60.8892845749847,4.00801565554107,337.853717914728));
#62087=CARTESIAN_POINT('Ctrl Pts',(60.8815109045801,4.08422770622956,337.740121731998));
#62088=CARTESIAN_POINT('Ctrl Pts',(60.874099100403,4.15689206762335,337.631813478903));
#62089=CARTESIAN_POINT('Ctrl Pts',(60.8666872962258,4.2251533706113,337.520749723517));
#62090=CARTESIAN_POINT('Ctrl Pts',(60.8592754920487,4.28881651212754,337.407329638376));
#62091=CARTESIAN_POINT('Ctrl Pts',(60.8515004132702,4.35559997385188,337.288350497001));
#62092=CARTESIAN_POINT('Ctrl Pts',(60.8437253344918,4.41753418605225,337.16640220795));
#62093=CARTESIAN_POINT('Ctrl Pts',(60.8359502557134,4.47434408888371,337.041917735065));
#62094=CARTESIAN_POINT('Ctrl Pts',(60.8281847446644,4.531084083513,336.917586448249));
#62095=CARTESIAN_POINT('Ctrl Pts',(60.8204192336153,4.58271215475666,336.790725539562));
#62096=CARTESIAN_POINT('Ctrl Pts',(60.8126537225663,4.62899795911042,336.661794499044));
#62097=CARTESIAN_POINT('Ctrl Pts',(60.8048959110441,4.67523787095444,336.532991294027));
#62098=CARTESIAN_POINT('Ctrl Pts',(60.7971380995219,4.71614592576654,336.40212240737));
#62099=CARTESIAN_POINT('Ctrl Pts',(60.7893802879997,4.75153908195503,336.269669017955));
#62100=CARTESIAN_POINT('Ctrl Pts',(60.7816283144767,4.78690560367109,336.137315303916));
#62101=CARTESIAN_POINT('Ctrl Pts',(60.7738763409537,4.81676538690688,336.003379836615));
#62102=CARTESIAN_POINT('Ctrl Pts',(60.7661243674307,4.84098474330442,335.868360396145));
#62103=CARTESIAN_POINT('Ctrl Pts',(60.7583756768731,4.86519384279014,335.73339813649));
#62104=CARTESIAN_POINT('Ctrl Pts',(60.7506269863155,4.8837671975729,335.597353200643));
#62105=CARTESIAN_POINT('Ctrl Pts',(60.7428782957579,4.89662194573607,335.460734829415));
#62106=CARTESIAN_POINT('Ctrl Pts',(60.7351312173801,4.90947401936153,335.32414488278));
#62107=CARTESIAN_POINT('Ctrl Pts',(60.7273841390022,4.91660981637787,335.186982126987));
#62108=CARTESIAN_POINT('Ctrl Pts',(60.7196370606244,4.9179982537162,335.049761822157));
#62109=CARTESIAN_POINT('Ctrl Pts',(60.7118899173186,4.91938670269097,334.91254036729));
#62110=CARTESIAN_POINT('Ctrl Pts',(60.7041427740128,4.91502769195745,334.775261753279));
#62111=CARTESIAN_POINT('Ctrl Pts',(60.696395630707,4.904942272072,334.638441747237));
#62112=CARTESIAN_POINT('Ctrl Pts',(60.6886467456789,4.89485458477002,334.501590981152));
#62113=CARTESIAN_POINT('Ctrl Pts',(60.6808978606508,4.87903795522636,334.365199417943));
#62114=CARTESIAN_POINT('Ctrl Pts',(60.6731489756227,4.85756532078576,334.229777813355));
#62115=CARTESIAN_POINT('Ctrl Pts',(60.665391865848,4.83606989506913,334.094212470877));
#62116=CARTESIAN_POINT('Ctrl Pts',(60.6576347560733,4.80890653352618,333.959619530252));
#62117=CARTESIAN_POINT('Ctrl Pts',(60.6498776462985,4.77619946108342,333.826500204326));
#62118=CARTESIAN_POINT('Ctrl Pts',(60.6421163913724,4.74347491102684,333.693309743688));
#62119=CARTESIAN_POINT('Ctrl Pts',(60.6343551364462,4.70520085627216,333.561594841977));
#62120=CARTESIAN_POINT('Ctrl Pts',(60.62659388152,4.66155118382066,333.431840689496));
#62121=CARTESIAN_POINT('Ctrl Pts',(60.6188202111154,4.6178316861187,333.301878972658));
#62122=CARTESIAN_POINT('Ctrl Pts',(60.6110465407107,4.5687195269991,333.173884637949));
#62123=CARTESIAN_POINT('Ctrl Pts',(60.6032728703061,4.51443678714722,333.04832288599));
#62124=CARTESIAN_POINT('Ctrl Pts',(60.5958610661289,4.46268092189494,332.928606063792));
#62125=CARTESIAN_POINT('Ctrl Pts',(60.5884492619519,4.40622514842957,332.811100706942));
#62126=CARTESIAN_POINT('Ctrl Pts',(60.5810374577747,4.34529955798734,332.696186896935));
#62127=CARTESIAN_POINT('Ctrl Pts',(60.5732623789963,4.28138782286967,332.575640818788));
#62128=CARTESIAN_POINT('Ctrl Pts',(60.5654873002178,4.21235506095974,332.457565801843));
#62129=CARTESIAN_POINT('Ctrl Pts',(60.5577122214394,4.13841651012453,332.342427451371));
#62130=CARTESIAN_POINT('Ctrl Pts',(60.5499467103904,4.06456894538324,332.227430785968));
#62131=CARTESIAN_POINT('Ctrl Pts',(60.5421811993413,3.98582781257757,332.115363922454));
#62132=CARTESIAN_POINT('Ctrl Pts',(60.5344156882923,3.90245485459703,332.006669218023));
#62133=CARTESIAN_POINT('Ctrl Pts',(60.5266578767701,3.81916456114723,331.898082284707));
#62134=CARTESIAN_POINT('Ctrl Pts',(60.5189000652479,3.73125181815416,331.792861164855));
#62135=CARTESIAN_POINT('Ctrl Pts',(60.5111422537257,3.63902220489834,331.69142017555));
#62136=CARTESIAN_POINT('Ctrl Pts',(60.5033902802027,3.54686199735138,331.590055523806));
#62137=CARTESIAN_POINT('Ctrl Pts',(60.4956383066798,3.45039164757307,331.492465628481));
#62138=CARTESIAN_POINT('Ctrl Pts',(60.4878863331568,3.34995740302223,331.399032288337));
#62139=CARTESIAN_POINT('Ctrl Pts',(60.4801376425991,3.24956569243358,331.305638517269));
#62140=CARTESIAN_POINT('Ctrl Pts',(60.4723889520415,3.14521371150051,331.216398065943));
#62141=CARTESIAN_POINT('Ctrl Pts',(60.4646402614839,3.03728485034606,331.131656194137));
#62142=CARTESIAN_POINT('Ctrl Pts',(60.4568931831061,2.92937844469239,331.046931953585));
#62143=CARTESIAN_POINT('Ctrl Pts',(60.4491461047282,2.81789694632411,330.966704672081));
#62144=CARTESIAN_POINT('Ctrl Pts',(60.4413990263504,2.70325682763859,330.89127932486));
#62145=CARTESIAN_POINT('Ctrl Pts',(60.4336518830446,2.58861574815877,330.815853345501));
#62146=CARTESIAN_POINT('Ctrl Pts',(60.4259047397388,2.47081632209832,330.745229595536));
#62147=CARTESIAN_POINT('Ctrl Pts',(60.418157596433,2.35030366068907,330.679669484281));
#62148=CARTESIAN_POINT('Ctrl Pts',(60.410408711405,2.22976390547539,330.614094633721));
#62149=CARTESIAN_POINT('Ctrl Pts',(60.4026598263769,2.10651004438315,330.553585873939));
#62150=CARTESIAN_POINT('Ctrl Pts',(60.3949109413488,1.98101105339722,330.498358269607));
#62151=CARTESIAN_POINT('Ctrl Pts',(60.3871538315741,1.85537885648518,330.443072046124));
#62152=CARTESIAN_POINT('Ctrl Pts',(60.3793967217994,1.72749712773497,330.393078333237));
#62153=CARTESIAN_POINT('Ctrl Pts',(60.3716396120246,1.5978545729571,330.348543902585));
#62154=CARTESIAN_POINT('Ctrl Pts',(60.3638783570985,1.46814274134284,330.303985674157));
#62155=CARTESIAN_POINT('Ctrl Pts',(60.3561171021723,1.33666858328727,330.264892652226));
#62156=CARTESIAN_POINT('Ctrl Pts',(60.3483558472462,1.20393420590136,330.231381175816));
#62157=CARTESIAN_POINT('Ctrl Pts',(60.3405821768415,1.07098749676984,330.197816091965));
#62158=CARTESIAN_POINT('Ctrl Pts',(60.3328085064368,0.936776922719063,330.169850475507));
#62159=CARTESIAN_POINT('Ctrl Pts',(60.3250348360322,0.801813861477001,330.147549320803));
#62160=CARTESIAN_POINT('Ctrl Pts',(60.3176230318551,0.673133363205629,330.126286290215));
#62161=CARTESIAN_POINT('Ctrl Pts',(60.310211227678,0.543769143310523,330.110172263506));
#62162=CARTESIAN_POINT('Ctrl Pts',(60.3027994235009,0.414165335998664,330.099219435951));
#62163=CARTESIAN_POINT('Ctrl Pts',(60.2950243447224,0.27820926002092,330.087729777691));
#62164=CARTESIAN_POINT('Ctrl Pts',(60.287249265944,0.141559870683655,330.081883733119));
#62165=CARTESIAN_POINT('Ctrl Pts',(60.2794741871656,0.00472518295217616,
330.081752269848));
#62166=CARTESIAN_POINT('Ctrl Pts',(60.2717086761166,-0.131941120984726,
330.081620968351));
#62167=CARTESIAN_POINT('Ctrl Pts',(60.2639431650675,-0.268791882480986,
330.087190256553));
#62168=CARTESIAN_POINT('Ctrl Pts',(60.2561776540185,-0.405313469839718,
330.098479414134));
#62169=CARTESIAN_POINT('Ctrl Pts',(60.2484198424964,-0.541699695646555,
330.109757378483));
#62170=CARTESIAN_POINT('Ctrl Pts',(60.2406620309742,-0.677757009789399,
330.126743894063));
#62171=CARTESIAN_POINT('Ctrl Pts',(60.232904219452,-0.812971637710933,330.149406203486));
#62172=CARTESIAN_POINT('Ctrl Pts',(60.225152245929,-0.94808451233687,330.172051458803));
#62173=CARTESIAN_POINT('Ctrl Pts',(60.2174002724061,-1.08235557903715,330.200363941969));
#62174=CARTESIAN_POINT('Ctrl Pts',(60.2096482988831,-1.21527640071851,330.234259099326));
#62175=CARTESIAN_POINT('Ctrl Pts',(60.2018996083255,-1.34814093035378,330.268139902064));
#62176=CARTESIAN_POINT('Ctrl Pts',(60.1941509177679,-1.47965597433335,330.307598580255));
#62177=CARTESIAN_POINT('Ctrl Pts',(60.1864022272102,-1.60932372195161,330.352499572839));
#62178=CARTESIAN_POINT('Ctrl Pts',(60.1786551488324,-1.73896449111171,330.397391223396));
#62179=CARTESIAN_POINT('Ctrl Pts',(60.1709080704546,-1.86675835927599,330.447722808265));
#62180=CARTESIAN_POINT('Ctrl Pts',(60.1631609920767,-1.99222348915277,330.50330914652));
#62181=CARTESIAN_POINT('Ctrl Pts',(60.1554138487709,-2.11768967054852,330.558895950643));
#62182=CARTESIAN_POINT('Ctrl Pts',(60.1476667054651,-2.24082671735732,330.619737437661));
#62183=CARTESIAN_POINT('Ctrl Pts',(60.1399195621593,-2.36117392967945,330.685600767627));
#62184=CARTESIAN_POINT('Ctrl Pts',(60.1321706771312,-2.48154819860988,330.751478905067));
#62185=CARTESIAN_POINT('Ctrl Pts',(60.1244217921031,-2.59913104215112,330.822380944456));
#62186=CARTESIAN_POINT('Ctrl Pts',(60.116672907075,-2.71348781801745,330.898028897716));
#62187=CARTESIAN_POINT('Ctrl Pts',(60.1089157973002,-2.82796597334706,330.973757144496));
#62188=CARTESIAN_POINT('Ctrl Pts',(60.1011586875255,-2.93921089436184,331.054241151757));
#62189=CARTESIAN_POINT('Ctrl Pts',(60.0934015777507,-3.04681787247629,331.139160206061));
#62190=CARTESIAN_POINT('Ctrl Pts',(60.0856403228246,-3.15448235231953,331.224124638394));
#62191=CARTESIAN_POINT('Ctrl Pts',(60.0778790678984,-3.25850471938399,331.313528585457));
#62192=CARTESIAN_POINT('Ctrl Pts',(60.0701178129722,-3.35851542273365,331.407012772391));
#62193=CARTESIAN_POINT('Ctrl Pts',(60.0623441425675,-3.45868611061499,331.500646503558));
#62194=CARTESIAN_POINT('Ctrl Pts',(60.0545704721628,-3.55483203673541,331.598373238802));
#62195=CARTESIAN_POINT('Ctrl Pts',(60.0467968017582,-3.64662181011738,331.69979812186));
#62196=CARTESIAN_POINT('Ctrl Pts',(60.0393849975811,-3.73413874746507,331.796501652211));
#62197=CARTESIAN_POINT('Ctrl Pts',(60.031973193404,-3.8176957786048,331.896566560111));
#62198=CARTESIAN_POINT('Ctrl Pts',(60.0245613892269,-3.89704230176514,331.999625963192));
#62199=CARTESIAN_POINT('Ctrl Pts',(60.016776715821,-3.98038054896428,332.107870025667));
#62200=CARTESIAN_POINT('Ctrl Pts',(60.008992042415,-4.05934074947212,332.219764549991));
#62201=CARTESIAN_POINT('Ctrl Pts',(60.0012073690091,-4.13358642093639,332.334920946172));
#62202=CARTESIAN_POINT('Ctrl Pts',(59.9934321517147,-4.20774190552753,332.449937460862));
#62203=CARTESIAN_POINT('Ctrl Pts',(59.9856569344203,-4.2771940441256,332.568207642411));
#62204=CARTESIAN_POINT('Ctrl Pts',(59.9778817171259,-4.34164653907798,332.689309974875));
#62205=CARTESIAN_POINT('Ctrl Pts',(59.9701142788049,-4.40603455039957,332.810291146505));
#62206=CARTESIAN_POINT('Ctrl Pts',(59.9623468404838,-4.46543268857561,332.934098490605));
#62207=CARTESIAN_POINT('Ctrl Pts',(59.9545794021628,-4.51958814211101,333.060281956523));
#62208=CARTESIAN_POINT('Ctrl Pts',(59.9468180714008,-4.57370101305762,333.186366204019));
#62209=CARTESIAN_POINT('Ctrl Pts',(59.9390567406389,-4.62257925027931,333.314822499283));
#62210=CARTESIAN_POINT('Ctrl Pts',(59.9312954098769,-4.66601633569451,333.445176981926));
#62211=CARTESIAN_POINT('Ctrl Pts',(59.9235382621031,-4.70943001058681,333.575461209703));
#62212=CARTESIAN_POINT('Ctrl Pts',(59.9157811143292,-4.74740824704905,333.707641220669));
#62213=CARTESIAN_POINT('Ctrl Pts',(59.9080239665553,-4.77979308485661,333.841224297607));
#62214=CARTESIAN_POINT('Ctrl Pts',(59.9002694187959,-4.81216706802442,333.974762600624));
#62215=CARTESIAN_POINT('Ctrl Pts',(59.8925148710364,-4.83895129421285,334.109702655429));
#62216=CARTESIAN_POINT('Ctrl Pts',(59.884760323277,-4.86003810017957,334.245538120709));
#62217=CARTESIAN_POINT('Ctrl Pts',(59.8770048338147,-4.88112746690225,334.381390081682));
#62218=CARTESIAN_POINT('Ctrl Pts',(59.8692493443525,-4.89651796439513,334.518137286886));
#62219=CARTESIAN_POINT('Ctrl Pts',(59.8614938548903,-4.90615334902285,334.655264770625));
#62220=CARTESIAN_POINT('Ctrl Pts',(59.8549350287631,-4.91430200459762,334.771233637256));
#62221=CARTESIAN_POINT('Ctrl Pts',(59.8483762026358,-4.91833541644559,334.887474215136));
#62222=CARTESIAN_POINT('Ctrl Pts',(59.8418173765087,-4.91824862818281,335.003673401407));
#62223=CARTESIAN_POINT('',(58.0918173765376,-4.9182497400553,335.001599045328));
#62224=CARTESIAN_POINT('Ctrl Pts',(59.841817376455,-4.9182486281821,335.003673402358));
#62225=CARTESIAN_POINT('Ctrl Pts',(59.8328697105503,-4.91813023007766,335.16219437501));
#62226=CARTESIAN_POINT('Ctrl Pts',(59.8239220446457,-4.91034393130489,335.320402619854));
#62227=CARTESIAN_POINT('Ctrl Pts',(59.8149743787411,-4.89500389926988,335.47761897851));
#62228=CARTESIAN_POINT('Ctrl Pts',(59.8059790090573,-4.87958208305695,335.635673523854));
#62229=CARTESIAN_POINT('Ctrl Pts',(59.7969836393734,-4.85652588434234,335.792725455033));
#62230=CARTESIAN_POINT('Ctrl Pts',(59.7879882696896,-4.82600062916286,335.948103891891));
#62231=CARTESIAN_POINT('Ctrl Pts',(59.7789342593916,-4.79527638052607,336.104495237312));
#62232=CARTESIAN_POINT('Ctrl Pts',(59.7698802490936,-4.75698546075449,336.259191077032));
#62233=CARTESIAN_POINT('Ctrl Pts',(59.7608262387955,-4.71134483422381,336.411528574111));
#62234=CARTESIAN_POINT('Ctrl Pts',(59.7559919441813,-4.6869754964648,336.492867595985));
#62235=CARTESIAN_POINT('Ctrl Pts',(59.7511576495671,-4.66051163143577,336.573534645542));
#62236=CARTESIAN_POINT('Ctrl Pts',(59.7463233549529,-4.63199173944947,336.653431458565));
#62237=CARTESIAN_POINT('Ctrl Pts',(59.7385482761745,-4.58612270898243,336.781930870572));
#62238=CARTESIAN_POINT('Ctrl Pts',(59.730773197396,-4.53482995317445,336.908723161525));
#62239=CARTESIAN_POINT('Ctrl Pts',(59.7229981186176,-4.47825935071902,337.033316564187));
#62240=CARTESIAN_POINT('Ctrl Pts',(59.7152326075686,-4.42175836199133,337.157756646736));
#62241=CARTESIAN_POINT('Ctrl Pts',(59.7074670965196,-4.35999260931081,337.280002872399));
#62242=CARTESIAN_POINT('Ctrl Pts',(59.6997015854705,-4.29315734170597,337.399579776097));
#62243=CARTESIAN_POINT('Ctrl Pts',(59.6919437739483,-4.22638834146355,337.519038118948));
#62244=CARTESIAN_POINT('Ctrl Pts',(59.6841859624261,-4.15456001867061,337.635832067799));
#62245=CARTESIAN_POINT('Ctrl Pts',(59.6764281509039,-4.07791504264166,337.749507586368));
#62246=CARTESIAN_POINT('Ctrl Pts',(59.6686761773809,-4.00132774438777,337.863097560505));
#62247=CARTESIAN_POINT('Ctrl Pts',(59.6609242038579,-3.91993122529002,337.973573452603));
#62248=CARTESIAN_POINT('Ctrl Pts',(59.6531722303349,-3.83401308530189,338.080507543285));
#62249=CARTESIAN_POINT('Ctrl Pts',(59.6454235397773,-3.74813133169705,338.187396347315));
#62250=CARTESIAN_POINT('Ctrl Pts',(59.6376748492196,-3.65773201013273,338.290746029164));
#62251=CARTESIAN_POINT('Ctrl Pts',(59.629926158662,-3.56314474203457,338.390159673203));
#62252=CARTESIAN_POINT('Ctrl Pts',(59.6221790802842,-3.46857715360755,338.489552633403));
#62253=CARTESIAN_POINT('Ctrl Pts',(59.6144320019064,-3.3698236210594,338.585010901694));
#62254=CARTESIAN_POINT('Ctrl Pts',(59.6066849235285,-3.26725230917648,338.676172657899));
#62255=CARTESIAN_POINT('Ctrl Pts',(59.5989377802227,-3.16468013764717,338.767335178126));
#62256=CARTESIAN_POINT('Ctrl Pts',(59.5911906369169,-3.05829041512443,338.854200854782));
#62257=CARTESIAN_POINT('Ctrl Pts',(59.5834434936111,-2.94848592568758,338.936446850717));
#62258=CARTESIAN_POINT('Ctrl Pts',(59.575694608583,-2.8386567498703,339.018711337298));
#62259=CARTESIAN_POINT('Ctrl Pts',(59.5679457235549,-2.72541159226266,339.096353842172));
#62260=CARTESIAN_POINT('Ctrl Pts',(59.5601968385268,-2.60918353253,339.169093949058));
#62261=CARTESIAN_POINT('Ctrl Pts',(59.552439728752,-2.49283210713396,339.241911263045));
#62262=CARTESIAN_POINT('Ctrl Pts',(59.5446826189773,-2.37349178692383,339.309815576962));
#62263=CARTESIAN_POINT('Ctrl Pts',(59.5369255092025,-2.25162213623948,339.372571419439));
#62264=CARTESIAN_POINT('Ctrl Pts',(59.5291642542764,-2.12968736231044,339.435360796632));
#62265=CARTESIAN_POINT('Ctrl Pts',(59.5214029993502,-2.00522091924836,339.492996056252));
#62266=CARTESIAN_POINT('Ctrl Pts',(59.513641744424,-1.87870290202377,339.545289701265));
#62267=CARTESIAN_POINT('Ctrl Pts',(59.5058680740194,-1.75198249720375,339.597666999067));
#62268=CARTESIAN_POINT('Ctrl Pts',(59.4980944036147,-1.6232043274728,339.644685473008));
#62269=CARTESIAN_POINT('Ctrl Pts',(59.49032073321,-1.49286506234389,339.686207098297));
#62270=CARTESIAN_POINT('Ctrl Pts',(59.482908929033,-1.36859312136543,339.725795881939));
#62271=CARTESIAN_POINT('Ctrl Pts',(59.475497124856,-1.2429024297093,339.760387980409));
#62272=CARTESIAN_POINT('Ctrl Pts',(59.4680853206789,-1.11623072592643,339.789907309019));
#62273=CARTESIAN_POINT('Ctrl Pts',(59.4603102419005,-0.983350464604767,
339.820873467859));
#62274=CARTESIAN_POINT('Ctrl Pts',(59.4525351631221,-0.848970668802507,
339.846354879191));
#62275=CARTESIAN_POINT('Ctrl Pts',(59.4447600843437,-0.713583819411007,
339.866208092054));
#62276=CARTESIAN_POINT('Ctrl Pts',(59.4369945732947,-0.578363572156741,
339.886036874275));
#62277=CARTESIAN_POINT('Ctrl Pts',(59.4292290622456,-0.442139120093809,
339.900251182325));
#62278=CARTESIAN_POINT('Ctrl Pts',(59.4214635511966,-0.305415952404884,
339.908757903841));
#62279=CARTESIAN_POINT('Ctrl Pts',(59.4137057396744,-0.168828346134968,
339.917256190917));
#62280=CARTESIAN_POINT('Ctrl Pts',(59.4059479281523,-0.0317433958850884,
339.920058129249));
#62281=CARTESIAN_POINT('Ctrl Pts',(59.3981901166301,0.105325767257696,339.917122079555));
#62282=CARTESIAN_POINT('Ctrl Pts',(59.3904381431071,0.242291781508595,339.914188239332));
#62283=CARTESIAN_POINT('Ctrl Pts',(59.3826861695841,0.379241643088397,339.905525014224));
#62284=CARTESIAN_POINT('Ctrl Pts',(59.3749341960611,0.515660036810762,339.89114278967));
#62285=CARTESIAN_POINT('Ctrl Pts',(59.3671855055035,0.652020657262393,339.876766655996));
#62286=CARTESIAN_POINT('Ctrl Pts',(59.3594368149458,0.787849869607818,339.856676380959));
#62287=CARTESIAN_POINT('Ctrl Pts',(59.3516881243882,0.922635521961498,339.830934356428));
#62288=CARTESIAN_POINT('Ctrl Pts',(59.3439410460104,1.05739313103445,339.80519768774));
#62289=CARTESIAN_POINT('Ctrl Pts',(59.3361939676326,1.19110722829154,339.773811681772));
#62290=CARTESIAN_POINT('Ctrl Pts',(59.3284468892547,1.32327431633506,339.73689013449));
#62291=CARTESIAN_POINT('Ctrl Pts',(59.3206997459489,1.45544251206599,339.699968277769));
#62292=CARTESIAN_POINT('Ctrl Pts',(59.3129526026431,1.58606329626199,339.657510892365));
#62293=CARTESIAN_POINT('Ctrl Pts',(59.3052054593373,1.71464721869942,339.609681982296));
#62294=CARTESIAN_POINT('Ctrl Pts',(59.2974565743092,1.84326004953243,339.561842319273));
#62295=CARTESIAN_POINT('Ctrl Pts',(59.2897076892811,1.96983474109831,339.508628864775));
#62296=CARTESIAN_POINT('Ctrl Pts',(59.281958804253,2.09390112110671,339.450254055391));
#62297=CARTESIAN_POINT('Ctrl Pts',(59.2742016944783,2.21809918645279,339.391817286382));
#62298=CARTESIAN_POINT('Ctrl Pts',(59.2664445847036,2.3397832677126,339.328208385713));
#62299=CARTESIAN_POINT('Ctrl Pts',(59.2586874749288,2.45850665535286,339.259686383771));
#62300=CARTESIAN_POINT('Ctrl Pts',(59.2509262200027,2.57729348497537,339.191127765863));
#62301=CARTESIAN_POINT('Ctrl Pts',(59.2431649650766,2.6931161386087,339.117651024608));
#62302=CARTESIAN_POINT('Ctrl Pts',(59.2354037101504,2.80555713905839,339.039558416706));
#62303=CARTESIAN_POINT('Ctrl Pts',(59.2276300397458,2.91817800846444,338.961340886081));
#62304=CARTESIAN_POINT('Ctrl Pts',(59.2198563693411,3.02740610322768,338.878492969962));
#62305=CARTESIAN_POINT('Ctrl Pts',(59.2120826989365,3.13285657898505,338.791357635203));
#62306=CARTESIAN_POINT('Ctrl Pts',(59.2046708947593,3.23339830972656,338.70827847124));
#62307=CARTESIAN_POINT('Ctrl Pts',(59.1972590905822,3.33050598870649,338.621302256508));
#62308=CARTESIAN_POINT('Ctrl Pts',(59.1898472864051,3.42387874924105,338.530755920904));
#62309=CARTESIAN_POINT('Ctrl Pts',(59.1820722076266,3.52182798691203,338.435771639668));
#62310=CARTESIAN_POINT('Ctrl Pts',(59.1742971288482,3.61597646754352,338.336558256306));
#62311=CARTESIAN_POINT('Ctrl Pts',(59.1665220500698,3.70593705049126,338.233452278958));
#62312=CARTESIAN_POINT('Ctrl Pts',(59.1587565390208,3.79578693121451,338.130473180079));
#62313=CARTESIAN_POINT('Ctrl Pts',(59.1509910279717,3.88145891367139,338.023611309821));
#62314=CARTESIAN_POINT('Ctrl Pts',(59.1432255169227,3.962601148487,337.913241356378));
#62315=CARTESIAN_POINT('Ctrl Pts',(59.1354677054005,4.04366293054049,337.802980835065));
#62316=CARTESIAN_POINT('Ctrl Pts',(59.1277098938783,4.12020367277377,337.689219465427));
#62317=CARTESIAN_POINT('Ctrl Pts',(59.1199520823561,4.19191067515202,337.572366216939));
#62318=CARTESIAN_POINT('Ctrl Pts',(59.1122001088331,4.26356371573701,337.455600904225));
#62319=CARTESIAN_POINT('Ctrl Pts',(59.1044481353101,4.33039005320381,337.335748675723));
#62320=CARTESIAN_POINT('Ctrl Pts',(59.0966961617871,4.39211955427367,337.213248491125));
#62321=CARTESIAN_POINT('Ctrl Pts',(59.0889474712295,4.45382291286317,337.090800185428));
#62322=CARTESIAN_POINT('Ctrl Pts',(59.0811987806718,4.51043355265627,336.965706502375));
#62323=CARTESIAN_POINT('Ctrl Pts',(59.0734500901142,4.56172678553355,336.838431885234));
#62324=CARTESIAN_POINT('Ctrl Pts',(59.0657030117364,4.61300934642532,336.71118374864));
#62325=CARTESIAN_POINT('Ctrl Pts',(59.0579559333585,4.65897655495544,336.581755942834));
#62326=CARTESIAN_POINT('Ctrl Pts',(59.0502088549807,4.69945163324512,336.450633451045));
#62327=CARTESIAN_POINT('Ctrl Pts',(59.0424617116749,4.73992705075491,336.319509860323));
#62328=CARTESIAN_POINT('Ctrl Pts',(59.0347145683691,4.77491013092729,336.186691928773));
#62329=CARTESIAN_POINT('Ctrl Pts',(59.0269674250633,4.80427391864021,336.052679997518));
#62330=CARTESIAN_POINT('Ctrl Pts',(59.0192185400352,4.83364430795601,335.918637937534));
#62331=CARTESIAN_POINT('Ctrl Pts',(59.0114696550071,4.85739280726976,335.783401725428));
#62332=CARTESIAN_POINT('Ctrl Pts',(59.003720769979,4.87544362183722,335.647481700735));
#62333=CARTESIAN_POINT('Ctrl Pts',(58.9959636602043,4.89351359572576,335.511417409124));
#62334=CARTESIAN_POINT('Ctrl Pts',(58.9882065504296,4.9058737527173,335.374668243146));
#62335=CARTESIAN_POINT('Ctrl Pts',(58.9804494406548,4.91250017683042,335.237750026585));
#62336=CARTESIAN_POINT('Ctrl Pts',(58.9726881857287,4.9191301418927,335.100758645306));
#62337=CARTESIAN_POINT('Ctrl Pts',(58.9649269308025,4.92002026639768,334.963598424111));
#62338=CARTESIAN_POINT('Ctrl Pts',(58.9571656758764,4.91519880358639,334.82678399692));
#62339=CARTESIAN_POINT('Ctrl Pts',(58.9493920054717,4.9103696280059,334.689750711234));
#62340=CARTESIAN_POINT('Ctrl Pts',(58.941618335067,4.8998106374413,334.553064714843));
#62341=CARTESIAN_POINT('Ctrl Pts',(58.9338446646624,4.88360197867112,334.417235230629));
#62342=CARTESIAN_POINT('Ctrl Pts',(58.9264328604853,4.86814783686622,334.287728641584));
#62343=CARTESIAN_POINT('Ctrl Pts',(58.9190210563082,4.84755821947558,334.159000902143));
#62344=CARTESIAN_POINT('Ctrl Pts',(58.9116092521311,4.82194523259748,334.031481938046));
#62345=CARTESIAN_POINT('Ctrl Pts',(58.9038341733526,4.79507687693537,333.89771288966));
#62346=CARTESIAN_POINT('Ctrl Pts',(58.8960590945742,4.76259537134975,333.764851369127));
#62347=CARTESIAN_POINT('Ctrl Pts',(58.8882840157958,4.7245741886985,333.633405035139));
#62348=CARTESIAN_POINT('Ctrl Pts',(58.8805185047467,4.68659979353305,333.502120454233));
#62349=CARTESIAN_POINT('Ctrl Pts',(58.8727529936978,4.64309939259957,333.372247966724));
#62350=CARTESIAN_POINT('Ctrl Pts',(58.8649874826488,4.59419766330899,333.244286215539));
#62351=CARTESIAN_POINT('Ctrl Pts',(58.8572296711266,4.54534442022537,333.116451338803));
#62352=CARTESIAN_POINT('Ctrl Pts',(58.8494718596044,4.49110064503393,332.990523790997));
#62353=CARTESIAN_POINT('Ctrl Pts',(58.8417140480822,4.4316410289586,332.8669878451));
#62354=CARTESIAN_POINT('Ctrl Pts',(58.8339620745592,4.37222615812998,332.74354486392));
#62355=CARTESIAN_POINT('Ctrl Pts',(58.8262101010361,4.30760342794561,332.622490253105));
#62356=CARTESIAN_POINT('Ctrl Pts',(58.8184581275131,4.23799578435709,332.504288719769));
#62357=CARTESIAN_POINT('Ctrl Pts',(58.8107094369555,4.16841761964691,332.386137244853));
#62358=CARTESIAN_POINT('Ctrl Pts',(58.8029607463979,4.09385893832118,332.270836780342));
#62359=CARTESIAN_POINT('Ctrl Pts',(58.7952120558402,4.0145887089974,332.158827608171));
#62360=CARTESIAN_POINT('Ctrl Pts',(58.7874649774624,3.93533497250691,332.046841740444));
#62361=CARTESIAN_POINT('Ctrl Pts',(58.7797178990845,3.8513718635168,331.938146121836));
#62362=CARTESIAN_POINT('Ctrl Pts',(58.7719708207067,3.76301155011732,331.83315186089));
#62363=CARTESIAN_POINT('Ctrl Pts',(58.7642236774009,3.67465049617336,331.728156719991));
#62364=CARTESIAN_POINT('Ctrl Pts',(58.7564765340951,3.58189241599727,331.62686329769));
#62365=CARTESIAN_POINT('Ctrl Pts',(58.7487293907893,3.48508935441027,331.529649116548));
#62366=CARTESIAN_POINT('Ctrl Pts',(58.7409805057612,3.38826452943997,331.432413079594));
#62367=CARTESIAN_POINT('Ctrl Pts',(58.7332316207331,3.28739318920863,331.339258385646));
#62368=CARTESIAN_POINT('Ctrl Pts',(58.725482735705,3.18286347223618,331.250524946129));
#62369=CARTESIAN_POINT('Ctrl Pts',(58.7177256259303,3.07822280634199,331.161697324021));
#62370=CARTESIAN_POINT('Ctrl Pts',(58.7099685161556,2.96991630542968,331.077300583939));
#62371=CARTESIAN_POINT('Ctrl Pts',(58.7022114063809,2.85836479441284,330.997633979187));
#62372=CARTESIAN_POINT('Ctrl Pts',(58.6944501514547,2.74675367383532,330.917924803148));
#62373=CARTESIAN_POINT('Ctrl Pts',(58.6866888965286,2.6318944150919,330.842951012521));
#62374=CARTESIAN_POINT('Ctrl Pts',(58.6789276416024,2.51423507427683,330.772967346498));
#62375=CARTESIAN_POINT('Ctrl Pts',(58.6711539711977,2.39638751686146,330.702871729416));
#62376=CARTESIAN_POINT('Ctrl Pts',(58.663380300793,2.27573127075965,330.63778237416));
#62377=CARTESIAN_POINT('Ctrl Pts',(58.6556066303884,2.15273792437585,330.577907453314));
#62378=CARTESIAN_POINT('Ctrl Pts',(58.6481948262113,2.03546994785687,330.520819724439));
#62379=CARTESIAN_POINT('Ctrl Pts',(58.6407830220342,1.9160778220735,330.468472006755));
#62380=CARTESIAN_POINT('Ctrl Pts',(58.6333712178572,1.7949837477944,330.421002685341));
#62381=CARTESIAN_POINT('Ctrl Pts',(58.6255961390787,1.66795449221406,330.37120675108));
#62382=CARTESIAN_POINT('Ctrl Pts',(58.6178210603003,1.53865079866103,330.326622149737));
#62383=CARTESIAN_POINT('Ctrl Pts',(58.6100459815219,1.40753932853812,330.287461819665));
#62384=CARTESIAN_POINT('Ctrl Pts',(58.6022804704729,1.27658919942616,330.248349678872));
#62385=CARTESIAN_POINT('Ctrl Pts',(58.5945149594238,1.14383609097412,330.214648638984));
#62386=CARTESIAN_POINT('Ctrl Pts',(58.5867494483748,1.00976679275898,330.186523700407));
#62387=CARTESIAN_POINT('Ctrl Pts',(58.5789916368526,0.875830424643447,330.158426647789));
#62388=CARTESIAN_POINT('Ctrl Pts',(58.5712338253304,0.740580843883713,330.135894773749));
#62389=CARTESIAN_POINT('Ctrl Pts',(58.5634760138082,0.604519821404695,330.119043244606));
#62390=CARTESIAN_POINT('Ctrl Pts',(58.5557240402852,0.468561189159927,330.102204396773));
#62391=CARTESIAN_POINT('Ctrl Pts',(58.5479720667622,0.331792716984758,330.091037433226));
#62392=CARTESIAN_POINT('Ctrl Pts',(58.5402200932392,0.194725835852015,330.085606353643));
#62393=CARTESIAN_POINT('Ctrl Pts',(58.5324714026816,0.057717002624715,330.080177574126));
#62394=CARTESIAN_POINT('Ctrl Pts',(58.524722712124,-0.0795895984514916,
330.080479862606));
#62395=CARTESIAN_POINT('Ctrl Pts',(58.5169740215664,-0.216678170552494,
330.086525299454));
#62396=CARTESIAN_POINT('Ctrl Pts',(58.5092269431886,-0.353738220231084,
330.092569478498));
#62397=CARTESIAN_POINT('Ctrl Pts',(58.5014798648107,-0.490579940914575,
330.10435441194));
#62398=CARTESIAN_POINT('Ctrl Pts',(58.4937327864329,-0.626688690592526,
330.121840065395));
#62399=CARTESIAN_POINT('Ctrl Pts',(58.4859856431271,-0.762798580992895,
330.139325865397));
#62400=CARTESIAN_POINT('Ctrl Pts',(58.4782384998213,-0.89817510044688,330.162512430901));
#62401=CARTESIAN_POINT('Ctrl Pts',(58.4704913565155,-1.03231027052626,330.191308019028));
#62402=CARTESIAN_POINT('Ctrl Pts',(58.4627424714874,-1.16647559703955,330.220110081014));
#62403=CARTESIAN_POINT('Ctrl Pts',(58.4549935864593,-1.29939863674428,330.2545235929));
#62404=CARTESIAN_POINT('Ctrl Pts',(58.4472447014312,-1.43058350684719,330.294406106299));
#62405=CARTESIAN_POINT('Ctrl Pts',(58.4394875916564,-1.56190761792671,330.33433095141));
#62406=CARTESIAN_POINT('Ctrl Pts',(58.4317304818817,-1.69148949945696,330.379736279902));
#62407=CARTESIAN_POINT('Ctrl Pts',(58.423973372107,-1.8188497704412,330.430430154263));
#62408=CARTESIAN_POINT('Ctrl Pts',(58.4162121171808,-1.94627809868206,330.48115111781));
#62409=CARTESIAN_POINT('Ctrl Pts',(58.4084508622546,-2.071482094245,330.537166098798));
#62410=CARTESIAN_POINT('Ctrl Pts',(58.4006896073285,-2.19400507264695,330.598236171295));
#62411=CARTESIAN_POINT('Ctrl Pts',(58.3929159369238,-2.31672404788412,330.659403936004));
#62412=CARTESIAN_POINT('Ctrl Pts',(58.3851422665192,-2.43675309335869,330.725642762484));
#62413=CARTESIAN_POINT('Ctrl Pts',(58.3773685961145,-2.5536619487584,330.796668736114));
#62414=CARTESIAN_POINT('Ctrl Pts',(58.3699567919374,-2.66512866881277,330.864388433584));
#62415=CARTESIAN_POINT('Ctrl Pts',(58.3625449877603,-2.77375891138264,330.936459465524));
#62416=CARTESIAN_POINT('Ctrl Pts',(58.3551331835832,-2.87920782844273,331.012601682408));
#62417=CARTESIAN_POINT('Ctrl Pts',(58.3474209354891,-2.98893120890391,331.091830390158));
#62418=CARTESIAN_POINT('Ctrl Pts',(58.3397086873949,-3.09556902993061,331.175726748648));
#62419=CARTESIAN_POINT('Ctrl Pts',(58.3319964393008,-3.19869354984864,331.264020525129));
#62420=CARTESIAN_POINT('Ctrl Pts',(58.3242937129603,-3.30169074939654,331.352205291684));
#62421=CARTESIAN_POINT('Ctrl Pts',(58.3165909866199,-3.40118297654752,331.444776421024));
#62422=CARTESIAN_POINT('Ctrl Pts',(58.3088882602795,-3.49677157664729,331.541420580173));
#62423=CARTESIAN_POINT('Ctrl Pts',(58.3011931263538,-3.59226595708197,331.637969479215));
#62424=CARTESIAN_POINT('Ctrl Pts',(58.2934979924281,-3.68386408741934,331.738583139987));
#62425=CARTESIAN_POINT('Ctrl Pts',(58.2858028585024,-3.77120087739879,331.842908457962));
#62426=CARTESIAN_POINT('Ctrl Pts',(58.2777201300872,-3.86293671473137,331.952488514679));
#62427=CARTESIAN_POINT('Ctrl Pts',(58.269637401672,-3.94997042934416,332.066163570637));
#62428=CARTESIAN_POINT('Ctrl Pts',(58.2615546732568,-4.03192290163398,332.18348073364));
#62429=CARTESIAN_POINT('Ctrl Pts',(58.2538683894613,-4.10985573908783,332.295043681521));
#62430=CARTESIAN_POINT('Ctrl Pts',(58.2461821056658,-4.18319365383043,332.409899603287));
#62431=CARTESIAN_POINT('Ctrl Pts',(58.2384958218702,-4.25165263303496,332.527626049622));
#62432=CARTESIAN_POINT('Ctrl Pts',(58.2308108083021,-4.32010029877827,332.645333040605));
#62433=CARTESIAN_POINT('Ctrl Pts',(58.223125794734,-4.38367043255201,332.765909268929));
#62434=CARTESIAN_POINT('Ctrl Pts',(58.2154407811659,-4.44212360917944,332.888905283207));
#62435=CARTESIAN_POINT('Ctrl Pts',(58.2077553068613,-4.50058029022692,333.011908671416));
#62436=CARTESIAN_POINT('Ctrl Pts',(58.2000698325566,-4.55391923342674,333.137331774642));
#62437=CARTESIAN_POINT('Ctrl Pts',(58.1923843582519,-4.60194825193857,333.264703094863));
#62438=CARTESIAN_POINT('Ctrl Pts',(58.1846966922218,-4.64999096725272,333.392110738537));
#62439=CARTESIAN_POINT('Ctrl Pts',(58.1770090261917,-4.6927206059285,333.52146733209));
#62440=CARTESIAN_POINT('Ctrl Pts',(58.1693213601616,-4.72999430503115,333.652284548997));
#62441=CARTESIAN_POINT('Ctrl Pts',(58.161625698353,-4.76730677171792,333.783237826117));
#62442=CARTESIAN_POINT('Ctrl Pts',(58.1539300365445,-4.79915186202804,333.915654376344));
#62443=CARTESIAN_POINT('Ctrl Pts',(58.1462343747359,-4.82543739887673,334.049033664096));
#62444=CARTESIAN_POINT('Ctrl Pts',(58.1385340507997,-4.85173885983083,334.182493754682));
#62445=CARTESIAN_POINT('Ctrl Pts',(58.1308337268634,-4.87247400025397,334.316917351973));
#62446=CARTESIAN_POINT('Ctrl Pts',(58.1231334029271,-4.88760246885154,334.45179824063));
#62447=CARTESIAN_POINT('Ctrl Pts',(58.1154224216085,-4.90275187551296,334.586865806785));
#62448=CARTESIAN_POINT('Ctrl Pts',(58.1077114402899,-4.9122790939977,334.722391532249));
#62449=CARTESIAN_POINT('Ctrl Pts',(58.1000004589713,-4.91619585075647,334.857868302251));
#62450=CARTESIAN_POINT('Ctrl Pts',(58.0972727648267,-4.91758137019104,334.905792058903));
#62451=CARTESIAN_POINT('Ctrl Pts',(58.0945450706822,-4.91826531006321,334.953709729097));
#62452=CARTESIAN_POINT('Ctrl Pts',(58.0918173765376,-4.9182497400553,335.001599045328));
#62453=CARTESIAN_POINT('',(56.3418173765458,-4.91824791469108,334.995470967337));
#62454=CARTESIAN_POINT('Ctrl Pts',(58.0918173765087,-4.91824974005514,335.001599045835));
#62455=CARTESIAN_POINT('Ctrl Pts',(58.0868433007755,-4.91822134742056,335.088927416654));
#62456=CARTESIAN_POINT('Ctrl Pts',(58.0818692250423,-4.91586720613331,335.176215108472));
#62457=CARTESIAN_POINT('Ctrl Pts',(58.0768951493091,-4.91119287755596,335.26337726163));
#62458=CARTESIAN_POINT('Ctrl Pts',(58.0691200705307,-4.90388633964328,335.39962219308));
#62459=CARTESIAN_POINT('Ctrl Pts',(58.0613449917522,-4.89089445730422,335.535778143507));
#62460=CARTESIAN_POINT('Ctrl Pts',(58.0535699129738,-4.87221676308775,335.671332165166));
#62461=CARTESIAN_POINT('Ctrl Pts',(58.0458044019248,-4.85356205296308,335.806719378972));
#62462=CARTESIAN_POINT('Ctrl Pts',(58.0380388908758,-4.82923550533785,335.941505754299));
#62463=CARTESIAN_POINT('Ctrl Pts',(58.0302733798268,-4.79928862213002,336.075179884481));
#62464=CARTESIAN_POINT('Ctrl Pts',(58.0225155683046,-4.76937143134412,336.208721476374));
#62465=CARTESIAN_POINT('Ctrl Pts',(58.0147577567824,-4.73384507962182,336.341152638782));
#62466=CARTESIAN_POINT('Ctrl Pts',(58.0069999452602,-4.69281263168756,336.471968976023));
#62467=CARTESIAN_POINT('Ctrl Pts',(57.9992479717372,-4.65181106197162,336.602686869821));
#62468=CARTESIAN_POINT('Ctrl Pts',(57.9914959982142,-4.60531176001444,336.731791985806));
#62469=CARTESIAN_POINT('Ctrl Pts',(57.9837440246912,-4.55346836156164,336.85879233449));
#62470=CARTESIAN_POINT('Ctrl Pts',(57.9759953341336,-4.5016469188188,336.98573889845));
#62471=CARTESIAN_POINT('Ctrl Pts',(57.9682466435759,-4.44448602840014,337.110582106852));
#62472=CARTESIAN_POINT('Ctrl Pts',(57.9604979530183,-4.38218838873212,337.232847506697));
#62473=CARTESIAN_POINT('Ctrl Pts',(57.9527508746405,-4.31990371060835,337.355087468204));
#62474=CARTESIAN_POINT('Ctrl Pts',(57.9450037962627,-4.25248458638428,337.474750339909));
#62475=CARTESIAN_POINT('Ctrl Pts',(57.9372567178848,-4.18018066785445,337.591384310865));
#62476=CARTESIAN_POINT('Ctrl Pts',(57.929509574579,-4.10787614334819,337.708019259325));
#62477=CARTESIAN_POINT('Ctrl Pts',(57.9217624312732,-4.03068694882805,337.821624924187));
#62478=CARTESIAN_POINT('Ctrl Pts',(57.9140152879674,-3.94890703743601,337.931776982001));
#62479=CARTESIAN_POINT('Ctrl Pts',(57.9062664029393,-3.86710874018376,338.041953804335));
#62480=CARTESIAN_POINT('Ctrl Pts',(57.8985175179112,-3.78071790526986,338.148675160808));
#62481=CARTESIAN_POINT('Ctrl Pts',(57.8907686328831,-3.69006962383433,338.251548743869));
#62482=CARTESIAN_POINT('Ctrl Pts',(57.8830115231084,-3.59932512737618,338.354531518014));
#62483=CARTESIAN_POINT('Ctrl Pts',(57.8752544133336,-3.50431441629685,338.453658066711));
#62484=CARTESIAN_POINT('Ctrl Pts',(57.8674973035589,-3.40541078719704,338.548571604596));
#62485=CARTESIAN_POINT('Ctrl Pts',(57.8597360486327,-3.30645430716023,338.64353586124));
#62486=CARTESIAN_POINT('Ctrl Pts',(57.8519747937065,-3.20360105696828,338.734282362688));
#62487=CARTESIAN_POINT('Ctrl Pts',(57.8442135387804,-3.09725769623202,338.820494447795));
#62488=CARTESIAN_POINT('Ctrl Pts',(57.8364398683757,-2.99074422077581,338.906844444141));
#62489=CARTESIAN_POINT('Ctrl Pts',(57.8286661979711,-2.88072979204245,338.98864529598));
#62490=CARTESIAN_POINT('Ctrl Pts',(57.8208925275664,-2.76765106825078,339.065623030596));
#62491=CARTESIAN_POINT('Ctrl Pts',(57.8134807233894,-2.65983618625762,339.139017433145));
#62492=CARTESIAN_POINT('Ctrl Pts',(57.8060689192124,-2.54923611906024,339.208027493147));
#62493=CARTESIAN_POINT('Ctrl Pts',(57.7986571150353,-2.43624871202379,339.272455415293));
#62494=CARTESIAN_POINT('Ctrl Pts',(57.7908820362569,-2.31772345559552,339.340041141824));
#62495=CARTESIAN_POINT('Ctrl Pts',(57.7831069574784,-2.19619635911406,339.402797788198));
#62496=CARTESIAN_POINT('Ctrl Pts',(57.7753318787,-2.07209851831654,339.460447375868));
#62497=CARTESIAN_POINT('Ctrl Pts',(57.767566367651,-1.94815338781258,339.518026022051));
#62498=CARTESIAN_POINT('Ctrl Pts',(57.759800856602,-1.82164415848191,339.570509950898));
#62499=CARTESIAN_POINT('Ctrl Pts',(57.752035345553,-1.69302875374377,339.617665719982));
#62500=CARTESIAN_POINT('Ctrl Pts',(57.7442775340308,-1.56454087155396,339.664774733983));
#62501=CARTESIAN_POINT('Ctrl Pts',(57.7365197225086,-1.43395133437161,339.706565967776));
#62502=CARTESIAN_POINT('Ctrl Pts',(57.7287619109864,-1.30174007352346,339.74285313324));
#62503=CARTESIAN_POINT('Ctrl Pts',(57.7210099374634,-1.16962830584176,339.779112991461));
#62504=CARTESIAN_POINT('Ctrl Pts',(57.7132579639404,-1.03589761905483,339.809876922736));
#62505=CARTESIAN_POINT('Ctrl Pts',(57.7055059904174,-0.901044878736802,
339.835007878898));
#62506=CARTESIAN_POINT('Ctrl Pts',(57.6977572998598,-0.766249248634269,
339.860128192085));
#62507=CARTESIAN_POINT('Ctrl Pts',(57.6900086093022,-0.630332893579719,
339.879620203426));
#62508=CARTESIAN_POINT('Ctrl Pts',(57.6822599187446,-0.493804482970295,
339.89339761261));
#62509=CARTESIAN_POINT('Ctrl Pts',(57.6745128403667,-0.357304478237098,
339.90717215529));
#62510=CARTESIAN_POINT('Ctrl Pts',(57.6667657619889,-0.220193059898798,
339.91523442154));
#62511=CARTESIAN_POINT('Ctrl Pts',(57.6590186836111,-0.0829852663312264,
339.917549848052));
#62512=CARTESIAN_POINT('Ctrl Pts',(57.6512715403053,0.0542236771699033,
339.919865293969));
#62513=CARTESIAN_POINT('Ctrl Pts',(57.6435243969995,0.19152860669271,339.916433797486));
#62514=CARTESIAN_POINT('Ctrl Pts',(57.6357772536937,0.328413624683528,339.907272924306));
#62515=CARTESIAN_POINT('Ctrl Pts',(57.6280283686656,0.465329417332357,339.898109991566));
#62516=CARTESIAN_POINT('Ctrl Pts',(57.6202794836375,0.601824720668057,339.883215145077));
#62517=CARTESIAN_POINT('Ctrl Pts',(57.6125305986095,0.737388297857424,339.862657870001));
#62518=CARTESIAN_POINT('Ctrl Pts',(57.6047734888347,0.873095763628347,339.842078775221));
#62519=CARTESIAN_POINT('Ctrl Pts',(57.59701637906,1.00786914067846,339.81582530469));
#62520=CARTESIAN_POINT('Ctrl Pts',(57.5892592692853,1.14120638837211,339.784018294451));
#62521=CARTESIAN_POINT('Ctrl Pts',(57.5814980143591,1.27461488722762,339.752194287562));
#62522=CARTESIAN_POINT('Ctrl Pts',(57.5737367594329,1.40658535168398,339.714810934165));
#62523=CARTESIAN_POINT('Ctrl Pts',(57.5659755045068,1.53663142777966,339.672038839485));
#62524=CARTESIAN_POINT('Ctrl Pts',(57.5582018341021,1.66688553521517,339.629198323394));
#62525=CARTESIAN_POINT('Ctrl Pts',(57.5504281636975,1.79520873668472,339.580951977879));
#62526=CARTESIAN_POINT('Ctrl Pts',(57.5426544932928,1.92113434187087,339.527518735796));
#62527=CARTESIAN_POINT('Ctrl Pts',(57.5352426891157,2.04119807984042,339.476572823987));
#62528=CARTESIAN_POINT('Ctrl Pts',(57.5278308849385,2.15908215415359,339.420912171195));
#62529=CARTESIAN_POINT('Ctrl Pts',(57.5204190807614,2.27440493756041,339.360764295683));
#62530=CARTESIAN_POINT('Ctrl Pts',(57.512644001983,2.39538003411008,339.297668393621));
#62531=CARTESIAN_POINT('Ctrl Pts',(57.5048689232046,2.51391872203002,339.229434887852));
#62532=CARTESIAN_POINT('Ctrl Pts',(57.4970938444261,2.62955395258996,339.156275865835));
#62533=CARTESIAN_POINT('Ctrl Pts',(57.4893283333771,2.74504688663707,339.083206870652));
#62534=CARTESIAN_POINT('Ctrl Pts',(57.4815628223281,2.85764314518981,339.005224626178));
#62535=CARTESIAN_POINT('Ctrl Pts',(57.4737973112791,2.96689861289058,338.922587880893));
#62536=CARTESIAN_POINT('Ctrl Pts',(57.4660394997569,3.07604575347703,338.840033070181));
#62537=CARTESIAN_POINT('Ctrl Pts',(57.4582816882347,3.18185838534588,338.752833176945));
#62538=CARTESIAN_POINT('Ctrl Pts',(57.4505238767125,3.28392013646286,338.661290974483));
#62539=CARTESIAN_POINT('Ctrl Pts',(57.4427719031895,3.38590508287556,338.569817660433));
#62540=CARTESIAN_POINT('Ctrl Pts',(57.4350199296665,3.48414447708982,338.474008801341));
#62541=CARTESIAN_POINT('Ctrl Pts',(57.4272679561435,3.57825418990664,338.374208057443));
#62542=CARTESIAN_POINT('Ctrl Pts',(57.4195192655859,3.67232404720414,338.27444957922));
#62543=CARTESIAN_POINT('Ctrl Pts',(57.4117705750282,3.76226743398327,338.170702862394));
#62544=CARTESIAN_POINT('Ctrl Pts',(57.4040218844706,3.847736508274,338.063348955864));
#62545=CARTESIAN_POINT('Ctrl Pts',(57.3962748060928,3.93318780000991,337.956017385211));
#62546=CARTESIAN_POINT('Ctrl Pts',(57.388527727715,4.0141663876148,337.845080423267));
#62547=CARTESIAN_POINT('Ctrl Pts',(57.3807806493371,4.09036448924706,337.730952472601));
#62548=CARTESIAN_POINT('Ctrl Pts',(57.3730335060313,4.16656322949281,337.616823565433));
#62549=CARTESIAN_POINT('Ctrl Pts',(57.3652863627255,4.2379811868127,337.499503941279));
#62550=CARTESIAN_POINT('Ctrl Pts',(57.3575392194197,4.30435395081173,337.379436935208));
#62551=CARTESIAN_POINT('Ctrl Pts',(57.3497903343917,4.37074163681724,337.259342935525));
#62552=CARTESIAN_POINT('Ctrl Pts',(57.3420414493635,4.43208168337109,337.136500666849));
#62553=CARTESIAN_POINT('Ctrl Pts',(57.3342925643354,4.48815586244286,337.011377641548));
#62554=CARTESIAN_POINT('Ctrl Pts',(57.3265354545607,4.54428955922765,336.886121809376));
#62555=CARTESIAN_POINT('Ctrl Pts',(57.318778344786,4.59514606338159,336.758580742022));
#62556=CARTESIAN_POINT('Ctrl Pts',(57.3110212350113,4.64055530551533,336.629242007485));
#62557=CARTESIAN_POINT('Ctrl Pts',(57.3032599800851,4.68598881289616,336.499834158463));
#62558=CARTESIAN_POINT('Ctrl Pts',(57.2954987251589,4.72596914426627,336.368627101856));
#62559=CARTESIAN_POINT('Ctrl Pts',(57.2877374702328,4.76037657116539,336.236122147362));
#62560=CARTESIAN_POINT('Ctrl Pts',(57.2799637998281,4.7948390387342,336.103405228125));
#62561=CARTESIAN_POINT('Ctrl Pts',(57.2721901294235,4.82371070499877,335.969386644421));
#62562=CARTESIAN_POINT('Ctrl Pts',(57.2644164590188,4.84692312235904,335.834577323225));
#62563=CARTESIAN_POINT('Ctrl Pts',(57.2570046548417,4.86905499610667,335.706043408364));
#62564=CARTESIAN_POINT('Ctrl Pts',(57.2495928506646,4.88604260250294,335.576791002294));
#62565=CARTESIAN_POINT('Ctrl Pts',(57.2421810464875,4.89787074610759,335.4472641467));
#62566=CARTESIAN_POINT('Ctrl Pts',(57.2344059677091,4.9102786222645,335.311388794073));
#62567=CARTESIAN_POINT('Ctrl Pts',(57.2266308889306,4.91704769734693,335.17478201728));
#62568=CARTESIAN_POINT('Ctrl Pts',(57.2188558101522,4.9181035733576,335.037951340255));
#62569=CARTESIAN_POINT('Ctrl Pts',(57.2110902991032,4.91915815004562,334.90128904209));
#62570=CARTESIAN_POINT('Ctrl Pts',(57.2033247880542,4.91451351326451,334.764403779032));
#62571=CARTESIAN_POINT('Ctrl Pts',(57.1955592770051,4.90414691382683,334.62780904081));
#62572=CARTESIAN_POINT('Ctrl Pts',(57.1878014654829,4.89379059290269,334.491349736669));
#62573=CARTESIAN_POINT('Ctrl Pts',(57.1800436539608,4.87772362898367,334.355180771358));
#62574=CARTESIAN_POINT('Ctrl Pts',(57.1722858424386,4.85597530779821,334.219816129009));
#62575=CARTESIAN_POINT('Ctrl Pts',(57.1645338689155,4.83424335291412,334.084553352847));
#62576=CARTESIAN_POINT('Ctrl Pts',(57.1567818953925,4.80683861249617,333.950094079241));
#62577=CARTESIAN_POINT('Ctrl Pts',(57.1490299218695,4.77384220341668,333.816947304902));
#62578=CARTESIAN_POINT('Ctrl Pts',(57.1412812313119,4.74085976833602,333.683856918302));
#62579=CARTESIAN_POINT('Ctrl Pts',(57.1335325407543,4.70229046835472,333.552078304041));
#62580=CARTESIAN_POINT('Ctrl Pts',(57.1257838501967,4.6582664983716,333.422110177278));
#62581=CARTESIAN_POINT('Ctrl Pts',(57.1180367718188,4.61425168794314,333.29216909147));
#62582=CARTESIAN_POINT('Ctrl Pts',(57.110289693441,4.56478459021156,333.164038113881));
#62583=CARTESIAN_POINT('Ctrl Pts',(57.1025426150632,4.51004712672267,333.038200321837));
#62584=CARTESIAN_POINT('Ctrl Pts',(57.0947954717574,4.45530920448116,332.912361475151));
#62585=CARTESIAN_POINT('Ctrl Pts',(57.0870483284516,4.39530098429308,332.788816210778));
#62586=CARTESIAN_POINT('Ctrl Pts',(57.0793011851458,4.33025218843889,332.668026791102));
#62587=CARTESIAN_POINT('Ctrl Pts',(57.0715523001177,4.26518876823442,332.5472102154));
#62588=CARTESIAN_POINT('Ctrl Pts',(57.0638034150896,4.19508270266151,332.429151061352));
#62589=CARTESIAN_POINT('Ctrl Pts',(57.0560545300615,4.12020903713502,332.314285839332));
#62590=CARTESIAN_POINT('Ctrl Pts',(57.0482974202868,4.04525589992625,332.199298698179));
#62591=CARTESIAN_POINT('Ctrl Pts',(57.0405403105121,3.96552526796268,332.08751258901));
#62592=CARTESIAN_POINT('Ctrl Pts',(57.0327832007373,3.88133511326965,331.979334377823));
#62593=CARTESIAN_POINT('Ctrl Pts',(57.0250219458112,3.7970999700499,331.871098359659));
#62594=CARTESIAN_POINT('Ctrl Pts',(57.017260690885,3.70840080834417,331.766474379077));
#62595=CARTESIAN_POINT('Ctrl Pts',(57.0094994359588,3.61559439823423,331.665834405739));
#62596=CARTESIAN_POINT('Ctrl Pts',(57.0017257655541,3.52263952811359,331.565033441241));
#62597=CARTESIAN_POINT('Ctrl Pts',(56.9939520951495,3.42556455718725,331.468229495502));
#62598=CARTESIAN_POINT('Ctrl Pts',(56.9861784247448,3.32476209392481,331.375756619472));
#62599=CARTESIAN_POINT('Ctrl Pts',(56.9787666205677,3.22865200957877,331.287588378069));
#62600=CARTESIAN_POINT('Ctrl Pts',(56.9713548163906,3.12915387240548,331.20335724401));
#62601=CARTESIAN_POINT('Ctrl Pts',(56.9639430122135,3.0266328634056,331.123316291899));
#62602=CARTESIAN_POINT('Ctrl Pts',(56.9561679334351,2.91908699436039,331.039352294296));
#62603=CARTESIAN_POINT('Ctrl Pts',(56.9483928546567,2.80787457631343,330.959734269229));
#62604=CARTESIAN_POINT('Ctrl Pts',(56.9406177758782,2.69338213594443,330.884799429885));
#62605=CARTESIAN_POINT('Ctrl Pts',(56.9328522648292,2.57903058581233,330.809956802631));
#62606=CARTESIAN_POINT('Ctrl Pts',(56.9250867537802,2.46140736831671,330.739786106474));
#62607=CARTESIAN_POINT('Ctrl Pts',(56.9173212427312,2.34093197703384,330.674584350447));
#62608=CARTESIAN_POINT('Ctrl Pts',(56.909563431209,2.22057603745219,330.60944724215));
#62609=CARTESIAN_POINT('Ctrl Pts',(56.9018056196868,2.09737389338583,330.54926945438));
#62610=CARTESIAN_POINT('Ctrl Pts',(56.8940478081646,1.97177361324516,330.494304506449));
#62611=CARTESIAN_POINT('Ctrl Pts',(56.8862958346416,1.84626785129832,330.439380921384));
#62612=CARTESIAN_POINT('Ctrl Pts',(56.8785438611186,1.71836790203643,330.389662524036));
#62613=CARTESIAN_POINT('Ctrl Pts',(56.8707918875955,1.5885456886467,330.345356548823));
#62614=CARTESIAN_POINT('Ctrl Pts',(56.8630431970379,1.45877845504142,330.301069337218));
#62615=CARTESIAN_POINT('Ctrl Pts',(56.8552945064803,1.32709094561055,330.26219011478));
#62616=CARTESIAN_POINT('Ctrl Pts',(56.8475458159227,1.19397407881431,330.228877599388));
#62617=CARTESIAN_POINT('Ctrl Pts',(56.8397987375448,1.06088490809403,330.195572014943));
#62618=CARTESIAN_POINT('Ctrl Pts',(56.832051659167,0.926367350480988,330.167830928633));
#62619=CARTESIAN_POINT('Ctrl Pts',(56.8243045807892,0.790926084190972,330.145762779607));
#62620=CARTESIAN_POINT('Ctrl Pts',(56.8165574374834,0.655483682772783,330.123694445629));
#62621=CARTESIAN_POINT('Ctrl Pts',(56.8088102941776,0.519117943023406,330.107299206626));
#62622=CARTESIAN_POINT('Ctrl Pts',(56.8010631508718,0.382341907152689,330.096634040933));
#62623=CARTESIAN_POINT('Ctrl Pts',(56.7933142658437,0.245535121125271,330.085966477484));
#62624=CARTESIAN_POINT('Ctrl Pts',(56.7855653808156,0.108318245037932,330.081031581184));
#62625=CARTESIAN_POINT('Ctrl Pts',(56.7778164957875,-0.0287928073667623,
330.081834281285));
#62626=CARTESIAN_POINT('Ctrl Pts',(56.7700593860127,-0.166049390859194,
330.08263783338));
#62627=CARTESIAN_POINT('Ctrl Pts',(56.762302276238,-0.303199534809589,330.08919114482));
#62628=CARTESIAN_POINT('Ctrl Pts',(56.7545451664633,-0.439729024012318,
330.101447004682));
#62629=CARTESIAN_POINT('Ctrl Pts',(56.7467839115371,-0.576331470208617,
330.113709413683));
#62630=CARTESIAN_POINT('Ctrl Pts',(56.7390226566109,-0.712312213490378,
330.13168039186));
#62631=CARTESIAN_POINT('Ctrl Pts',(56.7312614016848,-0.84716538787191,330.155261217765));
#62632=CARTESIAN_POINT('Ctrl Pts',(56.7234877312801,-0.982234283383906,
330.178879765307));
#62633=CARTESIAN_POINT('Ctrl Pts',(56.7157140608755,-1.11617162350625,330.208126009714));
#62634=CARTESIAN_POINT('Ctrl Pts',(56.7079403904708,-1.24848403469736,330.242850572285));
#62635=CARTESIAN_POINT('Ctrl Pts',(56.7005285862938,-1.37463727131428,330.275958698115));
#62636=CARTESIAN_POINT('Ctrl Pts',(56.6931167821167,-1.49931318016239,330.314046504542));
#62637=CARTESIAN_POINT('Ctrl Pts',(56.6857049779397,-1.62210132501434,330.356943856264));
#62638=CARTESIAN_POINT('Ctrl Pts',(56.6779298991612,-1.75090768261332,330.401943734978));
#62639=CARTESIAN_POINT('Ctrl Pts',(56.6701548203828,-1.87804359924059,330.452378748082));
#62640=CARTESIAN_POINT('Ctrl Pts',(56.6623797416044,-2.00301633336829,330.508106342448));
#62641=CARTESIAN_POINT('Ctrl Pts',(56.6546142305554,-2.12783528059057,330.563765360461));
#62642=CARTESIAN_POINT('Ctrl Pts',(56.6468487195063,-2.25049598822098,330.62470384335));
#62643=CARTESIAN_POINT('Ctrl Pts',(56.6390832084573,-2.37052168298279,330.690729758647));
#62644=CARTESIAN_POINT('Ctrl Pts',(56.6313253969351,-2.4904283719188,330.756690209057));
#62645=CARTESIAN_POINT('Ctrl Pts',(56.6235675854129,-2.60770490698363,330.827727866442));
#62646=CARTESIAN_POINT('Ctrl Pts',(56.6158097738907,-2.72189562285166,330.903603134363));
#62647=CARTESIAN_POINT('Ctrl Pts',(56.6080578003677,-2.8360004065848,330.979421303739));
#62648=CARTESIAN_POINT('Ctrl Pts',(56.6003058268446,-2.94702366905328,331.060069622053));
#62649=CARTESIAN_POINT('Ctrl Pts',(56.5925538533216,-3.05453575769835,331.145263385464));
#62650=CARTESIAN_POINT('Ctrl Pts',(56.584805162764,-3.16200231491004,331.230421069266));
#62651=CARTESIAN_POINT('Ctrl Pts',(56.5770564722064,-3.26596035009034,331.320120127226));
#62652=CARTESIAN_POINT('Ctrl Pts',(56.5693077816487,-3.36601072984262,331.414033626889));
#62653=CARTESIAN_POINT('Ctrl Pts',(56.5615607032709,-3.46604029327769,331.507927587063));
#62654=CARTESIAN_POINT('Ctrl Pts',(56.553813624893,-3.56216353362662,331.606033977481));
#62655=CARTESIAN_POINT('Ctrl Pts',(56.5460665465152,-3.65401615175325,331.707987086109));
#62656=CARTESIAN_POINT('Ctrl Pts',(56.5383194032094,-3.74586953969322,331.809941049202));
#62657=CARTESIAN_POINT('Ctrl Pts',(56.5305722599036,-3.83345197239091,331.91574150441));
#62658=CARTESIAN_POINT('Ctrl Pts',(56.5228251165978,-3.91643789897057,332.024987857839));
#62659=CARTESIAN_POINT('Ctrl Pts',(56.5150762315697,-3.99944248254826,332.134258772167));
#62660=CARTESIAN_POINT('Ctrl Pts',(56.5073273465416,-4.07784826728229,332.24697681511));
#62661=CARTESIAN_POINT('Ctrl Pts',(56.4995784615135,-4.15137191752904,332.362710811297));
#62662=CARTESIAN_POINT('Ctrl Pts',(56.4918213517388,-4.22497360653796,332.478567648743));
#62663=CARTESIAN_POINT('Ctrl Pts',(56.484064241964,-4.29368259970469,332.59744650361));
#62664=CARTESIAN_POINT('Ctrl Pts',(56.4763071321892,-4.35726032634769,332.718889412822));
#62665=CARTESIAN_POINT('Ctrl Pts',(56.4685458772631,-4.42087202689499,332.840397217241));
#62666=CARTESIAN_POINT('Ctrl Pts',(56.4607846223369,-4.47934683071558,332.964471452755));
#62667=CARTESIAN_POINT('Ctrl Pts',(56.4530233674108,-4.53249400166833,333.090633302024));
#62668=CARTESIAN_POINT('Ctrl Pts',(56.4452496970061,-4.58572619077395,333.216996969135));
#62669=CARTESIAN_POINT('Ctrl Pts',(56.4374760266014,-4.63361357997391,333.34545455687));
#62670=CARTESIAN_POINT('Ctrl Pts',(56.4297023561968,-4.67601479227158,333.475510339505));
#62671=CARTESIAN_POINT('Ctrl Pts',(56.4222905520197,-4.71644221793553,333.599511994168));
#62672=CARTESIAN_POINT('Ctrl Pts',(56.4148787478426,-4.75188265712274,333.724966123298));
#62673=CARTESIAN_POINT('Ctrl Pts',(56.4074669436656,-4.78225706964697,333.851435512341));
#62674=CARTESIAN_POINT('Ctrl Pts',(56.3965253491456,-4.82709696256397,334.038134559028));
#62675=CARTESIAN_POINT('Ctrl Pts',(56.3855837546257,-4.8610201363199,334.227549293209));
#62676=CARTESIAN_POINT('Ctrl Pts',(56.3746421601057,-4.88376345013037,334.41858996769));
#62677=CARTESIAN_POINT('Ctrl Pts',(56.3644648444204,-4.90491812589157,334.596286303392));
#62678=CARTESIAN_POINT('Ctrl Pts',(56.354287528735,-4.91640065640646,334.775389583627));
#62679=CARTESIAN_POINT('Ctrl Pts',(56.3441102130496,-4.91804411929726,334.954998853952));
#62680=CARTESIAN_POINT('Ctrl Pts',(56.343345934215,-4.9181675372929,334.968486847059));
#62681=CARTESIAN_POINT('Ctrl Pts',(56.3425816553804,-4.91823548922244,334.981977680854));
#62682=CARTESIAN_POINT('Ctrl Pts',(56.3418173765457,-4.91824791469108,334.995470967337));
#62683=CARTESIAN_POINT('',(54.5918173764761,-4.91824995138137,335.000691546911));
#62684=CARTESIAN_POINT('Ctrl Pts',(56.3418173765086,-4.91824791469168,334.995470967994));
#62685=CARTESIAN_POINT('Ctrl Pts',(56.3341582515252,-4.91837243495727,335.130692254957));
#62686=CARTESIAN_POINT('Ctrl Pts',(56.3264991265419,-4.91291614338096,335.266068753081));
#62687=CARTESIAN_POINT('Ctrl Pts',(56.3188400015585,-4.90186747110353,335.401096445057));
#62688=CARTESIAN_POINT('Ctrl Pts',(56.3109395393849,-4.89047065781402,335.540378827203));
#62689=CARTESIAN_POINT('Ctrl Pts',(56.3030390772113,-4.87312317390013,335.679289627408));
#62690=CARTESIAN_POINT('Ctrl Pts',(56.2951386150377,-4.84987048605147,335.817275553915));
#62691=CARTESIAN_POINT('Ctrl Pts',(56.2874875112519,-4.82735171131172,335.950906298734));
#62692=CARTESIAN_POINT('Ctrl Pts',(56.2798364074662,-4.79929494347988,336.083669245075));
#62693=CARTESIAN_POINT('Ctrl Pts',(56.2721853036804,-4.76579405557933,336.215067933206));
#62694=CARTESIAN_POINT('Ctrl Pts',(56.2645351706831,-4.73229741834303,336.34644994919));
#62695=CARTESIAN_POINT('Ctrl Pts',(56.2568850376858,-4.69335813369513,336.476467662015));
#62696=CARTESIAN_POINT('Ctrl Pts',(56.2492349046884,-4.64912076540291,336.604636772357));
#62697=CARTESIAN_POINT('Ctrl Pts',(56.2415839872594,-4.60487886108559,336.732819024943));
#62698=CARTESIAN_POINT('Ctrl Pts',(56.2339330698303,-4.55533792414488,336.859151918501));
#62699=CARTESIAN_POINT('Ctrl Pts',(56.2262821524012,-4.50069158786027,336.983168750627));
#62700=CARTESIAN_POINT('Ctrl Pts',(56.21862869494,-4.44602710950884,337.107226755168));
#62701=CARTESIAN_POINT('Ctrl Pts',(56.2109752374786,-4.38625402331418,337.228966802032));
#62702=CARTESIAN_POINT('Ctrl Pts',(56.2033217800173,-4.32161281349888,337.34794500632));
#62703=CARTESIAN_POINT('Ctrl Pts',(56.1956599813704,-4.25690115391134,337.467052880015));
#62704=CARTESIAN_POINT('Ctrl Pts',(56.1879981827234,-4.1873109740053,337.583392551033));
#62705=CARTESIAN_POINT('Ctrl Pts',(56.1803363840764,-4.11312728368153,337.696547238736));
#62706=CARTESIAN_POINT('Ctrl Pts',(56.1726695744164,-4.03889507532004,337.809775932509));
#62707=CARTESIAN_POINT('Ctrl Pts',(56.1650027647564,-3.96006360955949,337.919815171335));
#62708=CARTESIAN_POINT('Ctrl Pts',(56.1573359550964,-3.87695858740802,338.026280749373));
#62709=CARTESIAN_POINT('Ctrl Pts',(56.1496584941899,-3.79373811018218,338.132894236537));
#62710=CARTESIAN_POINT('Ctrl Pts',(56.1419810332834,-3.7062324894227,338.235923852889));
#62711=CARTESIAN_POINT('Ctrl Pts',(56.1343035723768,-3.61480482110838,338.335021614292));
#62712=CARTESIAN_POINT('Ctrl Pts',(56.1326120180485,-3.59466080866041,338.356855557736));
#62713=CARTESIAN_POINT('Ctrl Pts',(56.1309204637201,-3.57432653234455,338.378498786957));
#62714=CARTESIAN_POINT('Ctrl Pts',(56.1292289093917,-3.55380608746057,338.399947845957));
#62715=CARTESIAN_POINT('Ctrl Pts',(56.1214538306133,-3.45948569061267,338.498536534865));
#62716=CARTESIAN_POINT('Ctrl Pts',(56.1136787518349,-3.36091061132691,338.593353124064));
#62717=CARTESIAN_POINT('Ctrl Pts',(56.1059036730564,-3.25841473465418,338.68400820839));
#62718=CARTESIAN_POINT('Ctrl Pts',(56.0981381620074,-3.1560449856829,338.774551735864));
#62719=CARTESIAN_POINT('Ctrl Pts',(56.0903726509584,-3.04976432925985,338.860943691297));
#62720=CARTESIAN_POINT('Ctrl Pts',(56.0826071399094,-2.9399450680366,338.942829702058));
#62721=CARTESIAN_POINT('Ctrl Pts',(56.0748493283872,-2.83023469293087,339.0246345226));
#62722=CARTESIAN_POINT('Ctrl Pts',(56.067091516865,-2.71699300654682,339.101942057215));
#62723=CARTESIAN_POINT('Ctrl Pts',(56.0593337053428,-2.60062685651415,339.174436850124));
#62724=CARTESIAN_POINT('Ctrl Pts',(56.0515817318198,-2.4843482756998,339.246877088403));
#62725=CARTESIAN_POINT('Ctrl Pts',(56.0438297582968,-2.36495024172537,339.314511588024));
#62726=CARTESIAN_POINT('Ctrl Pts',(56.0360777847739,-2.24286987932212,339.377067256386));
#62727=CARTESIAN_POINT('Ctrl Pts',(56.0283290942162,-2.12084121802434,339.439596432386));
#62728=CARTESIAN_POINT('Ctrl Pts',(56.0205804036586,-1.99613283479763,339.497050877214));
#62729=CARTESIAN_POINT('Ctrl Pts',(56.012831713101,-1.86920764438197,339.549202770232));
#62730=CARTESIAN_POINT('Ctrl Pts',(56.0050846347231,-1.74230886181227,339.601343812613));
#62731=CARTESIAN_POINT('Ctrl Pts',(55.9973375563453,-1.61319455078081,339.648184349146));
#62732=CARTESIAN_POINT('Ctrl Pts',(55.9895904779675,-1.48234848918881,339.68954432958));
#62733=CARTESIAN_POINT('Ctrl Pts',(55.9818433346616,-1.35150133098089,339.730904656651));
#62734=CARTESIAN_POINT('Ctrl Pts',(55.9740961913558,-1.21892276596177,339.766784218199));
#62735=CARTESIAN_POINT('Ctrl Pts',(55.96634904805,-1.0851122661618,339.797052681838));
#62736=CARTESIAN_POINT('Ctrl Pts',(55.9586001630219,-0.951271682920421,
339.82732795047));
#62737=CARTESIAN_POINT('Ctrl Pts',(55.9508512779938,-0.816198994936311,
339.85198952474));
#62738=CARTESIAN_POINT('Ctrl Pts',(55.9431023929657,-0.680404018054023,
339.870958163926));
#62739=CARTESIAN_POINT('Ctrl Pts',(55.935345283191,-0.544464906980432,339.889946936622));
#62740=CARTESIAN_POINT('Ctrl Pts',(55.9275881734162,-0.407802363290806,
339.903230649533));
#62741=CARTESIAN_POINT('Ctrl Pts',(55.9198310636415,-0.270932037427168,
339.910781902467));
#62742=CARTESIAN_POINT('Ctrl Pts',(55.9120698087153,-0.133988572437559,
339.918337190549));
#62743=CARTESIAN_POINT('Ctrl Pts',(55.9043085537891,0.00316250532587717,
339.920153909691));
#62744=CARTESIAN_POINT('Ctrl Pts',(55.896547298863,0.14000638281425,339.916256835772));
#62745=CARTESIAN_POINT('Ctrl Pts',(55.8887736284583,0.277069165909103,339.912353527804));
#62746=CARTESIAN_POINT('Ctrl Pts',(55.8809999580537,0.413823376612783,339.90271818942));
#62747=CARTESIAN_POINT('Ctrl Pts',(55.873226287649,0.549759262217033,339.887427525407));
#62748=CARTESIAN_POINT('Ctrl Pts',(55.8658144834719,0.679367299642118,339.872848645483));
#62749=CARTESIAN_POINT('Ctrl Pts',(55.8584026792948,0.808231199029922,339.853129145481));
#62750=CARTESIAN_POINT('Ctrl Pts',(55.8509908751177,0.935920287095614,339.828378224487));
#62751=CARTESIAN_POINT('Ctrl Pts',(55.8432157963393,1.06986779773376,339.802414187127));
#62752=CARTESIAN_POINT('Ctrl Pts',(55.8354407175609,1.20294572205231,339.770830996938));
#62753=CARTESIAN_POINT('Ctrl Pts',(55.8276656387824,1.3346459165838,339.733698695507));
#62754=CARTESIAN_POINT('Ctrl Pts',(55.8199001277334,1.46618404564138,339.696612087737));
#62755=CARTESIAN_POINT('Ctrl Pts',(55.8121346166844,1.59634744562955,339.653990060607));
#62756=CARTESIAN_POINT('Ctrl Pts',(55.8043691056354,1.72463664271504,339.605953919994));
#62757=CARTESIAN_POINT('Ctrl Pts',(55.7966112941132,1.85279864068811,339.557965407354));
#62758=CARTESIAN_POINT('Ctrl Pts',(55.788853482591,1.97908977013931,339.504573600254));
#62759=CARTESIAN_POINT('Ctrl Pts',(55.7810956710688,2.10302458897682,339.445949914322));
#62760=CARTESIAN_POINT('Ctrl Pts',(55.7733436975458,2.22686614293313,339.387370344573));
#62761=CARTESIAN_POINT('Ctrl Pts',(55.7655917240228,2.34835456382472,339.323566899169));
#62762=CARTESIAN_POINT('Ctrl Pts',(55.7578397504998,2.46702364898416,339.254759379548));
#62763=CARTESIAN_POINT('Ctrl Pts',(55.7500910599421,2.58564247771533,339.185980999953));
#62764=CARTESIAN_POINT('Ctrl Pts',(55.7423423693845,2.70144400803694,339.112202956792));
#62765=CARTESIAN_POINT('Ctrl Pts',(55.7345936788269,2.81398615098719,339.033691238128));
#62766=CARTESIAN_POINT('Ctrl Pts',(55.7268466004491,2.92650487860456,338.955195854483));
#62767=CARTESIAN_POINT('Ctrl Pts',(55.7190995220712,3.03576524735114,338.871968977832));
#62768=CARTESIAN_POINT('Ctrl Pts',(55.7113524436934,3.14135404914752,338.784319991809));
#62769=CARTESIAN_POINT('Ctrl Pts',(55.7036053003876,3.24694373588011,338.696670271203));
#62770=CARTESIAN_POINT('Ctrl Pts',(55.6958581570817,3.34886149353085,338.604598616961));
#62771=CARTESIAN_POINT('Ctrl Pts',(55.6881110137759,3.44672742984101,338.508454515436));
#62772=CARTESIAN_POINT('Ctrl Pts',(55.6803621287478,3.54461536849108,338.412288798676));
#62773=CARTESIAN_POINT('Ctrl Pts',(55.6726132437198,3.63844939436345,338.312049086619));
#62774=CARTESIAN_POINT('Ctrl Pts',(55.6648643586917,3.72788698163816,338.208121212584));
#62775=CARTESIAN_POINT('Ctrl Pts',(55.657107248917,3.81741949889219,338.10408302843));
#62776=CARTESIAN_POINT('Ctrl Pts',(55.6493501391422,3.90254600056036,337.996349159149));
#62777=CARTESIAN_POINT('Ctrl Pts',(55.6415930293675,3.982964397194,337.885338398383));
#62778=CARTESIAN_POINT('Ctrl Pts',(55.6338317744413,4.06342576684751,337.774268317016));
#62779=CARTESIAN_POINT('Ctrl Pts',(55.6260705195151,4.13917380263726,337.659918180706));
#62780=CARTESIAN_POINT('Ctrl Pts',(55.618309264589,4.20995074424667,337.542734314378));
#62781=CARTESIAN_POINT('Ctrl Pts',(55.6105355941843,4.28084090589646,337.425362992054));
#62782=CARTESIAN_POINT('Ctrl Pts',(55.6027619237796,4.3467438946554,337.305149224275));
#62783=CARTESIAN_POINT('Ctrl Pts',(55.594988253375,4.40744835677482,337.18256318233));
#62784=CARTESIAN_POINT('Ctrl Pts',(55.5875764491979,4.46532701157748,337.065683550131));
#62785=CARTESIAN_POINT('Ctrl Pts',(55.5801646450209,4.51848011349623,336.94664779499));
#62786=CARTESIAN_POINT('Ctrl Pts',(55.5727528408439,4.56676642834532,336.825877173152));
#62787=CARTESIAN_POINT('Ctrl Pts',(55.5649777620655,4.61741939932305,336.69918722338));
#62788=CARTESIAN_POINT('Ctrl Pts',(55.557202683287,4.66287652175415,336.570187681274));
#62789=CARTESIAN_POINT('Ctrl Pts',(55.5494276045086,4.70292170951451,336.439343759036));
#62790=CARTESIAN_POINT('Ctrl Pts',(55.5416620934596,4.74291761912187,336.308660848576));
#62791=CARTESIAN_POINT('Ctrl Pts',(55.5338965824106,4.77751473171469,336.17613844408));
#62792=CARTESIAN_POINT('Ctrl Pts',(55.5261310713616,4.80654476204257,336.042262209322));
#62793=CARTESIAN_POINT('Ctrl Pts',(55.5183732598395,4.83554600901076,335.908518713241));
#62794=CARTESIAN_POINT('Ctrl Pts',(55.5106154483173,4.85899107608548,335.77342443774));
#62795=CARTESIAN_POINT('Ctrl Pts',(55.5028576367951,4.87676140975535,335.637480364263));
#62796=CARTESIAN_POINT('Ctrl Pts',(55.4951056632721,4.89451837068569,335.501638593011));
#62797=CARTESIAN_POINT('Ctrl Pts',(55.4873536897491,4.90660904780779,335.364948682693));
#62798=CARTESIAN_POINT('Ctrl Pts',(55.4796017162261,4.91296598782485,335.227921620247));
#62799=CARTESIAN_POINT('Ctrl Pts',(55.4718530256685,4.91932023567402,335.090952588844));
#62800=CARTESIAN_POINT('Ctrl Pts',(55.4641043351109,4.91994555794236,334.953647078942));
#62801=CARTESIAN_POINT('Ctrl Pts',(55.4563556445532,4.91482638996126,334.816520793984));
#62802=CARTESIAN_POINT('Ctrl Pts',(55.4486085661754,4.90970828706581,334.679423039294));
#62803=CARTESIAN_POINT('Ctrl Pts',(55.4408614877976,4.89884808580942,334.542504825734));
#62804=CARTESIAN_POINT('Ctrl Pts',(55.4331144094198,4.88228234289008,334.40628105403));
#62805=CARTESIAN_POINT('Ctrl Pts',(55.425367266114,4.86571646113385,334.27005614064));
#62806=CARTESIAN_POINT('Ctrl Pts',(55.4176201228081,4.84344498952357,334.134526068731));
#62807=CARTESIAN_POINT('Ctrl Pts',(55.4098729795023,4.81555623709075,334.000199424927));
#62808=CARTESIAN_POINT('Ctrl Pts',(55.4021240944742,4.78766121467436,333.865842581642));
#62809=CARTESIAN_POINT('Ctrl Pts',(55.3943752094461,4.75414647788029,333.732690087478));
#62810=CARTESIAN_POINT('Ctrl Pts',(55.386626324418,4.71515112180248,333.601238776251));
#62811=CARTESIAN_POINT('Ctrl Pts',(55.3788692146433,4.67611437565081,333.469647941244));
#62812=CARTESIAN_POINT('Ctrl Pts',(55.3711121048686,4.63158550118186,333.339762271461));
#62813=CARTESIAN_POINT('Ctrl Pts',(55.3633549950939,4.58175319296852,333.212062433634));
#62814=CARTESIAN_POINT('Ctrl Pts',(55.3555937401677,4.53189425596296,333.084294357097));
#62815=CARTESIAN_POINT('Ctrl Pts',(55.3478324852415,4.47672639537413,332.958714797621));
#62816=CARTESIAN_POINT('Ctrl Pts',(55.3400712303154,4.41648544645576,332.835782043383));
#62817=CARTESIAN_POINT('Ctrl Pts',(55.3322975599107,4.35614813165165,332.712652636802));
#62818=CARTESIAN_POINT('Ctrl Pts',(55.3245238895061,4.29072169840841,332.592178839966));
#62819=CARTESIAN_POINT('Ctrl Pts',(55.3167502191014,4.22048714815252,332.474792821415));
#62820=CARTESIAN_POINT('Ctrl Pts',(55.3093384149243,4.15352203310783,332.362871150267));
#62821=CARTESIAN_POINT('Ctrl Pts',(55.3019266107471,4.08218652046496,332.253756495513));
#62822=CARTESIAN_POINT('Ctrl Pts',(55.29451480657,4.0067584236649,332.147795589918));
#62823=CARTESIAN_POINT('Ctrl Pts',(55.2867397277915,3.92763337115265,332.0366412247));
#62824=CARTESIAN_POINT('Ctrl Pts',(55.2789646490131,3.84375436138737,331.928606306436));
#62825=CARTESIAN_POINT('Ctrl Pts',(55.2711895702346,3.75539566463496,331.824124299576));
#62826=CARTESIAN_POINT('Ctrl Pts',(55.2634240591856,3.66714569888416,331.719770864478));
#62827=CARTESIAN_POINT('Ctrl Pts',(55.2556585481366,3.57442726450781,331.618961937195));
#62828=CARTESIAN_POINT('Ctrl Pts',(55.2478930370876,3.47755769772876,331.522101852919));
#62829=CARTESIAN_POINT('Ctrl Pts',(55.2401352255654,3.38078417740746,331.425337805699));
#62830=CARTESIAN_POINT('Ctrl Pts',(55.2323774140432,3.27986799010021,331.332515084436));
#62831=CARTESIAN_POINT('Ctrl Pts',(55.2246196025211,3.17516626568361,331.244004493112));
#62832=CARTESIAN_POINT('Ctrl Pts',(55.2168676289981,3.07054333263469,331.155560508814));
#62833=CARTESIAN_POINT('Ctrl Pts',(55.2091156554751,2.96214083005063,331.07142244674));
#62834=CARTESIAN_POINT('Ctrl Pts',(55.2013636819521,2.8503519549001,330.99192355416));
#62835=CARTESIAN_POINT('Ctrl Pts',(55.1936149913945,2.73861042240456,330.912458329408));
#62836=CARTESIAN_POINT('Ctrl Pts',(55.1858663008369,2.62348568760364,330.837628592575));
#62837=CARTESIAN_POINT('Ctrl Pts',(55.1781176102793,2.50540299358856,330.767726509048));
#62838=CARTESIAN_POINT('Ctrl Pts',(55.1703705319014,2.38734486766413,330.697838969232));
#62839=CARTESIAN_POINT('Ctrl Pts',(55.1626234535236,2.26633034280122,330.632877242438));
#62840=CARTESIAN_POINT('Ctrl Pts',(55.1548763751457,2.14281219293304,330.573089229687));
#62841=CARTESIAN_POINT('Ctrl Pts',(55.1471292318399,2.01929300786379,330.513300715854));
#62842=CARTESIAN_POINT('Ctrl Pts',(55.1393820885341,1.89327050776298,330.458686172848));
#62843=CARTESIAN_POINT('Ctrl Pts',(55.1316349452283,1.76522016305758,330.409446565126));
#62844=CARTESIAN_POINT('Ctrl Pts',(55.1238860602002,1.63714102991557,330.360195887294));
#62845=CARTESIAN_POINT('Ctrl Pts',(55.116137175172,1.50703350973344,330.316322689589));
#62846=CARTESIAN_POINT('Ctrl Pts',(55.1083882901439,1.37539067300435,330.277978869264));
#62847=CARTESIAN_POINT('Ctrl Pts',(55.1006311803692,1.24360810920885,330.239594350413));
#62848=CARTESIAN_POINT('Ctrl Pts',(55.0928740705945,1.11028734945773,330.206751042178));
#62849=CARTESIAN_POINT('Ctrl Pts',(55.0851169608197,0.975934710121021,330.179550383618));
#62850=CARTESIAN_POINT('Ctrl Pts',(55.0773557058936,0.841510277029617,330.152335189895));
#62851=CARTESIAN_POINT('Ctrl Pts',(55.0695944509674,0.706053251448218,330.130768715433));
#62852=CARTESIAN_POINT('Ctrl Pts',(55.0618331960412,0.570076641669434,330.114900647364));
#62853=CARTESIAN_POINT('Ctrl Pts',(55.0540595256366,0.433882513629586,330.099007195558));
#62854=CARTESIAN_POINT('Ctrl Pts',(55.0462858552319,0.297167530478643,330.088830394832));
#62855=CARTESIAN_POINT('Ctrl Pts',(55.0385121848272,0.160447177956737,330.084367816284));
#62856=CARTESIAN_POINT('Ctrl Pts',(55.0311003806502,0.0300911907387572,
330.080112971841));
#62857=CARTESIAN_POINT('Ctrl Pts',(55.0236885764732,-0.100269389422622,
330.081052325614));
#62858=CARTESIAN_POINT('Ctrl Pts',(55.0162767722961,-0.230192646753969,
330.087139895348));
#62859=CARTESIAN_POINT('Ctrl Pts',(55.0085016935177,-0.366483829949416,
330.093525835009));
#62860=CARTESIAN_POINT('Ctrl Pts',(55.0007266147393,-0.50272444270147,330.105597590486));
#62861=CARTESIAN_POINT('Ctrl Pts',(54.9929515359609,-0.63840155212901,330.123359094547));
#62862=CARTESIAN_POINT('Ctrl Pts',(54.9851860249118,-0.773911702235956,
330.141098741946));
#62863=CARTESIAN_POINT('Ctrl Pts',(54.9774205138628,-0.908859344876275,
330.164514156507));
#62864=CARTESIAN_POINT('Ctrl Pts',(54.9696550028138,-1.04273273712167,330.193557292401));
#62865=CARTESIAN_POINT('Ctrl Pts',(54.9618971912916,-1.17647339350881,330.222571631941));
#62866=CARTESIAN_POINT('Ctrl Pts',(54.9541393797694,-1.309141539627,330.257202506158));
#62867=CARTESIAN_POINT('Ctrl Pts',(54.9463815682472,-1.4402320950282,330.297350260231));
#62868=CARTESIAN_POINT('Ctrl Pts',(54.9386295947241,-1.57122400062969,330.337467801846));
#62869=CARTESIAN_POINT('Ctrl Pts',(54.9308776212012,-1.70064030631718,330.383093845706));
#62870=CARTESIAN_POINT('Ctrl Pts',(54.9231256476781,-1.8279879959111,330.434078083311));
#62871=CARTESIAN_POINT('Ctrl Pts',(54.9153769571205,-1.95528175368235,330.48504072906));
#62872=CARTESIAN_POINT('Ctrl Pts',(54.9076282665629,-2.08050827566386,330.541356910303));
#62873=CARTESIAN_POINT('Ctrl Pts',(54.8998795760052,-2.20319175031282,330.602827138507));
#62874=CARTESIAN_POINT('Ctrl Pts',(54.8921324976274,-2.32584969964054,330.664284577316));
#62875=CARTESIAN_POINT('Ctrl Pts',(54.8843854192495,-2.44596530481481,330.730893755133));
#62876=CARTESIAN_POINT('Ctrl Pts',(54.8766383408717,-2.56308507862277,330.802408078167));
#62877=CARTESIAN_POINT('Ctrl Pts',(54.8688911975659,-2.68020583400715,330.873923000558));
#62878=CARTESIAN_POINT('Ctrl Pts',(54.8611440542601,-2.79433037434501,330.950342946463));
#62879=CARTESIAN_POINT('Ctrl Pts',(54.8533969109542,-2.90503240000683,331.031376836054));
#62880=CARTESIAN_POINT('Ctrl Pts',(54.8456480259262,-3.01575931383354,331.112428943783));
#62881=CARTESIAN_POINT('Ctrl Pts',(54.8378991408981,-3.12306186651507,331.198096828503));
#62882=CARTESIAN_POINT('Ctrl Pts',(54.8301502558701,-3.22654549567289,331.288048057039));
#62883=CARTESIAN_POINT('Ctrl Pts',(54.8223931460953,-3.33013896342452,331.378094760739));
#62884=CARTESIAN_POINT('Ctrl Pts',(54.8146360363206,-3.42990511504537,331.472433633252));
#62885=CARTESIAN_POINT('Ctrl Pts',(54.8068789265458,-3.52548465142783,331.570693796838));
#62886=CARTESIAN_POINT('Ctrl Pts',(54.7991176716197,-3.62111526245843,331.669006467513));
#62887=CARTESIAN_POINT('Ctrl Pts',(54.7913564166935,-3.71255453999873,331.771244313358));
#62888=CARTESIAN_POINT('Ctrl Pts',(54.7835951617674,-3.79948308285538,331.877002823313));
#62889=CARTESIAN_POINT('Ctrl Pts',(54.7758214913627,-3.88655068305071,331.982930512418));
#62890=CARTESIAN_POINT('Ctrl Pts',(54.7680478209581,-3.96909289398145,332.092389807617));
#62891=CARTESIAN_POINT('Ctrl Pts',(54.7602741505534,-4.04683279924899,332.204945911539));
#62892=CARTESIAN_POINT('Ctrl Pts',(54.7528623463762,-4.12095389322377,332.312262501744));
#62893=CARTESIAN_POINT('Ctrl Pts',(54.7454505421991,-4.19070956061081,332.422393832951));
#62894=CARTESIAN_POINT('Ctrl Pts',(54.7380387380219,-4.25589932288684,332.534943405122));
#62895=CARTESIAN_POINT('Ctrl Pts',(54.7299509628006,-4.32703451904377,332.657757718508));
#62896=CARTESIAN_POINT('Ctrl Pts',(54.7218631875793,-4.39294259267623,332.783813504407));
#62897=CARTESIAN_POINT('Ctrl Pts',(54.713775412358,-4.4533284598564,332.912645528155));
#62898=CARTESIAN_POINT('Ctrl Pts',(54.7057004306988,-4.51361880628807,333.041273760321));
#62899=CARTESIAN_POINT('Ctrl Pts',(54.6976254490397,-4.56840420158663,333.172669170312));
#62900=CARTESIAN_POINT('Ctrl Pts',(54.6895504673805,-4.61743424595299,333.306340043928));
#62901=CARTESIAN_POINT('Ctrl Pts',(54.6814060431412,-4.66688593496565,333.441160449612));
#62902=CARTESIAN_POINT('Ctrl Pts',(54.6732616189019,-4.71048260241859,333.578295351565));
#62903=CARTESIAN_POINT('Ctrl Pts',(54.6651171946625,-4.74801496691996,333.717215163637));
#62904=CARTESIAN_POINT('Ctrl Pts',(54.6570678915408,-4.78510897993681,333.85451249051));
#62905=CARTESIAN_POINT('Ctrl Pts',(54.649018588419,-4.81627946047852,333.993552920156));
#62906=CARTESIAN_POINT('Ctrl Pts',(54.6409692852972,-4.84137278189544,334.133805651587));
#62907=CARTESIAN_POINT('Ctrl Pts',(54.6327773004991,-4.86691090668357,334.276544498217));
#62908=CARTESIAN_POINT('Ctrl Pts',(54.624585315701,-4.88615423912597,334.420538700199));
#62909=CARTESIAN_POINT('Ctrl Pts',(54.6163933309029,-4.8989941346828,334.565213235202));
#62910=CARTESIAN_POINT('Ctrl Pts',(54.6082013461048,-4.91183403023962,334.709887770205));
#62911=CARTESIAN_POINT('Ctrl Pts',(54.6000093613067,-4.91827040274491,334.855242264824));
#62912=CARTESIAN_POINT('Ctrl Pts',(54.5918173765086,-4.91824995138145,335.000691546333));
#62913=CARTESIAN_POINT('',(52.8418173765483,-4.9182481654623,335.0042479909));
#62914=CARTESIAN_POINT('Ctrl Pts',(54.5918173764761,-4.91824995138137,335.000691546911));
#62915=CARTESIAN_POINT('Ctrl Pts',(54.5836110677012,-4.91822946424087,335.146395151661));
#62916=CARTESIAN_POINT('Ctrl Pts',(54.5754047589264,-4.91172998599915,335.291945594707));
#62917=CARTESIAN_POINT('Ctrl Pts',(54.5671984501516,-4.89881778224724,335.436769274146));
#62918=CARTESIAN_POINT('Ctrl Pts',(54.5589779382225,-4.88588323056439,335.581843608675));
#62919=CARTESIAN_POINT('Ctrl Pts',(54.5507574262934,-4.86651382143102,335.726188354007));
#62920=CARTESIAN_POINT('Ctrl Pts',(54.5425369143643,-4.84082709624967,335.86923879729));
#62921=CARTESIAN_POINT('Ctrl Pts',(54.5342938029828,-4.81506975430787,336.012682508257));
#62922=CARTESIAN_POINT('Ctrl Pts',(54.5260506916014,-4.782960419235,336.154824488968));
#62923=CARTESIAN_POINT('Ctrl Pts',(54.5178075802199,-4.74466735313486,336.295111875707));
#62924=CARTESIAN_POINT('Ctrl Pts',(54.5095521161366,-4.70631690301917,336.435609489894));
#62925=CARTESIAN_POINT('Ctrl Pts',(54.5012966520531,-4.66176431752209,336.574246661269));
#62926=CARTESIAN_POINT('Ctrl Pts',(54.4930411879697,-4.61122656490549,336.710489003066));
#62927=CARTESIAN_POINT('Ctrl Pts',(54.4847663984023,-4.56057050682228,336.847050278987));
#62928=CARTESIAN_POINT('Ctrl Pts',(54.4764916088349,-4.50390138954868,336.981205224612));
#62929=CARTESIAN_POINT('Ctrl Pts',(54.4682168192675,-4.44148355973158,337.112440969858));
#62930=CARTESIAN_POINT('Ctrl Pts',(54.4654114474277,-4.42032226968963,337.156933347711));
#62931=CARTESIAN_POINT('Ctrl Pts',(54.4626060755879,-4.3985006058219,337.201090428254));
#62932=CARTESIAN_POINT('Ctrl Pts',(54.4598007037481,-4.37603000737524,337.244892967839));
#62933=CARTESIAN_POINT('Ctrl Pts',(54.4520256249696,-4.31375281807674,337.366291561469));
#62934=CARTESIAN_POINT('Ctrl Pts',(54.4442505461912,-4.24632168263603,337.485288510239));
#62935=CARTESIAN_POINT('Ctrl Pts',(54.4364754674127,-4.17394552842669,337.601415343275));
#62936=CARTESIAN_POINT('Ctrl Pts',(54.4287099563637,-4.10165843768284,337.71739927485));
#62937=CARTESIAN_POINT('Ctrl Pts',(54.4209444453147,-4.02443864066394,337.830519789531));
#62938=CARTESIAN_POINT('Ctrl Pts',(54.4131789342657,-3.94254187962858,337.940331034063));
#62939=CARTESIAN_POINT('Ctrl Pts',(54.4054211227435,-3.86072631947018,338.050033400427));
#62940=CARTESIAN_POINT('Ctrl Pts',(54.3976633112213,-3.77424325580748,338.156432715007));
#62941=CARTESIAN_POINT('Ctrl Pts',(54.3899054996991,-3.68339264214193,338.25911056982));
#62942=CARTESIAN_POINT('Ctrl Pts',(54.3821535261761,-3.59261039644439,338.361711156292));
#62943=CARTESIAN_POINT('Ctrl Pts',(54.3744015526532,-3.49746740077174,338.460595565733));
#62944=CARTESIAN_POINT('Ctrl Pts',(54.3666495791302,-3.39830471245034,338.555377356039));
#62945=CARTESIAN_POINT('Ctrl Pts',(54.3589008885725,-3.29918401958624,338.650119006202));
#62946=CARTESIAN_POINT('Ctrl Pts',(54.3511521980149,-3.19604730188507,338.740761223404));
#62947=CARTESIAN_POINT('Ctrl Pts',(54.3434035074573,-3.0892732496295,338.826953599356));
#62948=CARTESIAN_POINT('Ctrl Pts',(54.3356564290795,-2.98252141260715,338.913128042265));
#62949=CARTESIAN_POINT('Ctrl Pts',(54.3279093507016,-2.87213405026839,338.994854240095));
#62950=CARTESIAN_POINT('Ctrl Pts',(54.3201622723237,-2.75852347643963,339.071821618444));
#62951=CARTESIAN_POINT('Ctrl Pts',(54.3124151290179,-2.64491195044507,339.148789641855));
#62952=CARTESIAN_POINT('Ctrl Pts',(54.3046679857122,-2.52807748268486,339.220998547002));
#62953=CARTESIAN_POINT('Ctrl Pts',(54.2969208424064,-2.40846161182988,339.28818093448));
#62954=CARTESIAN_POINT('Ctrl Pts',(54.2891719573783,-2.28881884878754,339.355378425986));
#62955=CARTESIAN_POINT('Ctrl Pts',(54.2814230723502,-2.16639377906995,339.417546959742));
#62956=CARTESIAN_POINT('Ctrl Pts',(54.2736741873221,-2.04165243009053,339.474465154318));
#62957=CARTESIAN_POINT('Ctrl Pts',(54.2659170775474,-1.91677867935449,339.531443762454));
#62958=CARTESIAN_POINT('Ctrl Pts',(54.2581599677726,-1.78958409439328,339.583160736775));
#62959=CARTESIAN_POINT('Ctrl Pts',(54.2504028579979,-1.66055508313776,339.629442717905));
#62960=CARTESIAN_POINT('Ctrl Pts',(54.2426416030717,-1.53145712290427,339.675749430646));
#62961=CARTESIAN_POINT('Ctrl Pts',(54.2348803481456,-1.4005231560564,339.716615246746));
#62962=CARTESIAN_POINT('Ctrl Pts',(54.2271190932194,-1.26825367200316,339.751917053774));
#62963=CARTESIAN_POINT('Ctrl Pts',(54.2193454228147,-1.13577259988187,339.787275332189));
#62964=CARTESIAN_POINT('Ctrl Pts',(54.2115717524101,-1.00195212315458,339.817051730551));
#62965=CARTESIAN_POINT('Ctrl Pts',(54.2037980820054,-0.867302694724706,
339.841174351149));
#62966=CARTESIAN_POINT('Ctrl Pts',(54.1963862778283,-0.738921229583391,
339.864174057954));
#62967=CARTESIAN_POINT('Ctrl Pts',(54.1889744736512,-0.60978653644116,339.882034468721));
#62968=CARTESIAN_POINT('Ctrl Pts',(54.1815626694742,-0.480342544192952,
339.894737388537));
#62969=CARTESIAN_POINT('Ctrl Pts',(54.1737875906957,-0.344554116290516,
339.908062916293));
#62970=CARTESIAN_POINT('Ctrl Pts',(54.1660125119173,-0.207996186796566,
339.915754712944));
#62971=CARTESIAN_POINT('Ctrl Pts',(54.1582374331389,-0.071175765453526,
339.917734953504));
#62972=CARTESIAN_POINT('Ctrl Pts',(54.1504719220899,0.0654762896507296,
339.919712757252));
#62973=CARTESIAN_POINT('Ctrl Pts',(54.1427064110408,0.202389806803813,339.915992983874));
#62974=CARTESIAN_POINT('Ctrl Pts',(54.1349408999918,0.339051461682754,339.906549415713));
#62975=CARTESIAN_POINT('Ctrl Pts',(54.1271830884696,0.475577616133003,339.897115210877));
#62976=CARTESIAN_POINT('Ctrl Pts',(54.1194252769474,0.611852017837889,339.881968531918));
#62977=CARTESIAN_POINT('Ctrl Pts',(54.1116674654252,0.747360496548205,339.861135191568));
#62978=CARTESIAN_POINT('Ctrl Pts',(54.1039154919022,0.882767000831071,339.840317528967));
#62979=CARTESIAN_POINT('Ctrl Pts',(54.0961635183792,1.0174083445987,339.813821782053));
#62980=CARTESIAN_POINT('Ctrl Pts',(54.0884115448561,1.15077499475336,339.781725627214));
#62981=CARTESIAN_POINT('Ctrl Pts',(54.0806628542985,1.28408516405241,339.749643065114));
#62982=CARTESIAN_POINT('Ctrl Pts',(54.0729141637409,1.41612133419609,339.711964903651));
#62983=CARTESIAN_POINT('Ctrl Pts',(54.0651654731833,1.54638390833746,339.66881996553));
#62984=CARTESIAN_POINT('Ctrl Pts',(54.0574183948055,1.67661938026239,339.625684004074));
#62985=CARTESIAN_POINT('Ctrl Pts',(54.0496713164276,1.80508161935684,339.577083651167));
#62986=CARTESIAN_POINT('Ctrl Pts',(54.0419242380497,1.93128633031,339.523197560671));
#62987=CARTESIAN_POINT('Ctrl Pts',(54.0341770947439,2.05749209897993,339.469311018558));
#62988=CARTESIAN_POINT('Ctrl Pts',(54.0264299514382,2.18143994229291,339.410138803985));
#62989=CARTESIAN_POINT('Ctrl Pts',(54.0186828081324,2.30266605647411,339.34590751108));
#62990=CARTESIAN_POINT('Ctrl Pts',(54.0109339231043,2.42391942485956,339.281661777616));
#62991=CARTESIAN_POINT('Ctrl Pts',(54.0031850380761,2.54244950117534,339.212354885512));
#62992=CARTESIAN_POINT('Ctrl Pts',(53.995436153048,2.65781792688049,339.138258924965));
#62993=CARTESIAN_POINT('Ctrl Pts',(53.9876790432733,2.77330880582467,339.064084318201));
#62994=CARTESIAN_POINT('Ctrl Pts',(53.9799219334986,2.88563100121114,338.985110700454));
#62995=CARTESIAN_POINT('Ctrl Pts',(53.9721648237238,2.99437550819959,338.901653287825));
#62996=CARTESIAN_POINT('Ctrl Pts',(53.9644035687977,3.1031781247756,338.818151278223));
#62997=CARTESIAN_POINT('Ctrl Pts',(53.9566423138715,3.20839894381921,338.730160950119));
#62998=CARTESIAN_POINT('Ctrl Pts',(53.9488810589453,3.30966359392258,338.638036552533));
#62999=CARTESIAN_POINT('Ctrl Pts',(53.9411073885407,3.41109023446403,338.545764785934));
#63000=CARTESIAN_POINT('Ctrl Pts',(53.933333718136,3.50854778167336,338.449346009842));
#63001=CARTESIAN_POINT('Ctrl Pts',(53.9255600477314,3.60169953987352,338.349170567017));
#63002=CARTESIAN_POINT('Ctrl Pts',(53.9181482435543,3.69051506131787,338.253658315157));
#63003=CARTESIAN_POINT('Ctrl Pts',(53.9107364393772,3.77541645397247,338.154731489822));
#63004=CARTESIAN_POINT('Ctrl Pts',(53.9033246352002,3.8561481819506,338.05275355398));
#63005=CARTESIAN_POINT('Ctrl Pts',(53.8955495564218,3.94083681240484,337.945777375726));
#63006=CARTESIAN_POINT('Ctrl Pts',(53.8877744776433,4.02120433964719,337.835105372002));
#63007=CARTESIAN_POINT('Ctrl Pts',(53.8799993988649,4.09691094692358,337.721121782552));
#63008=CARTESIAN_POINT('Ctrl Pts',(53.8722338878159,4.17252439239999,337.607278457165));
#63009=CARTESIAN_POINT('Ctrl Pts',(53.8644683767669,4.24348811583597,337.490131976854));
#63010=CARTESIAN_POINT('Ctrl Pts',(53.8567028657179,4.30950228099872,337.370099819115));
#63011=CARTESIAN_POINT('Ctrl Pts',(53.8489450541957,4.37545099292452,337.250186673609));
#63012=CARTESIAN_POINT('Ctrl Pts',(53.8411872426735,4.43645972563388,337.127393884827));
#63013=CARTESIAN_POINT('Ctrl Pts',(53.8334294311513,4.49227193857836,337.002167798253));
#63014=CARTESIAN_POINT('Ctrl Pts',(53.8256774576283,4.54804215106267,336.87703594828));
#63015=CARTESIAN_POINT('Ctrl Pts',(53.8179254841053,4.59862346905246,336.749474800878));
#63016=CARTESIAN_POINT('Ctrl Pts',(53.8101735105823,4.64380547468176,336.61995486845));
#63017=CARTESIAN_POINT('Ctrl Pts',(53.8024248200247,4.68896834570485,336.49048978779));
#63018=CARTESIAN_POINT('Ctrl Pts',(53.7946761294671,4.72873632380081,336.359067940308));
#63019=CARTESIAN_POINT('Ctrl Pts',(53.7869274389095,4.76294737821085,336.22617916101));
#63020=CARTESIAN_POINT('Ctrl Pts',(53.7791803605316,4.79715131472528,336.093318030331));
#63021=CARTESIAN_POINT('Ctrl Pts',(53.7714332821538,4.82580052985802,335.958990953209));
#63022=CARTESIAN_POINT('Ctrl Pts',(53.763686203776,4.8487831774724,335.823701863759));
#63023=CARTESIAN_POINT('Ctrl Pts',(53.7559390604702,4.8717660177035,335.688411640456));
#63024=CARTESIAN_POINT('Ctrl Pts',(53.7481919171644,4.88908213022821,335.552159774097));
#63025=CARTESIAN_POINT('Ctrl Pts',(53.7404447738586,4.90067107204616,335.415458910255));
#63026=CARTESIAN_POINT('Ctrl Pts',(53.7326958888305,4.91226261930427,335.278727313156));
#63027=CARTESIAN_POINT('Ctrl Pts',(53.7249470038024,4.91812440068441,335.141546907107));
#63028=CARTESIAN_POINT('Ctrl Pts',(53.7171981187743,4.91824800168097,335.004433560777));
#63029=CARTESIAN_POINT('Ctrl Pts',(53.7094410089996,4.9183717338689,334.867174680925));
#63030=CARTESIAN_POINT('Ctrl Pts',(53.7016838992249,4.91274511884748,334.729983394468));
#63031=CARTESIAN_POINT('Ctrl Pts',(53.6939267894502,4.90141189257198,334.59337422382));
#63032=CARTESIAN_POINT('Ctrl Pts',(53.686165534524,4.89007261018273,334.4566920536));
#63033=CARTESIAN_POINT('Ctrl Pts',(53.6784042795978,4.87302068884256,334.320593006657));
#63034=CARTESIAN_POINT('Ctrl Pts',(53.6706430246717,4.85035143026003,334.185583604368));
#63035=CARTESIAN_POINT('Ctrl Pts',(53.662869354267,4.82764590825166,334.050358231035));
#63036=CARTESIAN_POINT('Ctrl Pts',(53.6550956838624,4.7993051733402,333.91622636817));
#63037=CARTESIAN_POINT('Ctrl Pts',(53.6473220134577,4.76547526772822,333.783682387215));
#63038=CARTESIAN_POINT('Ctrl Pts',(53.6399102092806,4.73322015236124,333.657308360461));
#63039=CARTESIAN_POINT('Ctrl Pts',(53.6324984051034,4.69597548963163,333.532377986476));
#63040=CARTESIAN_POINT('Ctrl Pts',(53.6250866009263,4.65390863817244,333.409302841505));
#63041=CARTESIAN_POINT('Ctrl Pts',(53.6173115221479,4.60977996501279,333.280195417058));
#63042=CARTESIAN_POINT('Ctrl Pts',(53.6095364433694,4.56020499647602,333.15272167726));
#63043=CARTESIAN_POINT('Ctrl Pts',(53.601761364591,4.50532295361591,333.027375315444));
#63044=CARTESIAN_POINT('Ctrl Pts',(53.593995853542,4.45050844660351,332.902183200305));
#63045=CARTESIAN_POINT('Ctrl Pts',(53.586230342493,4.39040001474811,332.779113608963));
#63046=CARTESIAN_POINT('Ctrl Pts',(53.5784648314439,4.32518646519238,332.65864460113));
#63047=CARTESIAN_POINT('Ctrl Pts',(53.5707070199217,4.26003757506089,332.53829503867));
#63048=CARTESIAN_POINT('Ctrl Pts',(53.5629492083995,4.18979382525483,332.420541269912));
#63049=CARTESIAN_POINT('Ctrl Pts',(53.5551913968773,4.11469172840129,332.305840568428));
#63050=CARTESIAN_POINT('Ctrl Pts',(53.5474394233543,4.03964614825732,332.191226182861));
#63051=CARTESIAN_POINT('Ctrl Pts',(53.5396874498313,3.95974971152921,332.079660617142));
#63052=CARTESIAN_POINT('Ctrl Pts',(53.5319354763083,3.87528421295256,331.971575437403));
#63053=CARTESIAN_POINT('Ctrl Pts',(53.5241867857507,3.7908544855647,331.863536031802));
#63054=CARTESIAN_POINT('Ctrl Pts',(53.5164380951931,3.70185978508869,331.758974387952));
#63055=CARTESIAN_POINT('Ctrl Pts',(53.5086894046355,3.60862434008963,331.658291838803));
#63056=CARTESIAN_POINT('Ctrl Pts',(53.5009423262576,3.51540829350356,331.557630237499));
#63057=CARTESIAN_POINT('Ctrl Pts',(53.4931952478798,3.41795352280899,331.460846412172));
#63058=CARTESIAN_POINT('Ctrl Pts',(53.4854481695019,3.31662327059217,331.368307124292));
#63059=CARTESIAN_POINT('Ctrl Pts',(53.4777010261961,3.21529216913031,331.275767060844));
#63060=CARTESIAN_POINT('Ctrl Pts',(53.4699538828903,3.110085809988,331.187471869381));
#63061=CARTESIAN_POINT('Ctrl Pts',(53.4622067395845,3.00140257858864,331.103749799648));
#63062=CARTESIAN_POINT('Ctrl Pts',(53.4544578545564,2.89269491289152,331.020008907416));
#63063=CARTESIAN_POINT('Ctrl Pts',(53.4467089695283,2.78050912908314,330.940843421275));
#63064=CARTESIAN_POINT('Ctrl Pts',(53.4389600845002,2.6652744785608,330.866539583299));
#63065=CARTESIAN_POINT('Ctrl Pts',(53.4312029747255,2.54991751678973,330.792156878462));
#63066=CARTESIAN_POINT('Ctrl Pts',(53.4234458649507,2.43150555291668,330.722646341935));
#63067=CARTESIAN_POINT('Ctrl Pts',(53.415688755176,2.31049492785192,330.658249632824));
#63068=CARTESIAN_POINT('Ctrl Pts',(53.4079275002498,2.18941963857838,330.593818512171));
#63069=CARTESIAN_POINT('Ctrl Pts',(53.4001662453236,2.06574327338222,330.53450683295));
#63070=CARTESIAN_POINT('Ctrl Pts',(53.3924049903975,1.93994335011714,330.480508561703));
#63071=CARTESIAN_POINT('Ctrl Pts',(53.3846313199928,1.81394218797293,330.42642391082));
#63072=CARTESIAN_POINT('Ctrl Pts',(53.3768576495881,1.68581104506024,330.37766979195));
#63073=CARTESIAN_POINT('Ctrl Pts',(53.3690839791834,1.55604468068748,330.334390927842));
#63074=CARTESIAN_POINT('Ctrl Pts',(53.3616721750064,1.43231897179732,330.293126705271));
#63075=CARTESIAN_POINT('Ctrl Pts',(53.3542603708294,1.30710713094088,330.256839542874));
#63076=CARTESIAN_POINT('Ctrl Pts',(53.3468485666524,1.18084582872362,330.225611432729));
#63077=CARTESIAN_POINT('Ctrl Pts',(53.339073487874,1.04839608397063,330.192852739882));
#63078=CARTESIAN_POINT('Ctrl Pts',(53.3312984090956,0.914372836555685,330.165558033514));
#63079=CARTESIAN_POINT('Ctrl Pts',(53.3235233303171,0.779266584234283,330.143877405461));
#63080=CARTESIAN_POINT('Ctrl Pts',(53.3157578192681,0.644326588757556,330.1222234568));
#63081=CARTESIAN_POINT('Ctrl Pts',(53.3079923082191,0.508306622325505,330.106169901897));
#63082=CARTESIAN_POINT('Ctrl Pts',(53.3002267971701,0.371710869928192,330.09581667434));
#63083=CARTESIAN_POINT('Ctrl Pts',(53.2924689856479,0.235250552617069,330.085473712039));
#63084=CARTESIAN_POINT('Ctrl Pts',(53.2847111741257,0.0982159726965942,
330.08081985885));
#63085=CARTESIAN_POINT('Ctrl Pts',(53.2769533626035,-0.0388803481775629,
330.08190368323));
#63086=CARTESIAN_POINT('Ctrl Pts',(53.2692013890805,-0.175873499722502,
330.082986691998));
#63087=CARTESIAN_POINT('Ctrl Pts',(53.2614494155575,-0.312927910452457,
330.089798780917));
#63088=CARTESIAN_POINT('Ctrl Pts',(53.2536974420345,-0.44952817189983,330.102336527979));
#63089=CARTESIAN_POINT('Ctrl Pts',(53.2459487514769,-0.586070583055472,
330.114868965298));
#63090=CARTESIAN_POINT('Ctrl Pts',(53.2382000609192,-0.722158839036186,
330.133122202314));
#63091=CARTESIAN_POINT('Ctrl Pts',(53.2304513703616,-0.85727999172154,330.157040772596));
#63092=CARTESIAN_POINT('Ctrl Pts',(53.2227042919838,-0.992373031322524,
330.18095436642));
#63093=CARTESIAN_POINT('Ctrl Pts',(53.214957213606,-1.1264989832079,330.210530880865));
#63094=CARTESIAN_POINT('Ctrl Pts',(53.2072101352282,-1.25915285842844,330.245663333165));
#63095=CARTESIAN_POINT('Ctrl Pts',(53.1994629919224,-1.39180784541614,330.280796079909));
#63096=CARTESIAN_POINT('Ctrl Pts',(53.1917158486166,-1.5229903532837,330.321484757313));
#63097=CARTESIAN_POINT('Ctrl Pts',(53.1839687053107,-1.65220876060685,330.367571989348));
#63098=CARTESIAN_POINT('Ctrl Pts',(53.1762198202827,-1.78145621897136,330.413669582771));
#63099=CARTESIAN_POINT('Ctrl Pts',(53.1684709352546,-1.90873833002666,330.465168014688));
#63100=CARTESIAN_POINT('Ctrl Pts',(53.1607220502265,-2.03358209414407,330.521861220454));
#63101=CARTESIAN_POINT('Ctrl Pts',(53.1529649404518,-2.15855836872268,330.578614600973));
#63102=CARTESIAN_POINT('Ctrl Pts',(53.145207830677,-2.28109076995865,330.640573607775));
#63103=CARTESIAN_POINT('Ctrl Pts',(53.1374507209023,-2.40072912930451,330.707485269657));
#63104=CARTESIAN_POINT('Ctrl Pts',(53.1296894659761,-2.52043141956423,330.774432686993));
#63105=CARTESIAN_POINT('Ctrl Pts',(53.12192821105,-2.63723625373589,330.846337828076));
#63106=CARTESIAN_POINT('Ctrl Pts',(53.1141669561238,-2.75072210890685,330.922904104381));
#63107=CARTESIAN_POINT('Ctrl Pts',(53.1063932857192,-2.86438950446113,330.999592861776));
#63108=CARTESIAN_POINT('Ctrl Pts',(53.0986196153145,-2.97472699673653,331.080957422177));
#63109=CARTESIAN_POINT('Ctrl Pts',(53.0908459449099,-3.08134514263344,331.166660049713));
#63110=CARTESIAN_POINT('Ctrl Pts',(53.0834341407327,-3.1830001881896,331.248373199319));
#63111=CARTESIAN_POINT('Ctrl Pts',(53.0760223365555,-3.2812741489455,331.334029441844));
#63112=CARTESIAN_POINT('Ctrl Pts',(53.0686105323783,-3.37586176849261,331.42330594228));
#63113=CARTESIAN_POINT('Ctrl Pts',(53.0609503198048,-3.47361951481569,331.515574566059));
#63114=CARTESIAN_POINT('Ctrl Pts',(53.0532901072313,-3.56776814878884,331.61202089573));
#63115=CARTESIAN_POINT('Ctrl Pts',(53.0456298946578,-3.65792139769576,331.712326945881));
#63116=CARTESIAN_POINT('Ctrl Pts',(53.0379792275201,-3.74796230611111,331.812508004076));
#63117=CARTESIAN_POINT('Ctrl Pts',(53.0303285603824,-3.83401746346419,331.916538921007));
#63118=CARTESIAN_POINT('Ctrl Pts',(53.0226778932446,-3.91573487042647,332.024062586843));
#63119=CARTESIAN_POINT('Ctrl Pts',(53.0150358707388,-3.99735994336243,332.131464759679));
#63120=CARTESIAN_POINT('Ctrl Pts',(53.0073938482329,-4.07465677894538,332.242351507227));
#63121=CARTESIAN_POINT('Ctrl Pts',(52.9997518257271,-4.14731185508742,332.356330686498));
#63122=CARTESIAN_POINT('Ctrl Pts',(52.9921146466571,-4.21992088318378,332.470237626928));
#63123=CARTESIAN_POINT('Ctrl Pts',(52.9844774675871,-4.28789378438795,332.587232763907));
#63124=CARTESIAN_POINT('Ctrl Pts',(52.9768402885171,-4.35095889711398,332.70689299462));
#63125=CARTESIAN_POINT('Ctrl Pts',(52.9692061827568,-4.41399863153953,332.82650507235));
#63126=CARTESIAN_POINT('Ctrl Pts',(52.9615720769966,-4.47213431715448,332.94877975483));
#63127=CARTESIAN_POINT('Ctrl Pts',(52.9539379712363,-4.52513931028059,333.073267718376));
#63128=CARTESIAN_POINT('Ctrl Pts',(52.9463051715254,-4.57813523526711,333.197734384413));
#63129=CARTESIAN_POINT('Ctrl Pts',(52.9386723718145,-4.62600205673172,333.324413206935));
#63130=CARTESIAN_POINT('Ctrl Pts',(52.9310395721036,-4.66856075493242,333.452833706415));
#63131=CARTESIAN_POINT('Ctrl Pts',(52.9234031308337,-4.71113975761084,333.581315474479));
#63132=CARTESIAN_POINT('Ctrl Pts',(52.9157666895637,-4.74840544637987,333.71154019753));
#63133=CARTESIAN_POINT('Ctrl Pts',(52.9081302482938,-4.78022829497211,333.843020955052));
#63134=CARTESIAN_POINT('Ctrl Pts',(52.9004921312646,-4.81205812684748,333.974530565031));
#63135=CARTESIAN_POINT('Ctrl Pts',(52.8928540142355,-4.83844265646304,334.107296363423));
#63136=CARTESIAN_POINT('Ctrl Pts',(52.8852158972064,-4.85930351266948,334.240821210611));
#63137=CARTESIAN_POINT('Ctrl Pts',(52.8775694218147,-4.88018719683203,334.374492173534));
#63138=CARTESIAN_POINT('Ctrl Pts',(52.8699229464229,-4.89553508175743,334.508923443894));
#63139=CARTESIAN_POINT('Ctrl Pts',(52.8622764710312,-4.90532067276581,334.643612346122));
#63140=CARTESIAN_POINT('Ctrl Pts',(52.8554567728702,-4.91404819408577,334.763737974177));
#63141=CARTESIAN_POINT('Ctrl Pts',(52.8486370747092,-4.91835196711398,334.884068288334));
#63142=CARTESIAN_POINT('Ctrl Pts',(52.8418173765482,-4.9182481654623,335.0042479909));
#63143=CARTESIAN_POINT('',(51.0918173764711,-4.91824913722187,334.99708680308));
#63144=CARTESIAN_POINT('Ctrl Pts',(52.8418173765087,-4.9182481654617,335.004247991597));
#63145=CARTESIAN_POINT('Ctrl Pts',(52.8301934007741,-4.91807123855823,335.209090773998));
#63146=CARTESIAN_POINT('Ctrl Pts',(52.8185694250394,-4.90509378189171,335.41340122439));
#63147=CARTESIAN_POINT('Ctrl Pts',(52.8069454493047,-4.87953275582671,335.615908391982));
#63148=CARTESIAN_POINT('Ctrl Pts',(52.801421132238,-4.86738482849455,335.712150317087));
#63149=CARTESIAN_POINT('Ctrl Pts',(52.7958968151712,-4.85239533518121,335.807985504501));
#63150=CARTESIAN_POINT('Ctrl Pts',(52.7903724981044,-4.83459084839709,335.903279796683));
#63151=CARTESIAN_POINT('Ctrl Pts',(52.7825974193259,-4.80953231434074,336.037399656186));
#63152=CARTESIAN_POINT('Ctrl Pts',(52.7748223405475,-4.77884888101143,336.170687910591));
#63153=CARTESIAN_POINT('Ctrl Pts',(52.7670472617691,-4.74260715552524,336.302635954847));
#63154=CARTESIAN_POINT('Ctrl Pts',(52.7592817507201,-4.70641002778952,336.434421628634));
#63155=CARTESIAN_POINT('Ctrl Pts',(52.7515162396711,-4.66466831973847,336.564870000422));
#63156=CARTESIAN_POINT('Ctrl Pts',(52.743750728622,-4.6174999601803,336.693480788269));
#63157=CARTESIAN_POINT('Ctrl Pts',(52.7359929170998,-4.57037836818793,336.821964058144));
#63158=CARTESIAN_POINT('Ctrl Pts',(52.7282351055777,-4.51784096598995,336.948613005293));
#63159=CARTESIAN_POINT('Ctrl Pts',(52.7204772940555,-4.46005588579636,337.072941040665));
#63160=CARTESIAN_POINT('Ctrl Pts',(52.7127253205324,-4.40231429070805,337.197175515248));
#63161=CARTESIAN_POINT('Ctrl Pts',(52.7049733470094,-4.33933304208548,337.319092201465));
#63162=CARTESIAN_POINT('Ctrl Pts',(52.6972213734864,-4.27132878681837,337.438223422371));
#63163=CARTESIAN_POINT('Ctrl Pts',(52.6894726829288,-4.20335333139382,337.557304191134));
#63164=CARTESIAN_POINT('Ctrl Pts',(52.6817239923712,-4.13035929364046,337.673601502065));
#63165=CARTESIAN_POINT('Ctrl Pts',(52.6739753018135,-4.05260966892441,337.786671479353));
#63166=CARTESIAN_POINT('Ctrl Pts',(52.6662282234357,-3.97487622066722,337.899717931488));
#63167=CARTESIAN_POINT('Ctrl Pts',(52.6584811450579,-3.89238937484226,338.009538063712));
#63168=CARTESIAN_POINT('Ctrl Pts',(52.65073406668,-3.80545571651025,338.115716587268));
#63169=CARTESIAN_POINT('Ctrl Pts',(52.6429869233742,-3.71852132959033,338.221896000703));
#63170=CARTESIAN_POINT('Ctrl Pts',(52.6352397800684,-3.62714030344766,338.32443344216));
#63171=CARTESIAN_POINT('Ctrl Pts',(52.6274926367626,-3.53165955001809,338.42294666702));
#63172=CARTESIAN_POINT('Ctrl Pts',(52.6197437517345,-3.43615733048816,338.521482039745));
#63173=CARTESIAN_POINT('Ctrl Pts',(52.6119948667064,-3.33655382156292,338.615991114941));
#63174=CARTESIAN_POINT('Ctrl Pts',(52.6042459816783,-3.23323253375071,338.706128768027));
#63175=CARTESIAN_POINT('Ctrl Pts',(52.5964888719036,-3.12980157965603,338.796362094149));
#63176=CARTESIAN_POINT('Ctrl Pts',(52.5887317621288,-3.02264525899864,338.882214472215));
#63177=CARTESIAN_POINT('Ctrl Pts',(52.5809746523541,-2.91218031503351,338.963380990421));
#63178=CARTESIAN_POINT('Ctrl Pts',(52.5732133974279,-2.80165634213445,339.044590881419));
#63179=CARTESIAN_POINT('Ctrl Pts',(52.5654521425018,-2.68782054721736,339.121109705219));
#63180=CARTESIAN_POINT('Ctrl Pts',(52.5576908875756,-2.57111750366757,339.192676692142));
#63181=CARTESIAN_POINT('Ctrl Pts',(52.5499172171709,-2.45422777328145,339.264358162922));
#63182=CARTESIAN_POINT('Ctrl Pts',(52.5421435467662,-2.33446197040156,339.331071777361));
#63183=CARTESIAN_POINT('Ctrl Pts',(52.5343698763616,-2.21228882774224,339.392603010192));
#63184=CARTESIAN_POINT('Ctrl Pts',(52.5269580721845,-2.09580287426769,339.451269949331));
#63185=CARTESIAN_POINT('Ctrl Pts',(52.5195462680075,-1.97712892258029,339.505226009569));
#63186=CARTESIAN_POINT('Ctrl Pts',(52.5121344638305,-1.85668726517371,339.554327114058));
#63187=CARTESIAN_POINT('Ctrl Pts',(52.5043593850521,-1.73034240335963,339.605834809942));
#63188=CARTESIAN_POINT('Ctrl Pts',(52.4965843062737,-1.60165290026027,339.652162378791));
#63189=CARTESIAN_POINT('Ctrl Pts',(52.4888092274952,-1.4710824976472,339.69309059657));
#63190=CARTESIAN_POINT('Ctrl Pts',(52.4810437164462,-1.34067277022698,339.733968449572));
#63191=CARTESIAN_POINT('Ctrl Pts',(52.4732782053972,-1.20838711803129,339.769460055852));
#63192=CARTESIAN_POINT('Ctrl Pts',(52.4655126943482,-1.07471005686374,339.799393852996));
#63193=CARTESIAN_POINT('Ctrl Pts',(52.457754882826,-0.941165536891718,339.829297970693));
#63194=CARTESIAN_POINT('Ctrl Pts',(52.4499970713038,-0.806232732373306,
339.853655160765));
#63195=CARTESIAN_POINT('Ctrl Pts',(52.4422392597816,-0.670411812406666,
339.872343487921));
#63196=CARTESIAN_POINT('Ctrl Pts',(52.4344872862586,-0.53469310198943,339.891017751518));
#63197=CARTESIAN_POINT('Ctrl Pts',(52.4267353127356,-0.39808799207893,339.904031590395));
#63198=CARTESIAN_POINT('Ctrl Pts',(52.4189833392126,-0.261107002257901,
339.911314100714));
#63199=CARTESIAN_POINT('Ctrl Pts',(52.411234648655,-0.124184023967295,339.918593526886));
#63200=CARTESIAN_POINT('Ctrl Pts',(52.4034859580974,0.0131141281146278,
339.920146431363));
#63201=CARTESIAN_POINT('Ctrl Pts',(52.3957372675398,0.150271867464594,339.915953765888));
#63202=CARTESIAN_POINT('Ctrl Pts',(52.387990189162,0.28740107000123,339.911761972732));
#63203=CARTESIAN_POINT('Ctrl Pts',(52.3802431107841,0.424389527468195,339.901826999323));
#63204=CARTESIAN_POINT('Ctrl Pts',(52.3724960324063,0.560722103922002,339.886181923002));
#63205=CARTESIAN_POINT('Ctrl Pts',(52.3647488891005,0.697055822974018,339.870536715561));
#63206=CARTESIAN_POINT('Ctrl Pts',(52.3570017457947,0.832733261723166,339.849181354318));
#63207=CARTESIAN_POINT('Ctrl Pts',(52.3492546024889,0.967245248560456,339.822200710426));
#63208=CARTESIAN_POINT('Ctrl Pts',(52.3415057174608,1.10178747654825,339.795214000713));
#63209=CARTESIAN_POINT('Ctrl Pts',(52.3337568324328,1.23516334807102,339.762599568629));
#63210=CARTESIAN_POINT('Ctrl Pts',(52.3260079474047,1.36687510096273,339.724493149627));
#63211=CARTESIAN_POINT('Ctrl Pts',(52.31825083763,1.49872665406979,339.686346284078));
#63212=CARTESIAN_POINT('Ctrl Pts',(52.3104937278552,1.62891018410178,339.642695895937));
#63213=CARTESIAN_POINT('Ctrl Pts',(52.3027366180805,1.75694376052957,339.593727428226));
#63214=CARTESIAN_POINT('Ctrl Pts',(52.2949753631543,1.88504575400688,339.544732793331));
#63215=CARTESIAN_POINT('Ctrl Pts',(52.2872141082282,2.01099514592363,339.490414571013));
#63216=CARTESIAN_POINT('Ctrl Pts',(52.279452853302,2.13433206532665,339.431005495079));
#63217=CARTESIAN_POINT('Ctrl Pts',(52.2716791828974,2.25786628360531,339.371501383985));
#63218=CARTESIAN_POINT('Ctrl Pts',(52.2639055124927,2.37877933335822,339.306890330051));
#63219=CARTESIAN_POINT('Ctrl Pts',(52.2561318420881,2.49663715754374,339.237450408686));
#63220=CARTESIAN_POINT('Ctrl Pts',(52.2487200379109,2.60900867165918,339.171242932366));
#63221=CARTESIAN_POINT('Ctrl Pts',(52.2413082337338,2.71860275858495,339.100646194786));
#63222=CARTESIAN_POINT('Ctrl Pts',(52.2338964295567,2.82507081664059,339.025935660622));
#63223=CARTESIAN_POINT('Ctrl Pts',(52.2261213507782,2.93675719137287,338.947563340627));
#63224=CARTESIAN_POINT('Ctrl Pts',(52.2183462719998,3.0453563067021,338.86441609778));
#63225=CARTESIAN_POINT('Ctrl Pts',(52.2105711932214,3.15043285518016,338.776765267726));
#63226=CARTESIAN_POINT('Ctrl Pts',(52.2028056821724,3.25538010027588,338.689222297599));
#63227=CARTESIAN_POINT('Ctrl Pts',(52.1950401711233,3.35681310612936,338.597187015143));
#63228=CARTESIAN_POINT('Ctrl Pts',(52.1872746600743,3.45432540294311,338.500974017767));
#63229=CARTESIAN_POINT('Ctrl Pts',(52.1795168485521,3.5517410160306,338.404856415859));
#63230=CARTESIAN_POINT('Ctrl Pts',(52.1717590370299,3.64524337976807,338.304569615038));
#63231=CARTESIAN_POINT('Ctrl Pts',(52.1640012255077,3.73445928596813,338.200468231985));
#63232=CARTESIAN_POINT('Ctrl Pts',(52.1562492519847,3.82360805436958,338.096445188525));
#63233=CARTESIAN_POINT('Ctrl Pts',(52.1484972784616,3.90847653249157,337.988613572209));
#63234=CARTESIAN_POINT('Ctrl Pts',(52.1407453049386,3.98872882434416,337.877364319711));
#63235=CARTESIAN_POINT('Ctrl Pts',(52.132996614381,4.06894712930346,337.766162181338));
#63236=CARTESIAN_POINT('Ctrl Pts',(52.1252479238234,4.14455290806584,337.651545601842));
#63237=CARTESIAN_POINT('Ctrl Pts',(52.1174992332658,4.21525112909324,337.533937840828));
#63238=CARTESIAN_POINT('Ctrl Pts',(52.1097521548879,4.28593464076531,337.41635454909));
#63239=CARTESIAN_POINT('Ctrl Pts',(52.1020050765101,4.35171242440333,337.295781648504));
#63240=CARTESIAN_POINT('Ctrl Pts',(52.0942579981323,4.41233352583294,337.172670227925));
#63241=CARTESIAN_POINT('Ctrl Pts',(52.0865108548265,4.47295513532572,337.049557775553));
#63242=CARTESIAN_POINT('Ctrl Pts',(52.0787637115206,4.52841980373728,336.923907111419));
#63243=CARTESIAN_POINT('Ctrl Pts',(52.0710165682148,4.5785233590557,336.796192337441));
#63244=CARTESIAN_POINT('Ctrl Pts',(52.0632676831867,4.62863817871705,336.66844885047));
#63245=CARTESIAN_POINT('Ctrl Pts',(52.0555187981587,4.6733893441656,336.538640694041));
#63246=CARTESIAN_POINT('Ctrl Pts',(52.0477699131306,4.71262163057042,336.407259901219));
#63247=CARTESIAN_POINT('Ctrl Pts',(52.0400128033558,4.7518955585294,336.275739659467));
#63248=CARTESIAN_POINT('Ctrl Pts',(52.0322556935811,4.78563879393154,336.142643822037));
#63249=CARTESIAN_POINT('Ctrl Pts',(52.0244985838063,4.81374647950684,336.008478008454));
#63250=CARTESIAN_POINT('Ctrl Pts',(52.0167373288802,4.8418691849306,335.87424050095));
#63251=CARTESIAN_POINT('Ctrl Pts',(52.008976073954,4.86435027589497,335.738932263399));
#63252=CARTESIAN_POINT('Ctrl Pts',(52.0012148190278,4.88113660066499,335.603065956715));
#63253=CARTESIAN_POINT('Ctrl Pts',(51.9934411486231,4.89794977808398,335.466982308219));
#63254=CARTESIAN_POINT('Ctrl Pts',(51.9856674782185,4.9090499536254,335.33033919645));
#63255=CARTESIAN_POINT('Ctrl Pts',(51.9778938078138,4.91443607366073,335.193652111794));
#63256=CARTESIAN_POINT('Ctrl Pts',(51.9704820036368,4.91957146851257,335.063327843813));
#63257=CARTESIAN_POINT('Ctrl Pts',(51.9630701994597,4.91951281470945,334.932963892487));
#63258=CARTESIAN_POINT('Ctrl Pts',(51.9556583952827,4.91430310800094,334.803002474147));
#63259=CARTESIAN_POINT('Ctrl Pts',(51.9478833165042,4.90883805804771,334.666671259558));
#63260=CARTESIAN_POINT('Ctrl Pts',(51.9401082377258,4.89768698038941,334.530352202525));
#63261=CARTESIAN_POINT('Ctrl Pts',(51.9323331589474,4.88084247712137,334.394558197654));
#63262=CARTESIAN_POINT('Ctrl Pts',(51.9245676478984,4.86401870208698,334.258931295952));
#63263=CARTESIAN_POINT('Ctrl Pts',(51.9168021368494,4.84151548927516,334.123828545031));
#63264=CARTESIAN_POINT('Ctrl Pts',(51.9090366258004,4.81337742622822,333.989762000726));
#63265=CARTESIAN_POINT('Ctrl Pts',(51.9012788142782,4.78526726215274,333.855828383791));
#63266=CARTESIAN_POINT('Ctrl Pts',(51.893521002756,4.75153344599989,333.722929308959));
#63267=CARTESIAN_POINT('Ctrl Pts',(51.8857631912338,4.71227221813807,333.591570518391));
#63268=CARTESIAN_POINT('Ctrl Pts',(51.8780112177108,4.67304053559524,333.46031057948));
#63269=CARTESIAN_POINT('Ctrl Pts',(51.8702592441877,4.62828983221271,333.330588990672));
#63270=CARTESIAN_POINT('Ctrl Pts',(51.8625072706647,4.57816708238549,333.202899772338));
#63271=CARTESIAN_POINT('Ctrl Pts',(51.8547585801071,4.52806555957258,333.075264630464));
#63272=CARTESIAN_POINT('Ctrl Pts',(51.8470098895495,4.47259665778465,332.949660510262));
#63273=CARTESIAN_POINT('Ctrl Pts',(51.8392611989919,4.41195664655668,332.826564560102));
#63274=CARTESIAN_POINT('Ctrl Pts',(51.8315141206141,4.35132925198956,332.703494221083));
#63275=CARTESIAN_POINT('Ctrl Pts',(51.8237670422362,4.28553306063243,332.582931364536));
#63276=CARTESIAN_POINT('Ctrl Pts',(51.8160199638584,4.21481159702181,332.465331133242));
#63277=CARTESIAN_POINT('Ctrl Pts',(51.8082728205526,4.1440895406972,332.347729916345));
#63278=CARTESIAN_POINT('Ctrl Pts',(51.8005256772468,4.06844233122693,332.233091709194));
#63279=CARTESIAN_POINT('Ctrl Pts',(51.792778533941,3.98815816183793,332.121844768143));
#63280=CARTESIAN_POINT('Ctrl Pts',(51.7850296489129,3.90785594286322,332.010572816418));
#63281=CARTESIAN_POINT('Ctrl Pts',(51.7772807638848,3.82291491823161,331.902693964833));
#63282=CARTESIAN_POINT('Ctrl Pts',(51.7695318788567,3.73366484798352,331.798605012587));
#63283=CARTESIAN_POINT('Ctrl Pts',(51.761774769082,3.64432004678869,331.694405579252));
#63284=CARTESIAN_POINT('Ctrl Pts',(51.7540176593073,3.55065731848177,331.594004378051));
#63285=CARTESIAN_POINT('Ctrl Pts',(51.7462605495326,3.45304510502089,331.497763205437));
#63286=CARTESIAN_POINT('Ctrl Pts',(51.7384992946064,3.35538073071417,331.401470604617));
#63287=CARTESIAN_POINT('Ctrl Pts',(51.7307380396802,3.25376295536853,331.309342724288));
#63288=CARTESIAN_POINT('Ctrl Pts',(51.722976784754,3.14859412302986,331.221701691115));
#63289=CARTESIAN_POINT('Ctrl Pts',(51.7152031143494,3.04325705483388,331.133920460851));
#63290=CARTESIAN_POINT('Ctrl Pts',(51.7074294439447,2.9343578889078,331.050640658068));
#63291=CARTESIAN_POINT('Ctrl Pts',(51.69965577354,2.82232954193554,330.972142130211));
#63292=CARTESIAN_POINT('Ctrl Pts',(51.692243969363,2.71551614146754,330.897297727712));
#63293=CARTESIAN_POINT('Ctrl Pts',(51.6848321651859,2.60585857266585,330.826799636602));
#63294=CARTESIAN_POINT('Ctrl Pts',(51.6774203610088,2.49375197214532,330.760851009469));
#63295=CARTESIAN_POINT('Ctrl Pts',(51.6696452822304,2.37615069318461,330.691670043669));
#63296=CARTESIAN_POINT('Ctrl Pts',(51.661870203452,2.25548260191611,330.627277159023));
#63297=CARTESIAN_POINT('Ctrl Pts',(51.6540951246735,2.13217499892654,330.567956133289));
#63298=CARTESIAN_POINT('Ctrl Pts',(51.6463296136245,2.00901913379259,330.508708105853));
#63299=CARTESIAN_POINT('Ctrl Pts',(51.6385641025755,1.88323056856601,330.454519686874));
#63300=CARTESIAN_POINT('Ctrl Pts',(51.6307985915265,1.75526403079943,330.40563048453));
#63301=CARTESIAN_POINT('Ctrl Pts',(51.6230407800043,1.6274243722277,330.356789755972));
#63302=CARTESIAN_POINT('Ctrl Pts',(51.6152829684821,1.49741140135767,330.313237926515));
#63303=CARTESIAN_POINT('Ctrl Pts',(51.6075251569599,1.36570248874796,330.275167751684));
#63304=CARTESIAN_POINT('Ctrl Pts',(51.5997731834369,1.2340926912719,330.237126225867));
#63305=CARTESIAN_POINT('Ctrl Pts',(51.5920212099139,1.10078986635988,330.204558251928));
#63306=CARTESIAN_POINT('Ctrl Pts',(51.5842692363909,0.966288982558887,330.177607578734));
#63307=CARTESIAN_POINT('Ctrl Pts',(51.5765205458332,0.831845059961858,330.150668319165));
#63308=CARTESIAN_POINT('Ctrl Pts',(51.5687718552756,0.696204470074705,330.129341705451));
#63309=CARTESIAN_POINT('Ctrl Pts',(51.561023164718,0.559874669850121,330.113720902715));
#63310=CARTESIAN_POINT('Ctrl Pts',(51.5532760863402,0.42357323417903,330.098103350018));
#63311=CARTESIAN_POINT('Ctrl Pts',(51.5455290079624,0.286583261484846,330.088189291458));
#63312=CARTESIAN_POINT('Ctrl Pts',(51.5377819295845,0.149419276142205,330.084020245931));
#63313=CARTESIAN_POINT('Ctrl Pts',(51.5300347862787,0.0122541412333472,
330.079851165464));
#63314=CARTESIAN_POINT('Ctrl Pts',(51.5222876429728,-0.12508461853898,330.081427205941));
#63315=CARTESIAN_POINT('Ctrl Pts',(51.514540499667,-0.262080915379637,330.088737773617));
#63316=CARTESIAN_POINT('Ctrl Pts',(51.5067916146389,-0.399108011896339,
330.096049984864));
#63317=CARTESIAN_POINT('Ctrl Pts',(51.4990427296108,-0.535792102031358,
330.109099267934));
#63318=CARTESIAN_POINT('Ctrl Pts',(51.4912938445827,-0.671621056794774,
330.12782305139));
#63319=CARTESIAN_POINT('Ctrl Pts',(51.483536734808,-0.807594181814151,330.146566708462));
#63320=CARTESIAN_POINT('Ctrl Pts',(51.4757796250333,-0.942709970522598,
330.170996843913));
#63321=CARTESIAN_POINT('Ctrl Pts',(51.4680225152585,-1.07646479548064,330.200999415858));
#63322=CARTESIAN_POINT('Ctrl Pts',(51.4602612603324,-1.21029109474039,330.231018020219));
#63323=CARTESIAN_POINT('Ctrl Pts',(51.4525000054062,-1.3427546038373,330.266614893085));
#63324=CARTESIAN_POINT('Ctrl Pts',(51.44473875048,-1.47336670813691,330.307626015986));
#63325=CARTESIAN_POINT('Ctrl Pts',(51.4369650800753,-1.60418774923711,330.348702743318));
#63326=CARTESIAN_POINT('Ctrl Pts',(51.4291914096707,-1.73315109940952,330.395210895327));
#63327=CARTESIAN_POINT('Ctrl Pts',(51.421417739266,-1.85978715290873,330.446937864648));
#63328=CARTESIAN_POINT('Ctrl Pts',(51.4140059350889,-1.9805282676512,330.496256931103));
#63329=CARTESIAN_POINT('Ctrl Pts',(51.4065941309118,-2.09915361910606,330.550319757871));
#63330=CARTESIAN_POINT('Ctrl Pts',(51.3991823267346,-2.21527854083245,330.608904003665));
#63331=CARTESIAN_POINT('Ctrl Pts',(51.3914072479562,-2.33709509089033,330.670359637859));
#63332=CARTESIAN_POINT('Ctrl Pts',(51.3836321691778,-2.45654486946993,330.736985325403));
#63333=CARTESIAN_POINT('Ctrl Pts',(51.3758570903994,-2.57315800493463,330.808575308545));
#63334=CARTESIAN_POINT('Ctrl Pts',(51.3680915793503,-2.68962764051227,330.880077195655));
#63335=CARTESIAN_POINT('Ctrl Pts',(51.3603260683013,-2.80326724848132,330.956531020895));
#63336=CARTESIAN_POINT('Ctrl Pts',(51.3525605572523,-2.91362925804211,331.037684059899));
#63337=CARTESIAN_POINT('Ctrl Pts',(51.3448027457301,-3.0238818433491,331.118756635428));
#63338=CARTESIAN_POINT('Ctrl Pts',(51.3370449342079,-3.13086298455721,331.204518922415));
#63339=CARTESIAN_POINT('Ctrl Pts',(51.3292871226857,-3.23415225683324,331.294673800848));
#63340=CARTESIAN_POINT('Ctrl Pts',(51.3215351491626,-3.33736380065632,331.384760834876));
#63341=CARTESIAN_POINT('Ctrl Pts',(51.3137831756397,-3.4368887122227,331.479233624788));
#63342=CARTESIAN_POINT('Ctrl Pts',(51.3060312021167,-3.53233825416323,331.577753731732));
#63343=CARTESIAN_POINT('Ctrl Pts',(51.298282511559,-3.62774737316614,331.676232115352));
#63344=CARTESIAN_POINT('Ctrl Pts',(51.2905338210014,-3.71908428386492,331.778754126752));
#63345=CARTESIAN_POINT('Ctrl Pts',(51.2827851304438,-3.80599602764457,331.884943451548));
#63346=CARTESIAN_POINT('Ctrl Pts',(51.275038052066,-3.89288968870991,331.991110682768));
#63347=CARTESIAN_POINT('Ctrl Pts',(51.2672909736881,-3.97535976676811,332.100943407404));
#63348=CARTESIAN_POINT('Ctrl Pts',(51.2595438953103,-4.05309290903067,332.214031419189));
#63349=CARTESIAN_POINT('Ctrl Pts',(51.2517967520045,-4.13082670277188,332.327120378761));
#63350=CARTESIAN_POINT('Ctrl Pts',(51.2440496086987,-4.20382326011985,332.443464357784));
#63351=CARTESIAN_POINT('Ctrl Pts',(51.2363024653929,-4.27181220486338,332.562623634134));
#63352=CARTESIAN_POINT('Ctrl Pts',(51.2285535803648,-4.33981643496509,332.68180970002));
#63353=CARTESIAN_POINT('Ctrl Pts',(51.2208046953367,-4.40281061854024,332.803811983279));
#63354=CARTESIAN_POINT('Ctrl Pts',(51.2130558103086,-4.46057023086444,332.928165962721));
#63355=CARTESIAN_POINT('Ctrl Pts',(51.2052987005339,-4.51839114983793,333.052651932762));
#63356=CARTESIAN_POINT('Ctrl Pts',(51.1975415907591,-4.57096623395574,333.179494230149));
#63357=CARTESIAN_POINT('Ctrl Pts',(51.1897844809844,-4.61811884176474,333.308207629218));
#63358=CARTESIAN_POINT('Ctrl Pts',(51.1820232260582,-4.66529664641974,333.436989808611));
#63359=CARTESIAN_POINT('Ctrl Pts',(51.1742619711321,-4.7070460821278,333.567644709851));
#63360=CARTESIAN_POINT('Ctrl Pts',(51.1665007162059,-4.74324065810402,333.699672686664));
#63361=CARTESIAN_POINT('Ctrl Pts',(51.1587270458012,-4.779493133606,333.831911865211));
#63362=CARTESIAN_POINT('Ctrl Pts',(51.1509533753965,-4.81017290506724,333.965528127372));
#63363=CARTESIAN_POINT('Ctrl Pts',(51.1431797049919,-4.83520462794207,334.100011517614));
#63364=CARTESIAN_POINT('Ctrl Pts',(51.1357679008148,-4.85907111809463,334.228234673684));
#63365=CARTESIAN_POINT('Ctrl Pts',(51.1283560966379,-4.8778035180788,334.35724576017));
#63366=CARTESIAN_POINT('Ctrl Pts',(51.1209442924608,-4.8913806343428,334.486600981228));
#63367=CARTESIAN_POINT('Ctrl Pts',(51.1112353204767,-4.90916575632966,334.656047743074));
#63368=CARTESIAN_POINT('Ctrl Pts',(51.1015263484927,-4.91814805570971,334.826434437093));
#63369=CARTESIAN_POINT('Ctrl Pts',(51.0918173765087,-4.91824913722148,334.997086802418));
#63370=CARTESIAN_POINT('',(49.3418173765595,-4.9182492637269,334.997308838587));
#63371=CARTESIAN_POINT('Ctrl Pts',(51.0918173764711,-4.91824913722187,334.99708680308));
#63372=CARTESIAN_POINT('Ctrl Pts',(51.0841469556418,-4.91832899506454,335.131908024081));
#63373=CARTESIAN_POINT('Ctrl Pts',(51.0764765348125,-4.91286100890517,335.266951588975));
#63374=CARTESIAN_POINT('Ctrl Pts',(51.0688061139833,-4.90181674892083,335.401715847956));
#63375=CARTESIAN_POINT('Ctrl Pts',(51.0611442022096,-4.89078474070522,335.536330608416));
#63376=CARTESIAN_POINT('Ctrl Pts',(51.053482290436,-4.87418879416588,335.670666282156));
#63377=CARTESIAN_POINT('Ctrl Pts',(51.0458203786623,-4.85205248533923,335.804219958726));
#63378=CARTESIAN_POINT('Ctrl Pts',(51.0381650213289,-4.82993511318494,335.937659385796));
#63379=CARTESIAN_POINT('Ctrl Pts',(51.0305096639954,-4.80228687237235,336.07031775213));
#63380=CARTESIAN_POINT('Ctrl Pts',(51.022854306662,-4.76918321498598,336.201696519258));
#63381=CARTESIAN_POINT('Ctrl Pts',(51.0152031031228,-4.73609751963295,336.333004000311));
#63382=CARTESIAN_POINT('Ctrl Pts',(51.0075518995837,-4.69756239229167,336.463032874332));
#63383=CARTESIAN_POINT('Ctrl Pts',(50.9999006960446,-4.65370443417213,336.591294473649));
#63384=CARTESIAN_POINT('Ctrl Pts',(50.992251590838,-4.60985850403989,336.719520897391));
#63385=CARTESIAN_POINT('Ctrl Pts',(50.9846024856314,-4.56069277513262,336.845980630099));
#63386=CARTESIAN_POINT('Ctrl Pts',(50.9769533804247,-4.50638366360705,336.97020032963));
#63387=CARTESIAN_POINT('Ctrl Pts',(50.9693046166191,-4.45207697604924,337.094414484889));
#63388=CARTESIAN_POINT('Ctrl Pts',(50.9616558528135,-4.39262752341957,337.216388437617));
#63389=CARTESIAN_POINT('Ctrl Pts',(50.9540070890078,-4.32825958614541,337.335669500901));
#63390=CARTESIAN_POINT('Ctrl Pts',(50.9463569101738,-4.26387974074317,337.454972631292));
#63391=CARTESIAN_POINT('Ctrl Pts',(50.9387067313398,-4.19457979238958,337.571581528133));
#63392=CARTESIAN_POINT('Ctrl Pts',(50.9310565525058,-4.12062935113851,337.685069238034));
#63393=CARTESIAN_POINT('Ctrl Pts',(50.9233986125228,-4.04660388675388,337.798672081847));
#63394=CARTESIAN_POINT('Ctrl Pts',(50.9157406725398,-3.96791872714121,337.909147077951));
#63395=CARTESIAN_POINT('Ctrl Pts',(50.9080827325569,-3.8848862990819,338.016097065034));
#63396=CARTESIAN_POINT('Ctrl Pts',(50.9004207899194,-3.80181047160636,338.123102952771));
#63397=CARTESIAN_POINT('Ctrl Pts',(50.8927588472818,-3.71438311033859,338.226579856244));
#63398=CARTESIAN_POINT('Ctrl Pts',(50.8850969046443,-3.62295524746866,338.326165711046));
#63399=CARTESIAN_POINT('Ctrl Pts',(50.8774230661438,-3.53138543452352,338.425906181949));
#63400=CARTESIAN_POINT('Ctrl Pts',(50.8697492276433,-3.43580299719714,338.521743253069));
#63401=CARTESIAN_POINT('Ctrl Pts',(50.8620753891428,-3.33659440678278,338.613353127931));
#63402=CARTESIAN_POINT('Ctrl Pts',(50.8556190121575,-3.25312535021489,338.690429012137));
#63403=CARTESIAN_POINT('Ctrl Pts',(50.8491626351722,-3.1670901464203,338.764513228407));
#63404=CARTESIAN_POINT('Ctrl Pts',(50.8427062581869,-3.07873491637792,338.835436660561));
#63405=CARTESIAN_POINT('Ctrl Pts',(50.8349311794085,-2.97233331132417,338.920846058663));
#63406=CARTESIAN_POINT('Ctrl Pts',(50.8271561006301,-2.86220677301116,339.001959420094));
#63407=CARTESIAN_POINT('Ctrl Pts',(50.8193810218516,-2.74873723671036,339.078434340041));
#63408=CARTESIAN_POINT('Ctrl Pts',(50.8116155108026,-2.63540733189781,339.15481515273));
#63409=CARTESIAN_POINT('Ctrl Pts',(50.8038499997536,-2.51874293535591,339.226568664648));
#63410=CARTESIAN_POINT('Ctrl Pts',(50.7960844887046,-2.39915948944647,339.293392226049));
#63411=CARTESIAN_POINT('Ctrl Pts',(50.7883266771824,-2.27969461087205,339.360149531694));
#63412=CARTESIAN_POINT('Ctrl Pts',(50.7805688656602,-2.15731678165935,339.421986424894));
#63413=CARTESIAN_POINT('Ctrl Pts',(50.772811054138,-2.03247060399064,339.478643355573));
#63414=CARTESIAN_POINT('Ctrl Pts',(50.765059080615,-1.9077183770299,339.535257650114));
#63415=CARTESIAN_POINT('Ctrl Pts',(50.7573071070921,-1.78050185340068,339.586699580206));
#63416=CARTESIAN_POINT('Ctrl Pts',(50.7495551335691,-1.65129011324519,339.632755554138));
#63417=CARTESIAN_POINT('Ctrl Pts',(50.7418064430115,-1.52213309433811,339.678792023338));
#63418=CARTESIAN_POINT('Ctrl Pts',(50.7340577524539,-1.39098290691982,339.719446942075));
#63419=CARTESIAN_POINT('Ctrl Pts',(50.7263090618962,-1.2583282801843,339.754554974105));
#63420=CARTESIAN_POINT('Ctrl Pts',(50.7185619835184,-1.12570125335173,339.789655701616));
#63421=CARTESIAN_POINT('Ctrl Pts',(50.7108149051406,-0.991570787430775,
339.819211738016));
#63422=CARTESIAN_POINT('Ctrl Pts',(50.7030678267627,-0.856440049436659,
339.843107835287));
#63423=CARTESIAN_POINT('Ctrl Pts',(50.6953206834569,-0.721308178916805,
339.867004132831));
#63424=CARTESIAN_POINT('Ctrl Pts',(50.6875735401511,-0.585176404505199,
339.885240328567));
#63425=CARTESIAN_POINT('Ctrl Pts',(50.6798263968453,-0.44855695174069,339.897752517589));
#63426=CARTESIAN_POINT('Ctrl Pts',(50.6720775118172,-0.311906784022686,
339.910267519616));
#63427=CARTESIAN_POINT('Ctrl Pts',(50.6643286267892,-0.174769108948748,
339.917055918543));
#63428=CARTESIAN_POINT('Ctrl Pts',(50.6565797417611,-0.0376597265694707,
339.918105814996));
#63429=CARTESIAN_POINT('Ctrl Pts',(50.6488226319864,0.0995951851247759,
339.91915682582));
#63430=CARTESIAN_POINT('Ctrl Pts',(50.6410655222116,0.236821352656112,339.914457164016));
#63431=CARTESIAN_POINT('Ctrl Pts',(50.6333084124369,0.373503969883856,339.904047088577));
#63432=CARTESIAN_POINT('Ctrl Pts',(50.6255471575107,0.510259625931983,339.893631450327));
#63433=CARTESIAN_POINT('Ctrl Pts',(50.6177859025845,0.646470764952424,339.877499364075));
#63434=CARTESIAN_POINT('Ctrl Pts',(50.6100246476584,0.781630233297696,339.855742707444));
#63435=CARTESIAN_POINT('Ctrl Pts',(50.6022509772537,0.917005912743952,339.833951247253));
#63436=CARTESIAN_POINT('Ctrl Pts',(50.5944773068491,1.05132617655124,339.806517315313));
#63437=CARTESIAN_POINT('Ctrl Pts',(50.5867036364444,1.18409567793988,339.773583610662));
#63438=CARTESIAN_POINT('Ctrl Pts',(50.5792918322673,1.31068472709719,339.742182977887));
#63439=CARTESIAN_POINT('Ctrl Pts',(50.5718800280901,1.43586386437549,339.705783158708));
#63440=CARTESIAN_POINT('Ctrl Pts',(50.564468223913,1.55922039229397,339.66454872745));
#63441=CARTESIAN_POINT('Ctrl Pts',(50.5566931451346,1.68862299110521,339.621293273885));
#63442=CARTESIAN_POINT('Ctrl Pts',(50.5489180663561,1.81642873615065,339.572580612525));
#63443=CARTESIAN_POINT('Ctrl Pts',(50.5411429875777,1.94214300482772,339.518546625996));
#63444=CARTESIAN_POINT('Ctrl Pts',(50.5333774765287,2.06770257409373,339.464579131728));
#63445=CARTESIAN_POINT('Ctrl Pts',(50.5256119654797,2.1911754322309,339.405303494265));
#63446=CARTESIAN_POINT('Ctrl Pts',(50.5178464544306,2.31208225490912,339.340905286808));
#63447=CARTESIAN_POINT('Ctrl Pts',(50.5100886429084,2.43286919812064,339.276570930361));
#63448=CARTESIAN_POINT('Ctrl Pts',(50.5023308313862,2.5510948262701,339.20712429407));
#63449=CARTESIAN_POINT('Ctrl Pts',(50.494573019864,2.66630027840952,339.132798795956));
#63450=CARTESIAN_POINT('Ctrl Pts',(50.486821046341,2.78141903479267,339.058529230136));
#63451=CARTESIAN_POINT('Ctrl Pts',(50.479069072818,2.8935218118911,338.979388321481));
#63452=CARTESIAN_POINT('Ctrl Pts',(50.471317099295,3.00217514969789,338.895654942758));
#63453=CARTESIAN_POINT('Ctrl Pts',(50.4635684087374,3.11078247275177,338.811957025171));
#63454=CARTESIAN_POINT('Ctrl Pts',(50.4558197181798,3.21594295306105,338.723670743912));
#63455=CARTESIAN_POINT('Ctrl Pts',(50.4480710276222,3.31725307643952,338.631117608857));
#63456=CARTESIAN_POINT('Ctrl Pts',(50.4403239492443,3.41854212140067,338.538583730255));
#63457=CARTESIAN_POINT('Ctrl Pts',(50.4325768708665,3.51598211447419,338.441785027135));
#63458=CARTESIAN_POINT('Ctrl Pts',(50.4248297924887,3.60920384859934,338.34108225606));
#63459=CARTESIAN_POINT('Ctrl Pts',(50.4170826491828,3.70242636401235,338.240378640998));
#63460=CARTESIAN_POINT('Ctrl Pts',(50.409335505877,3.79143028443259,338.135771179556));
#63461=CARTESIAN_POINT('Ctrl Pts',(50.4015883625712,3.87588467622995,338.027656030507));
#63462=CARTESIAN_POINT('Ctrl Pts',(50.3938394775432,3.96035805516715,337.919516574878));
#63463=CARTESIAN_POINT('Ctrl Pts',(50.3860905925151,4.04027962958914,337.807868170382));
#63464=CARTESIAN_POINT('Ctrl Pts',(50.378341707487,4.1153602640547,337.693138124854));
#63465=CARTESIAN_POINT('Ctrl Pts',(50.3705845977123,4.19052058988183,337.578286303668));
#63466=CARTESIAN_POINT('Ctrl Pts',(50.3628274879376,4.26082949729539,337.460346635131));
#63467=CARTESIAN_POINT('Ctrl Pts',(50.3550703781628,4.32604224979836,337.339773817158));
#63468=CARTESIAN_POINT('Ctrl Pts',(50.3473091232367,4.39128984991135,337.219136568927));
#63469=CARTESIAN_POINT('Ctrl Pts',(50.3395478683104,4.45143569753717,337.095863718657));
#63470=CARTESIAN_POINT('Ctrl Pts',(50.3317866133843,4.50628260458853,336.970431462925));
#63471=CARTESIAN_POINT('Ctrl Pts',(50.3240129429796,4.5612172488165,336.844798556461));
#63472=CARTESIAN_POINT('Ctrl Pts',(50.3162392725749,4.61083587221203,336.716999706297));
#63473=CARTESIAN_POINT('Ctrl Pts',(50.3084656021702,4.65499041287568,336.587528682744));
#63474=CARTESIAN_POINT('Ctrl Pts',(50.3010537979931,4.69708954904838,336.464084566487));
#63475=CARTESIAN_POINT('Ctrl Pts',(50.2936419938161,4.7342217785034,336.339120728592));
#63476=CARTESIAN_POINT('Ctrl Pts',(50.286230189639,4.76630216101283,336.213073275785));
#63477=CARTESIAN_POINT('Ctrl Pts',(50.2784551108606,4.79995489863162,336.08084786184));
#63478=CARTESIAN_POINT('Ctrl Pts',(50.2706800320822,4.8281544045909,335.947012068022));
#63479=CARTESIAN_POINT('Ctrl Pts',(50.2629049533037,4.85074727681879,335.812055366915));
#63480=CARTESIAN_POINT('Ctrl Pts',(50.2551394422547,4.87331234707906,335.67726473862));
#63481=CARTESIAN_POINT('Ctrl Pts',(50.2473739312057,4.89028444735542,335.541356329369));
#63482=CARTESIAN_POINT('Ctrl Pts',(50.2396084201567,4.90156024021243,335.404833637521));
#63483=CARTESIAN_POINT('Ctrl Pts',(50.2318506086345,4.91282485308801,335.26844630832));
#63484=CARTESIAN_POINT('Ctrl Pts',(50.2240927971123,4.91840436622867,335.131446295632));
#63485=CARTESIAN_POINT('Ctrl Pts',(50.2163349855901,4.91824674983992,334.994345781301));
#63486=CARTESIAN_POINT('Ctrl Pts',(50.2085830120671,4.91808925206249,334.857348439456));
#63487=CARTESIAN_POINT('Ctrl Pts',(50.2008310385441,4.91220321872094,334.720251135808));
#63488=CARTESIAN_POINT('Ctrl Pts',(50.1930790650211,4.90058858979415,334.583569290182));
#63489=CARTESIAN_POINT('Ctrl Pts',(50.1853303744635,4.88897887966959,334.446945329399));
#63490=CARTESIAN_POINT('Ctrl Pts',(50.1775816839058,4.87164543225606,334.310736865351));
#63491=CARTESIAN_POINT('Ctrl Pts',(50.1698329933482,4.8486402473879,334.17545720917));
#63492=CARTESIAN_POINT('Ctrl Pts',(50.1620859149704,4.8256398489406,334.040205699051));
#63493=CARTESIAN_POINT('Ctrl Pts',(50.1543388365926,4.79697012573504,333.905882997518));
#63494=CARTESIAN_POINT('Ctrl Pts',(50.1465917582148,4.76273464653511,333.77299480474));
#63495=CARTESIAN_POINT('Ctrl Pts',(50.138844614909,4.72849888040889,333.640105498232));
#63496=CARTESIAN_POINT('Ctrl Pts',(50.1310974716031,4.68869736276388,333.508651102975));
#63497=CARTESIAN_POINT('Ctrl Pts',(50.1233503282973,4.64348414478651,333.37912429236));
#63498=CARTESIAN_POINT('Ctrl Pts',(50.1156014432692,4.59826076191777,333.249568361369));
#63499=CARTESIAN_POINT('Ctrl Pts',(50.1078525582411,4.54762338648169,333.121941246328));
#63500=CARTESIAN_POINT('Ctrl Pts',(50.100103673213,4.49177488297321,332.996717328186));
#63501=CARTESIAN_POINT('Ctrl Pts',(50.0923465634383,4.43586710128616,332.871360496083));
#63502=CARTESIAN_POINT('Ctrl Pts',(50.0845894536636,4.37473730200621,332.748412313842));
#63503=CARTESIAN_POINT('Ctrl Pts',(50.0768323438888,4.308635409351,332.628324648737));
#63504=CARTESIAN_POINT('Ctrl Pts',(50.0690710889627,4.24249819395783,332.508172812624));
#63505=CARTESIAN_POINT('Ctrl Pts',(50.0613098340365,4.17138379357379,332.390884873525));
#63506=CARTESIAN_POINT('Ctrl Pts',(50.0535485791103,4.09558594226896,332.2768843484));
#63507=CARTESIAN_POINT('Ctrl Pts',(50.0457749087057,4.0196668391046,332.162701459588));
#63508=CARTESIAN_POINT('Ctrl Pts',(50.038001238301,3.93904954376794,332.051816809687));
#63509=CARTESIAN_POINT('Ctrl Pts',(50.0302275678964,3.85406915345952,331.944622114557));
#63510=CARTESIAN_POINT('Ctrl Pts',(50.0228157637193,3.77304462076529,331.842417358276));
#63511=CARTESIAN_POINT('Ctrl Pts',(50.0154039595422,3.6880542434981,331.743566971237));
#63512=CARTESIAN_POINT('Ctrl Pts',(50.0079921553652,3.59941878707636,331.648378383865));
#63513=CARTESIAN_POINT('Ctrl Pts',(50.0002170765867,3.50643904290366,331.548524320274));
#63514=CARTESIAN_POINT('Ctrl Pts',(49.9924419978083,3.40915403938212,331.452384526571));
#63515=CARTESIAN_POINT('Ctrl Pts',(49.9846669190299,3.30789236978766,331.360352883534));
#63516=CARTESIAN_POINT('Ctrl Pts',(49.9769014079809,3.20675530912421,331.268434491293));
#63517=CARTESIAN_POINT('Ctrl Pts',(49.9691358969318,3.10165160562392,331.180614451417));
#63518=CARTESIAN_POINT('Ctrl Pts',(49.9613703858828,2.99294873998521,331.097252134416));
#63519=CARTESIAN_POINT('Ctrl Pts',(49.9536125743606,2.88435365355442,331.013972471395));
#63520=CARTESIAN_POINT('Ctrl Pts',(49.9458547628384,2.77216681483068,330.935141971837));
#63521=CARTESIAN_POINT('Ctrl Pts',(49.9380969513163,2.6567907721474,330.861081559691));
#63522=CARTESIAN_POINT('Ctrl Pts',(49.9303449777932,2.54150155359495,330.787076880353));
#63523=CARTESIAN_POINT('Ctrl Pts',(49.9225930042703,2.4230282357331,330.717835353718));
#63524=CARTESIAN_POINT('Ctrl Pts',(49.9148410307473,2.30180421360705,330.653635953499));
#63525=CARTESIAN_POINT('Ctrl Pts',(49.9070923401896,2.18063152992625,330.589463741763));
#63526=CARTESIAN_POINT('Ctrl Pts',(49.899343649632,2.05671080363995,330.53032959195));
#63527=CARTESIAN_POINT('Ctrl Pts',(49.8915949590744,1.93050182912259,330.476467558395));
#63528=CARTESIAN_POINT('Ctrl Pts',(49.8838478806965,1.80431911343667,330.422616731286));
#63529=CARTESIAN_POINT('Ctrl Pts',(49.8761008023187,1.67584945577339,330.374035991936));
#63530=CARTESIAN_POINT('Ctrl Pts',(49.8683537239409,1.54557415719535,330.330911910543));
#63531=CARTESIAN_POINT('Ctrl Pts',(49.8606065806351,1.41529776678448,330.287787467728));
#63532=CARTESIAN_POINT('Ctrl Pts',(49.8528594373292,1.28321607634723,330.250119896918));
#63533=CARTESIAN_POINT('Ctrl Pts',(49.8451122940234,1.14982675138656,330.218046267027));
#63534=CARTESIAN_POINT('Ctrl Pts',(49.8373634089953,1.01640743767406,330.185965426303));
#63535=CARTESIAN_POINT('Ctrl Pts',(49.8296145239672,0.881680284410798,330.159481120417));
#63536=CARTESIAN_POINT('Ctrl Pts',(49.8218656389391,0.74615399027515,330.138679471039));
#63537=CARTESIAN_POINT('Ctrl Pts',(49.8141085291644,0.610483847130658,330.117855742576));
#63538=CARTESIAN_POINT('Ctrl Pts',(49.8063514193896,0.474013255682081,330.102726778761));
#63539=CARTESIAN_POINT('Ctrl Pts',(49.7985943096149,0.337257449096062,330.0933269443));
#63540=CARTESIAN_POINT('Ctrl Pts',(49.7908330546887,0.200428564579514,330.083922086868));
#63541=CARTESIAN_POINT('Ctrl Pts',(49.7830717997626,0.063314551771338,330.080252469483));
#63542=CARTESIAN_POINT('Ctrl Pts',(49.7753105448364,-0.0735694885215804,
330.082300274228));
#63543=CARTESIAN_POINT('Ctrl Pts',(49.7675368744317,-0.21067249866847,330.084351354793));
#63544=CARTESIAN_POINT('Ctrl Pts',(49.7597632040271,-0.347544410716231,
330.092138111715));
#63545=CARTESIAN_POINT('Ctrl Pts',(49.7519895336224,-0.483674482119245,
330.105590734537));
#63546=CARTESIAN_POINT('Ctrl Pts',(49.7445777294453,-0.613467665948094,
330.118417134531));
#63547=CARTESIAN_POINT('Ctrl Pts',(49.7371659252682,-0.742586235176362,
330.136393739505));
#63548=CARTESIAN_POINT('Ctrl Pts',(49.729754121091,-0.870598080429284,330.159417179218));
#63549=CARTESIAN_POINT('Ctrl Pts',(49.7219790423126,-1.00488416754517,330.183569066294));
#63550=CARTESIAN_POINT('Ctrl Pts',(49.7142039635341,-1.13837666874033,330.213351342367));
#63551=CARTESIAN_POINT('Ctrl Pts',(49.7064288847557,-1.27056654059029,330.248700837831));
#63552=CARTESIAN_POINT('Ctrl Pts',(49.6986633737067,-1.40259374438759,330.284006833489));
#63553=CARTESIAN_POINT('Ctrl Pts',(49.6908978626577,-1.53332113429082,330.324866317363));
#63554=CARTESIAN_POINT('Ctrl Pts',(49.6831323516087,-1.66224764308061,330.371164743094));
#63555=CARTESIAN_POINT('Ctrl Pts',(49.6753745400865,-1.79104632086087,330.417417263802));
#63556=CARTESIAN_POINT('Ctrl Pts',(49.6676167285643,-1.91804730542709,330.469097863282));
#63557=CARTESIAN_POINT('Ctrl Pts',(49.6598589170421,-2.04276288298187,330.526041700417));
#63558=CARTESIAN_POINT('Ctrl Pts',(49.6521069435191,-2.16738460810976,330.582942685508));
#63559=CARTESIAN_POINT('Ctrl Pts',(49.6443549699961,-2.28972399535329,330.645098862875));
#63560=CARTESIAN_POINT('Ctrl Pts',(49.6366029964731,-2.40931191483704,330.712296750063));
#63561=CARTESIAN_POINT('Ctrl Pts',(49.6288543059155,-2.52884918876582,330.779466178905));
#63562=CARTESIAN_POINT('Ctrl Pts',(49.6211056153578,-2.64563697247861,330.851672879791));
#63563=CARTESIAN_POINT('Ctrl Pts',(49.6133569248002,-2.75922962357171,330.928656862053));
#63564=CARTESIAN_POINT('Ctrl Pts',(49.6056098464224,-2.87279864076539,331.005624827156));
#63565=CARTESIAN_POINT('Ctrl Pts',(49.5978627680445,-2.98317352425808,331.087367877441));
#63566=CARTESIAN_POINT('Ctrl Pts',(49.5901156896667,-3.08993692356965,331.173582240416));
#63567=CARTESIAN_POINT('Ctrl Pts',(49.5823685463608,-3.1967012176614,331.25979732595));
#63568=CARTESIAN_POINT('Ctrl Pts',(49.574621403055,-3.29985366309907,331.350483553349));
#63569=CARTESIAN_POINT('Ctrl Pts',(49.5668742597492,-3.39900968034968,331.445296600926));
#63570=CARTESIAN_POINT('Ctrl Pts',(49.5591253747211,-3.49818798997778,331.540130964489));
#63571=CARTESIAN_POINT('Ctrl Pts',(49.551376489693,-3.59336780108802,331.639093724362));
#63572=CARTESIAN_POINT('Ctrl Pts',(49.5436276046649,-3.68420140608735,331.741803710351));
#63573=CARTESIAN_POINT('Ctrl Pts',(49.5358704948902,-3.77513142281352,331.84462271378));
#63574=CARTESIAN_POINT('Ctrl Pts',(49.5281133851154,-3.86170575896089,331.951196595182));
#63575=CARTESIAN_POINT('Ctrl Pts',(49.5203562753407,-3.943616694286,332.061110680708));
#63576=CARTESIAN_POINT('Ctrl Pts',(49.5125950204145,-4.0255714001959,332.171083500807));
#63577=CARTESIAN_POINT('Ctrl Pts',(49.5048337654884,-4.10285751967344,332.284399758847));
#63578=CARTESIAN_POINT('Ctrl Pts',(49.4970725105622,-4.17521128558254,332.400616653272));
#63579=CARTESIAN_POINT('Ctrl Pts',(49.4892988401575,-4.24768079393711,332.517019456854));
#63580=CARTESIAN_POINT('Ctrl Pts',(49.4815251697528,-4.31520198923567,332.636331828704));
#63581=CARTESIAN_POINT('Ctrl Pts',(49.4737514993482,-4.3775571844831,332.758086496075));
#63582=CARTESIAN_POINT('Ctrl Pts',(49.4663396951712,-4.43700973038937,332.874173454387));
#63583=CARTESIAN_POINT('Ctrl Pts',(49.4589278909942,-4.49176628638325,332.992480186322));
#63584=CARTESIAN_POINT('Ctrl Pts',(49.4515160868172,-4.54167993952892,333.112587382319));
#63585=CARTESIAN_POINT('Ctrl Pts',(49.442374527629,-4.60324236125915,333.260725003728));
#63586=CARTESIAN_POINT('Ctrl Pts',(49.4332329684409,-4.65761130890345,333.412019090102));
#63587=CARTESIAN_POINT('Ctrl Pts',(49.4240914092527,-4.70449014120338,333.565790958814));
#63588=CARTESIAN_POINT('Ctrl Pts',(49.4154417871895,-4.74884627059188,333.711287861579));
#63589=CARTESIAN_POINT('Ctrl Pts',(49.4067921651262,-4.7864970205464,333.859002619526));
#63590=CARTESIAN_POINT('Ctrl Pts',(49.3981425430629,-4.81723850715545,334.00833663591));
#63591=CARTESIAN_POINT('Ctrl Pts',(49.389518895868,-4.847887676891,334.157222201323));
#63592=CARTESIAN_POINT('Ctrl Pts',(49.3808952486729,-4.87166890175579,334.307717107534));
#63593=CARTESIAN_POINT('Ctrl Pts',(49.372271601478,-4.88842790078164,334.459208245847));
#63594=CARTESIAN_POINT('Ctrl Pts',(49.3636874533892,-4.90511013814649,334.610005505524));
#63595=CARTESIAN_POINT('Ctrl Pts',(49.3551033053004,-4.91483423476958,334.761789673102));
#63596=CARTESIAN_POINT('Ctrl Pts',(49.3465191572117,-4.91749699019781,334.913939475394));
#63597=CARTESIAN_POINT('Ctrl Pts',(49.3449518969943,-4.91798314567977,334.941718391805));
#63598=CARTESIAN_POINT('Ctrl Pts',(49.3433846367768,-4.91823405249636,334.969509456849));
#63599=CARTESIAN_POINT('Ctrl Pts',(49.3418173765594,-4.91824926372691,334.997308838587));
#63600=CARTESIAN_POINT('',(47.5918173764616,-4.91824832477837,335.004059349057));
#63601=CARTESIAN_POINT('Ctrl Pts',(49.3418173765087,-4.9182492637274,334.997308839488));
#63602=CARTESIAN_POINT('Ctrl Pts',(49.3339770743027,-4.918325358688,335.136376718293));
#63603=CARTESIAN_POINT('Ctrl Pts',(49.3261367720966,-4.91249870650781,335.275447231013));
#63604=CARTESIAN_POINT('Ctrl Pts',(49.3182964698906,-4.90079520016747,335.413992111659));
#63605=CARTESIAN_POINT('Ctrl Pts',(49.3104544424886,-4.88908911856388,335.552567478));
#63606=CARTESIAN_POINT('Ctrl Pts',(49.3026124150866,-4.87150363858987,335.690616605482));
#63607=CARTESIAN_POINT('Ctrl Pts',(49.2947703876846,-4.84811653661624,335.82761652345));
#63608=CARTESIAN_POINT('Ctrl Pts',(49.2869250969572,-4.82471970250068,335.964673451588));
#63609=CARTESIAN_POINT('Ctrl Pts',(49.2790798062298,-4.79551650137673,336.100679928484));
#63610=CARTESIAN_POINT('Ctrl Pts',(49.2712345155024,-4.7606357602937,336.235123564795));
#63611=CARTESIAN_POINT('Ctrl Pts',(49.2630714769224,-4.72434228882767,336.375012401063));
#63612=CARTESIAN_POINT('Ctrl Pts',(49.2549084383425,-4.68190184646951,336.513208706157));
#63613=CARTESIAN_POINT('Ctrl Pts',(49.2467453997626,-4.63351621607897,336.649154491803));
#63614=CARTESIAN_POINT('Ctrl Pts',(49.2388840795037,-4.58691899217707,336.780075514452));
#63615=CARTESIAN_POINT('Ctrl Pts',(49.2310227592448,-4.53480843673019,336.908909094979));
#63616=CARTESIAN_POINT('Ctrl Pts',(49.2231614389859,-4.47741306156182,337.035179436476));
#63617=CARTESIAN_POINT('Ctrl Pts',(49.2152934719634,-4.41996915847789,337.161556539824));
#63618=CARTESIAN_POINT('Ctrl Pts',(49.2074255049411,-4.35723170070286,337.285365749583));
#63619=CARTESIAN_POINT('Ctrl Pts',(49.1995575379187,-4.28947437167885,337.406157242827));
#63620=CARTESIAN_POINT('Ctrl Pts',(49.1916774945105,-4.22161304328106,337.527134136527));
#63621=CARTESIAN_POINT('Ctrl Pts',(49.1837974511023,-4.14871665890939,337.645083747083));
#63622=CARTESIAN_POINT('Ctrl Pts',(49.1759174076941,-4.07110155546219,337.759586053671));
#63623=CARTESIAN_POINT('Ctrl Pts',(49.1750376226438,-4.0624360438459,337.772369919487));
#63624=CARTESIAN_POINT('Ctrl Pts',(49.1741578375935,-4.05371175306366,337.785110849596));
#63625=CARTESIAN_POINT('Ctrl Pts',(49.1732780525432,-4.04492915320926,337.797808286502));
#63626=CARTESIAN_POINT('Ctrl Pts',(49.1655029737647,-3.96731314265758,337.910021573363));
#63627=CARTESIAN_POINT('Ctrl Pts',(49.1577278949863,-3.8849014615822,338.019179929276));
#63628=CARTESIAN_POINT('Ctrl Pts',(49.1499528162079,-3.7979624986255,338.124846223662));
#63629=CARTESIAN_POINT('Ctrl Pts',(49.1421873051589,-3.71113051959753,338.230382488945));
#63630=CARTESIAN_POINT('Ctrl Pts',(49.1344217941098,-3.61978258956768,338.33243494395));
#63631=CARTESIAN_POINT('Ctrl Pts',(49.1266562830608,-3.52423055277304,338.430595002824));
#63632=CARTESIAN_POINT('Ctrl Pts',(49.1188984715386,-3.42877325610114,338.528657735714));
#63633=CARTESIAN_POINT('Ctrl Pts',(49.1111406600165,-3.32912041887219,338.622835474462));
#63634=CARTESIAN_POINT('Ctrl Pts',(49.1033828484943,-3.22562412838877,338.712752623709));
#63635=CARTESIAN_POINT('Ctrl Pts',(49.0956308749713,-3.12220572214578,338.802602107449));
#63636=CARTESIAN_POINT('Ctrl Pts',(49.0878789014482,-3.01494991355094,338.888197128208));
#63637=CARTESIAN_POINT('Ctrl Pts',(49.0801269279252,-2.90424536113982,338.969199156605));
#63638=CARTESIAN_POINT('Ctrl Pts',(49.0723782373676,-2.79358769217252,339.050166880595));
#63639=CARTESIAN_POINT('Ctrl Pts',(49.0646295468099,-2.67948449910283,339.126545250627));
#63640=CARTESIAN_POINT('Ctrl Pts',(49.0568808562523,-2.56235703872575,339.198036382476));
#63641=CARTESIAN_POINT('Ctrl Pts',(49.0491337778745,-2.44525394769507,339.269512639998));
#63642=CARTESIAN_POINT('Ctrl Pts',(49.0413866994967,-2.32512817435458,339.336103478371));
#63643=CARTESIAN_POINT('Ctrl Pts',(49.0336396211189,-2.20242910188921,339.397554901721));
#63644=CARTESIAN_POINT('Ctrl Pts',(49.0258924778131,-2.07972900108753,339.459006840094));
#63645=CARTESIAN_POINT('Ctrl Pts',(49.0181453345072,-1.95445590763695,339.515319102494));
#63646=CARTESIAN_POINT('Ctrl Pts',(49.0103981912014,-1.82708253330984,339.566284318675));
#63647=CARTESIAN_POINT('Ctrl Pts',(49.0026493061733,-1.69968052274406,339.617260992918));
#63648=CARTESIAN_POINT('Ctrl Pts',(48.9949004211453,-1.57017765453207,339.662888083659));
#63649=CARTESIAN_POINT('Ctrl Pts',(48.9871515361172,-1.43906490185854,339.703007045576));
#63650=CARTESIAN_POINT('Ctrl Pts',(48.9793944263425,-1.30781298475477,339.743168590174));
#63651=CARTESIAN_POINT('Ctrl Pts',(48.9716373165678,-1.17494814416339,339.777810212697));
#63652=CARTESIAN_POINT('Ctrl Pts',(48.963880206793,-1.04097527968342,339.806823642447));
#63653=CARTESIAN_POINT('Ctrl Pts',(48.9561189518669,-0.906930824388212,
339.835852576047));
#63654=CARTESIAN_POINT('Ctrl Pts',(48.9483576969407,-0.771777550358167,
339.859247257473));
#63655=CARTESIAN_POINT('Ctrl Pts',(48.9405964420145,-0.636027747730289,
339.876951072814));
#63656=CARTESIAN_POINT('Ctrl Pts',(48.9328227716099,-0.500060789658963,
339.894683208489));
#63657=CARTESIAN_POINT('Ctrl Pts',(48.9250491012052,-0.363495785686038,
339.906706252232));
#63658=CARTESIAN_POINT('Ctrl Pts',(48.9172754308006,-0.226848207315626,
339.913015667931));
#63659=CARTESIAN_POINT('Ctrl Pts',(48.9098636266235,-0.0965616065939597,
339.919031378812));
#63660=CARTESIAN_POINT('Ctrl Pts',(48.9024518224464,0.0337997660645954,
339.919853427656));
#63661=CARTESIAN_POINT('Ctrl Pts',(48.8950400182694,0.163793413952805,339.915521821744));
#63662=CARTESIAN_POINT('Ctrl Pts',(48.8872649394909,0.300158437755397,339.910977910924));
#63663=CARTESIAN_POINT('Ctrl Pts',(48.8794898607125,0.436549717445622,339.900748020022));
#63664=CARTESIAN_POINT('Ctrl Pts',(48.871714781934,0.572454420098576,339.884821286333));
#63665=CARTESIAN_POINT('Ctrl Pts',(48.863949270885,0.708191883362706,339.868914151503));
#63666=CARTESIAN_POINT('Ctrl Pts',(48.856183759836,0.843443576451924,339.84732416749));
#63667=CARTESIAN_POINT('Ctrl Pts',(48.848418248787,0.977697153996748,339.820092461516));
#63668=CARTESIAN_POINT('Ctrl Pts',(48.8406604372648,1.11181761872857,339.792887755858));
#63669=CARTESIAN_POINT('Ctrl Pts',(48.8329026257426,1.24494155673891,339.760052537386));
#63670=CARTESIAN_POINT('Ctrl Pts',(48.8251448142204,1.37656258723531,339.721679627624));
#63671=CARTESIAN_POINT('Ctrl Pts',(48.8173928406974,1.50808456873214,339.683335594694));
#63672=CARTESIAN_POINT('Ctrl Pts',(48.8096408671744,1.63810552014544,339.639462274219));
#63673=CARTESIAN_POINT('Ctrl Pts',(48.8018888936514,1.76613043946227,339.590203299779));
#63674=CARTESIAN_POINT('Ctrl Pts',(48.7941402030938,1.89410114014984,339.540965186545));
#63675=CARTESIAN_POINT('Ctrl Pts',(48.7863915125361,2.02007712598061,339.486346095822));
#63676=CARTESIAN_POINT('Ctrl Pts',(48.7786428219785,2.14357993353085,339.42653906919));
#63677=CARTESIAN_POINT('Ctrl Pts',(48.7708957436007,2.26705704529046,339.366744485909));
#63678=CARTESIAN_POINT('Ctrl Pts',(48.7631486652229,2.38806165070146,339.301764283961));
#63679=CARTESIAN_POINT('Ctrl Pts',(48.755401586845,2.50613697218775,339.231838907512));
#63680=CARTESIAN_POINT('Ctrl Pts',(48.7476544435392,2.62421328325871,339.161912945021));
#63681=CARTESIAN_POINT('Ctrl Pts',(48.7399073002334,2.73935992511543,339.087041924536));
#63682=CARTESIAN_POINT('Ctrl Pts',(48.7321601569276,2.85114670422752,339.007511139532));
#63683=CARTESIAN_POINT('Ctrl Pts',(48.7244112718995,2.96295861538101,338.927962474318));
#63684=CARTESIAN_POINT('Ctrl Pts',(48.7166623868714,3.07140884225921,338.843752186498));
#63685=CARTESIAN_POINT('Ctrl Pts',(48.7089135018433,3.17609836695589,338.755207347926));
#63686=CARTESIAN_POINT('Ctrl Pts',(48.7011563920686,3.28089901019566,338.666568526948));
#63687=CARTESIAN_POINT('Ctrl Pts',(48.6933992822939,3.38193067864855,338.573586217631));
#63688=CARTESIAN_POINT('Ctrl Pts',(48.6856421725192,3.47882909503142,338.476626409332));
#63689=CARTESIAN_POINT('Ctrl Pts',(48.677880917593,3.57577929083006,338.379614788811));
#63690=CARTESIAN_POINT('Ctrl Pts',(48.6701196626668,3.66859156921593,338.278621721817));
#63691=CARTESIAN_POINT('Ctrl Pts',(48.6623584077407,3.75694109275471,338.174047367018));
#63692=CARTESIAN_POINT('Ctrl Pts',(48.654584737336,3.84543194673788,338.069305727332));
#63693=CARTESIAN_POINT('Ctrl Pts',(48.6468110669313,3.92944554046913,337.960971660855));
#63694=CARTESIAN_POINT('Ctrl Pts',(48.6390373965267,4.00869910822896,337.849476183825));
#63695=CARTESIAN_POINT('Ctrl Pts',(48.6316255923496,4.08426340334254,337.743170848074));
#63696=CARTESIAN_POINT('Ctrl Pts',(48.6242137881725,4.15550070063262,337.633992046465));
#63697=CARTESIAN_POINT('Ctrl Pts',(48.6168019839954,4.22220518271761,337.522333534157));
#63698=CARTESIAN_POINT('Ctrl Pts',(48.6090269052169,4.29217905017198,337.405202305547));
#63699=CARTESIAN_POINT('Ctrl Pts',(48.6012518264385,4.35738566423734,337.284971987716));
#63700=CARTESIAN_POINT('Ctrl Pts',(48.59347674766,4.41753836691207,337.162067954381));
#63701=CARTESIAN_POINT('Ctrl Pts',(48.585711236611,4.47761704785652,337.039315162283));
#63702=CARTESIAN_POINT('Ctrl Pts',(48.577945725562,4.53265402156882,336.913895548913));
#63703=CARTESIAN_POINT('Ctrl Pts',(48.570180214513,4.58240661333048,336.786262212724));
#63704=CARTESIAN_POINT('Ctrl Pts',(48.5624224029907,4.63210987525269,336.658755425359));
#63705=CARTESIAN_POINT('Ctrl Pts',(48.5546645914685,4.67653904103847,336.529039645011));
#63706=CARTESIAN_POINT('Ctrl Pts',(48.5469067799463,4.7154981345845,336.397590929146));
#63707=CARTESIAN_POINT('Ctrl Pts',(48.5391548064233,4.75442791017694,336.266241132608));
#63708=CARTESIAN_POINT('Ctrl Pts',(48.5314028329004,4.78789569640302,336.13316136953));
#63709=CARTESIAN_POINT('Ctrl Pts',(48.5236508593774,4.81575440381345,335.998845626036));
#63710=CARTESIAN_POINT('Ctrl Pts',(48.5159021688198,4.84360131304485,335.864586765339));
#63711=CARTESIAN_POINT('Ctrl Pts',(48.5081534782621,4.86584378884237,335.729093347241));
#63712=CARTESIAN_POINT('Ctrl Pts',(48.5004047877045,4.88238523997546,335.592872187718));
#63713=CARTESIAN_POINT('Ctrl Pts',(48.4926577093267,4.89892324952146,335.456679370145));
#63714=CARTESIAN_POINT('Ctrl Pts',(48.4849106309489,4.90976254664243,335.319759500098));
#63715=CARTESIAN_POINT('Ctrl Pts',(48.4771635525711,4.91485813741064,335.18262680972));
#63716=CARTESIAN_POINT('Ctrl Pts',(48.4694164092653,4.9199537708848,335.045492970038));
#63717=CARTESIAN_POINT('Ctrl Pts',(48.4616692659594,4.91930558747766,334.908146697072));
#63718=CARTESIAN_POINT('Ctrl Pts',(48.4539221226536,4.91292069415397,334.771104138409));
#63719=CARTESIAN_POINT('Ctrl Pts',(48.4461732376256,4.90653436537073,334.634030769669));
#63720=CARTESIAN_POINT('Ctrl Pts',(48.4384243525975,4.89440877843182,334.497261641479));
#63721=CARTESIAN_POINT('Ctrl Pts',(48.4306754675695,4.87660304355248,334.361309293856));
#63722=CARTESIAN_POINT('Ctrl Pts',(48.4229183577947,4.85877840948209,334.225212645006));
#63723=CARTESIAN_POINT('Ctrl Pts',(48.41516124802,4.83526163488226,334.089934896692));
#63724=CARTESIAN_POINT('Ctrl Pts',(48.4074041382453,4.80616335667175,333.955980435296));
#63725=CARTESIAN_POINT('Ctrl Pts',(48.3996428833192,4.77704952927181,333.821954392918));
#63726=CARTESIAN_POINT('Ctrl Pts',(48.391881628393,4.74234835404569,333.689253424429));
#63727=CARTESIAN_POINT('Ctrl Pts',(48.3841203734669,4.70222054478059,333.558367241374));
#63728=CARTESIAN_POINT('Ctrl Pts',(48.3763467030622,4.66202854409822,333.427271683082));
#63729=CARTESIAN_POINT('Ctrl Pts',(48.3685730326576,4.61639269265932,333.297997080184));
#63730=CARTESIAN_POINT('Ctrl Pts',(48.3607993622529,4.56552242045621,333.171014464023));
#63731=CARTESIAN_POINT('Ctrl Pts',(48.3533875580758,4.51702017166269,333.049942919195));
#63732=CARTESIAN_POINT('Ctrl Pts',(48.3459757538987,4.46375997732151,332.930955041894));
#63733=CARTESIAN_POINT('Ctrl Pts',(48.3385639497216,4.40596157494998,332.814436991857));
#63734=CARTESIAN_POINT('Ctrl Pts',(48.3307888709431,4.34533030070588,332.692208045098));
#63735=CARTESIAN_POINT('Ctrl Pts',(48.3230137921647,4.27951310186669,332.572310888417));
#63736=CARTESIAN_POINT('Ctrl Pts',(48.3152387133863,4.20871255717112,332.455216772766));
#63737=CARTESIAN_POINT('Ctrl Pts',(48.3074732023373,4.13799913705294,332.338266748879));
#63738=CARTESIAN_POINT('Ctrl Pts',(48.2997076912882,4.06231477295682,332.224113234152));
#63739=CARTESIAN_POINT('Ctrl Pts',(48.2919421802392,3.98190915982253,332.113205496503));
#63740=CARTESIAN_POINT('Ctrl Pts',(48.284184368717,3.90158326908809,332.002407724199));
#63741=CARTESIAN_POINT('Ctrl Pts',(48.2764265571948,3.81654567298116,331.894849639));
#63742=CARTESIAN_POINT('Ctrl Pts',(48.2686687456726,3.72709064446503,331.790953663401));
#63743=CARTESIAN_POINT('Ctrl Pts',(48.2609167721496,3.63770293369469,331.687135872818));
#63744=CARTESIAN_POINT('Ctrl Pts',(48.2531647986267,3.54390466129782,331.58697500146));
#63745=CARTESIAN_POINT('Ctrl Pts',(48.2454128251037,3.44603163220536,331.490862064219));
#63746=CARTESIAN_POINT('Ctrl Pts',(48.2376641345461,3.3482000523987,331.394789830863));
#63747=CARTESIAN_POINT('Ctrl Pts',(48.2299154439884,3.24629742642207,331.302762395299));
#63748=CARTESIAN_POINT('Ctrl Pts',(48.2221667534308,3.14069767558466,331.215135250359));
#63749=CARTESIAN_POINT('Ctrl Pts',(48.214419675053,3.0351198956574,331.127526336978));
#63750=CARTESIAN_POINT('Ctrl Pts',(48.2066725966751,2.92584682150826,331.044316142639));
#63751=CARTESIAN_POINT('Ctrl Pts',(48.1989255182973,2.81328653312129,330.965820784217));
#63752=CARTESIAN_POINT('Ctrl Pts',(48.1911783749915,2.70072530137045,330.887324767927));
#63753=CARTESIAN_POINT('Ctrl Pts',(48.1834312316857,2.58487712104461,330.813543889953));
#63754=CARTESIAN_POINT('Ctrl Pts',(48.1756840883799,2.46617987764701,330.744751490972));
#63755=CARTESIAN_POINT('Ctrl Pts',(48.1679352033518,2.3474559485894,330.675943625998));
#63756=CARTESIAN_POINT('Ctrl Pts',(48.1601863183237,2.22588201999382,330.612126667668));
#63757=CARTESIAN_POINT('Ctrl Pts',(48.1524374332956,2.10192108562494,330.553528273754));
#63758=CARTESIAN_POINT('Ctrl Pts',(48.1446803235208,1.97782857783931,330.494867682899));
#63759=CARTESIAN_POINT('Ctrl Pts',(48.1369232137461,1.85134435712972,330.44143688852));
#63760=CARTESIAN_POINT('Ctrl Pts',(48.1291661039714,1.72295244474943,330.393415806085));
#63761=CARTESIAN_POINT('Ctrl Pts',(48.1214048490452,1.59449192383661,330.345369062718));
#63762=CARTESIAN_POINT('Ctrl Pts',(48.113643594119,1.4641220513151,330.302737912853));
#63763=CARTESIAN_POINT('Ctrl Pts',(48.1058823391928,1.3323416075233,330.265652219855));
#63764=CARTESIAN_POINT('Ctrl Pts',(48.0981086687882,1.2003503579684,330.228507201834));
#63765=CARTESIAN_POINT('Ctrl Pts',(48.0903349983835,1.06694440864054,330.196925457504));
#63766=CARTESIAN_POINT('Ctrl Pts',(48.0825613279789,0.932633194431056,330.170985774804));
#63767=CARTESIAN_POINT('Ctrl Pts',(48.0751495238017,0.804574199555421,330.146253590574));
#63768=CARTESIAN_POINT('Ctrl Pts',(48.0677377196246,0.675692607809895,330.126650056321));
#63769=CARTESIAN_POINT('Ctrl Pts',(48.0603259154474,0.546432061734352,330.112199363271));
#63770=CARTESIAN_POINT('Ctrl Pts',(48.052550836669,0.410836071249504,330.097040398708));
#63771=CARTESIAN_POINT('Ctrl Pts',(48.0447757578906,0.274394531420278,330.087504254182));
#63772=CARTESIAN_POINT('Ctrl Pts',(48.0370006791121,0.137613354207217,330.083675597843));
#63773=CARTESIAN_POINT('Ctrl Pts',(48.0292351680631,0.00100049494072593,
330.079851652909));
#63774=CARTESIAN_POINT('Ctrl Pts',(48.0214696570141,-0.135950783131938,
330.081721232386));
#63775=CARTESIAN_POINT('Ctrl Pts',(48.0137041459651,-0.272727556773448,
330.089317487123));
#63776=CARTESIAN_POINT('Ctrl Pts',(48.0059463344429,-0.40936871584577,330.096906210151));
#63777=CARTESIAN_POINT('Ctrl Pts',(47.9981885229207,-0.545835327050987,
330.110210287332));
#63778=CARTESIAN_POINT('Ctrl Pts',(47.9904307113985,-0.681612918314197,
330.129210855304));
#63779=CARTESIAN_POINT('Ctrl Pts',(47.9826787378755,-0.817288332634226,
330.148197124747));
#63780=CARTESIAN_POINT('Ctrl Pts',(47.9749267643525,-0.952275373536065,
330.172871298382));
#63781=CARTESIAN_POINT('Ctrl Pts',(47.9671747908295,-1.08606350493718,330.203162591275));
#63782=CARTESIAN_POINT('Ctrl Pts',(47.9594261002719,-1.2197949769853,330.233441055788));
#63783=CARTESIAN_POINT('Ctrl Pts',(47.9516774097142,-1.35232816895784,330.269331822052));
#63784=CARTESIAN_POINT('Ctrl Pts',(47.9439287191566,-1.48316178907224,330.310712829231));
#63785=CARTESIAN_POINT('Ctrl Pts',(47.9361816407788,-1.61396818815906,330.352085226746));
#63786=CARTESIAN_POINT('Ctrl Pts',(47.928434562401,-1.74307534629962,330.398945475281));
#63787=CARTESIAN_POINT('Ctrl Pts',(47.9206874840232,-1.86999659857624,330.451121480649));
#63788=CARTESIAN_POINT('Ctrl Pts',(47.9129403407174,-1.99691891457528,330.503297923302));
#63789=CARTESIAN_POINT('Ctrl Pts',(47.9051931974116,-2.121654926651,330.560790063033));
#63790=CARTESIAN_POINT('Ctrl Pts',(47.8974460541058,-2.24373781182481,330.623377592905));
#63791=CARTESIAN_POINT('Ctrl Pts',(47.8896971690777,-2.36584814382302,330.685979193782));
#63792=CARTESIAN_POINT('Ctrl Pts',(47.8819482840495,-2.48530381423137,330.753678286036));
#63793=CARTESIAN_POINT('Ctrl Pts',(47.8741993990214,-2.60166282827983,330.826208727015));
#63794=CARTESIAN_POINT('Ctrl Pts',(47.8664422892467,-2.71814534698785,330.898816152553));
#63795=CARTESIAN_POINT('Ctrl Pts',(47.858685179472,-2.83152431136569,330.976264963474));
#63796=CARTESIAN_POINT('Ctrl Pts',(47.8509280696973,-2.94138649498551,331.058245498561));
#63797=CARTESIAN_POINT('Ctrl Pts',(47.8431668147711,-3.05130738544384,331.140269841425));
#63798=CARTESIAN_POINT('Ctrl Pts',(47.835405559845,-3.15770744750401,331.226830487181));
#63799=CARTESIAN_POINT('Ctrl Pts',(47.8276443049188,-3.26020755763102,331.31757827732));
#63800=CARTESIAN_POINT('Ctrl Pts',(47.8198706345141,-3.36287163452938,331.408471234349));
#63801=CARTESIAN_POINT('Ctrl Pts',(47.8120969641094,-3.46162301111644,331.503564449213));
#63802=CARTESIAN_POINT('Ctrl Pts',(47.8043232937048,-3.55611974848233,331.602472163918));
#63803=CARTESIAN_POINT('Ctrl Pts',(47.7969114895277,-3.64621763998886,331.696775700707));
#63804=CARTESIAN_POINT('Ctrl Pts',(47.7894996853507,-3.73244789468158,331.794546383538));
#63805=CARTESIAN_POINT('Ctrl Pts',(47.7820878811736,-3.81455008920872,331.895424235194));
#63806=CARTESIAN_POINT('Ctrl Pts',(47.7741599434793,-3.90236960888749,332.003326886636));
#63807=CARTESIAN_POINT('Ctrl Pts',(47.7662320057849,-3.98575743039446,332.115143472683));
#63808=CARTESIAN_POINT('Ctrl Pts',(47.7583040680905,-4.06434425910569,332.230471374769));
#63809=CARTESIAN_POINT('Ctrl Pts',(47.7505666293383,-4.1410427395082,332.343028084119));
#63810=CARTESIAN_POINT('Ctrl Pts',(47.7428291905861,-4.21316804587119,332.458928960272));
#63811=CARTESIAN_POINT('Ctrl Pts',(47.7350917518339,-4.28041534114292,332.577763931858));
#63812=CARTESIAN_POINT('Ctrl Pts',(47.7273617014445,-4.3475984229928,332.696485429732));
#63813=CARTESIAN_POINT('Ctrl Pts',(47.7196316510551,-4.40991256644573,332.818135110118));
#63814=CARTESIAN_POINT('Ctrl Pts',(47.7119016006658,-4.46709565679131,332.942273231069));
#63815=CARTESIAN_POINT('Ctrl Pts',(47.7041772301748,-4.52423673005729,333.066320137619));
#63816=CARTESIAN_POINT('Ctrl Pts',(47.6964528596838,-4.57625408746932,333.192851490939));
#63817=CARTESIAN_POINT('Ctrl Pts',(47.6887284891928,-4.62293129577608,333.321402580416));
#63818=CARTESIAN_POINT('Ctrl Pts',(47.6806525631358,-4.67173290145687,333.455804353917));
#63819=CARTESIAN_POINT('Ctrl Pts',(47.6725766370788,-4.7146966125614,333.59241364941));
#63820=CARTESIAN_POINT('Ctrl Pts',(47.6645007110218,-4.75163105817567,333.730675238767));
#63821=CARTESIAN_POINT('Ctrl Pts',(47.6567817387722,-4.786933011009,333.862825702241));
#63822=CARTESIAN_POINT('Ctrl Pts',(47.6490627665226,-4.81672717171253,333.996485105244));
#63823=CARTESIAN_POINT('Ctrl Pts',(47.641343794273,-4.84089748737306,334.131153305096));
#63824=CARTESIAN_POINT('Ctrl Pts',(47.6336254228008,-4.86506592182759,334.265811023553));
#63825=CARTESIAN_POINT('Ctrl Pts',(47.6259070513286,-4.88361131809932,334.401476994412));
#63826=CARTESIAN_POINT('Ctrl Pts',(47.6181886798563,-4.89646894791932,334.537642016872));
#63827=CARTESIAN_POINT('Ctrl Pts',(47.6104678657073,-4.90933064686615,334.673850132248));
#63828=CARTESIAN_POINT('Ctrl Pts',(47.6027470515583,-4.9165009547583,334.810557222311));
#63829=CARTESIAN_POINT('Ctrl Pts',(47.5950262374094,-4.91796711350799,334.947250280058));
#63830=CARTESIAN_POINT('Ctrl Pts',(47.5939566171091,-4.91817023109789,334.966187359315));
#63831=CARTESIAN_POINT('Ctrl Pts',(47.5928869968089,-4.91826395320588,334.985124169515));
#63832=CARTESIAN_POINT('Ctrl Pts',(47.5918173765087,-4.91824832477906,335.004059348224));
#63833=CARTESIAN_POINT('',(45.8418173765417,-4.91824993362185,335.000808040044));
#63834=CARTESIAN_POINT('Ctrl Pts',(47.5918173764616,-4.91824832477837,335.004059349057));
#63835=CARTESIAN_POINT('Ctrl Pts',(47.5826404069209,-4.91811423829332,335.166516585725));
#63836=CARTESIAN_POINT('Ctrl Pts',(47.5734634373801,-4.90992702535072,335.328629453609));
#63837=CARTESIAN_POINT('Ctrl Pts',(47.5642864678394,-4.89381185941993,335.489682087788));
#63838=CARTESIAN_POINT('Ctrl Pts',(47.5550435007526,-4.87758079886826,335.651892956022));
#63839=CARTESIAN_POINT('Ctrl Pts',(47.5458005336658,-4.8533074482954,335.813028237604));
#63840=CARTESIAN_POINT('Ctrl Pts',(47.536557566579,-4.82116847162421,335.972377308824));
#63841=CARTESIAN_POINT('Ctrl Pts',(47.5272433712864,-4.78878182538708,336.13295435677));
#63842=CARTESIAN_POINT('Ctrl Pts',(47.5179291759937,-4.74840792014492,336.291717514412));
#63843=CARTESIAN_POINT('Ctrl Pts',(47.508614980701,-4.70027563195492,336.447961341387));
#63844=CARTESIAN_POINT('Ctrl Pts',(47.5070266027672,-4.69206748706824,336.474606074428));
#63845=CARTESIAN_POINT('Ctrl Pts',(47.5054382248335,-4.68363382787156,336.501177593195));
#63846=CARTESIAN_POINT('Ctrl Pts',(47.5038498468996,-4.67497592595325,336.527672463016));
#63847=CARTESIAN_POINT('Ctrl Pts',(47.4960747681212,-4.6325956661689,336.657364330235));
#63848=CARTESIAN_POINT('Ctrl Pts',(47.4882996893428,-4.5847475352392,336.785496247453));
#63849=CARTESIAN_POINT('Ctrl Pts',(47.4805246105644,-4.53156407116226,336.91157268537));
#63850=CARTESIAN_POINT('Ctrl Pts',(47.4727590995154,-4.47844605272372,337.037493978203));
#63851=CARTESIAN_POINT('Ctrl Pts',(47.4649935884664,-4.42000591500347,337.161364467814));
#63852=CARTESIAN_POINT('Ctrl Pts',(47.4572280774174,-4.35642598878991,337.28270358713));
#63853=CARTESIAN_POINT('Ctrl Pts',(47.4494702658952,-4.29290910225829,337.403922398356));
#63854=CARTESIAN_POINT('Ctrl Pts',(47.4417124543731,-4.2242627490384,337.52261449006));
#63855=CARTESIAN_POINT('Ctrl Pts',(47.4339546428509,-4.15071724189254,337.638319434859));
#63856=CARTESIAN_POINT('Ctrl Pts',(47.4262026693279,-4.07722708007316,337.753937308018));
#63857=CARTESIAN_POINT('Ctrl Pts',(47.4184506958049,-3.99884531149489,337.866572180107));
#63858=CARTESIAN_POINT('Ctrl Pts',(47.4106987222819,-3.91584787423138,337.975788717026));
#63859=CARTESIAN_POINT('Ctrl Pts',(47.4029500317243,-3.83288558643161,338.084959000676));
#63860=CARTESIAN_POINT('Ctrl Pts',(47.3952013411667,-3.74531175379001,338.190713517903));
#63861=CARTESIAN_POINT('Ctrl Pts',(47.387452650609,-3.65344515282044,338.2926465917));
#63862=CARTESIAN_POINT('Ctrl Pts',(47.3797055722312,-3.56159766546455,338.394558457469));
#63863=CARTESIAN_POINT('Ctrl Pts',(47.3719584938535,-3.46545944782824,338.492650171113));
#63864=CARTESIAN_POINT('Ctrl Pts',(47.3642114154757,-3.36538875398464,338.586550096828));
#63865=CARTESIAN_POINT('Ctrl Pts',(47.3564642721699,-3.26531722145224,338.680450809514));
#63866=CARTESIAN_POINT('Ctrl Pts',(47.3487171288641,-3.1613134320139,338.770159396739));
#63867=CARTESIAN_POINT('Ctrl Pts',(47.3409699855583,-3.05377129970843,338.855342256088));
#63868=CARTESIAN_POINT('Ctrl Pts',(47.3332211005302,-2.94620498964865,338.940544266352));
#63869=CARTESIAN_POINT('Ctrl Pts',(47.3254722155021,-2.83509906011699,339.021218281422));
#63870=CARTESIAN_POINT('Ctrl Pts',(47.317723330474,-2.72087885587924,339.097072285685));
#63871=CARTESIAN_POINT('Ctrl Pts',(47.3099662206993,-2.60653741713644,339.173006802172));
#63872=CARTESIAN_POINT('Ctrl Pts',(47.3022091109246,-2.48907542672063,339.244110871563));
#63873=CARTESIAN_POINT('Ctrl Pts',(47.2944520011499,-2.36894591880351,339.310136691137));
#63874=CARTESIAN_POINT('Ctrl Pts',(47.2866907462237,-2.24875221751827,339.376197792798));
#63875=CARTESIAN_POINT('Ctrl Pts',(47.2789294912976,-2.12588850836958,339.437175063762));
#63876=CARTESIAN_POINT('Ctrl Pts',(47.2711682363714,-2.00082964491927,339.492868103396));
#63877=CARTESIAN_POINT('Ctrl Pts',(47.2633945659668,-1.87557072804404,339.548650233743));
#63878=CARTESIAN_POINT('Ctrl Pts',(47.2556208955621,-1.74811000338902,339.599131097061));
#63879=CARTESIAN_POINT('Ctrl Pts',(47.2478472251574,-1.61894022973554,339.64415929906));
#63880=CARTESIAN_POINT('Ctrl Pts',(47.2404354209802,-1.4957833401193,339.687091427424));
#63881=CARTESIAN_POINT('Ctrl Pts',(47.2330236168029,-1.37107320855419,339.725067029216));
#63882=CARTESIAN_POINT('Ctrl Pts',(47.2256118126257,-1.2452453579823,339.757998219937));
#63883=CARTESIAN_POINT('Ctrl Pts',(47.2178367338473,-1.11325030963496,339.792543466411));
#63884=CARTESIAN_POINT('Ctrl Pts',(47.2100616550688,-0.97960807770071,339.821646484932));
#63885=CARTESIAN_POINT('Ctrl Pts',(47.2022865762904,-0.844807087254626,
339.845150570191));
#63886=CARTESIAN_POINT('Ctrl Pts',(47.1945210652414,-0.710171978009045,
339.868625732178));
#63887=CARTESIAN_POINT('Ctrl Pts',(47.1867555541924,-0.574381328819445,
339.886515603218));
#63888=CARTESIAN_POINT('Ctrl Pts',(47.1789900431434,-0.437937928439986,
339.898713446746));
#63889=CARTESIAN_POINT('Ctrl Pts',(47.1712322316212,-0.301629812089341,
339.910899196077));
#63890=CARTESIAN_POINT('Ctrl Pts',(47.163474420099,-0.164670619336524,339.91740411452));
#63891=CARTESIAN_POINT('Ctrl Pts',(47.1557166085768,-0.0275721688405922,
339.918172713316));
#63892=CARTESIAN_POINT('Ctrl Pts',(47.1479646350538,0.1094231107237,339.918940733717));
#63893=CARTESIAN_POINT('Ctrl Pts',(47.1402126615308,0.246557050145736,339.913981024592));
#63894=CARTESIAN_POINT('Ctrl Pts',(47.1324606880078,0.383314241768882,339.903290043895));
#63895=CARTESIAN_POINT('Ctrl Pts',(47.1247119974501,0.520013516640182,339.892603590834));
#63896=CARTESIAN_POINT('Ctrl Pts',(47.1169633068925,0.656335972177747,339.876190724124));
#63897=CARTESIAN_POINT('Ctrl Pts',(47.1092146163349,0.79176795766934,339.854099974631));
#63898=CARTESIAN_POINT('Ctrl Pts',(47.1014675379571,0.927171765405202,339.832013821302));
#63899=CARTESIAN_POINT('Ctrl Pts',(47.0937204595792,1.06168508607588,339.804252197826));
#63900=CARTESIAN_POINT('Ctrl Pts',(47.0859733812014,1.19480153137067,339.770915254239));
#63901=CARTESIAN_POINT('Ctrl Pts',(47.0782262378956,1.32791909230939,339.737578031257));
#63902=CARTESIAN_POINT('Ctrl Pts',(47.0704790945898,1.45963937535645,339.698665489919));
#63903=CARTESIAN_POINT('Ctrl Pts',(47.062731951284,1.58946867763668,339.654328349538));
#63904=CARTESIAN_POINT('Ctrl Pts',(47.0549830662559,1.71932716830042,339.609981241226));
#63905=CARTESIAN_POINT('Ctrl Pts',(47.0472341812278,1.84729346240389,339.56020723337));
#63906=CARTESIAN_POINT('Ctrl Pts',(47.0394852961997,1.97289181933021,339.505205981053));
#63907=CARTESIAN_POINT('Ctrl Pts',(47.031728186425,2.09862348765025,339.45014634984));
#63908=CARTESIAN_POINT('Ctrl Pts',(47.0239710766503,2.22198183952132,339.389848548055));
#63909=CARTESIAN_POINT('Ctrl Pts',(47.0162139668755,2.34251332956389,339.324559441529));
#63910=CARTESIAN_POINT('Ctrl Pts',(47.0084527119494,2.46310922778097,339.259235446592));
#63911=CARTESIAN_POINT('Ctrl Pts',(47.0006914570232,2.58087491876656,339.18891503258));
#63912=CARTESIAN_POINT('Ctrl Pts',(46.992930202097,2.69538491084248,339.113889065702));
#63913=CARTESIAN_POINT('Ctrl Pts',(46.9851565316924,2.81007808158692,339.038743081728));
#63914=CARTESIAN_POINT('Ctrl Pts',(46.9773828612877,2.9215048283188,338.958876730843));
#63915=CARTESIAN_POINT('Ctrl Pts',(46.969609190883,3.02927118029817,338.874622456281));
#63916=CARTESIAN_POINT('Ctrl Pts',(46.9621973867059,3.13202098266611,338.794290238469));
#63917=CARTESIAN_POINT('Ctrl Pts',(46.9547855825288,3.23144328444129,338.709969605433));
#63918=CARTESIAN_POINT('Ctrl Pts',(46.9473737783517,3.32722849521764,338.62197923836));
#63919=CARTESIAN_POINT('Ctrl Pts',(46.9395986995733,3.4277084245034,338.529676201287));
#63920=CARTESIAN_POINT('Ctrl Pts',(46.9318236207949,3.5245032537523,338.433042910573));
#63921=CARTESIAN_POINT('Ctrl Pts',(46.9240485420164,3.61721689129453,338.332405291052));
#63922=CARTESIAN_POINT('Ctrl Pts',(46.9162830309674,3.70981643880332,338.231891512529));
#63923=CARTESIAN_POINT('Ctrl Pts',(46.9085175199184,3.79834452496752,338.1273834944));
#63924=CARTESIAN_POINT('Ctrl Pts',(46.9007520088694,3.88243930488574,338.019246281173));
#63925=CARTESIAN_POINT('Ctrl Pts',(46.8929941973472,3.96645070458483,337.911216286309));
#63926=CARTESIAN_POINT('Ctrl Pts',(46.885236385825,4.04603730719556,337.799564563848));
#63927=CARTESIAN_POINT('Ctrl Pts',(46.8774785743028,4.12087547659111,337.684691484869));
#63928=CARTESIAN_POINT('Ctrl Pts',(46.8697266007797,4.19565732789087,337.569904851525));
#63929=CARTESIAN_POINT('Ctrl Pts',(46.8619746272568,4.26569764604235,337.451902013046));
#63930=CARTESIAN_POINT('Ctrl Pts',(46.8542226537338,4.33071453580504,337.331114469919));
#63931=CARTESIAN_POINT('Ctrl Pts',(46.8464739631761,4.39570389087636,337.210378080389));
#63932=CARTESIAN_POINT('Ctrl Pts',(46.8387252726185,4.45567386397908,337.086859675268));
#63933=CARTESIAN_POINT('Ctrl Pts',(46.8309765820609,4.51038729987976,336.961017457236));
#63934=CARTESIAN_POINT('Ctrl Pts',(46.823229503683,4.56508935219312,336.835201421728));
#63935=CARTESIAN_POINT('Ctrl Pts',(46.8154824253052,4.61453688693182,336.707062893235));
#63936=CARTESIAN_POINT('Ctrl Pts',(46.8077353469274,4.65854008662604,336.577081901424));
#63937=CARTESIAN_POINT('Ctrl Pts',(46.7999882036216,4.70254365510943,336.447099820246));
#63938=CARTESIAN_POINT('Ctrl Pts',(46.7922410603157,4.74110267220092,336.315275615184));
#63939=CARTESIAN_POINT('Ctrl Pts',(46.7844939170099,4.77407671003051,336.182106014385));
#63940=CARTESIAN_POINT('Ctrl Pts',(46.7767450319818,4.80705816112386,336.048906474232));
#63941=CARTESIAN_POINT('Ctrl Pts',(46.7689961469537,4.83445204047934,335.914361315796));
#63942=CARTESIAN_POINT('Ctrl Pts',(46.7612472619256,4.85616879177119,335.778978644333));
#63943=CARTESIAN_POINT('Ctrl Pts',(46.7534901521509,4.87790859344723,335.643452276305));
#63944=CARTESIAN_POINT('Ctrl Pts',(46.7457330423761,4.89395916802745,335.507087006048));
#63945=CARTESIAN_POINT('Ctrl Pts',(46.7379759326014,4.90428267082493,335.370397822815));
#63946=CARTESIAN_POINT('Ctrl Pts',(46.7302146776752,4.91461169017222,335.233635597253));
#63947=CARTESIAN_POINT('Ctrl Pts',(46.7224534227491,4.91920752659564,335.096549504276));
#63948=CARTESIAN_POINT('Ctrl Pts',(46.7146921678229,4.91808451773345,334.959654753309));
#63949=CARTESIAN_POINT('Ctrl Pts',(46.7069184974182,4.91695971242307,334.822541015355));
#63950=CARTESIAN_POINT('Ctrl Pts',(46.6991448270135,4.91009780041177,334.685619621648));
#63951=CARTESIAN_POINT('Ctrl Pts',(46.6913711566089,4.89756514013403,334.5494017747));
#63952=CARTESIAN_POINT('Ctrl Pts',(46.6839593524318,4.88561587820755,334.4195249013));
#63953=CARTESIAN_POINT('Ctrl Pts',(46.6765475482549,4.86851197132704,334.290287833804));
#63954=CARTESIAN_POINT('Ctrl Pts',(46.6691357440779,4.84635386816852,334.162123370067));
#63955=CARTESIAN_POINT('Ctrl Pts',(46.6613606652994,4.82310973036836,334.027677184178));
#63956=CARTESIAN_POINT('Ctrl Pts',(46.653585586521,4.79422997081942,333.893986528814));
#63957=CARTESIAN_POINT('Ctrl Pts',(46.6458105077426,4.75977431873624,333.761560862537));
#63958=CARTESIAN_POINT('Ctrl Pts',(46.6380449966936,4.72536106652648,333.629298154474));
#63959=CARTESIAN_POINT('Ctrl Pts',(46.6302794856445,4.68538567166479,333.498297712876));
#63960=CARTESIAN_POINT('Ctrl Pts',(46.6225139745955,4.63995929282773,333.369061367371));
#63961=CARTESIAN_POINT('Ctrl Pts',(46.6147561630733,4.59457795437758,333.239953160079));
#63962=CARTESIAN_POINT('Ctrl Pts',(46.6069983515511,4.54375651632663,333.11260593444));
#63963=CARTESIAN_POINT('Ctrl Pts',(46.5992405400289,4.48765652117703,332.987508506742));
#63964=CARTESIAN_POINT('Ctrl Pts',(46.5914885665059,4.43159874305277,332.862505218825));
#63965=CARTESIAN_POINT('Ctrl Pts',(46.5837365929829,4.37027047375947,332.739748714144));
#63966=CARTESIAN_POINT('Ctrl Pts',(46.5759846194599,4.3038820215742,332.619709554094));
#63967=CARTESIAN_POINT('Ctrl Pts',(46.5682359289023,4.23752168493788,332.4997212307));
#63968=CARTESIAN_POINT('Ctrl Pts',(46.5604872383447,4.16610561644475,332.38244830442));
#63969=CARTESIAN_POINT('Ctrl Pts',(46.552738547787,4.08989079019746,332.268338163909));
#63970=CARTESIAN_POINT('Ctrl Pts',(46.5449914694092,4.01369182108139,332.154251764965));
#63971=CARTESIAN_POINT('Ctrl Pts',(46.5372443910314,3.93269629710292,332.043327167733));
#63972=CARTESIAN_POINT('Ctrl Pts',(46.5294973126536,3.84720516432347,331.935983765366));
#63973=CARTESIAN_POINT('Ctrl Pts',(46.5217501693478,3.76171331504598,331.828639463358));
#63974=CARTESIAN_POINT('Ctrl Pts',(46.514003026042,3.67172602532727,331.724876721834));
#63975=CARTESIAN_POINT('Ctrl Pts',(46.5062558827362,3.57758501088609,331.625082437691));
#63976=CARTESIAN_POINT('Ctrl Pts',(46.4985069977081,3.48342283154625,331.525265717673));
#63977=CARTESIAN_POINT('Ctrl Pts',(46.49075811268,3.3851053374024,331.429419514672));
#63978=CARTESIAN_POINT('Ctrl Pts',(46.4830092276519,3.28301134093816,331.337894103419));
#63979=CARTESIAN_POINT('Ctrl Pts',(46.4752521178772,3.18080898085117,331.24627154615));
#63980=CARTESIAN_POINT('Ctrl Pts',(46.4674950081024,3.0748224027545,331.158979203188));
#63981=CARTESIAN_POINT('Ctrl Pts',(46.4597378983277,2.96546419216445,331.076327589172));
#63982=CARTESIAN_POINT('Ctrl Pts',(46.4519766434016,2.85604754404326,330.993631808777));
#63983=CARTESIAN_POINT('Ctrl Pts',(46.4442153884754,2.74325599465342,330.915581920972));
#63984=CARTESIAN_POINT('Ctrl Pts',(46.4364541335492,2.62753055351063,330.842444678315));
#63985=CARTESIAN_POINT('Ctrl Pts',(46.4286804631446,2.51161998937685,330.769190439906));
#63986=CARTESIAN_POINT('Ctrl Pts',(46.4209067927399,2.39276649399367,330.700864745426));
#63987=CARTESIAN_POINT('Ctrl Pts',(46.4131331223353,2.27143585881414,330.637688433663));
#63988=CARTESIAN_POINT('Ctrl Pts',(46.4057213181582,2.1557531938922,330.577452994413));
#63989=CARTESIAN_POINT('Ctrl Pts',(46.398309513981,2.03781908124668,330.52189844176));
#63990=CARTESIAN_POINT('Ctrl Pts',(46.3908977098039,1.91805182836833,330.471174518024));
#63991=CARTESIAN_POINT('Ctrl Pts',(46.3831226310255,1.79241442565861,330.417964463687));
#63992=CARTESIAN_POINT('Ctrl Pts',(46.375347552247,1.66436260638541,330.369902384829));
#63993=CARTESIAN_POINT('Ctrl Pts',(46.3675724734686,1.534357108029,330.327213751139));
#63994=CARTESIAN_POINT('Ctrl Pts',(46.3598069624196,1.40451158971479,330.284577648531));
#63995=CARTESIAN_POINT('Ctrl Pts',(46.3520414513706,1.27271754365588,330.247301955156));
#63996=CARTESIAN_POINT('Ctrl Pts',(46.3442759403216,1.13945712343001,330.215564764116));
#63997=CARTESIAN_POINT('Ctrl Pts',(46.3365181287993,1.00632883129877,330.183859040594));
#63998=CARTESIAN_POINT('Ctrl Pts',(46.3287603172772,0.871737436162197,330.157680981104));
#63999=CARTESIAN_POINT('Ctrl Pts',(46.321002505755,0.736181413981547,330.137159267649));
#64000=CARTESIAN_POINT('Ctrl Pts',(46.313250532232,0.600727402006408,330.116652997435));
#64001=CARTESIAN_POINT('Ctrl Pts',(46.3054985587089,0.464310592794973,330.101794659016));
#64002=CARTESIAN_POINT('Ctrl Pts',(46.2977465851859,0.327440501340161,330.092662047445));
#64003=CARTESIAN_POINT('Ctrl Pts',(46.2899978946283,0.190628374450339,330.083533303542));
#64004=CARTESIAN_POINT('Ctrl Pts',(46.2822492040707,0.0533637363179859,
330.080125489603));
#64005=CARTESIAN_POINT('Ctrl Pts',(46.2745005135131,-0.0838381309592026,
330.082464618297));
#64006=CARTESIAN_POINT('Ctrl Pts',(46.2667534351352,-0.221011452241972,
330.084803260316));
#64007=CARTESIAN_POINT('Ctrl Pts',(46.2590063567574,-0.358121638074713,
330.092886459979));
#64008=CARTESIAN_POINT('Ctrl Pts',(46.2512592783796,-0.494653152623377,
330.106688103023));
#64009=CARTESIAN_POINT('Ctrl Pts',(46.2435121350738,-0.631185811437452,
330.120489861737));
#64010=CARTESIAN_POINT('Ctrl Pts',(46.235764991768,-0.767139400401763,330.140010120114));
#64011=CARTESIAN_POINT('Ctrl Pts',(46.2280178484622,-0.902003647680204,
330.165170894223));
#64012=CARTESIAN_POINT('Ctrl Pts',(46.2202689634341,-1.03689821530477,330.190337325008));
#64013=CARTESIAN_POINT('Ctrl Pts',(46.212520078406,-1.17070256973624,330.221146723247));
#64014=CARTESIAN_POINT('Ctrl Pts',(46.2047711933779,-1.30291716030652,330.257470091198));
#64015=CARTESIAN_POINT('Ctrl Pts',(46.1970140836032,-1.43527208480926,330.293832013147));
#64016=CARTESIAN_POINT('Ctrl Pts',(46.1892569738284,-1.56603349722304,330.335719492183));
#64017=CARTESIAN_POINT('Ctrl Pts',(46.1814998640537,-1.6947170054669,330.382953613631));
#64018=CARTESIAN_POINT('Ctrl Pts',(46.1737386091275,-1.82346927806306,330.430212975483));
#64019=CARTESIAN_POINT('Ctrl Pts',(46.1659773542014,-1.95014107319188,330.482824522875));
#64020=CARTESIAN_POINT('Ctrl Pts',(46.1582160992752,-2.07426941738349,330.54056175661));
#64021=CARTESIAN_POINT('Ctrl Pts',(46.1504424288706,-2.19859632647247,330.598391351103));
#64022=CARTESIAN_POINT('Ctrl Pts',(46.1426687584659,-2.32037130678936,330.661362837188));
#64023=CARTESIAN_POINT('Ctrl Pts',(46.1348950880612,-2.43915658380393,330.729204029436));
#64024=CARTESIAN_POINT('Ctrl Pts',(46.1274832838841,-2.55241237759628,330.793887197863));
#64025=CARTESIAN_POINT('Ctrl Pts',(46.1200714797069,-2.66295030153696,330.862996753041));
#64026=CARTESIAN_POINT('Ctrl Pts',(46.1126596755298,-2.77041806393055,330.936261965438));
#64027=CARTESIAN_POINT('Ctrl Pts',(46.104918932011,-2.88265529596461,331.012778722283));
#64028=CARTESIAN_POINT('Ctrl Pts',(46.0971781884923,-2.99190525043291,331.094075106653));
#64029=CARTESIAN_POINT('Ctrl Pts',(46.0894374449736,-3.09773120365827,331.179889471183));
#64030=CARTESIAN_POINT('Ctrl Pts',(46.0817062475476,-3.20342664947599,331.265598007133));
#64031=CARTESIAN_POINT('Ctrl Pts',(46.0739750501217,-3.30570619071891,331.355813192939));
#64032=CARTESIAN_POINT('Ctrl Pts',(46.0662438526958,-3.40416116482187,331.450229609338));
#64033=CARTESIAN_POINT('Ctrl Pts',(46.0585202979289,-3.50251881146617,331.544552690586));
#64034=CARTESIAN_POINT('Ctrl Pts',(46.050796743162,-3.59705913062881,331.643068467432));
#64035=CARTESIAN_POINT('Ctrl Pts',(46.0430731883951,-3.68740604249248,331.745430943997));
#64036=CARTESIAN_POINT('Ctrl Pts',(46.0353553798691,-3.7776857372343,331.847717263992));
#64037=CARTESIAN_POINT('Ctrl Pts',(46.0276375713431,-3.86377797347314,331.953844293326));
#64038=CARTESIAN_POINT('Ctrl Pts',(46.0199197628172,-3.94534340329375,332.063429126926));
#64039=CARTESIAN_POINT('Ctrl Pts',(46.0122051006626,-4.02687558078156,332.172969285332));
#64040=CARTESIAN_POINT('Ctrl Pts',(46.004490438508,-4.10388438634641,332.285964128855));
#64041=CARTESIAN_POINT('Ctrl Pts',(45.9967757763534,-4.17607085085154,332.401997823102));
#64042=CARTESIAN_POINT('Ctrl Pts',(45.9890625812274,-4.24824358830057,332.518009452256));
#64043=CARTESIAN_POINT('Ctrl Pts',(45.9813493861013,-4.31559560005693,332.63705844786));
#64044=CARTESIAN_POINT('Ctrl Pts',(45.9736361909752,-4.37787160560738,332.758700540464));
#64045=CARTESIAN_POINT('Ctrl Pts',(45.9659227545427,-4.44014955945599,332.880346438628));
#64046=CARTESIAN_POINT('Ctrl Pts',(45.9582093181101,-4.49735101127524,333.004585243802));
#64047=CARTESIAN_POINT('Ctrl Pts',(45.9504958816776,-4.54926716230683,333.130949078153));
#64048=CARTESIAN_POINT('Ctrl Pts',(45.9427804957732,-4.60119643447799,333.257344849338));
#64049=CARTESIAN_POINT('Ctrl Pts',(45.9350651098687,-4.64783759855045,333.38586635311));
#64050=CARTESIAN_POINT('Ctrl Pts',(45.9273497239643,-4.68903058355568,333.516027207467));
#64051=CARTESIAN_POINT('Ctrl Pts',(45.9196261803307,-4.73026712324766,333.64632568514));
#64052=CARTESIAN_POINT('Ctrl Pts',(45.9119026366971,-4.7660438609636,333.778266598071));
#64053=CARTESIAN_POINT('Ctrl Pts',(45.9041790930635,-4.79625094802646,333.91134950234));
#64054=CARTESIAN_POINT('Ctrl Pts',(45.896451155459,-4.8264752200848,334.044508118282));
#64055=CARTESIAN_POINT('Ctrl Pts',(45.8887232178545,-4.8511234588629,334.178809631967));
#64056=CARTESIAN_POINT('Ctrl Pts',(45.8809952802499,-4.87013743076969,334.313746061639));
#64057=CARTESIAN_POINT('Ctrl Pts',(45.8732556814828,-4.8891800940337,334.448886105228));
#64058=CARTESIAN_POINT('Ctrl Pts',(45.8655160827156,-4.90257147075479,334.584662586107));
#64059=CARTESIAN_POINT('Ctrl Pts',(45.8577764839485,-4.91030537113275,334.720564453362));
#64060=CARTESIAN_POINT('Ctrl Pts',(45.8524567814796,-4.91562115689539,334.813974657239));
#64061=CARTESIAN_POINT('Ctrl Pts',(45.8471370790106,-4.91826527278068,334.907444081807));
#64062=CARTESIAN_POINT('Ctrl Pts',(45.8418173765417,-4.91824993362185,335.000808040044));
#64063=CARTESIAN_POINT('',(44.0918173765497,-4.91824794925201,334.995508655169));
#64064=CARTESIAN_POINT('Ctrl Pts',(45.8418173765086,-4.91824993362175,335.000808040625));
#64065=CARTESIAN_POINT('Ctrl Pts',(45.8393521314244,-4.91824282517663,335.044074565478));
#64066=CARTESIAN_POINT('Ctrl Pts',(45.8368868863402,-4.91766479712218,335.08733580685));
#64067=CARTESIAN_POINT('Ctrl Pts',(45.8344216412559,-4.91651619026007,335.130581826494));
#64068=CARTESIAN_POINT('Ctrl Pts',(45.8266465624775,-4.91289362595788,335.266974435788));
#64069=CARTESIAN_POINT('Ctrl Pts',(45.8188714836991,-4.90358538870505,335.403431713215));
#64070=CARTESIAN_POINT('Ctrl Pts',(45.8110964049206,-4.88857715149386,335.539440910937));
#64071=CARTESIAN_POINT('Ctrl Pts',(45.8033308938716,-4.87358738287399,335.675282740682));
#64072=CARTESIAN_POINT('Ctrl Pts',(45.7955653828226,-4.85291161302988,335.810677203031));
#64073=CARTESIAN_POINT('Ctrl Pts',(45.7877998717736,-4.82658750698835,335.94511168646));
#64074=CARTESIAN_POINT('Ctrl Pts',(45.7800420602514,-4.80028950137461,336.079412877708));
#64075=CARTESIAN_POINT('Ctrl Pts',(45.7722842487292,-4.76835437918846,336.212755603099));
#64076=CARTESIAN_POINT('Ctrl Pts',(45.764526437207,-4.73087153887271,336.344632866319));
#64077=CARTESIAN_POINT('Ctrl Pts',(45.7567744636839,-4.69341690558295,336.476410887716));
#64078=CARTESIAN_POINT('Ctrl Pts',(45.7490224901609,-4.65042297039963,336.606725267558));
#64079=CARTESIAN_POINT('Ctrl Pts',(45.7412705166379,-4.60203001953569,336.73508004478));
#64080=CARTESIAN_POINT('Ctrl Pts',(45.7335218260803,-4.55365756311524,336.863380463677));
#64081=CARTESIAN_POINT('Ctrl Pts',(45.7257731355226,-4.49989077628166,336.989722565571));
#64082=CARTESIAN_POINT('Ctrl Pts',(45.718024444965,-4.44091946384773,337.113626593824));
#64083=CARTESIAN_POINT('Ctrl Pts',(45.7102773665872,-4.38196042088796,337.237504842808));
#64084=CARTESIAN_POINT('Ctrl Pts',(45.7025302882094,-4.31779917405665,337.358945674413));
#64085=CARTESIAN_POINT('Ctrl Pts',(45.6947832098316,-4.24867307617483,337.477490697114));
#64086=CARTESIAN_POINT('Ctrl Pts',(45.6870360665258,-4.17954639894964,337.596036713337));
#64087=CARTESIAN_POINT('Ctrl Pts',(45.67928892322,-4.10545498457594,337.711686534588));
#64088=CARTESIAN_POINT('Ctrl Pts',(45.6715417799142,-4.02668121375347,337.824008049795));
#64089=CARTESIAN_POINT('Ctrl Pts',(45.6637928948861,-3.94788973291502,337.936354817262));
#64090=CARTESIAN_POINT('Ctrl Pts',(45.656044009858,-3.86441402527817,338.045371469748));
#64091=CARTESIAN_POINT('Ctrl Pts',(45.6482951248299,-3.77657845958326,338.150656788848));
#64092=CARTESIAN_POINT('Ctrl Pts',(45.6405380150551,-3.68864966431141,338.256053858873));
#64093=CARTESIAN_POINT('Ctrl Pts',(45.6327809052804,-3.5963520177112,338.357711383476));
#64094=CARTESIAN_POINT('Ctrl Pts',(45.6250237955057,-3.50004903983596,338.455262621168));
#64095=CARTESIAN_POINT('Ctrl Pts',(45.6172625405795,-3.40369460072845,338.552865987123));
#64096=CARTESIAN_POINT('Ctrl Pts',(45.6095012856534,-3.30333085142551,338.646358427598));
#64097=CARTESIAN_POINT('Ctrl Pts',(45.6017400307272,-3.19935574695672,338.735412409215));
#64098=CARTESIAN_POINT('Ctrl Pts',(45.5939663603225,-3.0952143162062,338.82460884818));
#64099=CARTESIAN_POINT('Ctrl Pts',(45.5861926899179,-2.98745029356408,338.909352398465));
#64100=CARTESIAN_POINT('Ctrl Pts',(45.5784190195132,-2.8764927751468,338.989357388982));
#64101=CARTESIAN_POINT('Ctrl Pts',(45.5710072153362,-2.77070035590728,339.065638127943));
#64102=CARTESIAN_POINT('Ctrl Pts',(45.5635954111591,-2.66200530443199,339.137611380129));
#64103=CARTESIAN_POINT('Ctrl Pts',(45.5561836069821,-2.55079997644987,339.205068672762));
#64104=CARTESIAN_POINT('Ctrl Pts',(45.5484085282036,-2.43414414407918,339.275832248251));
#64105=CARTESIAN_POINT('Ctrl Pts',(45.5406334494252,-2.314357087019,339.341849615695));
#64106=CARTESIAN_POINT('Ctrl Pts',(45.5328583706467,-2.19186223269826,339.402831249931));
#64107=CARTESIAN_POINT('Ctrl Pts',(45.5250928595977,-2.06951811609416,339.463737842384));
#64108=CARTESIAN_POINT('Ctrl Pts',(45.5173273485488,-1.94447317875349,339.519620858933));
#64109=CARTESIAN_POINT('Ctrl Pts',(45.5095618374997,-1.81717886934789,339.570234569395));
#64110=CARTESIAN_POINT('Ctrl Pts',(45.5018040259775,-1.69001077262058,339.620798096216));
#64111=CARTESIAN_POINT('Ctrl Pts',(45.4940462144554,-1.56059810304602,339.666102570577));
#64112=CARTESIAN_POINT('Ctrl Pts',(45.4862884029332,-1.42941558326661,339.705948804738));
#64113=CARTESIAN_POINT('Ctrl Pts',(45.4785364294102,-1.29833178249355,339.745765053344));
#64114=CARTESIAN_POINT('Ctrl Pts',(45.4707844558872,-1.16548115503049,339.780131124383));
#64115=CARTESIAN_POINT('Ctrl Pts',(45.4630324823642,-1.03135668203651,339.808896594534));
#64116=CARTESIAN_POINT('Ctrl Pts',(45.4552837918066,-0.897289010836286,
339.837649882491));
#64117=CARTESIAN_POINT('Ctrl Pts',(45.4475351012489,-0.761948948469715,
339.860807205221));
#64118=CARTESIAN_POINT('Ctrl Pts',(45.4397864106913,-0.625842646804415,
339.878268549797));
#64119=CARTESIAN_POINT('Ctrl Pts',(45.4320393323134,-0.489764663192144,
339.895726261394));
#64120=CARTESIAN_POINT('Ctrl Pts',(45.4242922539356,-0.352921144837132,
339.907490302369));
#64121=CARTESIAN_POINT('Ctrl Pts',(45.4165451755578,-0.215826008181983,
339.913512205815));
#64122=CARTESIAN_POINT('Ctrl Pts',(45.408798032252,-0.0787297225375417,
339.919534159731));
#64123=CARTESIAN_POINT('Ctrl Pts',(45.4010508889462,0.058617795115445,339.919813862977));
#64124=CARTESIAN_POINT('Ctrl Pts',(45.3933037456404,0.195700360956632,339.914354935413));
#64125=CARTESIAN_POINT('Ctrl Pts',(45.3855548606123,0.33281374586878,339.908894780567));
#64126=CARTESIAN_POINT('Ctrl Pts',(45.3778059755842,0.469661669949456,339.897693443173));
#64127=CARTESIAN_POINT('Ctrl Pts',(45.3700570905561,0.605731205545558,339.880806569526));
#64128=CARTESIAN_POINT('Ctrl Pts',(45.3622999807814,0.741945166752789,339.863901771977));
#64129=CARTESIAN_POINT('Ctrl Pts',(45.3545428710067,0.877378700573073,339.841299431537));
#64130=CARTESIAN_POINT('Ctrl Pts',(45.346785761232,1.01152668470462,339.813106775112));
#64131=CARTESIAN_POINT('Ctrl Pts',(45.3390245063058,1.14574635322976,339.784899053433));
#64132=CARTESIAN_POINT('Ctrl Pts',(45.3312632513797,1.27867872461738,339.751095159613));
#64133=CARTESIAN_POINT('Ctrl Pts',(45.3235019964535,1.40983301276093,339.711852495424));
#64134=CARTESIAN_POINT('Ctrl Pts',(45.3157283260488,1.54119710502226,339.67254705576));
#64135=CARTESIAN_POINT('Ctrl Pts',(45.3079546556442,1.67077706053139,339.627785587719));
#64136=CARTESIAN_POINT('Ctrl Pts',(45.3001809852395,1.79810044384551,339.577774334362));
#64137=CARTESIAN_POINT('Ctrl Pts',(45.2927691810624,1.91949689303481,339.53009111688));
#64138=CARTESIAN_POINT('Ctrl Pts',(45.2853573768853,2.03884186555602,339.477635985769));
#64139=CARTESIAN_POINT('Ctrl Pts',(45.2779455727082,2.15574772600152,339.420626064749));
#64140=CARTESIAN_POINT('Ctrl Pts',(45.2701704939297,2.27838349091159,339.360821917676));
#64141=CARTESIAN_POINT('Ctrl Pts',(45.2623954151513,2.39872255356924,339.295816211449));
#64142=CARTESIAN_POINT('Ctrl Pts',(45.2546203363729,2.51629230521065,339.225808336548));
#64143=CARTESIAN_POINT('Ctrl Pts',(45.2468548253238,2.63371737978781,339.155886610794));
#64144=CARTESIAN_POINT('Ctrl Pts',(45.2390893142748,2.74837959128799,339.080975162089));
#64145=CARTESIAN_POINT('Ctrl Pts',(45.2313238032258,2.85982799517733,339.00132064455));
#64146=CARTESIAN_POINT('Ctrl Pts',(45.2235659917036,2.97116589764981,338.921745104697));
#64147=CARTESIAN_POINT('Ctrl Pts',(45.2158081801814,3.0792960178723,338.8374360806));
#64148=CARTESIAN_POINT('Ctrl Pts',(45.2080503686592,3.18379395496485,338.748684984742));
#64149=CARTESIAN_POINT('Ctrl Pts',(45.2002983951362,3.28821325404591,338.660000676898));
#64150=CARTESIAN_POINT('Ctrl Pts',(45.1925464216132,3.38900551383834,338.566881202984));
#64151=CARTESIAN_POINT('Ctrl Pts',(45.1847944480901,3.4857774597702,338.469659718684));
#64152=CARTESIAN_POINT('Ctrl Pts',(45.1770457575325,3.58250842272536,338.37247940774));
#64153=CARTESIAN_POINT('Ctrl Pts',(45.1692970669749,3.6752221830072,338.271200818039));
#64154=CARTESIAN_POINT('Ctrl Pts',(45.1615483764173,3.76356072979137,338.16619546075));
#64155=CARTESIAN_POINT('Ctrl Pts',(45.1538012980394,3.85188089700307,338.061211950702));
#64156=CARTESIAN_POINT('Ctrl Pts',(45.1460542196616,3.93582740989455,337.95250351428));
#64157=CARTESIAN_POINT('Ctrl Pts',(45.1383071412838,4.01508140193562,337.840476086562));
#64158=CARTESIAN_POINT('Ctrl Pts',(45.130559997978,4.09433605820147,337.728447719946));
#64159=CARTESIAN_POINT('Ctrl Pts',(45.1228128546722,4.16889788942985,337.613100625647));
#64160=CARTESIAN_POINT('Ctrl Pts',(45.1150657113664,4.23849060295287,337.494870832564));
#64161=CARTESIAN_POINT('Ctrl Pts',(45.1073168263383,4.30809896239539,337.376614458914));
#64162=CARTESIAN_POINT('Ctrl Pts',(45.0995679413101,4.3727357828634,337.255474433636));
#64163=CARTESIAN_POINT('Ctrl Pts',(45.091819056282,4.43217028392748,337.131912201938));
#64164=CARTESIAN_POINT('Ctrl Pts',(45.0840619465073,4.49166786938506,337.00821882001));
#64165=CARTESIAN_POINT('Ctrl Pts',(45.0763048367326,4.54595193543428,336.882098448739));
#64166=CARTESIAN_POINT('Ctrl Pts',(45.0685477269579,4.59483930080565,336.754033882875));
#64167=CARTESIAN_POINT('Ctrl Pts',(45.0607864720317,4.64375279002193,336.625900883401));
#64168=CARTESIAN_POINT('Ctrl Pts',(45.0530252171055,4.68726370835036,336.495821989701));
#64169=CARTESIAN_POINT('Ctrl Pts',(45.0452639621793,4.72523882577344,336.36429509341));
#64170=CARTESIAN_POINT('Ctrl Pts',(45.0374902917747,4.76327469100834,336.23255779695));
#64171=CARTESIAN_POINT('Ctrl Pts',(45.02971662137,4.79575696681091,336.099368249126));
#64172=CARTESIAN_POINT('Ctrl Pts',(45.0219429509654,4.82260342544471,335.965235340934));
#64173=CARTESIAN_POINT('Ctrl Pts',(45.0145311467884,4.84820017496996,335.837346351891));
#64174=CARTESIAN_POINT('Ctrl Pts',(45.0071193426114,4.86867394878192,335.708600137068));
#64175=CARTESIAN_POINT('Ctrl Pts',(44.9997075384343,4.88399755908635,335.579440165452));
#64176=CARTESIAN_POINT('Ctrl Pts',(44.9919324596559,4.90007222517866,335.443949678877));
#64177=CARTESIAN_POINT('Ctrl Pts',(44.9841573808775,4.91052991183441,335.307575676101));
#64178=CARTESIAN_POINT('Ctrl Pts',(44.976382302099,4.91528253504174,335.170823485545));
#64179=CARTESIAN_POINT('Ctrl Pts',(44.96861679105,4.92002930984365,335.034239577265));
#64180=CARTESIAN_POINT('Ctrl Pts',(44.960851280001,4.91908497642098,334.897278794092));
#64181=CARTESIAN_POINT('Ctrl Pts',(44.953085768952,4.91241291952042,334.760453823598));
#64182=CARTESIAN_POINT('Ctrl Pts',(44.9453279574298,4.90574747798371,334.623764515461));
#64183=CARTESIAN_POINT('Ctrl Pts',(44.9375701459076,4.89336563352381,334.487211139922));
#64184=CARTESIAN_POINT('Ctrl Pts',(44.9298123343854,4.8752827734466,334.351308284749));
#64185=CARTESIAN_POINT('Ctrl Pts',(44.9220603608624,4.85721352129504,334.215507700786));
#64186=CARTESIAN_POINT('Ctrl Pts',(44.9143083873394,4.83345184429638,334.080357048689));
#64187=CARTESIAN_POINT('Ctrl Pts',(44.9065564138164,4.80406507673578,333.946367331093));
#64188=CARTESIAN_POINT('Ctrl Pts',(44.8988077232587,4.77469075448868,333.812434358223));
#64189=CARTESIAN_POINT('Ctrl Pts',(44.8910590327011,4.73969616332807,333.679661722989));
#64190=CARTESIAN_POINT('Ctrl Pts',(44.8833103421435,4.69919997472217,333.548551530342));
#64191=CARTESIAN_POINT('Ctrl Pts',(44.8755632637656,4.65871221168655,333.417468616267));
#64192=CARTESIAN_POINT('Ctrl Pts',(44.8678161853878,4.61272524328237,333.288047830019));
#64193=CARTESIAN_POINT('Ctrl Pts',(44.8600691070099,4.56140787200017,333.160776988031));
#64194=CARTESIAN_POINT('Ctrl Pts',(44.8523219637041,4.51009007062896,333.033505079391));
#64195=CARTESIAN_POINT('Ctrl Pts',(44.8445748203984,4.45344192344516,332.908383513464));
#64196=CARTESIAN_POINT('Ctrl Pts',(44.8368276770925,4.3916805786366,332.785880590906));
#64197=CARTESIAN_POINT('Ctrl Pts',(44.8290787920645,4.32990534856658,332.663350127091));
#64198=CARTESIAN_POINT('Ctrl Pts',(44.8213299070363,4.26301480931614,332.543439827102));
#64199=CARTESIAN_POINT('Ctrl Pts',(44.8135810220082,4.19127211147331,332.426593473606));
#64200=CARTESIAN_POINT('Ctrl Pts',(44.8058239122335,4.11945326518965,332.309623098184));
#64201=CARTESIAN_POINT('Ctrl Pts',(44.7980668024588,4.04277217728585,332.195723499263));
#64202=CARTESIAN_POINT('Ctrl Pts',(44.790309692684,3.96153571027199,332.085309985824));
#64203=CARTESIAN_POINT('Ctrl Pts',(44.7825484377578,3.88025583308765,331.974837470933));
#64204=CARTESIAN_POINT('Ctrl Pts',(44.7747871828317,3.7944159708271,331.867855058139));
#64205=CARTESIAN_POINT('Ctrl Pts',(44.7670259279055,3.70436271278245,331.76474422114));
#64206=CARTESIAN_POINT('Ctrl Pts',(44.7592522575008,3.61416539887323,331.661468440405));
#64207=CARTESIAN_POINT('Ctrl Pts',(44.7514785870963,3.51974148990276,331.562076894961));
#64208=CARTESIAN_POINT('Ctrl Pts',(44.7437049166916,3.42147442502101,331.466914121985));
#64209=CARTESIAN_POINT('Ctrl Pts',(44.7362931125145,3.32778171565066,331.376181198985));
#64210=CARTESIAN_POINT('Ctrl Pts',(44.7288813083373,3.23059581071873,331.2892924015));
#64211=CARTESIAN_POINT('Ctrl Pts',(44.7214695041601,3.13027491988188,331.206510578839));
#64212=CARTESIAN_POINT('Ctrl Pts',(44.7136944253817,3.02503700334512,331.119671372456));
#64213=CARTESIAN_POINT('Ctrl Pts',(44.7059193466033,2.91601644931012,331.037077482602));
#64214=CARTESIAN_POINT('Ctrl Pts',(44.6981442678248,2.80359053191454,330.959076443205));
#64215=CARTESIAN_POINT('Ctrl Pts',(44.6903787567758,2.69130296176771,330.881171389053));
#64216=CARTESIAN_POINT('Ctrl Pts',(44.6826132457268,2.57561868426577,330.807848160592));
#64217=CARTESIAN_POINT('Ctrl Pts',(44.6748477346778,2.45694901471351,330.739414993032));
#64218=CARTESIAN_POINT('Ctrl Pts',(44.6670899231556,2.33839700648403,330.671049677158));
#64219=CARTESIAN_POINT('Ctrl Pts',(44.6593321116334,2.21686583324678,330.607564967384));
#64220=CARTESIAN_POINT('Ctrl Pts',(44.6515743001112,2.09279654978999,330.549226397166));
#64221=CARTESIAN_POINT('Ctrl Pts',(44.6438223265881,1.96882063240347,330.490931728572));
#64222=CARTESIAN_POINT('Ctrl Pts',(44.6360703530651,1.8423107588735,330.437775656901));
#64223=CARTESIAN_POINT('Ctrl Pts',(44.6283183795421,1.7137330806627,330.389978092162));
#64224=CARTESIAN_POINT('Ctrl Pts',(44.6205696889845,1.58520985517514,330.342200769721));
#64225=CARTESIAN_POINT('Ctrl Pts',(44.6128209984268,1.45462093236078,330.299777576588));
#64226=CARTESIAN_POINT('Ctrl Pts',(44.6050723078692,1.3224527629256,330.262880437193));
#64227=CARTESIAN_POINT('Ctrl Pts',(44.5973252294914,1.19031209218196,330.225990974556));
#64228=CARTESIAN_POINT('Ctrl Pts',(44.5895781511136,1.05659320462003,330.194625383774));
#64229=CARTESIAN_POINT('Ctrl Pts',(44.5818310727357,0.921797664197005,330.168905700695));
#64230=CARTESIAN_POINT('Ctrl Pts',(44.5740839294299,0.787000994057517,330.143185802059));
#64231=CARTESIAN_POINT('Ctrl Pts',(44.5663367861241,0.651128037006763,330.123111978764));
#64232=CARTESIAN_POINT('Ctrl Pts',(44.5585896428183,0.514690108401413,330.108755050622));
#64233=CARTESIAN_POINT('Ctrl Pts',(44.5508407577902,0.378221505653054,330.094394894738));
#64234=CARTESIAN_POINT('Ctrl Pts',(44.5430918727621,0.241188067251386,330.085754232465));
#64235=CARTESIAN_POINT('Ctrl Pts',(44.535342987734,0.104105385391348,330.082851931126));
#64236=CARTESIAN_POINT('Ctrl Pts',(44.5275858779592,-0.0331227974435458,
330.079946549254));
#64237=CARTESIAN_POINT('Ctrl Pts',(44.5198287681845,-0.170399936742121,
330.082791703458));
#64238=CARTESIAN_POINT('Ctrl Pts',(44.5120716584098,-0.307210729410955,
330.091354094026));
#64239=CARTESIAN_POINT('Ctrl Pts',(44.5043104034836,-0.444094629393122,
330.099921060062));
#64240=CARTESIAN_POINT('Ctrl Pts',(44.4965491485574,-0.580511297640694,
330.114211309338));
#64241=CARTESIAN_POINT('Ctrl Pts',(44.4887878936312,-0.71595238542965,330.134139824831));
#64242=CARTESIAN_POINT('Ctrl Pts',(44.4810142232266,-0.851610134818735,
330.154100219454));
#64243=CARTESIAN_POINT('Ctrl Pts',(44.4732405528219,-0.986288800994723,
330.179716830628));
#64244=CARTESIAN_POINT('Ctrl Pts',(44.4654668824172,-1.11949115436959,330.210853665027));
#64245=CARTESIAN_POINT('Ctrl Pts',(44.4580550782402,-1.24649290614678,330.240541072293));
#64246=CARTESIAN_POINT('Ctrl Pts',(44.4506432740633,-1.37215241932634,330.275246259122));
#64247=CARTESIAN_POINT('Ctrl Pts',(44.4432314698863,-1.4960548105155,330.314810242217));
#64248=CARTESIAN_POINT('Ctrl Pts',(44.4354563911078,-1.62603002698441,330.356313373979));
#64249=CARTESIAN_POINT('Ctrl Pts',(44.4276813123294,-1.75448226841276,330.403294790682));
#64250=CARTESIAN_POINT('Ctrl Pts',(44.419906233551,-1.88091512142092,330.455625305005));
#64251=CARTESIAN_POINT('Ctrl Pts',(44.412140722502,-2.00719239075435,330.507891423299));
#64252=CARTESIAN_POINT('Ctrl Pts',(44.4043752114529,-2.13145485836897,330.56549339406));
#64253=CARTESIAN_POINT('Ctrl Pts',(44.3966097004039,-2.25322073638608,330.628252137232));
#64254=CARTESIAN_POINT('Ctrl Pts',(44.3888518888817,-2.37486588318055,330.690948654927));
#64255=CARTESIAN_POINT('Ctrl Pts',(44.3810940773596,-2.49401902131213,330.758791592045));
#64256=CARTESIAN_POINT('Ctrl Pts',(44.3733362658374,-2.61021817797946,330.831553751595));
#64257=CARTESIAN_POINT('Ctrl Pts',(44.3655842923144,-2.72632989109651,330.904261155311));
#64258=CARTESIAN_POINT('Ctrl Pts',(44.3578323187914,-2.83949171750165,330.981880206456));
#64259=CARTESIAN_POINT('Ctrl Pts',(44.3500803452684,-2.94926646887166,331.064137914244));
#64260=CARTESIAN_POINT('Ctrl Pts',(44.3423316547108,-3.05899473056944,331.146360785844));
#64261=CARTESIAN_POINT('Ctrl Pts',(44.3345829641532,-3.16533845806015,331.233218172985));
#64262=CARTESIAN_POINT('Ctrl Pts',(44.3268342735956,-3.26788983003292,331.324394047063));
#64263=CARTESIAN_POINT('Ctrl Pts',(44.3190871952177,-3.37041986533623,331.415550951239));
#64264=CARTESIAN_POINT('Ctrl Pts',(44.3113401168399,-3.46915882262787,331.511024295628));
#64265=CARTESIAN_POINT('Ctrl Pts',(44.3035930384621,-3.56373265432442,331.610458344997));
#64266=CARTESIAN_POINT('Ctrl Pts',(44.2958458951563,-3.65830727864065,331.709893227719));
#64267=CARTESIAN_POINT('Ctrl Pts',(44.2880987518504,-3.74871643835432,331.813288598404));
#64268=CARTESIAN_POINT('Ctrl Pts',(44.2803516085446,-3.83462387749575,331.920252805726));
#64269=CARTESIAN_POINT('Ctrl Pts',(44.2726027235165,-3.92055063045348,332.027241060872));
#64270=CARTESIAN_POINT('Ctrl Pts',(44.2648538384884,-4.00197340419532,332.137799444548));
#64271=CARTESIAN_POINT('Ctrl Pts',(44.2571049534603,-4.07859731626657,332.251504594466));
#64272=CARTESIAN_POINT('Ctrl Pts',(44.2493478436856,-4.15530255774978,332.365330432205));
#64273=CARTESIAN_POINT('Ctrl Pts',(44.2415907339108,-4.22719854391608,332.482309383515));
#64274=CARTESIAN_POINT('Ctrl Pts',(44.2338336241361,-4.29403441713169,332.601990098647));
#64275=CARTESIAN_POINT('Ctrl Pts',(44.22607236921,-4.3609060053008,332.721734767326));
#64276=CARTESIAN_POINT('Ctrl Pts',(44.2183111142838,-4.42271191659104,332.844183727834));
#64277=CARTESIAN_POINT('Ctrl Pts',(44.2105498593577,-4.4792485469673,332.968863491296));
#64278=CARTESIAN_POINT('Ctrl Pts',(44.202776188953,-4.535875617527,333.093742701746));
#64279=CARTESIAN_POINT('Ctrl Pts',(44.1950025185483,-4.58721641681267,333.220859483564));
#64280=CARTESIAN_POINT('Ctrl Pts',(44.1872288481436,-4.63311622505206,333.349722111989));
#64281=CARTESIAN_POINT('Ctrl Pts',(44.1798170439665,-4.67687938617506,333.472586154058));
#64282=CARTESIAN_POINT('Ctrl Pts',(44.1724052397894,-4.71569662709086,333.597036887497));
#64283=CARTESIAN_POINT('Ctrl Pts',(44.1649934356124,-4.74947712303642,333.722639393024));
#64284=CARTESIAN_POINT('Ctrl Pts',(44.1550194885169,-4.79493499960332,333.891660688684));
#64285=CARTESIAN_POINT('Ctrl Pts',(44.1450455414214,-4.83139011897056,334.063198460588));
#64286=CARTESIAN_POINT('Ctrl Pts',(44.1350715943259,-4.85861284657801,334.236413548073));
#64287=CARTESIAN_POINT('Ctrl Pts',(44.125280948658,-4.88533527427563,334.406445284722));
#64288=CARTESIAN_POINT('Ctrl Pts',(44.1154903029901,-4.90316156846626,334.578093430656));
#64289=CARTESIAN_POINT('Ctrl Pts',(44.1056996573222,-4.91191959658431,334.750542710688));
#64290=CARTESIAN_POINT('Ctrl Pts',(44.101072230398,-4.91605896966456,334.832048718416));
#64291=CARTESIAN_POINT('Ctrl Pts',(44.0964448034738,-4.9181732720366,334.91373335727));
#64292=CARTESIAN_POINT('Ctrl Pts',(44.0918173765497,-4.91824794925201,334.995508655169));
#64293=CARTESIAN_POINT('',(42.3418173764774,-4.91824979877521,335.001406892883));
#64294=CARTESIAN_POINT('Ctrl Pts',(44.0918173765087,-4.91824794925267,334.995508655893));
#64295=CARTESIAN_POINT('Ctrl Pts',(44.0841435815425,-4.9183717886037,335.131118980953));
#64296=CARTESIAN_POINT('Ctrl Pts',(44.0764697865763,-4.9128826557159,335.266862873519));
#64297=CARTESIAN_POINT('Ctrl Pts',(44.0687959916102,-4.90177426318535,335.402233931032));
#64298=CARTESIAN_POINT('Ctrl Pts',(44.0611261793002,-4.89067163584767,335.537534731733));
#64299=CARTESIAN_POINT('Ctrl Pts',(44.0534563669902,-4.87395558128148,335.672462684876));
#64300=CARTESIAN_POINT('Ctrl Pts',(44.0457865546802,-4.85167188648578,335.806512844525));
#64301=CARTESIAN_POINT('Ctrl Pts',(44.0381187493999,-4.82939402286746,335.940527926047));
#64302=CARTESIAN_POINT('Ctrl Pts',(44.0304509441195,-4.80155148122578,336.073665276805));
#64303=CARTESIAN_POINT('Ctrl Pts',(44.0227831388392,-4.76824169222321,336.205426989512));
#64304=CARTESIAN_POINT('Ctrl Pts',(44.0151155972268,-4.73493304862312,336.337184171413));
#64305=CARTESIAN_POINT('Ctrl Pts',(44.0074480556143,-4.69615762947972,336.467565421799));
#64306=CARTESIAN_POINT('Ctrl Pts',(43.9997805140019,-4.65206345607596,336.596085418498));
#64307=CARTESIAN_POINT('Ctrl Pts',(43.9921114931604,-4.6079607759841,336.724630209393));
#64308=CARTESIAN_POINT('Ctrl Pts',(43.9844424723189,-4.55853743080427,336.851312654494));
#64309=CARTESIAN_POINT('Ctrl Pts',(43.9767734514774,-4.50399036886354,336.975665411876));
#64310=CARTESIAN_POINT('Ctrl Pts',(43.9690964997169,-4.44938689707111,337.10014676868));
#64311=CARTESIAN_POINT('Ctrl Pts',(43.9614195479563,-4.38964928656962,337.222293259315));
#64312=CARTESIAN_POINT('Ctrl Pts',(43.9537425961958,-4.3250216222201,337.341659887735));
#64313=CARTESIAN_POINT('Ctrl Pts',(43.9460616123199,-4.26036001390261,337.461089210314));
#64314=CARTESIAN_POINT('Ctrl Pts',(43.9383806284439,-4.19080344141514,337.577735420031));
#64315=CARTESIAN_POINT('Ctrl Pts',(43.930699644568,-4.11663984716378,337.69118179082));
#64316=CARTESIAN_POINT('Ctrl Pts',(43.9230064624217,-4.04235847274442,337.804808327266));
#64317=CARTESIAN_POINT('Ctrl Pts',(43.9153132802754,-3.9634556925758,337.915224547863));
#64318=CARTESIAN_POINT('Ctrl Pts',(43.9076200981291,-3.88026076241978,338.022045578433));
#64319=CARTESIAN_POINT('Ctrl Pts',(43.9006651991989,-3.80504970934187,338.118615431727));
#64320=CARTESIAN_POINT('Ctrl Pts',(43.8937103002687,-3.72633143770651,338.212247304725));
#64321=CARTESIAN_POINT('Ctrl Pts',(43.8867554013385,-3.64437438191438,338.302683519041));
#64322=CARTESIAN_POINT('Ctrl Pts',(43.87898032256,-3.5527522646666,338.4037847281));
#64323=CARTESIAN_POINT('Ctrl Pts',(43.8712052437816,-3.45677509712101,338.501230175163));
#64324=CARTESIAN_POINT('Ctrl Pts',(43.8634301650032,-3.35676612079108,338.594621575745));
#64325=CARTESIAN_POINT('Ctrl Pts',(43.8556646539542,-3.2568802118734,338.687898052262));
#64326=CARTESIAN_POINT('Ctrl Pts',(43.8478991429051,-3.15297264887849,338.777130144279));
#64327=CARTESIAN_POINT('Ctrl Pts',(43.8401336318561,-3.04540602346491,338.861953549014));
#64328=CARTESIAN_POINT('Ctrl Pts',(43.8323758203339,-2.93794605067338,338.946692851097));
#64329=CARTESIAN_POINT('Ctrl Pts',(43.8246180088117,-2.82683454027944,339.027031924415));
#64330=CARTESIAN_POINT('Ctrl Pts',(43.8168601972895,-2.71246966783161,339.102644435433));
#64331=CARTESIAN_POINT('Ctrl Pts',(43.8091082237665,-2.59819085857779,339.178200045639));
#64332=CARTESIAN_POINT('Ctrl Pts',(43.8013562502436,-2.48066388514998,339.249035958655));
#64333=CARTESIAN_POINT('Ctrl Pts',(43.7936042767206,-2.36031833378726,339.314867370579));
#64334=CARTESIAN_POINT('Ctrl Pts',(43.785855586163,-2.24002374883649,339.380670902862));
#64335=CARTESIAN_POINT('Ctrl Pts',(43.7781068956054,-2.1169133022824,339.441473962214));
#64336=CARTESIAN_POINT('Ctrl Pts',(43.7703582050478,-1.99144358419451,339.49703630333));
#64337=CARTESIAN_POINT('Ctrl Pts',(43.7626111266699,-1.86599997112941,339.552587084237));
#64338=CARTESIAN_POINT('Ctrl Pts',(43.7548640482921,-1.73819842007227,339.602899157572));
#64339=CARTESIAN_POINT('Ctrl Pts',(43.7471169699143,-1.60851766738135,339.647779467253));
#64340=CARTESIAN_POINT('Ctrl Pts',(43.7393698266085,-1.47883582784099,339.692660153075));
#64341=CARTESIAN_POINT('Ctrl Pts',(43.7316226833027,-1.34727512463209,339.732108856609));
#64342=CARTESIAN_POINT('Ctrl Pts',(43.7238755399969,-1.21433132587712,339.765981797436));
#64343=CARTESIAN_POINT('Ctrl Pts',(43.7161266549688,-1.08135763853389,339.79986235362));
#64344=CARTESIAN_POINT('Ctrl Pts',(43.7083777699407,-0.947000615589204,
339.828164556184));
#64345=CARTESIAN_POINT('Ctrl Pts',(43.7006288849126,-0.811767745687939,
339.850795418234));
#64346=CARTESIAN_POINT('Ctrl Pts',(43.6928717751379,-0.676391338220975,
339.873450300915));
#64347=CARTESIAN_POINT('Ctrl Pts',(43.6851146653632,-0.540137612890575,
339.89042175371));
#64348=CARTESIAN_POINT('Ctrl Pts',(43.6773575555884,-0.40352129152778,339.901668453678));
#64349=CARTESIAN_POINT('Ctrl Pts',(43.6695963006623,-0.266831966770898,
339.912921163523));
#64350=CARTESIAN_POINT('Ctrl Pts',(43.6618350457361,-0.129780050257217,
339.91844300923));
#64351=CARTESIAN_POINT('Ctrl Pts',(43.6540737908099,0.00711916348447759,
339.918244847505));
#64352=CARTESIAN_POINT('Ctrl Pts',(43.6463001204053,0.144237371352623,339.918046368786));
#64353=CARTESIAN_POINT('Ctrl Pts',(43.6385264500007,0.281201997602636,339.912109614865));
#64354=CARTESIAN_POINT('Ctrl Pts',(43.630752779596,0.41750140309195,339.900497489125));
#64355=CARTESIAN_POINT('Ctrl Pts',(43.6233409754188,0.547456038465653,339.889425910631));
#64356=CARTESIAN_POINT('Ctrl Pts',(43.6159291712417,0.676805705832155,339.873195482469));
#64357=CARTESIAN_POINT('Ctrl Pts',(43.6085173670645,0.80511693861203,339.851903727163));
#64358=CARTESIAN_POINT('Ctrl Pts',(43.600742288286,0.939717087128626,339.829568399505));
#64359=CARTESIAN_POINT('Ctrl Pts',(43.5929672095076,1.07359979499925,339.801592474557));
#64360=CARTESIAN_POINT('Ctrl Pts',(43.5851921307291,1.20625521177272,339.768032238416));
#64361=CARTESIAN_POINT('Ctrl Pts',(43.5774266196801,1.33874738761023,339.734513300281));
#64362=CARTESIAN_POINT('Ctrl Pts',(43.5696611086311,1.47001490202124,339.695423818914));
#64363=CARTESIAN_POINT('Ctrl Pts',(43.5618955975821,1.59955518587435,339.650871560239));
#64364=CARTESIAN_POINT('Ctrl Pts',(43.5541377860599,1.72896703015913,339.606363475258));
#64365=CARTESIAN_POINT('Ctrl Pts',(43.5463799745377,1.856654684722,339.556403518135));
#64366=CARTESIAN_POINT('Ctrl Pts',(43.5386221630155,1.98212825309632,339.501149925383));
#64367=CARTESIAN_POINT('Ctrl Pts',(43.5308701894925,2.10750739863111,339.445937912712));
#64368=CARTESIAN_POINT('Ctrl Pts',(43.5231182159695,2.23067541812224,339.385440350525));
#64369=CARTESIAN_POINT('Ctrl Pts',(43.5153662424465,2.35116034013002,339.319864363322));
#64370=CARTESIAN_POINT('Ctrl Pts',(43.5076175518889,2.47159423670197,339.254316147588));
#64371=CARTESIAN_POINT('Ctrl Pts',(43.4998688613313,2.5893469531945,339.183693970929));
#64372=CARTESIAN_POINT('Ctrl Pts',(43.4921201707736,2.70396937511788,339.108251779154));
#64373=CARTESIAN_POINT('Ctrl Pts',(43.4843730923958,2.81856794888919,339.032825283757));
#64374=CARTESIAN_POINT('Ctrl Pts',(43.476626014018,2.93003719724586,338.952580982734));
#64375=CARTESIAN_POINT('Ctrl Pts',(43.4688789356402,3.03795570349791,338.867816981979));
#64376=CARTESIAN_POINT('Ctrl Pts',(43.4611317923344,3.14587511421085,338.78305227082));
#64377=CARTESIAN_POINT('Ctrl Pts',(43.4533846490285,3.25024341607144,338.693768025815));
#64378=CARTESIAN_POINT('Ctrl Pts',(43.4456375057227,3.35067141248078,338.600303341121));
#64379=CARTESIAN_POINT('Ctrl Pts',(43.4378886206946,3.45112198723546,338.506817643581));
#64380=CARTESIAN_POINT('Ctrl Pts',(43.4301397356665,3.54763020769234,338.409149902393));
#64381=CARTESIAN_POINT('Ctrl Pts',(43.4223908506385,3.63984324796233,338.30767655504));
#64382=CARTESIAN_POINT('Ctrl Pts',(43.4146337408637,3.73215416410649,338.206095502827));
#64383=CARTESIAN_POINT('Ctrl Pts',(43.406876631089,3.82016052984577,338.10070106528));
#64384=CARTESIAN_POINT('Ctrl Pts',(43.3991195213143,3.90354905031887,337.991903720753));
#64385=CARTESIAN_POINT('Ctrl Pts',(43.3913582663881,3.98698213095089,337.883048238403));
#64386=CARTESIAN_POINT('Ctrl Pts',(43.383597011462,4.06579222487243,337.770786545488));
#64387=CARTESIAN_POINT('Ctrl Pts',(43.3758357565358,4.13970960628091,337.655557839356));
#64388=CARTESIAN_POINT('Ctrl Pts',(43.3680620861311,4.21374523141002,337.540144804847));
#64389=CARTESIAN_POINT('Ctrl Pts',(43.3602884157265,4.28287230667495,337.421755610424));
#64390=CARTESIAN_POINT('Ctrl Pts',(43.3525147453218,4.34686685157477,337.300854544985));
#64391=CARTESIAN_POINT('Ctrl Pts',(43.3451029411448,4.40788243501296,337.185581453231));
#64392=CARTESIAN_POINT('Ctrl Pts',(43.3376911369677,4.46423244880345,337.06802534241));
#64393=CARTESIAN_POINT('Ctrl Pts',(43.3302793327907,4.51576432808058,336.948603498851));
#64394=CARTESIAN_POINT('Ctrl Pts',(43.3225042540122,4.56982193826697,336.823328434999));
#64395=CARTESIAN_POINT('Ctrl Pts',(43.3147291752338,4.61874800155502,336.695604231441));
#64396=CARTESIAN_POINT('Ctrl Pts',(43.3069540964554,4.66231394078948,336.565890091935));
#64397=CARTESIAN_POINT('Ctrl Pts',(43.2991885854064,4.70582626936205,336.436335573936));
#64398=CARTESIAN_POINT('Ctrl Pts',(43.2914230743574,4.74399147471954,336.304796359277));
#64399=CARTESIAN_POINT('Ctrl Pts',(43.2836575633084,4.77662821053168,336.171753387387));
#64400=CARTESIAN_POINT('Ctrl Pts',(43.2758997517862,4.80923258692527,336.038842327991));
#64401=CARTESIAN_POINT('Ctrl Pts',(43.268141940264,4.83631930973145,335.904430855672));
#64402=CARTESIAN_POINT('Ctrl Pts',(43.2603841287418,4.85775633232206,335.769016565677));
#64403=CARTESIAN_POINT('Ctrl Pts',(43.2526321552188,4.87917722287348,335.633704179228));
#64404=CARTESIAN_POINT('Ctrl Pts',(43.2448801816957,4.89495681489762,335.497390861714));
#64405=CARTESIAN_POINT('Ctrl Pts',(43.2371282081727,4.90501387297808,335.360585590939));
#64406=CARTESIAN_POINT('Ctrl Pts',(43.2293795176151,4.91506667188842,335.223838257278));
#64407=CARTESIAN_POINT('Ctrl Pts',(43.2216308270574,4.91940172842132,335.086599773745));
#64408=CARTESIAN_POINT('Ctrl Pts',(43.2138821364998,4.91798954940518,334.949385234946));
#64409=CARTESIAN_POINT('Ctrl Pts',(43.206135058122,4.91657766420467,334.812199244778));
#64410=CARTESIAN_POINT('Ctrl Pts',(43.1983879797441,4.90942092592708,334.675037580042));
#64411=CARTESIAN_POINT('Ctrl Pts',(43.1906409013663,4.89654196542704,334.538415941229));
#64412=CARTESIAN_POINT('Ctrl Pts',(43.1828937580605,4.8836628969889,334.401793157394));
#64413=CARTESIAN_POINT('Ctrl Pts',(43.1751466147547,4.86506154735705,334.265710797658));
#64414=CARTESIAN_POINT('Ctrl Pts',(43.1673994714489,4.84081245143042,334.13067964905));
#64415=CARTESIAN_POINT('Ctrl Pts',(43.1596505864208,4.81655790379226,333.995618142573));
#64416=CARTESIAN_POINT('Ctrl Pts',(43.1519017013927,4.78665315230708,333.861608702147));
#64417=CARTESIAN_POINT('Ctrl Pts',(43.1441528163646,4.75122381695227,333.729151738513));
#64418=CARTESIAN_POINT('Ctrl Pts',(43.1363957065899,4.71575687653477,333.596554183688));
#64419=CARTESIAN_POINT('Ctrl Pts',(43.1286385968151,4.67475373981558,333.465512775516));
#64420=CARTESIAN_POINT('Ctrl Pts',(43.1208814870404,4.62839004497313,333.336513103721));
#64421=CARTESIAN_POINT('Ctrl Pts',(43.1131202321142,4.58200157485461,333.207444498625));
#64422=CARTESIAN_POINT('Ctrl Pts',(43.1053589771881,4.53024698622739,333.080420165695));
#64423=CARTESIAN_POINT('Ctrl Pts',(43.0975977222619,4.47334964540293,332.955904598001));
#64424=CARTESIAN_POINT('Ctrl Pts',(43.0898240518573,4.41636128737603,332.831189845978));
#64425=CARTESIAN_POINT('Ctrl Pts',(43.0820503814527,4.3542139149992,332.708992227353));
#64426=CARTESIAN_POINT('Ctrl Pts',(43.074276711048,4.2871767500129,332.589751345473));
#64427=CARTESIAN_POINT('Ctrl Pts',(43.0668649068709,4.22326018118429,332.476061155331));
#64428=CARTESIAN_POINT('Ctrl Pts',(43.0594531026937,4.15489896546934,332.365058869625));
#64429=CARTESIAN_POINT('Ctrl Pts',(43.0520412985165,4.08236144624151,332.257098600981));
#64430=CARTESIAN_POINT('Ctrl Pts',(43.0442662197381,4.00626864711869,332.143846877975));
#64431=CARTESIAN_POINT('Ctrl Pts',(43.0364911409596,3.92533933969223,332.033585012205));
#64432=CARTESIAN_POINT('Ctrl Pts',(43.0287160621812,3.8398359819844,331.926753720582));
#64433=CARTESIAN_POINT('Ctrl Pts',(43.0209505511322,3.75443784160177,331.820053891664));
#64434=CARTESIAN_POINT('Ctrl Pts',(43.0131850400832,3.66447709226651,331.716776539489));
#64435=CARTESIAN_POINT('Ctrl Pts',(43.0054195290342,3.57026002930011,331.617334425977));
#64436=CARTESIAN_POINT('Ctrl Pts',(42.9976617175119,3.47613638282589,331.517990909609));
#64437=CARTESIAN_POINT('Ctrl Pts',(42.9899039059897,3.37776508815547,331.422475346331));
#64438=CARTESIAN_POINT('Ctrl Pts',(42.9821460944675,3.2754931257408,331.331168054309));
#64439=CARTESIAN_POINT('Ctrl Pts',(42.9743941209445,3.17329812622122,331.23992947392));
#64440=CARTESIAN_POINT('Ctrl Pts',(42.9666421474215,3.06720859208385,331.152893120581));
#64441=CARTESIAN_POINT('Ctrl Pts',(42.9588901738985,2.95760857247817,331.070402743982));
#64442=CARTESIAN_POINT('Ctrl Pts',(42.9511414833409,2.84805496854586,330.987947302107));
#64443=CARTESIAN_POINT('Ctrl Pts',(42.9433927927833,2.73499414772412,330.910034242402));
#64444=CARTESIAN_POINT('Ctrl Pts',(42.9356441022256,2.61884330360773,330.836967113552));
#64445=CARTESIAN_POINT('Ctrl Pts',(42.9278970238478,2.50271662564458,330.763915186928));
#64446=CARTESIAN_POINT('Ctrl Pts',(42.9201499454699,2.38350153381684,330.695707393705));
#64447=CARTESIAN_POINT('Ctrl Pts',(42.9124028670921,2.26164393852248,330.63260377824));
#64448=CARTESIAN_POINT('Ctrl Pts',(42.9046557237863,2.13978532194394,330.569499633906));
#64449=CARTESIAN_POINT('Ctrl Pts',(42.8969085804805,2.01528450482106,330.511499932397));
#64450=CARTESIAN_POINT('Ctrl Pts',(42.8891614371747,1.88861135397397,330.458818411895));
#64451=CARTESIAN_POINT('Ctrl Pts',(42.8814125521465,1.76190972431323,330.40612504747));
#64452=CARTESIAN_POINT('Ctrl Pts',(42.8736636671184,1.63303514992976,330.358752393309));
#64453=CARTESIAN_POINT('Ctrl Pts',(42.8659147820903,1.50247641706839,330.316865613859));
#64454=CARTESIAN_POINT('Ctrl Pts',(42.8581576723156,1.3717791078192,330.274934375349));
#64455=CARTESIAN_POINT('Ctrl Pts',(42.8504005625409,1.23939444200347,330.238500762664));
#64456=CARTESIAN_POINT('Ctrl Pts',(42.8426434527661,1.1058258102754,330.207679858375));
#64457=CARTESIAN_POINT('Ctrl Pts',(42.83488219784,0.972185803741678,330.17684248438));
#64458=CARTESIAN_POINT('Ctrl Pts',(42.8271209429138,0.837360954652679,330.15162386689));
#64459=CARTESIAN_POINT('Ctrl Pts',(42.8193596879877,0.701862741466809,330.132087536259));
#64460=CARTESIAN_POINT('Ctrl Pts',(42.811586017583,0.566147775298238,330.112519953867));
#64461=CARTESIAN_POINT('Ctrl Pts',(42.8038123471784,0.429757681615977,330.098652862019));
#64462=CARTESIAN_POINT('Ctrl Pts',(42.7960386767737,0.293207823584374,330.090497761006));
#64463=CARTESIAN_POINT('Ctrl Pts',(42.7886268725967,0.163014394297436,330.082722281907));
#64464=CARTESIAN_POINT('Ctrl Pts',(42.7812150684197,0.0326760277303745,
330.080138980519));
#64465=CARTESIAN_POINT('Ctrl Pts',(42.7738032642427,-0.0973642792573438,
330.082713831835));
#64466=CARTESIAN_POINT('Ctrl Pts',(42.7660281854642,-0.233778249062257,
330.085414884285));
#64467=CARTESIAN_POINT('Ctrl Pts',(42.7582531066858,-0.370295296292574,
330.093801043059));
#64468=CARTESIAN_POINT('Ctrl Pts',(42.7504780279073,-0.506402781601683,
330.107890098814));
#64469=CARTESIAN_POINT('Ctrl Pts',(42.7427125168583,-0.642342777984723,
330.121961817088));
#64470=CARTESIAN_POINT('Ctrl Pts',(42.7349470058093,-0.777873830166071,
330.141722429118));
#64471=CARTESIAN_POINT('Ctrl Pts',(42.7271814947603,-0.91248308386811,330.16713773379));
#64472=CARTESIAN_POINT('Ctrl Pts',(42.7194236832382,-1.04695887210274,330.192527839114));
#64473=CARTESIAN_POINT('Ctrl Pts',(42.7116658717159,-1.18051429908788,330.22356140749));
#64474=CARTESIAN_POINT('Ctrl Pts',(42.7039080601938,-1.31264177613079,330.260152467636));
#64475=CARTESIAN_POINT('Ctrl Pts',(42.6961560866708,-1.44466982305722,330.296715991849));
#64476=CARTESIAN_POINT('Ctrl Pts',(42.6884041131478,-1.57527168375651,330.33882857949));
#64477=CARTESIAN_POINT('Ctrl Pts',(42.6806521396248,-1.70395046074921,330.386353298115));
#64478=CARTESIAN_POINT('Ctrl Pts',(42.6729034490672,-1.83257474220416,330.433857889995));
#64479=CARTESIAN_POINT('Ctrl Pts',(42.6651547585096,-1.95927719388752,330.486769919014));
#64480=CARTESIAN_POINT('Ctrl Pts',(42.6574060679519,-2.08357678784231,330.544902825789));
#64481=CARTESIAN_POINT('Ctrl Pts',(42.6496589895741,-2.20785052022823,330.603023637527));
#64482=CARTESIAN_POINT('Ctrl Pts',(42.6419119111963,-2.32972203544762,330.666363000912));
#64483=CARTESIAN_POINT('Ctrl Pts',(42.6341648328185,-2.44873134894977,330.7346866653));
#64484=CARTESIAN_POINT('Ctrl Pts',(42.6264176895126,-2.56774165986492,330.803010902306));
#64485=CARTESIAN_POINT('Ctrl Pts',(42.6186705462068,-2.6838893822343,330.876319329024));
#64486=CARTESIAN_POINT('Ctrl Pts',(42.6109234029009,-2.79674050716217,330.954332490417));
#64487=CARTESIAN_POINT('Ctrl Pts',(42.6031745178728,-2.90961700341836,331.032363190824));
#64488=CARTESIAN_POINT('Ctrl Pts',(42.5954256328448,-3.01919510597351,331.115100508432));
#64489=CARTESIAN_POINT('Ctrl Pts',(42.5876767478167,-3.1250714142378,331.20222279242));
#64490=CARTESIAN_POINT('Ctrl Pts',(42.5799196380419,-3.23106010070959,331.2894375489));
#64491=CARTESIAN_POINT('Ctrl Pts',(42.5721625282672,-3.33333884179704,331.381046320303));
#64492=CARTESIAN_POINT('Ctrl Pts',(42.5644054184925,-3.43153844854347,331.476688072471));
#64493=CARTESIAN_POINT('Ctrl Pts',(42.5566441635664,-3.52979053002,331.572380932533));
#64494=CARTESIAN_POINT('Ctrl Pts',(42.5488829086402,-3.62395886557364,331.672110783526));
#64495=CARTESIAN_POINT('Ctrl Pts',(42.541121653714,-3.71371324083096,331.775481892224));
#64496=CARTESIAN_POINT('Ctrl Pts',(42.5333479833094,-3.80361119383781,331.879018361007));
#64497=CARTESIAN_POINT('Ctrl Pts',(42.5255743129047,-3.88908083296764,331.986207421446));
#64498=CARTESIAN_POINT('Ctrl Pts',(42.5178006425,-3.96983359480141,332.096621917131));
#64499=CARTESIAN_POINT('Ctrl Pts',(42.510388838323,-4.04682729614372,332.201896591476));
#64500=CARTESIAN_POINT('Ctrl Pts',(42.5029770341459,-4.11953321835733,332.31010293196));
#64501=CARTESIAN_POINT('Ctrl Pts',(42.4955652299688,-4.18774024277605,332.420850000187));
#64502=CARTESIAN_POINT('Ctrl Pts',(42.4875585982108,-4.26142115969982,332.540484973317));
#64503=CARTESIAN_POINT('Ctrl Pts',(42.4795519664529,-4.33007336350018,332.663444420362));
#64504=CARTESIAN_POINT('Ctrl Pts',(42.471545334695,-4.39339327032408,332.789280968831));
#64505=CARTESIAN_POINT('Ctrl Pts',(42.4635504411677,-4.45662034614245,332.914933032927));
#64506=CARTESIAN_POINT('Ctrl Pts',(42.4555555476405,-4.51453053311371,333.043453480308));
#64507=CARTESIAN_POINT('Ctrl Pts',(42.4475606541133,-4.56686405814061,333.174367031147));
#64508=CARTESIAN_POINT('Ctrl Pts',(42.4395761882949,-4.61912932475261,333.305109831946));
#64509=CARTESIAN_POINT('Ctrl Pts',(42.4315917224765,-4.66583228396669,333.438239187889));
#64510=CARTESIAN_POINT('Ctrl Pts',(42.4236072566581,-4.70675956403405,333.573256340868));
#64511=CARTESIAN_POINT('Ctrl Pts',(42.4156345323191,-4.7476266588835,333.708074945672));
#64512=CARTESIAN_POINT('Ctrl Pts',(42.40766180798,-4.78273490269389,333.84477547108));
#64513=CARTESIAN_POINT('Ctrl Pts',(42.399689083641,-4.81191961162198,333.982840861129));
#64514=CARTESIAN_POINT('Ctrl Pts',(42.3917232936735,-4.84107893680364,334.12078616717));
#64515=CARTESIAN_POINT('Ctrl Pts',(42.3837575037059,-4.86432491301446,334.260093623737));
#64516=CARTESIAN_POINT('Ctrl Pts',(42.3757917137383,-4.8815429408814,334.400232062518));
#64517=CARTESIAN_POINT('Ctrl Pts',(42.367832966357,-4.89874574622204,334.540246604354));
#64518=CARTESIAN_POINT('Ctrl Pts',(42.3598742189758,-4.9099311821094,334.681090308325));
#64519=CARTESIAN_POINT('Ctrl Pts',(42.3519154715946,-4.91503595708922,334.82222316512));
#64520=CARTESIAN_POINT('Ctrl Pts',(42.3485494398993,-4.91719494437154,334.881913169898));
#64521=CARTESIAN_POINT('Ctrl Pts',(42.345183408204,-4.91826689118854,334.941654801808));
#64522=CARTESIAN_POINT('Ctrl Pts',(42.3418173765087,-4.91824979877537,335.001406892326));
#64523=CARTESIAN_POINT('',(40.5918173765378,-4.91824844260515,335.003913989273));
#64524=CARTESIAN_POINT('Ctrl Pts',(42.3418173764773,-4.91824979877521,335.001406892883));
#64525=CARTESIAN_POINT('Ctrl Pts',(42.3335008810188,-4.91820756832534,335.14903710983));
#64526=CARTESIAN_POINT('Ctrl Pts',(42.3251843855604,-4.91151404239866,335.296481149157));
#64527=CARTESIAN_POINT('Ctrl Pts',(42.3168678901019,-4.89824458647915,335.443151253555));
#64528=CARTESIAN_POINT('Ctrl Pts',(42.3085205834487,-4.88492596949262,335.590364745631));
#64529=CARTESIAN_POINT('Ctrl Pts',(42.3001732767955,-4.86498268740323,335.736798269062));
#64530=CARTESIAN_POINT('Ctrl Pts',(42.2918259701422,-4.83854181084379,335.881870856314));
#64531=CARTESIAN_POINT('Ctrl Pts',(42.2834633353011,-4.81205238081165,336.027209840859));
#64532=CARTESIAN_POINT('Ctrl Pts',(42.2751007004599,-4.77904159042933,336.171182611566));
#64533=CARTESIAN_POINT('Ctrl Pts',(42.2667380656187,-4.73968664218145,336.313222599724));
#64534=CARTESIAN_POINT('Ctrl Pts',(42.258349086423,-4.70020771617673,336.455710048746));
#64535=CARTESIAN_POINT('Ctrl Pts',(42.2499601072272,-4.65434472893535,336.596252249629));
#64536=CARTESIAN_POINT('Ctrl Pts',(42.2415711280315,-4.60232439377681,336.734299062142));
#64537=CARTESIAN_POINT('Ctrl Pts',(42.2334898172526,-4.55221192056292,336.867282964941));
#64538=CARTESIAN_POINT('Ctrl Pts',(42.2254085064738,-4.49638586911976,336.997951091023));
#64539=CARTESIAN_POINT('Ctrl Pts',(42.2173271956949,-4.4350887964449,337.125834055177));
#64540=CARTESIAN_POINT('Ctrl Pts',(42.2095521169165,-4.37611450601408,337.248871041122));
#64541=CARTESIAN_POINT('Ctrl Pts',(42.2017770381381,-4.31192325927031,337.369646517461));
#64542=CARTESIAN_POINT('Ctrl Pts',(42.1940019593596,-4.24271124933489,337.48768653919));
#64543=CARTESIAN_POINT('Ctrl Pts',(42.1862364483106,-4.17358440918395,337.605581305158));
#64544=CARTESIAN_POINT('Ctrl Pts',(42.1784709372616,-4.09944929484068,337.720746980229));
#64545=CARTESIAN_POINT('Ctrl Pts',(42.1707054262125,-4.02054950834209,337.832730963835));
#64546=CARTESIAN_POINT('Ctrl Pts',(42.1629476146903,-3.94172795121146,337.944603914996));
#64547=CARTESIAN_POINT('Ctrl Pts',(42.1551898031681,-3.85815134700235,338.053301135164));
#64548=CARTESIAN_POINT('Ctrl Pts',(42.1474319916459,-3.7701082344178,338.158396264447));
#64549=CARTESIAN_POINT('Ctrl Pts',(42.1396800181229,-3.6821313770676,338.263412306313));
#64550=CARTESIAN_POINT('Ctrl Pts',(42.1319280445999,-3.58969495162526,338.364831354363));
#64551=CARTESIAN_POINT('Ctrl Pts',(42.1241760710769,-3.49312944932227,338.462257892298));
#64552=CARTESIAN_POINT('Ctrl Pts',(42.1164273805192,-3.39660484256669,338.559643170036));
#64553=CARTESIAN_POINT('Ctrl Pts',(42.1086786899616,-3.29595491151265,338.653039023564));
#64554=CARTESIAN_POINT('Ctrl Pts',(42.1009299994039,-3.1915487402333,338.742084940406));
#64555=CARTESIAN_POINT('Ctrl Pts',(42.0931829210261,-3.0871642915299,338.831112330502));
#64556=CARTESIAN_POINT('Ctrl Pts',(42.0854358426483,-2.9790254543068,338.915791330614));
#64557=CARTESIAN_POINT('Ctrl Pts',(42.0776887642704,-2.86753600020716,338.995800339108));
#64558=CARTESIAN_POINT('Ctrl Pts',(42.0699416209646,-2.75604561171866,339.075810018155));
#64559=CARTESIAN_POINT('Ctrl Pts',(42.0621944776588,-2.64120486790648,339.151149399624));
#64560=CARTESIAN_POINT('Ctrl Pts',(42.0544473343529,-2.52344792116647,339.221539251465));
#64561=CARTESIAN_POINT('Ctrl Pts',(42.0466984493248,-2.40566450016495,339.29194492844));
#64562=CARTESIAN_POINT('Ctrl Pts',(42.0389495642967,-2.28496390705461,339.357398661011));
#64563=CARTESIAN_POINT('Ctrl Pts',(42.0312006792686,-2.16180601742788,339.417666556624));
#64564=CARTESIAN_POINT('Ctrl Pts',(42.0234435694939,-2.03851740674447,339.477998421204));
#64565=CARTESIAN_POINT('Ctrl Pts',(42.0156864597192,-1.912766641066,339.53313328139));
#64566=CARTESIAN_POINT('Ctrl Pts',(42.0079293499445,-1.78503526660596,339.58288469847));
#64567=CARTESIAN_POINT('Ctrl Pts',(42.0001680950183,-1.65723563658356,339.632662701117));
#64568=CARTESIAN_POINT('Ctrl Pts',(41.9924068400921,-1.52745365852669,339.677051402064));
#64569=CARTESIAN_POINT('Ctrl Pts',(41.9846455851659,-1.39618631264649,339.715914210721));
#64570=CARTESIAN_POINT('Ctrl Pts',(41.9768719147613,-1.2647089817928,339.754839187207));
#64571=CARTESIAN_POINT('Ctrl Pts',(41.9690982443566,-1.13174191426479,339.788220511985));
#64572=CARTESIAN_POINT('Ctrl Pts',(41.9613245739519,-0.997793433939985,
339.815972521276));
#64573=CARTESIAN_POINT('Ctrl Pts',(41.9539127697749,-0.870080287601892,
339.842432667857));
#64574=CARTESIAN_POINT('Ctrl Pts',(41.9465009655979,-0.741475325697093,
339.863775746802));
#64575=CARTESIAN_POINT('Ctrl Pts',(41.9390891614209,-0.612421823419636,
339.879971574989));
#64576=CARTESIAN_POINT('Ctrl Pts',(41.9313140826425,-0.477043024563564,
339.89696120896));
#64577=CARTESIAN_POINT('Ctrl Pts',(41.923539003864,-0.340742782972515,339.908339960455));
#64578=CARTESIAN_POINT('Ctrl Pts',(41.9157639250856,-0.204025820466614,
339.91401633362));
#64579=CARTESIAN_POINT('Ctrl Pts',(41.9079984140366,-0.0674770968869047,
339.919685721646));
#64580=CARTESIAN_POINT('Ctrl Pts',(41.9002329029876,0.0694869404750382,
339.919666677377));
#64581=CARTESIAN_POINT('Ctrl Pts',(41.8924673919386,0.206353863106128,339.913919122827));
#64582=CARTESIAN_POINT('Ctrl Pts',(41.8847095804164,0.343085081785045,339.908177266993));
#64583=CARTESIAN_POINT('Ctrl Pts',(41.8769517688942,0.479718989340334,339.896718220363));
#64584=CARTESIAN_POINT('Ctrl Pts',(41.869193957372,0.615740905792668,339.879553893486));
#64585=CARTESIAN_POINT('Ctrl Pts',(41.861441983849,0.751660461439184,339.862402483309));
#64586=CARTESIAN_POINT('Ctrl Pts',(41.853690010326,0.886968556433025,339.839554387434));
#64587=CARTESIAN_POINT('Ctrl Pts',(41.845938036803,1.02115374490959,339.811073486422));
#64588=CARTESIAN_POINT('Ctrl Pts',(41.8381893462454,1.15528210587917,339.78260464709));
#64589=CARTESIAN_POINT('Ctrl Pts',(41.8304406556877,1.28828812460929,339.748507828192));
#64590=CARTESIAN_POINT('Ctrl Pts',(41.8226919651301,1.41966890589686,339.708898306412));
#64591=CARTESIAN_POINT('Ctrl Pts',(41.8149448867523,1.55102235231557,339.669297025724));
#64592=CARTESIAN_POINT('Ctrl Pts',(41.8071978083745,1.68075085988325,339.624185436303));
#64593=CARTESIAN_POINT('Ctrl Pts',(41.7994507299967,1.8083654829202,339.57372904124));
#64594=CARTESIAN_POINT('Ctrl Pts',(41.7917035866909,1.9359811754906,339.523272223304));
#64595=CARTESIAN_POINT('Ctrl Pts',(41.7839564433851,2.06148258469986,339.467470654098));
#64596=CARTESIAN_POINT('Ctrl Pts',(41.7762093000793,2.18439995358816,339.406538313151));
#64597=CARTESIAN_POINT('Ctrl Pts',(41.7684604150512,2.3073449569106,339.345592273319));
#64598=CARTESIAN_POINT('Ctrl Pts',(41.7607115300231,2.42770441375425,339.279513339967));
#64599=CARTESIAN_POINT('Ctrl Pts',(41.752962644995,2.54503277380992,339.208561659609));
#64600=CARTESIAN_POINT('Ctrl Pts',(41.7452055352202,2.66248566739918,339.137534670405));
#64601=CARTESIAN_POINT('Ctrl Pts',(41.7374484254455,2.77690070246621,339.061624805255));
#64602=CARTESIAN_POINT('Ctrl Pts',(41.7296913156707,2.88786050643372,338.98113611396));
#64603=CARTESIAN_POINT('Ctrl Pts',(41.7219300607446,2.99887960377259,338.900604412083));
#64604=CARTESIAN_POINT('Ctrl Pts',(41.7141688058185,3.10643948460496,338.815489251063));
#64605=CARTESIAN_POINT('Ctrl Pts',(41.7064075508923,3.21015634248099,338.726134635159));
#64606=CARTESIAN_POINT('Ctrl Pts',(41.6986338804877,3.31403911352837,338.636637080989));
#64607=CARTESIAN_POINT('Ctrl Pts',(41.690860210083,3.41406629158227,338.542886787435));
#64608=CARTESIAN_POINT('Ctrl Pts',(41.6830865396784,3.50989075692392,338.445264857302));
#64609=CARTESIAN_POINT('Ctrl Pts',(41.6756747355012,3.60125457035065,338.352187251502));
#64610=CARTESIAN_POINT('Ctrl Pts',(41.6682629313241,3.68879794500973,338.255590560051));
#64611=CARTESIAN_POINT('Ctrl Pts',(41.6608511271469,3.77225561762683,338.155831208696));
#64612=CARTESIAN_POINT('Ctrl Pts',(41.6530760483685,3.85980379938591,338.051182354365));
#64613=CARTESIAN_POINT('Ctrl Pts',(41.6453009695901,3.94313231590458,337.94272226872));
#64614=CARTESIAN_POINT('Ctrl Pts',(41.6375258908116,4.02189109242853,337.830825869449));
#64615=CARTESIAN_POINT('Ctrl Pts',(41.6297603797626,4.10055295126395,337.719067165822));
#64616=CARTESIAN_POINT('Ctrl Pts',(41.6219948687136,4.17465603614357,337.603880878858));
#64617=CARTESIAN_POINT('Ctrl Pts',(41.6142293576646,4.24388934016124,337.485676232128));
#64618=CARTESIAN_POINT('Ctrl Pts',(41.6064715461424,4.31305399915637,337.367588785649));
#64619=CARTESIAN_POINT('Ctrl Pts',(41.5987137346202,4.37735828980762,337.246489270178));
#64620=CARTESIAN_POINT('Ctrl Pts',(41.590955923098,4.43653370507974,337.122816936571));
#64621=CARTESIAN_POINT('Ctrl Pts',(41.583203949575,4.49566458897523,336.999237670316));
#64622=CARTESIAN_POINT('Ctrl Pts',(41.575451976052,4.54967411188905,336.873089790863));
#64623=CARTESIAN_POINT('Ctrl Pts',(41.567700002529,4.59833921964451,336.744837953387));
#64624=CARTESIAN_POINT('Ctrl Pts',(41.5599513119714,4.64698371769801,336.61664043064));
#64625=CARTESIAN_POINT('Ctrl Pts',(41.5522026214138,4.69028816388154,336.48634108675));
#64626=CARTESIAN_POINT('Ctrl Pts',(41.5444539308562,4.72807735136723,336.35442519985));
#64627=CARTESIAN_POINT('Ctrl Pts',(41.5367068524783,4.76585867649684,336.222536759152));
#64628=CARTESIAN_POINT('Ctrl Pts',(41.5289597741005,4.79812691780422,336.089032819964));
#64629=CARTESIAN_POINT('Ctrl Pts',(41.5212126957227,4.82475665380657,335.954414110357));
#64630=CARTESIAN_POINT('Ctrl Pts',(41.5134655524169,4.85138661299176,335.819794272516));
#64631=CARTESIAN_POINT('Ctrl Pts',(41.505718409111,4.87237789676472,335.684060029066));
#64632=CARTESIAN_POINT('Ctrl Pts',(41.4979712658052,4.88765623263011,335.547722205257));
#64633=CARTESIAN_POINT('Ctrl Pts',(41.4902223807771,4.90293800338975,335.411353729811));
#64634=CARTESIAN_POINT('Ctrl Pts',(41.482473495749,4.91250422692397,335.27438179235));
#64635=CARTESIAN_POINT('Ctrl Pts',(41.4747246107209,4.91633255314925,335.13732184584));
#64636=CARTESIAN_POINT('Ctrl Pts',(41.4669675009462,4.92016494279956,335.000116422487));
#64637=CARTESIAN_POINT('Ctrl Pts',(41.4592103911715,4.91824725833746,334.862823194821));
#64638=CARTESIAN_POINT('Ctrl Pts',(41.4514532813968,4.91060931747564,334.725957679142));
#64639=CARTESIAN_POINT('Ctrl Pts',(41.4436920264706,4.90296729514245,334.589019026906));
#64640=CARTESIAN_POINT('Ctrl Pts',(41.4359307715444,4.88959896369185,334.45250893089));
#64641=CARTESIAN_POINT('Ctrl Pts',(41.4281695166183,4.87058590394933,334.316936302568));
#64642=CARTESIAN_POINT('Ctrl Pts',(41.4203958462136,4.85154242950756,334.181146802222));
#64643=CARTESIAN_POINT('Ctrl Pts',(41.412622175809,4.82683625318615,334.046298150978));
#64644=CARTESIAN_POINT('Ctrl Pts',(41.4048485054043,4.79660000606752,333.912888485806));
#64645=CARTESIAN_POINT('Ctrl Pts',(41.3974367012273,4.76777126352681,333.785689072645));
#64646=CARTESIAN_POINT('Ctrl Pts',(41.3900248970502,4.73391578815166,333.659797968779));
#64647=CARTESIAN_POINT('Ctrl Pts',(41.3826130928731,4.69518975677905,333.535631122177));
#64648=CARTESIAN_POINT('Ctrl Pts',(41.3748380140947,4.65456564724977,333.405378488548));
#64649=CARTESIAN_POINT('Ctrl Pts',(41.3670629353163,4.60845308901366,333.276611785491));
#64650=CARTESIAN_POINT('Ctrl Pts',(41.3592878565378,4.55697791281717,333.149828287808));
#64651=CARTESIAN_POINT('Ctrl Pts',(41.3515223454888,4.50556608010206,333.02320080529));
#64652=CARTESIAN_POINT('Ctrl Pts',(41.3437568344398,4.44880490526497,332.898552031031));
#64653=CARTESIAN_POINT('Ctrl Pts',(41.3359913233908,4.386870209454,332.776364951728));
#64654=CARTESIAN_POINT('Ctrl Pts',(41.3282335118686,4.32499692207421,332.654299021269));
#64655=CARTESIAN_POINT('Ctrl Pts',(41.3204757003464,4.25796049742053,332.534690274878));
#64656=CARTESIAN_POINT('Ctrl Pts',(41.3127178888242,4.18598500634489,332.418002209692));
#64657=CARTESIAN_POINT('Ctrl Pts',(41.3049659153011,4.11406367910875,332.301401955975));
#64658=CARTESIAN_POINT('Ctrl Pts',(41.2972139417781,4.03721088794364,332.187718339978));
#64659=CARTESIAN_POINT('Ctrl Pts',(41.2894619682551,3.95569666388645,332.077390384294));
#64660=CARTESIAN_POINT('Ctrl Pts',(41.2817132776974,3.87421696115165,331.967109152565));
#64661=CARTESIAN_POINT('Ctrl Pts',(41.2739645871398,3.78807998369841,331.860181068356));
#64662=CARTESIAN_POINT('Ctrl Pts',(41.2662158965822,3.69759899779396,331.757016078669));
#64663=CARTESIAN_POINT('Ctrl Pts',(41.2584688182044,3.60713683721434,331.653872553319));
#64664=CARTESIAN_POINT('Ctrl Pts',(41.2507217398265,3.51233272349198,331.554490858842));
#64665=CARTESIAN_POINT('Ctrl Pts',(41.2429746614487,3.41353985678451,331.459247437529));
#64666=CARTESIAN_POINT('Ctrl Pts',(41.2352275181429,3.31474616209768,331.364003217985));
#64667=CARTESIAN_POINT('Ctrl Pts',(41.2274803748371,3.21196392914661,331.272897612071));
#64668=CARTESIAN_POINT('Ctrl Pts',(41.2197332315313,3.10558252867318,331.186269513967));
#64669=CARTESIAN_POINT('Ctrl Pts',(41.2119843465032,2.99917721140252,331.099621940027));
#64670=CARTESIAN_POINT('Ctrl Pts',(41.2042354614751,2.88917141948723,331.017454123762));
#64671=CARTESIAN_POINT('Ctrl Pts',(41.196486576447,2.77598651341125,330.940063801011));
#64672=CARTESIAN_POINT('Ctrl Pts',(41.1887294666722,2.66268147170639,330.862591335372));
#64673=CARTESIAN_POINT('Ctrl Pts',(41.1809723568975,2.54619089844095,330.789906713775));
#64674=CARTESIAN_POINT('Ctrl Pts',(41.1732152471228,2.42696443834278,330.722263837318));
#64675=CARTESIAN_POINT('Ctrl Pts',(41.1654539921966,2.30767426743638,330.65458481467));
#64676=CARTESIAN_POINT('Ctrl Pts',(41.1576927372704,2.18564564415852,330.591953083886));
#64677=CARTESIAN_POINT('Ctrl Pts',(41.1499314823442,2.0613506710906,330.534575443108));
#64678=CARTESIAN_POINT('Ctrl Pts',(41.1421578119396,1.93685686657358,330.477106016804));
#64679=CARTESIAN_POINT('Ctrl Pts',(41.1343841415349,1.81008982922438,330.424907624753));
#64680=CARTESIAN_POINT('Ctrl Pts',(41.1266104711302,1.6815402273399,330.378138305148));
#64681=CARTESIAN_POINT('Ctrl Pts',(41.1191986669532,1.55897464035021,330.333546108623));
#64682=CARTESIAN_POINT('Ctrl Pts',(41.111786862776,1.4347889849869,330.293889000208));
#64683=CARTESIAN_POINT('Ctrl Pts',(41.1043750585989,1.30941755702012,330.259260740784));
#64684=CARTESIAN_POINT('Ctrl Pts',(41.0965999798205,1.17790130190658,330.222935247214));
#64685=CARTESIAN_POINT('Ctrl Pts',(41.0888249010421,1.04466448298867,330.192029229547));
#64686=CARTESIAN_POINT('Ctrl Pts',(41.0810498222637,0.910193363494851,330.166705977954));
#64687=CARTESIAN_POINT('Ctrl Pts',(41.0732843112146,0.775887719274416,330.141413888233));
#64688=CARTESIAN_POINT('Ctrl Pts',(41.0655188001656,0.640351177074994,330.121690967004));
#64689=CARTESIAN_POINT('Ctrl Pts',(41.0577532891166,0.504085037626447,330.107650734326));
#64690=CARTESIAN_POINT('Ctrl Pts',(41.0499954775944,0.367954006451984,330.09362442258));
#64691=CARTESIAN_POINT('Ctrl Pts',(41.0422376660722,0.23109520394211,330.08526962641));
#64692=CARTESIAN_POINT('Ctrl Pts',(41.03447985455,0.0940196523223843,330.082648744753));
#64693=CARTESIAN_POINT('Ctrl Pts',(41.026727881027,-0.0429527455978324,
330.080029835393));
#64694=CARTESIAN_POINT('Ctrl Pts',(41.018975907504,-0.180141178734972,330.083136259286));
#64695=CARTESIAN_POINT('Ctrl Pts',(41.0112239339809,-0.317030334335458,
330.091978521888));
#64696=CARTESIAN_POINT('Ctrl Pts',(41.0034752434233,-0.453861517297275,
330.100817039787));
#64697=CARTESIAN_POINT('Ctrl Pts',(40.9957265528657,-0.590393285558151,
330.115386539881));
#64698=CARTESIAN_POINT('Ctrl Pts',(40.9879778623081,-0.726111379585388,
330.13564543573));
#64699=CARTESIAN_POINT('Ctrl Pts',(40.9802307839303,-0.861801236329623,
330.155900116546));
#64700=CARTESIAN_POINT('Ctrl Pts',(40.9724837055525,-0.99667736922515,330.18184178093));
#64701=CARTESIAN_POINT('Ctrl Pts',(40.9647366271746,-1.13023208304531,330.213377129859));
#64702=CARTESIAN_POINT('Ctrl Pts',(40.9569894838688,-1.26378791618261,330.244912743085));
#64703=CARTESIAN_POINT('Ctrl Pts',(40.949242340563,-1.39602192774177,330.282042044537));
#64704=CARTESIAN_POINT('Ctrl Pts',(40.9414951972572,-1.52643842352645,330.32462099914));
#64705=CARTESIAN_POINT('Ctrl Pts',(40.9337463122291,-1.6568842397082,330.367209526396));
#64706=CARTESIAN_POINT('Ctrl Pts',(40.925997427201,-1.78551135551533,330.415250023519));
#64707=CARTESIAN_POINT('Ctrl Pts',(40.9182485421729,-1.91184137619329,330.468549281436));
#64708=CARTESIAN_POINT('Ctrl Pts',(40.9104914323981,-2.03830548486043,330.521905111736));
#64709=CARTESIAN_POINT('Ctrl Pts',(40.9027343226234,-2.16246726724153,330.580530700623));
#64710=CARTESIAN_POINT('Ctrl Pts',(40.8949772128487,-2.28386988392361,330.644185332707));
#64711=CARTESIAN_POINT('Ctrl Pts',(40.8872159579225,-2.40533737428225,330.70787397979));
#64712=CARTESIAN_POINT('Ctrl Pts',(40.8794547029963,-2.52404242294461,330.776596829136));
#64713=CARTESIAN_POINT('Ctrl Pts',(40.8716934480702,-2.63955564714407,330.850068789952));
#64714=CARTESIAN_POINT('Ctrl Pts',(40.8639197776655,-2.75525365485657,330.923658281961));
#64715=CARTESIAN_POINT('Ctrl Pts',(40.8561461072609,-2.86774931413656,331.002011843043));
#64716=CARTESIAN_POINT('Ctrl Pts',(40.8483724368562,-2.97664419852648,331.084802383292));
#64717=CARTESIAN_POINT('Ctrl Pts',(40.8409606326792,-3.08046999984856,331.163739003973));
#64718=CARTESIAN_POINT('Ctrl Pts',(40.8335488285022,-3.18102249224915,331.246708634064));
#64719=CARTESIAN_POINT('Ctrl Pts',(40.8261370243251,-3.277987807843,331.33339680438));
#64720=CARTESIAN_POINT('Ctrl Pts',(40.8184774883965,-3.37819408702793,331.422982435525));
#64721=CARTESIAN_POINT('Ctrl Pts',(40.8108179524678,-3.47490617038605,331.516841100302));
#64722=CARTESIAN_POINT('Ctrl Pts',(40.8031584165391,-3.56772938716284,331.614665440097));
#64723=CARTESIAN_POINT('Ctrl Pts',(40.7955083882634,-3.66043738404334,331.712368352185));
#64724=CARTESIAN_POINT('Ctrl Pts',(40.7878583599877,-3.74926583893483,331.814026860542));
#64725=CARTESIAN_POINT('Ctrl Pts',(40.780208331712,-3.83385327521381,331.919293566951));
#64726=CARTESIAN_POINT('Ctrl Pts',(40.7723587085798,-3.92064765983382,332.027306759047));
#64727=CARTESIAN_POINT('Ctrl Pts',(40.7645090854475,-4.00297633942959,332.139118761692));
#64728=CARTESIAN_POINT('Ctrl Pts',(40.7566594623152,-4.08048871165239,332.254313394326));
#64729=CARTESIAN_POINT('Ctrl Pts',(40.7490228558809,-4.15589761606571,332.366381968569));
#64730=CARTESIAN_POINT('Ctrl Pts',(40.7413862494465,-4.22674798672772,332.481651599997));
#64731=CARTESIAN_POINT('Ctrl Pts',(40.7337496430121,-4.2927580134138,332.599705913691));
#64732=CARTESIAN_POINT('Ctrl Pts',(40.7261160083527,-4.35874235238795,332.717714286709));
#64733=CARTESIAN_POINT('Ctrl Pts',(40.7184823736934,-4.41988989621217,332.838504835659));
#64734=CARTESIAN_POINT('Ctrl Pts',(40.710848739034,-4.47596320614106,332.961633879851));
#64735=CARTESIAN_POINT('Ctrl Pts',(40.7032163086797,-4.53202766977587,333.084743498835));
#64736=CARTESIAN_POINT('Ctrl Pts',(40.6955838783255,-4.58301932528335,333.210190511906));
#64737=CARTESIAN_POINT('Ctrl Pts',(40.6879514479713,-4.62874783466262,333.337508933676));
#64738=CARTESIAN_POINT('Ctrl Pts',(40.6799402753518,-4.67674551892118,333.471145247026));
#64739=CARTESIAN_POINT('Ctrl Pts',(40.6719291027324,-4.71894414040573,333.606843010139));
#64740=CARTESIAN_POINT('Ctrl Pts',(40.6639179301129,-4.75518202848812,333.744043416975));
#64741=CARTESIAN_POINT('Ctrl Pts',(40.6562793750924,-4.78973441115363,333.874862325298));
#64742=CARTESIAN_POINT('Ctrl Pts',(40.6486408200718,-4.81886799955878,334.007046828186));
#64743=CARTESIAN_POINT('Ctrl Pts',(40.6410022650512,-4.84249495174764,334.14010134039));
#64744=CARTESIAN_POINT('Ctrl Pts',(40.6333603033609,-4.86613244116799,334.273215192716));
#64745=CARTESIAN_POINT('Ctrl Pts',(40.6257183416706,-4.88425835008275,334.407199427809));
#64746=CARTESIAN_POINT('Ctrl Pts',(40.6180763799803,-4.89683667030984,334.541552961828));
#64747=CARTESIAN_POINT('Ctrl Pts',(40.6104262848455,-4.90942837781545,334.676049490153));
#64748=CARTESIAN_POINT('Ctrl Pts',(40.6027761897107,-4.91646069565557,334.810915700099));
#64749=CARTESIAN_POINT('Ctrl Pts',(40.5951260945759,-4.91794969000303,334.945650123284));
#64750=CARTESIAN_POINT('Ctrl Pts',(40.5940231885632,-4.91816435672152,334.965074640604));
#64751=CARTESIAN_POINT('Ctrl Pts',(40.5929202825506,-4.91826389528749,334.984496426894));
#64752=CARTESIAN_POINT('Ctrl Pts',(40.5918173765378,-4.91824844260515,335.003913989272));
#64753=CARTESIAN_POINT('',(38.8418173764735,-4.9182487714237,334.996523667274));
#64754=CARTESIAN_POINT('Ctrl Pts',(40.5918173765087,-4.91824844260474,335.003913989785));
#64755=CARTESIAN_POINT('Ctrl Pts',(40.5790493522362,-4.91806955134227,335.228705499584));
#64756=CARTESIAN_POINT('Ctrl Pts',(40.5662813279637,-4.90247682601608,335.452900204882));
#64757=CARTESIAN_POINT('Ctrl Pts',(40.5535133036912,-4.87172844847187,335.674866643753));
#64758=CARTESIAN_POINT('Ctrl Pts',(40.5516418658112,-4.86722158999028,335.707400761243));
#64759=CARTESIAN_POINT('Ctrl Pts',(40.5497704279312,-4.86238919688565,335.739887074424));
#64760=CARTESIAN_POINT('Ctrl Pts',(40.5478989900512,-4.85723214447028,335.772320501621));
#64761=CARTESIAN_POINT('Ctrl Pts',(40.5401239112727,-4.8358066463429,335.907068469592));
#64762=CARTESIAN_POINT('Ctrl Pts',(40.5323488324943,-4.80873583282199,336.041137119539));
#64763=CARTESIAN_POINT('Ctrl Pts',(40.5245737537158,-4.77607254431648,336.174016232395));
#64764=CARTESIAN_POINT('Ctrl Pts',(40.5168082426668,-4.74344945006692,336.306731829042));
#64765=CARTESIAN_POINT('Ctrl Pts',(40.5090427316178,-4.70524766624566,336.438260425195));
#64766=CARTESIAN_POINT('Ctrl Pts',(40.5012772205688,-4.66157156110468,336.568098735157));
#64767=CARTESIAN_POINT('Ctrl Pts',(40.4935194090466,-4.61793876094902,336.697808310056));
#64768=CARTESIAN_POINT('Ctrl Pts',(40.4857615975244,-4.5688425649342,336.825830565857));
#64769=CARTESIAN_POINT('Ctrl Pts',(40.4780037860021,-4.51443789636349,336.951674548273));
#64770=CARTESIAN_POINT('Ctrl Pts',(40.4702518124791,-4.46007416903115,337.077423829102));
#64771=CARTESIAN_POINT('Ctrl Pts',(40.462499838956,-4.40041007506831,337.200997741995));
#64772=CARTESIAN_POINT('Ctrl Pts',(40.454747865433,-4.33564954574583,337.32192292701));
#64773=CARTESIAN_POINT('Ctrl Pts',(40.4469991748753,-4.27091644254605,337.442796900137));
#64774=CARTESIAN_POINT('Ctrl Pts',(40.4392504843177,-4.20109138092865,337.561024032588));
#64775=CARTESIAN_POINT('Ctrl Pts',(40.4315017937601,-4.12642526682002,337.676153504538));
#64776=CARTESIAN_POINT('Ctrl Pts',(40.4237547153822,-4.05177468762015,337.791259022839));
#64777=CARTESIAN_POINT('Ctrl Pts',(40.4160076370044,-3.97228527191546,337.903267834844));
#64778=CARTESIAN_POINT('Ctrl Pts',(40.4082605586266,-3.8882522718278,338.011756519562));
#64779=CARTESIAN_POINT('Ctrl Pts',(40.4005134153208,-3.80421856746266,338.12024611352));
#64780=CARTESIAN_POINT('Ctrl Pts',(40.392766272015,-3.71564144211904,338.225215212332));
#64781=CARTESIAN_POINT('Ctrl Pts',(40.3850191287092,-3.62285735291542,338.326272337456));
#64782=CARTESIAN_POINT('Ctrl Pts',(40.3772702436811,-3.53005240387855,338.427352182368));
#64783=CARTESIAN_POINT('Ctrl Pts',(40.3695213586529,-3.43303887321729,338.52451801563));
#64784=CARTESIAN_POINT('Ctrl Pts',(40.3617724736248,-3.3321908062351,338.6174144763));
#64785=CARTESIAN_POINT('Ctrl Pts',(40.3540153638501,-3.2312356980728,338.710409538233));
#64786=CARTESIAN_POINT('Ctrl Pts',(40.3462582540754,-3.12643821129529,338.799125910124));
#64787=CARTESIAN_POINT('Ctrl Pts',(40.3385011443006,-3.01820669835919,338.883247531188));
#64788=CARTESIAN_POINT('Ctrl Pts',(40.3307398893745,-2.90991734996322,338.967414104157));
#64789=CARTESIAN_POINT('Ctrl Pts',(40.3229786344483,-2.79819063716515,339.04698080729));
#64790=CARTESIAN_POINT('Ctrl Pts',(40.3152173795221,-2.68346392510102,339.121674953848));
#64791=CARTESIAN_POINT('Ctrl Pts',(40.3074437091174,-2.56855368768694,339.196488586699));
#64792=CARTESIAN_POINT('Ctrl Pts',(40.2996700387128,-2.45063419752518,339.266413887778));
#64793=CARTESIAN_POINT('Ctrl Pts',(40.2918963683082,-2.33016821977328,339.331223745093));
#64794=CARTESIAN_POINT('Ctrl Pts',(40.2844845641312,-2.21530996227013,339.393016687957));
#64795=CARTESIAN_POINT('Ctrl Pts',(40.2770727599542,-2.09813721855394,339.450159591062));
#64796=CARTESIAN_POINT('Ctrl Pts',(40.2696609557773,-1.97906623474684,339.502497073956));
#64797=CARTESIAN_POINT('Ctrl Pts',(40.2618858769988,-1.85415922732714,339.557399772794));
#64798=CARTESIAN_POINT('Ctrl Pts',(40.2541107982204,-1.7267684688382,339.607187587518));
#64799=CARTESIAN_POINT('Ctrl Pts',(40.246335719442,-1.59735160835744,339.65162884394));
#64800=CARTESIAN_POINT('Ctrl Pts',(40.238570208393,-1.46809400356259,339.696015412568));
#64801=CARTESIAN_POINT('Ctrl Pts',(40.230804697344,-1.33681562377427,339.735068388041));
#64802=CARTESIAN_POINT('Ctrl Pts',(40.223039186295,-1.20399617232307,339.76860317908));
#64803=CARTESIAN_POINT('Ctrl Pts',(40.2152813747728,-1.07130841174459,339.802104720276));
#64804=CARTESIAN_POINT('Ctrl Pts',(40.2075235632506,-0.937082996803846,
339.830098870155));
#64805=CARTESIAN_POINT('Ctrl Pts',(40.1997657517284,-0.801816619324115,
339.852450223493));
#64806=CARTESIAN_POINT('Ctrl Pts',(40.1920137782054,-0.666652034083164,
339.874784756728));
#64807=CARTESIAN_POINT('Ctrl Pts',(40.1842618046824,-0.530448429629785,
339.891484882174));
#64808=CARTESIAN_POINT('Ctrl Pts',(40.1765098311594,-0.393714223350742,
339.902465927758));
#64809=CARTESIAN_POINT('Ctrl Pts',(40.1687611406018,-0.257037924089238,
339.913442322864));
#64810=CARTESIAN_POINT('Ctrl Pts',(40.1610124500441,-0.119831858743799,
339.918704424138));
#64811=CARTESIAN_POINT('Ctrl Pts',(40.1532637594865,0.0173890890826273,
339.918219259252));
#64812=CARTESIAN_POINT('Ctrl Pts',(40.1455166811087,0.154581486944766,339.917734195309));
#64813=CARTESIAN_POINT('Ctrl Pts',(40.1377696027309,0.291788370502441,339.911504245051));
#64814=CARTESIAN_POINT('Ctrl Pts',(40.1300225243531,0.428493898146529,339.899548554893));
#64815=CARTESIAN_POINT('Ctrl Pts',(40.1222753810473,0.56520057151461,339.887592764534));
#64816=CARTESIAN_POINT('Ctrl Pts',(40.1145282377414,0.701405491200203,339.869911172615));
#64817=CARTESIAN_POINT('Ctrl Pts',(40.1067810944356,0.836597378294582,339.846574861604));
#64818=CARTESIAN_POINT('Ctrl Pts',(40.0990322094075,0.971819659395384,339.823233304094));
#64819=CARTESIAN_POINT('Ctrl Pts',(40.0912833243795,1.10602806960277,339.794234564221));
#64820=CARTESIAN_POINT('Ctrl Pts',(40.0835344393514,1.23872136094388,339.759700878463));
#64821=CARTESIAN_POINT('Ctrl Pts',(40.0757773295767,1.37155549431541,339.725130538294));
#64822=CARTESIAN_POINT('Ctrl Pts',(40.0680202198019,1.50287091749337,339.685013615282));
#64823=CARTESIAN_POINT('Ctrl Pts',(40.0602631100272,1.63218086527492,339.639522463091));
#64824=CARTESIAN_POINT('Ctrl Pts',(40.052501855101,1.76155991215795,339.594007001884));
#64825=CARTESIAN_POINT('Ctrl Pts',(40.0447406001749,1.88893098547589,339.543111734109));
#64826=CARTESIAN_POINT('Ctrl Pts',(40.0369793452487,2.01382809376192,339.487056883));
#64827=CARTESIAN_POINT('Ctrl Pts',(40.0292056748441,2.13892499671734,339.430912362397));
#64828=CARTESIAN_POINT('Ctrl Pts',(40.0214320044394,2.2615396765308,339.369591940145));
#64829=CARTESIAN_POINT('Ctrl Pts',(40.0136583340347,2.38123072110303,339.303361862007));
#64830=CARTESIAN_POINT('Ctrl Pts',(40.0062465298576,2.49535011875538,339.24021480994));
#64831=CARTESIAN_POINT('Ctrl Pts',(39.9988347256805,2.60681170006456,339.172605053705));
#64832=CARTESIAN_POINT('Ctrl Pts',(39.9914229215033,2.71525954763402,339.100798538271));
#64833=CARTESIAN_POINT('Ctrl Pts',(39.9836478427249,2.8290227472616,339.025472571614));
#64834=CARTESIAN_POINT('Ctrl Pts',(39.9758727639464,2.93982883193801,338.945290008409));
#64835=CARTESIAN_POINT('Ctrl Pts',(39.968097685168,3.04723532172076,338.860510323333));
#64836=CARTESIAN_POINT('Ctrl Pts',(39.960332174119,3.15450964098001,338.775834965056));
#64837=CARTESIAN_POINT('Ctrl Pts',(39.95256666307,3.25839238526958,338.686573980678));
#64838=CARTESIAN_POINT('Ctrl Pts',(39.944801152021,3.35846873284634,338.593030870031));
#64839=CARTESIAN_POINT('Ctrl Pts',(39.9370433404988,3.45844585443319,338.49958050765));
#64840=CARTESIAN_POINT('Ctrl Pts',(39.9292855289766,3.5546238061729,338.401856733456));
#64841=CARTESIAN_POINT('Ctrl Pts',(39.9215277174544,3.64661993447727,338.300203950663));
#64842=CARTESIAN_POINT('Ctrl Pts',(39.9137757439313,3.73854683277773,338.198627664813));
#64843=CARTESIAN_POINT('Ctrl Pts',(39.9060237704083,3.82629791027722,338.093128544183));
#64844=CARTESIAN_POINT('Ctrl Pts',(39.8982717968853,3.90952683060465,337.984088306884));
#64845=CARTESIAN_POINT('Ctrl Pts',(39.8905231063277,3.9927205034348,337.875094248191));
#64846=CARTESIAN_POINT('Ctrl Pts',(39.8827744157701,4.07139559149932,337.762562365618));
#64847=CARTESIAN_POINT('Ctrl Pts',(39.8750257252125,4.14524573460145,337.646907792551));
#64848=CARTESIAN_POINT('Ctrl Pts',(39.8672786468346,4.21908051256449,337.531277282385));
#64849=CARTESIAN_POINT('Ctrl Pts',(39.8595315684567,4.2880921321048,337.412525703261));
#64850=CARTESIAN_POINT('Ctrl Pts',(39.8517844900789,4.35201754235686,337.291097198619));
#64851=CARTESIAN_POINT('Ctrl Pts',(39.8440373467731,4.41594348836542,337.169667676288));
#64852=CARTESIAN_POINT('Ctrl Pts',(39.8362902034673,4.47478295797907,337.045561529563));
#64853=CARTESIAN_POINT('Ctrl Pts',(39.8285430601615,4.52831904360689,336.919247170587));
#64854=CARTESIAN_POINT('Ctrl Pts',(39.8207941751334,4.58186716528338,336.792904413462));
#64855=CARTESIAN_POINT('Ctrl Pts',(39.8130452901053,4.6301093779028,336.664352816015));
#64856=CARTESIAN_POINT('Ctrl Pts',(39.8052964050772,4.67287721868922,336.534080037532));
#64857=CARTESIAN_POINT('Ctrl Pts',(39.7975392953025,4.71569045370373,336.403668986177));
#64858=CARTESIAN_POINT('Ctrl Pts',(39.7897821855277,4.7530175876444,336.271533476384));
#64859=CARTESIAN_POINT('Ctrl Pts',(39.782025075753,4.78474013980417,336.138176109856));
#64860=CARTESIAN_POINT('Ctrl Pts',(39.7742638208268,4.8164796434815,336.004747481415));
#64861=CARTESIAN_POINT('Ctrl Pts',(39.7665025659007,4.84260852332958,335.870096078756));
#64862=CARTESIAN_POINT('Ctrl Pts',(39.7587413109745,4.86305979504189,335.734732939473));
#64863=CARTESIAN_POINT('Ctrl Pts',(39.7509676405698,4.88354378212388,335.599153263282));
#64864=CARTESIAN_POINT('Ctrl Pts',(39.7431939701652,4.8983319697141,335.462859964112));
#64865=CARTESIAN_POINT('Ctrl Pts',(39.7354202997605,4.90740937613979,335.326368315673));
#64866=CARTESIAN_POINT('Ctrl Pts',(39.7280084955835,4.91606422711237,335.196230386308));
#64867=CARTESIAN_POINT('Ctrl Pts',(39.7205966914065,4.91952799801445,335.065912446114));
#64868=CARTESIAN_POINT('Ctrl Pts',(39.7131848872295,4.91783172031658,334.935857711703));
#64869=CARTESIAN_POINT('Ctrl Pts',(39.7054098084511,4.91605230299578,334.799428607344));
#64870=CARTESIAN_POINT('Ctrl Pts',(39.6976347296726,4.90858860544711,334.66285802097));
#64871=CARTESIAN_POINT('Ctrl Pts',(39.6898596508942,4.8954193741753,334.526658460043));
#64872=CARTESIAN_POINT('Ctrl Pts',(39.6820941398451,4.88226634848097,334.390626501346));
#64873=CARTESIAN_POINT('Ctrl Pts',(39.6743286287961,4.86342179614393,334.254965044991));
#64874=CARTESIAN_POINT('Ctrl Pts',(39.6665631177471,4.83891645279941,334.120187164604));
#64875=CARTESIAN_POINT('Ctrl Pts',(39.6588053062249,4.81443540657418,333.985542916879));
#64876=CARTESIAN_POINT('Ctrl Pts',(39.6510474947027,4.7843048083855,333.851780883789));
#64877=CARTESIAN_POINT('Ctrl Pts',(39.6432896831805,4.74860719843016,333.719409223242));
#64878=CARTESIAN_POINT('Ctrl Pts',(39.6355377096575,4.71293645205835,333.587137176567));
#64879=CARTESIAN_POINT('Ctrl Pts',(39.6277857361345,4.67170713398622,333.4562537957));
#64880=CARTESIAN_POINT('Ctrl Pts',(39.6200337626115,4.6250528166342,333.327256891856));
#64881=CARTESIAN_POINT('Ctrl Pts',(39.6122850720539,4.57841825741328,333.198314618277));
#64882=CARTESIAN_POINT('Ctrl Pts',(39.6045363814962,4.52636340112238,333.071257599526));
#64883=CARTESIAN_POINT('Ctrl Pts',(39.5967876909386,4.46907155320163,332.946568112923));
#64884=CARTESIAN_POINT('Ctrl Pts',(39.5890406125608,4.41179162532834,332.82190456901));
#64885=CARTESIAN_POINT('Ctrl Pts',(39.5812935341829,4.3492770362089,332.699607932412));
#64886=CARTESIAN_POINT('Ctrl Pts',(39.5735464558051,4.28175892361804,332.580139759714));
#64887=CARTESIAN_POINT('Ctrl Pts',(39.5657993124993,4.21424024516036,332.460670585757));
#64888=CARTESIAN_POINT('Ctrl Pts',(39.5580521691935,4.14171815190668,332.344030263272));
#64889=CARTESIAN_POINT('Ctrl Pts',(39.5503050258877,4.06446916047856,332.230654679167));
#64890=CARTESIAN_POINT('Ctrl Pts',(39.5425561408596,3.98720280183722,332.117253605824));
#64891=CARTESIAN_POINT('Ctrl Pts',(39.5348072558315,3.90520765040178,332.007119054362));
#64892=CARTESIAN_POINT('Ctrl Pts',(39.5270583708034,3.81880262439616,331.900656589146));
#64893=CARTESIAN_POINT('Ctrl Pts',(39.5193012610287,3.7323058872031,331.794081123569));
#64894=CARTESIAN_POINT('Ctrl Pts',(39.511544151254,3.64139017203667,331.691185834016));
#64895=CARTESIAN_POINT('Ctrl Pts',(39.5037870414792,3.54641401068168,331.592342340061));
#64896=CARTESIAN_POINT('Ctrl Pts',(39.4960257865531,3.45138709710289,331.493446027304));
#64897=CARTESIAN_POINT('Ctrl Pts',(39.4882645316268,3.35229569610611,331.39860609453));
#64898=CARTESIAN_POINT('Ctrl Pts',(39.4805032767007,3.24953330105455,331.308155422037));
#64899=CARTESIAN_POINT('Ctrl Pts',(39.472729606296,3.14660651966109,331.217560057945));
#64900=CARTESIAN_POINT('Ctrl Pts',(39.4649559358914,3.03999731354977,331.13136823082));
#64901=CARTESIAN_POINT('Ctrl Pts',(39.4571822654867,2.93013087993433,331.049871383239));
#64902=CARTESIAN_POINT('Ctrl Pts',(39.4497704613096,2.82537875523543,330.972168233519));
#64903=CARTESIAN_POINT('Ctrl Pts',(39.4423586571325,2.717666064299,330.898732959589));
#64904=CARTESIAN_POINT('Ctrl Pts',(39.4349468529553,2.60738231034018,330.829779316364));
#64905=CARTESIAN_POINT('Ctrl Pts',(39.4271717741769,2.49169322108207,330.757446049682));
#64906=CARTESIAN_POINT('Ctrl Pts',(39.4193966953984,2.37280906638468,330.689816251477));
#64907=CARTESIAN_POINT('Ctrl Pts',(39.41162161662,2.25114932321885,330.62718514146));
#64908=CARTESIAN_POINT('Ctrl Pts',(39.403856105571,2.12963929011222,330.56463110301));
#64909=CARTESIAN_POINT('Ctrl Pts',(39.396090594522,2.00536080868306,330.507063690815));
#64910=CARTESIAN_POINT('Ctrl Pts',(39.388325083473,1.87876196630618,330.454734712202));
#64911=CARTESIAN_POINT('Ctrl Pts',(39.3805672719508,1.75228864705019,330.402457617924));
#64912=CARTESIAN_POINT('Ctrl Pts',(39.3728094604286,1.62349990416403,330.35540876938));
#64913=CARTESIAN_POINT('Ctrl Pts',(39.3650516489064,1.49286772570919,330.31379375016));
#64914=CARTESIAN_POINT('Ctrl Pts',(39.3572996753834,1.36233385211122,330.272210047562));
#64915=CARTESIAN_POINT('Ctrl Pts',(39.3495477018604,1.22995967511856,330.236052153244));
#64916=CARTESIAN_POINT('Ctrl Pts',(39.3417957283374,1.09623609850447,330.205477137521));
#64917=CARTESIAN_POINT('Ctrl Pts',(39.3340470377797,0.962569153904467,330.174915070335));
#64918=CARTESIAN_POINT('Ctrl Pts',(39.3262983472222,0.827554326547805,330.149931266155));
#64919=CARTESIAN_POINT('Ctrl Pts',(39.3185496566645,0.691696370814679,330.130632567458));
#64920=CARTESIAN_POINT('Ctrl Pts',(39.3108025782867,0.555866681463951,330.111337884016));
#64921=CARTESIAN_POINT('Ctrl Pts',(39.3030554999089,0.419194599405768,330.097726008254));
#64922=CARTESIAN_POINT('Ctrl Pts',(39.295308421531,0.282193339330844,330.089852346239));
#64923=CARTESIAN_POINT('Ctrl Pts',(39.2875612782252,0.145190931053404,330.081978618234));
#64924=CARTESIAN_POINT('Ctrl Pts',(39.2798141349194,0.00785972948689445,
330.079843222325));
#64925=CARTESIAN_POINT('Ctrl Pts',(39.2720669916136,-0.129284079756904,
330.083449513203));
#64926=CARTESIAN_POINT('Ctrl Pts',(39.2643181065855,-0.26645872184048,330.087056614852));
#64927=CARTESIAN_POINT('Ctrl Pts',(39.2565692215574,-0.403445497104939,
330.096407961669));
#64928=CARTESIAN_POINT('Ctrl Pts',(39.2488203365293,-0.539730772873343,
330.111454842664));
#64929=CARTESIAN_POINT('Ctrl Pts',(39.2410632267546,-0.676160703241725,
330.126517694574));
#64930=CARTESIAN_POINT('Ctrl Pts',(39.2333061169799,-0.811887257620853,
330.147288113752));
#64931=CARTESIAN_POINT('Ctrl Pts',(39.2255490072052,-0.946403911061024,
330.173665707845));
#64932=CARTESIAN_POINT('Ctrl Pts',(39.217787752279,-1.08099244589969,330.200057397282));
#64933=CARTESIAN_POINT('Ctrl Pts',(39.2100264973528,-1.21436941163332,330.232062140864));
#64934=CARTESIAN_POINT('Ctrl Pts',(39.2022652424267,-1.34604194028045,330.269529182258));
#64935=CARTESIAN_POINT('Ctrl Pts',(39.194491572022,-1.47792510206144,330.307056158708));
#64936=CARTESIAN_POINT('Ctrl Pts',(39.1867179016173,-1.60809800697529,330.350062771191));
#64937=CARTESIAN_POINT('Ctrl Pts',(39.1789442312127,-1.73608547612891,330.398349178602));
#64938=CARTESIAN_POINT('Ctrl Pts',(39.1715324270356,-1.85811509780055,330.44438784213));
#64939=CARTESIAN_POINT('Ctrl Pts',(39.1641206228586,-1.97815790393833,330.495225701449));
#64940=CARTESIAN_POINT('Ctrl Pts',(39.1567088186816,-2.09582336093403,330.550650890044));
#64941=CARTESIAN_POINT('Ctrl Pts',(39.1489337399031,-2.2192559524852,330.608792632236));
#64942=CARTESIAN_POINT('Ctrl Pts',(39.1411586611247,-2.34046233029253,330.672166489798));
#64943=CARTESIAN_POINT('Ctrl Pts',(39.1333835823463,-2.45896723474375,330.74057947592));
#64944=CARTESIAN_POINT('Ctrl Pts',(39.1256180712973,-2.57732631136565,330.808908275507));
#64945=CARTESIAN_POINT('Ctrl Pts',(39.1178525602483,-2.69299019382656,330.882263671949));
#64946=CARTESIAN_POINT('Ctrl Pts',(39.1100870491993,-2.80550464618219,330.960405126408));
#64947=CARTESIAN_POINT('Ctrl Pts',(39.1023292376771,-2.91790754013065,331.038469103387));
#64948=CARTESIAN_POINT('Ctrl Pts',(39.0945714261548,-3.02716689928622,331.121309473258));
#64949=CARTESIAN_POINT('Ctrl Pts',(39.0868136146327,-3.13285442420018,331.208640584267));
#64950=CARTESIAN_POINT('Ctrl Pts',(39.0790616411097,-3.2384624159001,331.295905975845));
#64951=CARTESIAN_POINT('Ctrl Pts',(39.0713096675867,-3.34050362342662,331.387655134002));
#64952=CARTESIAN_POINT('Ctrl Pts',(39.0635576940637,-3.43858030680065,331.483560247042));
#64953=CARTESIAN_POINT('Ctrl Pts',(39.0558090035061,-3.53661545464118,331.57942474421));
#64954=CARTESIAN_POINT('Ctrl Pts',(39.0480603129484,-3.63068913881398,331.679441422937));
#64955=CARTESIAN_POINT('Ctrl Pts',(39.0403116223908,-3.72043836164334,331.783243643091));
#64956=CARTESIAN_POINT('Ctrl Pts',(39.032564544013,-3.81016891139729,331.887024266327));
#64957=CARTESIAN_POINT('Ctrl Pts',(39.0248174656351,-3.89557653396605,331.994588568876));
#64958=CARTESIAN_POINT('Ctrl Pts',(39.0170703872573,-3.97633690728958,332.10553496096));
#64959=CARTESIAN_POINT('Ctrl Pts',(39.0093232439515,-4.05709795746283,332.216482282881));
#64960=CARTESIAN_POINT('Ctrl Pts',(39.0015761006457,-4.13321145066981,332.330811434855));
#64961=CARTESIAN_POINT('Ctrl Pts',(38.9938289573398,-4.20439522822558,332.448090160806));
#64962=CARTESIAN_POINT('Ctrl Pts',(38.9860800723118,-4.27559500940562,332.565395253504));
#64963=CARTESIAN_POINT('Ctrl Pts',(38.9783311872837,-4.34186266676034,332.685650905652));
#64964=CARTESIAN_POINT('Ctrl Pts',(38.9705823022556,-4.40296120628621,332.80839883226));
#64965=CARTESIAN_POINT('Ctrl Pts',(38.9628251924808,-4.46412459643327,332.931277044786));
#64966=CARTESIAN_POINT('Ctrl Pts',(38.9550680827062,-4.520107734392,333.056652465586));
#64967=CARTESIAN_POINT('Ctrl Pts',(38.9473109729314,-4.57072093251787,333.184044818961));
#64968=CARTESIAN_POINT('Ctrl Pts',(38.9395497180053,-4.62136117671847,333.311505246736));
#64969=CARTESIAN_POINT('Ctrl Pts',(38.9317884630791,-4.666625634376,333.440984385878));
#64970=CARTESIAN_POINT('Ctrl Pts',(38.9240272081529,-4.7063743605626,333.571986190284));
#64971=CARTESIAN_POINT('Ctrl Pts',(38.9162535377483,-4.74618667175707,333.703197554884));
#64972=CARTESIAN_POINT('Ctrl Pts',(38.9084798673436,-4.78046552198303,333.835936073477));
#64973=CARTESIAN_POINT('Ctrl Pts',(38.9007061969389,-4.80912181532459,333.969694012504));
#64974=CARTESIAN_POINT('Ctrl Pts',(38.8932943927618,-4.83644415131691,334.097225487291));
#64975=CARTESIAN_POINT('Ctrl Pts',(38.8858825885847,-4.85865556129401,334.225683326727));
#64976=CARTESIAN_POINT('Ctrl Pts',(38.8784707844075,-4.87572286818258,334.354624469645));
#64977=CARTESIAN_POINT('Ctrl Pts',(38.8662529817746,-4.90385704200283,334.567174261542));
#64978=CARTESIAN_POINT('Ctrl Pts',(38.8540351791416,-4.91809686045341,334.781602982594));
#64979=CARTESIAN_POINT('Ctrl Pts',(38.8418173765087,-4.91824877142326,334.996523666654));
#64980=CARTESIAN_POINT('',(37.0918173765509,-4.91824956715858,334.997936593961));
#64981=CARTESIAN_POINT('Ctrl Pts',(38.8418173764734,-4.9182487714237,334.996523667274));
#64982=CARTESIAN_POINT('Ctrl Pts',(38.834160190451,-4.91834397760622,335.131219545687));
#64983=CARTESIAN_POINT('Ctrl Pts',(38.8265030044285,-4.91290165709758,335.266129879067));
#64984=CARTESIAN_POINT('Ctrl Pts',(38.8188458184061,-4.90189549404558,335.40075382463));
#64985=CARTESIAN_POINT('Ctrl Pts',(38.8111966330448,-4.89090083085527,335.535237107481));
#64986=CARTESIAN_POINT('Ctrl Pts',(38.8035474476834,-4.8743539196612,335.669434199112));
#64987=CARTESIAN_POINT('Ctrl Pts',(38.795898262322,-4.85228046796019,335.80284327409));
#64988=CARTESIAN_POINT('Ctrl Pts',(38.7882551171631,-4.8302244466272,335.936147002189));
#64989=CARTESIAN_POINT('Ctrl Pts',(38.7806119720041,-4.80265063162728,336.068663555743));
#64990=CARTESIAN_POINT('Ctrl Pts',(38.7729688268452,-4.76963658908505,336.199895774874));
#64991=CARTESIAN_POINT('Ctrl Pts',(38.7653291508184,-4.73663753122204,336.33106842927));
#64992=CARTESIAN_POINT('Ctrl Pts',(38.7576894747917,-4.69820325282644,336.460957518196));
#64993=CARTESIAN_POINT('Ctrl Pts',(38.7500497987649,-4.6544624227726,336.589076026343));
#64994=CARTESIAN_POINT('Ctrl Pts',(38.7424117446963,-4.61073087921174,336.717167334008));
#64995=CARTESIAN_POINT('Ctrl Pts',(38.7347736906278,-4.56169515389472,336.843488427036));
#64996=CARTESIAN_POINT('Ctrl Pts',(38.7271356365592,-4.50753363509457,336.967567938088));
#64997=CARTESIAN_POINT('Ctrl Pts',(38.7194974409813,-4.45337111285035,337.091649747946));
#64998=CARTESIAN_POINT('Ctrl Pts',(38.7118592454035,-4.39408276977663,337.213489523975));
#64999=CARTESIAN_POINT('Ctrl Pts',(38.7042210498256,-4.32989471712629,337.332636877249));
#65000=CARTESIAN_POINT('Ctrl Pts',(38.6965809493652,-4.26569065667752,337.45181394457));
#65001=CARTESIAN_POINT('Ctrl Pts',(38.6889408489049,-4.19658464836199,337.568296899509));
#65002=CARTESIAN_POINT('Ctrl Pts',(38.6813007484445,-4.12284794474613,337.681661404242));
#65003=CARTESIAN_POINT('Ctrl Pts',(38.6736526768816,-4.0490343098345,337.79514418492));
#65004=CARTESIAN_POINT('Ctrl Pts',(38.6660046053187,-3.97058055467107,337.905501682156));
#65005=CARTESIAN_POINT('Ctrl Pts',(38.6583565337558,-3.88780047989959,338.012339703784));
#65006=CARTESIAN_POINT('Ctrl Pts',(38.650704005967,-3.80497217248358,338.119239975661));
#65007=CARTESIAN_POINT('Ctrl Pts',(38.6430514781781,-3.71781278668029,338.22261638246));
#65008=CARTESIAN_POINT('Ctrl Pts',(38.6353989503893,-3.62667443205167,338.322110116538));
#65009=CARTESIAN_POINT('Ctrl Pts',(38.6277352273408,-3.53540274663827,338.421749404896));
#65010=CARTESIAN_POINT('Ctrl Pts',(38.6200715042925,-3.44014075536484,338.517494396713));
#65011=CARTESIAN_POINT('Ctrl Pts',(38.6124077812441,-3.34127548888804,338.609024961102));
#65012=CARTESIAN_POINT('Ctrl Pts',(38.6083494375406,-3.28892113981219,338.657495200346));
#65013=CARTESIAN_POINT('Ctrl Pts',(38.6042910938371,-3.23555687192711,338.704784305858));
#65014=CARTESIAN_POINT('Ctrl Pts',(38.6002327501337,-3.18124346485195,338.750849647725));
#65015=CARTESIAN_POINT('Ctrl Pts',(38.5924576713552,-3.07718844891677,338.839102809146));
#65016=CARTESIAN_POINT('Ctrl Pts',(38.5846825925768,-2.96929378179727,338.923162149202));
#65017=CARTESIAN_POINT('Ctrl Pts',(38.5769075137984,-2.85793200762272,339.002675068289));
#65018=CARTESIAN_POINT('Ctrl Pts',(38.5691420027494,-2.74670727120093,339.082090141668));
#65019=CARTESIAN_POINT('Ctrl Pts',(38.5613764917004,-2.63202423189635,339.156969700888));
#65020=CARTESIAN_POINT('Ctrl Pts',(38.5536109806514,-2.51429000286758,339.226999981545));
#65021=CARTESIAN_POINT('Ctrl Pts',(38.5458531691292,-2.39667250766975,339.296960826974));
#65022=CARTESIAN_POINT('Ctrl Pts',(38.538095357607,-2.27601017696682,339.362081763644));
#65023=CARTESIAN_POINT('Ctrl Pts',(38.5303375460848,-2.15274043763464,339.422091323195));
#65024=CARTESIAN_POINT('Ctrl Pts',(38.5225855725618,-2.02956346269024,339.482055723649));
#65025=CARTESIAN_POINT('Ctrl Pts',(38.5148335990388,-1.90378333472289,339.536916232802));
#65026=CARTESIAN_POINT('Ctrl Pts',(38.5070816255158,-1.77586319141563,339.586446662491));
#65027=CARTESIAN_POINT('Ctrl Pts',(38.4993329349581,-1.64799722236501,339.635956116014));
#65028=CARTESIAN_POINT('Ctrl Pts',(38.4915842444005,-1.51799340428276,339.680139838825));
#65029=CARTESIAN_POINT('Ctrl Pts',(38.4838355538429,-1.38633582058112,339.718819349697));
#65030=CARTESIAN_POINT('Ctrl Pts',(38.4760884754651,-1.2547056293394,339.757490812973));
#65031=CARTESIAN_POINT('Ctrl Pts',(38.4683413970872,-1.12142273166649,339.790660232078));
#65032=CARTESIAN_POINT('Ctrl Pts',(38.4605943187094,-0.986986996896747,
339.818198805618));
#65033=CARTESIAN_POINT('Ctrl Pts',(38.4528471754036,-0.852550135426429,
339.845737609957));
#65034=CARTESIAN_POINT('Ctrl Pts',(38.4451000320978,-0.71696080051072,339.867645396162));
#65035=CARTESIAN_POINT('Ctrl Pts',(38.437352888792,-0.580729303979137,339.883844442445));
#65036=CARTESIAN_POINT('Ctrl Pts',(38.4296040037639,-0.444467179714485,
339.900047130617));
#65037=CARTESIAN_POINT('Ctrl Pts',(38.4218551187358,-0.307562994614751,
339.910538478809));
#65038=CARTESIAN_POINT('Ctrl Pts',(38.4141062337077,-0.170532038893409,
339.915292655195));
#65039=CARTESIAN_POINT('Ctrl Pts',(38.406349123933,-0.0333556371000553,
339.920051877712));
#65040=CARTESIAN_POINT('Ctrl Pts',(38.3985920141582,0.103947412846171,339.919061750516));
#65041=CARTESIAN_POINT('Ctrl Pts',(38.3908349043835,0.24086140497208,339.912348607957));
#65042=CARTESIAN_POINT('Ctrl Pts',(38.3830736494573,0.377848559558,339.905631878109));
#65043=CARTESIAN_POINT('Ctrl Pts',(38.3753123945312,0.514445852999584,339.893186074617));
#65044=CARTESIAN_POINT('Ctrl Pts',(38.367551139605,0.650143834299697,339.875089338384));
#65045=CARTESIAN_POINT('Ctrl Pts',(38.3597774692003,0.786058888145837,339.85696365327));
#65046=CARTESIAN_POINT('Ctrl Pts',(38.3520037987957,0.921071369944786,339.833169039395));
#65047=CARTESIAN_POINT('Ctrl Pts',(38.344230128391,1.05468225807374,339.803834759544));
#65048=CARTESIAN_POINT('Ctrl Pts',(38.3368183242139,1.18207352721536,339.775865997478));
#65049=CARTESIAN_POINT('Ctrl Pts',(38.3294065200368,1.30819047607783,339.742861778726));
#65050=CARTESIAN_POINT('Ctrl Pts',(38.3219947158597,1.4326161110969,339.704975466538));
#65051=CARTESIAN_POINT('Ctrl Pts',(38.3142196370813,1.56314021713336,339.665232233332));
#65052=CARTESIAN_POINT('Ctrl Pts',(38.3064445583028,1.69221550488667,339.619990638147));
#65053=CARTESIAN_POINT('Ctrl Pts',(38.2986694795244,1.81934386082462,339.569373149413));
#65054=CARTESIAN_POINT('Ctrl Pts',(38.2909039684754,1.94631577722685,339.518817948722));
#65055=CARTESIAN_POINT('Ctrl Pts',(38.2831384574264,2.07134516913963,339.462900160397));
#65056=CARTESIAN_POINT('Ctrl Pts',(38.2753729463774,2.1939478730902,339.401792338657));
#65057=CARTESIAN_POINT('Ctrl Pts',(38.2676151348552,2.3164290161031,339.3407451055));
#65058=CARTESIAN_POINT('Ctrl Pts',(38.2598573233329,2.43648791178982,339.274518252865));
#65059=CARTESIAN_POINT('Ctrl Pts',(38.2520995118107,2.5536595598327,339.203332715236));
#65060=CARTESIAN_POINT('Ctrl Pts',(38.2443475382877,2.67074303249455,339.132200746982));
#65061=CARTESIAN_POINT('Ctrl Pts',(38.2365955647647,2.7849432495444,339.056117723371));
#65062=CARTESIAN_POINT('Ctrl Pts',(38.2288435912417,2.89581937415523,338.975350703368));
#65063=CARTESIAN_POINT('Ctrl Pts',(38.2210949006841,3.00664854266145,338.894617888245));
#65064=CARTESIAN_POINT('Ctrl Pts',(38.2133462101265,3.11415610337385,338.809205251785));
#65065=CARTESIAN_POINT('Ctrl Pts',(38.2055975195689,3.21793000230823,338.719423283621));
#65066=CARTESIAN_POINT('Ctrl Pts',(38.1978504411911,3.32168231021606,338.629659995346));
#65067=CARTESIAN_POINT('Ctrl Pts',(38.1901033628132,3.42170220608201,338.535529439166));
#65068=CARTESIAN_POINT('Ctrl Pts',(38.1823562844353,3.51761087008556,338.437382264043));
#65069=CARTESIAN_POINT('Ctrl Pts',(38.1746091411295,3.61352033789635,338.339234266352));
#65070=CARTESIAN_POINT('Ctrl Pts',(38.1668619978237,3.70531823193607,338.237069862133));
#65071=CARTESIAN_POINT('Ctrl Pts',(38.1591148545179,3.79266303528185,338.131276123772));
#65072=CARTESIAN_POINT('Ctrl Pts',(38.1513659694898,3.88002747559357,338.025458600733));
#65073=CARTESIAN_POINT('Ctrl Pts',(38.1436170844617,3.96293658422882,337.91601042126));
#65074=CARTESIAN_POINT('Ctrl Pts',(38.1358681994336,4.04108978555278,337.803350924804));
#65075=CARTESIAN_POINT('Ctrl Pts',(38.1281110896589,4.11932593949221,337.690571850394));
#65076=CARTESIAN_POINT('Ctrl Pts',(38.1203539798842,4.19279587918222,337.574574971823));
#65077=CARTESIAN_POINT('Ctrl Pts',(38.1125968701095,4.26124267164846,337.455808208273));
#65078=CARTESIAN_POINT('Ctrl Pts',(38.1048356151833,4.32972603989205,337.336977979563));
#65079=CARTESIAN_POINT('Ctrl Pts',(38.0970743602571,4.39318073164775,337.215375262923));
#65080=CARTESIAN_POINT('Ctrl Pts',(38.0893131053309,4.45139676410234,337.091470753092));
#65081=CARTESIAN_POINT('Ctrl Pts',(38.0815394349263,4.5097059232363,336.967368036426));
#65082=CARTESIAN_POINT('Ctrl Pts',(38.0737657645216,4.56275952570881,336.840956529214));
#65083=CARTESIAN_POINT('Ctrl Pts',(38.0659920941169,4.61039622212024,336.712725820895));
#65084=CARTESIAN_POINT('Ctrl Pts',(38.0585802899399,4.65581541885267,336.590464282899));
#65085=CARTESIAN_POINT('Ctrl Pts',(38.0511684857629,4.69631058480863,336.466549373467));
#65086=CARTESIAN_POINT('Ctrl Pts',(38.0437566815859,4.7317850272708,336.341414745034));
#65087=CARTESIAN_POINT('Ctrl Pts',(38.0359816028074,4.76899817783125,336.210146895705));
#65088=CARTESIAN_POINT('Ctrl Pts',(38.028206524029,4.800803599795,336.077121909416));
#65089=CARTESIAN_POINT('Ctrl Pts',(38.0204314452506,4.82703472166327,335.942824935159));
#65090=CARTESIAN_POINT('Ctrl Pts',(38.0126659342016,4.85323356446613,335.808693221878));
#65091=CARTESIAN_POINT('Ctrl Pts',(38.0049004231525,4.87387168145963,335.673293015009));
#65092=CARTESIAN_POINT('Ctrl Pts',(37.9971349121035,4.88883216852958,335.537124836933));
#65093=CARTESIAN_POINT('Ctrl Pts',(37.9893771005813,4.90377782223305,335.401091670002));
#65094=CARTESIAN_POINT('Ctrl Pts',(37.9816192890591,4.91305700639798,335.264292433218));
#65095=CARTESIAN_POINT('Ctrl Pts',(37.9738614775369,4.91660387119302,335.127237715595));
#65096=CARTESIAN_POINT('Ctrl Pts',(37.9661095040138,4.92014806685982,334.990286135993));
#65097=CARTESIAN_POINT('Ctrl Pts',(37.9583575304908,4.91796851939799,334.853079847402));
#65098=CARTESIAN_POINT('Ctrl Pts',(37.9506055569678,4.91005124228594,334.716134079844));
#65099=CARTESIAN_POINT('Ctrl Pts',(37.9428568664102,4.90213731814548,334.579246308899));
#65100=CARTESIAN_POINT('Ctrl Pts',(37.9351081758526,4.88849051983128,334.442619228958));
#65101=CARTESIAN_POINT('Ctrl Pts',(37.9273594852949,4.86914895864659,334.306767368764));
#65102=CARTESIAN_POINT('Ctrl Pts',(37.9196124069171,4.84981142163528,334.170943773683));
#65103=CARTESIAN_POINT('Ctrl Pts',(37.9118653285393,4.82478153354952,334.03589546426));
#65104=CARTESIAN_POINT('Ctrl Pts',(37.9041182501614,4.7941491614406,333.902130754435));
#65105=CARTESIAN_POINT('Ctrl Pts',(37.8963711068556,4.7635165326029,333.768364923532));
#65106=CARTESIAN_POINT('Ctrl Pts',(37.8886239635498,4.72728141334067,333.635883094698));
#65107=CARTESIAN_POINT('Ctrl Pts',(37.880876820244,4.68558448667703,333.505181923874));
#65108=CARTESIAN_POINT('Ctrl Pts',(37.8731279352159,4.64387818565897,333.374451368653));
#65109=CARTESIAN_POINT('Ctrl Pts',(37.8653790501878,4.59670775257178,333.245502640365));
#65110=CARTESIAN_POINT('Ctrl Pts',(37.8576301651597,4.54426316018289,333.118815428113));
#65111=CARTESIAN_POINT('Ctrl Pts',(37.849873055385,4.49176290256177,332.991993748745));
#65112=CARTESIAN_POINT('Ctrl Pts',(37.8421159456103,4.43397745275645,332.867438742153));
#65113=CARTESIAN_POINT('Ctrl Pts',(37.8343588358355,4.37114443438962,332.745608863528));
#65114=CARTESIAN_POINT('Ctrl Pts',(37.8265975809094,4.30827784006682,332.623713882911));
#65115=CARTESIAN_POINT('Ctrl Pts',(37.8188363259832,4.24035849610238,332.504547271331));
#65116=CARTESIAN_POINT('Ctrl Pts',(37.811075071057,4.16766858599533,332.388540327746));
#65117=CARTESIAN_POINT('Ctrl Pts',(37.8033014006524,4.0948623957217,332.272347810859));
#65118=CARTESIAN_POINT('Ctrl Pts',(37.7955277302477,4.01727061094869,332.159325384647));
#65119=CARTESIAN_POINT('Ctrl Pts',(37.787754059843,3.93521762246236,332.049873676203));
#65120=CARTESIAN_POINT('Ctrl Pts',(37.7803422556659,3.85698422033066,331.945516971118));
#65121=CARTESIAN_POINT('Ctrl Pts',(37.7729304514888,3.77469578729007,331.844406254409));
#65122=CARTESIAN_POINT('Ctrl Pts',(37.7655186473117,3.68866466494969,331.746857511259));
#65123=CARTESIAN_POINT('Ctrl Pts',(37.7577435685333,3.59841690103013,331.644527613625));
#65124=CARTESIAN_POINT('Ctrl Pts',(37.7499684897548,3.50376509091556,331.545794302704));
#65125=CARTESIAN_POINT('Ctrl Pts',(37.7421934109764,3.40502706534648,331.451060193979));
#65126=CARTESIAN_POINT('Ctrl Pts',(37.7344278999274,3.30641054320355,331.356442661606));
#65127=CARTESIAN_POINT('Ctrl Pts',(37.7266623888783,3.20371808993043,331.265814807532));
#65128=CARTESIAN_POINT('Ctrl Pts',(37.7188968778293,3.09730734195156,331.179545800302));
#65129=CARTESIAN_POINT('Ctrl Pts',(37.7111390663071,2.99100210053962,331.093362329043));
#65130=CARTESIAN_POINT('Ctrl Pts',(37.7033812547849,2.88098620283537,331.011529348554));
#65131=CARTESIAN_POINT('Ctrl Pts',(37.6956234432627,2.76765337891204,330.934378542375));
#65132=CARTESIAN_POINT('Ctrl Pts',(37.6878714697397,2.65440584153209,330.857285794625));
#65133=CARTESIAN_POINT('Ctrl Pts',(37.6801194962166,2.5378466680937,330.784868426932));
#65134=CARTESIAN_POINT('Ctrl Pts',(37.6723675226936,2.41840155760518,330.717417021391));
#65135=CARTESIAN_POINT('Ctrl Pts',(37.664618832136,2.2990070321922,330.64999418156));
#65136=CARTESIAN_POINT('Ctrl Pts',(37.6568701415783,2.17672934023772,330.587533312788));
#65137=CARTESIAN_POINT('Ctrl Pts',(37.6491214510207,2.05202178415196,330.530280807493));
#65138=CARTESIAN_POINT('Ctrl Pts',(37.6413743726429,1.92734017451499,330.47304021406));
#65139=CARTESIAN_POINT('Ctrl Pts',(37.6336272942651,1.80023006133307,330.421005991641));
#65140=CARTESIAN_POINT('Ctrl Pts',(37.6258802158872,1.67116752886275,330.374377646957));
#65141=CARTESIAN_POINT('Ctrl Pts',(37.6181330725814,1.54210391472391,330.327748911482));
#65142=CARTESIAN_POINT('Ctrl Pts',(37.6103859292756,1.41108821627704,330.286526276924));
#65143=CARTESIAN_POINT('Ctrl Pts',(37.6026387859698,1.27861421375738,330.250860208956));
#65144=CARTESIAN_POINT('Ctrl Pts',(37.5948899009417,1.14611042826981,330.215186122499));
#65145=CARTESIAN_POINT('Ctrl Pts',(37.5871410159136,1.01214806366985,330.185071190066));
#65146=CARTESIAN_POINT('Ctrl Pts',(37.5793921308855,0.877233305922503,330.160615246803));
#65147=CARTESIAN_POINT('Ctrl Pts',(37.5716350211108,0.742175348257355,330.136133345748));
#65148=CARTESIAN_POINT('Ctrl Pts',(37.5638779113361,0.606163363331336,330.117322502256));
#65149=CARTESIAN_POINT('Ctrl Pts',(37.5561208015613,0.46971146767299,330.104230989963));
#65150=CARTESIAN_POINT('Ctrl Pts',(37.5483595466352,0.333186656484583,330.091132481985));
#65151=CARTESIAN_POINT('Ctrl Pts',(37.5405982917091,0.196221856268451,330.083759416016));
#65152=CARTESIAN_POINT('Ctrl Pts',(37.5328370367829,0.0593324612038433,
330.082107898546));
#65153=CARTESIAN_POINT('Ctrl Pts',(37.5250633663782,-0.0777759122809043,
330.080453739186));
#65154=CARTESIAN_POINT('Ctrl Pts',(37.5172896959735,-0.214808248666145,
330.084539406301));
#65155=CARTESIAN_POINT('Ctrl Pts',(37.5095160255689,-0.351252105616479,
330.094308915066));
#65156=CARTESIAN_POINT('Ctrl Pts',(37.5021042213919,-0.481344468197614,
330.103623650848));
#65157=CARTESIAN_POINT('Ctrl Pts',(37.4946924172149,-0.610901619807047,
330.118104939194));
#65158=CARTESIAN_POINT('Ctrl Pts',(37.4872806130379,-0.739488815793786,
330.1376611231));
#65159=CARTESIAN_POINT('Ctrl Pts',(37.4795055342595,-0.874378453298963,
330.158175813833));
#65160=CARTESIAN_POINT('Ctrl Pts',(37.471730455481,-1.0086269264079,330.184340280411));
#65161=CARTESIAN_POINT('Ctrl Pts',(37.4639553767026,-1.14172367072025,330.216105130522));
#65162=CARTESIAN_POINT('Ctrl Pts',(37.4561898656536,-1.274656631015,330.247830891963));
#65163=CARTESIAN_POINT('Ctrl Pts',(37.4484243546047,-1.40644030592325,330.285143234703));
#65164=CARTESIAN_POINT('Ctrl Pts',(37.4406588435557,-1.53657071614992,330.327941192925));
#65165=CARTESIAN_POINT('Ctrl Pts',(37.4329010320335,-1.66657210169624,330.370696716846));
#65166=CARTESIAN_POINT('Ctrl Pts',(37.4251432205113,-1.79492311577844,330.418926910994));
#65167=CARTESIAN_POINT('Ctrl Pts',(37.4173854089891,-1.92113176869542,330.472480172345));
#65168=CARTESIAN_POINT('Ctrl Pts',(37.409633435466,-2.04724544559947,330.525993133169));
#65169=CARTESIAN_POINT('Ctrl Pts',(37.401881461943,-2.17121961196057,330.584821035828));
#65170=CARTESIAN_POINT('Ctrl Pts',(37.3941294884199,-2.29257954093718,330.648763151588));
#65171=CARTESIAN_POINT('Ctrl Pts',(37.3863807978623,-2.41388807391132,330.712678187824));
#65172=CARTESIAN_POINT('Ctrl Pts',(37.3786321073047,-2.53258422641506,330.781702947572));
#65173=CARTESIAN_POINT('Ctrl Pts',(37.370883416747,-2.64821549386231,330.85558957624));
#65174=CARTESIAN_POINT('Ctrl Pts',(37.3631363383692,-2.7638227032586,330.929460832178));
#65175=CARTESIAN_POINT('Ctrl Pts',(37.3553892599913,-2.87636596681179,331.008191734654));
#65176=CARTESIAN_POINT('Ctrl Pts',(37.3476421816135,-2.98541987855531,331.091489898794));
#65177=CARTESIAN_POINT('Ctrl Pts',(37.3398950383077,-3.09447470427565,331.174788761053));
#65178=CARTESIAN_POINT('Ctrl Pts',(37.332147895002,-3.20003980923074,331.262654724061));
#65179=CARTESIAN_POINT('Ctrl Pts',(37.3244007516961,-3.30172145080692,331.354753983092));
#65180=CARTESIAN_POINT('Ctrl Pts',(37.3166518666681,-3.40342595257434,331.446873947992));
#65181=CARTESIAN_POINT('Ctrl Pts',(37.30890298164,-3.50124496397462,331.543228840412));
#65182=CARTESIAN_POINT('Ctrl Pts',(37.3011540966119,-3.59482060523396,331.643447024299));
#65183=CARTESIAN_POINT('Ctrl Pts',(37.2933969868372,-3.68849556864625,331.743771580803));
#65184=CARTESIAN_POINT('Ctrl Pts',(37.2856398770624,-3.77791789766018,331.847967333836));
#65185=CARTESIAN_POINT('Ctrl Pts',(37.2778827672877,-3.86276877999129,331.955628075477));
#65186=CARTESIAN_POINT('Ctrl Pts',(37.2701215123615,-3.94766500392096,332.063346347575));
#65187=CARTESIAN_POINT('Ctrl Pts',(37.2623602574353,-4.02798468482792,332.174532981031));
#65188=CARTESIAN_POINT('Ctrl Pts',(37.2545990025092,-4.10345218748378,332.288752462881));
#65189=CARTESIAN_POINT('Ctrl Pts',(37.2468253321045,-4.17904041354899,332.403154658678));
#65190=CARTESIAN_POINT('Ctrl Pts',(37.2390516616998,-4.2497607490397,332.520599062712));
#65191=CARTESIAN_POINT('Ctrl Pts',(37.2312779912952,-4.31538296083877,332.640624454691));
#65192=CARTESIAN_POINT('Ctrl Pts',(37.2238661871181,-4.37795044289079,332.755062635796));
#65193=CARTESIAN_POINT('Ctrl Pts',(37.216454382941,-4.43588362729956,332.871846664628));
#65194=CARTESIAN_POINT('Ctrl Pts',(37.2090425787639,-4.48902432512157,332.990561354267));
#65195=CARTESIAN_POINT('Ctrl Pts',(37.2005133259487,-4.55017683747444,333.127174191925));
#65196=CARTESIAN_POINT('Ctrl Pts',(37.1919840731336,-4.60515010793779,333.266716439433));
#65197=CARTESIAN_POINT('Ctrl Pts',(37.1834548203184,-4.65368063737661,333.408635934864));
#65198=CARTESIAN_POINT('Ctrl Pts',(37.174957512741,-4.70202940185503,333.550023888773));
#65199=CARTESIAN_POINT('Ctrl Pts',(37.1664602051637,-4.74398346463822,333.693771082907));
#65200=CARTESIAN_POINT('Ctrl Pts',(37.1579628975863,-4.7793279453148,333.839307338856));
#65201=CARTESIAN_POINT('Ctrl Pts',(37.1494858615255,-4.81458810678542,333.984496397695));
#65202=CARTESIAN_POINT('Ctrl Pts',(37.1410088254647,-4.84327005782944,334.131465754266));
#65203=CARTESIAN_POINT('Ctrl Pts',(37.1325317894039,-4.86520793403035,334.279628692168));
#65204=CARTESIAN_POINT('Ctrl Pts',(37.1240869843794,-4.88706239894484,334.427228291069));
#65205=CARTESIAN_POINT('Ctrl Pts',(37.1156421793548,-4.9022238761433,334.576012161315));
#65206=CARTESIAN_POINT('Ctrl Pts',(37.1071973743303,-4.91057723754466,334.72538343712));
#65207=CARTESIAN_POINT('Ctrl Pts',(37.1020707084038,-4.91564838994467,334.816063639663));
#65208=CARTESIAN_POINT('Ctrl Pts',(37.0969440424774,-4.91821139877864,334.906960017087));
#65209=CARTESIAN_POINT('Ctrl Pts',(37.0918173765509,-4.91824956715858,334.997936593961));
#65210=CARTESIAN_POINT('',(35.34181657491,-4.91667364108997,335.004349070568));
#65211=CARTESIAN_POINT('Ctrl Pts',(37.0918173765087,-4.91824956715889,334.99793659471));
#65212=CARTESIAN_POINT('Ctrl Pts',(37.0839206660765,-4.91830835868908,335.138069713192));
#65213=CARTESIAN_POINT('Ctrl Pts',(37.0760239556444,-4.91237368761718,335.278174596858));
#65214=CARTESIAN_POINT('Ctrl Pts',(37.0681272452122,-4.90047919903303,335.417716030749));
#65215=CARTESIAN_POINT('Ctrl Pts',(37.0602271166153,-4.88857956180854,335.557317866451));
#65216=CARTESIAN_POINT('Ctrl Pts',(37.0523269880183,-4.87071499803595,335.696355398293));
#65217=CARTESIAN_POINT('Ctrl Pts',(37.0444268594214,-4.84697094239054,335.83429955419));
#65218=CARTESIAN_POINT('Ctrl Pts',(37.0365218817839,-4.82321231281928,335.97232837919));
#65219=CARTESIAN_POINT('Ctrl Pts',(37.0286169041465,-4.7935670632542,336.109262127297));
#65220=CARTESIAN_POINT('Ctrl Pts',(37.020711926509,-4.75817151016775,336.244583039547));
#65221=CARTESIAN_POINT('Ctrl Pts',(37.0127949002831,-4.72272200797866,336.380110204876));
#65222=CARTESIAN_POINT('Ctrl Pts',(37.0048778740573,-4.68150478494827,336.514019265025));
#65223=CARTESIAN_POINT('Ctrl Pts',(36.9969608478314,-4.63470602834046,336.645807732806));
#65224=CARTESIAN_POINT('Ctrl Pts',(36.9890374299877,-4.5878694898993,336.777702596789));
#65225=CARTESIAN_POINT('Ctrl Pts',(36.9811140121441,-4.53544257188891,336.907473113106));
#65226=CARTESIAN_POINT('Ctrl Pts',(36.9731905943004,-4.47765897625038,337.03463833516));
#65227=CARTESIAN_POINT('Ctrl Pts',(36.9652525752252,-4.41976889731394,337.162037896599));
#65228=CARTESIAN_POINT('Ctrl Pts',(36.95731455615,-4.35650257943818,337.286822239184));
#65229=CARTESIAN_POINT('Ctrl Pts',(36.9493765370747,-4.288139472326,337.408535432245));
#65230=CARTESIAN_POINT('Ctrl Pts',(36.9431858728799,-4.23482478065828,337.503456532734));
#65231=CARTESIAN_POINT('Ctrl Pts',(36.9369952086849,-4.17841111909408,337.596510255459));
#65232=CARTESIAN_POINT('Ctrl Pts',(36.9308045444901,-4.11904846917579,337.687493771357));
#65233=CARTESIAN_POINT('Ctrl Pts',(36.9230294657116,-4.04449277287554,337.801763255434));
#65234=CARTESIAN_POINT('Ctrl Pts',(36.9152543869332,-3.96506061343784,337.913108501809));
#65235=CARTESIAN_POINT('Ctrl Pts',(36.9074793081548,-3.88100847035088,338.021085287701));
#65236=CARTESIAN_POINT('Ctrl Pts',(36.8997137971058,-3.7970597587769,338.128929201284));
#65237=CARTESIAN_POINT('Ctrl Pts',(36.8919482860568,-3.70850261324296,338.233412596463));
#65238=CARTESIAN_POINT('Ctrl Pts',(36.8841827750078,-3.61563772423811,338.334118610603));
#65239=CARTESIAN_POINT('Ctrl Pts',(36.8764249634856,-3.52286491104113,338.434724774436));
#65240=CARTESIAN_POINT('Ctrl Pts',(36.8686671519634,-3.42579311745344,338.531560725059));
#65241=CARTESIAN_POINT('Ctrl Pts',(36.8609093404412,-3.32476415373212,338.624241490927));
#65242=CARTESIAN_POINT('Ctrl Pts',(36.8531573669182,-3.2238112175098,338.71685251158));
#65243=CARTESIAN_POINT('Ctrl Pts',(36.8454053933952,-3.11890732538444,338.805314308266));
#65244=CARTESIAN_POINT('Ctrl Pts',(36.8376534198722,-3.01043184700796,338.88927797374));
#65245=CARTESIAN_POINT('Ctrl Pts',(36.8299047293146,-2.90200230806113,338.973206080552));
#65246=CARTESIAN_POINT('Ctrl Pts',(36.822156038757,-2.79000449971037,339.052639606232));
#65247=CARTESIAN_POINT('Ctrl Pts',(36.8144073481994,-2.67485147618795,339.127269393053));
#65248=CARTESIAN_POINT('Ctrl Pts',(36.8066602698216,-2.55972241121386,339.201883652524));
#65249=CARTESIAN_POINT('Ctrl Pts',(36.7989131914438,-2.44143976463688,339.27169594868));
#65250=CARTESIAN_POINT('Ctrl Pts',(36.7911661130659,-2.32044589266319,339.336440236152));
#65251=CARTESIAN_POINT('Ctrl Pts',(36.7834189697601,-2.19945100664414,339.401185066245));
#65252=CARTESIAN_POINT('Ctrl Pts',(36.7756718264544,-2.07574519454169,339.46086161852));
#65253=CARTESIAN_POINT('Ctrl Pts',(36.7679246831486,-1.94979539244553,339.515249825879));
#65254=CARTESIAN_POINT('Ctrl Pts',(36.7601757981205,-1.82381727416021,339.569650260861));
#65255=CARTESIAN_POINT('Ctrl Pts',(36.7524269130924,-1.69559452076537,339.618759830157));
#65256=CARTESIAN_POINT('Ctrl Pts',(36.7446780280643,-1.56561364233383,339.662406780348));
#65257=CARTESIAN_POINT('Ctrl Pts',(36.7369209182896,-1.43549480085479,339.706100057864));
#65258=CARTESIAN_POINT('Ctrl Pts',(36.7291638085149,-1.30361447777166,339.744319009443));
#65259=CARTESIAN_POINT('Ctrl Pts',(36.7214066987401,-1.17047446289557,339.776941761651));
#65260=CARTESIAN_POINT('Ctrl Pts',(36.713645443814,-1.03726330225261,339.809581946415));
#65261=CARTESIAN_POINT('Ctrl Pts',(36.7058841888879,-0.902791491537083,
339.836619896095));
#65262=CARTESIAN_POINT('Ctrl Pts',(36.6981229339617,-0.767569604154022,
339.85798517549));
#65263=CARTESIAN_POINT('Ctrl Pts',(36.6903492635571,-0.632131405819857,
339.879384632369));
#65264=CARTESIAN_POINT('Ctrl Pts',(36.6825755931524,-0.495941121610227,
339.895093240766));
#65265=CARTESIAN_POINT('Ctrl Pts',(36.6748019227477,-0.359513912265738,
339.90509253831));
#65266=CARTESIAN_POINT('Ctrl Pts',(36.6673901185705,-0.229437422335778,
339.914626366148));
#65267=CARTESIAN_POINT('Ctrl Pts',(36.6599783143933,-0.0991458562419824,
339.918970448477));
#65268=CARTESIAN_POINT('Ctrl Pts',(36.652566510216,0.0309173698767789,339.918152821816));
#65269=CARTESIAN_POINT('Ctrl Pts',(36.6447914314376,0.167355382142981,339.917295120837));
#65270=CARTESIAN_POINT('Ctrl Pts',(36.6370163526592,0.30397327455472,339.910754225158));
#65271=CARTESIAN_POINT('Ctrl Pts',(36.6292412738808,0.440258694930354,339.898505419415));
#65272=CARTESIAN_POINT('Ctrl Pts',(36.6214757628317,0.57637640742023,339.886271686607));
#65273=CARTESIAN_POINT('Ctrl Pts',(36.6137102517827,0.712162076337915,339.868344054031));
#65274=CARTESIAN_POINT('Ctrl Pts',(36.6059447407337,0.847102432123598,339.844749790442));
#65275=CARTESIAN_POINT('Ctrl Pts',(36.5981869292115,0.981908994153377,339.821178920635));
#65276=CARTESIAN_POINT('Ctrl Pts',(36.5904291176893,1.11587152842548,339.791952667799));
#65277=CARTESIAN_POINT('Ctrl Pts',(36.5826713061672,1.24848133101156,339.757150137279));
#65278=CARTESIAN_POINT('Ctrl Pts',(36.5749193326442,1.38099134051589,339.722373796768));
#65279=CARTESIAN_POINT('Ctrl Pts',(36.5671673591212,1.51215026801197,339.682029629977));
#65280=CARTESIAN_POINT('Ctrl Pts',(36.5594153855982,1.64145941126676,339.636247843209));
#65281=CARTESIAN_POINT('Ctrl Pts',(36.5516666950406,1.77071379202244,339.590485445056));
#65282=CARTESIAN_POINT('Ctrl Pts',(36.5439180044829,1.8981195789383,339.539290137286));
#65283=CARTESIAN_POINT('Ctrl Pts',(36.5361693139253,2.02319326733982,339.482841963029));
#65284=CARTESIAN_POINT('Ctrl Pts',(36.5284222355475,2.14824093311601,339.426405533286));
#65285=CARTESIAN_POINT('Ctrl Pts',(36.5206751571697,2.27095710945309,339.364718571608));
#65286=CARTESIAN_POINT('Ctrl Pts',(36.5129280787919,2.39087868879991,339.298009092352));
#65287=CARTESIAN_POINT('Ctrl Pts',(36.5051809354861,2.5108012732049,339.231299054007));
#65288=CARTESIAN_POINT('Ctrl Pts',(36.4974337921803,2.62792887232276,339.159566604138));
#65289=CARTESIAN_POINT('Ctrl Pts',(36.4896866488745,2.74182374112443,339.083085308331));
#65290=CARTESIAN_POINT('Ctrl Pts',(36.4819377638464,2.85574421591082,339.006586817904));
#65291=CARTESIAN_POINT('Ctrl Pts',(36.4741888788183,2.96643018972047,338.925337574914));
#65292=CARTESIAN_POINT('Ctrl Pts',(36.4664399937902,3.07347395292423,338.839653750431));
#65293=CARTESIAN_POINT('Ctrl Pts',(36.4586828840155,3.18063133348421,338.75387898025));
#65294=CARTESIAN_POINT('Ctrl Pts',(36.4509257742408,3.28413847534477,338.663660470729));
#65295=CARTESIAN_POINT('Ctrl Pts',(36.4431686644661,3.38362134527426,338.569354234915));
#65296=CARTESIAN_POINT('Ctrl Pts',(36.4354074095399,3.48315737566853,338.474997604864));
#65297=CARTESIAN_POINT('Ctrl Pts',(36.4276461546138,3.57866457715264,338.376549176411));
#65298=CARTESIAN_POINT('Ctrl Pts',(36.4198848996876,3.6698074186975,338.274400185098));
#65299=CARTESIAN_POINT('Ctrl Pts',(36.412111229283,3.76109605908532,338.17208778869));
#65300=CARTESIAN_POINT('Ctrl Pts',(36.4043375588784,3.84800614039774,338.066063302569));
#65301=CARTESIAN_POINT('Ctrl Pts',(36.3965638884737,3.9302433541959,337.956749945345));
#65302=CARTESIAN_POINT('Ctrl Pts',(36.3891520842966,4.00865240590784,337.852525151198));
#65303=CARTESIAN_POINT('Ctrl Pts',(36.3817402801194,4.08281367995659,337.745311025833));
#65304=CARTESIAN_POINT('Ctrl Pts',(36.3743284759422,4.15251079493285,337.635495619512));
#65305=CARTESIAN_POINT('Ctrl Pts',(36.3665533971637,4.22562397313061,337.520297833004));
#65306=CARTESIAN_POINT('Ctrl Pts',(36.3587783183852,4.2940553751274,337.401873278691));
#65307=CARTESIAN_POINT('Ctrl Pts',(36.3510032396068,4.35750695408287,337.28063942955));
#65308=CARTESIAN_POINT('Ctrl Pts',(36.3432377285577,4.42088045183075,337.15955476638));
#65309=CARTESIAN_POINT('Ctrl Pts',(36.3354722175087,4.47928613995949,337.035668029852));
#65310=CARTESIAN_POINT('Ctrl Pts',(36.3277067064597,4.53246918973772,336.909425595979));
#65311=CARTESIAN_POINT('Ctrl Pts',(36.3199488949374,4.58559950836736,336.783308331846));
#65312=CARTESIAN_POINT('Ctrl Pts',(36.3121910834152,4.63351734290625,336.654840376399));
#65313=CARTESIAN_POINT('Ctrl Pts',(36.3044332718929,4.67601392584138,336.524492318064));
#65314=CARTESIAN_POINT('Ctrl Pts',(36.2966812983699,4.71847852875002,336.394242350778));
#65315=CARTESIAN_POINT('Ctrl Pts',(36.2889293248469,4.75552987975614,336.262115466895));
#65316=CARTESIAN_POINT('Ctrl Pts',(36.2811773513239,4.78700759572399,336.128601497864));
#65317=CARTESIAN_POINT('Ctrl Pts',(36.2734286607663,4.81847198086049,335.995144072078));
#65318=CARTESIAN_POINT('Ctrl Pts',(36.2656799702086,4.84436733619497,335.860301109156));
#65319=CARTESIAN_POINT('Ctrl Pts',(36.257931279651,4.86458341171398,335.724576630162));
#65320=CARTESIAN_POINT('Ctrl Pts',(36.2501842012731,4.88479528110962,335.58888038978));
#65321=CARTESIAN_POINT('Ctrl Pts',(36.2424371228952,4.89933016346967,335.452303384502));
#65322=CARTESIAN_POINT('Ctrl Pts',(36.2346900445174,4.90812918686222,335.315358443));
#65323=CARTESIAN_POINT('Ctrl Pts',(36.2269429012115,4.91692828399907,335.178412353767));
#65324=CARTESIAN_POINT('Ctrl Pts',(36.2191957579057,4.91999140122227,335.041098712229));
#65325=CARTESIAN_POINT('Ctrl Pts',(36.2114486145999,4.91731169671548,334.903933669555));
#65326=CARTESIAN_POINT('Ctrl Pts',(36.2036997295718,4.91463138975423,334.766737789268));
#65327=CARTESIAN_POINT('Ctrl Pts',(36.1959508445437,4.90620569953516,334.629690965047));
#65328=CARTESIAN_POINT('Ctrl Pts',(36.1882019595155,4.89207986598166,334.493307146925));
#65329=CARTESIAN_POINT('Ctrl Pts',(36.1804448497408,4.87793903912246,334.35677856961));
#65330=CARTESIAN_POINT('Ctrl Pts',(36.172687739966,4.85808602343729,334.220914793552));
#65331=CARTESIAN_POINT('Ctrl Pts',(36.1649306301912,4.83261778704999,334.086223010364));
#65332=CARTESIAN_POINT('Ctrl Pts',(36.157169375265,4.80713594125147,333.951459252194));
#65333=CARTESIAN_POINT('Ctrl Pts',(36.1494081203388,4.77603298438545,333.817869115303));
#65334=CARTESIAN_POINT('Ctrl Pts',(36.1416468654126,4.73945633967175,333.685946474893));
#65335=CARTESIAN_POINT('Ctrl Pts',(36.1338731950079,4.7028211842468,333.553812801252));
#65336=CARTESIAN_POINT('Ctrl Pts',(36.1260995246033,4.6606949638316,333.423352326607));
#65337=CARTESIAN_POINT('Ctrl Pts',(36.1183258541986,4.61327430479938,333.295041569076));
#65338=CARTESIAN_POINT('Ctrl Pts',(36.1109140500217,4.56806108885559,333.172703708183));
#65339=CARTESIAN_POINT('Ctrl Pts',(36.1035022458449,4.51803536428646,333.0523201955));
#65340=CARTESIAN_POINT('Ctrl Pts',(36.0960904416681,4.46340635443777,332.934282987032));
#65341=CARTESIAN_POINT('Ctrl Pts',(36.0883153628896,4.40609981408298,332.810460423358));
#65342=CARTESIAN_POINT('Ctrl Pts',(36.0805402841112,4.34354623809749,332.688828675961));
#65343=CARTESIAN_POINT('Ctrl Pts',(36.0727652053328,4.27593539816851,332.569864297372));
#65344=CARTESIAN_POINT('Ctrl Pts',(36.0649996942838,4.20840775768237,332.451046312023));
#65345=CARTESIAN_POINT('Ctrl Pts',(36.0572341832348,4.13583542709292,332.334889501091));
#65346=CARTESIAN_POINT('Ctrl Pts',(36.0494686721858,4.05845587106273,332.221849715164));
#65347=CARTESIAN_POINT('Ctrl Pts',(36.0417108606636,3.98115303708789,332.108922008514));
#65348=CARTESIAN_POINT('Ctrl Pts',(36.0339530491414,3.89905268240325,331.999105496987));
#65349=CARTESIAN_POINT('Ctrl Pts',(36.0261952376192,3.81243755877643,331.892830400038));
#65350=CARTESIAN_POINT('Ctrl Pts',(36.0184432640962,3.72588761577616,331.786635278468));
#65351=CARTESIAN_POINT('Ctrl Pts',(36.0106912905731,3.63482991235051,331.683976568643));
#65352=CARTESIAN_POINT('Ctrl Pts',(36.00293931705,3.53958956569751,331.585254216065));
#65353=CARTESIAN_POINT('Ctrl Pts',(35.9951906264924,3.44438955338826,331.486573672462));
#65354=CARTESIAN_POINT('Ctrl Pts',(35.9874419359348,3.34501069176538,331.391826451183));
#65355=CARTESIAN_POINT('Ctrl Pts',(35.9796932453771,3.24181716028654,331.301378018536));
#65356=CARTESIAN_POINT('Ctrl Pts',(35.9719461669993,3.13864509908395,331.21094840444));
#65357=CARTESIAN_POINT('Ctrl Pts',(35.9641990886215,3.03166024045969,331.124816057433));
#65358=CARTESIAN_POINT('Ctrl Pts',(35.9564520102437,2.92126197400406,331.043308005197));
#65359=CARTESIAN_POINT('Ctrl Pts',(35.9487048669378,2.81086278230462,330.961799269845));
#65360=CARTESIAN_POINT('Ctrl Pts',(35.9409577236321,2.6970504401689,330.884915138733));
#65361=CARTESIAN_POINT('Ctrl Pts',(35.9332105803263,2.58025528762715,330.812940684302));
#65362=CARTESIAN_POINT('Ctrl Pts',(35.9254616952982,2.46343387705549,330.740950048486));
#65363=CARTESIAN_POINT('Ctrl Pts',(35.9177128102701,2.34362865435892,330.673871490815));
#65364=CARTESIAN_POINT('Ctrl Pts',(35.909963925242,2.22129629300343,330.611945095924));
#65365=CARTESIAN_POINT('Ctrl Pts',(35.9022068154673,2.09883408681583,330.549952971717));
#65366=CARTESIAN_POINT('Ctrl Pts',(35.8944497056925,1.97383973304959,330.493124111066));
#65367=CARTESIAN_POINT('Ctrl Pts',(35.8866925959178,1.84679221496803,330.441651441889));
#65368=CARTESIAN_POINT('Ctrl Pts',(35.8789313409916,1.71967680675508,330.390151267364));
#65369=CARTESIAN_POINT('Ctrl Pts',(35.8711700860655,1.59050641597652,330.344013118873));
#65370=CARTESIAN_POINT('Ctrl Pts',(35.8634088311393,1.45977613198823,330.303380289296));
#65371=CARTESIAN_POINT('Ctrl Pts',(35.8556351607347,1.32883672215045,330.262682460433));
#65372=CARTESIAN_POINT('Ctrl Pts',(35.84786149033,1.19633281070121,330.227507649253));
#65373=CARTESIAN_POINT('Ctrl Pts',(35.8400878199253,1.06277151770532,330.197948379739));
#65374=CARTESIAN_POINT('Ctrl Pts',(35.8326760157483,0.935427535032283,330.169765101332));
#65375=CARTESIAN_POINT('Ctrl Pts',(35.8252642115713,0.807122680904278,330.146686374056));
#65376=CARTESIAN_POINT('Ctrl Pts',(35.8178524073943,0.67829978224585,330.128748367421));
#65377=CARTESIAN_POINT('Ctrl Pts',(35.8100773286159,0.5431628895795,330.109931165645));
#65378=CARTESIAN_POINT('Ctrl Pts',(35.8023022498374,0.407028829004848,330.096711884469));
#65379=CARTESIAN_POINT('Ctrl Pts',(35.794527171059,0.270401040060297,330.08918883075));
#65380=CARTESIAN_POINT('Ctrl Pts',(35.78676166001,0.133941380308749,330.081675034627));
#65381=CARTESIAN_POINT('Ctrl Pts',(35.7789961489611,-0.00301041238201688,
330.07984354021));
#65382=CARTESIAN_POINT('Ctrl Pts',(35.7712306379121,-0.139942497771345,
330.08374134531));
#65383=CARTESIAN_POINT('Ctrl Pts',(35.7634728263899,-0.276738814600179,
330.087635285724));
#65384=CARTESIAN_POINT('Ctrl Pts',(35.7557150148676,-0.413515074813833,
330.097247209855));
#65385=CARTESIAN_POINT('Ctrl Pts',(35.7479572033454,-0.549756484487828,
330.112572162143));
#65386=CARTESIAN_POINT('Ctrl Pts',(35.7402052298225,-0.685895368179283,
330.127885581917));
#65387=CARTESIAN_POINT('Ctrl Pts',(35.7324532562995,-0.821499815610984,
330.148903428916));
#65388=CARTESIAN_POINT('Ctrl Pts',(35.7247012827766,-0.956057564505091,
330.175568738613));
#65389=CARTESIAN_POINT('Ctrl Pts',(35.716952592219,-1.09055832811339,330.202222755534));
#65390=CARTESIAN_POINT('Ctrl Pts',(35.7092039016614,-1.22401289221155,330.234519402399));
#65391=CARTESIAN_POINT('Ctrl Pts',(35.7014552111038,-1.35591684998379,330.272350207722));
#65392=CARTESIAN_POINT('Ctrl Pts',(35.6937081327259,-1.4877933640363,330.310173142029));
#65393=CARTESIAN_POINT('Ctrl Pts',(35.6859610543481,-1.61811953797953,330.353527836829));
#65394=CARTESIAN_POINT('Ctrl Pts',(35.6782139759703,-1.74640423463299,330.402255410339));
#65395=CARTESIAN_POINT('Ctrl Pts',(35.6704668326645,-1.87469000643559,330.450983392233));
#65396=CARTESIAN_POINT('Ctrl Pts',(35.6627196893587,-2.00093390141979,330.505084203859));
#65397=CARTESIAN_POINT('Ctrl Pts',(35.6549725460529,-2.1246633144027,330.564350232161));
#65398=CARTESIAN_POINT('Ctrl Pts',(35.6472236610248,-2.248420544384,330.623629584724));
#65399=CARTESIAN_POINT('Ctrl Pts',(35.6394747759968,-2.3696618150113,330.688076295898));
#65400=CARTESIAN_POINT('Ctrl Pts',(35.6317258909687,-2.48793810177526,330.757436262796));
#65401=CARTESIAN_POINT('Ctrl Pts',(35.623968781194,-2.60633992821235,330.82686984908));
#65402=CARTESIAN_POINT('Ctrl Pts',(35.6162116714193,-2.72177014652231,330.901226910462));
#65403=CARTESIAN_POINT('Ctrl Pts',(35.6084545616446,-2.83380731417333,330.980209064063));
#65404=CARTESIAN_POINT('Ctrl Pts',(35.6006933067184,-2.94590435090457,331.059233423203));
#65405=CARTESIAN_POINT('Ctrl Pts',(35.5929320517923,-3.05460441453063,331.142887560983));
#65406=CARTESIAN_POINT('Ctrl Pts',(35.5851707968661,-3.15951908575393,331.230832690201));
#65407=CARTESIAN_POINT('Ctrl Pts',(35.5773971264615,-3.26460158625944,331.318918502965));
#65408=CARTESIAN_POINT('Ctrl Pts',(35.5696234560568,-3.36588630496086,331.411308760289));
#65409=CARTESIAN_POINT('Ctrl Pts',(35.5618497856522,-3.4630210047002,331.50762708413));
#65410=CARTESIAN_POINT('Ctrl Pts',(35.5544379814749,-3.55563406079991,331.599461766825));
#65411=CARTESIAN_POINT('Ctrl Pts',(35.5470261772976,-3.64447457363195,331.694866832342));
#65412=CARTESIAN_POINT('Ctrl Pts',(35.5396143731203,-3.72927248842552,331.79348947147));
#65413=CARTESIAN_POINT('Ctrl Pts',(35.5318949702201,-3.81758961793084,331.896205067876));
#65414=CARTESIAN_POINT('Ctrl Pts',(35.5241755673199,-3.90181143064435,332.002748566461));
#65415=CARTESIAN_POINT('Ctrl Pts',(35.5164561644196,-3.98158401450764,332.112757059422));
#65416=CARTESIAN_POINT('Ctrl Pts',(35.5087491506717,-4.06122856843044,332.222588995725));
#65417=CARTESIAN_POINT('Ctrl Pts',(35.5010421369238,-4.13643788138174,332.335874534719));
#65418=CARTESIAN_POINT('Ctrl Pts',(35.4933351231759,-4.20689668647199,332.452215995841));
#65419=CARTESIAN_POINT('Ctrl Pts',(35.485635267547,-4.27729005084497,332.56844940136));
#65420=CARTESIAN_POINT('Ctrl Pts',(35.477935411918,-4.3429414775011,332.687732747526));
#65421=CARTESIAN_POINT('Ctrl Pts',(35.470235556289,-4.40357747833596,332.809637369112));
#65422=CARTESIAN_POINT('Ctrl Pts',(35.4625411241838,-4.46417076917623,332.931456125111));
#65423=CARTESIAN_POINT('Ctrl Pts',(35.4548466920786,-4.51975548521717,333.055892129898));
#65424=CARTESIAN_POINT('Ctrl Pts',(35.4471522599734,-4.57010304589883,333.182490381768));
#65425=CARTESIAN_POINT('Ctrl Pts',(35.4394615211818,-4.62042643984248,333.309027866706));
#65426=CARTESIAN_POINT('Ctrl Pts',(35.4317707823901,-4.66551753426074,333.437725165319));
#65427=CARTESIAN_POINT('Ctrl Pts',(35.4240800435984,-4.70519525290871,333.568105906673));
#65428=CARTESIAN_POINT('Ctrl Pts',(35.4163898424677,-4.74487019768002,333.698477533085));
#65429=CARTESIAN_POINT('Ctrl Pts',(35.408699641337,-4.77913239507231,333.830531991193));
#65430=CARTESIAN_POINT('Ctrl Pts',(35.4010094402063,-4.80785023672204,333.963776489481));
#65431=CARTESIAN_POINT('Ctrl Pts',(35.3933196499584,-4.83656654399476,334.097013868596));
#65432=CARTESIAN_POINT('Ctrl Pts',(35.3856298597104,-4.85973900678302,334.231440772012));
#65433=CARTESIAN_POINT('Ctrl Pts',(35.3779400694625,-4.87728703847865,334.366553706469));
#65434=CARTESIAN_POINT('Ctrl Pts',(35.3702464555423,-4.89484379575984,334.501733824499));
#65435=CARTESIAN_POINT('Ctrl Pts',(35.3625528416222,-4.90677048988907,334.637600260297));
#65436=CARTESIAN_POINT('Ctrl Pts',(35.354859227702,-4.91303836375677,334.773643867425));
#65437=CARTESIAN_POINT('Ctrl Pts',(35.3505119439709,-4.9165800317396,334.850515434691));
#65438=CARTESIAN_POINT('Ctrl Pts',(35.3461646602398,-4.91831588271506,334.927443513891));
#65439=CARTESIAN_POINT('Ctrl Pts',(35.3418173765088,-4.91824808840549,335.004336288243));
#65440=CARTESIAN_POINT('',(33.5918173765087,-4.92635458438153,334.999985596072));
#65441=CARTESIAN_POINT('Ctrl Pts',(35.3418159898256,-4.91552445706615,335.004358400345));
#65442=CARTESIAN_POINT('Ctrl Pts',(35.3150027728325,-4.91951882428191,335.478359568893));
#65443=CARTESIAN_POINT('Ctrl Pts',(35.1954435444147,-4.63874791474335,337.587276797197));
#65444=CARTESIAN_POINT('Ctrl Pts',(34.9831383045724,-1.62400073114428,340.584538520919));
#65445=CARTESIAN_POINT('Ctrl Pts',(34.7049002702985,3.81731760238167,339.387771095783));
#65446=CARTESIAN_POINT('Ctrl Pts',(34.4266622360246,5.75553991572094,334.164410899434));
#65447=CARTESIAN_POINT('Ctrl Pts',(34.1484242017505,2.41198820003029,329.707858487404));
#65448=CARTESIAN_POINT('Ctrl Pts',(33.9629321789013,-1.29267692394935,329.974503648868));
#65449=CARTESIAN_POINT('Ctrl Pts',(33.7773965704874,-4.03594356099226,331.738054986346));
#65450=CARTESIAN_POINT('Ctrl Pts',(33.684606973498,-4.92642524185015,333.368987177956));
#65451=CARTESIAN_POINT('Ctrl Pts',(33.5918173765087,-4.92635458438153,334.999985596072));
#65452=CARTESIAN_POINT('',(31.8418181870771,-4.91665217595445,334.995658470632));
#65453=CARTESIAN_POINT('Ctrl Pts',(33.5918173765087,-4.92635458438153,334.999985596072));
#65454=CARTESIAN_POINT('Ctrl Pts',(33.4991149506488,-4.92628399329202,336.629451773736));
#65455=CARTESIAN_POINT('Ctrl Pts',(33.3136665133641,-3.14873109843668,339.889282125032));
#65456=CARTESIAN_POINT('Ctrl Pts',(33.0354720646549,2.40701815814295,340.294403880779));
#65457=CARTESIAN_POINT('Ctrl Pts',(32.7572340303809,5.75475281454385,335.840992812056));
#65458=CARTESIAN_POINT('Ctrl Pts',(32.478995996107,3.82143575305017,330.615815052746));
#65459=CARTESIAN_POINT('Ctrl Pts',(32.200757961833,-1.61875649471839,329.413939109063));
#65460=CARTESIAN_POINT('Ctrl Pts',(31.9883655570254,-4.63755548700006,332.409598265075));
#65461=CARTESIAN_POINT('Ctrl Pts',(31.8687191636425,-4.91947903470235,334.520096393768));
#65462=CARTESIAN_POINT('Ctrl Pts',(31.8418187816841,-4.91548146079034,334.995648989438));
#65463=CARTESIAN_POINT('',(30.0918173764651,-4.91824955753923,335.002086208329));
#65464=CARTESIAN_POINT('Ctrl Pts',(31.8418173765087,-4.91824809517395,334.995671395399));
#65465=CARTESIAN_POINT('Ctrl Pts',(31.8341227429724,-4.91836788126847,335.131774778698));
#65466=CARTESIAN_POINT('Ctrl Pts',(31.8264281094361,-4.91283380696339,335.267987972518));
#65467=CARTESIAN_POINT('Ctrl Pts',(31.8187334758998,-4.90164537475895,335.403801538635));
#65468=CARTESIAN_POINT('Ctrl Pts',(31.8110415252819,-4.89046084366948,335.539567750098));
#65469=CARTESIAN_POINT('Ctrl Pts',(31.8033495746639,-4.87362590555103,335.674934215789));
#65470=CARTESIAN_POINT('Ctrl Pts',(31.7956576240459,-4.85119212798663,335.809393600086));
#65471=CARTESIAN_POINT('Ctrl Pts',(31.787966822558,-4.82876170189046,335.943832896979));
#65472=CARTESIAN_POINT('Ctrl Pts',(31.7802760210701,-4.80073416488714,336.077364990455));
#65473=CARTESIAN_POINT('Ctrl Pts',(31.7725852195822,-4.76721263948652,336.209490269667));
#65474=CARTESIAN_POINT('Ctrl Pts',(31.7648938427455,-4.73368860634084,336.341625433171));
#65475=CARTESIAN_POINT('Ctrl Pts',(31.7572024659088,-4.69466986486908,336.472353188198));
#65476=CARTESIAN_POINT('Ctrl Pts',(31.7495110890721,-4.65030996766537,336.60118714307));
#65477=CARTESIAN_POINT('Ctrl Pts',(31.7418174123076,-4.60593680566352,336.730059622747));
#65478=CARTESIAN_POINT('Ctrl Pts',(31.7341237355431,-4.55621944013669,336.857036800591));
#65479=CARTESIAN_POINT('Ctrl Pts',(31.7264300587786,-4.50136012885213,336.981650840305));
#65480=CARTESIAN_POINT('Ctrl Pts',(31.7187278898555,-4.44644026472813,337.106402427023));
#65481=CARTESIAN_POINT('Ctrl Pts',(31.7110257209323,-4.38636728307101,337.228785304049));
#65482=CARTESIAN_POINT('Ctrl Pts',(31.7033235520092,-4.3213902894302,337.348354536461));
#65483=CARTESIAN_POINT('Ctrl Pts',(31.6956166515253,-4.25637337942362,337.46799722209));
#65484=CARTESIAN_POINT('Ctrl Pts',(31.6879097510415,-4.1864466617007,337.584822481246));
#65485=CARTESIAN_POINT('Ctrl Pts',(31.6802028505576,-4.11190277012035,337.698414103057));
#65486=CARTESIAN_POINT('Ctrl Pts',(31.672484341483,-4.03724659610824,337.812176823308));
#65487=CARTESIAN_POINT('Ctrl Pts',(31.6647658324084,-3.95795959260941,337.922695859222));
#65488=CARTESIAN_POINT('Ctrl Pts',(31.6570473233338,-3.87437518747252,338.029587425574));
#65489=CARTESIAN_POINT('Ctrl Pts',(31.6527921799842,-3.82829587057259,338.088515766953));
#65490=CARTESIAN_POINT('Ctrl Pts',(31.6485370366347,-3.78091115388401,338.146342273655));
#65491=CARTESIAN_POINT('Ctrl Pts',(31.6442818932852,-3.73228155061267,338.203007569372));
#65492=CARTESIAN_POINT('Ctrl Pts',(31.6365068145068,-3.64342461552501,338.30654747438));
#65493=CARTESIAN_POINT('Ctrl Pts',(31.6287317357283,-3.5501154423416,338.406550624546));
#65494=CARTESIAN_POINT('Ctrl Pts',(31.6209566569499,-3.45266639300717,338.50261014689));
#65495=CARTESIAN_POINT('Ctrl Pts',(31.6131911459009,-3.35533726093187,338.598551461877));
#65496=CARTESIAN_POINT('Ctrl Pts',(31.6054256348519,-3.25387866476962,338.690558533115));
#65497=CARTESIAN_POINT('Ctrl Pts',(31.5976601238029,-3.14864322042121,338.778257393693));
#65498=CARTESIAN_POINT('Ctrl Pts',(31.5899023122807,-3.04351211732204,338.865869300595));
#65499=CARTESIAN_POINT('Ctrl Pts',(31.5821445007585,-2.93461191665274,338.949181248944));
#65500=CARTESIAN_POINT('Ctrl Pts',(31.5743866892363,-2.82233183113247,339.027856265742));
#65501=CARTESIAN_POINT('Ctrl Pts',(31.5666347157133,-2.71013623993746,339.106472077094));
#65502=CARTESIAN_POINT('Ctrl Pts',(31.5588827421903,-2.59456614536722,339.180457679052));
#65503=CARTESIAN_POINT('Ctrl Pts',(31.5511307686673,-2.47604328148428,339.249516764376));
#65504=CARTESIAN_POINT('Ctrl Pts',(31.5433820781096,-2.3575706121044,339.318546603138));
#65505=CARTESIAN_POINT('Ctrl Pts',(31.535633387552,-2.23614799759166,339.382653878562));
#65506=CARTESIAN_POINT('Ctrl Pts',(31.5278846969944,-2.11222536994269,339.4415860961));
#65507=CARTESIAN_POINT('Ctrl Pts',(31.5201376186166,-1.98832852543143,339.500506052298));
#65508=CARTESIAN_POINT('Ctrl Pts',(31.5123905402387,-1.86193305516648,339.554252924508));
#65509=CARTESIAN_POINT('Ctrl Pts',(31.5046434618609,-1.73351230438936,339.602620791791));
#65510=CARTESIAN_POINT('Ctrl Pts',(31.4968963185551,-1.60509047732282,339.650989064444));
#65511=CARTESIAN_POINT('Ctrl Pts',(31.4891491752493,-1.4746437016785,339.693978104481));
#65512=CARTESIAN_POINT('Ctrl Pts',(31.4814020319435,-1.3426636796606,339.731430788442));
#65513=CARTESIAN_POINT('Ctrl Pts',(31.4736531469154,-1.21065398573155,339.768891892562));
#65514=CARTESIAN_POINT('Ctrl Pts',(31.4659042618874,-1.07711073545531,339.800814057125));
#65515=CARTESIAN_POINT('Ctrl Pts',(31.4581553768593,-0.942538719708399,
339.827090616961));
#65516=CARTESIAN_POINT('Ctrl Pts',(31.4503982670845,-0.807823867833764,
339.853395067009));
#65517=CARTESIAN_POINT('Ctrl Pts',(31.4426411573098,-0.672078453466667,
339.874041867117));
#65518=CARTESIAN_POINT('Ctrl Pts',(31.434884047535,-0.53581589397678,339.888975801767));
#65519=CARTESIAN_POINT('Ctrl Pts',(31.4271227926089,-0.399480520131655,
339.903917716634));
#65520=CARTESIAN_POINT('Ctrl Pts',(31.4193615376827,-0.262627840311631,
339.913140656849));
#65521=CARTESIAN_POINT('Ctrl Pts',(31.4116002827565,-0.125773254256806,
339.916641552016));
#65522=CARTESIAN_POINT('Ctrl Pts',(31.4038266123519,0.011300254534714,339.920148047475));
#65523=CARTESIAN_POINT('Ctrl Pts',(31.3960529419472,0.148375284626583,339.917914213039));
#65524=CARTESIAN_POINT('Ctrl Pts',(31.3882792715425,0.28493868404132,339.909989104757));
#65525=CARTESIAN_POINT('Ctrl Pts',(31.3808674673655,0.415145024357676,339.902432912173));
#65526=CARTESIAN_POINT('Ctrl Pts',(31.3734556631884,0.544886008445155,339.889703407325));
#65527=CARTESIAN_POINT('Ctrl Pts',(31.3660438590113,0.673725692947513,339.871886364968));
#65528=CARTESIAN_POINT('Ctrl Pts',(31.3582687802329,0.808880194181423,339.853196056291));
#65529=CARTESIAN_POINT('Ctrl Pts',(31.3504937014545,0.943469924318875,339.828847824632));
#65530=CARTESIAN_POINT('Ctrl Pts',(31.3427186226761,1.07698369821825,339.798884159497));
#65531=CARTESIAN_POINT('Ctrl Pts',(31.3349531116271,1.21033317491894,339.76895736656));
#65532=CARTESIAN_POINT('Ctrl Pts',(31.3271876005781,1.34260895208501,339.733428974134));
#65533=CARTESIAN_POINT('Ctrl Pts',(31.319422089529,1.47330573226343,339.6923931295));
#65534=CARTESIAN_POINT('Ctrl Pts',(31.3116642780068,1.60387292620369,339.651397972025));
#65535=CARTESIAN_POINT('Ctrl Pts',(31.3039064664846,1.73286386822704,339.604906345689));
#65536=CARTESIAN_POINT('Ctrl Pts',(31.2961486549624,1.85978456521492,339.553063192345));
#65537=CARTESIAN_POINT('Ctrl Pts',(31.2883966814394,1.98660975035308,339.501259052619));
#65538=CARTESIAN_POINT('Ctrl Pts',(31.2806447079164,2.11136743103507,339.444111549027));
#65539=CARTESIAN_POINT('Ctrl Pts',(31.2728927343935,2.23358021168292,339.381814977892));
#65540=CARTESIAN_POINT('Ctrl Pts',(31.2651440438358,2.35574123514595,339.319544789392));
#65541=CARTESIAN_POINT('Ctrl Pts',(31.2573953532782,2.47535915466006,339.252130047617));
#65542=CARTESIAN_POINT('Ctrl Pts',(31.2496466627206,2.5919781581514,339.179812470694));
#65543=CARTESIAN_POINT('Ctrl Pts',(31.2418995843427,2.70857289808504,339.107509940046));
#65544=CARTESIAN_POINT('Ctrl Pts',(31.2341525059649,2.82216963109671,339.030306809119));
#65545=CARTESIAN_POINT('Ctrl Pts',(31.2264054275871,2.93233903960476,338.948489688388));
#65546=CARTESIAN_POINT('Ctrl Pts',(31.2186582842812,3.04250937143871,338.866671881952));
#65547=CARTESIAN_POINT('Ctrl Pts',(31.2109111409754,3.14925200767299,338.780240241627));
#65548=CARTESIAN_POINT('Ctrl Pts',(31.2031639976696,3.25216873156023,338.689523221768));
#65549=CARTESIAN_POINT('Ctrl Pts',(31.1954151126415,3.35510859331142,338.598785806797));
#65550=CARTESIAN_POINT('Ctrl Pts',(31.1876662276135,3.45422053795569,338.503761353558));
#65551=CARTESIAN_POINT('Ctrl Pts',(31.1799173425854,3.54914169716858,338.404816628824));
#65552=CARTESIAN_POINT('Ctrl Pts',(31.1721602328107,3.64416360668084,338.305766883138));
#65553=CARTESIAN_POINT('Ctrl Pts',(31.1644031230359,3.73498557415616,338.202788836447));
#65554=CARTESIAN_POINT('Ctrl Pts',(31.1566460132612,3.82128332808883,338.096284352086));
#65555=CARTESIAN_POINT('Ctrl Pts',(31.1488847583351,3.90762719678175,337.989722955134));
#65556=CARTESIAN_POINT('Ctrl Pts',(31.1411235034089,3.98944180162696,337.879631679212));
#65557=CARTESIAN_POINT('Ctrl Pts',(31.1333622484828,4.06644564828986,337.766442273391));
#65558=CARTESIAN_POINT('Ctrl Pts',(31.1255885780781,4.14357267601213,337.653071801408));
#65559=CARTESIAN_POINT('Ctrl Pts',(31.1178149076735,4.21587336112481,337.536593628246));
#65560=CARTESIAN_POINT('Ctrl Pts',(31.1100412372688,4.28311125992551,337.417465821392));
#65561=CARTESIAN_POINT('Ctrl Pts',(31.1026294330916,4.34721921836145,337.303883442606));
#65562=CARTESIAN_POINT('Ctrl Pts',(31.0952176289144,4.40672499718929,337.18789281569));
#65563=CARTESIAN_POINT('Ctrl Pts',(31.0878058247372,4.46146481226643,337.069906952355));
#65564=CARTESIAN_POINT('Ctrl Pts',(31.0800307459588,4.5188875887413,336.946138250398));
#65565=CARTESIAN_POINT('Ctrl Pts',(31.0722556671803,4.57124686702669,336.819782649727));
#65566=CARTESIAN_POINT('Ctrl Pts',(31.0644805884019,4.61830174584348,336.691293010344));
#65567=CARTESIAN_POINT('Ctrl Pts',(31.0567150773529,4.66529872063617,336.562961485643));
#65568=CARTESIAN_POINT('Ctrl Pts',(31.0489495663039,4.70700415048781,336.432501510884));
#65569=CARTESIAN_POINT('Ctrl Pts',(31.0411840552549,4.74322376040758,336.30038894997));
#65570=CARTESIAN_POINT('Ctrl Pts',(31.0334262437326,4.77940745847878,336.168407379045));
#65571=CARTESIAN_POINT('Ctrl Pts',(31.0256684322104,4.8101160582647,336.034776857297));
#65572=CARTESIAN_POINT('Ctrl Pts',(31.0179106206881,4.83520411644096,335.899991230431));
#65573=CARTESIAN_POINT('Ctrl Pts',(31.0101586471651,4.86027329505767,335.765307034024));
#65574=CARTESIAN_POINT('Ctrl Pts',(31.0024066736422,4.87973027970994,335.629469845434));
#65575=CARTESIAN_POINT('Ctrl Pts',(30.9946547001192,4.89348011217991,335.492986261674));
#65576=CARTESIAN_POINT('Ctrl Pts',(30.9869060095615,4.90722412158774,335.356560478793));
#65577=CARTESIAN_POINT('Ctrl Pts',(30.9791573190039,4.9152657469226,335.219489233305));
#65578=CARTESIAN_POINT('Ctrl Pts',(30.9714086284463,4.91756158804584,335.082286634857));
#65579=CARTESIAN_POINT('Ctrl Pts',(30.9636615500684,4.91985695150017,334.945112582555));
#65580=CARTESIAN_POINT('Ctrl Pts',(30.9559144716906,4.91640890205861,334.807807622225));
#65581=CARTESIAN_POINT('Ctrl Pts',(30.9481673933127,4.90722612820735,334.670887877557));
#65582=CARTESIAN_POINT('Ctrl Pts',(30.9404202500069,4.89804327739564,334.533966985369));
#65583=CARTESIAN_POINT('Ctrl Pts',(30.9326731067011,4.88312563246593,334.39743170528));
#65584=CARTESIAN_POINT('Ctrl Pts',(30.9249259633953,4.86253389975909,334.261794651744));
#65585=CARTESIAN_POINT('Ctrl Pts',(30.9171770783672,4.84193753759356,334.126127104119));
#65586=CARTESIAN_POINT('Ctrl Pts',(30.9094281933391,4.81566460789602,333.991358571257));
#65587=CARTESIAN_POINT('Ctrl Pts',(30.901679308311,4.78382716379953,333.85799267542));
#65588=CARTESIAN_POINT('Ctrl Pts',(30.8939221985362,4.75195592711084,333.724485223643));
#65589=CARTESIAN_POINT('Ctrl Pts',(30.8861650887615,4.71450846867204,333.592383763648));
#65590=CARTESIAN_POINT('Ctrl Pts',(30.8784079789868,4.67164724201592,333.46217845357));
#65591=CARTESIAN_POINT('Ctrl Pts',(30.8706467240606,4.62876311169068,333.331903565937));
#65592=CARTESIAN_POINT('Ctrl Pts',(30.8628854691344,4.58045958627627,333.203527212847));
#65593=CARTESIAN_POINT('Ctrl Pts',(30.8551242142082,4.52694740003962,333.077519753086));
#65594=CARTESIAN_POINT('Ctrl Pts',(30.8473505438035,4.47334961174464,332.951310722455));
#65595=CARTESIAN_POINT('Ctrl Pts',(30.8395768733989,4.41452668030623,332.827478510862));
#65596=CARTESIAN_POINT('Ctrl Pts',(30.8318032029942,4.35073585119288,332.706469835462));
#65597=CARTESIAN_POINT('Ctrl Pts',(30.8243913988173,4.28991450052324,332.591094143017));
#65598=CARTESIAN_POINT('Ctrl Pts',(30.8169795946403,4.22457749916489,332.47828528034));
#65599=CARTESIAN_POINT('Ctrl Pts',(30.8095677904634,4.15498352447909,332.368404481345));
#65600=CARTESIAN_POINT('Ctrl Pts',(30.8017927116849,4.08197854178278,332.25313809707));
#65601=CARTESIAN_POINT('Ctrl Pts',(30.7940176329065,4.00405803135536,332.140729797118));
#65602=CARTESIAN_POINT('Ctrl Pts',(30.7862425541281,3.92147244732838,332.031627229045));
#65603=CARTESIAN_POINT('Ctrl Pts',(30.7784770430791,3.83898849012032,331.922658918629));
#65604=CARTESIAN_POINT('Ctrl Pts',(30.7707115320301,3.75185111525413,331.816988554787));
#65605=CARTESIAN_POINT('Ctrl Pts',(30.7629460209811,3.66035535349278,331.715037024766));
#65606=CARTESIAN_POINT('Ctrl Pts',(30.7551882094589,3.56895031004566,331.613186579985));
#65607=CARTESIAN_POINT('Ctrl Pts',(30.7474303979367,3.47319573882904,331.51504792025));
#65608=CARTESIAN_POINT('Ctrl Pts',(30.7396725864145,3.37342821750476,331.421010600205));
#65609=CARTESIAN_POINT('Ctrl Pts',(30.7319206128915,3.27373577440354,331.327044046225));
#65610=CARTESIAN_POINT('Ctrl Pts',(30.7241686393685,3.17003667539488,331.237172955651));
#65611=CARTESIAN_POINT('Ctrl Pts',(30.7164166658455,3.06270554137598,331.151751329588));
#65612=CARTESIAN_POINT('Ctrl Pts',(30.7086679752878,2.95541986215649,331.066365879635));
#65613=CARTESIAN_POINT('Ctrl Pts',(30.7009192847302,2.84450551243674,330.985426389251));
#65614=CARTESIAN_POINT('Ctrl Pts',(30.6931705941726,2.73037133167992,330.909247568767));
#65615=CARTESIAN_POINT('Ctrl Pts',(30.6854235157948,2.61626089749268,330.833084597923));
#65616=CARTESIAN_POINT('Ctrl Pts',(30.677676437417,2.49893228967761,330.761680543668));
#65617=CARTESIAN_POINT('Ctrl Pts',(30.6699293590392,2.37882422949319,330.695307403812));
#65618=CARTESIAN_POINT('Ctrl Pts',(30.6621822157334,2.25871516268753,330.628933707685));
#65619=CARTESIAN_POINT('Ctrl Pts',(30.6544350724276,2.1358269391622,330.567591199111));
#65620=CARTESIAN_POINT('Ctrl Pts',(30.6466879291218,2.01062347903329,330.511506233929));
#65621=CARTESIAN_POINT('Ctrl Pts',(30.6389390440937,1.88539187050874,330.455408659656));
#65622=CARTESIAN_POINT('Ctrl Pts',(30.6311901590656,1.75784434626526,330.404571140598));
#65623=CARTESIAN_POINT('Ctrl Pts',(30.6234412740376,1.62846505138709,330.35917198779));
#65624=CARTESIAN_POINT('Ctrl Pts',(30.6156841642628,1.49894843198843,330.313724647852));
#65625=CARTESIAN_POINT('Ctrl Pts',(30.6079270544881,1.36759652752169,330.273727334576));
#65626=CARTESIAN_POINT('Ctrl Pts',(30.6001699447134,1.23490943534894,330.239308690013));
#65627=CARTESIAN_POINT('Ctrl Pts',(30.5924086897872,1.10215143943639,330.204871653227));
#65628=CARTESIAN_POINT('Ctrl Pts',(30.584647434861,0.968057216076455,330.176019307367));
#65629=CARTESIAN_POINT('Ctrl Pts',(30.5768861799348,0.833136340411268,330.152828979623));
#65630=CARTESIAN_POINT('Ctrl Pts',(30.5691125095302,0.69799963531581,330.129601554911));
#65631=CARTESIAN_POINT('Ctrl Pts',(30.5613388391255,0.562034023282853,330.112054297706));
#65632=CARTESIAN_POINT('Ctrl Pts',(30.5535651687209,0.425754368582244,330.10021262909));
#65633=CARTESIAN_POINT('Ctrl Pts',(30.5461533645437,0.295818564593465,330.088922192996));
#65634=CARTESIAN_POINT('Ctrl Pts',(30.5387415603666,0.16559758482116,330.082818122776));
#65635=CARTESIAN_POINT('Ctrl Pts',(30.5313297561895,0.0355351837341363,
330.081878375516));
#65636=CARTESIAN_POINT('Ctrl Pts',(30.523554677411,-0.10090196306498,330.080892568444));
#65637=CARTESIAN_POINT('Ctrl Pts',(30.5157795986325,-0.237595759891083,
330.085587006932));
#65638=CARTESIAN_POINT('Ctrl Pts',(30.508004519854,-0.374034235261797,330.095993326539));
#65639=CARTESIAN_POINT('Ctrl Pts',(30.500239008805,-0.510304814402098,330.106386840506));
#65640=CARTESIAN_POINT('Ctrl Pts',(30.492473497756,-0.646320311217115,330.122478220786));
#65641=CARTESIAN_POINT('Ctrl Pts',(30.484707986707,-0.781567134566584,330.144247135957));
#65642=CARTESIAN_POINT('Ctrl Pts',(30.4769501751849,-0.916679860296481,
330.165994467184));
#65643=CARTESIAN_POINT('Ctrl Pts',(30.4691923636627,-1.05102504584502,330.193408068977));
#65644=CARTESIAN_POINT('Ctrl Pts',(30.4614345521406,-1.18409296491653,330.226415716368));
#65645=CARTESIAN_POINT('Ctrl Pts',(30.4536825786176,-1.31706074615948,330.259398524459));
#65646=CARTESIAN_POINT('Ctrl Pts',(30.4459306050945,-1.44875279626469,330.297966905227));
#65647=CARTESIAN_POINT('Ctrl Pts',(30.4381786315715,-1.57866869928789,330.341997402278));
#65648=CARTESIAN_POINT('Ctrl Pts',(30.4304299410139,-1.7085295828492,330.386009252387));
#65649=CARTESIAN_POINT('Ctrl Pts',(30.4226812504563,-1.83661544597911,330.435478492766));
#65650=CARTESIAN_POINT('Ctrl Pts',(30.4149325598987,-1.96244039555348,330.490231629407));
#65651=CARTESIAN_POINT('Ctrl Pts',(30.4071854815209,-2.08823916619601,330.5449733742));
#65652=CARTESIAN_POINT('Ctrl Pts',(30.399438403143,-2.21177760076029,330.604996672687));
#65653=CARTESIAN_POINT('Ctrl Pts',(30.3916913247652,-2.33258955323889,330.670079788423));
#65654=CARTESIAN_POINT('Ctrl Pts',(30.3839441814594,-2.45340251823852,330.735163449619));
#65655=CARTESIAN_POINT('Ctrl Pts',(30.3761970381535,-2.57148861145812,330.805306827265));
#65656=CARTESIAN_POINT('Ctrl Pts',(30.3684498948476,-2.68640643164944,330.880242295172));
#65657=CARTESIAN_POINT('Ctrl Pts',(30.3607010098195,-2.80135008780619,330.955194610162));
#65658=CARTESIAN_POINT('Ctrl Pts',(30.3529521247915,-2.91312372619639,331.034940945788));
#65659=CARTESIAN_POINT('Ctrl Pts',(30.3452032397634,-3.02131540258246,331.11917066845));
#65660=CARTESIAN_POINT('Ctrl Pts',(30.3374461299887,-3.12962191473137,331.20348979341));
#65661=CARTESIAN_POINT('Ctrl Pts',(30.329689020214,-3.23433856124815,331.292301570887));
#65662=CARTESIAN_POINT('Ctrl Pts',(30.3219319104392,-3.3350865329092,331.385255073936));
#65663=CARTESIAN_POINT('Ctrl Pts',(30.3141706555131,-3.43588834106494,331.478258248364));
#65664=CARTESIAN_POINT('Ctrl Pts',(30.306409400587,-3.53271697282055,331.57540728167));
#65665=CARTESIAN_POINT('Ctrl Pts',(30.2986481456608,-3.6252316417453,331.676315507424));
#65666=CARTESIAN_POINT('Ctrl Pts',(30.2908744752562,-3.71789430399012,331.777385153454));
#65667=CARTESIAN_POINT('Ctrl Pts',(30.2831008048515,-3.80622896130463,331.882225709576));
#65668=CARTESIAN_POINT('Ctrl Pts',(30.2753271344468,-3.88993561395867,331.99041797225));
#65669=CARTESIAN_POINT('Ctrl Pts',(30.2679153302697,-3.96974570179313,332.093573859067));
#65670=CARTESIAN_POINT('Ctrl Pts',(30.2605035260926,-4.04534878889836,332.199776196451));
#65671=CARTESIAN_POINT('Ctrl Pts',(30.2530917219155,-4.1165232706243,332.308639893119));
#65672=CARTESIAN_POINT('Ctrl Pts',(30.2451556062878,-4.19273263925065,332.425204613904));
#65673=CARTESIAN_POINT('Ctrl Pts',(30.2372194906601,-4.26409775774852,332.545177455763));
#65674=CARTESIAN_POINT('Ctrl Pts',(30.2292833750324,-4.33030650368065,332.668127652147));
#65675=CARTESIAN_POINT('Ctrl Pts',(30.2213581817776,-4.39642412737518,332.790908633772));
#65676=CARTESIAN_POINT('Ctrl Pts',(30.2134329885229,-4.45739933324267,332.916658489957));
#65677=CARTESIAN_POINT('Ctrl Pts',(30.2055077952681,-4.51296290784668,333.044917174414));
#65678=CARTESIAN_POINT('Ctrl Pts',(30.1975920649108,-4.56846013802329,333.173022714496));
#65679=CARTESIAN_POINT('Ctrl Pts',(30.1896763345534,-4.61855845715624,333.303630781464));
#65680=CARTESIAN_POINT('Ctrl Pts',(30.1817606041961,-4.66303434688629,333.436256497293));
#65681=CARTESIAN_POINT('Ctrl Pts',(30.1738548472716,-4.70745419917215,333.568715111211));
#65682=CARTESIAN_POINT('Ctrl Pts',(30.1659490903471,-4.74626562370331,333.703185958915));
#65683=CARTESIAN_POINT('Ctrl Pts',(30.1580433334226,-4.77929323461932,333.839164421625));
#65684=CARTESIAN_POINT('Ctrl Pts',(30.1501434334114,-4.81229637730814,333.975042145837));
#65685=CARTESIAN_POINT('Ctrl Pts',(30.1422435334003,-4.8395241506503,334.112424903701));
#65686=CARTESIAN_POINT('Ctrl Pts',(30.1343436333892,-4.86085091019586,334.250792758078));
#65687=CARTESIAN_POINT('Ctrl Pts',(30.1264486619213,-4.88216436452783,334.38907428833));
#65688=CARTESIAN_POINT('Ctrl Pts',(30.1185536904535,-4.89758408313149,334.528339326433));
#65689=CARTESIAN_POINT('Ctrl Pts',(30.1106587189856,-4.90703550375296,334.668057795079));
#65690=CARTESIAN_POINT('Ctrl Pts',(30.1043782714933,-4.91455410609148,334.779203795999));
#65691=CARTESIAN_POINT('Ctrl Pts',(30.098097824001,-4.91829683194439,334.890636452684));
#65692=CARTESIAN_POINT('Ctrl Pts',(30.0918173765087,-4.91824955753956,335.002086207555));
#65693=CARTESIAN_POINT('',(28.3418173765442,-4.91824878394571,335.00345857146));
#65694=CARTESIAN_POINT('Ctrl Pts',(30.0918173764651,-4.91824955753923,335.002086208329));
#65695=CARTESIAN_POINT('Ctrl Pts',(30.0833748463321,-4.91818600860648,335.151903226139));
#65696=CARTESIAN_POINT('Ctrl Pts',(30.0749323161992,-4.91127285299927,335.301501189361));
#65697=CARTESIAN_POINT('Ctrl Pts',(30.0664897860662,-4.89759480406423,335.450275690775));
#65698=CARTESIAN_POINT('Ctrl Pts',(30.0580087662007,-4.88385439651897,335.59972845933));
#65699=CARTESIAN_POINT('Ctrl Pts',(30.0495277463351,-4.86328735742158,335.748349980473));
#65700=CARTESIAN_POINT('Ctrl Pts',(30.0410467264695,-4.83603008344163,335.895542346596));
#65701=CARTESIAN_POINT('Ctrl Pts',(30.0325460595063,-4.80870966536653,336.043075697985));
#65702=CARTESIAN_POINT('Ctrl Pts',(30.0240453925431,-4.77466809916791,336.18917301959));
#65703=CARTESIAN_POINT('Ctrl Pts',(30.0155447255798,-4.73409179891901,336.333250877332));
#65704=CARTESIAN_POINT('Ctrl Pts',(30.0070152556246,-4.69337801312253,336.477816917167));
#65705=CARTESIAN_POINT('Ctrl Pts',(29.9984857856693,-4.64608526133677,336.620349544757));
#65706=CARTESIAN_POINT('Ctrl Pts',(29.989956315714,-4.59244935944606,336.760281779552));
#65707=CARTESIAN_POINT('Ctrl Pts',(29.9849221063565,-4.56079271951306,336.842871690708));
#65708=CARTESIAN_POINT('Ctrl Pts',(29.9798878969991,-4.52692731909805,336.924556191571));
#65709=CARTESIAN_POINT('Ctrl Pts',(29.9748536876417,-4.4909090793162,337.005222856397));
#65710=CARTESIAN_POINT('Ctrl Pts',(29.9670786088632,-4.435280750838,337.129808392928));
#65711=CARTESIAN_POINT('Ctrl Pts',(29.9593035300848,-4.37437626530274,337.252274206464));
#65712=CARTESIAN_POINT('Ctrl Pts',(29.9515284513063,-4.30837893831905,337.372141223947));
#65713=CARTESIAN_POINT('Ctrl Pts',(29.9437629402573,-4.24246282524772,337.491860737434));
#65714=CARTESIAN_POINT('Ctrl Pts',(29.9359974292083,-4.17146652711353,337.608987478806));
#65715=CARTESIAN_POINT('Ctrl Pts',(29.9282319181593,-4.09562132785343,337.723062430671));
#65716=CARTESIAN_POINT('Ctrl Pts',(29.9204741066371,-4.01985132932916,337.83702427689));
#65717=CARTESIAN_POINT('Ctrl Pts',(29.9127162951148,-3.93924221229227,337.94794003183));
#65718=CARTESIAN_POINT('Ctrl Pts',(29.9049584835926,-3.85407088995616,338.055375695016));
#65719=CARTESIAN_POINT('Ctrl Pts',(29.8972065100696,-3.76896366174128,338.162730509457));
#65720=CARTESIAN_POINT('Ctrl Pts',(29.8894545365467,-3.67930130369825,338.266610139829));
#65721=CARTESIAN_POINT('Ctrl Pts',(29.8817025630237,-3.58540349963867,338.366610284437));
#65722=CARTESIAN_POINT('Ctrl Pts',(29.8739538724661,-3.49154546135472,338.466568078925));
#65723=CARTESIAN_POINT('Ctrl Pts',(29.8662051819084,-3.3934558116268,338.562649371036));
#65724=CARTESIAN_POINT('Ctrl Pts',(29.8584564913508,-3.29149375881297,338.654483807352));
#65725=CARTESIAN_POINT('Ctrl Pts',(29.850709412973,-3.18955292005598,338.746299136746));
#65726=CARTESIAN_POINT('Ctrl Pts',(29.8429623345951,-3.08374157103421,338.83386910645));
#65727=CARTESIAN_POINT('Ctrl Pts',(29.8352152562173,-2.97445464637312,338.916861322433));
#65728=CARTESIAN_POINT('Ctrl Pts',(29.8274681129115,-2.86516680578219,338.99985423397));
#65729=CARTESIAN_POINT('Ctrl Pts',(29.8197209696057,-2.75240364274228,339.07826907887));
#65730=CARTESIAN_POINT('Ctrl Pts',(29.8119738262999,-2.63659160635575,339.151814996335));
#65731=CARTESIAN_POINT('Ctrl Pts',(29.8042249412718,-2.52075353296469,339.225377448484));
#65732=CARTESIAN_POINT('Ctrl Pts',(29.7964760562436,-2.40186555215315,339.294068585491));
#65733=CARTESIAN_POINT('Ctrl Pts',(29.7887271712155,-2.280381051891,339.357642174465));
#65734=CARTESIAN_POINT('Ctrl Pts',(29.7809700614408,-2.1587676067251,339.421283241103));
#65735=CARTESIAN_POINT('Ctrl Pts',(29.7732129516661,-2.03455248366223,339.479795727625));
#65736=CARTESIAN_POINT('Ctrl Pts',(29.7654558418914,-1.90821201557302,339.532980252121));
#65737=CARTESIAN_POINT('Ctrl Pts',(29.7576945869652,-1.78180403517733,339.586193196727));
#65738=CARTESIAN_POINT('Ctrl Pts',(29.7499333320391,-1.65326881283957,339.634072369847));
#65739=CARTESIAN_POINT('Ctrl Pts',(29.7421720771129,-1.52309945667756,339.676467802473));
#65740=CARTESIAN_POINT('Ctrl Pts',(29.7343984067082,-1.39272187196779,339.718931053975));
#65741=CARTESIAN_POINT('Ctrl Pts',(29.7266247363035,-1.26070530632257,339.755892930093));
#65742=CARTESIAN_POINT('Ctrl Pts',(29.7188510658989,-1.12755558341491,339.787254063533));
#65743=CARTESIAN_POINT('Ctrl Pts',(29.7114392617218,-1.00060401214312,339.817155328665));
#65744=CARTESIAN_POINT('Ctrl Pts',(29.7040274575448,-0.872622688943411,
339.841965491052));
#65745=CARTESIAN_POINT('Ctrl Pts',(29.6966156533677,-0.744053911628984,
339.8616424014));
#65746=CARTESIAN_POINT('Ctrl Pts',(29.6888405745893,-0.609183595551083,
339.882283735738));
#65747=CARTESIAN_POINT('Ctrl Pts',(29.6810654958108,-0.473240568433122,
339.897341133303));
#65748=CARTESIAN_POINT('Ctrl Pts',(29.6732904170324,-0.336726895624577,
339.906709494179));
#65749=CARTESIAN_POINT('Ctrl Pts',(29.6655249059834,-0.200381211581309,
339.91606632669));
#65750=CARTESIAN_POINT('Ctrl Pts',(29.6577593949344,-0.0634666652849358,
339.919748025437));
#65751=CARTESIAN_POINT('Ctrl Pts',(29.6499938838853,0.0735055847371469,
339.917700681367));
#65752=CARTESIAN_POINT('Ctrl Pts',(29.6422360723631,0.210342026374456,339.915655367244));
#65753=CARTESIAN_POINT('Ctrl Pts',(29.634478260841,0.347235669566546,339.90789232035));
#65754=CARTESIAN_POINT('Ctrl Pts',(29.6267204493188,0.483671700423804,339.894409540354));
#65755=CARTESIAN_POINT('Ctrl Pts',(29.6189684757958,0.620005058841578,339.880936906577));
#65756=CARTESIAN_POINT('Ctrl Pts',(29.6112165022727,0.75588110295841,339.861753145442));
#65757=CARTESIAN_POINT('Ctrl Pts',(29.6034645287496,0.890786847601078,339.836908295041));
#65758=CARTESIAN_POINT('Ctrl Pts',(29.595715838192,1.02563545958043,339.812073966449));
#65759=CARTESIAN_POINT('Ctrl Pts',(29.5879671476344,1.15951420577163,339.781583387647));
#65760=CARTESIAN_POINT('Ctrl Pts',(29.5802184570768,1.29191725983002,339.74553820512));
#65761=CARTESIAN_POINT('Ctrl Pts',(29.5724713786989,1.42429276632716,339.709500522094));
#65762=CARTESIAN_POINT('Ctrl Pts',(29.5647243003211,1.55519281448465,339.667910636687));
#65763=CARTESIAN_POINT('Ctrl Pts',(29.5569772219433,1.68412416528252,339.620920780365));
#65764=CARTESIAN_POINT('Ctrl Pts',(29.5492300786375,1.81305659664911,339.573930530224));
#65765=CARTESIAN_POINT('Ctrl Pts',(29.5414829353317,1.94001993050217,339.521540352745));
#65766=CARTESIAN_POINT('Ctrl Pts',(29.5337357920259,2.06453879971386,339.463951456611));
#65767=CARTESIAN_POINT('Ctrl Pts',(29.5259869069978,2.18908566341097,339.40634961327));
#65768=CARTESIAN_POINT('Ctrl Pts',(29.5182380219697,2.31118661418876,339.343546889572));
#65769=CARTESIAN_POINT('Ctrl Pts',(29.5104891369416,2.43038923531106,339.27579129839));
#65770=CARTESIAN_POINT('Ctrl Pts',(29.5027320271669,2.54971837932717,339.207963790722));
#65771=CARTESIAN_POINT('Ctrl Pts',(29.4949749173921,2.66614270810379,339.135173107628));
#65772=CARTESIAN_POINT('Ctrl Pts',(29.4872178076174,2.77923678609253,339.057711910588));
#65773=CARTESIAN_POINT('Ctrl Pts',(29.4794565526912,2.89239129794042,338.980209320762));
#65774=CARTESIAN_POINT('Ctrl Pts',(29.4716952977651,3.00221170023099,338.898031478001));
#65775=CARTESIAN_POINT('Ctrl Pts',(29.463934042839,3.10830503172824,338.811511890606));
#65776=CARTESIAN_POINT('Ctrl Pts',(29.4561603724343,3.21456807798016,338.724853900068));
#65777=CARTESIAN_POINT('Ctrl Pts',(29.4483867020296,3.31709184693499,338.633840545607));
#65778=CARTESIAN_POINT('Ctrl Pts',(29.4406130316249,3.41551904829943,338.538843411795));
#65779=CARTESIAN_POINT('Ctrl Pts',(29.4332012274478,3.50936443976054,338.448268417416));
#65780=CARTESIAN_POINT('Ctrl Pts',(29.4257894232707,3.59948587216437,338.354072394849));
#65781=CARTESIAN_POINT('Ctrl Pts',(29.4183776190936,3.68560854854448,338.25660447236));
#65782=CARTESIAN_POINT('Ctrl Pts',(29.4106025403151,3.77595235383988,338.154359356648));
#65783=CARTESIAN_POINT('Ctrl Pts',(29.4028274615367,3.86218101307005,338.048190386743));
#65784=CARTESIAN_POINT('Ctrl Pts',(29.3950523827583,3.94393444910542,337.938462884513));
#65785=CARTESIAN_POINT('Ctrl Pts',(29.3872868717093,4.02558728233306,337.82887040896));
#65786=CARTESIAN_POINT('Ctrl Pts',(29.3795213606602,4.10277561851078,337.715728424483));
#65787=CARTESIAN_POINT('Ctrl Pts',(29.3717558496112,4.17517750715662,337.599437601912));
#65788=CARTESIAN_POINT('Ctrl Pts',(29.363998038089,4.24750760911913,337.483262082029));
#65789=CARTESIAN_POINT('Ctrl Pts',(29.3562402265668,4.31506050265605,337.363944266854));
#65790=CARTESIAN_POINT('Ctrl Pts',(29.3484824150446,4.37755591030942,337.241915991873));
#65791=CARTESIAN_POINT('Ctrl Pts',(29.3407304415216,4.44000428818668,337.119979547039));
#65792=CARTESIAN_POINT('Ctrl Pts',(29.3329784679986,4.49740257821792,336.995337048839));
#65793=CARTESIAN_POINT('Ctrl Pts',(29.3252264944755,4.5495152527901,336.868446955932));
#65794=CARTESIAN_POINT('Ctrl Pts',(29.3174778039179,4.60160585761365,336.741610601054));
#65795=CARTESIAN_POINT('Ctrl Pts',(29.3097291133602,4.64841515093551,336.612528905465));
#65796=CARTESIAN_POINT('Ctrl Pts',(29.3019804228026,4.68975487779492,336.481682236075));
#65797=CARTESIAN_POINT('Ctrl Pts',(29.2942333444247,4.73108600357889,336.350862790426));
#65798=CARTESIAN_POINT('Ctrl Pts',(29.2864862660469,4.76694970875933,336.218279473879));
#65799=CARTESIAN_POINT('Ctrl Pts',(29.2787391876691,4.79720708809017,336.08442944283));
#65800=CARTESIAN_POINT('Ctrl Pts',(29.2709920443633,4.82746472100695,335.95057828999));
#65801=CARTESIAN_POINT('Ctrl Pts',(29.2632449010575,4.85211584817201,335.815460782727));
#65802=CARTESIAN_POINT('Ctrl Pts',(29.2554977577516,4.87107242182887,335.679585552965));
#65803=CARTESIAN_POINT('Ctrl Pts',(29.2477488727235,4.89003325732592,335.543679775566));
#65804=CARTESIAN_POINT('Ctrl Pts',(29.2399999876955,4.90329693774831,335.407016323735));
#65805=CARTESIAN_POINT('Ctrl Pts',(29.2322511026674,4.91082719375468,335.270109858353));
#65806=CARTESIAN_POINT('Ctrl Pts',(29.2244939928926,4.91836544245259,335.133058079034));
#65807=CARTESIAN_POINT('Ctrl Pts',(29.2167368831179,4.92015808884482,334.99576316181));
#65808=CARTESIAN_POINT('Ctrl Pts',(29.2089797733431,4.91622101062853,334.858741240432));
#65809=CARTESIAN_POINT('Ctrl Pts',(29.201218518417,4.91228182856354,334.721646098921));
#65810=CARTESIAN_POINT('Ctrl Pts',(29.1934572634908,4.90260684857121,334.584824633638));
#65811=CARTESIAN_POINT('Ctrl Pts',(29.1856960085646,4.88726387102354,334.448787774548));
#65812=CARTESIAN_POINT('Ctrl Pts',(29.1779223381599,4.87189634971204,334.312533300817));
#65813=CARTESIAN_POINT('Ctrl Pts',(29.1701486677553,4.85084277245481,334.17706632781));
#65814=CARTESIAN_POINT('Ctrl Pts',(29.1623749973506,4.8242222623668,334.04288839429));
#65815=CARTESIAN_POINT('Ctrl Pts',(29.1549631931737,4.79884094342834,333.914956475859));
#65816=CARTESIAN_POINT('Ctrl Pts',(29.1475513889967,4.76839937670889,333.788196567919));
#65817=CARTESIAN_POINT('Ctrl Pts',(29.1401395848197,4.73304244320891,333.66302868644));
#65818=CARTESIAN_POINT('Ctrl Pts',(29.1323645060413,4.69595256107468,333.531725954231));
#65819=CARTESIAN_POINT('Ctrl Pts',(29.1245894272628,4.65333608457454,333.401760313487));
#65820=CARTESIAN_POINT('Ctrl Pts',(29.1168143484844,4.60530536226591,333.273632257372));
#65821=CARTESIAN_POINT('Ctrl Pts',(29.1090488374354,4.55733374481887,333.145661870988));
#65822=CARTESIAN_POINT('Ctrl Pts',(29.1012833263864,4.50396127406574,333.019524932469));
#65823=CARTESIAN_POINT('Ctrl Pts',(29.0935178153374,4.44535065677531,332.895709002821));
#65824=CARTESIAN_POINT('Ctrl Pts',(29.0857600038152,4.3867981520826,332.772015837028));
#65825=CARTESIAN_POINT('Ctrl Pts',(29.0780021922929,4.32301800264464,332.650639451429));
#65826=CARTESIAN_POINT('Ctrl Pts',(29.0702443807708,4.25422167392141,332.532049228279));
#65827=CARTESIAN_POINT('Ctrl Pts',(29.0624924072478,4.1854771166172,332.413548248033));
#65828=CARTESIAN_POINT('Ctrl Pts',(29.0547404337248,4.11172408899903,332.297829593646));
#65829=CARTESIAN_POINT('Ctrl Pts',(29.0469884602018,4.03322066122813,332.1853394236));
#65830=CARTESIAN_POINT('Ctrl Pts',(29.0392397696442,3.95475047970551,332.072896893207));
#65831=CARTESIAN_POINT('Ctrl Pts',(29.0314910790866,3.87153412258074,331.963680447631));
#65832=CARTESIAN_POINT('Ctrl Pts',(29.023742388529,3.78387366507585,331.858108348583));
#65833=CARTESIAN_POINT('Ctrl Pts',(29.0159953101512,3.69623144606129,331.752558214692));
#65834=CARTESIAN_POINT('Ctrl Pts',(29.0082482317734,3.60414721536821,331.650651219674));
#65835=CARTESIAN_POINT('Ctrl Pts',(29.0005011533955,3.50796387281852,331.552773211769));
#65836=CARTESIAN_POINT('Ctrl Pts',(28.9927540100897,3.41177972415979,331.454894383551));
#65837=CARTESIAN_POINT('Ctrl Pts',(28.9850068667839,3.31149666908763,331.361044888588));
#65838=CARTESIAN_POINT('Ctrl Pts',(28.9772597234781,3.20749477934344,331.271574018036));
#65839=CARTESIAN_POINT('Ctrl Pts',(28.96951083845,3.10346950776641,331.182083032532));
#65840=CARTESIAN_POINT('Ctrl Pts',(28.9617619534219,2.99572403408152,331.096972885164));
#65841=CARTESIAN_POINT('Ctrl Pts',(28.9540130683938,2.88467152018146,331.016552588127));
#65842=CARTESIAN_POINT('Ctrl Pts',(28.9462559586191,2.77350113399575,330.936046932157));
#65843=CARTESIAN_POINT('Ctrl Pts',(28.9384988488444,2.65901701286916,330.860241299871));
#65844=CARTESIAN_POINT('Ctrl Pts',(28.9307417390696,2.54166177701609,330.789401648963));
#65845=CARTESIAN_POINT('Ctrl Pts',(28.9229804841435,2.42424383027719,330.718524143611));
#65846=CARTESIAN_POINT('Ctrl Pts',(28.9152192292173,2.30395205433861,330.652618095014));
#65847=CARTESIAN_POINT('Ctrl Pts',(28.9074579742911,2.1812527917797,330.591902981915));
#65848=CARTESIAN_POINT('Ctrl Pts',(28.8996843038865,2.05835725038846,330.531090744421));
#65849=CARTESIAN_POINT('Ctrl Pts',(28.8919106334818,1.93304688401821,330.475486194508));
#65850=CARTESIAN_POINT('Ctrl Pts',(28.8841369630772,1.80580791166782,330.425260570409));
#65851=CARTESIAN_POINT('Ctrl Pts',(28.8767251589001,1.68449194409125,330.377372961194));
#65852=CARTESIAN_POINT('Ctrl Pts',(28.8693133547229,1.56142315470923,330.334374864422));
#65853=CARTESIAN_POINT('Ctrl Pts',(28.8619015505458,1.43703314733344,330.296371741308));
#65854=CARTESIAN_POINT('Ctrl Pts',(28.8541264717673,1.30654641515847,330.256505971925));
#65855=CARTESIAN_POINT('Ctrl Pts',(28.8463513929889,1.17419331439411,330.222011210563));
#65856=CARTESIAN_POINT('Ctrl Pts',(28.8385763142105,1.04045551867186,330.193063826494));
#65857=CARTESIAN_POINT('Ctrl Pts',(28.8308108031615,0.90688229582142,330.164152064023));
#65858=CARTESIAN_POINT('Ctrl Pts',(28.8230452921124,0.77192814677124,330.140774178162));
#65859=CARTESIAN_POINT('Ctrl Pts',(28.8152797810634,0.636091121940693,330.123057192555));
#65860=CARTESIAN_POINT('Ctrl Pts',(28.8075219695412,0.500388779915651,330.105357773391));
#65861=CARTESIAN_POINT('Ctrl Pts',(28.799764158019,0.363805689248478,330.09330813492));
#65862=CARTESIAN_POINT('Ctrl Pts',(28.7920063464968,0.226850999585688,330.086984460997));
#65863=CARTESIAN_POINT('Ctrl Pts',(28.7842543729738,0.0899993726701375,
330.080665545839));
#65864=CARTESIAN_POINT('Ctrl Pts',(28.7765023994509,-0.0472229077451133,
330.080064036391));
#65865=CARTESIAN_POINT('Ctrl Pts',(28.7687504259279,-0.184301000902406,
330.085204357904));
#65866=CARTESIAN_POINT('Ctrl Pts',(28.7610017353703,-0.321321041405862,
330.090342502488));
#65867=CARTESIAN_POINT('Ctrl Pts',(28.7532530448127,-0.458196626315287,
330.101217626997));
#65868=CARTESIAN_POINT('Ctrl Pts',(28.745504354255,-0.594412560198523,330.117802055347));
#65869=CARTESIAN_POINT('Ctrl Pts',(28.7377572758772,-0.730600153219017,
330.134383033167));
#65870=CARTESIAN_POINT('Ctrl Pts',(28.7300101974994,-0.866127980439663,
330.156670904861));
#65871=CARTESIAN_POINT('Ctrl Pts',(28.7222631191215,-1.00048601107593,330.184586123276));
#65872=CARTESIAN_POINT('Ctrl Pts',(28.7145159758157,-1.13484516776191,330.212501575648));
#65873=CARTESIAN_POINT('Ctrl Pts',(28.70676883251,-1.26803412560718,330.246044389296));
#65874=CARTESIAN_POINT('Ctrl Pts',(28.6990216892042,-1.39955347959971,330.285083975272));
#65875=CARTESIAN_POINT('Ctrl Pts',(28.6912728041761,-1.53110240193507,330.324132338175));
#65876=CARTESIAN_POINT('Ctrl Pts',(28.683523919148,-1.66098059884722,330.368679821285));
#65877=CARTESIAN_POINT('Ctrl Pts',(28.6757750341199,-1.78870462978005,330.418546212183));
#65878=CARTESIAN_POINT('Ctrl Pts',(28.6680179243452,-1.91656422831913,330.468465531783));
#65879=CARTESIAN_POINT('Ctrl Pts',(28.6602608145705,-2.04226472878972,330.523714894294));
#65880=CARTESIAN_POINT('Ctrl Pts',(28.6525037047958,-2.16534295449788,330.584066015903));
#65881=CARTESIAN_POINT('Ctrl Pts',(28.6447424498696,-2.28848694927466,330.644449387221));
#65882=CARTESIAN_POINT('Ctrl Pts',(28.6369811949434,-2.40900553388457,330.709939763336));
#65883=CARTESIAN_POINT('Ctrl Pts',(28.6292199400172,-2.52646177924276,330.780263759365));
#65884=CARTESIAN_POINT('Ctrl Pts',(28.6214462696126,-2.64410591631447,330.85070025087));
#65885=CARTESIAN_POINT('Ctrl Pts',(28.613672599208,-2.75867759815802,330.925985598783));
#65886=CARTESIAN_POINT('Ctrl Pts',(28.6058989288033,-2.86976970588929,331.005803598011));
#65887=CARTESIAN_POINT('Ctrl Pts',(28.5984871246262,-2.97569044927921,331.081906050173));
#65888=CARTESIAN_POINT('Ctrl Pts',(28.591075320449,-3.07844804979954,331.162128483327));
#65889=CARTESIAN_POINT('Ctrl Pts',(28.5836635162719,-3.17772025727494,331.246165023738));
#65890=CARTESIAN_POINT('Ctrl Pts',(28.5759987752936,-3.28038024915522,331.333069412949));
#65891=CARTESIAN_POINT('Ctrl Pts',(28.5683340343153,-3.37965706404458,331.424344666846));
#65892=CARTESIAN_POINT('Ctrl Pts',(28.560669293337,-3.47514759112905,331.519693651075));
#65893=CARTESIAN_POINT('Ctrl Pts',(28.5530140433566,-3.57051987542011,331.614924567777));
#65894=CARTESIAN_POINT('Ctrl Pts',(28.5453587933761,-3.66211491337428,331.714218901576));
#65895=CARTESIAN_POINT('Ctrl Pts',(28.5377035433956,-3.74956170951572,331.817238612614));
#65896=CARTESIAN_POINT('Ctrl Pts',(28.5300558174099,-3.83692255820402,331.920157070294));
#65897=CARTESIAN_POINT('Ctrl Pts',(28.5224080914242,-3.92014301570395,332.02679331707));
#65898=CARTESIAN_POINT('Ctrl Pts',(28.5147603654385,-3.99888847757235,332.136772100157));
#65899=CARTESIAN_POINT('Ctrl Pts',(28.507118327176,-4.07757537531465,332.246669090451));
#65900=CARTESIAN_POINT('Ctrl Pts',(28.4994762889135,-4.15179366607566,332.359903344221));
#65901=CARTESIAN_POINT('Ctrl Pts',(28.491834250651,-4.22124899208689,332.476066560048));
#65902=CARTESIAN_POINT('Ctrl Pts',(28.4841952106736,-4.29067706792492,332.592184200282));
#65903=CARTESIAN_POINT('Ctrl Pts',(28.4765561706961,-4.35534568807508,332.711228172525));
#65904=CARTESIAN_POINT('Ctrl Pts',(28.4689171307186,-4.41500402604019,332.832761546911));
#65905=CARTESIAN_POINT('Ctrl Pts',(28.4612793247114,-4.47465272711185,332.954275289436));
#65906=CARTESIAN_POINT('Ctrl Pts',(28.4536415187043,-4.52929257855681,333.078277272578));
#65907=CARTESIAN_POINT('Ctrl Pts',(28.4460037126971,-4.57871916181047,333.204306846989));
#65908=CARTESIAN_POINT('Ctrl Pts',(28.4383653776117,-4.62814916889134,333.330345151591));
#65909=CARTESIAN_POINT('Ctrl Pts',(28.4307270425263,-4.6723650439274,333.458410951158));
#65910=CARTESIAN_POINT('Ctrl Pts',(28.4230887074409,-4.7112110844228,333.588025077945));
#65911=CARTESIAN_POINT('Ctrl Pts',(28.415444459477,-4.75008719585863,333.717739539764));
#65912=CARTESIAN_POINT('Ctrl Pts',(28.407800211513,-4.7835850566836,333.849004335692));
#65913=CARTESIAN_POINT('Ctrl Pts',(28.4001559635491,-4.81159925285147,333.981326503506));
#65914=CARTESIAN_POINT('Ctrl Pts',(28.3925084442849,-4.83962543749063,334.113705297628));
#65915=CARTESIAN_POINT('Ctrl Pts',(28.3848609250207,-4.86216321672974,334.247141967853));
#65916=CARTESIAN_POINT('Ctrl Pts',(28.3772134057565,-4.87915880462597,334.381136184819));
#65917=CARTESIAN_POINT('Ctrl Pts',(28.3695564433058,-4.8961753787402,334.515295858364));
#65918=CARTESIAN_POINT('Ctrl Pts',(28.3618994808551,-4.90763606336808,334.65001405242));
#65919=CARTESIAN_POINT('Ctrl Pts',(28.3542425184044,-4.91353913253374,334.784787882405));
#65920=CARTESIAN_POINT('Ctrl Pts',(28.350100804451,-4.91673215118683,334.8576881553));
#65921=CARTESIAN_POINT('Ctrl Pts',(28.3459590904975,-4.9183000156394,334.930604730489));
#65922=CARTESIAN_POINT('Ctrl Pts',(28.3418173765441,-4.91824878394571,335.003458571461));
#65923=CARTESIAN_POINT('',(26.59181737648,-4.9182484316936,334.996072323401));
#65924=CARTESIAN_POINT('Ctrl Pts',(28.3418173765088,-4.91824878394527,335.003458572083));
#65925=CARTESIAN_POINT('Ctrl Pts',(28.3296867450051,-4.9180987318373,335.216839580139));
#65926=CARTESIAN_POINT('Ctrl Pts',(28.3175561135015,-4.90406196907175,335.429737823245));
#65927=CARTESIAN_POINT('Ctrl Pts',(28.3054254819979,-4.87632668485687,335.64079725737));
#65928=CARTESIAN_POINT('Ctrl Pts',(28.2976504032195,-4.85854986757834,335.776074940709));
#65929=CARTESIAN_POINT('Ctrl Pts',(28.2898753244411,-4.83511144100055,335.910826089138));
#65930=CARTESIAN_POINT('Ctrl Pts',(28.2821002456626,-4.8060504402412,336.044539242134));
#65931=CARTESIAN_POINT('Ctrl Pts',(28.2743347346136,-4.77702520089336,336.178087852582));
#65932=CARTESIAN_POINT('Ctrl Pts',(28.2665692235646,-4.74239123628207,336.310600630791));
#65933=CARTESIAN_POINT('Ctrl Pts',(28.2588037125156,-4.70223927789326,336.441571654805));
#65934=CARTESIAN_POINT('Ctrl Pts',(28.2510459009934,-4.66212713028812,336.572412820668));
#65935=CARTESIAN_POINT('Ctrl Pts',(28.2432880894712,-4.61650799054735,336.701714903145));
#65936=CARTESIAN_POINT('Ctrl Pts',(28.235530277949,-4.56552345994233,336.828982941204));
#65937=CARTESIAN_POINT('Ctrl Pts',(28.227778304426,-4.51457729681361,336.956155206029));
#65938=CARTESIAN_POINT('Ctrl Pts',(28.220026330903,-4.45827392429117,337.081296111805));
#65939=CARTESIAN_POINT('Ctrl Pts',(28.21227435738,-4.39680440911616,337.203926961239));
#65940=CARTESIAN_POINT('Ctrl Pts',(28.2045256668224,-4.33536092631716,337.326505876436));
#65941=CARTESIAN_POINT('Ctrl Pts',(28.1967769762649,-4.2687558271648,337.446576500838));
#65942=CARTESIAN_POINT('Ctrl Pts',(28.1890282857073,-4.19722774493399,337.563681399795));
#65943=CARTESIAN_POINT('Ctrl Pts',(28.1812812073295,-4.1257145447181,337.6807619341));
#65944=CARTESIAN_POINT('Ctrl Pts',(28.1735341289516,-4.04928060238351,337.794877636942));
#65945=CARTESIAN_POINT('Ctrl Pts',(28.1657870505738,-3.96820962151983,337.905597264278));
#65946=CARTESIAN_POINT('Ctrl Pts',(28.158039907268,-3.88713796120325,338.016317819551));
#65947=CARTESIAN_POINT('Ctrl Pts',(28.1502927639621,-3.80142941576291,338.123641927177));
#65948=CARTESIAN_POINT('Ctrl Pts',(28.1425456206563,-3.71140974181861,338.227169160554));
#65949=CARTESIAN_POINT('Ctrl Pts',(28.1347967356282,-3.62136982954056,338.330719669051));
#65950=CARTESIAN_POINT('Ctrl Pts',(28.1270478506002,-3.52701711651951,338.430471309791));
#65951=CARTESIAN_POINT('Ctrl Pts',(28.1192989655721,-3.4287159097258,338.526058744958));
#65952=CARTESIAN_POINT('Ctrl Pts',(28.1115418557974,-3.33031036501543,338.621747637616));
#65953=CARTESIAN_POINT('Ctrl Pts',(28.1037847460227,-3.227948235346,338.713263222551));
#65954=CARTESIAN_POINT('Ctrl Pts',(28.096027636248,-3.12202918419641,338.800278520783));
#65955=CARTESIAN_POINT('Ctrl Pts',(28.0882663813218,-3.01605353329245,338.887340317209));
#65956=CARTESIAN_POINT('Ctrl Pts',(28.0805051263956,-2.90651748556918,338.96989679999));
#65957=CARTESIAN_POINT('Ctrl Pts',(28.0727438714694,-2.7938508785489,339.047663564445));
#65958=CARTESIAN_POINT('Ctrl Pts',(28.0649702010648,-2.68100404167551,339.125554730378));
#65959=CARTESIAN_POINT('Ctrl Pts',(28.0571965306601,-2.56501696915984,339.198640658573));
#65960=CARTESIAN_POINT('Ctrl Pts',(28.0494228602555,-2.44634612069107,339.266681816152));
#65961=CARTESIAN_POINT('Ctrl Pts',(28.0420110560783,-2.33319942876795,339.331555641476));
#65962=CARTESIAN_POINT('Ctrl Pts',(28.0345992519012,-2.21761345267156,339.391843661645));
#65963=CARTESIAN_POINT('Ctrl Pts',(28.027187447724,-2.10000008820916,339.447379306066));
#65964=CARTESIAN_POINT('Ctrl Pts',(28.0194123689456,-1.9766221424033,339.505636917851));
#65965=CARTESIAN_POINT('Ctrl Pts',(28.0116372901671,-1.85062314938169,339.558848623339));
#65966=CARTESIAN_POINT('Ctrl Pts',(28.0038622113887,-1.72245433135183,339.606770467356));
#65967=CARTESIAN_POINT('Ctrl Pts',(27.9960967003397,-1.59444323321236,339.654633340494));
#65968=CARTESIAN_POINT('Ctrl Pts',(27.9883311892907,-1.46426798543332,339.697219168639));
#65969=CARTESIAN_POINT('Ctrl Pts',(27.9805656782417,-1.33240312859241,339.734330466435));
#65970=CARTESIAN_POINT('Ctrl Pts',(27.9728078667195,-1.20066901614088,339.771404968272));
#65971=CARTESIAN_POINT('Ctrl Pts',(27.9650500551973,-1.06724900230795,339.803015636602));
#65972=CARTESIAN_POINT('Ctrl Pts',(27.9572922436751,-0.932635938957153,
339.829013695142));
#65973=CARTESIAN_POINT('Ctrl Pts',(27.9495402701521,-0.798124176205531,
339.854992189317));
#65974=CARTESIAN_POINT('Ctrl Pts',(27.9417882966291,-0.662421533215169,
339.875366406883));
#65975=CARTESIAN_POINT('Ctrl Pts',(27.9340363231061,-0.526033953929984,
339.890037969363));
#65976=CARTESIAN_POINT('Ctrl Pts',(27.9262876325485,-0.389704134865414,
339.904703318428));
#65977=CARTESIAN_POINT('Ctrl Pts',(27.9185389419909,-0.252690344260004,
339.913670774108));
#65978=CARTESIAN_POINT('Ctrl Pts',(27.9107902514332,-0.115506386827868,
339.916893464079));
#65979=CARTESIAN_POINT('Ctrl Pts',(27.9030431730554,0.0216490283361404,
339.920115483542));
#65980=CARTESIAN_POINT('Ctrl Pts',(27.8952960946776,0.158974149383418,339.917595105551));
#65981=CARTESIAN_POINT('Ctrl Pts',(27.8875490162998,0.295952805707266,339.909337531612));
#65982=CARTESIAN_POINT('Ctrl Pts',(27.879801872994,0.432932610044187,339.901079888466));
#65983=CARTESIAN_POINT('Ctrl Pts',(27.8720547296881,0.569565553700036,339.887084976986));
#65984=CARTESIAN_POINT('Ctrl Pts',(27.8643075863823,0.705338623802703,339.867410039053));
#65985=CARTESIAN_POINT('Ctrl Pts',(27.8565587013542,0.841142218573888,339.847730677775));
#65986=CARTESIAN_POINT('Ctrl Pts',(27.8488098163261,0.976085168352783,339.822368805021));
#65987=CARTESIAN_POINT('Ctrl Pts',(27.841060931298,1.10966310537149,339.791433069039));
#65988=CARTESIAN_POINT('Ctrl Pts',(27.8333038215233,1.24338282339285,339.760464497546));
#65989=CARTESIAN_POINT('Ctrl Pts',(27.8255467117486,1.37573425306583,339.723910333078));
#65990=CARTESIAN_POINT('Ctrl Pts',(27.8177896019738,1.5062261499503,339.681929714093));
#65991=CARTESIAN_POINT('Ctrl Pts',(27.8100283470477,1.63678777753205,339.639926662007));
#65992=CARTESIAN_POINT('Ctrl Pts',(27.8022670921215,1.76548752576845,339.59249151255));
#65993=CARTESIAN_POINT('Ctrl Pts',(27.7945058371953,1.89185362294645,339.539831817573));
#65994=CARTESIAN_POINT('Ctrl Pts',(27.7867321667907,2.01842186469732,339.487087884245));
#65995=CARTESIAN_POINT('Ctrl Pts',(27.778958496386,2.14264864121181,339.429102869907));
#65996=CARTESIAN_POINT('Ctrl Pts',(27.7711848259813,2.26408550765253,339.366130996264));
#65997=CARTESIAN_POINT('Ctrl Pts',(27.7637730218042,2.37986945874392,339.30609047849));
#65998=CARTESIAN_POINT('Ctrl Pts',(27.7563612176272,2.49311714507877,339.241517072312));
#65999=CARTESIAN_POINT('Ctrl Pts',(27.7489494134502,2.60346559343578,339.172667008796));
#66000=CARTESIAN_POINT('Ctrl Pts',(27.7411743346717,2.71922254795856,339.100442398573));
#66001=CARTESIAN_POINT('Ctrl Pts',(27.7333992558933,2.83215469127028,339.023283064397));
#66002=CARTESIAN_POINT('Ctrl Pts',(27.7256241771148,2.94181269403341,338.941436430506));
#66003=CARTESIAN_POINT('Ctrl Pts',(27.7178586660658,3.05133575564297,338.859690514109));
#66004=CARTESIAN_POINT('Ctrl Pts',(27.7100931550168,3.15759238308679,338.773269006268));
#66005=CARTESIAN_POINT('Ctrl Pts',(27.7023276439678,3.26015970557934,338.682464087621));
#66006=CARTESIAN_POINT('Ctrl Pts',(27.6945698324456,3.36262533227309,338.591749202314));
#66007=CARTESIAN_POINT('Ctrl Pts',(27.6868120209233,3.46140864278015,338.496659812744));
#66008=CARTESIAN_POINT('Ctrl Pts',(27.6790542094011,3.55611781752552,338.397529857172));
#66009=CARTESIAN_POINT('Ctrl Pts',(27.6713022358781,3.65075572061336,338.298474500036));
#66010=CARTESIAN_POINT('Ctrl Pts',(27.663550262355,3.74132532156719,338.195384910653));
#66011=CARTESIAN_POINT('Ctrl Pts',(27.655798288832,3.82747009652994,338.088633309843));
#66012=CARTESIAN_POINT('Ctrl Pts',(27.6480495982744,3.91357838912935,337.981926918398));
#66013=CARTESIAN_POINT('Ctrl Pts',(27.6403009077167,3.99526533786943,337.871561903638));
#66014=CARTESIAN_POINT('Ctrl Pts',(27.6325522171591,4.07221347759927,337.757944969603));
#66015=CARTESIAN_POINT('Ctrl Pts',(27.6248051387812,4.14914560762594,337.64435167452));
#66016=CARTESIAN_POINT('Ctrl Pts',(27.6170580604034,4.22134067071622,337.527508129378));
#66017=CARTESIAN_POINT('Ctrl Pts',(27.6093109820256,4.2885237113934,337.407851207886));
#66018=CARTESIAN_POINT('Ctrl Pts',(27.6015638387197,4.35570731512909,337.288193283553));
#66019=CARTESIAN_POINT('Ctrl Pts',(27.593816695414,4.41787862130623,337.165722276667));
#66020=CARTESIAN_POINT('Ctrl Pts',(27.5860695521081,4.47480814514108,337.040900567563));
#66021=CARTESIAN_POINT('Ctrl Pts',(27.57832066708,4.53175046794154,336.916050795888));
#66022=CARTESIAN_POINT('Ctrl Pts',(27.5705717820519,4.58344850122072,336.788849625926));
#66023=CARTESIAN_POINT('Ctrl Pts',(27.5628228970238,4.62972066726931,336.659779987095));
#66024=CARTESIAN_POINT('Ctrl Pts',(27.5550657872491,4.6760419470731,336.530573352414));
#66025=CARTESIAN_POINT('Ctrl Pts',(27.5473086774744,4.71692572324246,336.399494655737));
#66026=CARTESIAN_POINT('Ctrl Pts',(27.5395515676996,4.75223997814796,336.267043113944));
#66027=CARTESIAN_POINT('Ctrl Pts',(27.5317903127734,4.78757310386213,336.134520794282));
#66028=CARTESIAN_POINT('Ctrl Pts',(27.5240290578473,4.8173306932602,336.000624549101));
#66029=CARTESIAN_POINT('Ctrl Pts',(27.5162678029211,4.84143197837612,335.865863419517));
#66030=CARTESIAN_POINT('Ctrl Pts',(27.5084941325164,4.86557181769364,335.730886716043));
#66031=CARTESIAN_POINT('Ctrl Pts',(27.5007204621117,4.88403721898356,335.595042750972));
#66032=CARTESIAN_POINT('Ctrl Pts',(27.4929467917071,4.8967992834685,335.458846205087));
#66033=CARTESIAN_POINT('Ctrl Pts',(27.48553498753,4.90896727078115,335.328989641181));
#66034=CARTESIAN_POINT('Ctrl Pts',(27.4781231833531,4.91595093713944,335.198812870405));
#66035=CARTESIAN_POINT('Ctrl Pts',(27.470711379176,4.91776932707573,335.068759786017));
#66036=CARTESIAN_POINT('Ctrl Pts',(27.4629363003976,4.91967684171952,334.932332412554));
#66037=CARTESIAN_POINT('Ctrl Pts',(27.4551612216192,4.91590597427971,334.795610020817));
#66038=CARTESIAN_POINT('Ctrl Pts',(27.4473861428407,4.90642163118969,334.659104356886));
#66039=CARTESIAN_POINT('Ctrl Pts',(27.4396206317917,4.89694895918766,334.522766671865));
#66040=CARTESIAN_POINT('Ctrl Pts',(27.4318551207428,4.881776827636,334.386645570204));
#66041=CARTESIAN_POINT('Ctrl Pts',(27.4240896096938,4.86092209781968,334.251254768677));
#66042=CARTESIAN_POINT('Ctrl Pts',(27.4163317981716,4.8400880455287,334.115998207525));
#66043=CARTESIAN_POINT('Ctrl Pts',(27.4085739866494,4.81358266669662,333.981470889346));
#66044=CARTESIAN_POINT('Ctrl Pts',(27.4008161751272,4.78147474107766,333.848183016736));
#66045=CARTESIAN_POINT('Ctrl Pts',(27.3930642016042,4.74939097769094,333.714995447476));
#66046=CARTESIAN_POINT('Ctrl Pts',(27.3853122280812,4.71171315061781,333.583045845723));
#66047=CARTESIAN_POINT('Ctrl Pts',(27.3775602545582,4.66856133276941,333.452835450034));
#66048=CARTESIAN_POINT('Ctrl Pts',(27.3698115640006,4.62542778974149,333.322680198526));
#66049=CARTESIAN_POINT('Ctrl Pts',(27.362062873443,4.57682498945489,333.194263058386));
#66050=CARTESIAN_POINT('Ctrl Pts',(27.3543141828854,4.52292313940507,333.068071083726));
#66051=CARTESIAN_POINT('Ctrl Pts',(27.3465671045076,4.46903250408535,332.941905364361));
#66052=CARTESIAN_POINT('Ctrl Pts',(27.3388200261297,4.40984516541813,332.817964248837));
#66053=CARTESIAN_POINT('Ctrl Pts',(27.3310729477519,4.34557970563935,332.696715370512));
#66054=CARTESIAN_POINT('Ctrl Pts',(27.3233258044461,4.28131370725411,332.575465476005));
#66055=CARTESIAN_POINT('Ctrl Pts',(27.3155786611403,4.21196968592095,332.456908209063));
#66056=CARTESIAN_POINT('Ctrl Pts',(27.3078315178345,4.13781227974334,332.341486768868));
#66057=CARTESIAN_POINT('Ctrl Pts',(27.3000826328064,4.06363820140642,332.226039379482));
#66058=CARTESIAN_POINT('Ctrl Pts',(27.2923337477783,3.98464879610733,332.1137295485));
#66059=CARTESIAN_POINT('Ctrl Pts',(27.2845848627502,3.90115190737911,332.004971309311));
#66060=CARTESIAN_POINT('Ctrl Pts',(27.2768277529754,3.81756639419051,331.896097633002));
#66061=CARTESIAN_POINT('Ctrl Pts',(27.2690706432008,3.72946407890935,331.790783389338));
#66062=CARTESIAN_POINT('Ctrl Pts',(27.261313533426,3.63719332134686,331.689409749659));
#66063=CARTESIAN_POINT('Ctrl Pts',(27.2535522784999,3.5448732572417,331.587981939149));
#66064=CARTESIAN_POINT('Ctrl Pts',(27.2457910235737,3.44838058723222,331.490499206142));
#66065=CARTESIAN_POINT('Ctrl Pts',(27.2380297686475,3.34809966666967,331.397304941499));
#66066=CARTESIAN_POINT('Ctrl Pts',(27.2302560982428,3.24765832931582,331.303961596405));
#66067=CARTESIAN_POINT('Ctrl Pts',(27.2224824278382,3.14341692916654,331.214920682293));
#66068=CARTESIAN_POINT('Ctrl Pts',(27.2147087574336,3.03579263348591,331.130485024067));
#66069=CARTESIAN_POINT('Ctrl Pts',(27.2072969532564,2.93317827466126,331.049979866044));
#66070=CARTESIAN_POINT('Ctrl Pts',(27.1998851490793,2.82748911350364,330.973661031803));
#66071=CARTESIAN_POINT('Ctrl Pts',(27.1924733449022,2.71910873541287,330.901752722504));
#66072=CARTESIAN_POINT('Ctrl Pts',(27.1846982661237,2.60541631214426,330.826319972763));
#66073=CARTESIAN_POINT('Ctrl Pts',(27.1769231873453,2.48840290334483,330.755502644344));
#66074=CARTESIAN_POINT('Ctrl Pts',(27.1691481085668,2.368479856067,330.689607183341));
#66075=CARTESIAN_POINT('Ctrl Pts',(27.1613825975178,2.24870438173336,330.623792810898));
#66076=CARTESIAN_POINT('Ctrl Pts',(27.1536170864689,2.12602673237098,330.562888441267));
#66077=CARTESIAN_POINT('Ctrl Pts',(27.1458515754198,2.00088802798299,330.507157897057));
#66078=CARTESIAN_POINT('Ctrl Pts',(27.1380937638976,1.87587339898483,330.451482609844));
#66079=CARTESIAN_POINT('Ctrl Pts',(27.1303359523754,1.74840292574922,330.400971097329));
#66080=CARTESIAN_POINT('Ctrl Pts',(27.1225781408532,1.61894286919439,330.355841621049));
#66081=CARTESIAN_POINT('Ctrl Pts',(27.1148261673302,1.4895802354377,330.31074610613));
#66082=CARTESIAN_POINT('Ctrl Pts',(27.1070741938072,1.35823136611897,330.271024693962));
#66083=CARTESIAN_POINT('Ctrl Pts',(27.0993222202842,1.22538274177925,330.236847661616));
#66084=CARTESIAN_POINT('Ctrl Pts',(27.0915735297266,1.09259037891063,330.202685103264));
#66085=CARTESIAN_POINT('Ctrl Pts',(27.083824839169,0.958299902044125,330.174062351817));
#66086=CARTESIAN_POINT('Ctrl Pts',(27.0760761486113,0.823012994415282,330.151099849087));
#66087=CARTESIAN_POINT('Ctrl Pts',(27.0683290702335,0.687754234357693,330.128142123898));
#66088=CARTESIAN_POINT('Ctrl Pts',(27.0605819918557,0.551499841024263,330.11084237034));
#66089=CARTESIAN_POINT('Ctrl Pts',(27.0528349134779,0.414761344671912,330.09926984119));
#66090=CARTESIAN_POINT('Ctrl Pts',(27.0450877701721,0.278021702319259,330.087697215052));
#66091=CARTESIAN_POINT('Ctrl Pts',(27.0373406268663,0.14079833833711,330.081851942024));
#66092=CARTESIAN_POINT('Ctrl Pts',(27.0295934835605,0.0036071592346469,
330.081751322788));
#66093=CARTESIAN_POINT('Ctrl Pts',(27.0218445985324,-0.13361486335753,330.081650680929));
#66094=CARTESIAN_POINT('Ctrl Pts',(27.0140957135042,-0.270804295873701,
330.087297263129));
#66095=CARTESIAN_POINT('Ctrl Pts',(27.0063468284761,-0.407446377004991,
330.098656254417));
#66096=CARTESIAN_POINT('Ctrl Pts',(26.9985897187014,-0.54423349145297,330.110027302255));
#66097=CARTESIAN_POINT('Ctrl Pts',(26.9908326089267,-0.680471703839216,
330.127122838579));
#66098=CARTESIAN_POINT('Ctrl Pts',(26.983075499152,-0.815651961568826,330.149856193875));
#66099=CARTESIAN_POINT('Ctrl Pts',(26.9753142442258,-0.950904455305848,
330.17260169715));
#66100=CARTESIAN_POINT('Ctrl Pts',(26.9675529892997,-1.0850974856846,330.200990941553));
#66101=CARTESIAN_POINT('Ctrl Pts',(26.9597917343736,-1.2177342912693,330.23488654297));
#66102=CARTESIAN_POINT('Ctrl Pts',(26.9520180639689,-1.3505832725167,330.268836366303));
#66103=CARTESIAN_POINT('Ctrl Pts',(26.9442443935642,-1.48187067978886,330.308310035788));
#66104=CARTESIAN_POINT('Ctrl Pts',(26.9364707231596,-1.61111610802111,330.353120622506));
#66105=CARTESIAN_POINT('Ctrl Pts',(26.9290589189825,-1.73434513047501,330.395845265632));
#66106=CARTESIAN_POINT('Ctrl Pts',(26.9216471148053,-1.85571773592336,330.443421035647));
#66107=CARTESIAN_POINT('Ctrl Pts',(26.9142353106282,-1.9748378087586,330.495646695518));
#66108=CARTESIAN_POINT('Ctrl Pts',(26.9064602318498,-2.09979631120362,330.550432090551));
#66109=CARTESIAN_POINT('Ctrl Pts',(26.8986851530714,-2.2226707832227,330.610507842477));
#66110=CARTESIAN_POINT('Ctrl Pts',(26.8909100742929,-2.34298092426293,330.67569387635));
#66111=CARTESIAN_POINT('Ctrl Pts',(26.8831445632439,-2.4631430160153,330.740799694658));
#66112=CARTESIAN_POINT('Ctrl Pts',(26.8753790521949,-2.58074671508766,330.81100309812));
#66113=CARTESIAN_POINT('Ctrl Pts',(26.8676135411459,-2.69533145207467,330.886075909067));
#66114=CARTESIAN_POINT('Ctrl Pts',(26.8598557296237,-2.80980257796128,330.961074285104));
#66115=CARTESIAN_POINT('Ctrl Pts',(26.8520979181015,-2.92126037377313,331.040932247739));
#66116=CARTESIAN_POINT('Ctrl Pts',(26.8443401065793,-3.0292689781907,331.125375822061));
#66117=CARTESIAN_POINT('Ctrl Pts',(26.8365881330563,-3.13719630270815,331.209755849915));
#66118=CARTESIAN_POINT('Ctrl Pts',(26.8288361595333,-3.24167929560479,331.298714380992));
#66119=CARTESIAN_POINT('Ctrl Pts',(26.8210841860103,-3.34231150472172,331.39193447012));
#66120=CARTESIAN_POINT('Ctrl Pts',(26.8133354954527,-3.44290109603848,331.485115080486));
#66121=CARTESIAN_POINT('Ctrl Pts',(26.8055868048951,-3.53964286098858,331.582553394263));
#66122=CARTESIAN_POINT('Ctrl Pts',(26.7978381143375,-3.63216402789683,331.683892713293));
#66123=CARTESIAN_POINT('Ctrl Pts',(26.7900910359596,-3.72466594500342,331.78521094783));
#66124=CARTESIAN_POINT('Ctrl Pts',(26.7823439575818,-3.81294874735247,331.890428284735));
#66125=CARTESIAN_POINT('Ctrl Pts',(26.774596879204,-3.89667738043269,331.999152043951));
#66126=CARTESIAN_POINT('Ctrl Pts',(26.7668497358982,-3.98040671523949,332.107876714377));
#66127=CARTESIAN_POINT('Ctrl Pts',(26.7591025925923,-4.0595815661577,332.220107556045));
#66128=CARTESIAN_POINT('Ctrl Pts',(26.7513554492865,-4.13390819806113,332.335420094555));
#66129=CARTESIAN_POINT('Ctrl Pts',(26.7436065642584,-4.20825154016942,332.450758557772));
#66130=CARTESIAN_POINT('Ctrl Pts',(26.7358576792304,-4.27774428259524,332.569179768012));
#66131=CARTESIAN_POINT('Ctrl Pts',(26.7281087942023,-4.34213713510919,332.690232011131));
#66132=CARTESIAN_POINT('Ctrl Pts',(26.7203516844276,-4.4065983348621,332.811412740351));
#66133=CARTESIAN_POINT('Ctrl Pts',(26.7125945746528,-4.46594864771926,332.935229735308));
#66134=CARTESIAN_POINT('Ctrl Pts',(26.7048374648781,-4.51998547835482,333.061208020967));
#66135=CARTESIAN_POINT('Ctrl Pts',(26.697076209952,-4.57405118454495,333.187253625395));
#66136=CARTESIAN_POINT('Ctrl Pts',(26.6893149550258,-4.62279761200044,333.315462456644));
#66137=CARTESIAN_POINT('Ctrl Pts',(26.6815537000996,-4.66607146383841,333.445342430999));
#66138=CARTESIAN_POINT('Ctrl Pts',(26.673780029695,-4.7094145397364,333.575430170984));
#66139=CARTESIAN_POINT('Ctrl Pts',(26.6660063592904,-4.74726743827675,333.707194020211));
#66140=CARTESIAN_POINT('Ctrl Pts',(26.6582326888857,-4.77952737723128,333.840128837846));
#66141=CARTESIAN_POINT('Ctrl Pts',(26.6508208847086,-4.81028560826618,333.966875507738));
#66142=CARTESIAN_POINT('Ctrl Pts',(26.6434090805315,-4.8359598094424,334.094686300082));
#66143=CARTESIAN_POINT('Ctrl Pts',(26.6359972763544,-4.85650484439102,334.223119211908));
#66144=CARTESIAN_POINT('Ctrl Pts',(26.6232769885537,-4.89176464769647,334.443538365258));
#66145=CARTESIAN_POINT('Ctrl Pts',(26.6105567007529,-4.91202471847816,334.666418079846));
#66146=CARTESIAN_POINT('Ctrl Pts',(26.5978364129523,-4.91702307292733,334.890149361402));
#66147=CARTESIAN_POINT('Ctrl Pts',(26.5958300674711,-4.91781145334917,334.925438047694));
#66148=CARTESIAN_POINT('Ctrl Pts',(26.5938237219899,-4.91822022182113,334.960747840938));
#66149=CARTESIAN_POINT('Ctrl Pts',(26.5918173765088,-4.91824843169319,334.996072322894));
#66150=CARTESIAN_POINT('',(24.8418173765385,-4.918249805682,334.998617462852));
#66151=CARTESIAN_POINT('Ctrl Pts',(26.59181737648,-4.9182484316936,334.996072323402));
#66152=CARTESIAN_POINT('Ctrl Pts',(26.5841678104404,-4.91835598707401,335.130753493758));
#66153=CARTESIAN_POINT('Ctrl Pts',(26.5765182444006,-4.91292722848413,335.265637886173));
#66154=CARTESIAN_POINT('Ctrl Pts',(26.5688686783609,-4.90193871815958,335.400224769234));
#66155=CARTESIAN_POINT('Ctrl Pts',(26.5612265307403,-4.89096086430546,335.534681132224));
#66156=CARTESIAN_POINT('Ctrl Pts',(26.5535843831196,-4.8744340150351,335.668840160233));
#66157=CARTESIAN_POINT('Ctrl Pts',(26.545942235499,-4.85238677358813,335.802200512345));
#66158=CARTESIAN_POINT('Ctrl Pts',(26.5381012774399,-4.82976597324687,335.939030233462));
#66159=CARTESIAN_POINT('Ctrl Pts',(26.5302603193808,-4.80133360103861,336.075018722663));
#66160=CARTESIAN_POINT('Ctrl Pts',(26.5224193613217,-4.76717746666161,336.209628895097));
#66161=CARTESIAN_POINT('Ctrl Pts',(26.5147854354675,-4.73392318888911,336.340684828293));
#66162=CARTESIAN_POINT('Ctrl Pts',(26.5071515096133,-4.69524372704886,336.470433902881));
#66163=CARTESIAN_POINT('Ctrl Pts',(26.4995175837591,-4.65127190295312,336.598390674178));
#66164=CARTESIAN_POINT('Ctrl Pts',(26.4918847006607,-4.6073060851869,336.726329967224));
#66165=CARTESIAN_POINT('Ctrl Pts',(26.4842518175623,-4.55804947356832,336.852477062175));
#66166=CARTESIAN_POINT('Ctrl Pts',(26.4766189344639,-4.50368444236786,336.976362695983));
#66167=CARTESIAN_POINT('Ctrl Pts',(26.4689853277714,-4.44931425738553,337.100260074097));
#66168=CARTESIAN_POINT('Ctrl Pts',(26.4613517210788,-4.38983485245253,337.221895195404));
#66169=CARTESIAN_POINT('Ctrl Pts',(26.4537181143863,-4.32547609201762,337.340820292095));
#66170=CARTESIAN_POINT('Ctrl Pts',(26.4457215416942,-4.25805717368356,337.465400090206));
#66171=CARTESIAN_POINT('Ctrl Pts',(26.4377249690021,-4.18528371274943,337.587005379117));
#66172=CARTESIAN_POINT('Ctrl Pts',(26.42972839631,-4.10747234174323,337.705153234905));
#66173=CARTESIAN_POINT('Ctrl Pts',(26.4220838676935,-4.03308656733136,337.818099705764));
#66174=CARTESIAN_POINT('Ctrl Pts',(26.4144393390768,-3.95409729883626,337.927886382928));
#66175=CARTESIAN_POINT('Ctrl Pts',(26.4067948104603,-3.87082327377047,338.034124296356));
#66176=CARTESIAN_POINT('Ctrl Pts',(26.3991452178191,-3.78749408484368,338.140432585792));
#66177=CARTESIAN_POINT('Ctrl Pts',(26.3914956251781,-3.69987475117922,338.243187127118));
#66178=CARTESIAN_POINT('Ctrl Pts',(26.3838460325369,-3.60832169700361,338.342034947967));
#66179=CARTESIAN_POINT('Ctrl Pts',(26.3761860433955,-3.51664421380359,338.4410171121));
#66180=CARTESIAN_POINT('Ctrl Pts',(26.3685260542541,-3.42102263016184,338.53608168211));
#66181=CARTESIAN_POINT('Ctrl Pts',(26.3608660651128,-3.32184738413784,338.626915082959));
#66182=CARTESIAN_POINT('Ctrl Pts',(26.3598304574353,-3.30843918677643,338.639195487742));
#66183=CARTESIAN_POINT('Ctrl Pts',(26.3587948497579,-3.29496607903849,338.651398618376));
#66184=CARTESIAN_POINT('Ctrl Pts',(26.3577592420804,-3.28142906622022,338.663523760789));
#66185=CARTESIAN_POINT('Ctrl Pts',(26.349984163302,-3.17979662047846,338.754556242985));
#66186=CARTESIAN_POINT('Ctrl Pts',(26.3422090845236,-3.0742126093444,338.841500181452));
#66187=CARTESIAN_POINT('Ctrl Pts',(26.3344340057451,-2.96503991377297,338.923993039269));
#66188=CARTESIAN_POINT('Ctrl Pts',(26.3266684946961,-2.85600156215402,339.006384384373));
#66189=CARTESIAN_POINT('Ctrl Pts',(26.3189029836472,-2.743383621755,339.084335313767));
#66190=CARTESIAN_POINT('Ctrl Pts',(26.3111374725982,-2.62758457925691,339.157521177499));
#66191=CARTESIAN_POINT('Ctrl Pts',(26.303379661076,-2.51190035184619,339.230634477234));
#66192=CARTESIAN_POINT('Ctrl Pts',(26.2956218495538,-2.39304162740545,339.298991906003));
#66193=CARTESIAN_POINT('Ctrl Pts',(26.2878640380316,-2.27143833809454,339.362310275386));
#66194=CARTESIAN_POINT('Ctrl Pts',(26.2801120645086,-2.14992655911526,339.425580995687));
#66195=CARTESIAN_POINT('Ctrl Pts',(26.2723600909856,-2.02567467158345,339.483820024704));
#66196=CARTESIAN_POINT('Ctrl Pts',(26.2646081174626,-1.89913953253943,339.536788742982));
#66197=CARTESIAN_POINT('Ctrl Pts',(26.256859426905,-1.77265798120192,339.589735028976));
#66198=CARTESIAN_POINT('Ctrl Pts',(26.2491107363474,-1.64389546137183,339.637415292864));
#66199=CARTESIAN_POINT('Ctrl Pts',(26.2413620457898,-1.51333105720149,339.67963803876));
#66200=CARTESIAN_POINT('Ctrl Pts',(26.233614967412,-1.38279381804611,339.721851999861));
#66201=CARTESIAN_POINT('Ctrl Pts',(26.2258678890341,-1.25045581192459,339.758610581329));
#66202=CARTESIAN_POINT('Ctrl Pts',(26.2181208106562,-1.11681324548536,339.789771522443));
#66203=CARTESIAN_POINT('Ctrl Pts',(26.2103736673504,-0.983169558992532,
339.820932724716));
#66204=CARTESIAN_POINT('Ctrl Pts',(26.2026265240447,-0.848221671037918,
339.846496104304));
#66205=CARTESIAN_POINT('Ctrl Pts',(26.1948793807389,-0.71247760711148,339.866370179288));
#66206=CARTESIAN_POINT('Ctrl Pts',(26.1871304957108,-0.576703025037542,
339.886248722387));
#66207=CARTESIAN_POINT('Ctrl Pts',(26.1793816106827,-0.440132297482836,
339.90043535905));
#66208=CARTESIAN_POINT('Ctrl Pts',(26.1716327256546,-0.303279828558278,
339.908890343865));
#66209=CARTESIAN_POINT('Ctrl Pts',(26.1638756158799,-0.16628210300944,339.917354302888));
#66210=CARTESIAN_POINT('Ctrl Pts',(26.1561185061052,-0.0290024294705457,
339.920074433289));
#66211=CARTESIAN_POINT('Ctrl Pts',(26.1483613963305,0.108042962821708,339.917063125554));
#66212=CARTESIAN_POINT('Ctrl Pts',(26.1406001414043,0.245161587789647,339.914050208672));
#66213=CARTESIAN_POINT('Ctrl Pts',(26.1328388864781,0.382045292173611,339.905299775877));
#66214=CARTESIAN_POINT('Ctrl Pts',(26.125077631552,0.518182699628412,339.890876174297));
#66215=CARTESIAN_POINT('Ctrl Pts',(26.1173039611473,0.65453788256825,339.876429499655));
#66216=CARTESIAN_POINT('Ctrl Pts',(26.1095302907427,0.790143996111655,339.856291578696));
#66217=CARTESIAN_POINT('Ctrl Pts',(26.1017566203381,0.92449870817882,339.830578143564));
#66218=CARTESIAN_POINT('Ctrl Pts',(26.0943448161609,1.0525991760772,339.806061675023));
#66219=CARTESIAN_POINT('Ctrl Pts',(26.0869330119837,1.17956184580616,339.776477156411));
#66220=CARTESIAN_POINT('Ctrl Pts',(26.0795212078065,1.30496573220709,339.741966627916));
#66221=CARTESIAN_POINT('Ctrl Pts',(26.0717461290281,1.43651603663802,339.705764635617));
#66222=CARTESIAN_POINT('Ctrl Pts',(26.0639710502496,1.56676661619699,339.664027142065));
#66223=CARTESIAN_POINT('Ctrl Pts',(26.0561959714712,1.69521623014514,339.616863112066));
#66224=CARTESIAN_POINT('Ctrl Pts',(26.0484304604222,1.82350777866566,339.569757120408));
#66225=CARTESIAN_POINT('Ctrl Pts',(26.0406649493732,1.9500024077694,339.517238012446));
#66226=CARTESIAN_POINT('Ctrl Pts',(26.0328994383241,2.07421146837759,339.459465197414));
#66227=CARTESIAN_POINT('Ctrl Pts',(26.0251416268019,2.19829737534065,339.401749664297));
#66228=CARTESIAN_POINT('Ctrl Pts',(26.0173838152797,2.32010187144078,339.33879095423));
#66229=CARTESIAN_POINT('Ctrl Pts',(26.0096260037575,2.43915415653436,339.270797356836));
#66230=CARTESIAN_POINT('Ctrl Pts',(26.0018740302345,2.55811685100805,339.202854926781));
#66231=CARTESIAN_POINT('Ctrl Pts',(25.9941220567115,2.67433111889856,339.129885344113));
#66232=CARTESIAN_POINT('Ctrl Pts',(25.9863700831884,2.78734906845822,339.052143658987));
#66233=CARTESIAN_POINT('Ctrl Pts',(25.9786213926308,2.90031915484929,338.97443489751));
#66234=CARTESIAN_POINT('Ctrl Pts',(25.9708727020732,3.01009529383858,338.891958274239));
#66235=CARTESIAN_POINT('Ctrl Pts',(25.9631240115155,3.11625719252611,338.805013031848));
#66236=CARTESIAN_POINT('Ctrl Pts',(25.9553769331377,3.22239700334379,338.71808587914));
#66237=CARTESIAN_POINT('Ctrl Pts',(25.9476298547598,3.32492376737622,338.626692204124));
#66238=CARTESIAN_POINT('Ctrl Pts',(25.939882776382,3.42344932865777,338.531172292117));
#66239=CARTESIAN_POINT('Ctrl Pts',(25.9321356330762,3.52197571567815,338.435651579561));
#66240=CARTESIAN_POINT('Ctrl Pts',(25.9243884897704,3.61650055242442,338.336004833114));
#66241=CARTESIAN_POINT('Ctrl Pts',(25.9166413464646,3.70667198805692,338.232609756134));
#66242=CARTESIAN_POINT('Ctrl Pts',(25.9088924614365,3.79686369614267,338.129191433746));
#66243=CARTESIAN_POINT('Ctrl Pts',(25.9011435764084,3.88269979867831,338.022023398464));
#66244=CARTESIAN_POINT('Ctrl Pts',(25.8933946913803,3.96386849931601,337.911516715156));
#66245=CARTESIAN_POINT('Ctrl Pts',(25.8856375816055,4.04512335325131,337.800892738912));
#66246=CARTESIAN_POINT('Ctrl Pts',(25.8778804718308,4.12170067739567,337.686923351341));
#66247=CARTESIAN_POINT('Ctrl Pts',(25.870123362056,4.19333152991012,337.570049365822));
#66248=CARTESIAN_POINT('Ctrl Pts',(25.8623621071299,4.2650006596618,337.453112926582));
#66249=CARTESIAN_POINT('Ctrl Pts',(25.8546008522037,4.33171786086935,337.333269137994));
#66250=CARTESIAN_POINT('Ctrl Pts',(25.8468395972775,4.39326050932327,337.21098284926));
#66251=CARTESIAN_POINT('Ctrl Pts',(25.8390659268729,4.45490160595802,337.088500942316));
#66252=CARTESIAN_POINT('Ctrl Pts',(25.8312922564681,4.51135144771493,336.963569083863));
#66253=CARTESIAN_POINT('Ctrl Pts',(25.8235185860635,4.56243551551167,336.836672324966));
#66254=CARTESIAN_POINT('Ctrl Pts',(25.8161067818864,4.61114160766195,336.715682640727));
#66255=CARTESIAN_POINT('Ctrl Pts',(25.8086949777095,4.65497014050902,336.592907142545));
#66256=CARTESIAN_POINT('Ctrl Pts',(25.8012831735325,4.69381273945129,336.468776711915));
#66257=CARTESIAN_POINT('Ctrl Pts',(25.793508094754,4.73455912987422,336.338562279114));
#66258=CARTESIAN_POINT('Ctrl Pts',(25.7857330159755,4.76994724349201,336.206445235331));
#66259=CARTESIAN_POINT('Ctrl Pts',(25.7779579371971,4.79979746100962,336.072906051705));
#66260=CARTESIAN_POINT('Ctrl Pts',(25.7701924261481,4.82961094593414,335.939531196547));
#66261=CARTESIAN_POINT('Ctrl Pts',(25.7624269150991,4.85390000967132,335.804738061425));
#66262=CARTESIAN_POINT('Ctrl Pts',(25.7546614040501,4.87253426679175,335.669023827259));
#66263=CARTESIAN_POINT('Ctrl Pts',(25.7469035925279,4.89115004799206,335.53344415415));
#66264=CARTESIAN_POINT('Ctrl Pts',(25.7391457810056,4.90412212751181,335.396945584207));
#66265=CARTESIAN_POINT('Ctrl Pts',(25.7313879694834,4.91137088356641,335.260036740781));
#66266=CARTESIAN_POINT('Ctrl Pts',(25.7236359959604,4.91861418470221,335.123230925601));
#66267=CARTESIAN_POINT('Ctrl Pts',(25.7158840224374,4.92014271462777,334.986015840234));
#66268=CARTESIAN_POINT('Ctrl Pts',(25.7081320489144,4.91592857053402,334.848906148678));
#66269=CARTESIAN_POINT('Ctrl Pts',(25.7003833583567,4.91171621113282,334.711854523158));
#66270=CARTESIAN_POINT('Ctrl Pts',(25.6926346677991,4.9017660268235,334.574908592552));
#66271=CARTESIAN_POINT('Ctrl Pts',(25.6848859772415,4.88610221254926,334.438583727506));
#66272=CARTESIAN_POINT('Ctrl Pts',(25.6771388988636,4.87044165726236,334.302287225986));
#66273=CARTESIAN_POINT('Ctrl Pts',(25.6693918204858,4.84906988114515,334.16661192108));
#66274=CARTESIAN_POINT('Ctrl Pts',(25.6616447421079,4.82206298391527,334.032068369329));
#66275=CARTESIAN_POINT('Ctrl Pts',(25.6538975988021,4.79505586034164,333.897523689973));
#66276=CARTESIAN_POINT('Ctrl Pts',(25.6461504554963,4.76241359838175,333.764111165923));
#66277=CARTESIAN_POINT('Ctrl Pts',(25.6384033121905,4.72426341016851,333.632331073014));
#66278=CARTESIAN_POINT('Ctrl Pts',(25.6306544271624,4.686104644983,333.500521353142));
#66279=CARTESIAN_POINT('Ctrl Pts',(25.6229055421343,4.64243559814119,333.370345170096));
#66280=CARTESIAN_POINT('Ctrl Pts',(25.6151566571062,4.59343321196466,333.242287170861));
#66281=CARTESIAN_POINT('Ctrl Pts',(25.6073995473314,4.54437881414915,333.114093249543));
#66282=CARTESIAN_POINT('Ctrl Pts',(25.5996424375567,4.48997990881064,332.988022368787));
#66283=CARTESIAN_POINT('Ctrl Pts',(25.591885327782,4.43046164546393,332.864539236939));
#66284=CARTESIAN_POINT('Ctrl Pts',(25.5841240728558,4.37091157746035,332.740990119653));
#66285=CARTESIAN_POINT('Ctrl Pts',(25.5763628179296,4.3062368846871,332.620031851169));
#66286=CARTESIAN_POINT('Ctrl Pts',(25.5686015630035,4.23670799402151,332.502103197509));
#66287=CARTESIAN_POINT('Ctrl Pts',(25.5608278925988,4.16706787979026,332.383985896437));
#66288=CARTESIAN_POINT('Ctrl Pts',(25.5530542221941,4.09255826317837,332.268908223001));
#66289=CARTESIAN_POINT('Ctrl Pts',(25.5452805517895,4.01349259168696,332.157279422987));
#66290=CARTESIAN_POINT('Ctrl Pts',(25.5378687476125,3.93810744622676,332.050846970471));
#66291=CARTESIAN_POINT('Ctrl Pts',(25.5304569434356,3.85858104450949,331.947549755237));
#66292=CARTESIAN_POINT('Ctrl Pts',(25.5230451392586,3.7752170762628,331.847712086501));
#66293=CARTESIAN_POINT('Ctrl Pts',(25.5152700604802,3.68776719160269,331.742981076217));
#66294=CARTESIAN_POINT('Ctrl Pts',(25.5074949817018,3.59581768974033,331.641726343238));
#66295=CARTESIAN_POINT('Ctrl Pts',(25.4997199029233,3.49967540680038,331.544358943765));
#66296=CARTESIAN_POINT('Ctrl Pts',(25.4919543918744,3.40365143306044,331.447111361076));
#66297=CARTESIAN_POINT('Ctrl Pts',(25.4841888808254,3.30344521614591,331.353741869352));
#66298=CARTESIAN_POINT('Ctrl Pts',(25.4764233697764,3.19940428706081,331.264629165607));
#66299=CARTESIAN_POINT('Ctrl Pts',(25.4686655582543,3.09546651486001,331.175604817367));
#66300=CARTESIAN_POINT('Ctrl Pts',(25.460907746732,2.98770189189243,331.090829110469));
#66301=CARTESIAN_POINT('Ctrl Pts',(25.4531499352099,2.876495042469,331.010644245852));
#66302=CARTESIAN_POINT('Ctrl Pts',(25.4453979616869,2.76537187972604,330.930519722889));
#66303=CARTESIAN_POINT('Ctrl Pts',(25.4376459881639,2.65081196233557,330.854979393372));
#66304=CARTESIAN_POINT('Ctrl Pts',(25.429894014641,2.53323298242315,330.784325235592));
#66305=CARTESIAN_POINT('Ctrl Pts',(25.4221453240834,2.41570379727869,330.71370099989));
#66306=CARTESIAN_POINT('Ctrl Pts',(25.4143966335258,2.29515842694781,330.647959021147));
#66307=CARTESIAN_POINT('Ctrl Pts',(25.4066479429682,2.1720433508746,330.587357849947));
#66308=CARTESIAN_POINT('Ctrl Pts',(25.3989008645903,2.04895388992109,330.526769287328));
#66309=CARTESIAN_POINT('Ctrl Pts',(25.3911537862125,1.9232961371507,330.471319577279));
#66310=CARTESIAN_POINT('Ctrl Pts',(25.3834067078347,1.79554061237672,330.421221017367));
#66311=CARTESIAN_POINT('Ctrl Pts',(25.3756595645289,1.6677840168884,330.37112203758));
#66312=CARTESIAN_POINT('Ctrl Pts',(25.3679124212231,1.53792997822426,330.326374440081));
#66313=CARTESIAN_POINT('Ctrl Pts',(25.3601652779173,1.40646803079301,330.287141977435));
#66314=CARTESIAN_POINT('Ctrl Pts',(25.3524163928893,1.27497652792514,330.247900694498));
#66315=CARTESIAN_POINT('Ctrl Pts',(25.3446675078612,1.14187677143915,330.214177125471));
#66316=CARTESIAN_POINT('Ctrl Pts',(25.3369186228331,1.00767206496916,330.186084746074));
#66317=CARTESIAN_POINT('Ctrl Pts',(25.3291615130584,0.873324912236947,330.157962549136));
#66318=CARTESIAN_POINT('Ctrl Pts',(25.3214044032837,0.737870849918725,330.135483561662));
#66319=CARTESIAN_POINT('Ctrl Pts',(25.313647293509,0.601822502496497,330.118709930972));
#66320=CARTESIAN_POINT('Ctrl Pts',(25.3058860385829,0.465701455187667,330.101927336991));
#66321=CARTESIAN_POINT('Ctrl Pts',(25.2981247836567,0.328985879395393,330.090856206257));
#66322=CARTESIAN_POINT('Ctrl Pts',(25.2903635287306,0.192191086329997,330.085506572511));
#66323=CARTESIAN_POINT('Ctrl Pts',(25.2825898583259,0.0551774661768272,
330.080148381094));
#66324=CARTESIAN_POINT('Ctrl Pts',(25.2748161879213,-0.0819152333988373,
330.080529975044));
#66325=CARTESIAN_POINT('Ctrl Pts',(25.2670425175166,-0.218573244457722,
330.086609236046));
#66326=CARTESIAN_POINT('Ctrl Pts',(25.2596307133393,-0.348869792228236,
330.092405505986));
#66327=CARTESIAN_POINT('Ctrl Pts',(25.252218909162,-0.478770923467465,330.103380903456));
#66328=CARTESIAN_POINT('Ctrl Pts',(25.2448071049847,-0.607839575699074,
330.11945555161));
#66329=CARTESIAN_POINT('Ctrl Pts',(25.2370320262062,-0.743234267048079,
330.136318066153));
#66330=CARTESIAN_POINT('Ctrl Pts',(25.2292569474278,-0.878140683704208,
330.158845617916));
#66331=CARTESIAN_POINT('Ctrl Pts',(25.2214818686493,-1.01204711310582,330.187002627951));
#66332=CARTESIAN_POINT('Ctrl Pts',(25.2137163576003,-1.14578876212116,330.215124988992));
#66333=CARTESIAN_POINT('Ctrl Pts',(25.2059508465513,-1.27853249346685,330.24886294509));
#66334=CARTESIAN_POINT('Ctrl Pts',(25.1981853355023,-1.40977178377825,330.288129184691));
#66335=CARTESIAN_POINT('Ctrl Pts',(25.1904275239801,-1.54088094995148,330.327356491701));
#66336=CARTESIAN_POINT('Ctrl Pts',(25.1826697124578,-1.67048827151333,330.372101062781));
#66337=CARTESIAN_POINT('Ctrl Pts',(25.1749119009356,-1.79809784211041,330.422224643705));
#66338=CARTESIAN_POINT('Ctrl Pts',(25.1671599274126,-1.92561138245871,330.472310505045));
#66339=CARTESIAN_POINT('Ctrl Pts',(25.1594079538895,-2.05112980187823,330.527767176804));
#66340=CARTESIAN_POINT('Ctrl Pts',(25.1516559803665,-2.17417312320725,330.58840683054));
#66341=CARTESIAN_POINT('Ctrl Pts',(25.1439072898089,-2.29716433561631,330.649020803348));
#66342=CARTESIAN_POINT('Ctrl Pts',(25.1361585992513,-2.41768218486336,330.71481322001));
#66343=CARTESIAN_POINT('Ctrl Pts',(25.1284099086937,-2.53526763459921,330.785548542995));
#66344=CARTESIAN_POINT('Ctrl Pts',(25.1206628303159,-2.65282861970047,330.856269148905));
#66345=CARTESIAN_POINT('Ctrl Pts',(25.112915751938,-2.76745808411275,330.93193041419));
#66346=CARTESIAN_POINT('Ctrl Pts',(25.1051686735602,-2.87872287701492,331.012251555094));
#66347=CARTESIAN_POINT('Ctrl Pts',(25.0974215302544,-2.98998860242262,331.092573369166));
#66348=CARTESIAN_POINT('Ctrl Pts',(25.0896743869486,-3.09788928315148,331.17755490797));
#66349=CARTESIAN_POINT('Ctrl Pts',(25.0819272436428,-3.20202230101834,331.266873127487));
#66350=CARTESIAN_POINT('Ctrl Pts',(25.0741783586147,-3.30617873019913,331.356211427636));
#66351=CARTESIAN_POINT('Ctrl Pts',(25.0664294735865,-3.40656551435227,331.449888094166));
#66352=CARTESIAN_POINT('Ctrl Pts',(25.0586805885584,-3.50281486284738,331.547541296537));
#66353=CARTESIAN_POINT('Ctrl Pts',(25.0509234787837,-3.59916637139516,331.645298149026));
#66354=CARTESIAN_POINT('Ctrl Pts',(25.0431663690089,-3.69137139700285,331.74703968985));
#66355=CARTESIAN_POINT('Ctrl Pts',(25.0354092592342,-3.77910026814199,331.852368473625));
#66356=CARTESIAN_POINT('Ctrl Pts',(25.027648004308,-3.8668760187849,331.957753541735));
#66357=CARTESIAN_POINT('Ctrl Pts',(25.0198867493818,-3.95017061161098,332.066729362017));
#66358=CARTESIAN_POINT('Ctrl Pts',(25.0121254944557,-4.02869674456863,332.178868028113));
#66359=CARTESIAN_POINT('Ctrl Pts',(25.004351824051,-4.10734849374729,332.29118607953));
#66360=CARTESIAN_POINT('Ctrl Pts',(24.9965781536464,-4.18121632937148,332.40667675773));
#66361=CARTESIAN_POINT('Ctrl Pts',(24.9888044832417,-4.25005764031842,332.524885231657));
#66362=CARTESIAN_POINT('Ctrl Pts',(24.9813926790647,-4.31569437167778,332.637591072682));
#66363=CARTESIAN_POINT('Ctrl Pts',(24.9739808748877,-4.3767618816319,332.752767122594));
#66364=CARTESIAN_POINT('Ctrl Pts',(24.9665690707106,-4.43309082073933,332.870002620289));
#66365=CARTESIAN_POINT('Ctrl Pts',(24.9581780317219,-4.49686184233671,333.002727070171));
#66366=CARTESIAN_POINT('Ctrl Pts',(24.9497869927331,-4.55473719931768,333.138460421256));
#66367=CARTESIAN_POINT('Ctrl Pts',(24.9413959537443,-4.60644548241803,333.276676733747));
#66368=CARTESIAN_POINT('Ctrl Pts',(24.9330321278271,-4.65798606981271,333.414444795383));
#66369=CARTESIAN_POINT('Ctrl Pts',(24.9246683019098,-4.70339937041807,333.554679484578));
#66370=CARTESIAN_POINT('Ctrl Pts',(24.9163044759925,-4.74246172510439,333.696834681086));
#66371=CARTESIAN_POINT('Ctrl Pts',(24.9079570496449,-4.78144748735369,333.838711143426));
#66372=CARTESIAN_POINT('Ctrl Pts',(24.8996096232974,-4.81410704695216,333.982500326997));
#66373=CARTESIAN_POINT('Ctrl Pts',(24.8912621969498,-4.84026523280527,334.127637954404));
#66374=CARTESIAN_POINT('Ctrl Pts',(24.8829409241885,-4.86634146161674,334.272320846508));
#66375=CARTESIAN_POINT('Ctrl Pts',(24.8746196514271,-4.88595688602604,334.418343470128));
#66376=CARTESIAN_POINT('Ctrl Pts',(24.8662983786658,-4.89898671254474,334.565129613781));
#66377=CARTESIAN_POINT('Ctrl Pts',(24.8581380446233,-4.91176453391375,334.709076819859));
#66378=CARTESIAN_POINT('Ctrl Pts',(24.8499777105809,-4.91820908518151,334.853757996438));
#66379=CARTESIAN_POINT('Ctrl Pts',(24.8418173765385,-4.918249805682,334.998617462852));
#66380=CARTESIAN_POINT('',(23.0918173764689,-4.91824794611119,335.004494782867));
#66381=CARTESIAN_POINT('Ctrl Pts',(24.8418173765088,-4.91824980568215,334.998617463379));
#66382=CARTESIAN_POINT('Ctrl Pts',(24.8338553286311,-4.91828953670899,335.139957021433));
#66383=CARTESIAN_POINT('Ctrl Pts',(24.8258932807534,-4.91223224148295,335.281236635687));
#66384=CARTESIAN_POINT('Ctrl Pts',(24.8179312328757,-4.90011963284472,335.421913079093));
#66385=CARTESIAN_POINT('Ctrl Pts',(24.8099637414546,-4.88799874298139,335.562685701062));
#66386=CARTESIAN_POINT('Ctrl Pts',(24.8019962500334,-4.86981431778907,335.702853972241));
#66387=CARTESIAN_POINT('Ctrl Pts',(24.7940287586123,-4.8456597466068,335.841881632187));
#66388=CARTESIAN_POINT('Ctrl Pts',(24.7860545473129,-4.8214848031681,335.981026549737));
#66389=CARTESIAN_POINT('Ctrl Pts',(24.7780803360135,-4.79132973732307,336.11902858484));
#66390=CARTESIAN_POINT('Ctrl Pts',(24.7701061247141,-4.75533864122688,336.25536348113));
#66391=CARTESIAN_POINT('Ctrl Pts',(24.7621181777571,-4.71928555011239,336.391933215625));
#66392=CARTESIAN_POINT('Ctrl Pts',(24.7541302308,-4.67737643562674,336.526829726102));
#66393=CARTESIAN_POINT('Ctrl Pts',(24.7461422838429,-4.6298050529789,336.659544586298));
#66394=CARTESIAN_POINT('Ctrl Pts',(24.7381465940739,-4.58218755882447,336.792388088586));
#66395=CARTESIAN_POINT('Ctrl Pts',(24.7301509043049,-4.52889698612354,336.923045391491));
#66396=CARTESIAN_POINT('Ctrl Pts',(24.7221552145359,-4.47017434920947,337.051030070518));
#66397=CARTESIAN_POINT('Ctrl Pts',(24.7141449758748,-4.41134486106237,337.179247629428));
#66398=CARTESIAN_POINT('Ctrl Pts',(24.7061347372136,-4.34706372268284,337.304782528415));
#66399=CARTESIAN_POINT('Ctrl Pts',(24.6981244985525,-4.27761732016084,337.427173896687));
#66400=CARTESIAN_POINT('Ctrl Pts',(24.6948600111806,-4.24931517915742,337.477053194054));
#66401=CARTESIAN_POINT('Ctrl Pts',(24.6915955238087,-4.22015563878822,337.526410738232));
#66402=CARTESIAN_POINT('Ctrl Pts',(24.6883310364368,-4.1901600519002,337.575216845619));
#66403=CARTESIAN_POINT('Ctrl Pts',(24.6805559576583,-4.11871911049332,337.691459087224));
#66404=CARTESIAN_POINT('Ctrl Pts',(24.6727808788798,-4.04232447413337,337.804909919654));
#66405=CARTESIAN_POINT('Ctrl Pts',(24.6650058001013,-3.96122052587272,337.915118352298));
#66406=CARTESIAN_POINT('Ctrl Pts',(24.6572402890523,-3.88021638118385,338.02519116645));
#66407=CARTESIAN_POINT('Ctrl Pts',(24.6494747780032,-3.79451468465992,338.132029207925));
#66408=CARTESIAN_POINT('Ctrl Pts',(24.6417092669542,-3.70440475347745,338.2352076417));
#66409=CARTESIAN_POINT('Ctrl Pts',(24.6339514554319,-3.61438416655415,338.338283773757));
#66410=CARTESIAN_POINT('Ctrl Pts',(24.6261936439097,-3.51996429852614,338.43770722655));
#66411=CARTESIAN_POINT('Ctrl Pts',(24.6184358323875,-3.42147643301484,338.533083933453));
#66412=CARTESIAN_POINT('Ctrl Pts',(24.6106838588645,-3.32306268274556,338.62838886636));
#66413=CARTESIAN_POINT('Ctrl Pts',(24.6029318853415,-3.22058730801388,338.719652844082));
#66414=CARTESIAN_POINT('Ctrl Pts',(24.5951799118184,-3.11442011257202,338.806516836283));
#66415=CARTESIAN_POINT('Ctrl Pts',(24.5874312212608,-3.00829787900045,338.893344041532));
#66416=CARTESIAN_POINT('Ctrl Pts',(24.5796825307031,-2.89848723627722,338.975774720422));
#66417=CARTESIAN_POINT('Ctrl Pts',(24.5719338401454,-2.78539273445925,339.053488667472));
#66418=CARTESIAN_POINT('Ctrl Pts',(24.5641867617676,-2.67232176289697,339.131186445486));
#66419=CARTESIAN_POINT('Ctrl Pts',(24.5564396833898,-2.55596861318709,339.204169222417));
#66420=CARTESIAN_POINT('Ctrl Pts',(24.5486926050119,-2.43676829154808,339.27215909767));
#66421=CARTESIAN_POINT('Ctrl Pts',(24.5409454617061,-2.31756697089557,339.340149542744));
#66422=CARTESIAN_POINT('Ctrl Pts',(24.5331983184002,-2.19551877024599,339.403146809016));
#66423=CARTESIAN_POINT('Ctrl Pts',(24.5254511750944,-2.07108450904925,339.46091829323));
#66424=CARTESIAN_POINT('Ctrl Pts',(24.5177022900663,-1.94662227238861,339.518702765701));
#66425=CARTESIAN_POINT('Ctrl Pts',(24.5099534050381,-1.81977326218987,339.571258953695));
#66426=CARTESIAN_POINT('Ctrl Pts',(24.50220452001,-1.69101917016387,339.618402021115));
#66427=CARTESIAN_POINT('Ctrl Pts',(24.4944474102352,-1.56212841721432,339.665595126674));
#66428=CARTESIAN_POINT('Ctrl Pts',(24.4866903004605,-1.43132891077975,339.707363499794));
#66429=CARTESIAN_POINT('Ctrl Pts',(24.4789331906857,-1.29911896447607,339.743571753293));
#66430=CARTESIAN_POINT('Ctrl Pts',(24.4711719357595,-1.16683836940443,339.779799355325));
#66431=CARTESIAN_POINT('Ctrl Pts',(24.4634106808333,-1.03314621345038,339.810460830121));
#66432=CARTESIAN_POINT('Ctrl Pts',(24.4556494259071,-0.89855098046584,339.835471972621));
#66433=CARTESIAN_POINT('Ctrl Pts',(24.4478757555024,-0.76374043897319,339.860523124798));
#66434=CARTESIAN_POINT('Ctrl Pts',(24.4401020850977,-0.62802432080506,339.879905827409));
#66435=CARTESIAN_POINT('Ctrl Pts',(24.432328414693,-0.491917099767684,339.893587705299));
#66436=CARTESIAN_POINT('Ctrl Pts',(24.4249166105163,-0.362145702621913,
339.906632688482));
#66437=CARTESIAN_POINT('Ctrl Pts',(24.4175048063396,-0.232019082134269,
339.914495632242));
#66438=CARTESIAN_POINT('Ctrl Pts',(24.4100930021629,-0.101981250092211,
339.917192581863));
#66439=CARTESIAN_POINT('Ctrl Pts',(24.4023179233844,0.034430123467639,339.920021717019));
#66440=CARTESIAN_POINT('Ctrl Pts',(24.394542844606,0.171174870082267,339.917174592731));
#66441=CARTESIAN_POINT('Ctrl Pts',(24.3867677658275,0.307741492433349,339.908612659024));
#66442=CARTESIAN_POINT('Ctrl Pts',(24.3790022547785,0.444140060861186,339.900061261322));
#66443=CARTESIAN_POINT('Ctrl Pts',(24.3712367437296,0.580360554778097,339.885809070958));
#66444=CARTESIAN_POINT('Ctrl Pts',(24.3634712326806,0.71588915522387,339.865869478308));
#66445=CARTESIAN_POINT('Ctrl Pts',(24.3557134211583,0.851283378667813,339.845949655823));
#66446=CARTESIAN_POINT('Ctrl Pts',(24.3479556096361,0.98598668962775,339.820353709662));
#66447=CARTESIAN_POINT('Ctrl Pts',(24.3401977981139,1.1194884324956,339.789146971227));
#66448=CARTESIAN_POINT('Ctrl Pts',(24.3324458245909,1.25288971106872,339.757963716852));
#66449=CARTESIAN_POINT('Ctrl Pts',(24.3246938510679,1.38509084227026,339.721178163095));
#66450=CARTESIAN_POINT('Ctrl Pts',(24.3169418775448,1.51558978779994,339.678906993905));
#66451=CARTESIAN_POINT('Ctrl Pts',(24.3091931869872,1.64603346694818,339.636653726581));
#66452=CARTESIAN_POINT('Ctrl Pts',(24.3014444964296,1.77477602311863,339.588919584627));
#66453=CARTESIAN_POINT('Ctrl Pts',(24.293695805872,1.90132926344153,339.535871481257));
#66454=CARTESIAN_POINT('Ctrl Pts',(24.2859487274942,2.02785617330561,339.482834414988));
#66455=CARTESIAN_POINT('Ctrl Pts',(24.2782016491163,2.152194313096,339.424485737461));
#66456=CARTESIAN_POINT('Ctrl Pts',(24.2704545707385,2.27387458344803,339.361040866725));
#66457=CARTESIAN_POINT('Ctrl Pts',(24.2627074274327,2.39555587359792,339.297595464261));
#66458=CARTESIAN_POINT('Ctrl Pts',(24.2549602841269,2.51457890328879,339.229053964113));
#66459=CARTESIAN_POINT('Ctrl Pts',(24.2472131408211,2.63049869563477,339.155678004221));
#66460=CARTESIAN_POINT('Ctrl Pts',(24.239464255793,2.7464445492108,339.082285547855));
#66461=CARTESIAN_POINT('Ctrl Pts',(24.231715370765,2.85928544694446,339.004056677972));
#66462=CARTESIAN_POINT('Ctrl Pts',(24.2239664857369,2.96860528519365,338.92129643399));
#66463=CARTESIAN_POINT('Ctrl Pts',(24.2162093759622,3.07804115664909,338.838448347429));
#66464=CARTESIAN_POINT('Ctrl Pts',(24.2084522661874,3.18394819090044,338.751059515348));
#66465=CARTESIAN_POINT('Ctrl Pts',(24.2006951564127,3.28594287188699,338.659475714525));
#66466=CARTESIAN_POINT('Ctrl Pts',(24.1929339014865,3.38799205556984,338.567842974246));
#66467=CARTESIAN_POINT('Ctrl Pts',(24.1851726465604,3.48612444069997,338.472011071475));
#66468=CARTESIAN_POINT('Ctrl Pts',(24.1774113916343,3.57999404765856,338.372362032942));
#66469=CARTESIAN_POINT('Ctrl Pts',(24.1696377212296,3.67401381539625,338.272553588423));
#66470=CARTESIAN_POINT('Ctrl Pts',(24.1618640508249,3.76375692246318,338.168916101842));
#66471=CARTESIAN_POINT('Ctrl Pts',(24.1540903804203,3.84891773260542,338.061864685145));
#66472=CARTESIAN_POINT('Ctrl Pts',(24.1466785762431,3.93011428654773,337.959796537649));
#66473=CARTESIAN_POINT('Ctrl Pts',(24.139266772066,4.0071453847187,337.85462537639));
#66474=CARTESIAN_POINT('Ctrl Pts',(24.1318549678888,4.07978423968329,337.746733263375));
#66475=CARTESIAN_POINT('Ctrl Pts',(24.1240798891104,4.15598334130899,337.633553036509));
#66476=CARTESIAN_POINT('Ctrl Pts',(24.116304810332,4.22758956255946,337.517020719439));
#66477=CARTESIAN_POINT('Ctrl Pts',(24.1085297315536,4.29429368538976,337.397545579571));
#66478=CARTESIAN_POINT('Ctrl Pts',(24.1007642205046,4.36091572455051,337.278217461469));
#66479=CARTESIAN_POINT('Ctrl Pts',(24.0929987094556,4.42264747920467,337.155954064));
#66480=CARTESIAN_POINT('Ctrl Pts',(24.0852331984065,4.47922215268417,337.031194714793));
#66481=CARTESIAN_POINT('Ctrl Pts',(24.0774753868844,4.53574073221009,336.906559064844));
#66482=CARTESIAN_POINT('Ctrl Pts',(24.0697175753621,4.58711224585203,336.779432741726));
#66483=CARTESIAN_POINT('Ctrl Pts',(24.06195976384,4.63311528712954,336.650280521204));
#66484=CARTESIAN_POINT('Ctrl Pts',(24.0542077903169,4.6790837096597,336.521225491824));
#66485=CARTESIAN_POINT('Ctrl Pts',(24.046455816794,4.7196915705131,336.390147966317));
#66486=CARTESIAN_POINT('Ctrl Pts',(24.038703843271,4.75476530997945,336.257533263781));
#66487=CARTESIAN_POINT('Ctrl Pts',(24.0309551527133,4.78982419569626,336.12497472365));
#66488=CARTESIAN_POINT('Ctrl Pts',(24.0232064621557,4.81935352175403,335.990880678369));
#66489=CARTESIAN_POINT('Ctrl Pts',(24.0154577715981,4.84322945986104,335.855751986053));
#66490=CARTESIAN_POINT('Ctrl Pts',(24.0077106932203,4.8671004303797,335.720651408391));
#66491=CARTESIAN_POINT('Ctrl Pts',(23.9999636148425,4.88532028459383,335.584516996546));
#66492=CARTESIAN_POINT('Ctrl Pts',(23.9922165364647,4.89781631555561,335.447859801252));
#66493=CARTESIAN_POINT('Ctrl Pts',(23.9844693931589,4.91031245124615,335.311201460638));
#66494=CARTESIAN_POINT('Ctrl Pts',(23.976722249853,4.91708463240899,335.174020717086));
#66495=CARTESIAN_POINT('Ctrl Pts',(23.9689751065472,4.91811207344259,335.036833348452));
#66496=CARTESIAN_POINT('Ctrl Pts',(23.9612262215191,4.91913974546676,334.899615137185));
#66497=CARTESIAN_POINT('Ctrl Pts',(23.9534773364911,4.91442010441552,334.76239068866));
#66498=CARTESIAN_POINT('Ctrl Pts',(23.945728451463,4.90398448688619,334.625674987638));
#66499=CARTESIAN_POINT('Ctrl Pts',(23.9379713416883,4.89353779288461,334.488814175159));
#66500=CARTESIAN_POINT('Ctrl Pts',(23.9302142319135,4.87736303280648,334.352463579221));
#66501=CARTESIAN_POINT('Ctrl Pts',(23.9224571221388,4.85554343517451,334.217132826315));
#66502=CARTESIAN_POINT('Ctrl Pts',(23.9146958672126,4.8337121778472,334.081729756982));
#66503=CARTESIAN_POINT('Ctrl Pts',(23.9069346122864,4.80623015075202,333.94734799934));
#66504=CARTESIAN_POINT('Ctrl Pts',(23.8991733573603,4.77323137889276,333.814485231617));
#66505=CARTESIAN_POINT('Ctrl Pts',(23.8913996869556,4.74017981975284,333.681409926766));
#66506=CARTESIAN_POINT('Ctrl Pts',(23.883626016551,4.70159399097006,333.549858842741));
#66507=CARTESIAN_POINT('Ctrl Pts',(23.8758523461463,4.65765757172184,333.420313636483));
#66508=CARTESIAN_POINT('Ctrl Pts',(23.8684405419692,4.61576640335982,333.296798790741));
#66509=CARTESIAN_POINT('Ctrl Pts',(23.8610287377921,4.56901167739254,333.175107546826));
#66510=CARTESIAN_POINT('Ctrl Pts',(23.8536169336149,4.51759195021922,333.055637370804));
#66511=CARTESIAN_POINT('Ctrl Pts',(23.8458418548365,4.46365198904594,332.930311605572));
#66512=CARTESIAN_POINT('Ctrl Pts',(23.8380667760581,4.40440771259694,332.807034083082));
#66513=CARTESIAN_POINT('Ctrl Pts',(23.8302916972796,4.34003594693644,332.686286309458));
#66514=CARTESIAN_POINT('Ctrl Pts',(23.8225261862306,4.2757433948317,332.565687123658));
#66515=CARTESIAN_POINT('Ctrl Pts',(23.8147606751816,4.20633609013593,332.447611834338));
#66516=CARTESIAN_POINT('Ctrl Pts',(23.8069951641326,4.13203909383756,332.332522541895));
#66517=CARTESIAN_POINT('Ctrl Pts',(23.7992373526104,4.05781576322758,332.217547360821));
#66518=CARTESIAN_POINT('Ctrl Pts',(23.7914795410882,3.97871259972482,332.105552611091));
#66519=CARTESIAN_POINT('Ctrl Pts',(23.7837217295661,3.8950006274356,331.996975994972));
#66520=CARTESIAN_POINT('Ctrl Pts',(23.775969756043,3.81135165105997,331.888481086199));
#66521=CARTESIAN_POINT('Ctrl Pts',(23.76821778252,3.72310100703136,331.783399499398));
#66522=CARTESIAN_POINT('Ctrl Pts',(23.760465808997,3.63056288741391,331.682139818643));
#66523=CARTESIAN_POINT('Ctrl Pts',(23.7527171184394,3.53806395774507,331.580923021423));
#66524=CARTESIAN_POINT('Ctrl Pts',(23.7449684278818,3.44128142701886,331.483525198944));
#66525=CARTESIAN_POINT('Ctrl Pts',(23.7372197373241,3.3405694669172,331.390321524124));
#66526=CARTESIAN_POINT('Ctrl Pts',(23.7294726589463,3.23987846078013,331.297137241108));
#66527=CARTESIAN_POINT('Ctrl Pts',(23.7217255805685,3.13525993813002,331.208145635356));
#66528=CARTESIAN_POINT('Ctrl Pts',(23.7139785021906,3.02710430652878,331.123684406567));
#66529=CARTESIAN_POINT('Ctrl Pts',(23.7062313588848,2.91894776847888,331.039222469911));
#66530=CARTESIAN_POINT('Ctrl Pts',(23.698484215579,2.80725437041722,330.959291226527));
#66531=CARTESIAN_POINT('Ctrl Pts',(23.6907370722732,2.69244659266633,330.884187272465));
#66532=CARTESIAN_POINT('Ctrl Pts',(23.6829881872451,2.57761300369018,330.80906643344));
#66533=CARTESIAN_POINT('Ctrl Pts',(23.675239302217,2.45966396878477,330.738775257255));
#66534=CARTESIAN_POINT('Ctrl Pts',(23.667490417189,2.33904950765398,330.673566080102));
#66535=CARTESIAN_POINT('Ctrl Pts',(23.6597333074142,2.21830702508764,330.608287689254));
#66536=CARTESIAN_POINT('Ctrl Pts',(23.6519761976395,2.09489380926462,330.54810225882));
#66537=CARTESIAN_POINT('Ctrl Pts',(23.6442190878648,1.96928345570421,330.493215588295));
#66538=CARTESIAN_POINT('Ctrl Pts',(23.6364578329386,1.84360597998719,330.438299588088));
#66539=CARTESIAN_POINT('Ctrl Pts',(23.6286965780125,1.71572939129793,330.388688131092));
#66540=CARTESIAN_POINT('Ctrl Pts',(23.6209353230863,1.58614472649503,330.344537835068));
#66541=CARTESIAN_POINT('Ctrl Pts',(23.6131616526817,1.45635276845982,330.300316912959));
#66542=CARTESIAN_POINT('Ctrl Pts',(23.605387982277,1.32484764937521,330.261574719609));
#66543=CARTESIAN_POINT('Ctrl Pts',(23.5976143118723,1.19213380417996,330.228417447489));
#66544=CARTESIAN_POINT('Ctrl Pts',(23.5902025076952,1.06559782040747,330.196803654362));
#66545=CARTESIAN_POINT('Ctrl Pts',(23.5827907035181,0.937963392224171,330.170266586172));
#66546=CARTESIAN_POINT('Ctrl Pts',(23.575378899341,0.809672207586631,330.148854364301));
#66547=CARTESIAN_POINT('Ctrl Pts',(23.5676038205626,0.675093089830752,330.126392665653));
#66548=CARTESIAN_POINT('Ctrl Pts',(23.5598287417841,0.539365913735656,330.109499900557));
#66549=CARTESIAN_POINT('Ctrl Pts',(23.5520536630057,0.402991278805547,330.098287942799));
#66550=CARTESIAN_POINT('Ctrl Pts',(23.5442881519567,0.266784461545384,330.087089782069));
#66551=CARTESIAN_POINT('Ctrl Pts',(23.5365226409077,0.129932156568909,330.081558551118));
#66552=CARTESIAN_POINT('Ctrl Pts',(23.5287571298587,-0.00705525262612259,
330.081755060399));
#66553=CARTESIAN_POINT('Ctrl Pts',(23.5209993183366,-0.143906838405085,
330.081951374841));
#66554=CARTESIAN_POINT('Ctrl Pts',(23.5132415068143,-0.280892873466163,
330.087864127286));
#66555=CARTESIAN_POINT('Ctrl Pts',(23.5054836952922,-0.417498617938304,
330.099502273593));
#66556=CARTESIAN_POINT('Ctrl Pts',(23.4977317217692,-0.554001562256641,
330.111131661826));
#66557=CARTESIAN_POINT('Ctrl Pts',(23.4899797482462,-0.690124397719518,
330.128477834937));
#66558=CARTESIAN_POINT('Ctrl Pts',(23.4822277747232,-0.825353509908196,
330.151497690401));
#66559=CARTESIAN_POINT('Ctrl Pts',(23.4744790841656,-0.960525352487391,
330.174507796944));
#66560=CARTESIAN_POINT('Ctrl Pts',(23.4667303936079,-1.09480384005777,330.203186741366));
#66561=CARTESIAN_POINT('Ctrl Pts',(23.4589817030503,-1.22768181908871,330.237439720741));
#66562=CARTESIAN_POINT('Ctrl Pts',(23.4512346246725,-1.36053215174629,330.271685573496));
#66563=CARTESIAN_POINT('Ctrl Pts',(23.4434875462947,-1.49198217719144,330.311503056921));
#66564=CARTESIAN_POINT('Ctrl Pts',(23.4357404679169,-1.62153664460972,330.356746617652));
#66565=CARTESIAN_POINT('Ctrl Pts',(23.4279933246111,-1.75109219781887,330.401990557567));
#66566=CARTESIAN_POINT('Ctrl Pts',(23.4202461813053,-1.87875179229501,330.452660536622));
#66567=CARTESIAN_POINT('Ctrl Pts',(23.4124990379995,-2.00403738574771,330.508561787242));
#66568=CARTESIAN_POINT('Ctrl Pts',(23.4047501529715,-2.12935114606187,330.56447560565));
#66569=CARTESIAN_POINT('Ctrl Pts',(23.3970012679434,-2.25228948641384,330.625622876693));
#66570=CARTESIAN_POINT('Ctrl Pts',(23.3892523829153,-2.37239668043311,330.691761722795));
#66571=CARTESIAN_POINT('Ctrl Pts',(23.3814952731406,-2.49263135746923,330.757970769352));
#66572=CARTESIAN_POINT('Ctrl Pts',(23.3737381633659,-2.61002854245246,330.829181785596));
#66573=CARTESIAN_POINT('Ctrl Pts',(23.3659810535912,-2.72415888448473,330.905107884866));
#66574=CARTESIAN_POINT('Ctrl Pts',(23.358219798665,-2.83835021412237,330.981074556617));
#66575=CARTESIAN_POINT('Ctrl Pts',(23.3504585437389,-2.94927090642088,331.061761102088));
#66576=CARTESIAN_POINT('Ctrl Pts',(23.3426972888127,-3.05652352994429,331.146839352765));
#66577=CARTESIAN_POINT('Ctrl Pts',(23.3349236184081,-3.16394772271194,331.232053700918));
#66578=CARTESIAN_POINT('Ctrl Pts',(23.3271499480034,-3.2676918253267,331.321673537246));
#66579=CARTESIAN_POINT('Ctrl Pts',(23.3193762775988,-3.36739355958634,331.415332138488));
#66580=CARTESIAN_POINT('Ctrl Pts',(23.3119644734215,-3.46245415413123,331.504630909311));
#66581=CARTESIAN_POINT('Ctrl Pts',(23.3045526692443,-3.55384005366963,331.597600692638));
#66582=CARTESIAN_POINT('Ctrl Pts',(23.2971408650671,-3.64127176920603,331.693896104887));
#66583=CARTESIAN_POINT('Ctrl Pts',(23.2894457560932,-3.73204542737938,331.793872260924));
#66584=CARTESIAN_POINT('Ctrl Pts',(23.2817506471191,-3.81885747554393,331.897764952859));
#66585=CARTESIAN_POINT('Ctrl Pts',(23.2740555381452,-3.90134557327747,332.005223584244));
#66586=CARTESIAN_POINT('Ctrl Pts',(23.2663725283596,-3.983703973169,332.11251325607));
#66587=CARTESIAN_POINT('Ctrl Pts',(23.258689518574,-4.06175171740237,332.223357390518));
#66588=CARTESIAN_POINT('Ctrl Pts',(23.2510065087884,-4.13516406474217,332.337369492369));
#66589=CARTESIAN_POINT('Ctrl Pts',(23.2433304517848,-4.2085099771733,332.45127841834));
#66590=CARTESIAN_POINT('Ctrl Pts',(23.2356543947813,-4.27722861842953,332.568349277977));
#66591=CARTESIAN_POINT('Ctrl Pts',(23.2279783377777,-4.34103612823051,332.688163414967));
#66592=CARTESIAN_POINT('Ctrl Pts',(23.2203074810163,-4.40480041082547,332.807896382352));
#66593=CARTESIAN_POINT('Ctrl Pts',(23.2126366242549,-4.46365999172824,332.9303685797));
#66594=CARTESIAN_POINT('Ctrl Pts',(23.2049657674934,-4.51737517144896,333.05513377764));
#66595=CARTESIAN_POINT('Ctrl Pts',(23.1972983628446,-4.57106617774835,333.179842827547));
#66596=CARTESIAN_POINT('Ctrl Pts',(23.1896309581957,-4.61961723109349,333.306842458638));
#66597=CARTESIAN_POINT('Ctrl Pts',(23.181963553547,-4.66283554291853,333.435663795025));
#66598=CARTESIAN_POINT('Ctrl Pts',(23.1742958932823,-4.70605529555513,333.564489426056));
#66599=CARTESIAN_POINT('Ctrl Pts',(23.1666282330176,-4.74394181174648,333.695136509071));
#66600=CARTESIAN_POINT('Ctrl Pts',(23.158960572753,-4.77635129521544,333.827118349025));
#66601=CARTESIAN_POINT('Ctrl Pts',(23.1512931116582,-4.8087599368379,333.95909676071));
#66602=CARTESIAN_POINT('Ctrl Pts',(23.1436256505635,-4.83569173914186,334.092409470559));
#66603=CARTESIAN_POINT('Ctrl Pts',(23.1359581894687,-4.85705365503044,334.226557788419));
#66604=CARTESIAN_POINT('Ctrl Pts',(23.1282854233609,-4.87843035094071,334.360798921691));
#66605=CARTESIAN_POINT('Ctrl Pts',(23.1206126572532,-4.89422940212695,334.495876422066));
#66606=CARTESIAN_POINT('Ctrl Pts',(23.1129398911455,-4.90440943298956,334.63128442384));
#66607=CARTESIAN_POINT('Ctrl Pts',(23.1058990529332,-4.91375103799781,334.755540242373));
#66608=CARTESIAN_POINT('Ctrl Pts',(23.098858214721,-4.91836165408909,334.880074063817));
#66609=CARTESIAN_POINT('Ctrl Pts',(23.0918173765087,-4.91824794611184,335.004494782163));
#66610=CARTESIAN_POINT('',(21.3418173764747,-4.91824992891069,334.999163776336));
#66611=CARTESIAN_POINT('Ctrl Pts',(23.0918173764689,-4.91824794611119,335.004494782867));
#66612=CARTESIAN_POINT('Ctrl Pts',(23.0820354501074,-4.91808997014287,335.177354074335));
#66613=CARTESIAN_POINT('Ctrl Pts',(23.0722535237459,-4.90881535265375,335.349806614891));
#66614=CARTESIAN_POINT('Ctrl Pts',(23.0624715973843,-4.89057380172721,335.521028744274));
#66615=CARTESIAN_POINT('Ctrl Pts',(23.0524996235227,-4.87197784605229,335.69557745131));
#66616=CARTESIAN_POINT('Ctrl Pts',(23.0425276496611,-4.84406315992271,335.868847655051));
#66617=CARTESIAN_POINT('Ctrl Pts',(23.0325556757995,-4.80703664690709,336.039991220055));
#66618=CARTESIAN_POINT('Ctrl Pts',(23.028004727464,-4.79013871374812,336.118096671703));
#66619=CARTESIAN_POINT('Ctrl Pts',(23.0234537791286,-4.77134364998109,336.195759508206));
#66620=CARTESIAN_POINT('Ctrl Pts',(23.0189028307932,-4.75067438848183,336.272900592003));
#66621=CARTESIAN_POINT('Ctrl Pts',(23.0111277520147,-4.71536193828395,336.404692464679));
#66622=CARTESIAN_POINT('Ctrl Pts',(23.0033526732363,-4.67450533258638,336.535222038394));
#66623=CARTESIAN_POINT('Ctrl Pts',(22.9955775944578,-4.62821014747037,336.663987347714));
#66624=CARTESIAN_POINT('Ctrl Pts',(22.9878120834088,-4.58197193152694,336.792594203123));
#66625=CARTESIAN_POINT('Ctrl Pts',(22.9800465723598,-4.53030858333734,336.919440749576));
#66626=CARTESIAN_POINT('Ctrl Pts',(22.9722810613108,-4.47337620732547,337.044037272222));
#66627=CARTESIAN_POINT('Ctrl Pts',(22.9645232497886,-4.41650027993013,337.168510257054));
#66628=CARTESIAN_POINT('Ctrl Pts',(22.9567654382663,-4.3543658826801,337.290737304477));
#66629=CARTESIAN_POINT('Ctrl Pts',(22.9490076267441,-4.287178119855,337.410246217949));
#66630=CARTESIAN_POINT('Ctrl Pts',(22.9412556532211,-4.22004091795226,337.529665197173));
#66631=CARTESIAN_POINT('Ctrl Pts',(22.9335036796981,-4.14785811057876,337.646369774528));
#66632=CARTESIAN_POINT('Ctrl Pts',(22.9257517061751,-4.07088171624043,337.759910345442));
#66633=CARTESIAN_POINT('Ctrl Pts',(22.9180030156175,-3.99393792145069,337.873402831858));
#66634=CARTESIAN_POINT('Ctrl Pts',(22.9102543250599,-3.91220479628132,337.983733654058));
#66635=CARTESIAN_POINT('Ctrl Pts',(22.9025056345023,-3.82597873719878,338.090480507138));
#66636=CARTESIAN_POINT('Ctrl Pts',(22.8947585561245,-3.73977061816789,338.197205150644));
#66637=CARTESIAN_POINT('Ctrl Pts',(22.8870114777466,-3.64907167005151,338.300347004353));
#66638=CARTESIAN_POINT('Ctrl Pts',(22.8792643993688,-3.55421954813177,338.399515622288));
#66639=CARTESIAN_POINT('Ctrl Pts',(22.871517256063,-3.45936663126001,338.498685071351));
#66640=CARTESIAN_POINT('Ctrl Pts',(22.8637701127571,-3.36036074133253,338.593880935752));
#66641=CARTESIAN_POINT('Ctrl Pts',(22.8560229694513,-3.25757719608487,338.684748821025));
#66642=CARTESIAN_POINT('Ctrl Pts',(22.8482740844232,-3.15477054291421,338.775637135329));
#66643=CARTESIAN_POINT('Ctrl Pts',(22.8405251993951,-3.04818483720247,338.862195275458));
#66644=CARTESIAN_POINT('Ctrl Pts',(22.832776314367,-2.93822902802969,338.944108675144));
#66645=CARTESIAN_POINT('Ctrl Pts',(22.8250192045923,-2.82815651062484,339.026109018559));
#66646=CARTESIAN_POINT('Ctrl Pts',(22.8172620948176,-2.71470705819097,339.103454539559));
#66647=CARTESIAN_POINT('Ctrl Pts',(22.8095049850429,-2.59831965715527,339.175873324437));
#66648=CARTESIAN_POINT('Ctrl Pts',(22.8017437301167,-2.48187006241388,339.248330807597));
#66649=CARTESIAN_POINT('Ctrl Pts',(22.7939824751905,-2.3624797308668,339.315856116431));
#66650=CARTESIAN_POINT('Ctrl Pts',(22.7862212202643,-2.24061199712329,339.378223491423));
#66651=CARTESIAN_POINT('Ctrl Pts',(22.7784475498597,-2.11854931472239,339.440690633889));
#66652=CARTESIAN_POINT('Ctrl Pts',(22.770673879455,-1.99400166609688,339.49798319111));
#66653=CARTESIAN_POINT('Ctrl Pts',(22.7629002090504,-1.86745291224435,339.549923371118));
#66654=CARTESIAN_POINT('Ctrl Pts',(22.7554884048733,-1.74679503333055,339.599445723252));
#66655=CARTESIAN_POINT('Ctrl Pts',(22.7480766006964,-1.62431842983969,339.644102691832));
#66656=CARTESIAN_POINT('Ctrl Pts',(22.7406647965193,-1.50045324128822,339.683782993821));
#66657=CARTESIAN_POINT('Ctrl Pts',(22.7328897177409,-1.3705170508693,339.725408145612));
#66658=CARTESIAN_POINT('Ctrl Pts',(22.7251146389625,-1.23864209391131,339.761687996366));
#66659=CARTESIAN_POINT('Ctrl Pts',(22.717339560184,-1.10530761713335,339.792439684963));
#66660=CARTESIAN_POINT('Ctrl Pts',(22.709574049135,-0.972137216917547,339.823153531649));
#66661=CARTESIAN_POINT('Ctrl Pts',(22.701808538086,-0.837511247705164,339.848352664706));
#66662=CARTESIAN_POINT('Ctrl Pts',(22.694043027037,-0.701925998222751,339.867903342869));
#66663=CARTESIAN_POINT('Ctrl Pts',(22.6862852155148,-0.566475181909853,
339.887434636479));
#66664=CARTESIAN_POINT('Ctrl Pts',(22.6785274039926,-0.430067362508664,
339.901328564999));
#66665=CARTESIAN_POINT('Ctrl Pts',(22.6707695924704,-0.293210613862012,
339.909502072351));
#66666=CARTESIAN_POINT('Ctrl Pts',(22.6630176189473,-0.156456854258879,
339.917669428879));
#66667=CARTESIAN_POINT('Ctrl Pts',(22.6552656454243,-0.0192552264593384,
339.92012490952));
#66668=CARTESIAN_POINT('Ctrl Pts',(22.6475136719013,0.117879805785627,339.91683713518));
#66669=CARTESIAN_POINT('Ctrl Pts',(22.6397649813437,0.254956761263019,339.913550753215));
#66670=CARTESIAN_POINT('Ctrl Pts',(22.6320162907861,0.391966787331368,339.904525963234));
#66671=CARTESIAN_POINT('Ctrl Pts',(22.6242676002285,0.528394361650382,339.889783477934));
#66672=CARTESIAN_POINT('Ctrl Pts',(22.6165205218506,0.66479355107328,339.875044059931));
#66673=CARTESIAN_POINT('Ctrl Pts',(22.6087734434728,0.800610141422339,339.854589354803));
#66674=CARTESIAN_POINT('Ctrl Pts',(22.6010263650949,0.935333073697483,339.828492011358));
#66675=CARTESIAN_POINT('Ctrl Pts',(22.5932792217891,1.07005713508019,339.802394449192));
#66676=CARTESIAN_POINT('Ctrl Pts',(22.5855320784833,1.20368713636607,339.770654228719));
#66677=CARTESIAN_POINT('Ctrl Pts',(22.5777849351775,1.33572195372598,339.733395179449));
#66678=CARTESIAN_POINT('Ctrl Pts',(22.5700360501494,1.4677864553162,339.696127753554));
#66679=CARTESIAN_POINT('Ctrl Pts',(22.5622871651213,1.59825468323484,339.653339136044));
#66680=CARTESIAN_POINT('Ctrl Pts',(22.5545382800932,1.72664080618307,339.605202991066));
#66681=CARTESIAN_POINT('Ctrl Pts',(22.5467811703185,1.85516319948868,339.557015753887));
#66682=CARTESIAN_POINT('Ctrl Pts',(22.5390240605438,1.98159870663285,339.503469788496));
#66683=CARTESIAN_POINT('Ctrl Pts',(22.531266950769,2.10548110883107,339.444787099835));
#66684=CARTESIAN_POINT('Ctrl Pts',(22.5235056958429,2.22942970982394,339.386073053021));
#66685=CARTESIAN_POINT('Ctrl Pts',(22.5157444409167,2.35082214162788,339.322216995354));
#66686=CARTESIAN_POINT('Ctrl Pts',(22.5079831859905,2.46921782130587,339.253486383362));
#66687=CARTESIAN_POINT('Ctrl Pts',(22.5002095155858,2.58780289548628,339.18464582479));
#66688=CARTESIAN_POINT('Ctrl Pts',(22.4924358451811,2.7033813083497,339.110915340112));
#66689=CARTESIAN_POINT('Ctrl Pts',(22.4846621747765,2.81554170588994,339.032605604928));
#66690=CARTESIAN_POINT('Ctrl Pts',(22.4772503705994,2.92248100994075,338.957941206756));
#66691=CARTESIAN_POINT('Ctrl Pts',(22.4698385664223,3.02631312539106,338.879114466072));
#66692=CARTESIAN_POINT('Ctrl Pts',(22.4624267622451,3.12671169878485,338.796426874731));
#66693=CARTESIAN_POINT('Ctrl Pts',(22.4546516834667,3.23203110533235,338.709686518226));
#66694=CARTESIAN_POINT('Ctrl Pts',(22.4468766046883,3.33390471202152,338.618423162471));
#66695=CARTESIAN_POINT('Ctrl Pts',(22.4391015259098,3.43191939913591,338.522940859614));
#66696=CARTESIAN_POINT('Ctrl Pts',(22.4313360148608,3.52981347293789,338.427576053808));
#66697=CARTESIAN_POINT('Ctrl Pts',(22.4235705038118,3.62385779830284,338.328002901001));
#66698=CARTESIAN_POINT('Ctrl Pts',(22.4158049927628,3.71367133904075,338.224566365899));
#66699=CARTESIAN_POINT('Ctrl Pts',(22.4080471812406,3.80339582939158,338.121232388422));
#66700=CARTESIAN_POINT('Ctrl Pts',(22.4002893697184,3.88889762845553,338.014042944911));
#66701=CARTESIAN_POINT('Ctrl Pts',(22.3925315581962,3.96983194469297,337.903380339087));
#66702=CARTESIAN_POINT('Ctrl Pts',(22.3847795846732,4.05070535529075,337.792801010383));
#66703=CARTESIAN_POINT('Ctrl Pts',(22.3770276111501,4.12701789477725,337.678754035968));
#66704=CARTESIAN_POINT('Ctrl Pts',(22.3692756376271,4.19846476994724,337.561655058358));
#66705=CARTESIAN_POINT('Ctrl Pts',(22.3615269470695,4.26988138732318,337.444605672234));
#66706=CARTESIAN_POINT('Ctrl Pts',(22.3537782565119,4.33643623563221,337.324507186632));
#66707=CARTESIAN_POINT('Ctrl Pts',(22.3460295659543,4.39786775390278,337.201804324113));
#66708=CARTESIAN_POINT('Ctrl Pts',(22.3382824875764,4.45928649083288,337.079126990949));
#66709=CARTESIAN_POINT('Ctrl Pts',(22.3305354091986,4.51558384310076,336.953846707969));
#66710=CARTESIAN_POINT('Ctrl Pts',(22.3227883308208,4.56654433928952,336.826432550028));
#66711=CARTESIAN_POINT('Ctrl Pts',(22.315041187515,4.61750526257631,336.699017324234));
#66712=CARTESIAN_POINT('Ctrl Pts',(22.3072940442091,4.66312909541628,336.56946855073));
#66713=CARTESIAN_POINT('Ctrl Pts',(22.2995469009033,4.70324878182811,336.438274646489));
#66714=CARTESIAN_POINT('Ctrl Pts',(22.2917980158752,4.74337748799716,336.307051247073));
#66715=CARTESIAN_POINT('Ctrl Pts',(22.2840491308471,4.77799947106941,336.174182354653));
#66716=CARTESIAN_POINT('Ctrl Pts',(22.276300245819,4.80699785773934,336.04017049477));
#66717=CARTESIAN_POINT('Ctrl Pts',(22.2685431360443,4.83602702359653,335.906016393313));
#66718=CARTESIAN_POINT('Ctrl Pts',(22.2607860262696,4.85942058672978,335.770717283632));
#66719=CARTESIAN_POINT('Ctrl Pts',(22.2530289164948,4.87711293809443,335.634785358662));
#66720=CARTESIAN_POINT('Ctrl Pts',(22.2452676615687,4.89481474368594,335.498780796018));
#66721=CARTESIAN_POINT('Ctrl Pts',(22.2375064066425,4.90680923282958,335.362143133456));
#66722=CARTESIAN_POINT('Ctrl Pts',(22.2297451517163,4.91308289071888,335.225387602644));
#66723=CARTESIAN_POINT('Ctrl Pts',(22.2219714813117,4.91936658441621,335.08841330755));
#66724=CARTESIAN_POINT('Ctrl Pts',(22.214197810907,4.91991115796733,334.951321158502));
#66725=CARTESIAN_POINT('Ctrl Pts',(22.2064241405023,4.9147552578573,334.814625196254));
#66726=CARTESIAN_POINT('Ctrl Pts',(22.1990123363253,4.90983936613787,334.684292463936));
#66727=CARTESIAN_POINT('Ctrl Pts',(22.1916005321483,4.89974179375709,334.554320150432));
#66728=CARTESIAN_POINT('Ctrl Pts',(22.1841887279713,4.884539463069,334.42514584787));
#66729=CARTESIAN_POINT('Ctrl Pts',(22.1764136491928,4.86859202086835,334.289640327947));
#66730=CARTESIAN_POINT('Ctrl Pts',(22.1686385704144,4.84697637208206,334.154584800215));
#66731=CARTESIAN_POINT('Ctrl Pts',(22.160863491636,4.81972463786244,334.020491205919));
#66732=CARTESIAN_POINT('Ctrl Pts',(22.1530979805869,4.79250643863674,333.886562622328));
#66733=CARTESIAN_POINT('Ctrl Pts',(22.1453324695379,4.7596660308589,333.753593996291));
#66734=CARTESIAN_POINT('Ctrl Pts',(22.1375669584889,4.7212873021629,333.622092429466));
#66735=CARTESIAN_POINT('Ctrl Pts',(22.1298091469667,4.68294662608811,333.490721246827));
#66736=CARTESIAN_POINT('Ctrl Pts',(22.1220513354445,4.63907866581843,333.36081460148));
#66737=CARTESIAN_POINT('Ctrl Pts',(22.1142935239223,4.58981832222422,333.232869322468));
#66738=CARTESIAN_POINT('Ctrl Pts',(22.1065415503993,4.54059504860078,333.105020326336));
#66739=CARTESIAN_POINT('Ctrl Pts',(22.0987895768763,4.48598760865884,332.979130121955));
#66740=CARTESIAN_POINT('Ctrl Pts',(22.0910376033533,4.42618058396466,332.85567994445));
#66741=CARTESIAN_POINT('Ctrl Pts',(22.0832889127956,4.36639888758086,332.732282048168));
#66742=CARTESIAN_POINT('Ctrl Pts',(22.0755402222381,4.30142215618538,332.61132247453));
#66743=CARTESIAN_POINT('Ctrl Pts',(22.0677915316805,4.23148282081839,332.493261840635));
#66744=CARTESIAN_POINT('Ctrl Pts',(22.0600444533026,4.16155803691427,332.37522577024));
#66745=CARTESIAN_POINT('Ctrl Pts',(22.0522973749248,4.08667290187253,332.260087775965));
#66746=CARTESIAN_POINT('Ctrl Pts',(22.0445502965469,4.00710526679841,332.148282895641));
#66747=CARTESIAN_POINT('Ctrl Pts',(22.0368031532411,3.92753696487097,332.036477078284));
#66748=CARTESIAN_POINT('Ctrl Pts',(22.0290560099353,3.84328631127445,331.928004749057));
#66749=CARTESIAN_POINT('Ctrl Pts',(22.0213088666295,3.75467362268367,331.823270699348));
#66750=CARTESIAN_POINT('Ctrl Pts',(22.0135599816014,3.6660410120792,331.718513103201));
#66751=CARTESIAN_POINT('Ctrl Pts',(22.0058110965733,3.57304466745953,331.617495757304));
#66752=CARTESIAN_POINT('Ctrl Pts',(21.9980622115452,3.47604392641988,331.520588888318));
#66753=CARTESIAN_POINT('Ctrl Pts',(21.9903051017705,3.37894022779148,331.423579161379));
#66754=CARTESIAN_POINT('Ctrl Pts',(21.9825479919958,3.27782391931504,331.330688903351));
#66755=CARTESIAN_POINT('Ctrl Pts',(21.9747908822211,3.17309021013766,331.242250463265));
#66756=CARTESIAN_POINT('Ctrl Pts',(21.9670296272949,3.06830053461491,331.153764764505));
#66757=CARTESIAN_POINT('Ctrl Pts',(21.9592683723687,2.95988991544971,331.069735863214));
#66758=CARTESIAN_POINT('Ctrl Pts',(21.9515071174426,2.84828430830456,330.990453945698));
#66759=CARTESIAN_POINT('Ctrl Pts',(21.9437334470379,2.73650016856,330.911045202953));
#66760=CARTESIAN_POINT('Ctrl Pts',(21.9359597766333,2.6215111556889,330.83639883124));
#66761=CARTESIAN_POINT('Ctrl Pts',(21.9281861062286,2.50377045135867,330.766760508853));
#66762=CARTESIAN_POINT('Ctrl Pts',(21.9207743020515,2.39151060514179,330.700363867128));
#66763=CARTESIAN_POINT('Ctrl Pts',(21.9133624978744,2.27674973806406,330.638519654518));
#66764=CARTESIAN_POINT('Ctrl Pts',(21.9059506936973,2.15989745778063,330.581399991584));
#66765=CARTESIAN_POINT('Ctrl Pts',(21.8981756149189,2.03731789915562,330.521480723819));
#66766=CARTESIAN_POINT('Ctrl Pts',(21.8904005361405,1.91204935673871,330.466571488493));
#66767=CARTESIAN_POINT('Ctrl Pts',(21.8826254573621,1.7845397154436,330.416922315026));
#66768=CARTESIAN_POINT('Ctrl Pts',(21.874859946313,1.65718698287976,330.367334238028));
#66769=CARTESIAN_POINT('Ctrl Pts',(21.8670944352641,1.52759899945329,330.322993484261));
#66770=CARTESIAN_POINT('Ctrl Pts',(21.859328924215,1.39624759417864,330.284103932628));
#66771=CARTESIAN_POINT('Ctrl Pts',(21.8515711126929,1.26502642420484,330.245252940099));
#66772=CARTESIAN_POINT('Ctrl Pts',(21.8438133011707,1.1320456842512,330.211842503933));
#66773=CARTESIAN_POINT('Ctrl Pts',(21.8360554896485,0.997796171060482,330.184028045813));
#66774=CARTESIAN_POINT('Ctrl Pts',(21.8283035161255,0.863647684885555,330.156234518954));
#66775=CARTESIAN_POINT('Ctrl Pts',(21.8205515426025,0.728232707145237,330.134028667031));
#66776=CARTESIAN_POINT('Ctrl Pts',(21.8127995690795,0.592055806398295,330.117515695406));
#66777=CARTESIAN_POINT('Ctrl Pts',(21.8050508785219,0.455936576649853,330.101009717033));
#66778=CARTESIAN_POINT('Ctrl Pts',(21.7973021879642,0.3190564528966,330.090191870727));
#66779=CARTESIAN_POINT('Ctrl Pts',(21.7895534974066,0.181928559655519,330.085115966609));
#66780=CARTESIAN_POINT('Ctrl Pts',(21.7818064190288,0.0448291970179419,
330.080041118575));
#66781=CARTESIAN_POINT('Ctrl Pts',(21.774059340651,-0.0925174422083032,
330.080705850917));
#66782=CARTESIAN_POINT('Ctrl Pts',(21.7663122622732,-0.229595164254071,
330.087111936645));
#66783=CARTESIAN_POINT('Ctrl Pts',(21.7585651189674,-0.366674035142992,
330.093518076063));
#66784=CARTESIAN_POINT('Ctrl Pts',(21.7508179756615,-0.50348359390794,330.105665646596));
#66785=CARTESIAN_POINT('Ctrl Pts',(21.7430708323558,-0.639510101102596,
330.123504342964));
#66786=CARTESIAN_POINT('Ctrl Pts',(21.7353219473277,-0.77556718994418,330.141347049851));
#66787=CARTESIAN_POINT('Ctrl Pts',(21.7275730622996,-0.910840489422211,
330.164883377792));
#66788=CARTESIAN_POINT('Ctrl Pts',(21.7198241772715,-1.04482420984807,330.194011503029));
#66789=CARTESIAN_POINT('Ctrl Pts',(21.7120670674968,-1.1789501419791,330.223170545159));
#66790=CARTESIAN_POINT('Ctrl Pts',(21.704309957722,-1.31178337825074,330.257933157518));
#66791=CARTESIAN_POINT('Ctrl Pts',(21.6965528479473,-1.44283056892518,330.298146853434));
#66792=CARTESIAN_POINT('Ctrl Pts',(21.6887915930212,-1.57394778702816,330.338382038263));
#66793=CARTESIAN_POINT('Ctrl Pts',(21.681030338095,-1.70327668943253,330.384073980692));
#66794=CARTESIAN_POINT('Ctrl Pts',(21.6732690831689,-1.83034274323121,330.435021521978));
#66795=CARTESIAN_POINT('Ctrl Pts',(21.6654954127642,-1.95761206130524,330.486050562727));
#66796=CARTESIAN_POINT('Ctrl Pts',(21.6577217423596,-2.08261094072176,330.542351841892));
#66797=CARTESIAN_POINT('Ctrl Pts',(21.6499480719549,-2.20488754275825,330.603677219961));
#66798=CARTESIAN_POINT('Ctrl Pts',(21.6425362677778,-2.32147213955305,330.662147886928));
#66799=CARTESIAN_POINT('Ctrl Pts',(21.6351244636006,-2.4355819474791,330.725185296306));
#66800=CARTESIAN_POINT('Ctrl Pts',(21.6277126594235,-2.54685056447943,330.792538144592));
#66801=CARTESIAN_POINT('Ctrl Pts',(21.619937580645,-2.66357278785013,330.863192156606));
#66802=CARTESIAN_POINT('Ctrl Pts',(21.6121625018666,-2.7775371314825,330.938818608485));
#66803=CARTESIAN_POINT('Ctrl Pts',(21.6043874230882,-2.88829096407598,331.019176169518));
#66804=CARTESIAN_POINT('Ctrl Pts',(21.5966219120391,-2.99890850702751,331.099434845455));
#66805=CARTESIAN_POINT('Ctrl Pts',(21.5888564009901,-3.10632308642778,331.184412819222));
#66806=CARTESIAN_POINT('Ctrl Pts',(21.5810908899411,-3.2101079224042,331.273823650306));
#66807=CARTESIAN_POINT('Ctrl Pts',(21.5733330784189,-3.31378985541352,331.363145830291));
#66808=CARTESIAN_POINT('Ctrl Pts',(21.5655752668967,-3.41384891278834,331.456891867438));
#66809=CARTESIAN_POINT('Ctrl Pts',(21.5578174553745,-3.50988879884018,331.554733147886));
#66810=CARTESIAN_POINT('Ctrl Pts',(21.5500654818515,-3.60585641183216,331.652500799667));
#66811=CARTESIAN_POINT('Ctrl Pts',(21.5423135083285,-3.69781060102026,331.754357282754));
#66812=CARTESIAN_POINT('Ctrl Pts',(21.5345615348055,-3.78538984597211,331.859935227338));
#66813=CARTESIAN_POINT('Ctrl Pts',(21.5268128442478,-3.87293200106186,331.9654684596));
#66814=CARTESIAN_POINT('Ctrl Pts',(21.5190641536902,-3.9561026479521,332.07471971851));
#66815=CARTESIAN_POINT('Ctrl Pts',(21.5113154631325,-4.03457885544455,332.187286626458));
#66816=CARTESIAN_POINT('Ctrl Pts',(21.5035683847547,-4.1130387353066,332.299830113921));
#66817=CARTESIAN_POINT('Ctrl Pts',(21.4958213063768,-4.18680589513273,332.415687557822));
#66818=CARTESIAN_POINT('Ctrl Pts',(21.488074227999,-4.25559950189281,332.534425839284));
#66819=CARTESIAN_POINT('Ctrl Pts',(21.4803270846931,-4.32439368520948,332.653165115888));
#66820=CARTESIAN_POINT('Ctrl Pts',(21.4725799413874,-4.38821403637023,332.77478494));
#66821=CARTESIAN_POINT('Ctrl Pts',(21.4648327980815,-4.44682484426436,332.898826074088));
#66822=CARTESIAN_POINT('Ctrl Pts',(21.4570839130534,-4.50544882911236,333.022895095256));
#66823=CARTESIAN_POINT('Ctrl Pts',(21.4493350280254,-4.55886077314829,333.14938615628));
#66824=CARTESIAN_POINT('Ctrl Pts',(21.4415861429973,-4.6068725903219,333.27781882514));
#66825=CARTESIAN_POINT('Ctrl Pts',(21.4338290332226,-4.65493536773438,333.406387813763));
#66826=CARTESIAN_POINT('Ctrl Pts',(21.4260719234478,-4.69758643149004,333.536902160242));
#66827=CARTESIAN_POINT('Ctrl Pts',(21.418314813673,-4.7346870310329,333.668864476971));
#66828=CARTESIAN_POINT('Ctrl Pts',(21.4105535587469,-4.77180745594989,333.800897310143));
#66829=CARTESIAN_POINT('Ctrl Pts',(21.4027923038207,-4.80337141674832,333.934379275138));
#66830=CARTESIAN_POINT('Ctrl Pts',(21.3950310488945,-4.82929127512125,334.068802468572));
#66831=CARTESIAN_POINT('Ctrl Pts',(21.3872573784899,-4.85525259682032,334.203440695307));
#66832=CARTESIAN_POINT('Ctrl Pts',(21.3794837080852,-4.87555171612219,334.339022772466));
#66833=CARTESIAN_POINT('Ctrl Pts',(21.3717100376805,-4.89015278297577,334.475034456698));
#66834=CARTESIAN_POINT('Ctrl Pts',(21.3642982335035,-4.90407416665439,334.604714764306));
#66835=CARTESIAN_POINT('Ctrl Pts',(21.3568864293264,-4.91281602895181,334.734785295515));
#66836=CARTESIAN_POINT('Ctrl Pts',(21.3494746251494,-4.91639141516887,334.864801940273));
#66837=CARTESIAN_POINT('Ctrl Pts',(21.3469222089359,-4.9176226772924,334.909576003941));
#66838=CARTESIAN_POINT('Ctrl Pts',(21.3443697927223,-4.91824231234348,334.954366964292));
#66839=CARTESIAN_POINT('Ctrl Pts',(21.3418173765088,-4.91824992891059,334.999163775737));
#66840=CARTESIAN_POINT('',(19.591817376556,-4.91824833437501,334.995952294795));
#66841=CARTESIAN_POINT('Ctrl Pts',(21.3418173764747,-4.91824992891069,334.999163776336));
#66842=CARTESIAN_POINT('Ctrl Pts',(21.3340781614017,-4.91827302318835,335.134992782795));
#66843=CARTESIAN_POINT('Ctrl Pts',(21.3263389463286,-4.91266500023186,335.271045543282));
#66844=CARTESIAN_POINT('Ctrl Pts',(21.3185997312556,-4.90139628266234,335.406813892098));
#66845=CARTESIAN_POINT('Ctrl Pts',(21.3108699817983,-4.89014134754353,335.542416186475));
#66846=CARTESIAN_POINT('Ctrl Pts',(21.3031402323411,-4.87323952338996,335.677734371529));
#66847=CARTESIAN_POINT('Ctrl Pts',(21.2954104828838,-4.85071320889987,335.812258842675));
#66848=CARTESIAN_POINT('Ctrl Pts',(21.2876882948886,-4.82820893029523,335.946651718135));
#66849=CARTESIAN_POINT('Ctrl Pts',(21.2799661068934,-4.80009117369241,336.080252037651));
#66850=CARTESIAN_POINT('Ctrl Pts',(21.2722439188982,-4.76643421685168,336.212554295248));
#66851=CARTESIAN_POINT('Ctrl Pts',(21.2645273951655,-4.73280194755231,336.344759508497));
#66852=CARTESIAN_POINT('Ctrl Pts',(21.2568108714327,-4.69363866102598,336.475668173544));
#66853=CARTESIAN_POINT('Ctrl Pts',(21.2490943476999,-4.64906981683823,336.604784378246));
#66854=CARTESIAN_POINT('Ctrl Pts',(21.2413808473697,-4.60451843511945,336.733849994073));
#66855=CARTESIAN_POINT('Ctrl Pts',(21.2336673470394,-4.55456583540986,336.861124173388));
#66856=CARTESIAN_POINT('Ctrl Pts',(21.2259538467092,-4.49938742338047,336.98612584617));
#66857=CARTESIAN_POINT('Ctrl Pts',(21.218241735535,-4.44421894865832,337.111105006887));
#66858=CARTESIAN_POINT('Ctrl Pts',(21.2105296243608,-4.38382669268926,337.233812113929));
#66859=CARTESIAN_POINT('Ctrl Pts',(21.2028175131865,-4.31843415111682,337.353786214797));
#66860=CARTESIAN_POINT('Ctrl Pts',(21.195105081932,-4.2530388955193,337.47376529502));
#66861=CARTESIAN_POINT('Ctrl Pts',(21.1873926506776,-4.18264313041195,337.591010796669));
#66862=CARTESIAN_POINT('Ctrl Pts',(21.1796802194231,-4.10751602150002,337.705086910918));
#66863=CARTESIAN_POINT('Ctrl Pts',(21.1719657589653,-4.03236914603591,337.819193039519));
#66864=CARTESIAN_POINT('Ctrl Pts',(21.1642512985076,-3.95248866740103,337.93012779214));
#66865=CARTESIAN_POINT('Ctrl Pts',(21.1565368380498,-3.86818646389571,338.037485233385));
#66866=CARTESIAN_POINT('Ctrl Pts',(21.1488141124454,-3.78379394038932,338.144957695636));
#66867=CARTESIAN_POINT('Ctrl Pts',(21.1410913868409,-3.69497047589397,338.248844881976));
#66868=CARTESIAN_POINT('Ctrl Pts',(21.1333686612365,-3.60206783149632,338.348774462367));
#66869=CARTESIAN_POINT('Ctrl Pts',(21.1256414708774,-3.5091114771092,338.448761815243));
#66870=CARTESIAN_POINT('Ctrl Pts',(21.1179142805183,-3.41207152574919,338.544786727556));
#66871=CARTESIAN_POINT('Ctrl Pts',(21.1101870901592,-3.31133500482889,338.636515302909));
#66872=CARTESIAN_POINT('Ctrl Pts',(21.1024481691868,-3.21044555624333,338.728383131006));
#66873=CARTESIAN_POINT('Ctrl Pts',(21.0947092482144,-3.10584863222559,338.815941342409));
#66874=CARTESIAN_POINT('Ctrl Pts',(21.0869703272419,-2.99796307032023,338.898897343031));
#66875=CARTESIAN_POINT('Ctrl Pts',(21.0817257484532,-2.92485025115604,338.955115681843));
#66876=CARTESIAN_POINT('Ctrl Pts',(21.0764811696644,-2.85022770775908,339.009221294894));
#66877=CARTESIAN_POINT('Ctrl Pts',(21.0712365908756,-2.77423242997752,339.061134999844));
#66878=CARTESIAN_POINT('Ctrl Pts',(21.0634615120971,-2.66156956507691,339.138096975616));
#66879=CARTESIAN_POINT('Ctrl Pts',(21.0556864333187,-2.54552365829148,339.210488821577));
#66880=CARTESIAN_POINT('Ctrl Pts',(21.0479113545403,-2.42650187869756,339.277998561848));
#66881=CARTESIAN_POINT('Ctrl Pts',(21.0401458434913,-2.30762656298088,339.345425227086));
#66882=CARTESIAN_POINT('Ctrl Pts',(21.0323803324422,-2.18578299752819,339.407981549316));
#66883=CARTESIAN_POINT('Ctrl Pts',(21.0246148213932,-2.0614086975397,339.465397769987));
#66884=CARTESIAN_POINT('Ctrl Pts',(21.0168570098711,-1.93715771503184,339.522757062309));
#66885=CARTESIAN_POINT('Ctrl Pts',(21.0090991983489,-1.81038134409719,339.574986232473));
#66886=CARTESIAN_POINT('Ctrl Pts',(21.0013413868267,-1.68154285413715,339.621860739161));
#66887=CARTESIAN_POINT('Ctrl Pts',(20.9935894133037,-1.5528013192265,339.668699971297));
#66888=CARTESIAN_POINT('Ctrl Pts',(20.9858374397807,-1.42200111993228,339.710192427485));
#66889=CARTESIAN_POINT('Ctrl Pts',(20.9780854662577,-1.28962639175671,339.746161273301));
#66890=CARTESIAN_POINT('Ctrl Pts',(20.9703367757001,-1.15730772435694,339.78211488629));
#66891=CARTESIAN_POINT('Ctrl Pts',(20.9625880851425,-1.02341623073437,339.812549439235));
#66892=CARTESIAN_POINT('Ctrl Pts',(20.9548393945848,-0.888451921028,339.837337723017));
#66893=CARTESIAN_POINT('Ctrl Pts',(20.947092316207,-0.753515691773504,339.86212084939));
#66894=CARTESIAN_POINT('Ctrl Pts',(20.9393452378292,-0.617507474614878,
339.881259972703));
#66895=CARTESIAN_POINT('Ctrl Pts',(20.9315981594513,-0.48093781743464,339.894678935156));
#66896=CARTESIAN_POINT('Ctrl Pts',(20.9238510161455,-0.344367015669321,
339.908098010073));
#66897=CARTESIAN_POINT('Ctrl Pts',(20.9161038728397,-0.2072351534981,339.915796790288));
#66898=CARTESIAN_POINT('Ctrl Pts',(20.9083567295339,-0.0700578565870874,
339.917751006225));
#66899=CARTESIAN_POINT('Ctrl Pts',(20.9006078445059,0.0671502806924412,
339.919705661512));
#66900=CARTESIAN_POINT('Ctrl Pts',(20.8928589594778,0.204403482279608,339.915913177015));
#66901=CARTESIAN_POINT('Ctrl Pts',(20.8851100744497,0.341186563463491,339.906401409527));
#66902=CARTESIAN_POINT('Ctrl Pts',(20.877352964675,0.478114827623163,339.896879546151));
#66903=CARTESIAN_POINT('Ctrl Pts',(20.8695958549003,0.614571584050395,339.881626300538));
#66904=CARTESIAN_POINT('Ctrl Pts',(20.8618387451255,0.750046655614415,339.86072145642));
#66905=CARTESIAN_POINT('Ctrl Pts',(20.8540774901994,0.885594120725117,339.839805441422));
#66906=CARTESIAN_POINT('Ctrl Pts',(20.8463162352732,1.02015847242363,339.81323188592));
#66907=CARTESIAN_POINT('Ctrl Pts',(20.8385549803471,1.15324113840553,339.781131449687));
#66908=CARTESIAN_POINT('Ctrl Pts',(20.8307813099424,1.28653669328146,339.748979663219));
#66909=CARTESIAN_POINT('Ctrl Pts',(20.8230076395377,1.41834545004566,339.711283436202));
#66910=CARTESIAN_POINT('Ctrl Pts',(20.815233969133,1.5481845218662,339.668223189689));
#66911=CARTESIAN_POINT('Ctrl Pts',(20.8078221649558,1.67197955365779,339.627167408011));
#66912=CARTESIAN_POINT('Ctrl Pts',(20.8004103607787,1.79398388203258,339.581235859985));
#66913=CARTESIAN_POINT('Ctrl Pts',(20.7929985566015,1.91379870860334,339.530624412313));
#66914=CARTESIAN_POINT('Ctrl Pts',(20.7852234778231,2.03948601673257,339.477532346828));
#66915=CARTESIAN_POINT('Ctrl Pts',(20.7774483990446,2.16316096328841,339.419122249775));
#66916=CARTESIAN_POINT('Ctrl Pts',(20.7696733202662,2.28434085854605,339.355567690265));
#66917=CARTESIAN_POINT('Ctrl Pts',(20.7619078092172,2.40537163422788,339.292091338686));
#66918=CARTESIAN_POINT('Ctrl Pts',(20.7541422981682,2.52391312482046,339.223483300518));
#66919=CARTESIAN_POINT('Ctrl Pts',(20.7463767871191,2.639501720024,339.149965509795));
#66920=CARTESIAN_POINT('Ctrl Pts',(20.7386189755969,2.75497570879895,339.076520612176));
#66921=CARTESIAN_POINT('Ctrl Pts',(20.7308611640747,2.86750230099026,338.998175858087));
#66922=CARTESIAN_POINT('Ctrl Pts',(20.7231033525525,2.97664197335678,338.915199308458));
#66923=CARTESIAN_POINT('Ctrl Pts',(20.7153513790295,3.08569951465867,338.832285201314));
#66924=CARTESIAN_POINT('Ctrl Pts',(20.7075994055065,3.19137489942236,338.744746472108));
#66925=CARTESIAN_POINT('Ctrl Pts',(20.6998474319835,3.29325743030678,338.652894545457));
#66926=CARTESIAN_POINT('Ctrl Pts',(20.6920987414259,3.39509681387887,338.561081518151));
#66927=CARTESIAN_POINT('Ctrl Pts',(20.6843500508682,3.49314624863431,338.464959187647));
#66928=CARTESIAN_POINT('Ctrl Pts',(20.6766013603106,3.58702817753414,338.364879182984));
#66929=CARTESIAN_POINT('Ctrl Pts',(20.6688542819328,3.68089057351467,338.264820000801));
#66930=CARTESIAN_POINT('Ctrl Pts',(20.6611072035549,3.77058692107839,338.160805067211));
#66931=CARTESIAN_POINT('Ctrl Pts',(20.6533601251771,3.85577689075191,338.053222499466));
#66932=CARTESIAN_POINT('Ctrl Pts',(20.6456129818713,3.94096757439943,337.945639030075));
#66933=CARTESIAN_POINT('Ctrl Pts',(20.6378658385655,4.02165156217347,337.834488173324));
#66934=CARTESIAN_POINT('Ctrl Pts',(20.6301186952597,4.09752941063708,337.720190396179));
#66935=CARTESIAN_POINT('Ctrl Pts',(20.6223698102316,4.17342431805196,337.605866922467));
#66936=CARTESIAN_POINT('Ctrl Pts',(20.6146209252034,4.24451071989516,337.488395446109));
#66937=CARTESIAN_POINT('Ctrl Pts',(20.6068720401753,4.31053324553024,337.368224271829));
#66938=CARTESIAN_POINT('Ctrl Pts',(20.5991149304006,4.37662584815616,337.247925546623));
#66939=CARTESIAN_POINT('Ctrl Pts',(20.5913578206259,4.43764364929566,337.124921742533));
#66940=CARTESIAN_POINT('Ctrl Pts',(20.5836007108511,4.49337765467301,336.999685053949));
#66941=CARTESIAN_POINT('Ctrl Pts',(20.575839455925,4.54914144252061,336.874381442883));
#66942=CARTESIAN_POINT('Ctrl Pts',(20.5680782009988,4.59961566478131,336.746842933062));
#66943=CARTESIAN_POINT('Ctrl Pts',(20.5603169460726,4.64464038996505,336.617559492076));
#66944=CARTESIAN_POINT('Ctrl Pts',(20.552543275668,4.68973714003569,336.488069239717));
#66945=CARTESIAN_POINT('Ctrl Pts',(20.5447696052633,4.72936685999392,336.35682885269));
#66946=CARTESIAN_POINT('Ctrl Pts',(20.5369959348586,4.76341995197727,336.224342037016));
#66947=CARTESIAN_POINT('Ctrl Pts',(20.5295841306816,4.79588786433558,336.098022514488));
#66948=CARTESIAN_POINT('Ctrl Pts',(20.5221723265046,4.82328658838349,335.970570275725));
#66949=CARTESIAN_POINT('Ctrl Pts',(20.5147605223277,4.84556501991885,335.842426673509));
#66950=CARTESIAN_POINT('Ctrl Pts',(20.5069854435492,4.86893538374813,335.708002371626));
#66951=CARTESIAN_POINT('Ctrl Pts',(20.4992103647708,4.88674469705931,335.572392415491));
#66952=CARTESIAN_POINT('Ctrl Pts',(20.4914352859923,4.89887770671504,335.436096637399));
#66953=CARTESIAN_POINT('Ctrl Pts',(20.4836697749433,4.91099578592995,335.299968579938));
#66954=CARTESIAN_POINT('Ctrl Pts',(20.4759042638943,4.91745142541496,335.163156765346));
#66955=CARTESIAN_POINT('Ctrl Pts',(20.4681387528453,4.91818036809998,335.026171154655));
#66956=CARTESIAN_POINT('Ctrl Pts',(20.4603809413231,4.9189085880362,334.889321365596));
#66957=CARTESIAN_POINT('Ctrl Pts',(20.4526231298009,4.91392140871967,334.752298511714));
#66958=CARTESIAN_POINT('Ctrl Pts',(20.4448653182787,4.90320639706054,334.615617260631));
#66959=CARTESIAN_POINT('Ctrl Pts',(20.4371133447557,4.89249944878744,334.479038866524));
#66960=CARTESIAN_POINT('Ctrl Pts',(20.4293613712326,4.87607327818888,334.342801951645));
#66961=CARTESIAN_POINT('Ctrl Pts',(20.4216093977096,4.85396751697297,334.207420409882));
#66962=CARTESIAN_POINT('Ctrl Pts',(20.413860707152,4.83187111756015,334.072096202283));
#66963=CARTESIAN_POINT('Ctrl Pts',(20.4061120165944,4.80409997438072,333.93762703227));
#66964=CARTESIAN_POINT('Ctrl Pts',(20.3983633260368,4.77074546201769,333.804520682263));
#66965=CARTESIAN_POINT('Ctrl Pts',(20.3906162476589,4.7373978893395,333.671442026143));
#66966=CARTESIAN_POINT('Ctrl Pts',(20.3828691692812,4.6984693530649,333.539726004948));
#66967=CARTESIAN_POINT('Ctrl Pts',(20.3751220909033,4.65410205746412,333.409868841508));
#66968=CARTESIAN_POINT('Ctrl Pts',(20.3673749475975,4.60973439002279,333.28001058974));
#66969=CARTESIAN_POINT('Ctrl Pts',(20.3596278042917,4.55992799871301,333.152011596681));
#66970=CARTESIAN_POINT('Ctrl Pts',(20.3518806609859,4.5048744171493,333.026351209507));
#66971=CARTESIAN_POINT('Ctrl Pts',(20.3441317759578,4.44980845837164,332.90066257121));
#66972=CARTESIAN_POINT('Ctrl Pts',(20.3363828909298,4.38949311873274,332.77731394297));
#66973=CARTESIAN_POINT('Ctrl Pts',(20.3286340059017,4.32416719153442,332.656762674811));
#66974=CARTESIAN_POINT('Ctrl Pts',(20.320876896127,4.25877192672194,332.536083452291));
#66975=CARTESIAN_POINT('Ctrl Pts',(20.3131197863522,4.18835563708923,332.418207865206));
#66976=CARTESIAN_POINT('Ctrl Pts',(20.3053626765775,4.11320230217769,332.303567192779));
#66977=CARTESIAN_POINT('Ctrl Pts',(20.2976014216514,4.03800880772707,332.188865260042));
#66978=CARTESIAN_POINT('Ctrl Pts',(20.2898401667252,3.95807345178008,332.0774020039));
#66979=CARTESIAN_POINT('Ctrl Pts',(20.2820789117991,3.87372171042888,331.969577063733));
#66980=CARTESIAN_POINT('Ctrl Pts',(20.2743052413944,3.78923503378156,331.861579638802));
#66981=CARTESIAN_POINT('Ctrl Pts',(20.2665315709897,3.70031810786214,331.757232457833));
#66982=CARTESIAN_POINT('Ctrl Pts',(20.258757900585,3.60733520011827,331.656900268241));
#66983=CARTESIAN_POINT('Ctrl Pts',(20.2513460964079,3.51868066909978,331.561238566212));
#66984=CARTESIAN_POINT('Ctrl Pts',(20.2439342922309,3.42633038416839,331.469226675029));
#66985=CARTESIAN_POINT('Ctrl Pts',(20.2365224880537,3.33062783287907,331.381146410622));
#66986=CARTESIAN_POINT('Ctrl Pts',(20.2287474092753,3.23023461446837,331.28874907008));
#66987=CARTESIAN_POINT('Ctrl Pts',(20.2209723304968,3.12583495057434,331.20038651001));
#66988=CARTESIAN_POINT('Ctrl Pts',(20.2131972517184,3.01778679075014,331.116426137168));
#66989=CARTESIAN_POINT('Ctrl Pts',(20.2054317406694,2.90987159106528,331.03256908291));
#66990=CARTESIAN_POINT('Ctrl Pts',(20.1976662296204,2.79831713437253,330.953103674806));
#66991=CARTESIAN_POINT('Ctrl Pts',(20.1899007185714,2.68351748459625,330.878359917173));
#66992=CARTESIAN_POINT('Ctrl Pts',(20.1821429070492,2.56883165900734,330.803690268194));
#66993=CARTESIAN_POINT('Ctrl Pts',(20.1743850955271,2.45090736903167,330.733733165073));
#66994=CARTESIAN_POINT('Ctrl Pts',(20.1666272840049,2.33017068139372,330.668777579242));
#66995=CARTESIAN_POINT('Ctrl Pts',(20.1588753104819,2.20952485194151,330.60387087455));
#66996=CARTESIAN_POINT('Ctrl Pts',(20.1511233369589,2.0860711802891,330.54395837993));
#66997=CARTESIAN_POINT('Ctrl Pts',(20.1433713634358,1.96026325776023,330.489284865703));
#66998=CARTESIAN_POINT('Ctrl Pts',(20.1356226728782,1.83450861496141,330.434634505742));
#66999=CARTESIAN_POINT('Ctrl Pts',(20.1278739823206,1.70640206204155,330.38521886878));
#67000=CARTESIAN_POINT('Ctrl Pts',(20.120125291763,1.57642005209949,330.341235906183));
#67001=CARTESIAN_POINT('Ctrl Pts',(20.1123782133851,1.44646508599987,330.297262094609));
#67002=CARTESIAN_POINT('Ctrl Pts',(20.1046311350074,1.31463580904178,330.258718834334));
#67003=CARTESIAN_POINT('Ctrl Pts',(20.0968840566295,1.18142646047917,330.225755077399));
#67004=CARTESIAN_POINT('Ctrl Pts',(20.0891369133238,1.04821599549483,330.192791044197));
#67005=CARTESIAN_POINT('Ctrl Pts',(20.0813897700179,0.913625815265672,330.165406701497));
#67006=CARTESIAN_POINT('Ctrl Pts',(20.0736426267122,0.778162662886691,330.143700386859));
#67007=CARTESIAN_POINT('Ctrl Pts',(20.065893741684,0.642669055513983,330.121989192181));
#67008=CARTESIAN_POINT('Ctrl Pts',(20.0581448566559,0.50630247132605,330.105958627571));
#67009=CARTESIAN_POINT('Ctrl Pts',(20.0503959716278,0.369576730474485,330.095655384989));
#67010=CARTESIAN_POINT('Ctrl Pts',(20.0426388618531,0.232705867509498,330.085341206438));
#67011=CARTESIAN_POINT('Ctrl Pts',(20.0348817520784,0.0954754767577634,
330.080766522784));
#67012=CARTESIAN_POINT('Ctrl Pts',(20.0271246423036,-0.0415980922557909,
330.081925919507));
#67013=CARTESIAN_POINT('Ctrl Pts',(20.0193633873775,-0.178744909002143,
330.083085935774));
#67014=CARTESIAN_POINT('Ctrl Pts',(20.0116021324513,-0.315734346848884,
330.089986118277));
#67015=CARTESIAN_POINT('Ctrl Pts',(20.0038408775251,-0.452054206727391,
330.102569035027));
#67016=CARTESIAN_POINT('Ctrl Pts',(19.9960672071205,-0.588592133954979,
330.115172080342));
#67017=CARTESIAN_POINT('Ctrl Pts',(19.9882935367158,-0.724457955247771,
330.133475973245));
#67018=CARTESIAN_POINT('Ctrl Pts',(19.9805198663111,-0.859147820708077,
330.157371779222));
#67019=CARTESIAN_POINT('Ctrl Pts',(19.973108062134,-0.987567840527064,330.180155229682));
#67020=CARTESIAN_POINT('Ctrl Pts',(19.9656962579569,-1.11491864104462,330.208021640528));
#67021=CARTESIAN_POINT('Ctrl Pts',(19.9582844537798,-1.24077735640801,330.240834672516));
#67022=CARTESIAN_POINT('Ctrl Pts',(19.9505093750013,-1.37280478232483,330.275255968947));
#67023=CARTESIAN_POINT('Ctrl Pts',(19.9427342962229,-1.50360739280519,330.315229822088));
#67024=CARTESIAN_POINT('Ctrl Pts',(19.9349592174445,-1.63268252062706,330.360654049401));
#67025=CARTESIAN_POINT('Ctrl Pts',(19.9271937063954,-1.76159881328716,330.40602237931));
#67026=CARTESIAN_POINT('Ctrl Pts',(19.9194281953464,-1.88879148779234,330.456827609804));
#67027=CARTESIAN_POINT('Ctrl Pts',(19.9116626842973,-2.01376978587077,330.512916948394));
#67028=CARTESIAN_POINT('Ctrl Pts',(19.9039048727751,-2.13862416760254,330.56895067424));
#67029=CARTESIAN_POINT('Ctrl Pts',(19.896147061253,-2.26126818788701,330.630257922849));
#67030=CARTESIAN_POINT('Ctrl Pts',(19.8883892497308,-2.38122827532967,330.696636784645));
#67031=CARTESIAN_POINT('Ctrl Pts',(19.8806372762077,-2.50109808900271,330.762965694243));
#67032=CARTESIAN_POINT('Ctrl Pts',(19.8728853026847,-2.61828764940724,330.834358431887));
#67033=CARTESIAN_POINT('Ctrl Pts',(19.8651333291616,-2.73234565966671,330.910566022223));
#67034=CARTESIAN_POINT('Ctrl Pts',(19.857384638604,-2.84635536629051,330.986741338598));
#67035=CARTESIAN_POINT('Ctrl Pts',(19.8496359480464,-2.95723583618581,331.067727235353));
#67036=CARTESIAN_POINT('Ctrl Pts',(19.8418872574888,-3.06456277171435,331.153230175755));
#67037=CARTESIAN_POINT('Ctrl Pts',(19.8341401791109,-3.17186737697768,331.238715326556));
#67038=CARTESIAN_POINT('Ctrl Pts',(19.8263931007331,-3.2756196129515,331.328715408258));
#67039=CARTESIAN_POINT('Ctrl Pts',(19.8186460223553,-3.37542676146652,331.422895411024));
#67040=CARTESIAN_POINT('Ctrl Pts',(19.8108988790495,-3.47523474646131,331.517076203108));
#67041=CARTESIAN_POINT('Ctrl Pts',(19.8031517357437,-3.57109729376166,331.615436717871));
#67042=CARTESIAN_POINT('Ctrl Pts',(19.7954045924379,-3.6626574814509,331.717604040328));
#67043=CARTESIAN_POINT('Ctrl Pts',(19.7876557074098,-3.75423825381433,331.819794332168));
#67044=CARTESIAN_POINT('Ctrl Pts',(19.7799068223817,-3.84151448100874,331.925792843721));
#67045=CARTESIAN_POINT('Ctrl Pts',(19.7721579373536,-3.9241688412019,332.035192760357));
#67046=CARTESIAN_POINT('Ctrl Pts',(19.7644008275789,-4.00691093158706,332.144708795195));
#67047=CARTESIAN_POINT('Ctrl Pts',(19.7566437178042,-4.08502111938218,332.25763313464));
#67048=CARTESIAN_POINT('Ctrl Pts',(19.7488866080294,-4.15822453141655,332.373528639253));
#67049=CARTESIAN_POINT('Ctrl Pts',(19.7411253531033,-4.23146706101377,332.489486074718));
#67050=CARTESIAN_POINT('Ctrl Pts',(19.7333640981771,-4.29979739560863,332.60841750023));
#67051=CARTESIAN_POINT('Ctrl Pts',(19.7256028432509,-4.36298665068126,332.729861116919));
#67052=CARTESIAN_POINT('Ctrl Pts',(19.7178291728463,-4.42627698796859,332.851499003816));
#67053=CARTESIAN_POINT('Ctrl Pts',(19.7100555024416,-4.48440964581031,332.975656758239));
#67054=CARTESIAN_POINT('Ctrl Pts',(19.7022818320369,-4.537203567473,333.101851731342));
#67055=CARTESIAN_POINT('Ctrl Pts',(19.6948700278599,-4.58753991938023,333.222172298085));
#67056=CARTESIAN_POINT('Ctrl Pts',(19.6874582236829,-4.63302328554313,333.344344417031));
#67057=CARTESIAN_POINT('Ctrl Pts',(19.6800464195059,-4.67353947956275,333.467938710277));
#67058=CARTESIAN_POINT('Ctrl Pts',(19.6707544085463,-4.72433371398656,333.622886075311));
#67059=CARTESIAN_POINT('Ctrl Pts',(19.6614623975868,-4.76745266189659,333.780466072888));
#67060=CARTESIAN_POINT('Ctrl Pts',(19.6521703866272,-4.80266013689503,333.939981758657));
#67061=CARTESIAN_POINT('Ctrl Pts',(19.6429295360595,-4.8376737649186,334.098619175447));
#67062=CARTESIAN_POINT('Ctrl Pts',(19.6336886854917,-4.86486272716904,334.259170985439));
#67063=CARTESIAN_POINT('Ctrl Pts',(19.6244478349239,-4.88404150409399,334.420930359294));
#67064=CARTESIAN_POINT('Ctrl Pts',(19.6152987034669,-4.90302992404358,334.581084207142));
#67065=CARTESIAN_POINT('Ctrl Pts',(19.6061495720097,-4.91416630650535,334.742421708532));
#67066=CARTESIAN_POINT('Ctrl Pts',(19.5970004405527,-4.91731760625495,334.904236636885));
#67067=CARTESIAN_POINT('Ctrl Pts',(19.5952727525538,-4.91791268599382,334.934793166876));
#67068=CARTESIAN_POINT('Ctrl Pts',(19.5935450645549,-4.91822316248318,334.965366664467));
#67069=CARTESIAN_POINT('Ctrl Pts',(19.591817376556,-4.91824833437501,334.995952294795));
#67070=CARTESIAN_POINT('',(17.841817376457,-4.91824925238431,335.002711811416));
#67071=CARTESIAN_POINT('Ctrl Pts',(19.5918173765088,-4.9182483343757,334.99595229563));
#67072=CARTESIAN_POINT('Ctrl Pts',(19.5839003352056,-4.91836368325021,335.136109371879));
#67073=CARTESIAN_POINT('Ctrl Pts',(19.5759832939023,-4.91248314281081,335.276354923141));
#67074=CARTESIAN_POINT('Ctrl Pts',(19.5680662525991,-4.90061363171136,335.416135909511));
#67075=CARTESIAN_POINT('Ctrl Pts',(19.5603456345828,-4.88903860541929,335.552448903266));
#67076=CARTESIAN_POINT('Ctrl Pts',(19.5526250165664,-4.8717683366803,335.688319701291));
#67077=CARTESIAN_POINT('Ctrl Pts',(19.5449043985501,-4.84886193943759,335.823238091182));
#67078=CARTESIAN_POINT('Ctrl Pts',(19.5371839329457,-4.82595599438794,335.958153817663));
#67079=CARTESIAN_POINT('Ctrl Pts',(19.5294634673413,-4.7974142076564,336.092116785396));
#67080=CARTESIAN_POINT('Ctrl Pts',(19.521743001737,-4.76334711911622,336.224625365288));
#67081=CARTESIAN_POINT('Ctrl Pts',(19.5140209910634,-4.72927321285147,336.357160463649));
#67082=CARTESIAN_POINT('Ctrl Pts',(19.5062989803899,-4.68967190260963,336.488240213965));
#67083=CARTESIAN_POINT('Ctrl Pts',(19.4985769697164,-4.64470394246313,336.617376996673));
#67084=CARTESIAN_POINT('Ctrl Pts',(19.4905129210093,-4.59774417560862,336.752233752207));
#67085=CARTESIAN_POINT('Ctrl Pts',(19.4824488723023,-4.54493159701169,336.884971021297));
#67086=CARTESIAN_POINT('Ctrl Pts',(19.4743848235953,-4.48650528533483,337.015056670956));
#67087=CARTESIAN_POINT('Ctrl Pts',(19.4666502342321,-4.43046599970475,337.139827628909));
#67088=CARTESIAN_POINT('Ctrl Pts',(19.4589156448689,-4.3692628586575,337.262159029399));
#67089=CARTESIAN_POINT('Ctrl Pts',(19.4511810555057,-4.30315346646788,337.381607294775));
#67090=CARTESIAN_POINT('Ctrl Pts',(19.4434408755016,-4.23699628972825,337.501141898588));
#67091=CARTESIAN_POINT('Ctrl Pts',(19.4357006954974,-4.16592600366716,337.617788882628));
#67092=CARTESIAN_POINT('Ctrl Pts',(19.4279605154933,-4.09024318364582,337.7311341529));
#67093=CARTESIAN_POINT('Ctrl Pts',(19.4202093897085,-4.0144533367149,337.844639710461));
#67094=CARTESIAN_POINT('Ctrl Pts',(19.4124582639238,-3.93403817053266,337.954833921385));
#67095=CARTESIAN_POINT('Ctrl Pts',(19.404707138139,-3.84933825326352,338.061335995029));
#67096=CARTESIAN_POINT('Ctrl Pts',(19.40374088717,-3.83877960934425,338.074612483467));
#67097=CARTESIAN_POINT('Ctrl Pts',(19.402774636201,-3.82815442665017,338.087831644003));
#67098=CARTESIAN_POINT('Ctrl Pts',(19.401808385232,-3.8174634036537,338.100992780428));
#67099=CARTESIAN_POINT('Ctrl Pts',(19.3940333064536,-3.73143653414728,338.206895776444));
#67100=CARTESIAN_POINT('Ctrl Pts',(19.3862582276751,-3.64086348977577,338.309383607315));
#67101=CARTESIAN_POINT('Ctrl Pts',(19.3784831488967,-3.54604552482822,338.408041108664));
#67102=CARTESIAN_POINT('Ctrl Pts',(19.3707176378477,-3.45134423942306,338.506577205677));
#67103=CARTESIAN_POINT('Ctrl Pts',(19.3629521267986,-3.35240869525998,338.601292072484));
#67104=CARTESIAN_POINT('Ctrl Pts',(19.3551866157496,-3.24958127500149,338.69180235111));
#67105=CARTESIAN_POINT('Ctrl Pts',(19.3474288042274,-3.14685580842964,338.78222288853));
#67106=CARTESIAN_POINT('Ctrl Pts',(19.3396709927052,-3.0402464365187,338.868446877444));
#67107=CARTESIAN_POINT('Ctrl Pts',(19.331913181183,-2.93013312495495,338.950126951446));
#67108=CARTESIAN_POINT('Ctrl Pts',(19.32416120766,-2.8201026771496,339.031745558603));
#67109=CARTESIAN_POINT('Ctrl Pts',(19.3164092341369,-2.70657385083344,339.108826825143));
#67110=CARTESIAN_POINT('Ctrl Pts',(19.3086572606139,-2.58996021994185,339.181063156856));
#67111=CARTESIAN_POINT('Ctrl Pts',(19.3009085700563,-2.47339597499264,339.253268896439));
#67112=CARTESIAN_POINT('Ctrl Pts',(19.2931598794986,-2.3537498554339,339.32063357674));
#67113=CARTESIAN_POINT('Ctrl Pts',(19.285411188941,-2.23146480664855,339.382892638337));
#67114=CARTESIAN_POINT('Ctrl Pts',(19.2776641105632,-2.10920520028877,339.445138746416));
#67115=CARTESIAN_POINT('Ctrl Pts',(19.2699170321853,-1.98430810491264,339.502281171483));
#67116=CARTESIAN_POINT('Ctrl Pts',(19.2621699538074,-1.85724112900778,339.554101278103));
#67117=CARTESIAN_POINT('Ctrl Pts',(19.2544228105016,-1.73017308815944,339.605921819026));
#67118=CARTESIAN_POINT('Ctrl Pts',(19.2466756671958,-1.60093549244348,339.652419804928));
#67119=CARTESIAN_POINT('Ctrl Pts',(19.23892852389,-1.47001561910445,339.693424884036));
#67120=CARTESIAN_POINT('Ctrl Pts',(19.2311796388619,-1.3390663121984,339.734439181957));
#67121=CARTESIAN_POINT('Ctrl Pts',(19.2234307538338,-1.20643434800378,339.769957998922));
#67122=CARTESIAN_POINT('Ctrl Pts',(19.2156818688057,-1.07262145102994,339.799861069374));
#67123=CARTESIAN_POINT('Ctrl Pts',(19.207924759031,-0.938666523664893,339.829795879254));
#67124=CARTESIAN_POINT('Ctrl Pts',(19.2001676492563,-0.803528541696102,
339.854102950361));
#67125=CARTESIAN_POINT('Ctrl Pts',(19.1924105394816,-0.667719243133995,
339.872713214919));
#67126=CARTESIAN_POINT('Ctrl Pts',(19.1846492845554,-0.531837372424799,
339.891333424208));
#67127=CARTESIAN_POINT('Ctrl Pts',(19.1768880296292,-0.395283859259923,
339.904250724331));
#67128=CARTESIAN_POINT('Ctrl Pts',(19.169126774703,-0.258573832245395,339.911448120033));
#67129=CARTESIAN_POINT('Ctrl Pts',(19.1613531042984,-0.121645113741525,
339.918657029223));
#67130=CARTESIAN_POINT('Ctrl Pts',(19.1535794338937,0.0154402278703251,
339.920127745421));
#67131=CARTESIAN_POINT('Ctrl Pts',(19.145805763489,0.152167902481845,339.91589544152));
#67132=CARTESIAN_POINT('Ctrl Pts',(19.138393959312,0.282530870945051,339.911860152383));
#67133=CARTESIAN_POINT('Ctrl Pts',(19.1309821551349,0.412568434761274,339.902640865946));
#67134=CARTESIAN_POINT('Ctrl Pts',(19.1235703509578,0.54184249212369,339.88831154656));
#67135=CARTESIAN_POINT('Ctrl Pts',(19.1157952721794,0.677452656125461,339.873279904546));
#67136=CARTESIAN_POINT('Ctrl Pts',(19.1080201934009,0.812651130976679,339.852577145278));
#67137=CARTESIAN_POINT('Ctrl Pts',(19.1002451146225,0.946925770113189,339.826231930647));
#67138=CARTESIAN_POINT('Ctrl Pts',(19.0924796035735,1.08103517575808,339.79991913548));
#67139=CARTESIAN_POINT('Ctrl Pts',(19.0847140925244,1.21422262777671,339.767977774863));
#67140=CARTESIAN_POINT('Ctrl Pts',(19.0769485814754,1.34598046936304,339.730488308684));
#67141=CARTESIAN_POINT('Ctrl Pts',(19.0691907699532,1.47760767266575,339.693036013419));
#67142=CARTESIAN_POINT('Ctrl Pts',(19.061432958431,1.60780771283721,339.650046666101));
#67143=CARTESIAN_POINT('Ctrl Pts',(19.0536751469088,1.73608286082123,339.601651808086));
#67144=CARTESIAN_POINT('Ctrl Pts',(19.0459231733858,1.86426147768855,339.553293368737));
#67145=CARTESIAN_POINT('Ctrl Pts',(19.0381711998628,1.99051772138093,339.499537652904));
#67146=CARTESIAN_POINT('Ctrl Pts',(19.0304192263397,2.11436912077686,339.440565986854));
#67147=CARTESIAN_POINT('Ctrl Pts',(19.0226705357821,2.23816806903145,339.38161929534));
#67148=CARTESIAN_POINT('Ctrl Pts',(19.0149218452245,2.3595638464446,339.31746121476));
#67149=CARTESIAN_POINT('Ctrl Pts',(19.0071731546669,2.47809427619279,339.248321059054));
#67150=CARTESIAN_POINT('Ctrl Pts',(18.999426076289,2.59660004469509,339.179195288534));
#67151=CARTESIAN_POINT('Ctrl Pts',(18.9916789979112,2.71224131391566,339.105089701505));
#67152=CARTESIAN_POINT('Ctrl Pts',(18.9839319195334,2.8245811788693,339.026279203741));
#67153=CARTESIAN_POINT('Ctrl Pts',(18.9761847762276,2.93692198533937,338.947468045469));
#67154=CARTESIAN_POINT('Ctrl Pts',(18.9684376329218,3.04596101236914,338.863952122293));
#67155=CARTESIAN_POINT('Ctrl Pts',(18.960690489616,3.15129131384103,338.776049008926));
#67156=CARTESIAN_POINT('Ctrl Pts',(18.9529416045879,3.25664529580049,338.688126133073));
#67157=CARTESIAN_POINT('Ctrl Pts',(18.9451927195598,3.35828859299271,338.595814354732));
#67158=CARTESIAN_POINT('Ctrl Pts',(18.9374438345317,3.4558485596247,338.499470502153));
#67159=CARTESIAN_POINT('Ctrl Pts',(18.929686724757,3.55351207741353,338.403024389214));
#67160=CARTESIAN_POINT('Ctrl Pts',(18.9219296149823,3.64708332833514,338.302537928049));
#67161=CARTESIAN_POINT('Ctrl Pts',(18.9141725052075,3.73622730102274,338.198404073533));
#67162=CARTESIAN_POINT('Ctrl Pts',(18.9064112502813,3.82541890939914,338.094214573214));
#67163=CARTESIAN_POINT('Ctrl Pts',(18.8986499953552,3.91017828406342,337.986374103044));
#67164=CARTESIAN_POINT('Ctrl Pts',(18.890888740429,3.99021236769644,337.875306648548));
#67165=CARTESIAN_POINT('Ctrl Pts',(18.8831150700244,4.07037447978013,337.764061522321));
#67166=CARTESIAN_POINT('Ctrl Pts',(18.8753413996197,4.14579598070891,337.649579422897));
#67167=CARTESIAN_POINT('Ctrl Pts',(18.867567729215,4.21622813623038,337.532311861868));
#67168=CARTESIAN_POINT('Ctrl Pts',(18.860155925038,4.28338165796657,337.42050313402));
#67169=CARTESIAN_POINT('Ctrl Pts',(18.852744120861,4.34599975065074,337.306162687484));
#67170=CARTESIAN_POINT('Ctrl Pts',(18.845332316684,4.40390753045873,337.189698957772));
#67171=CARTESIAN_POINT('Ctrl Pts',(18.8375572379056,4.46465354305414,337.067526993738));
#67172=CARTESIAN_POINT('Ctrl Pts',(18.8297821591271,4.52040780354033,336.942632260939));
#67173=CARTESIAN_POINT('Ctrl Pts',(18.8220070803487,4.57091726242068,336.815460944941));
#67174=CARTESIAN_POINT('Ctrl Pts',(18.8142415692997,4.62136456619628,336.688446121343));
#67175=CARTESIAN_POINT('Ctrl Pts',(18.8064760582507,4.66657976719625,336.559160648486));
#67176=CARTESIAN_POINT('Ctrl Pts',(18.7987105472017,4.70635580362896,336.428074967272));
#67177=CARTESIAN_POINT('Ctrl Pts',(18.7909527356795,4.74609240200571,336.297119257892));
#67178=CARTESIAN_POINT('Ctrl Pts',(18.7831949241573,4.78040045532157,336.164367263854));
#67179=CARTESIAN_POINT('Ctrl Pts',(18.7754371126351,4.8091212297588,336.030308720716));
#67180=CARTESIAN_POINT('Ctrl Pts',(18.7676851391121,4.8378203909024,335.896351060884));
#67181=CARTESIAN_POINT('Ctrl Pts',(18.7599331655891,4.86094056067386,335.761089189665));
#67182=CARTESIAN_POINT('Ctrl Pts',(18.7521811920662,4.87837312739248,335.625026953367));
#67183=CARTESIAN_POINT('Ctrl Pts',(18.7444325015085,4.89579831140878,335.489022339506));
#67184=CARTESIAN_POINT('Ctrl Pts',(18.736683810951,4.90754063354313,335.352218421623));
#67185=CARTESIAN_POINT('Ctrl Pts',(18.7289351203933,4.91354281838064,335.215127948998));
#67186=CARTESIAN_POINT('Ctrl Pts',(18.7211880420155,4.91954375441347,335.078065999191));
#67187=CARTESIAN_POINT('Ctrl Pts',(18.7134409636377,4.91980691157742,334.940718003486));
#67188=CARTESIAN_POINT('Ctrl Pts',(18.7056938852598,4.91432702964588,334.803600131894));
#67189=CARTESIAN_POINT('Ctrl Pts',(18.6979467419541,4.90884710178767,334.666481111124));
#67190=CARTESIAN_POINT('Ctrl Pts',(18.6901995986482,4.89762405443946,334.529592608876));
#67191=CARTESIAN_POINT('Ctrl Pts',(18.6824524553425,4.88070472105624,334.393448692723));
#67192=CARTESIAN_POINT('Ctrl Pts',(18.6747035703144,4.86378158384762,334.257274168527));
#67193=CARTESIAN_POINT('Ctrl Pts',(18.6669546852863,4.84115966045721,334.121844951344));
#67194=CARTESIAN_POINT('Ctrl Pts',(18.6592058002582,4.81293735535237,333.987667507212));
#67195=CARTESIAN_POINT('Ctrl Pts',(18.6514486904835,4.78468509480134,333.853347645756));
#67196=CARTESIAN_POINT('Ctrl Pts',(18.6436915807087,4.75082065881443,333.720282594553));
#67197=CARTESIAN_POINT('Ctrl Pts',(18.635934470934,4.71149319765503,333.588966722238));
#67198=CARTESIAN_POINT('Ctrl Pts',(18.6281732160078,4.67214472115781,333.457580678921));
#67199=CARTESIAN_POINT('Ctrl Pts',(18.6204119610816,4.62732753023863,333.327946046209));
#67200=CARTESIAN_POINT('Ctrl Pts',(18.6126507061555,4.57723957324151,333.200538705153));
#67201=CARTESIAN_POINT('Ctrl Pts',(18.6048770357508,4.52707149183689,333.072927553873));
#67202=CARTESIAN_POINT('Ctrl Pts',(18.5971033653462,4.47161595390004,332.947551171715));
#67203=CARTESIAN_POINT('Ctrl Pts',(18.5893296949415,4.41111804078659,332.824863063449));
#67204=CARTESIAN_POINT('Ctrl Pts',(18.5819178907644,4.35343632008304,332.707886116139));
#67205=CARTESIAN_POINT('Ctrl Pts',(18.5745060865872,4.29117124222047,332.593353049627));
#67206=CARTESIAN_POINT('Ctrl Pts',(18.5670942824101,4.22457162966154,332.481631955341));
#67207=CARTESIAN_POINT('Ctrl Pts',(18.5593192036316,4.15470777170164,332.364435077426));
#67208=CARTESIAN_POINT('Ctrl Pts',(18.5515441248532,4.07985295590634,332.249962423942));
#67209=CARTESIAN_POINT('Ctrl Pts',(18.5437690460748,4.00024544963459,332.138668246222));
#67210=CARTESIAN_POINT('Ctrl Pts',(18.5360035350258,3.92073590546758,332.027511023074));
#67211=CARTESIAN_POINT('Ctrl Pts',(18.5282380239768,3.83648553286708,331.919524808168));
#67212=CARTESIAN_POINT('Ctrl Pts',(18.5204725129279,3.7477778826058,331.815138306747));
#67213=CARTESIAN_POINT('Ctrl Pts',(18.5127147014057,3.65915818623771,331.710855304846));
#67214=CARTESIAN_POINT('Ctrl Pts',(18.5049568898834,3.56609025855625,331.6101652096));
#67215=CARTESIAN_POINT('Ctrl Pts',(18.4971990783612,3.46890002866377,331.513466527676));
#67216=CARTESIAN_POINT('Ctrl Pts',(18.4894471048383,3.37178293750176,331.416840614576));
#67217=CARTESIAN_POINT('Ctrl Pts',(18.4816951313153,3.2705499948068,331.324200410727));
#67218=CARTESIAN_POINT('Ctrl Pts',(18.4739431577923,3.1655661196753,331.235909910156));
#67219=CARTESIAN_POINT('Ctrl Pts',(18.4661944672347,3.06062670527681,331.147656800663));
#67220=CARTESIAN_POINT('Ctrl Pts',(18.4584457766771,2.951939816426,331.063749981695));
#67221=CARTESIAN_POINT('Ctrl Pts',(18.4506970861195,2.83990563991946,330.984515095427));
#67222=CARTESIAN_POINT('Ctrl Pts',(18.4429500077416,2.72789477305907,330.905296694639));
#67223=CARTESIAN_POINT('Ctrl Pts',(18.4352029293638,2.61253832272112,330.830748518663));
#67224=CARTESIAN_POINT('Ctrl Pts',(18.427455850986,2.49426750066995,330.761154320148));
#67225=CARTESIAN_POINT('Ctrl Pts',(18.4197087076802,2.37599568739553,330.691559538366));
#67226=CARTESIAN_POINT('Ctrl Pts',(18.4119615643744,2.25480979056905,330.626919015088));
#67227=CARTESIAN_POINT('Ctrl Pts',(18.4042144210686,2.13116744484765,330.567471558521));
#67228=CARTESIAN_POINT('Ctrl Pts',(18.3964655360405,2.00749730170211,330.508010736904));
#67229=CARTESIAN_POINT('Ctrl Pts',(18.3887166510124,1.88136996292533,330.453745474556));
#67230=CARTESIAN_POINT('Ctrl Pts',(18.3809677659843,1.75326457891779,330.404867098896));
#67231=CARTESIAN_POINT('Ctrl Pts',(18.3732106562096,1.62502322253156,330.355936843222));
#67232=CARTESIAN_POINT('Ctrl Pts',(18.3654535464348,1.49479999270271,330.312405035432));
#67233=CARTESIAN_POINT('Ctrl Pts',(18.35769643666,1.36309132832952,330.274413783124));
#67234=CARTESIAN_POINT('Ctrl Pts',(18.3499351817339,1.23131228305759,330.236402229504));
#67235=CARTESIAN_POINT('Ctrl Pts',(18.3421739268077,1.09804660116079,330.203937223287));
#67236=CARTESIAN_POINT('Ctrl Pts',(18.3344126718816,0.96380158237269,330.177109832029));
#67237=CARTESIAN_POINT('Ctrl Pts',(18.3266390014769,0.829341815304878,330.150239525687));
#67238=CARTESIAN_POINT('Ctrl Pts',(18.3188653310722,0.693899967144402,330.129024916149));
#67239=CARTESIAN_POINT('Ctrl Pts',(18.3110916606676,0.557990027312234,330.113505326728));
#67240=CARTESIAN_POINT('Ctrl Pts',(18.3036798564904,0.428406727876556,330.098708177927));
#67241=CARTESIAN_POINT('Ctrl Pts',(18.2962680523133,0.298398222389613,330.089087796073));
#67242=CARTESIAN_POINT('Ctrl Pts',(18.2888562481362,0.168408698899535,330.084634136442));
#67243=CARTESIAN_POINT('Ctrl Pts',(18.2810811693578,0.0320480016448979,
330.079962189685));
#67244=CARTESIAN_POINT('Ctrl Pts',(18.2733060905793,-0.104722730832196,
330.080961480005));
#67245=CARTESIAN_POINT('Ctrl Pts',(18.2655310118008,-0.241392568755692,
330.087677464758));
#67246=CARTESIAN_POINT('Ctrl Pts',(18.2577655007518,-0.377894225742424,
330.094385185064));
#67247=CARTESIAN_POINT('Ctrl Pts',(18.2499999897029,-0.514294848541628,
330.106795583653));
#67248=CARTESIAN_POINT('Ctrl Pts',(18.2422344786538,-0.65008048417517,330.124902213638));
#67249=CARTESIAN_POINT('Ctrl Pts',(18.2344766671316,-0.785731487955745,
330.142990890846));
#67250=CARTESIAN_POINT('Ctrl Pts',(18.2267188556095,-0.920768333081667,
330.166764508617));
#67251=CARTESIAN_POINT('Ctrl Pts',(18.2189610440873,-1.05467952785701,330.196164641037));
#67252=CARTESIAN_POINT('Ctrl Pts',(18.2112090705643,-1.18848995021189,330.225542648926));
#67253=CARTESIAN_POINT('Ctrl Pts',(18.2034570970412,-1.32117602805858,330.260538660152));
#67254=CARTESIAN_POINT('Ctrl Pts',(18.1957051235182,-1.45223419239217,330.301042784516));
#67255=CARTESIAN_POINT('Ctrl Pts',(18.1879564329605,-1.58323685351517,330.341529755359));
#67256=CARTESIAN_POINT('Ctrl Pts',(18.180207742403,-1.71261259966859,330.387520084611));
#67257=CARTESIAN_POINT('Ctrl Pts',(18.1724590518454,-1.83987102736082,330.438853470324));
#67258=CARTESIAN_POINT('Ctrl Pts',(18.1647119734675,-1.96710297787445,330.490176175696));
#67259=CARTESIAN_POINT('Ctrl Pts',(18.1569648950896,-2.09221812389769,330.546839580214));
#67260=CARTESIAN_POINT('Ctrl Pts',(18.1492178167118,-2.21474449834672,330.608634623543));
#67261=CARTESIAN_POINT('Ctrl Pts',(18.1414706734059,-2.33727189968494,330.670430184775));
#67262=CARTESIAN_POINT('Ctrl Pts',(18.1337235301001,-2.45721013717334,330.737357294586));
#67263=CARTESIAN_POINT('Ctrl Pts',(18.1259763867943,-2.57411073952276,330.809160351055));
#67264=CARTESIAN_POINT('Ctrl Pts',(18.1182275017662,-2.69103762360882,330.880979550374));
#67265=CARTESIAN_POINT('Ctrl Pts',(18.1104786167381,-2.80492518061293,330.957676673164));
#67266=CARTESIAN_POINT('Ctrl Pts',(18.10272973171,-2.91535322345182,331.038952329874));
#67267=CARTESIAN_POINT('Ctrl Pts',(18.0949726219353,-3.02589847575661,331.120314253406));
#67268=CARTESIAN_POINT('Ctrl Pts',(18.0872155121606,-3.13297656350486,331.206264186511));
#67269=CARTESIAN_POINT('Ctrl Pts',(18.0794584023859,-3.2361993338129,331.296461565701));
#67270=CARTESIAN_POINT('Ctrl Pts',(18.0716971474597,-3.33947726306918,331.386707143487));
#67271=CARTESIAN_POINT('Ctrl Pts',(18.0639358925335,-3.4388954866653,331.481204420788));
#67272=CARTESIAN_POINT('Ctrl Pts',(18.0561746376073,-3.53410289495589,331.579576080313));
#67273=CARTESIAN_POINT('Ctrl Pts',(18.0484009672026,-3.62946260407147,331.678105102435));
#67274=CARTESIAN_POINT('Ctrl Pts',(18.0406272967979,-3.7205977775169,331.780520599563));
#67275=CARTESIAN_POINT('Ctrl Pts',(18.0328536263933,-3.807197198311,331.88641162713));
#67276=CARTESIAN_POINT('Ctrl Pts',(18.0254418222163,-3.88976539523146,331.987373401886));
#67277=CARTESIAN_POINT('Ctrl Pts',(18.0180300180393,-3.96821044177837,332.091494187119));
#67278=CARTESIAN_POINT('Ctrl Pts',(18.0106182138623,-4.04230040913374,332.198395019847));
#67279=CARTESIAN_POINT('Ctrl Pts',(18.0027430572091,-4.12102214616636,332.311978809164));
#67280=CARTESIAN_POINT('Ctrl Pts',(17.9948679005558,-4.19507219954527,332.429055015561));
#67281=CARTESIAN_POINT('Ctrl Pts',(17.9869927439025,-4.26412989625754,332.549208435966));
#67282=CARTESIAN_POINT('Ctrl Pts',(17.9791278749331,-4.33309737968518,332.669204894363));
#67283=CARTESIAN_POINT('Ctrl Pts',(17.9712630059637,-4.39708529984977,332.792270242156));
#67284=CARTESIAN_POINT('Ctrl Pts',(17.9633981369942,-4.45581496266319,332.91795867452));
#67285=CARTESIAN_POINT('Ctrl Pts',(17.9555419936708,-4.51447946809779,333.043507662378));
#67286=CARTESIAN_POINT('Ctrl Pts',(17.9476858503473,-4.56789716993842,333.171673602145));
#67287=CARTESIAN_POINT('Ctrl Pts',(17.9398297070238,-4.61583432718745,333.301984532916));
#67288=CARTESIAN_POINT('Ctrl Pts',(17.9316620128142,-4.66567252712435,333.437463201122));
#67289=CARTESIAN_POINT('Ctrl Pts',(17.9234943186047,-4.70958633391736,333.575260143042));
#67290=CARTESIAN_POINT('Ctrl Pts',(17.9153266243951,-4.74736692646326,333.714818951267));
#67291=CARTESIAN_POINT('Ctrl Pts',(17.9074841982159,-4.78364295497812,333.848820007511));
#67292=CARTESIAN_POINT('Ctrl Pts',(17.8996417720367,-4.81426473902137,333.984444899537));
#67293=CARTESIAN_POINT('Ctrl Pts',(17.8917993458575,-4.83909747893079,334.121183379819));
#67294=CARTESIAN_POINT('Ctrl Pts',(17.8839605331121,-4.86391877704156,334.257858857221));
#67295=CARTESIAN_POINT('Ctrl Pts',(17.8761217203666,-4.88295627539233,334.395646530158));
#67296=CARTESIAN_POINT('Ctrl Pts',(17.8682829076212,-4.89612605567246,334.534024990514));
#67297=CARTESIAN_POINT('Ctrl Pts',(17.8604460906169,-4.90929248296112,334.672368220078));
#67298=CARTESIAN_POINT('Ctrl Pts',(17.8526092736126,-4.91659413243677,334.811301561753));
#67299=CARTESIAN_POINT('Ctrl Pts',(17.8447724566083,-4.91799885567452,334.950297705445));
#67300=CARTESIAN_POINT('Ctrl Pts',(17.8437874299084,-4.91817541841605,334.967768435288));
#67301=CARTESIAN_POINT('Ctrl Pts',(17.8428024032086,-4.91825888585813,334.985240153472));
#67302=CARTESIAN_POINT('Ctrl Pts',(17.8418173765088,-4.91824925238482,335.002711810498));
#67303=CARTESIAN_POINT('',(16.0918173765465,-4.91824914986108,335.002891779856));
#67304=CARTESIAN_POINT('Ctrl Pts',(17.841817376457,-4.91824925238431,335.002711811417));
#67305=CARTESIAN_POINT('Ctrl Pts',(17.8332302331793,-4.91816527086008,335.155024050462));
#67306=CARTESIAN_POINT('Ctrl Pts',(17.8246430899017,-4.91100184266203,335.307084674523));
#67307=CARTESIAN_POINT('Ctrl Pts',(17.8160559466241,-4.89685328824803,335.458269501357));
#67308=CARTESIAN_POINT('Ctrl Pts',(17.8074201728907,-4.88262460815933,335.610310513629));
#67309=CARTESIAN_POINT('Ctrl Pts',(17.7987843991574,-4.86133154917201,335.76146555601));
#67310=CARTESIAN_POINT('Ctrl Pts',(17.7901486254241,-4.83312016722997,335.911116080209));
#67311=CARTESIAN_POINT('Ctrl Pts',(17.7814876028616,-4.80482630230683,336.061204144879));
#67312=CARTESIAN_POINT('Ctrl Pts',(17.7728265802992,-4.76957371770995,336.209778671613));
#67313=CARTESIAN_POINT('Ctrl Pts',(17.7641655577368,-4.72755845325742,336.356235279564));
#67314=CARTESIAN_POINT('Ctrl Pts',(17.7554727122363,-4.68538881336621,336.503230008681));
#67315=CARTESIAN_POINT('Ctrl Pts',(17.7467798667357,-4.63640682438824,336.648091022477));
#67316=CARTESIAN_POINT('Ctrl Pts',(17.7380870212353,-4.58085791823456,336.790230095671));
#67317=CARTESIAN_POINT('Ctrl Pts',(17.7361847406862,-4.56870199027179,336.82133480059));
#67318=CARTESIAN_POINT('Ctrl Pts',(17.7342824601373,-4.55623176176412,336.852309250801));
#67319=CARTESIAN_POINT('Ctrl Pts',(17.7323801795882,-4.54345009596233,336.883147441917));
#67320=CARTESIAN_POINT('Ctrl Pts',(17.7246051008098,-4.49120834929648,337.009190556556));
#67321=CARTESIAN_POINT('Ctrl Pts',(17.7168300220313,-4.43363509748446,337.133257282632));
#67322=CARTESIAN_POINT('Ctrl Pts',(17.7090549432528,-4.37090064476501,337.254863768855));
#67323=CARTESIAN_POINT('Ctrl Pts',(17.7012894322037,-4.30824339078349,337.376320610554));
#67324=CARTESIAN_POINT('Ctrl Pts',(17.6935239211546,-4.24043775042469,337.495322892166));
#67325=CARTESIAN_POINT('Ctrl Pts',(17.6857584101056,-4.16770252064172,337.611405514648));
#67326=CARTESIAN_POINT('Ctrl Pts',(17.6780005985834,-4.0950394080509,337.727373040873));
#67327=CARTESIAN_POINT('Ctrl Pts',(17.6702427870611,-4.01745663904239,337.840426339792));
#67328=CARTESIAN_POINT('Ctrl Pts',(17.6624849755389,-3.93521929913768,337.950124087254));
#67329=CARTESIAN_POINT('Ctrl Pts',(17.6547330020159,-3.85304384543915,338.059739283681));
#67330=CARTESIAN_POINT('Ctrl Pts',(17.6469810284928,-3.7662210263367,338.166003643366));
#67331=CARTESIAN_POINT('Ctrl Pts',(17.6392290549698,-3.67505948478858,338.268504374445));
#67332=CARTESIAN_POINT('Ctrl Pts',(17.6314803644122,-3.58393655020742,338.370961696403));
#67333=CARTESIAN_POINT('Ctrl Pts',(17.6237316738546,-3.48847880696359,338.469658268443));
#67334=CARTESIAN_POINT('Ctrl Pts',(17.6159829832969,-3.3890353254058,338.564214166636));
#67335=CARTESIAN_POINT('Ctrl Pts',(17.608235904919,-3.28961253389491,338.658750391686));
#67336=CARTESIAN_POINT('Ctrl Pts',(17.6004888265411,-3.18620593662452,338.749147387305));
#67337=CARTESIAN_POINT('Ctrl Pts',(17.5927417481633,-3.07920134282074,338.835062209778));
#67338=CARTESIAN_POINT('Ctrl Pts',(17.5849946048574,-2.97219585221554,338.920977752301));
#67339=CARTESIAN_POINT('Ctrl Pts',(17.5772474615517,-2.86159260971993,339.002410802035));
#67340=CARTESIAN_POINT('Ctrl Pts',(17.5695003182458,-2.74781004974923,339.079059081822));
#67341=CARTESIAN_POINT('Ctrl Pts',(17.5617514332177,-2.63400190904338,339.155724593771));
#67342=CARTESIAN_POINT('Ctrl Pts',(17.5540025481896,-2.5170133526508,339.227602976877));
#67343=CARTESIAN_POINT('Ctrl Pts',(17.5462536631615,-2.39729094985445,339.294435837714));
#67344=CARTESIAN_POINT('Ctrl Pts',(17.5384965533867,-2.27744147246264,339.361339635641));
#67345=CARTESIAN_POINT('Ctrl Pts',(17.530739443612,-2.15485269401971,339.423187022623));
#67346=CARTESIAN_POINT('Ctrl Pts',(17.5229823338372,-2.02999538623468,339.479765819143));
#67347=CARTESIAN_POINT('Ctrl Pts',(17.515221078911,-1.90507135869679,339.536374849564));
#67348=CARTESIAN_POINT('Ctrl Pts',(17.5074598239849,-1.77787674862338,339.587709533438));
#67349=CARTESIAN_POINT('Ctrl Pts',(17.4996985690587,-1.64890043197093,339.633606632845));
#67350=CARTESIAN_POINT('Ctrl Pts',(17.491924898654,-1.51971779524494,339.679577152654));
#67351=CARTESIAN_POINT('Ctrl Pts',(17.4841512282493,-1.38874813010787,339.720092590514));
#67352=CARTESIAN_POINT('Ctrl Pts',(17.4763775578446,-1.25649439067527,339.755039948171));
#67353=CARTESIAN_POINT('Ctrl Pts',(17.4689657536678,-1.13039709463704,339.78836049792));
#67354=CARTESIAN_POINT('Ctrl Pts',(17.461553949491,-1.00313286223564,339.816619627343));
#67355=CARTESIAN_POINT('Ctrl Pts',(17.4541421453142,-0.875142690937076,
339.839763251751));
#67356=CARTESIAN_POINT('Ctrl Pts',(17.4463670665358,-0.740879340074871,
339.864041214134));
#67357=CARTESIAN_POINT('Ctrl Pts',(17.4385919877574,-0.605392793162187,
339.882766262841));
#67358=CARTESIAN_POINT('Ctrl Pts',(17.430816908979,-0.469182092469226,339.895819770642));
#67359=CARTESIAN_POINT('Ctrl Pts',(17.42305139793,-0.333139007715249,339.90885721527));
#67360=CARTESIAN_POINT('Ctrl Pts',(17.415285886881,-0.196373927621072,339.916236968652));
#67361=CARTESIAN_POINT('Ctrl Pts',(17.407520375832,-0.0593963674799437,
339.917891330035));
#67362=CARTESIAN_POINT('Ctrl Pts',(17.3997625643097,0.0774453790117849,
339.919544051113));
#67363=CARTESIAN_POINT('Ctrl Pts',(17.3920047527875,0.214498797968074,339.91548267254));
#67364=CARTESIAN_POINT('Ctrl Pts',(17.3842469412653,0.351249317506626,339.905691284564));
#67365=CARTESIAN_POINT('Ctrl Pts',(17.3764949677423,0.487896927942431,339.895907264919));
#67366=CARTESIAN_POINT('Ctrl Pts',(17.3687429942193,0.624241704360384,339.880401846525));
#67367=CARTESIAN_POINT('Ctrl Pts',(17.3609910206963,0.759769496860928,339.859211188469));
#67368=CARTESIAN_POINT('Ctrl Pts',(17.3532423301387,0.895239893260885,339.838029504669));
#67369=CARTESIAN_POINT('Ctrl Pts',(17.345493639581,1.02989360852097,339.811167430212));
#67370=CARTESIAN_POINT('Ctrl Pts',(17.3377449490234,1.16322225450981,339.778712907166));
#67371=CARTESIAN_POINT('Ctrl Pts',(17.3299978706456,1.29652316036027,339.746265136554));
#67372=CARTESIAN_POINT('Ctrl Pts',(17.3222507922677,1.4284991657636,339.708227324135));
#67373=CARTESIAN_POINT('Ctrl Pts',(17.3145037138899,1.55865309852318,339.664738318595));
#67374=CARTESIAN_POINT('Ctrl Pts',(17.3067565705841,1.68880812209789,339.621248948575));
#67375=CARTESIAN_POINT('Ctrl Pts',(17.2990094272783,1.8171406718436,339.572308418182));
#67376=CARTESIAN_POINT('Ctrl Pts',(17.2912622839725,1.94317011757803,339.518105018329));
#67377=CARTESIAN_POINT('Ctrl Pts',(17.2835133989445,2.06922789740754,339.463889432401));
#67378=CARTESIAN_POINT('Ctrl Pts',(17.2757645139163,2.19298118388524,339.404408776969));
#67379=CARTESIAN_POINT('Ctrl Pts',(17.2680156288882,2.31397102420308,339.339898750161));
#67380=CARTESIAN_POINT('Ctrl Pts',(17.2602585191135,2.43508928438749,339.275320251744));
#67381=CARTESIAN_POINT('Ctrl Pts',(17.2525014093388,2.55343789371412,339.205701902533));
#67382=CARTESIAN_POINT('Ctrl Pts',(17.244744299564,2.66858366431691,339.131324761991));
#67383=CARTESIAN_POINT('Ctrl Pts',(17.2369830446379,2.78379096513778,339.056907876684));
#67384=CARTESIAN_POINT('Ctrl Pts',(17.2292217897117,2.8957916979206,338.977727358523));
#67385=CARTESIAN_POINT('Ctrl Pts',(17.2214605347856,3.0041840335839,338.894105976326));
#67386=CARTESIAN_POINT('Ctrl Pts',(17.2136868643809,3.11274976165943,338.81035082717));
#67387=CARTESIAN_POINT('Ctrl Pts',(17.2059131939763,3.21769525855827,338.722140869843));
#67388=CARTESIAN_POINT('Ctrl Pts',(17.1981395235716,3.31865332430625,338.629837899352));
#67389=CARTESIAN_POINT('Ctrl Pts',(17.1907277193945,3.41491176780441,338.541831654344));
#67390=CARTESIAN_POINT('Ctrl Pts',(17.1833159152174,3.50754545119424,338.450105082691));
#67391=CARTESIAN_POINT('Ctrl Pts',(17.1759041110404,3.59627024447424,338.35499976024));
#67392=CARTESIAN_POINT('Ctrl Pts',(17.1681290322619,3.68934370417048,338.255233042632));
#67393=CARTESIAN_POINT('Ctrl Pts',(17.1603539534835,3.7784095418604,338.151432713152));
#67394=CARTESIAN_POINT('Ctrl Pts',(17.1525788747051,3.86309794096781,338.043954231093));
#67395=CARTESIAN_POINT('Ctrl Pts',(17.1448133636561,3.94768212560859,337.936608008149));
#67396=CARTESIAN_POINT('Ctrl Pts',(17.137047852607,4.02789935008547,337.825592942548));
#67397=CARTESIAN_POINT('Ctrl Pts',(17.129282341558,4.10341695542925,337.711300859808));
#67398=CARTESIAN_POINT('Ctrl Pts',(17.1215245300358,4.17885968484752,337.597122098001));
#67399=CARTESIAN_POINT('Ctrl Pts',(17.1137667185136,4.24961185408082,337.479673109107));
#67400=CARTESIAN_POINT('Ctrl Pts',(17.1060089069914,4.31538161990733,337.359377997919));
#67401=CARTESIAN_POINT('Ctrl Pts',(17.0982569334684,4.38110189189929,337.239173412618));
#67402=CARTESIAN_POINT('Ctrl Pts',(17.0905049599455,4.44184703676003,337.116127309747));
#67403=CARTESIAN_POINT('Ctrl Pts',(17.0827529864225,4.49736922542266,336.99069161668));
#67404=CARTESIAN_POINT('Ctrl Pts',(17.0750042958649,4.55286790040543,336.865309045705));
#67405=CARTESIAN_POINT('Ctrl Pts',(17.0672556053073,4.60314786067368,336.737539253998));
#67406=CARTESIAN_POINT('Ctrl Pts',(17.0595069147496,4.64800794059774,336.607857346483));
#67407=CARTESIAN_POINT('Ctrl Pts',(17.0517598363718,4.69285868700756,336.478202420373));
#67408=CARTESIAN_POINT('Ctrl Pts',(17.044012757994,4.73229166834846,336.346636538935));
#67409=CARTESIAN_POINT('Ctrl Pts',(17.0362656796161,4.76615459703989,336.213652923869));
#67410=CARTESIAN_POINT('Ctrl Pts',(17.0285185363103,4.80001780953523,336.080668194272));
#67411=CARTESIAN_POINT('Ctrl Pts',(17.0207713930045,4.82831077981538,335.946266086133));
#67412=CARTESIAN_POINT('Ctrl Pts',(17.0130242496987,4.85093174915527,335.810952666644));
#67413=CARTESIAN_POINT('Ctrl Pts',(17.0052753646706,4.8735578041693,335.675608825826));
#67414=CARTESIAN_POINT('Ctrl Pts',(16.9975264796425,4.89050925632769,335.539353651413));
#67415=CARTESIAN_POINT('Ctrl Pts',(16.9897775946145,4.90173594351511,335.402700636394));
#67416=CARTESIAN_POINT('Ctrl Pts',(16.9820204848397,4.91297454682432,335.265902576453));
#67417=CARTESIAN_POINT('Ctrl Pts',(16.974263375065,4.91847621507906,335.128706222555));
#67418=CARTESIAN_POINT('Ctrl Pts',(16.9665062652903,4.91824287436707,334.991627949022));
#67419=CARTESIAN_POINT('Ctrl Pts',(16.9587450103641,4.91800940896526,334.854476425241));
#67420=CARTESIAN_POINT('Ctrl Pts',(16.950983755438,4.91203484511147,334.717443497859));
#67421=CARTESIAN_POINT('Ctrl Pts',(16.9432225005118,4.90037315321631,334.58104174225));
#67422=CARTESIAN_POINT('Ctrl Pts',(16.9354488301072,4.88869280641467,334.444421788285));
#67423=CARTESIAN_POINT('Ctrl Pts',(16.9276751597025,4.87130720156489,334.308435411633));
#67424=CARTESIAN_POINT('Ctrl Pts',(16.9199014892979,4.84832186683064,334.173587186624));
#67425=CARTESIAN_POINT('Ctrl Pts',(16.9124896851208,4.82640650495809,334.045016178931));
#67426=CARTESIAN_POINT('Ctrl Pts',(16.9050778809436,4.7994010753556,333.917480027123));
#67427=CARTESIAN_POINT('Ctrl Pts',(16.8976660767665,4.76743905739485,333.791402508473));
#67428=CARTESIAN_POINT('Ctrl Pts',(16.8898909979881,4.73391048572407,333.659145555068));
#67429=CARTESIAN_POINT('Ctrl Pts',(16.8821159192096,4.69482120955295,333.528075877675));
#67430=CARTESIAN_POINT('Ctrl Pts',(16.8743408404312,4.65027001321283,333.398696822362));
#67431=CARTESIAN_POINT('Ctrl Pts',(16.8665753293822,4.60577363995606,333.269476976213));
#67432=CARTESIAN_POINT('Ctrl Pts',(16.8588098183332,4.55582884591748,333.141943978751));
#67433=CARTESIAN_POINT('Ctrl Pts',(16.8510443072842,4.50058510467792,333.016589609271));
#67434=CARTESIAN_POINT('Ctrl Pts',(16.843286495762,4.4453961377686,332.891359529014));
#67435=CARTESIAN_POINT('Ctrl Pts',(16.8355286842398,4.38491883587396,332.768304133362));
#67436=CARTESIAN_POINT('Ctrl Pts',(16.8277708727176,4.31935190464974,332.647898346946));
#67437=CARTESIAN_POINT('Ctrl Pts',(16.8200188991946,4.2538343146206,332.527583169703));
#67438=CARTESIAN_POINT('Ctrl Pts',(16.8122669256716,4.18323490508244,332.409913974801));
#67439=CARTESIAN_POINT('Ctrl Pts',(16.8045149521486,4.10779959687776,332.295343730824));
#67440=CARTESIAN_POINT('Ctrl Pts',(16.796766261591,4.03239623557089,332.180822007414));
#67441=CARTESIAN_POINT('Ctrl Pts',(16.7890175710333,3.95216126344027,332.069396950426));
#67442=CARTESIAN_POINT('Ctrl Pts',(16.7812688804757,3.86738534408705,331.961494830868));
#67443=CARTESIAN_POINT('Ctrl Pts',(16.7735218020979,3.78262706307192,331.853615161247));
#67444=CARTESIAN_POINT('Ctrl Pts',(16.7657747237201,3.69332995540377,331.749257278277));
#67445=CARTESIAN_POINT('Ctrl Pts',(16.7580276453423,3.59982637018302,331.648816154396));
#67446=CARTESIAN_POINT('Ctrl Pts',(16.7502805020365,3.50632200131228,331.548374188722));
#67447=CARTESIAN_POINT('Ctrl Pts',(16.7425333587307,3.40861135090441,331.451849333705));
#67448=CARTESIAN_POINT('Ctrl Pts',(16.7347862154249,3.30706491417161,331.359601022421));
#67449=CARTESIAN_POINT('Ctrl Pts',(16.7270373303968,3.20549564764379,331.267331971759));
#67450=CARTESIAN_POINT('Ctrl Pts',(16.7192884453687,3.10008916804011,331.179341640801));
#67451=CARTESIAN_POINT('Ctrl Pts',(16.7115395603406,2.99125013697079,331.095950092459));
#67452=CARTESIAN_POINT('Ctrl Pts',(16.7037824505659,2.88229558302938,331.012470031466));
#67453=CARTESIAN_POINT('Ctrl Pts',(16.6960253407912,2.76990151045928,330.933598741838));
#67454=CARTESIAN_POINT('Ctrl Pts',(16.6882682310165,2.65450319175973,330.859614043662));
#67455=CARTESIAN_POINT('Ctrl Pts',(16.6805069760903,2.53904320788847,330.785589810429));
#67456=CARTESIAN_POINT('Ctrl Pts',(16.6727457211641,2.42057611646222,330.716457568682));
#67457=CARTESIAN_POINT('Ctrl Pts',(16.664984466238,2.29956215953446,330.652449317496));
#67458=CARTESIAN_POINT('Ctrl Pts',(16.6572107958333,2.17835461971397,330.588338673969));
#67459=CARTESIAN_POINT('Ctrl Pts',(16.6494371254287,2.05459242607519,330.52936856869));
#67460=CARTESIAN_POINT('Ctrl Pts',(16.641663455024,1.92875699328141,330.475723314897));
#67461=CARTESIAN_POINT('Ctrl Pts',(16.6342516508469,1.80877923015725,330.424575260573));
#67462=CARTESIAN_POINT('Ctrl Pts',(16.6268398466697,1.68691717170806,330.378267572696));
#67463=CARTESIAN_POINT('Ctrl Pts',(16.6194280424926,1.56359941462945,330.33691733581));
#67464=CARTESIAN_POINT('Ctrl Pts',(16.6116529637141,1.4342374869328,330.293540400639));
#67465=CARTESIAN_POINT('Ctrl Pts',(16.6038778849357,1.30286474868591,330.255482083691));
#67466=CARTESIAN_POINT('Ctrl Pts',(16.5961028061573,1.16995793220479,330.222931704552));
#67467=CARTESIAN_POINT('Ctrl Pts',(16.5883372951082,1.03721466602261,330.190421380728));
#67468=CARTESIAN_POINT('Ctrl Pts',(16.5805717840592,0.902941453773608,330.163405600792));
#67469=CARTESIAN_POINT('Ctrl Pts',(16.5728062730102,0.767632731889764,330.142024799216));
#67470=CARTESIAN_POINT('Ctrl Pts',(16.565048461488,0.632458168997517,330.120665196767));
#67471=CARTESIAN_POINT('Ctrl Pts',(16.5572906499658,0.496250523279944,330.104929514653));
#67472=CARTESIAN_POINT('Ctrl Pts',(16.5495328384436,0.359516700022947,330.094907666016));
#67473=CARTESIAN_POINT('Ctrl Pts',(16.5417808649206,0.222885773304215,330.084893359139));
#67474=CARTESIAN_POINT('Ctrl Pts',(16.5340288913975,0.0857298454545552,
330.080584355574));
#67475=CARTESIAN_POINT('Ctrl Pts',(16.5262769178745,-0.0514370907015078,
330.08201898253));
#67476=CARTESIAN_POINT('Ctrl Pts',(16.5185282273169,-0.188545936578672,
330.08345300192));
#67477=CARTESIAN_POINT('Ctrl Pts',(16.5107795367593,-0.325665391450322,
330.090625809819));
#67478=CARTESIAN_POINT('Ctrl Pts',(16.5030308462017,-0.462279700181053,
330.103523660702));
#67479=CARTESIAN_POINT('Ctrl Pts',(16.4952837678239,-0.598865585163827,
330.116418828081));
#67480=CARTESIAN_POINT('Ctrl Pts',(16.4875366894461,-0.734946144157236,
330.13503663246));
#67481=CARTESIAN_POINT('Ctrl Pts',(16.4797896110682,-0.870009383243863,
330.159311336642));
#67482=CARTESIAN_POINT('Ctrl Pts',(16.4720424677624,-1.00507375429034,330.183586244268));
#67483=CARTESIAN_POINT('Ctrl Pts',(16.4642953244566,-1.13912040371388,330.213518077117));
#67484=CARTESIAN_POINT('Ctrl Pts',(16.4565481811508,-1.27164658035278,330.248989787721));
#67485=CARTESIAN_POINT('Ctrl Pts',(16.4487992961227,-1.4042025516898,330.28446947312));
#67486=CARTESIAN_POINT('Ctrl Pts',(16.4410504110946,-1.53523699252033,330.325491413601));
#67487=CARTESIAN_POINT('Ctrl Pts',(16.4333015260665,-1.66426176949551,330.371888524993));
#67488=CARTESIAN_POINT('Ctrl Pts',(16.4255444162918,-1.79342349470222,330.418334882757));
#67489=CARTESIAN_POINT('Ctrl Pts',(16.4177873065171,-1.9205709266335,330.470167675753));
#67490=CARTESIAN_POINT('Ctrl Pts',(16.4100301967423,-2.04523488952654,330.527171218439));
#67491=CARTESIAN_POINT('Ctrl Pts',(16.4022689418162,-2.16996546885528,330.584205221995));
#67492=CARTESIAN_POINT('Ctrl Pts',(16.39450768689,-2.29220958662364,330.646415303743));
#67493=CARTESIAN_POINT('Ctrl Pts',(16.3867464319638,-2.41152308647459,330.713539984334));
#67494=CARTESIAN_POINT('Ctrl Pts',(16.3789727615592,-2.53102744904113,330.780772042539));
#67495=CARTESIAN_POINT('Ctrl Pts',(16.3711990911545,-2.64759149309368,330.85293420385));
#67496=CARTESIAN_POINT('Ctrl Pts',(16.3634254207498,-2.76079970460016,330.929721378876));
#67497=CARTESIAN_POINT('Ctrl Pts',(16.3560136165728,-2.86873804662408,331.00293409243));
#67498=CARTESIAN_POINT('Ctrl Pts',(16.3486018123957,-2.97362572156053,331.080350750147));
#67499=CARTESIAN_POINT('Ctrl Pts',(16.3411900082187,-3.07513233225145,331.161674297087));
#67500=CARTESIAN_POINT('Ctrl Pts',(16.3335141690707,-3.18025497142408,331.245894879599));
#67501=CARTESIAN_POINT('Ctrl Pts',(16.3258383299227,-3.28210183978033,331.334587076303));
#67502=CARTESIAN_POINT('Ctrl Pts',(16.3181624907747,-3.38026131157352,331.427463572197));
#67503=CARTESIAN_POINT('Ctrl Pts',(16.3104961427773,-3.47829940949248,331.520225226599));
#67504=CARTESIAN_POINT('Ctrl Pts',(16.30282979478,-3.57265888958396,331.617160617445));
#67505=CARTESIAN_POINT('Ctrl Pts',(16.2951634467827,-3.66295916811724,331.717940708152));
#67506=CARTESIAN_POINT('Ctrl Pts',(16.2875046312394,-3.75317072348035,331.818621778908));
#67507=CARTESIAN_POINT('Ctrl Pts',(16.2798458156961,-3.83933074426663,331.923139738197));
#67508=CARTESIAN_POINT('Ctrl Pts',(16.2721870001528,-3.92109404713248,332.031127396461));
#67509=CARTESIAN_POINT('Ctrl Pts',(16.264533820451,-4.00279718338208,332.139035590568));
#67510=CARTESIAN_POINT('Ctrl Pts',(16.2568806407491,-4.0801097976907,332.250408084321));
#67511=CARTESIAN_POINT('Ctrl Pts',(16.2492274610473,-4.15272605244681,332.364843572797));
#67512=CARTESIAN_POINT('Ctrl Pts',(16.2415772870008,-4.2253137884121,332.479234118694));
#67513=CARTESIAN_POINT('Ctrl Pts',(16.2339271129543,-4.29320861703059,332.59668492898));
#67514=CARTESIAN_POINT('Ctrl Pts',(16.2262769389078,-4.35614744632711,332.716764907339));
#67515=CARTESIAN_POINT('Ctrl Pts',(16.2186280131359,-4.41907600593063,332.836825292316));
#67516=CARTESIAN_POINT('Ctrl Pts',(16.2109790873639,-4.47704998820667,332.959513636374));
#67517=CARTESIAN_POINT('Ctrl Pts',(16.203330161592,-4.5298520481639,333.084373866266));
#67518=CARTESIAN_POINT('Ctrl Pts',(16.1956807279596,-4.582657613983,333.209242386416));
#67519=CARTESIAN_POINT('Ctrl Pts',(16.1880312943272,-4.63029041903972,333.336282708764));
#67520=CARTESIAN_POINT('Ctrl Pts',(16.1803818606948,-4.67258130975759,333.465018903633));
#67521=CARTESIAN_POINT('Ctrl Pts',(16.172726057847,-4.71490741351321,333.593862289256));
#67522=CARTESIAN_POINT('Ctrl Pts',(16.1650702549992,-4.75188259296183,333.724403985612));
#67523=CARTESIAN_POINT('Ctrl Pts',(16.1574144521513,-4.783387564101,333.856152775016));
#67524=CARTESIAN_POINT('Ctrl Pts',(16.1497554281956,-4.81490579066376,333.987956996497));
#67525=CARTESIAN_POINT('Ctrl Pts',(16.1420964042399,-4.84094914721595,334.120968928487));
#67526=CARTESIAN_POINT('Ctrl Pts',(16.1344373802842,-4.86144977132166,334.254688532614));
#67527=CARTESIAN_POINT('Ctrl Pts',(16.126767680111,-4.88197897206121,334.388594533807));
#67528=CARTESIAN_POINT('Ctrl Pts',(16.1190979799378,-4.89694996133167,334.523209778453));
#67529=CARTESIAN_POINT('Ctrl Pts',(16.1114282797645,-4.90634686277453,334.658029936043));
#67530=CARTESIAN_POINT('Ctrl Pts',(16.1048913120252,-4.91435594268563,334.772938602729));
#67531=CARTESIAN_POINT('Ctrl Pts',(16.0983543442858,-4.9183167050879,334.887995953286));
#67532=CARTESIAN_POINT('Ctrl Pts',(16.0918173765464,-4.91824914986108,335.002891779856));
#67533=CARTESIAN_POINT('',(14.34181737647,-4.91824815738865,334.995742671829));
#67534=CARTESIAN_POINT('Ctrl Pts',(16.0918173765088,-4.91824914986069,335.002891780519));
#67535=CARTESIAN_POINT('Ctrl Pts',(16.0821955756541,-4.91814971490646,335.172007616235));
#67536=CARTESIAN_POINT('Ctrl Pts',(16.0725737747994,-4.90932828771645,335.34086422783));
#67537=CARTESIAN_POINT('Ctrl Pts',(16.0629519739447,-4.89186052670427,335.508806102334));
#67538=CARTESIAN_POINT('Ctrl Pts',(16.0551768951664,-4.87774537092409,335.644514721143));
#67539=CARTESIAN_POINT('Ctrl Pts',(16.0474018163881,-4.85795644605174,335.779849972631));
#67540=CARTESIAN_POINT('Ctrl Pts',(16.0396267376098,-4.83251895341018,335.91429952829));
#67541=CARTESIAN_POINT('Ctrl Pts',(16.0318612265609,-4.80711276322274,336.048583635211));
#67542=CARTESIAN_POINT('Ctrl Pts',(16.0240957155119,-4.77607190757694,336.181983834512));
#67543=CARTESIAN_POINT('Ctrl Pts',(16.016330204463,-4.73947341494043,336.313991937408));
#67544=CARTESIAN_POINT('Ctrl Pts',(16.0085723929409,-4.70291120981595,336.445869153885));
#67545=CARTESIAN_POINT('Ctrl Pts',(16.0008145814189,-4.66080243749055,336.576356646528));
#67546=CARTESIAN_POINT('Ctrl Pts',(15.9930567698968,-4.61327527380629,336.704955808984));
#67547=CARTESIAN_POINT('Ctrl Pts',(15.9853047963738,-4.56578387581976,336.833458196492));
#67548=CARTESIAN_POINT('Ctrl Pts',(15.9775528228508,-4.5128823375158,336.960074717139));
#67549=CARTESIAN_POINT('Ctrl Pts',(15.9698008493279,-4.45474872158878,337.084321685826));
#67550=CARTESIAN_POINT('Ctrl Pts',(15.9620521587703,-4.39663972528277,337.208516035847));
#67551=CARTESIAN_POINT('Ctrl Pts',(15.9543034682128,-4.33330322370507,337.330342476512));
#67552=CARTESIAN_POINT('Ctrl Pts',(15.9465547776553,-4.26496540322883,337.449337292363));
#67553=CARTESIAN_POINT('Ctrl Pts',(15.9388076992775,-4.1966418010069,337.56830735035));
#67554=CARTESIAN_POINT('Ctrl Pts',(15.9310606208997,-4.12331914418319,337.684446616628));
#67555=CARTESIAN_POINT('Ctrl Pts',(15.9233135425219,-4.04526938065443,337.797316339001));
#67556=CARTESIAN_POINT('Ctrl Pts',(15.9155663992162,-3.96721896299357,337.91018700733));
#67557=CARTESIAN_POINT('Ctrl Pts',(15.9078192559104,-3.88444158192184,338.019787755602));
#67558=CARTESIAN_POINT('Ctrl Pts',(15.9000721126046,-3.79725205569251,338.125709501543));
#67559=CARTESIAN_POINT('Ctrl Pts',(15.8923232275766,-3.7100429274066,338.231655060942));
#67560=CARTESIAN_POINT('Ctrl Pts',(15.8845743425486,-3.61841992847046,338.333919670413));
#67561=CARTESIAN_POINT('Ctrl Pts',(15.8768254575206,-3.52273736150397,338.432128282038));
#67562=CARTESIAN_POINT('Ctrl Pts',(15.8690683477459,-3.42695323607219,338.530441133298));
#67563=CARTESIAN_POINT('Ctrl Pts',(15.8613112379712,-3.32710120843979,338.624689106506));
#67564=CARTESIAN_POINT('Ctrl Pts',(15.8535541281965,-3.22357196127322,338.714534543249));
#67565=CARTESIAN_POINT('Ctrl Pts',(15.8457928732704,-3.11998739138741,338.804427990522));
#67566=CARTESIAN_POINT('Ctrl Pts',(15.8380316183443,-3.01272199207038,338.889913970127));
#67567=CARTESIAN_POINT('Ctrl Pts',(15.8302703634182,-2.90219775936294,338.970696567109));
#67568=CARTESIAN_POINT('Ctrl Pts',(15.8224966930136,-2.79149672390278,339.051608389919));
#67569=CARTESIAN_POINT('Ctrl Pts',(15.814723022609,-2.67752676290891,339.127801577814));
#67570=CARTESIAN_POINT('Ctrl Pts',(15.8069493522044,-2.56073769729483,339.199024351936));
#67571=CARTESIAN_POINT('Ctrl Pts',(15.7995375480264,-2.44938519076853,339.266931688796));
#67572=CARTESIAN_POINT('Ctrl Pts',(15.7921257438484,-2.33547038327594,339.330320803664));
#67573=CARTESIAN_POINT('Ctrl Pts',(15.7847139396704,-2.21940051954287,339.389014057434));
#67574=CARTESIAN_POINT('Ctrl Pts',(15.776938860892,-2.09764172604811,339.450584042402));
#67575=CARTESIAN_POINT('Ctrl Pts',(15.7691637821135,-1.97312650308235,339.507180783415));
#67576=CARTESIAN_POINT('Ctrl Pts',(15.7613887033351,-1.84629931650026,339.558548222449));
#67577=CARTESIAN_POINT('Ctrl Pts',(15.753623192286,-1.71962819884547,339.609852450579));
#67578=CARTESIAN_POINT('Ctrl Pts',(15.745857681237,-1.59065113716918,339.655940035183));
#67579=CARTESIAN_POINT('Ctrl Pts',(15.7380921701879,-1.45983716278622,339.696600741031));
#67580=CARTESIAN_POINT('Ctrl Pts',(15.7303343586657,-1.32915289083964,339.73722113167));
#67581=CARTESIAN_POINT('Ctrl Pts',(15.7225765471435,-1.19663570153935,339.772425236311));
#67582=CARTESIAN_POINT('Ctrl Pts',(15.7148187356213,-1.06277424690823,339.802051016244));
#67583=CARTESIAN_POINT('Ctrl Pts',(15.7070667620983,-0.929013527266889,
339.831654501838));
#67584=CARTESIAN_POINT('Ctrl Pts',(15.6993147885753,-0.793910935942417,
339.85568793425));
#67585=CARTESIAN_POINT('Ctrl Pts',(15.6915628150523,-0.657969573995112,
339.874039300436));
#67586=CARTESIAN_POINT('Ctrl Pts',(15.6838141244946,-0.522085783295301,
339.892382894808));
#67587=CARTESIAN_POINT('Ctrl Pts',(15.676065433937,-0.385364315034437,339.905049156849));
#67588=CARTESIAN_POINT('Ctrl Pts',(15.6683167433794,-0.248317519857097,
339.911977348465));
#67589=CARTESIAN_POINT('Ctrl Pts',(15.6605696650016,-0.111299238409945,
339.918904098613));
#67590=CARTESIAN_POINT('Ctrl Pts',(15.6528225866237,0.026043845188808,339.920095133272));
#67591=CARTESIAN_POINT('Ctrl Pts',(15.6450755082458,0.163195608243161,339.91554170524));
#67592=CARTESIAN_POINT('Ctrl Pts',(15.63732836494,0.300348520761203,339.910988239045));
#67593=CARTESIAN_POINT('Ctrl Pts',(15.6295812216343,0.437309718877592,339.900690227103));
#67594=CARTESIAN_POINT('Ctrl Pts',(15.6218340783285,0.573564830359344,339.884691028906));
#67595=CARTESIAN_POINT('Ctrl Pts',(15.6140851933004,0.709850574882936,339.86868823375));
#67596=CARTESIAN_POINT('Ctrl Pts',(15.6063363082722,0.845429528759173,339.846981747379));
#67597=CARTESIAN_POINT('Ctrl Pts',(15.5985874232441,0.979794572714952,339.819666550476));
#67598=CARTESIAN_POINT('Ctrl Pts',(15.5908303134694,1.11430223311664,339.792322360941));
#67599=CARTESIAN_POINT('Ctrl Pts',(15.5830732036947,1.24759302614062,339.759357646905));
#67600=CARTESIAN_POINT('Ctrl Pts',(15.57531609392,1.37917158681665,339.720918215413));
#67601=CARTESIAN_POINT('Ctrl Pts',(15.5675548389938,1.51082045886853,339.682458243118));
#67602=CARTESIAN_POINT('Ctrl Pts',(15.5597935840676,1.6407549053409,339.638517849172));
#67603=CARTESIAN_POINT('Ctrl Pts',(15.5520323291415,1.76849771876267,339.589291762487));
#67604=CARTESIAN_POINT('Ctrl Pts',(15.5442586587368,1.89644487905446,339.539986930106));
#67605=CARTESIAN_POINT('Ctrl Pts',(15.5364849883322,2.02219304175565,339.485379664396));
#67606=CARTESIAN_POINT('Ctrl Pts',(15.5287113179275,2.14528705674561,339.425711977373));
#67607=CARTESIAN_POINT('Ctrl Pts',(15.5212995137507,2.26265101571975,339.368821835537));
#67608=CARTESIAN_POINT('Ctrl Pts',(15.5138877095737,2.37760211350707,339.307331930981));
#67609=CARTESIAN_POINT('Ctrl Pts',(15.5064759053969,2.48977058610487,339.241488593768));
#67610=CARTESIAN_POINT('Ctrl Pts',(15.4987008266184,2.60743676968059,339.17241807846));
#67611=CARTESIAN_POINT('Ctrl Pts',(15.49092574784,2.7224125084653,339.098338315135));
#67612=CARTESIAN_POINT('Ctrl Pts',(15.4831506690616,2.83424195182712,339.019484496923));
#67613=CARTESIAN_POINT('Ctrl Pts',(15.4753851580126,2.94593378193949,338.940727713354));
#67614=CARTESIAN_POINT('Ctrl Pts',(15.4676196469635,3.0544867038435,338.85720878712));
#67615=CARTESIAN_POINT('Ctrl Pts',(15.4598541359145,3.15947010649189,338.769208366313));
#67616=CARTESIAN_POINT('Ctrl Pts',(15.4520963243923,3.26434941779098,338.681295198179));
#67617=CARTESIAN_POINT('Ctrl Pts',(15.4443385128701,3.36566595539473,338.588909627599));
#67618=CARTESIAN_POINT('Ctrl Pts',(15.4365807013479,3.4630190198484,338.492374884039));
#67619=CARTESIAN_POINT('Ctrl Pts',(15.4288287278249,3.56029882303368,338.395912785936));
#67620=CARTESIAN_POINT('Ctrl Pts',(15.4210767543019,3.65362081343013,338.29530800392));
#67621=CARTESIAN_POINT('Ctrl Pts',(15.4133247807789,3.74261854002876,338.190922989721));
#67622=CARTESIAN_POINT('Ctrl Pts',(15.4055760902212,3.83157857603734,338.086582182638));
#67623=CARTESIAN_POINT('Ctrl Pts',(15.3978273996636,3.91621773756256,337.978464624334));
#67624=CARTESIAN_POINT('Ctrl Pts',(15.3900787091059,3.99620768631268,337.866968292527));
#67625=CARTESIAN_POINT('Ctrl Pts',(15.3823316307281,4.07618099248586,337.755495158463));
#67626=CARTESIAN_POINT('Ctrl Pts',(15.3745845523503,4.15150678221994,337.640644966575));
#67627=CARTESIAN_POINT('Ctrl Pts',(15.3668374739724,4.22189839619979,337.522847001835));
#67628=CARTESIAN_POINT('Ctrl Pts',(15.3590903306666,4.29229060012918,337.405048049834));
#67629=CARTESIAN_POINT('Ctrl Pts',(15.3513431873609,4.35774834532099,337.284301611237));
#67630=CARTESIAN_POINT('Ctrl Pts',(15.343596044055,4.41802973736865,337.161063696939));
#67631=CARTESIAN_POINT('Ctrl Pts',(15.3358471590269,4.47832468195305,337.037798076141));
#67632=CARTESIAN_POINT('Ctrl Pts',(15.3280982739988,4.53344078593731,336.912040216083));
#67633=CARTESIAN_POINT('Ctrl Pts',(15.3203493889707,4.58318348926699,336.784267963679));
#67634=CARTESIAN_POINT('Ctrl Pts',(15.3125922791959,4.63297899001591,336.656360092486));
#67635=CARTESIAN_POINT('Ctrl Pts',(15.3048351694211,4.67738955504035,336.526433922717));
#67636=CARTESIAN_POINT('Ctrl Pts',(15.2970780596464,4.7162697261879,336.394984921905));
#67637=CARTESIAN_POINT('Ctrl Pts',(15.2893168047202,4.75517067365573,336.263465678951));
#67638=CARTESIAN_POINT('Ctrl Pts',(15.2815555497941,4.78853524358274,336.130422362419));
#67639=CARTESIAN_POINT('Ctrl Pts',(15.2737942948679,4.8162689433202,335.996361645242));
#67640=CARTESIAN_POINT('Ctrl Pts',(15.2660206244632,4.84404700793884,335.862086474608));
#67641=CARTESIAN_POINT('Ctrl Pts',(15.2582469540585,4.86617613947431,335.726791037033));
#67642=CARTESIAN_POINT('Ctrl Pts',(15.2504732836538,4.88261354314653,335.590989044553));
#67643=CARTESIAN_POINT('Ctrl Pts',(15.2430614794768,4.89828578172304,335.461508667497));
#67644=CARTESIAN_POINT('Ctrl Pts',(15.2356496752998,4.90878424405759,335.331568121346));
#67645=CARTESIAN_POINT('Ctrl Pts',(15.2282378711228,4.914115973838,335.201611651871));
#67646=CARTESIAN_POINT('Ctrl Pts',(15.2204627923444,4.9197090275774,335.065285628706));
#67647=CARTESIAN_POINT('Ctrl Pts',(15.2126877135659,4.91963374373762,334.928511266431));
#67648=CARTESIAN_POINT('Ctrl Pts',(15.2049126347875,4.91384121430612,334.791799176067));
#67649=CARTESIAN_POINT('Ctrl Pts',(15.1971471237385,4.90805581295086,334.655255318633));
#67650=CARTESIAN_POINT('Ctrl Pts',(15.1893816126895,4.89656718089003,334.518773967429));
#67651=CARTESIAN_POINT('Ctrl Pts',(15.1816161016405,4.87937829274619,334.382869107257));
#67652=CARTESIAN_POINT('Ctrl Pts',(15.1738582901183,4.86220644743501,334.247098997151));
#67653=CARTESIAN_POINT('Ctrl Pts',(15.1661004785962,4.83934564221326,334.111904625863));
#67654=CARTESIAN_POINT('Ctrl Pts',(15.158342667074,4.8108508461696,333.977797868125));
#67655=CARTESIAN_POINT('Ctrl Pts',(15.150590693551,4.7823774933636,333.843792029976));
#67656=CARTESIAN_POINT('Ctrl Pts',(15.142838720028,4.7482786696759,333.710872557064));
#67657=CARTESIAN_POINT('Ctrl Pts',(15.135086746505,4.70866086083099,333.579543749291));
#67658=CARTESIAN_POINT('Ctrl Pts',(15.1273380559474,4.66905983015165,333.448270559346));
#67659=CARTESIAN_POINT('Ctrl Pts',(15.1195893653898,4.62394457568195,333.318587068139));
#67660=CARTESIAN_POINT('Ctrl Pts',(15.1118406748322,4.57347208268703,333.190984750926));
#67661=CARTESIAN_POINT('Ctrl Pts',(15.1040935964544,4.52301009091583,333.063408982441));
#67662=CARTESIAN_POINT('Ctrl Pts',(15.0963465180766,4.46719322135376,332.937913889915));
#67663=CARTESIAN_POINT('Ctrl Pts',(15.0885994396988,4.40622734108901,332.814972842013));
#67664=CARTESIAN_POINT('Ctrl Pts',(15.080852296393,4.34526094987146,332.692030763747));
#67665=CARTESIAN_POINT('Ctrl Pts',(15.0731051530872,4.27914563553143,332.571643122982));
#67666=CARTESIAN_POINT('Ctrl Pts',(15.0653580097814,4.20813396441528,332.454260107545));
#67667=CARTESIAN_POINT('Ctrl Pts',(15.0576091247533,4.13710632836795,332.336850701915));
#67668=CARTESIAN_POINT('Ctrl Pts',(15.0498602397253,4.06118034734689,332.222447600163));
#67669=CARTESIAN_POINT('Ctrl Pts',(15.0421113546972,3.9806525654066,332.111473002373));
#67670=CARTESIAN_POINT('Ctrl Pts',(15.0343542449225,3.90003931044644,332.000380614998));
#67671=CARTESIAN_POINT('Ctrl Pts',(15.0265971351478,3.81481472744786,331.892724317787));
#67672=CARTESIAN_POINT('Ctrl Pts',(15.0188400253731,3.7253167498758,331.788894555516));
#67673=CARTESIAN_POINT('Ctrl Pts',(15.0110787704469,3.63577094744606,331.685009309939));
#67674=CARTESIAN_POINT('Ctrl Pts',(15.0033175155208,3.54194746746658,331.584954958687));
#67675=CARTESIAN_POINT('Ctrl Pts',(14.9955562605946,3.44422124662003,331.489085152438));
#67676=CARTESIAN_POINT('Ctrl Pts',(14.98778259019,3.34633869566916,331.393061985743));
#67677=CARTESIAN_POINT('Ctrl Pts',(14.9800089197853,3.24454121865485,331.301237002409));
#67678=CARTESIAN_POINT('Ctrl Pts',(14.9722352493806,3.13923764827562,331.213924188537));
#67679=CARTESIAN_POINT('Ctrl Pts',(14.9648234452034,3.03883598442941,331.130675807154));
#67680=CARTESIAN_POINT('Ctrl Pts',(14.9574116410261,2.93524752737839,331.05152914069));
#67681=CARTESIAN_POINT('Ctrl Pts',(14.9499998368489,2.82884966461261,330.976718672834));
#67682=CARTESIAN_POINT('Ctrl Pts',(14.9422247580704,2.71723692565213,330.898241521102));
#67683=CARTESIAN_POINT('Ctrl Pts',(14.9344496792919,2.60217970605613,330.82428837335));
#67684=CARTESIAN_POINT('Ctrl Pts',(14.9266746005135,2.48408092259265,330.755176678293));
#67685=CARTESIAN_POINT('Ctrl Pts',(14.9189090894644,2.36612746720076,330.686150029576));
#67686=CARTESIAN_POINT('Ctrl Pts',(14.9111435784154,2.24514022924499,330.62195317494));
#67687=CARTESIAN_POINT('Ctrl Pts',(14.9033780673664,2.12155303925051,330.562861759631));
#67688=CARTESIAN_POINT('Ctrl Pts',(14.8956202558442,1.99808838631481,330.503828933632));
#67689=CARTESIAN_POINT('Ctrl Pts',(14.887862444322,1.87202926179428,330.449891640701));
#67690=CARTESIAN_POINT('Ctrl Pts',(14.8801046327997,1.74383585899968,330.401280660948));
#67691=CARTESIAN_POINT('Ctrl Pts',(14.8723526592767,1.61573892580593,330.352706262499));
#67692=CARTESIAN_POINT('Ctrl Pts',(14.8646006857537,1.48551127523392,330.309450337095));
#67693=CARTESIAN_POINT('Ctrl Pts',(14.8568487122307,1.35363460936395,330.27169624423));
#67694=CARTESIAN_POINT('Ctrl Pts',(14.849100021673,1.2218137933401,330.233958140245));
#67695=CARTESIAN_POINT('Ctrl Pts',(14.8413513311153,1.08834572600145,330.201717341892));
#67696=CARTESIAN_POINT('Ctrl Pts',(14.8336026405576,0.953728653109309,330.175107802371));
#67697=CARTESIAN_POINT('Ctrl Pts',(14.8258555621798,0.819139588423713,330.148503799188));
#67698=CARTESIAN_POINT('Ctrl Pts',(14.818108483802,0.683402376906288,330.127528800131));
#67699=CARTESIAN_POINT('Ctrl Pts',(14.8103614054241,0.547026490860267,330.11226585412));
#67700=CARTESIAN_POINT('Ctrl Pts',(14.8026142621183,0.410649461852968,330.097002780192));
#67701=CARTESIAN_POINT('Ctrl Pts',(14.7948671188124,0.273634136089762,330.08745189827));
#67702=CARTESIAN_POINT('Ctrl Pts',(14.7871199755066,0.136495764261796,330.08364444239));
#67703=CARTESIAN_POINT('Ctrl Pts',(14.7793710904785,-0.000673439183687147,
330.079836130514));
#67704=CARTESIAN_POINT('Ctrl Pts',(14.7716222054503,-0.137965353093567,
330.081773824958));
#67705=CARTESIAN_POINT('Ctrl Pts',(14.7638733204222,-0.27486446340625,330.089436632192));
#67706=CARTESIAN_POINT('Ctrl Pts',(14.7561162106475,-0.411908879849051,
330.097107572809));
#67707=CARTESIAN_POINT('Ctrl Pts',(14.7483591008727,-0.548559268966453,
330.110515743102));
#67708=CARTESIAN_POINT('Ctrl Pts',(14.740601991098,-0.684304422229046,330.129588259683));
#67709=CARTESIAN_POINT('Ctrl Pts',(14.7328407361718,-0.820122113361162,
330.148670968007));
#67710=CARTESIAN_POINT('Ctrl Pts',(14.7250794812455,-0.955033220502945,
330.173423983378));
#67711=CARTESIAN_POINT('Ctrl Pts',(14.7173182263193,-1.08853745149997,330.203723394217));
#67712=CARTESIAN_POINT('Ctrl Pts',(14.7095445559147,-1.22225524575765,330.234071274238));
#67713=CARTESIAN_POINT('Ctrl Pts',(14.70177088551,-1.35456128919484,330.269983177016));
#67714=CARTESIAN_POINT('Ctrl Pts',(14.6939972151054,-1.48497030136749,330.311285222307));
#67715=CARTESIAN_POINT('Ctrl Pts',(14.6865854109286,-1.60930874264362,330.350664647452));
#67716=CARTESIAN_POINT('Ctrl Pts',(14.6791736067518,-1.7319225210002,330.394943588288));
#67717=CARTESIAN_POINT('Ctrl Pts',(14.671761802575,-1.85241022807443,330.443931584203));
#67718=CARTESIAN_POINT('Ctrl Pts',(14.6639867237966,-1.97880339659117,330.495320627727));
#67719=CARTESIAN_POINT('Ctrl Pts',(14.6562116450182,-2.10325623976096,330.552054406644));
#67720=CARTESIAN_POINT('Ctrl Pts',(14.6484365662398,-2.22528376680622,330.613965889361));
#67721=CARTESIAN_POINT('Ctrl Pts',(14.6406710551908,-2.34716113121096,330.675801186057));
#67722=CARTESIAN_POINT('Ctrl Pts',(14.6329055441418,-2.46661877255756,330.742801333945));
#67723=CARTESIAN_POINT('Ctrl Pts',(14.6251400330928,-2.58319012428785,330.814750683139));
#67724=CARTESIAN_POINT('Ctrl Pts',(14.6173822215707,-2.69964589518328,330.886628694345));
#67725=CARTESIAN_POINT('Ctrl Pts',(14.6096244100485,-2.81322074105874,330.963445937381));
#67726=CARTESIAN_POINT('Ctrl Pts',(14.6018665985264,-2.92347155699022,331.044940314234));
#67727=CARTESIAN_POINT('Ctrl Pts',(14.5941146250034,-3.03363940568646,331.126373363985));
#67728=CARTESIAN_POINT('Ctrl Pts',(14.5863626514804,-3.14048789036884,331.212476310374));
#67729=CARTESIAN_POINT('Ctrl Pts',(14.5786106779574,-3.24360214349043,331.30294330619));
#67730=CARTESIAN_POINT('Ctrl Pts',(14.5708619873999,-3.34667272766474,331.39337198918));
#67731=CARTESIAN_POINT('Ctrl Pts',(14.5631132968423,-3.44601193246008,331.488160788454));
#67732=CARTESIAN_POINT('Ctrl Pts',(14.5553646062847,-3.54123748440004,331.586963208288));
#67733=CARTESIAN_POINT('Ctrl Pts',(14.5476175279069,-3.63644322386857,331.685745071453));
#67734=CARTESIAN_POINT('Ctrl Pts',(14.539870449529,-3.72753674180896,331.788538612908));
#67735=CARTESIAN_POINT('Ctrl Pts',(14.5321233711512,-3.8141724959158,331.894960349062));
#67736=CARTESIAN_POINT('Ctrl Pts',(14.5243762278455,-3.90080897611358,332.001382977131));
#67737=CARTESIAN_POINT('Ctrl Pts',(14.5166290845397,-3.98298737118907,332.111433557421));
#67738=CARTESIAN_POINT('Ctrl Pts',(14.508881941234,-4.06040258406053,332.22469570716));
#67739=CARTESIAN_POINT('Ctrl Pts',(14.5011330562059,-4.13783520151542,332.337983320636));
#67740=CARTESIAN_POINT('Ctrl Pts',(14.4933841711778,-4.21050228534343,332.454483617685));
#67741=CARTESIAN_POINT('Ctrl Pts',(14.4856352861498,-4.27814243112122,332.573751784846));
#67742=CARTESIAN_POINT('Ctrl Pts',(14.4778781763751,-4.34585437084869,332.693146544472));
#67743=CARTESIAN_POINT('Ctrl Pts',(14.4701210666004,-4.40852852094766,332.815314702294));
#67744=CARTESIAN_POINT('Ctrl Pts',(14.4623639568257,-4.46594952634627,332.93978693077));
#67745=CARTESIAN_POINT('Ctrl Pts',(14.4546027018995,-4.52340121569416,333.064325673224));
#67746=CARTESIAN_POINT('Ctrl Pts',(14.4468414469735,-4.57559401825847,333.191170578366));
#67747=CARTESIAN_POINT('Ctrl Pts',(14.4390801920473,-4.62236139713883,333.319833884183));
#67748=CARTESIAN_POINT('Ctrl Pts',(14.4313065216427,-4.66920358858396,333.448703009357));
#67749=CARTESIAN_POINT('Ctrl Pts',(14.423532851238,-4.71060289521525,333.579395975125));
#67750=CARTESIAN_POINT('Ctrl Pts',(14.4157591808334,-4.74644292354394,333.711410602232));
#67751=CARTESIAN_POINT('Ctrl Pts',(14.408347376656,-4.78061458993301,333.837279916693));
#67752=CARTESIAN_POINT('Ctrl Pts',(14.4009355724785,-4.80973283498304,333.964350334385));
#67753=CARTESIAN_POINT('Ctrl Pts',(14.3935237683011,-4.83374059598813,334.092181233287));
#67754=CARTESIAN_POINT('Ctrl Pts',(14.3819320562446,-4.87128760155276,334.292102728315));
#67755=CARTESIAN_POINT('Ctrl Pts',(14.370340344188,-4.89644018138022,334.49441954545));
#67756=CARTESIAN_POINT('Ctrl Pts',(14.3587486321315,-4.90896216907168,334.697884980309));
#67757=CARTESIAN_POINT('Ctrl Pts',(14.3531048802573,-4.91505885187039,334.796947864525));
#67758=CARTESIAN_POINT('Ctrl Pts',(14.347461128383,-4.91816206293123,334.89628267684));
#67759=CARTESIAN_POINT('Ctrl Pts',(14.3418173765088,-4.91824815738806,334.995742671145));
#67760=CARTESIAN_POINT('',(12.5918173765377,-4.91824995487103,334.99933373343));
#67761=CARTESIAN_POINT('Ctrl Pts',(14.34181737647,-4.91824815738865,334.995742671829));
#67762=CARTESIAN_POINT('Ctrl Pts',(14.334169784482,-4.91836482006042,335.130516395504));
#67763=CARTESIAN_POINT('Ctrl Pts',(14.326522192494,-4.91293755736548,335.265479041663));
#67764=CARTESIAN_POINT('Ctrl Pts',(14.3188746005059,-4.9019465099734,335.400129323919));
#67765=CARTESIAN_POINT('Ctrl Pts',(14.3112337740706,-4.89096518597019,335.534660485857));
#67766=CARTESIAN_POINT('Ctrl Pts',(14.3035929476353,-4.87442990024653,335.668879433724));
#67767=CARTESIAN_POINT('Ctrl Pts',(14.2959521212,-4.85237284976637,335.802284730847));
#67768=CARTESIAN_POINT('Ctrl Pts',(14.2883157222692,-4.83032858032385,335.935612725788));
#67769=CARTESIAN_POINT('Ctrl Pts',(14.2806793233384,-4.8027689747445,336.068127610749));
#67770=CARTESIAN_POINT('Ctrl Pts',(14.2730429244076,-4.76977803608156,336.199333376928));
#67771=CARTESIAN_POINT('Ctrl Pts',(14.2654087960481,-4.73679690679058,336.330500130996));
#67772=CARTESIAN_POINT('Ctrl Pts',(14.2577746676886,-4.69838775293967,336.460358149181));
#67773=CARTESIAN_POINT('Ctrl Pts',(14.2501405393291,-4.65468552394845,336.588422404666));
#67774=CARTESIAN_POINT('Ctrl Pts',(14.2425069150414,-4.61098618055987,336.716478204231));
#67775=CARTESIAN_POINT('Ctrl Pts',(14.2348732907536,-4.56199458734832,336.842740094793));
#67776=CARTESIAN_POINT('Ctrl Pts',(14.2272396664659,-4.50789514943345,336.96673953136));
#67777=CARTESIAN_POINT('Ctrl Pts',(14.2196047803676,-4.4537867690765,337.090759464587));
#67778=CARTESIAN_POINT('Ctrl Pts',(14.2119698942693,-4.39456902696439,337.21251583062));
#67779=CARTESIAN_POINT('Ctrl Pts',(14.204335008171,-4.33047368489916,337.331561864265));
#67780=CARTESIAN_POINT('Ctrl Pts',(14.196692498292,-4.26631434072249,337.450726770784));
#67781=CARTESIAN_POINT('Ctrl Pts',(14.189049988413,-4.19726786124331,337.567175584188));
#67782=CARTESIAN_POINT('Ctrl Pts',(14.181407478534,-4.12361119678431,337.680487597482));
#67783=CARTESIAN_POINT('Ctrl Pts',(14.1737610855969,-4.04991710834897,337.793857183111));
#67784=CARTESIAN_POINT('Ctrl Pts',(14.1661146926598,-3.97160840464576,337.904086466819));
#67785=CARTESIAN_POINT('Ctrl Pts',(14.1584682997227,-3.88900346642052,338.010786458829));
#67786=CARTESIAN_POINT('Ctrl Pts',(14.1508099918539,-3.80626980970002,338.117652715263));
#67787=CARTESIAN_POINT('Ctrl Pts',(14.1431516839851,-3.71922680601404,338.220978386607));
#67788=CARTESIAN_POINT('Ctrl Pts',(14.1354933761164,-3.62823138199011,338.320409628531));
#67789=CARTESIAN_POINT('Ctrl Pts',(14.1287574954199,-3.54819616655459,338.407864585237));
#67790=CARTESIAN_POINT('Ctrl Pts',(14.1220216147235,-3.4651039971073,338.492307206725));
#67791=CARTESIAN_POINT('Ctrl Pts',(14.1152857340271,-3.37921856485625,338.573522765204));
#67792=CARTESIAN_POINT('Ctrl Pts',(14.1075106552484,-3.28008290141734,338.667268096168));
#67793=CARTESIAN_POINT('Ctrl Pts',(14.0997355764698,-3.17688664381494,338.7570331465));
#67794=CARTESIAN_POINT('Ctrl Pts',(14.0919604976912,-3.06998274485364,338.842445706682));
#67795=CARTESIAN_POINT('Ctrl Pts',(14.084194986642,-2.96321039794615,338.927753161271));
#67796=CARTESIAN_POINT('Ctrl Pts',(14.0764294755928,-2.85273979018041,339.008718540995));
#67797=CARTESIAN_POINT('Ctrl Pts',(14.0686639645436,-2.73896049078447,339.085006547415));
#67798=CARTESIAN_POINT('Ctrl Pts',(14.0609061530213,-2.62529400389491,339.161218914054));
#67799=CARTESIAN_POINT('Ctrl Pts',(14.0531483414989,-2.50832567647116,339.23276292026));
#67800=CARTESIAN_POINT('Ctrl Pts',(14.0453905299765,-2.38847763202022,339.29934386434));
#67801=CARTESIAN_POINT('Ctrl Pts',(14.0376385564533,-2.26871977702333,339.365874704148));
#67802=CARTESIAN_POINT('Ctrl Pts',(14.0298865829301,-2.14608685877421,339.427449726832));
#67803=CARTESIAN_POINT('Ctrl Pts',(14.0221346094069,-2.02102912007301,339.483818055889));
#67804=CARTESIAN_POINT('Ctrl Pts',(14.0143859188492,-1.89602434339856,339.540162512925));
#67805=CARTESIAN_POINT('Ctrl Pts',(14.0066372282914,-1.76859714433594,339.591304501714));
#67806=CARTESIAN_POINT('Ctrl Pts',(13.9988885377336,-1.63922125794991,339.637039651543));
#67807=CARTESIAN_POINT('Ctrl Pts',(13.9911414593556,-1.5098722892976,339.682765285793));
#67808=CARTESIAN_POINT('Ctrl Pts',(13.9833943809775,-1.37857580806597,339.723086188472));
#67809=CARTESIAN_POINT('Ctrl Pts',(13.9756473025995,-1.24582399588696,339.757846743409));
#67810=CARTESIAN_POINT('Ctrl Pts',(13.9679001592936,-1.11307107112008,339.792607589674));
#67811=CARTESIAN_POINT('Ctrl Pts',(13.9601530159876,-0.97886316920421,339.821807896238));
#67812=CARTESIAN_POINT('Ctrl Pts',(13.9524058726817,-0.843705658329049,
339.845342487854));
#67813=CARTESIAN_POINT('Ctrl Pts',(13.9446569876534,-0.708517761175785,
339.868882370546));
#67814=CARTESIAN_POINT('Ctrl Pts',(13.9369081026251,-0.572380215242268,
339.886753936584));
#67815=CARTESIAN_POINT('Ctrl Pts',(13.9291592175968,-0.43580616291851,339.898903555987));
#67816=CARTESIAN_POINT('Ctrl Pts',(13.9214021078219,-0.299087149484731,
339.911066071122));
#67817=CARTESIAN_POINT('Ctrl Pts',(13.913644998047,-0.161931094102431,339.917494472878));
#67818=CARTESIAN_POINT('Ctrl Pts',(13.9058878882721,-0.0248543723207421,
339.918187198824));
#67819=CARTESIAN_POINT('Ctrl Pts',(13.8981266333458,0.112295598878295,339.918880294941));
#67820=CARTESIAN_POINT('Ctrl Pts',(13.8903653784194,0.2493657615929,339.913831622414));
#67821=CARTESIAN_POINT('Ctrl Pts',(13.8826041234931,0.385843187537344,339.903091687612));
#67822=CARTESIAN_POINT('Ctrl Pts',(13.8748304530883,0.522538932885219,339.892334572415));
#67823=CARTESIAN_POINT('Ctrl Pts',(13.8670567826835,0.658639658458579,339.875868049097));
#67824=CARTESIAN_POINT('Ctrl Pts',(13.8592831122787,0.793640088523946,339.853794234657));
#67825=CARTESIAN_POINT('Ctrl Pts',(13.8518713081035,0.92235621605493,339.832747961595));
#67826=CARTESIAN_POINT('Ctrl Pts',(13.8444595039283,1.0500718983481,339.806604745773));
#67827=CARTESIAN_POINT('Ctrl Pts',(13.8370476997531,1.17636246605466,339.7754952006));
#67828=CARTESIAN_POINT('Ctrl Pts',(13.8292726209747,1.30884291071678,339.74286088394));
#67829=CARTESIAN_POINT('Ctrl Pts',(13.8214975421965,1.44017367297856,339.70465796878));
#67830=CARTESIAN_POINT('Ctrl Pts',(13.8137224634181,1.56985075090098,339.660981836737));
#67831=CARTESIAN_POINT('Ctrl Pts',(13.8059569523693,1.6993682529232,339.617359450956));
#67832=CARTESIAN_POINT('Ctrl Pts',(13.7981914413203,1.82723575271371,339.568277372861));
#67833=CARTESIAN_POINT('Ctrl Pts',(13.7904259302715,1.95296047239978,339.513881750306));
#67834=CARTESIAN_POINT('Ctrl Pts',(13.7826681187493,2.07856053566083,339.459540061168));
#67835=CARTESIAN_POINT('Ctrl Pts',(13.7749103072272,2.20202169041072,339.399895466182));
#67836=CARTESIAN_POINT('Ctrl Pts',(13.7671524957051,2.3228676804586,339.335143458016));
#67837=CARTESIAN_POINT('Ctrl Pts',(13.7594005221822,2.44362273006622,339.27044017779));
#67838=CARTESIAN_POINT('Ctrl Pts',(13.7516485486593,2.56176618902336,339.200637318527));
#67839=CARTESIAN_POINT('Ctrl Pts',(13.7438965751364,2.67684343771271,339.125977735334));
#67840=CARTESIAN_POINT('Ctrl Pts',(13.7361478845789,2.79187195111922,339.051349770519));
#67841=CARTESIAN_POINT('Ctrl Pts',(13.7283991940213,2.90383650973961,338.971869384951));
#67842=CARTESIAN_POINT('Ctrl Pts',(13.7206505034638,3.01230888865644,338.887824355835));
#67843=CARTESIAN_POINT('Ctrl Pts',(13.7129034250861,3.12075869898872,338.803796812989));
#67844=CARTESIAN_POINT('Ctrl Pts',(13.7051563467084,3.22571746604281,338.71520675489));
#67845=CARTESIAN_POINT('Ctrl Pts',(13.6974092683307,3.32678798113983,338.622383854735));
#67846=CARTESIAN_POINT('Ctrl Pts',(13.689662125025,3.42785934330497,338.529560176634));
#67847=CARTESIAN_POINT('Ctrl Pts',(13.6819149817193,3.52504210062894,338.432503850113));
#67848=CARTESIAN_POINT('Ctrl Pts',(13.6741678384136,3.6179743252772,338.331582933702));
#67849=CARTESIAN_POINT('Ctrl Pts',(13.6664189533856,3.71092744306256,338.230639328127));
#67850=CARTESIAN_POINT('Ctrl Pts',(13.6586700683576,3.79962786189173,338.125829691243));
#67851=CARTESIAN_POINT('Ctrl Pts',(13.6509211833296,3.88375279237792,338.017556513174));
#67852=CARTESIAN_POINT('Ctrl Pts',(13.643164073555,3.96796701393473,337.909168412834));
#67853=CARTESIAN_POINT('Ctrl Pts',(13.6354069637804,4.04759580569605,337.797309736825));
#67854=CARTESIAN_POINT('Ctrl Pts',(13.6276498540057,4.12235841333991,337.682413870838));
#67855=CARTESIAN_POINT('Ctrl Pts',(13.6198885990797,4.19716097173069,337.567456608175));
#67856=CARTESIAN_POINT('Ctrl Pts',(13.6121273441536,4.26709196542435,337.449459257694));
#67857=CARTESIAN_POINT('Ctrl Pts',(13.6043660892276,4.33191629137552,337.328880483626));
#67858=CARTESIAN_POINT('Ctrl Pts',(13.596592418823,4.39684431512211,337.208108822817));
#67859=CARTESIAN_POINT('Ctrl Pts',(13.5888187484184,4.45664917643405,337.08474783849));
#67860=CARTESIAN_POINT('Ctrl Pts',(13.5810450780138,4.51114331398031,336.959277689158));
#67861=CARTESIAN_POINT('Ctrl Pts',(13.5736332738356,4.56310073632166,336.839648205443));
#67862=CARTESIAN_POINT('Ctrl Pts',(13.5662214696574,4.61023063243016,336.718101769282));
#67863=CARTESIAN_POINT('Ctrl Pts',(13.5588096654792,4.65241302495513,336.595066176598));
#67864=CARTESIAN_POINT('Ctrl Pts',(13.5510345867012,4.69666290218368,336.466000243039));
#67865=CARTESIAN_POINT('Ctrl Pts',(13.5432595079232,4.7356078670183,336.334887613764));
#67866=CARTESIAN_POINT('Ctrl Pts',(13.5354844291451,4.76905538352588,336.202203731221));
#67867=CARTESIAN_POINT('Ctrl Pts',(13.5277189180965,4.80246174073503,336.069683124643));
#67868=CARTESIAN_POINT('Ctrl Pts',(13.519953407048,4.83038401531723,335.935595487355));
#67869=CARTESIAN_POINT('Ctrl Pts',(13.5121878959994,4.85267843573541,335.800434295772));
#67870=CARTESIAN_POINT('Ctrl Pts',(13.5044300844776,4.87495075117082,335.665407116904));
#67871=CARTESIAN_POINT('Ctrl Pts',(13.4966722729558,4.89160625382082,335.5293088852));
#67872=CARTESIAN_POINT('Ctrl Pts',(13.488914461434,4.90255160808747,335.39264588695));
#67873=CARTESIAN_POINT('Ctrl Pts',(13.4811624879114,4.91348872562795,335.25608573194));
#67874=CARTESIAN_POINT('Ctrl Pts',(13.4734105143888,4.91872421680874,335.118962044394));
#67875=CARTESIAN_POINT('Ctrl Pts',(13.4656585408661,4.91821628290792,334.981788546479));
#67876=CARTESIAN_POINT('Ctrl Pts',(13.4579098503089,4.91770856411742,334.844673141622));
#67877=CARTESIAN_POINT('Ctrl Pts',(13.4501611597518,4.91146225945038,334.70750835841));
#67878=CARTESIAN_POINT('Ctrl Pts',(13.4424124691946,4.89948762982278,334.57081003307));
#67879=CARTESIAN_POINT('Ctrl Pts',(13.4346653908171,4.88751549161688,334.434140148958));
#67880=CARTESIAN_POINT('Ctrl Pts',(13.4269183124397,4.86981743316448,334.297936918816));
#67881=CARTESIAN_POINT('Ctrl Pts',(13.4191712340623,4.84645573128148,334.16271276898));
#67882=CARTESIAN_POINT('Ctrl Pts',(13.4114240907569,4.82309383360491,334.027487485835));
#67883=CARTESIAN_POINT('Ctrl Pts',(13.4036769474515,4.79406826436447,333.893241684531));
#67884=CARTESIAN_POINT('Ctrl Pts',(13.3959298041461,4.75949267191243,333.760478895496));
#67885=CARTESIAN_POINT('Ctrl Pts',(13.3881809191184,4.724909306133,333.627686258566));
#67886=CARTESIAN_POINT('Ctrl Pts',(13.3804320340907,4.68477353272363,333.496377675542));
#67887=CARTESIAN_POINT('Ctrl Pts',(13.372683149063,4.6392491343566,333.367042397405));
#67888=CARTESIAN_POINT('Ctrl Pts',(13.3649260392887,4.59367641592292,333.237569841469));
#67889=CARTESIAN_POINT('Ctrl Pts',(13.3571689295144,4.54270377719256,333.110075143636));
#67890=CARTESIAN_POINT('Ctrl Pts',(13.3494118197401,4.48654372916801,332.985028926073));
#67891=CARTESIAN_POINT('Ctrl Pts',(13.3416505648143,4.43035367100932,332.859915887809));
#67892=CARTESIAN_POINT('Ctrl Pts',(13.3338893098885,4.36897085495944,332.73725428627));
#67893=CARTESIAN_POINT('Ctrl Pts',(13.3261280549627,4.30265375380793,332.617490034157));
#67894=CARTESIAN_POINT('Ctrl Pts',(13.3183543845584,4.23623056690736,332.497534198272));
#67895=CARTESIAN_POINT('Ctrl Pts',(13.3105807141541,4.16485752546075,332.380485307445));
#67896=CARTESIAN_POINT('Ctrl Pts',(13.3028070437499,4.08883690480455,332.266760927323));
#67897=CARTESIAN_POINT('Ctrl Pts',(13.2953952395683,4.01635506228222,332.158330444386));
#67898=CARTESIAN_POINT('Ctrl Pts',(13.2879834353868,3.9396487620986,332.052922158287));
#67899=CARTESIAN_POINT('Ctrl Pts',(13.2805716312053,3.85901282034596,331.950868465463));
#67900=CARTESIAN_POINT('Ctrl Pts',(13.2727965524257,3.7744246709235,331.8438128172));
#67901=CARTESIAN_POINT('Ctrl Pts',(13.265021473646,3.68524461891527,331.740110598454));
#67902=CARTESIAN_POINT('Ctrl Pts',(13.2572463948663,3.59176828177825,331.64018100599));
#67903=CARTESIAN_POINT('Ctrl Pts',(13.2494808838161,3.49840697322505,331.540374383251));
#67904=CARTESIAN_POINT('Ctrl Pts',(13.2417153727659,3.40076016332989,331.444331432359));
#67905=CARTESIAN_POINT('Ctrl Pts',(13.2339498617157,3.29916502390904,331.352440102272));
#67906=CARTESIAN_POINT('Ctrl Pts',(13.2261920501923,3.19767061636477,331.260639882706));
#67907=CARTESIAN_POINT('Ctrl Pts',(13.2184342386689,3.09223595794855,331.172983352695));
#67908=CARTESIAN_POINT('Ctrl Pts',(13.2106764271455,2.98323628635612,331.089822980699));
#67909=CARTESIAN_POINT('Ctrl Pts',(13.2029244536213,2.87431864047283,331.00672518952));
#67910=CARTESIAN_POINT('Ctrl Pts',(13.195172480097,2.7618416308738,330.928117057797));
#67911=CARTESIAN_POINT('Ctrl Pts',(13.1874205065728,2.64621463780284,330.854311739508));
#67912=CARTESIAN_POINT('Ctrl Pts',(13.1796718160139,2.53063661283239,330.780537677816));
#67913=CARTESIAN_POINT('Ctrl Pts',(13.1719231254551,2.41191158645138,330.711562593956));
#67914=CARTESIAN_POINT('Ctrl Pts',(13.1641744348963,2.29047888911821,330.647657007886));
#67915=CARTESIAN_POINT('Ctrl Pts',(13.1564273565173,2.1690714568721,330.583764717907));
#67916=CARTESIAN_POINT('Ctrl Pts',(13.1486802781382,2.04495781990597,330.524940009662));
#67917=CARTESIAN_POINT('Ctrl Pts',(13.1409331997592,1.91860259001596,330.471407816541));
#67918=CARTESIAN_POINT('Ctrl Pts',(13.1331860564521,1.79224630114725,330.417875174769));
#67919=CARTESIAN_POINT('Ctrl Pts',(13.1254389131451,1.66364874178968,330.369635289073));
#67920=CARTESIAN_POINT('Ctrl Pts',(13.1176917698381,1.53329484306708,330.326865079337));
#67921=CARTESIAN_POINT('Ctrl Pts',(13.1099428848088,1.40291163802091,330.284085253949));
#67922=CARTESIAN_POINT('Ctrl Pts',(13.1021939997795,1.27077167919907,330.246777673318));
#67923=CARTESIAN_POINT('Ctrl Pts',(13.0944451147502,1.13737502039215,330.21506937088));
#67924=CARTESIAN_POINT('Ctrl Pts',(13.0866880049744,1.0038367729939,330.183327412923));
#67925=CARTESIAN_POINT('Ctrl Pts',(13.0789308951985,0.869039541950893,330.157196695657));
#67926=CARTESIAN_POINT('Ctrl Pts',(13.0711737854226,0.733494085379904,330.136753194705));
#67927=CARTESIAN_POINT('Ctrl Pts',(13.0634125304953,0.597876197650747,330.116298769399));
#67928=CARTESIAN_POINT('Ctrl Pts',(13.0556512755679,0.461509676107818,330.101537658065));
#67929=CARTESIAN_POINT('Ctrl Pts',(13.0478900206406,0.32490937271186,330.092493814367));
#67930=CARTESIAN_POINT('Ctrl Pts',(13.0401163502348,0.188090553348807,330.083435503467));
#67931=CARTESIAN_POINT('Ctrl Pts',(13.032342679829,0.0510375957853707,330.080112745629));
#67932=CARTESIAN_POINT('Ctrl Pts',(13.0245690094232,-0.0857347815890412,
330.082497319805));
#67933=CARTESIAN_POINT('Ctrl Pts',(13.0171572052593,-0.216140371641192,
330.084770891475));
#67934=CARTESIAN_POINT('Ctrl Pts',(13.0097454010953,-0.346290628336729,
330.092232383816));
#67935=CARTESIAN_POINT('Ctrl Pts',(13.0023335969313,-0.475746490519923,
330.104813758471));
#67936=CARTESIAN_POINT('Ctrl Pts',(12.9945585181539,-0.611547370360238,
330.118011783797));
#67937=CARTESIAN_POINT('Ctrl Pts',(12.9867834393765,-0.747013221750016,
330.136885971101));
#67938=CARTESIAN_POINT('Ctrl Pts',(12.9790083605991,-0.881631557619445,
330.161414580778));
#67939=CARTESIAN_POINT('Ctrl Pts',(12.9712428495511,-1.01608423705616,330.185913006439));
#67940=CARTESIAN_POINT('Ctrl Pts',(12.9634773385032,-1.14969109522095,330.216051940399));
#67941=CARTESIAN_POINT('Ctrl Pts',(12.9557118274552,-1.28194343454362,330.251757789125));
#67942=CARTESIAN_POINT('Ctrl Pts',(12.9479540159341,-1.4140646452867,330.287428235399));
#67943=CARTESIAN_POINT('Ctrl Pts',(12.9401962044128,-1.54483363492008,330.328654510873));
#67944=CARTESIAN_POINT('Ctrl Pts',(12.9324383928917,-1.6737509425495,330.375311811072));
#67945=CARTESIAN_POINT('Ctrl Pts',(12.9246864193697,-1.80257123581654,330.421934000172));
#67946=CARTESIAN_POINT('Ctrl Pts',(12.9169344458478,-1.92954225460882,330.473978946502));
#67947=CARTESIAN_POINT('Ctrl Pts',(12.9091824723258,-2.05417912192438,330.531271859069));
#67948=CARTESIAN_POINT('Ctrl Pts',(12.9014337817692,-2.17876320545364,330.588540508053));
#67949=CARTESIAN_POINT('Ctrl Pts',(12.8936850912126,-2.30101474918216,330.65105253993));
#67950=CARTESIAN_POINT('Ctrl Pts',(12.8859364006559,-2.42046852018654,330.718584906215));
#67951=CARTESIAN_POINT('Ctrl Pts',(12.8781893222791,-2.539897437836,330.786103221828));
#67952=CARTESIAN_POINT('Ctrl Pts',(12.8704422439023,-2.65652940055067,330.858639601976));
#67953=CARTESIAN_POINT('Ctrl Pts',(12.8626951655255,-2.76992382894213,330.935925069052));
#67954=CARTESIAN_POINT('Ctrl Pts',(12.8549480222207,-2.88331920768811,331.013211183855));
#67955=CARTESIAN_POINT('Ctrl Pts',(12.8472008789158,-2.99347667500141,331.095246244836));
#67956=CARTESIAN_POINT('Ctrl Pts',(12.839453735611,-3.09998503112164,331.181718204569));
#67957=CARTESIAN_POINT('Ctrl Pts',(12.8317048505839,-3.20651733258199,331.268209605034));
#67958=CARTESIAN_POINT('Ctrl Pts',(12.8239559655567,-3.30939858695373,331.359139642861));
#67959=CARTESIAN_POINT('Ctrl Pts',(12.8162070805296,-3.40825136131104,331.454156557232));
#67960=CARTESIAN_POINT('Ctrl Pts',(12.8084499707558,-3.50720905902468,331.549274323537));
#67961=CARTESIAN_POINT('Ctrl Pts',(12.800692860982,-3.6021294530234,331.648487360358));
#67962=CARTESIAN_POINT('Ctrl Pts',(12.7929357512082,-3.69267225326139,331.751407275066));
#67963=CARTESIAN_POINT('Ctrl Pts',(12.785174496283,-3.78326343667678,331.854382186886));
#67964=CARTESIAN_POINT('Ctrl Pts',(12.7774132413578,-3.86947211962819,331.961067619721));
#67965=CARTESIAN_POINT('Ctrl Pts',(12.7696519864326,-3.95099954302915,332.071043586278));
#67966=CARTESIAN_POINT('Ctrl Pts',(12.7618783160288,-4.03265738373829,332.181195478541));
#67967=CARTESIAN_POINT('Ctrl Pts',(12.7541046456251,-4.10961878113251,332.294648099478));
#67968=CARTESIAN_POINT('Ctrl Pts',(12.7463309752213,-4.18162892323844,332.410953339386));
#67969=CARTESIAN_POINT('Ctrl Pts',(12.7389191710333,-4.25028697601363,332.521844542571));
#67970=CARTESIAN_POINT('Ctrl Pts',(12.7315073668454,-4.31444422005825,332.635328512064));
#67971=CARTESIAN_POINT('Ctrl Pts',(12.7240955626574,-4.37392026909127,332.75099921251));
#67972=CARTESIAN_POINT('Ctrl Pts',(12.7158245986272,-4.44029064932982,332.880078203058));
#67973=CARTESIAN_POINT('Ctrl Pts',(12.707553634597,-4.50102026115738,333.012246799271));
#67974=CARTESIAN_POINT('Ctrl Pts',(12.6992826705668,-4.55582953802183,333.147002352136));
#67975=CARTESIAN_POINT('Ctrl Pts',(12.6910273949352,-4.61053485242457,333.281502300115));
#67976=CARTESIAN_POINT('Ctrl Pts',(12.6827721193036,-4.65934209626467,333.418579133346));
#67977=CARTESIAN_POINT('Ctrl Pts',(12.674516843672,-4.70201793527007,333.557706548965));
#67978=CARTESIAN_POINT('Ctrl Pts',(12.6662830903639,-4.74458251412426,333.696471245592));
#67979=CARTESIAN_POINT('Ctrl Pts',(12.6580493370559,-4.78104747464785,333.837275562377));
#67980=CARTESIAN_POINT('Ctrl Pts',(12.6498155837478,-4.81122811232962,333.979575032827));
#67981=CARTESIAN_POINT('Ctrl Pts',(12.6415950492509,-4.84136029675637,334.12164604977));
#67982=CARTESIAN_POINT('Ctrl Pts',(12.6333745147539,-4.86522819715475,334.265207130258));
#67983=CARTESIAN_POINT('Ctrl Pts',(12.625153980257,-4.88269671584385,334.409698514666));
#67984=CARTESIAN_POINT('Ctrl Pts',(12.6169511416217,-4.90012763107903,334.553878860959));
#67985=CARTESIAN_POINT('Ctrl Pts',(12.6087483029864,-4.91118659541477,334.698985205665));
#67986=CARTESIAN_POINT('Ctrl Pts',(12.6005454643512,-4.91578952414677,334.844448025442));
#67987=CARTESIAN_POINT('Ctrl Pts',(12.5976361017467,-4.91742207957295,334.896040420103));
#67988=CARTESIAN_POINT('Ctrl Pts',(12.5947267391421,-4.91824295710074,334.947677557148));
#67989=CARTESIAN_POINT('Ctrl Pts',(12.5918173765376,-4.91824995487103,334.99933373343));
#67990=CARTESIAN_POINT('',(10.8418173764557,-4.91824791560711,335.004528037799));
#67991=CARTESIAN_POINT('Ctrl Pts',(12.5918173765088,-4.9182499548711,334.999333733942));
#67992=CARTESIAN_POINT('Ctrl Pts',(12.5837801713581,-4.91826928641542,335.142035535853));
#67993=CARTESIAN_POINT('Ctrl Pts',(12.5757429662075,-4.91207359840828,335.284645054202));
#67994=CARTESIAN_POINT('Ctrl Pts',(12.5677057610568,-4.89971296326426,335.426609821875));
#67995=CARTESIAN_POINT('Ctrl Pts',(12.5596606460499,-4.88734016333841,335.568714304894));
#67996=CARTESIAN_POINT('Ctrl Pts',(12.551615531043,-4.8687903455266,335.710172426349));
#67997=CARTESIAN_POINT('Ctrl Pts',(12.5435704160361,-4.84416512844621,335.850439457484));
#67998=CARTESIAN_POINT('Ctrl Pts',(12.5354276753984,-4.81924108998801,335.992408596965));
#67999=CARTESIAN_POINT('Ctrl Pts',(12.5272849347606,-4.78809332468382,336.13315719114));
#68000=CARTESIAN_POINT('Ctrl Pts',(12.5191421941229,-4.75087933018811,336.272135469394));
#68001=CARTESIAN_POINT('Ctrl Pts',(12.5110723034859,-4.71399827513448,336.4098703619));
#68002=CARTESIAN_POINT('Ctrl Pts',(12.5030024128489,-4.67115927453661,336.545866181394));
#68003=CARTESIAN_POINT('Ctrl Pts',(12.4949325222119,-4.62256446220816,336.679607351505));
#68004=CARTESIAN_POINT('Ctrl Pts',(12.4867533565739,-4.57331162384106,336.815159520942));
#68005=CARTESIAN_POINT('Ctrl Pts',(12.4785741909358,-4.51814612085063,336.94839519872));
#68006=CARTESIAN_POINT('Ctrl Pts',(12.4703950252977,-4.45732674295449,337.078802869212));
#68007=CARTESIAN_POINT('Ctrl Pts',(12.4622158596597,-4.39650736505842,337.209210539704));
#68008=CARTESIAN_POINT('Ctrl Pts',(12.4540366940216,-4.33003433733722,337.336789909527));
#68009=CARTESIAN_POINT('Ctrl Pts',(12.4458575283836,-4.25821197560238,337.461059494067));
#68010=CARTESIAN_POINT('Ctrl Pts',(12.438082449597,-4.18993795526356,337.579189613119));
#68011=CARTESIAN_POINT('Ctrl Pts',(12.4303073708104,-4.1166366253402,337.694663189806));
#68012=CARTESIAN_POINT('Ctrl Pts',(12.4225322920238,-4.03854009400104,337.807022794999));
#68013=CARTESIAN_POINT('Ctrl Pts',(12.4147667809667,-3.96053966541536,337.919244134546));
#68014=CARTESIAN_POINT('Ctrl Pts',(12.4070012699095,-3.87775599726861,338.02835880917));
#68015=CARTESIAN_POINT('Ctrl Pts',(12.3992357588523,-3.79046682216597,338.133934321673));
#68016=CARTESIAN_POINT('Ctrl Pts',(12.3914779473219,-3.70326419453443,338.239405155748));
#68017=CARTESIAN_POINT('Ctrl Pts',(12.3837201357915,-3.61156519743657,338.341343511684));
#68018=CARTESIAN_POINT('Ctrl Pts',(12.3759623242612,-3.51569034595541,338.439346515525));
#68019=CARTESIAN_POINT('Ctrl Pts',(12.36821035073,-3.41988764334016,338.537275768998));
#68020=CARTESIAN_POINT('Ctrl Pts',(12.3604583771988,-3.3199156134992,338.63127528677));
#68021=CARTESIAN_POINT('Ctrl Pts',(12.3527064036676,-3.21613422425481,338.720976177574));
#68022=CARTESIAN_POINT('Ctrl Pts',(12.3449577131019,-3.11239678649104,338.810639079998));
#68023=CARTESIAN_POINT('Ctrl Pts',(12.3372090225361,-3.00485349310262,338.896006721174));
#68024=CARTESIAN_POINT('Ctrl Pts',(12.3294603319704,-2.89390009456913,338.976748081681));
#68025=CARTESIAN_POINT('Ctrl Pts',(12.3217132535844,-2.78296978081719,339.057472643273));
#68026=CARTESIAN_POINT('Ctrl Pts',(12.3139661751985,-2.66863108901826,339.133572608903));
#68027=CARTESIAN_POINT('Ctrl Pts',(12.3062190968126,-2.55131135776195,339.204758425671));
#68028=CARTESIAN_POINT('Ctrl Pts',(12.2984719534987,-2.43399064325393,339.275944839045));
#68029=CARTESIAN_POINT('Ctrl Pts',(12.2907248101848,-2.31368917362621,339.342216818646));
#68030=CARTESIAN_POINT('Ctrl Pts',(12.2829776668709,-2.19086131519886,339.403329394908));
#68031=CARTESIAN_POINT('Ctrl Pts',(12.2752287818348,-2.06800584246158,339.464455710576));
#68032=CARTESIAN_POINT('Ctrl Pts',(12.2674798967986,-1.94262320057929,339.520420140665));
#68033=CARTESIAN_POINT('Ctrl Pts',(12.2597310117625,-1.81518991116986,339.571024901364));
#68034=CARTESIAN_POINT('Ctrl Pts',(12.2519739019798,-1.68762136275247,339.621683374478));
#68035=CARTESIAN_POINT('Ctrl Pts',(12.2442167921971,-1.55799818274094,339.666970669785));
#68036=CARTESIAN_POINT('Ctrl Pts',(12.2364596824145,-1.42681484468761,339.706737985216));
#68037=CARTESIAN_POINT('Ctrl Pts',(12.2286984274804,-1.29556140645355,339.746526551029));
#68038=CARTESIAN_POINT('Ctrl Pts',(12.2209371725463,-1.16274652724934,339.780789161833));
#68039=CARTESIAN_POINT('Ctrl Pts',(12.2131759176123,-1.02887623007913,339.809427904198));
#68040=CARTESIAN_POINT('Ctrl Pts',(12.2054022471999,-0.894791784064626,
339.838112459217));
#68041=CARTESIAN_POINT('Ctrl Pts',(12.1976285767875,-0.759648931827385,
339.86115510268));
#68042=CARTESIAN_POINT('Ctrl Pts',(12.1898549063751,-0.623961084570843,
339.878509570293));
#68043=CARTESIAN_POINT('Ctrl Pts',(12.1824431022865,-0.494589540922598,
339.895056183049));
#68044=CARTESIAN_POINT('Ctrl Pts',(12.1750312981979,-0.36472288615217,339.906432246523));
#68045=CARTESIAN_POINT('Ctrl Pts',(12.1676194941094,-0.234805403461494,
339.912641803043));
#68046=CARTESIAN_POINT('Ctrl Pts',(12.1598444153398,-0.0985202764682728,
339.919155708496));
#68047=CARTESIAN_POINT('Ctrl Pts',(12.1520693365704,0.0382514730609481,
339.920004434583));
#68048=CARTESIAN_POINT('Ctrl Pts',(12.1442942578008,0.17499957616798,339.915135624867));
#68049=CARTESIAN_POINT('Ctrl Pts',(12.1365287467607,0.311579402028877,339.910272806532));
#68050=CARTESIAN_POINT('Ctrl Pts',(12.1287632357205,0.448135252472564,339.899706465376));
#68051=CARTESIAN_POINT('Ctrl Pts',(12.1209977246804,0.584153134330435,339.883436103621));
#68052=CARTESIAN_POINT('Ctrl Pts',(12.113239913167,0.720036154063117,339.867181873977));
#68053=CARTESIAN_POINT('Ctrl Pts',(12.1054821016535,0.855381881093607,339.845234924731));
#68054=CARTESIAN_POINT('Ctrl Pts',(12.0977242901401,0.989678081016159,339.817646765637));
#68055=CARTESIAN_POINT('Ctrl Pts',(12.0899723166259,1.12387321878993,339.790079367508));
#68056=CARTESIAN_POINT('Ctrl Pts',(12.0822203431118,1.25702002018162,339.756879287711));
#68057=CARTESIAN_POINT('Ctrl Pts',(12.0744683695976,1.3886134774134,339.718149602635));
#68058=CARTESIAN_POINT('Ctrl Pts',(12.0667196790486,1.52015120473965,339.679436319603));
#68059=CARTESIAN_POINT('Ctrl Pts',(12.0589709884997,1.65013652211661,339.635198199079));
#68060=CARTESIAN_POINT('Ctrl Pts',(12.0512222979507,1.77807690495904,339.58558890248));
#68061=CARTESIAN_POINT('Ctrl Pts',(12.0434752195815,1.90599066873726,339.53598992751));
#68062=CARTESIAN_POINT('Ctrl Pts',(12.0357281412122,2.03185998005482,339.481022140509));
#68063=CARTESIAN_POINT('Ctrl Pts',(12.027981062843,2.15521009027124,339.420888205926));
#68064=CARTESIAN_POINT('Ctrl Pts',(12.0202339195457,2.27856123428174,339.360753767362));
#68065=CARTESIAN_POINT('Ctrl Pts',(12.0124867762485,2.39939278373208,339.295453266139));
#68066=CARTESIAN_POINT('Ctrl Pts',(12.0047396329512,2.517252854803,339.225236221501));
#68067=CARTESIAN_POINT('Ctrl Pts',(11.9969907479316,2.63513942332097,339.155003390581));
#68068=CARTESIAN_POINT('Ctrl Pts',(11.9892418629119,2.75005284837986,339.079852016752));
#68069=CARTESIAN_POINT('Ctrl Pts',(11.9814929778923,2.8615689361648,339.000075785042));
#68070=CARTESIAN_POINT('Ctrl Pts',(11.9737358681259,2.97320338828035,338.920214878012));
#68071=CARTESIAN_POINT('Ctrl Pts',(11.9659787583594,3.08143298145544,338.835719534948));
#68072=CARTESIAN_POINT('Ctrl Pts',(11.958221648593,3.18586499684499,338.74692504387));
#68073=CARTESIAN_POINT('Ctrl Pts',(11.950460393675,3.29035281736574,338.658083103853));
#68074=CARTESIAN_POINT('Ctrl Pts',(11.942699138757,3.39103872975003,338.564937703493));
#68075=CARTESIAN_POINT('Ctrl Pts',(11.934937883839,3.48756655842495,338.467861381753));
#68076=CARTESIAN_POINT('Ctrl Pts',(11.9271642134423,3.58424880017019,338.370629769533));
#68077=CARTESIAN_POINT('Ctrl Pts',(11.9193905430457,3.67675940248055,338.269454958878));
#68078=CARTESIAN_POINT('Ctrl Pts',(11.911616872649,3.7647816244639,338.164743651956));
#68079=CARTESIAN_POINT('Ctrl Pts',(11.9042050683778,3.84870639198813,338.064906680195));
#68080=CARTESIAN_POINT('Ctrl Pts',(11.8967932641067,3.92855106715021,337.961855277865));
#68081=CARTESIAN_POINT('Ctrl Pts',(11.8893814598356,4.00407862208117,337.855965239756));
#68082=CARTESIAN_POINT('Ctrl Pts',(11.881606381068,4.08330800634825,337.744885217013));
#68083=CARTESIAN_POINT('Ctrl Pts',(11.8738313023004,4.15803675980889,337.630330229376));
#68084=CARTESIAN_POINT('Ctrl Pts',(11.8660562235328,4.2279447190047,337.512701039826));
#68085=CARTESIAN_POINT('Ctrl Pts',(11.8582907124948,4.29776665200489,337.395216600483));
#68086=CARTESIAN_POINT('Ctrl Pts',(11.8505252014567,4.36277939651893,337.274665819115));
#68087=CARTESIAN_POINT('Ctrl Pts',(11.8427596904187,4.42270438275697,337.151480654164));
#68088=CARTESIAN_POINT('Ctrl Pts',(11.8350018789076,4.4825699531959,337.028417627665));
#68089=CARTESIAN_POINT('Ctrl Pts',(11.8272440673965,4.5373576343673,336.902725764835));
#68090=CARTESIAN_POINT('Ctrl Pts',(11.8194862558854,4.58683354249418,336.7748636894));
#68091=CARTESIAN_POINT('Ctrl Pts',(11.8117342823735,4.63627221843062,336.647097834233));
#68092=CARTESIAN_POINT('Ctrl Pts',(11.8039823088617,4.68040693722041,336.517165380239));
#68093=CARTESIAN_POINT('Ctrl Pts',(11.7962303353498,4.71905108931182,336.385546779782));
#68094=CARTESIAN_POINT('Ctrl Pts',(11.7884816448034,4.75767887558134,336.253983919883));
#68095=CARTESIAN_POINT('Ctrl Pts',(11.7807329542571,4.79082061004134,336.120736708045));
#68096=CARTESIAN_POINT('Ctrl Pts',(11.7729842637107,4.81833897654101,335.98630247371));
#68097=CARTESIAN_POINT('Ctrl Pts',(11.7652371853442,4.84585161761446,335.851896209541));
#68098=CARTESIAN_POINT('Ctrl Pts',(11.7574901069777,4.86774313958145,335.716303796809));
#68099=CARTESIAN_POINT('Ctrl Pts',(11.7497430286112,4.88392705356856,335.580034135134));
#68100=CARTESIAN_POINT('Ctrl Pts',(11.7419958853168,4.90011110319238,335.44376333139));
#68101=CARTESIAN_POINT('Ctrl Pts',(11.7342487420223,4.9105874033276,335.306815655528));
#68102=CARTESIAN_POINT('Ctrl Pts',(11.7265015987279,4.91532123976476,335.169706135474));
#68103=CARTESIAN_POINT('Ctrl Pts',(11.7187527137111,4.92005614046884,335.032565790288));
#68104=CARTESIAN_POINT('Ctrl Pts',(11.7110038286944,4.91904599498924,334.895263919071));
#68105=CARTESIAN_POINT('Ctrl Pts',(11.7032549436777,4.91230821371474,334.758316165268));
#68106=CARTESIAN_POINT('Ctrl Pts',(11.6954978339144,4.90556328088958,334.621223053705));
#68107=CARTESIAN_POINT('Ctrl Pts',(11.6877407241511,4.89307858739198,334.484485201398));
#68108=CARTESIAN_POINT('Ctrl Pts',(11.6799836143877,4.87492356136952,334.34861429759));
#68109=CARTESIAN_POINT('Ctrl Pts',(11.672222359473,4.85675883388164,334.212670788715));
#68110=CARTESIAN_POINT('Ctrl Pts',(11.6644611045581,4.83291780413792,334.077595536174));
#68111=CARTESIAN_POINT('Ctrl Pts',(11.6566998496434,4.80352100106055,333.943889657815));
#68112=CARTESIAN_POINT('Ctrl Pts',(11.64892617925,4.77407717267822,333.809969893623));
#68113=CARTESIAN_POINT('Ctrl Pts',(11.6411525088566,4.73905991114379,333.677424259092));
#68114=CARTESIAN_POINT('Ctrl Pts',(11.6333788384633,4.69863981431569,333.546739198276));
#68115=CARTESIAN_POINT('Ctrl Pts',(11.6259670341627,4.66010128202142,333.422137556225));
#68116=CARTESIAN_POINT('Ctrl Pts',(11.6185552298622,4.61665169435156,333.299227438073));
#68117=CARTESIAN_POINT('Ctrl Pts',(11.6111434255616,4.56847879578283,333.17841152974));
#68118=CARTESIAN_POINT('Ctrl Pts',(11.6033683467292,4.51794480044675,333.05167407508));
#68119=CARTESIAN_POINT('Ctrl Pts',(11.5955932678969,4.46205308333984,332.92684079404));
#68120=CARTESIAN_POINT('Ctrl Pts',(11.5878181890645,4.40096739579065,332.804397794753));
#68121=CARTESIAN_POINT('Ctrl Pts',(11.5800526779614,4.33995687806763,332.682105469368));
#68122=CARTESIAN_POINT('Ctrl Pts',(11.5722871668584,4.27376528000271,332.562197919625));
#68123=CARTESIAN_POINT('Ctrl Pts',(11.5645216557553,4.20260509457612,332.445143158308));
#68124=CARTESIAN_POINT('Ctrl Pts',(11.556763844179,4.13151546467916,332.328204457124));
#68125=CARTESIAN_POINT('Ctrl Pts',(11.5490060326026,4.05546725291025,332.214113247243));
#68126=CARTESIAN_POINT('Ctrl Pts',(11.5412482210263,3.97471955781791,332.103314394139));
#68127=CARTESIAN_POINT('Ctrl Pts',(11.5334962474491,3.89403262792669,331.992598920686));
#68128=CARTESIAN_POINT('Ctrl Pts',(11.525744273872,3.80865348324775,331.885171187078));
#68129=CARTESIAN_POINT('Ctrl Pts',(11.5179923002948,3.71888516129336,331.781448117614));
#68130=CARTESIAN_POINT('Ctrl Pts',(11.5102436096833,3.62915485627842,331.677768974933));
#68131=CARTESIAN_POINT('Ctrl Pts',(11.5024949190717,3.53503932630827,331.577791670851));
#68132=CARTESIAN_POINT('Ctrl Pts',(11.4947462284601,3.43688247667781,331.481900810949));
#68133=CARTESIAN_POINT('Ctrl Pts',(11.4869991500285,3.33874604940094,331.386029901941));
#68134=CARTESIAN_POINT('Ctrl Pts',(11.4792520715969,3.23657025435759,331.294244018941));
#68135=CARTESIAN_POINT('Ctrl Pts',(11.4715049931652,3.13073623201036,331.206891287074));
#68136=CARTESIAN_POINT('Ctrl Pts',(11.4637578498057,3.02490132267454,331.119537823109));
#68137=CARTESIAN_POINT('Ctrl Pts',(11.4560107064462,2.91540842633691,331.036617833197));
#68138=CARTESIAN_POINT('Ctrl Pts',(11.4482635630868,2.80267185512178,330.958439220424));
#68139=CARTESIAN_POINT('Ctrl Pts',(11.4405146780053,2.68990993833552,330.880243031441));
#68140=CARTESIAN_POINT('Ctrl Pts',(11.4327657929238,2.57390321668924,330.806790563438));
#68141=CARTESIAN_POINT('Ctrl Pts',(11.4250169078423,2.45509472752491,330.738346219907));
#68142=CARTESIAN_POINT('Ctrl Pts',(11.4172597980147,2.33616013381324,330.669829228849));
#68143=CARTESIAN_POINT('Ctrl Pts',(11.4095026881873,2.21441817131636,330.606331176248));
#68144=CARTESIAN_POINT('Ctrl Pts',(11.4017455783597,2.09033670199461,330.548070582905));
#68145=CARTESIAN_POINT('Ctrl Pts',(11.3939843233811,1.9661889275081,330.489778856966));
#68146=CARTESIAN_POINT('Ctrl Pts',(11.3862230684024,1.83969951541976,330.436730318105));
#68147=CARTESIAN_POINT('Ctrl Pts',(11.3784618134237,1.71135509154057,330.389094794603));
#68148=CARTESIAN_POINT('Ctrl Pts',(11.3706881429675,1.58280535842797,330.341383069794));
#68149=CARTESIAN_POINT('Ctrl Pts',(11.3629144725113,1.45239505576822,330.299101784325));
#68150=CARTESIAN_POINT('Ctrl Pts',(11.3551408020551,1.32062556504041,330.26237072161));
#68151=CARTESIAN_POINT('Ctrl Pts',(11.347728998466,1.19498998660669,330.227349501711));
#68152=CARTESIAN_POINT('Ctrl Pts',(11.3403171948769,1.06811919309805,330.197373472726));
#68153=CARTESIAN_POINT('Ctrl Pts',(11.3329053912877,0.940453410873421,330.172502672763));
#68154=CARTESIAN_POINT('Ctrl Pts',(11.3251303125808,0.8065303389734,330.146412878979));
#68155=CARTESIAN_POINT('Ctrl Pts',(11.3173552338738,0.671309156618477,330.125858965163));
#68156=CARTESIAN_POINT('Ctrl Pts',(11.3095801551669,0.535287257732207,330.110966290338));
#68157=CARTESIAN_POINT('Ctrl Pts',(11.3018146441893,0.399432742451233,330.096091941898));
#68158=CARTESIAN_POINT('Ctrl Pts',(11.2940491332117,0.262779856006339,330.086865013215));
#68159=CARTESIAN_POINT('Ctrl Pts',(11.286283622234,0.125837152462086,330.083360082988));
#68160=CARTESIAN_POINT('Ctrl Pts',(11.278525810783,-0.0109697719956586,
330.079858627908));
#68161=CARTESIAN_POINT('Ctrl Pts',(11.2707679993319,-0.148065553471827,
330.082067890877));
#68162=CARTESIAN_POINT('Ctrl Pts',(11.2630101878808,-0.284935882019815,
330.090010732635));
#68163=CARTESIAN_POINT('Ctrl Pts',(11.2552582144286,-0.421703211309805,
330.097947597154));
#68164=CARTESIAN_POINT('Ctrl Pts',(11.2475062409764,-0.558245036725915,
330.11160942971));
#68165=CARTESIAN_POINT('Ctrl Pts',(11.2397542675242,-0.694046766757465,
330.13096702126));
#68166=CARTESIAN_POINT('Ctrl Pts',(11.2320055770366,-0.829790984687955,
330.150316414861));
#68167=CARTESIAN_POINT('Ctrl Pts',(11.2242568865492,-0.964795344468126,
330.175356714802));
#68168=CARTESIAN_POINT('Ctrl Pts',(11.2165081960616,-1.0985503161835,330.206006855938));
#68169=CARTESIAN_POINT('Ctrl Pts',(11.2087611177534,-1.23227745906762,330.236650620058));
#68170=CARTESIAN_POINT('Ctrl Pts',(11.2010140394452,-1.36475535017717,330.272901816529));
#68171=CARTESIAN_POINT('Ctrl Pts',(11.193266961137,-1.49548498670334,330.314628326691));
#68172=CARTESIAN_POINT('Ctrl Pts',(11.1855198179003,-1.62621571887834,330.356355186565));
#68173=CARTESIAN_POINT('Ctrl Pts',(11.1777726746637,-1.75519779487862,330.403557332806));
#68174=CARTESIAN_POINT('Ctrl Pts',(11.170025531427,-1.88194808438028,330.456052985542));
#68175=CARTESIAN_POINT('Ctrl Pts',(11.1622766464675,-2.00872687004673,330.50856044042));
#68176=CARTESIAN_POINT('Ctrl Pts',(11.154527761508,-2.13327250972557,330.566363620406));
#68177=CARTESIAN_POINT('Ctrl Pts',(11.1467788765485,-2.25512290796421,330.629233049856));
#68178=CARTESIAN_POINT('Ctrl Pts',(11.1390217668411,-2.37710263949621,330.692169209578));
#68179=CARTESIAN_POINT('Ctrl Pts',(11.1312646571336,-2.49638106704423,330.760182181059));
#68180=CARTESIAN_POINT('Ctrl Pts',(11.1235075474261,-2.61252124486372,330.832996783342));
#68181=CARTESIAN_POINT('Ctrl Pts',(11.1157462925667,-2.72872348429026,330.905850295427));
#68182=CARTESIAN_POINT('Ctrl Pts',(11.1079850377072,-2.84178381042839,330.983510329784));
#68183=CARTESIAN_POINT('Ctrl Pts',(11.1002237828478,-2.95129606991621,331.065659576219));
#68184=CARTESIAN_POINT('Ctrl Pts',(11.0924501125081,-3.06098351335428,331.147940234695));
#68185=CARTESIAN_POINT('Ctrl Pts',(11.0846764421684,-3.16711124556448,331.234724208004));
#68186=CARTESIAN_POINT('Ctrl Pts',(11.0769027718288,-3.26930721184414,331.325654695448));
#68187=CARTESIAN_POINT('Ctrl Pts',(11.0694909668904,-3.36674594212936,331.412352356454));
#68188=CARTESIAN_POINT('Ctrl Pts',(11.0620791619521,-3.46061050821,331.50281897985));
#68189=CARTESIAN_POINT('Ctrl Pts',(11.0546673570138,-3.55061219086199,331.596716859766));
#68190=CARTESIAN_POINT('Ctrl Pts',(11.0469901530241,-3.64383661903929,331.693976998736));
#68191=CARTESIAN_POINT('Ctrl Pts',(11.0393129490344,-3.73322755412441,331.795243674666));
#68192=CARTESIAN_POINT('Ctrl Pts',(11.0316357450447,-3.81841425428008,331.900178126858));
#68193=CARTESIAN_POINT('Ctrl Pts',(11.0237266463557,-3.9061740714509,332.00828218914));
#68194=CARTESIAN_POINT('Ctrl Pts',(11.0158175476667,-3.98947129927634,332.120278873941));
#68195=CARTESIAN_POINT('Ctrl Pts',(11.0079084489777,-4.06793948211894,332.235754816895));
#68196=CARTESIAN_POINT('Ctrl Pts',(11.0002501000046,-4.14391991315414,332.347569715648));
#68197=CARTESIAN_POINT('Ctrl Pts',(10.9925917510315,-4.21537257413328,332.46264626105));
#68198=CARTESIAN_POINT('Ctrl Pts',(10.9849334020585,-4.2820045498982,332.580574428268));
#68199=CARTESIAN_POINT('Ctrl Pts',(10.9772800314538,-4.34859321103718,332.698425935378));
#68200=CARTESIAN_POINT('Ctrl Pts',(10.9696266608492,-4.41036722147423,332.819125029996));
#68201=CARTESIAN_POINT('Ctrl Pts',(10.9619732902445,-4.46707714790624,332.942233050816));
#68202=CARTESIAN_POINT('Ctrl Pts',(10.9543231381244,-4.5237632260189,333.065289300817));
#68203=CARTESIAN_POINT('Ctrl Pts',(10.9466729860044,-4.57538928856949,333.190752097796));
#68204=CARTESIAN_POINT('Ctrl Pts',(10.9390228338843,-4.62175226534308,333.318159026455));
#68205=CARTESIAN_POINT('Ctrl Pts',(10.9313741432867,-4.66810638470703,333.445541614671));
#68206=CARTESIAN_POINT('Ctrl Pts',(10.923725452689,-4.7091992830285,333.574867217875));
#68207=CARTESIAN_POINT('Ctrl Pts',(10.9160767620914,-4.7448765710052,333.70565484185));
#68208=CARTESIAN_POINT('Ctrl Pts',(10.9084255677315,-4.78056553777153,333.836485278528));
#68209=CARTESIAN_POINT('Ctrl Pts',(10.9007743733717,-4.81083524547869,333.968778304757));
#68210=CARTESIAN_POINT('Ctrl Pts',(10.8931231790118,-4.83558162769242,334.10203931911));
#68211=CARTESIAN_POINT('Ctrl Pts',(10.8854704134292,-4.86033309173711,334.235327699482));
#68212=CARTESIAN_POINT('Ctrl Pts',(10.8778176478466,-4.8795589094284,334.369584067083));
#68213=CARTESIAN_POINT('Ctrl Pts',(10.870164882264,-4.8932065976908,334.504306289312));
#68214=CARTESIAN_POINT('Ctrl Pts',(10.8625062805538,-4.90686469390964,334.639131252972));
#68215=CARTESIAN_POINT('Ctrl Pts',(10.8548476788436,-4.91493614280631,334.774422380051));
#68216=CARTESIAN_POINT('Ctrl Pts',(10.8471890771334,-4.9174205114799,334.909675165227));
#68217=CARTESIAN_POINT('Ctrl Pts',(10.8453985102585,-4.91800135226785,334.941297015538));
#68218=CARTESIAN_POINT('Ctrl Pts',(10.8436079433837,-4.91827701884567,334.972916779595));
#68219=CARTESIAN_POINT('Ctrl Pts',(10.8418173765088,-4.91824791560797,335.004528036861));
#68220=CARTESIAN_POINT('',(9.09181737647954,-4.91824973135284,334.998374408491));
#68221=CARTESIAN_POINT('Ctrl Pts',(10.8418173764556,-4.91824791560711,335.004528037799));
#68222=CARTESIAN_POINT('Ctrl Pts',(10.8316241091295,-4.91808223782791,335.184483335951));
#68223=CARTESIAN_POINT('Ctrl Pts',(10.8214308418033,-4.90803654552355,335.364000285683));
#68224=CARTESIAN_POINT('Ctrl Pts',(10.8112375744772,-4.88827494979252,335.542172553465));
#68225=CARTESIAN_POINT('Ctrl Pts',(10.8007669046654,-4.86797555635617,335.725193652185));
#68226=CARTESIAN_POINT('Ctrl Pts',(10.7902962348536,-4.8374241868972,335.906796289323));
#68227=CARTESIAN_POINT('Ctrl Pts',(10.7798255650418,-4.79684630554198,336.086024209449));
#68228=CARTESIAN_POINT('Ctrl Pts',(10.7786934842745,-4.79245905621744,336.105402194332));
#68229=CARTESIAN_POINT('Ctrl Pts',(10.7775614035072,-4.78795464471481,336.124752440221));
#68230=CARTESIAN_POINT('Ctrl Pts',(10.7764293227399,-4.78333338899957,336.144073752947));
#68231=CARTESIAN_POINT('Ctrl Pts',(10.7686542436122,-4.75159481530949,336.276771648393));
#68232=CARTESIAN_POINT('Ctrl Pts',(10.7608791644844,-4.71428000280257,336.408357507293));
#68233=CARTESIAN_POINT('Ctrl Pts',(10.7531040853567,-4.6714809260607,336.538326694805));
#68234=CARTESIAN_POINT('Ctrl Pts',(10.7453385739574,-4.62873451629988,336.668135946982));
#68235=CARTESIAN_POINT('Ctrl Pts',(10.7375730625581,-4.58051739144098,336.796332118426));
#68236=CARTESIAN_POINT('Ctrl Pts',(10.7298075511588,-4.52697236696789,336.922421455147));
#68237=CARTESIAN_POINT('Ctrl Pts',(10.7220497392858,-4.47348043253603,337.048385773939));
#68238=CARTESIAN_POINT('Ctrl Pts',(10.7142919274127,-4.41467126301592,337.172247057642));
#68239=CARTESIAN_POINT('Ctrl Pts',(10.7065341155397,-4.35073712919702,337.293527740213));
#68240=CARTESIAN_POINT('Ctrl Pts',(10.6987821416656,-4.28685110783728,337.414717155232));
#68241=CARTESIAN_POINT('Ctrl Pts',(10.6910301677915,-4.21784798028972,337.533329490164));
#68242=CARTESIAN_POINT('Ctrl Pts',(10.6832781939174,-4.14396752487062,337.648908495082));
#68243=CARTESIAN_POINT('Ctrl Pts',(10.6755295030096,-4.07011835787539,337.764438552211));
#68244=CARTESIAN_POINT('Ctrl Pts',(10.6677808121018,-3.99139618132735,337.876937505686));
#68245=CARTESIAN_POINT('Ctrl Pts',(10.660032121194,-3.90808587293053,337.985975196197));
#68246=CARTESIAN_POINT('Ctrl Pts',(10.6522850424666,-3.82479289794488,338.094990200497));
#68247=CARTESIAN_POINT('Ctrl Pts',(10.6445379637392,-3.73691392703545,338.200545063856));
#68248=CARTESIAN_POINT('Ctrl Pts',(10.6367908850117,-3.64477594247839,338.302240359458));
#68249=CARTESIAN_POINT('Ctrl Pts',(10.6290437413573,-3.55263718572722,338.403936507351));
#68250=CARTESIAN_POINT('Ctrl Pts',(10.6212965977028,-3.45623960657688,338.501772733305));
#68251=CARTESIAN_POINT('Ctrl Pts',(10.6135494540483,-3.35594881010928,338.595384631222));
#68252=CARTESIAN_POINT('Ctrl Pts',(10.6058005686728,-3.2556354661588,338.689017575065));
#68253=CARTESIAN_POINT('Ctrl Pts',(10.5980516832972,-3.15142744887184,338.778424034379));
#68254=CARTESIAN_POINT('Ctrl Pts',(10.5903027979217,-3.04372505854441,338.863278508015));
#68255=CARTESIAN_POINT('Ctrl Pts',(10.5825456878035,-2.93590835184696,338.948223047018));
#68256=CARTESIAN_POINT('Ctrl Pts',(10.5747885776854,-2.82459017062622,339.028605706644));
#68257=CARTESIAN_POINT('Ctrl Pts',(10.5670314675672,-2.71020199402079,339.104142811125));
#68258=CARTESIAN_POINT('Ctrl Pts',(10.5592702122992,-2.59575269205733,339.179720280202));
#68259=CARTESIAN_POINT('Ctrl Pts',(10.5515089570311,-2.47823046058554,339.250446833256));
#68260=CARTESIAN_POINT('Ctrl Pts',(10.543747701763,-2.35809236511287,339.31608427398));
#68261=CARTESIAN_POINT('Ctrl Pts',(10.5359740310227,-2.23776208794456,339.381826713161));
#68262=CARTESIAN_POINT('Ctrl Pts',(10.5282003602823,-2.11480793559586,339.442463599073));
#68263=CARTESIAN_POINT('Ctrl Pts',(10.520426689542,-1.98970878854097,339.497804130829));
#68264=CARTESIAN_POINT('Ctrl Pts',(10.5130148891833,-1.870433103477,339.550568518056));
#68265=CARTESIAN_POINT('Ctrl Pts',(10.5056030888245,-1.74920789841154,339.598518444527));
#68266=CARTESIAN_POINT('Ctrl Pts',(10.4981912884658,-1.62646014828702,339.641531045736));
#68267=CARTESIAN_POINT('Ctrl Pts',(10.4904162102366,-1.49769610804178,339.686651842716));
#68268=CARTESIAN_POINT('Ctrl Pts',(10.4826411320073,-1.36684958044363,339.726481676002));
#68269=CARTESIAN_POINT('Ctrl Pts',(10.4748660537781,-1.23439469630777,339.760824802093));
#68270=CARTESIAN_POINT('Ctrl Pts',(10.4671005432775,-1.10210280633826,339.795125666782));
#68271=CARTESIAN_POINT('Ctrl Pts',(10.459335032777,-0.968206872587985,339.823953161143));
#68272=CARTESIAN_POINT('Ctrl Pts',(10.4515695222765,-0.833199388867935,
339.847160183127));
#68273=CARTESIAN_POINT('Ctrl Pts',(10.4438117113015,-0.698325765448033,
339.870344195283));
#68274=CARTESIAN_POINT('Ctrl Pts',(10.4360539003264,-0.562343168052488,
339.887918759286));
#68275=CARTESIAN_POINT('Ctrl Pts',(10.4282960893514,-0.425757240810356,
339.899787121335));
#68276=CARTESIAN_POINT('Ctrl Pts',(10.4205441163737,-0.289274098784777,
339.911646552066));
#68277=CARTESIAN_POINT('Ctrl Pts',(10.412792143396,-0.152188918465723,339.917808294333));
#68278=CARTESIAN_POINT('Ctrl Pts',(10.4050401704183,-0.015015127859537,
339.918227079796));
#68279=CARTESIAN_POINT('Ctrl Pts',(10.3972914804014,0.122100569643539,339.918645687903));
#68280=CARTESIAN_POINT('Ctrl Pts',(10.3895427903844,0.259304412737212,339.913326175376));
#68281=CARTESIAN_POINT('Ctrl Pts',(10.3817941003674,0.396080507702657,339.902275318045));
#68282=CARTESIAN_POINT('Ctrl Pts',(10.3740470225274,0.532828145308602,339.891226759934));
#68283=CARTESIAN_POINT('Ctrl Pts',(10.3662999446873,0.66914782244632,339.874449260349));
#68284=CARTESIAN_POINT('Ctrl Pts',(10.3585528668472,0.804526703805565,339.852001632869));
#68285=CARTESIAN_POINT('Ctrl Pts',(10.3508057240757,0.939906719829884,339.829553817247));
#68286=CARTESIAN_POINT('Ctrl Pts',(10.3430585813042,1.07434553873882,339.80143584288));
#68287=CARTESIAN_POINT('Ctrl Pts',(10.3353114385327,1.20733887387551,339.767757953811));
#68288=CARTESIAN_POINT('Ctrl Pts',(10.327562554035,1.34036210880657,339.73407249322));
#68289=CARTESIAN_POINT('Ctrl Pts',(10.3198136695374,1.47193883445901,339.69482472652));
#68290=CARTESIAN_POINT('Ctrl Pts',(10.3120647850397,1.6015787046038,339.650175127397));
#68291=CARTESIAN_POINT('Ctrl Pts',(10.3043076757863,1.73135617600836,339.605478136672));
#68292=CARTESIAN_POINT('Ctrl Pts',(10.2965505665329,1.85919231509715,339.55536798767));
#68293=CARTESIAN_POINT('Ctrl Pts',(10.2887934572794,1.98461507483902,339.500054007145));
#68294=CARTESIAN_POINT('Ctrl Pts',(10.2810322028704,2.11010485656511,339.444710468566));
#68295=CARTESIAN_POINT('Ctrl Pts',(10.2732709484614,2.23317833868694,339.384157730011));
#68296=CARTESIAN_POINT('Ctrl Pts',(10.2655096940523,2.35338787257247,339.318651245902));
#68297=CARTESIAN_POINT('Ctrl Pts',(10.2577360241525,2.47378970273879,339.253039972656));
#68298=CARTESIAN_POINT('Ctrl Pts',(10.2499623542528,2.59131809442937,339.182459319926));
#68299=CARTESIAN_POINT('Ctrl Pts',(10.242188684353,2.70555344950424,339.107208735184));
#68300=CARTESIAN_POINT('Ctrl Pts',(10.2347768742993,2.81447121474806,339.035461021721));
#68301=CARTESIAN_POINT('Ctrl Pts',(10.2273650642456,2.92039538667276,338.95946852315));
#68302=CARTESIAN_POINT('Ctrl Pts',(10.219953254192,3.0229915839452,338.879523804012));
#68303=CARTESIAN_POINT('Ctrl Pts',(10.2121781755366,3.13061623942886,338.795660823866));
#68304=CARTESIAN_POINT('Ctrl Pts',(10.2044030968812,3.23491856376309,338.707183391269));
#68305=CARTESIAN_POINT('Ctrl Pts',(10.1966280182258,3.33547737264277,338.614384284922));
#68306=CARTESIAN_POINT('Ctrl Pts',(10.1888625073048,3.43591243744065,338.521699373843));
#68307=CARTESIAN_POINT('Ctrl Pts',(10.1810969963838,3.53261286816526,338.424703633052));
#68308=CARTESIAN_POINT('Ctrl Pts',(10.1733314854627,3.62518844687318,338.323731605764));
#68309=CARTESIAN_POINT('Ctrl Pts',(10.1655736740732,3.71767223656734,338.222859692599));
#68310=CARTESIAN_POINT('Ctrl Pts',(10.1578158626838,3.80603905073919,338.118019624991));
#68311=CARTESIAN_POINT('Ctrl Pts',(10.1500580512943,3.88993389396859,338.009584250865));
#68312=CARTESIAN_POINT('Ctrl Pts',(10.1423060779085,3.97376560361783,337.901230477861));
#68313=CARTESIAN_POINT('Ctrl Pts',(10.1345541045227,4.05313180257354,337.789287091577));
#68314=CARTESIAN_POINT('Ctrl Pts',(10.1268021311369,4.1277165783379,337.674161347304));
#68315=CARTESIAN_POINT('Ctrl Pts',(10.1190534407229,4.20226976734376,337.559084358947));
#68316=CARTESIAN_POINT('Ctrl Pts',(10.1113047503089,4.27204534853561,337.440828020513));
#68317=CARTESIAN_POINT('Ctrl Pts',(10.1035560598949,4.33676984012755,337.319829824849));
#68318=CARTESIAN_POINT('Ctrl Pts',(10.0958089816645,4.40148086521617,337.198856803931));
#68319=CARTESIAN_POINT('Ctrl Pts',(10.0880619034341,4.46114270681581,337.075143404929));
#68320=CARTESIAN_POINT('Ctrl Pts',(10.0803148252037,4.51552729787316,336.949152709426));
#68321=CARTESIAN_POINT('Ctrl Pts',(10.072567682049,4.56991234469991,336.823160958059));
#68322=CARTESIAN_POINT('Ctrl Pts',(10.0648205388942,4.61901989786494,336.694892230992));
#68323=CARTESIAN_POINT('Ctrl Pts',(10.0570733957395,4.66266976545344,336.564830253039));
#68324=CARTESIAN_POINT('Ctrl Pts',(10.0493245108661,4.70632944643928,336.434739034451));
#68325=CARTESIAN_POINT('Ctrl Pts',(10.0415756259925,4.74452887591398,336.302854133222));
#68326=CARTESIAN_POINT('Ctrl Pts',(10.033826741119,4.77713764510589,336.16967473351));
#68327=CARTESIAN_POINT('Ctrl Pts',(10.0260696315036,4.80978102556353,336.036353975884));
#68328=CARTESIAN_POINT('Ctrl Pts',(10.0183125218881,4.83682179894804,335.901736355353));
#68329=CARTESIAN_POINT('Ctrl Pts',(10.0105554122726,4.85818054082088,335.766332105088));
#68330=CARTESIAN_POINT('Ctrl Pts',(10.0027941575084,4.87955069611507,335.630855499169));
#68331=CARTESIAN_POINT('Ctrl Pts',(9.99503290274435,4.89523272514184,335.494591814046));
#68332=CARTESIAN_POINT('Ctrl Pts',(9.98727164798021,4.90519919657519,335.35805572809));
#68333=CARTESIAN_POINT('Ctrl Pts',(9.97949797774061,4.91518161111121,335.221301228942));
#68334=CARTESIAN_POINT('Ctrl Pts',(9.97172430750101,4.91943018545769,335.084273849091));
#68335=CARTESIAN_POINT('Ctrl Pts',(9.96395063726141,4.91796966271429,334.947488485816));
#68336=CARTESIAN_POINT('Ctrl Pts',(9.95653883148027,4.91657712732504,334.817070483117));
#68337=CARTESIAN_POINT('Ctrl Pts',(9.94912702569913,4.90999506239017,334.686872759848));
#68338=CARTESIAN_POINT('Ctrl Pts',(9.941715219918,4.8982885385814,334.557334827096));
#68339=CARTESIAN_POINT('Ctrl Pts',(9.93394013893002,4.88600824233666,334.421447845178));
#68340=CARTESIAN_POINT('Ctrl Pts',(9.92616505794206,4.86804964710762,334.285857538581));
#68341=CARTESIAN_POINT('Ctrl Pts',(9.91838997695407,4.84443102997917,334.151076529789));
#68342=CARTESIAN_POINT('Ctrl Pts',(9.9106244636881,4.82084147703193,334.016461377433));
#68343=CARTESIAN_POINT('Ctrl Pts',(9.90285895042208,4.79160582738062,333.882653922671));
#68344=CARTESIAN_POINT('Ctrl Pts',(9.89509343715611,4.75679423645525,333.750163348863));
#68345=CARTESIAN_POINT('Ctrl Pts',(9.88733562341187,4.72201716129104,333.61780413972));
#68346=CARTESIAN_POINT('Ctrl Pts',(9.87957780966763,4.68167524568344,333.486759588742));
#68347=CARTESIAN_POINT('Ctrl Pts',(9.8718199959234,4.63588991723467,333.357529988772));
#68348=CARTESIAN_POINT('Ctrl Pts',(9.86406802017565,4.59013904367161,333.228397638102));
#68349=CARTESIAN_POINT('Ctrl Pts',(9.85631604442789,4.53895304083585,333.101077886818));
#68350=CARTESIAN_POINT('Ctrl Pts',(9.84856406868013,4.4825034202272,332.976056781886));
#68351=CARTESIAN_POINT('Ctrl Pts',(9.84081537590146,4.42607770608643,332.85108862351));
#68352=CARTESIAN_POINT('Ctrl Pts',(9.83306668312281,4.36439296830595,332.728417530807));
#68353=CARTESIAN_POINT('Ctrl Pts',(9.82531799034413,4.29766910747938,332.608510233115));
#68354=CARTESIAN_POINT('Ctrl Pts',(9.81757090974782,4.23095912912753,332.48862788317));
#68355=CARTESIAN_POINT('Ctrl Pts',(9.80982382915152,4.15921230307949,332.371508525797));
#68356=CARTESIAN_POINT('Ctrl Pts',(9.80207674855521,4.08269462455298,332.257594547638));
#68357=CARTESIAN_POINT('Ctrl Pts',(9.79432960303557,4.00617630478068,332.143679614838));
#68358=CARTESIAN_POINT('Ctrl Pts',(9.78658245751594,3.92488727073439,332.032970439301));
#68359=CARTESIAN_POINT('Ctrl Pts',(9.77883531199629,3.83913678494635,331.925880319673));
#68360=CARTESIAN_POINT('Ctrl Pts',(9.77108642476111,3.75336702070884,331.818766124013));
#68361=CARTESIAN_POINT('Ctrl Pts',(9.76333753752587,3.66313405308759,331.715272908363));
#68362=CARTESIAN_POINT('Ctrl Pts',(9.75558865029069,3.56878708521855,331.615780473598));
#68363=CARTESIAN_POINT('Ctrl Pts',(9.74783153833195,3.47433997681248,331.516182436862));
#68364=CARTESIAN_POINT('Ctrl Pts',(9.74007442637327,3.37577041479077,331.420593947781));
#68365=CARTESIAN_POINT('Ctrl Pts',(9.73231731441453,3.27346448418863,331.329357912673));
#68366=CARTESIAN_POINT('Ctrl Pts',(9.72455605731347,3.17110388470388,331.238073124066));
#68367=CARTESIAN_POINT('Ctrl Pts',(9.71679480021239,3.06500324045312,331.151145671403));
#68368=CARTESIAN_POINT('Ctrl Pts',(9.70903354311133,2.95558051099265,331.068877144436));
#68369=CARTESIAN_POINT('Ctrl Pts',(9.70125987056932,2.8459827414042,330.986477015072));
#68370=CARTESIAN_POINT('Ctrl Pts',(9.6934861980273,2.73305258933912,330.908750925908));
#68371=CARTESIAN_POINT('Ctrl Pts',(9.68571252548529,2.61723643301779,330.835956710578));
#68372=CARTESIAN_POINT('Ctrl Pts',(9.67830074553823,2.50681193798943,330.766551329462));
#68373=CARTESIAN_POINT('Ctrl Pts',(9.67088896559113,2.39376434723797,330.701629109301));
#68374=CARTESIAN_POINT('Ctrl Pts',(9.66347718564407,2.27849846405012,330.641373173599));
#68375=CARTESIAN_POINT('Ctrl Pts',(9.65570211094242,2.15758272468133,330.578163741499));
#68376=CARTESIAN_POINT('Ctrl Pts',(9.6479270362408,2.03384361502961,330.519889851457));
#68377=CARTESIAN_POINT('Ctrl Pts',(9.64015196153915,1.90772210024274,330.466813543351));
#68378=CARTESIAN_POINT('Ctrl Pts',(9.63238645456454,1.78175578605197,330.413802549039));
#68379=CARTESIAN_POINT('Ctrl Pts',(9.6246209475899,1.65341325680026,330.365976560709));
#68380=CARTESIAN_POINT('Ctrl Pts',(9.6168554406153,1.52316065999553,330.323552131549));
#68381=CARTESIAN_POINT('Ctrl Pts',(9.60909763316098,1.39303720897802,330.28116976632));
#68382=CARTESIAN_POINT('Ctrl Pts',(9.60133982570669,1.26100782851349,330.244178422469));
#68383=CARTESIAN_POINT('Ctrl Pts',(9.59358201825236,1.12755893623701,330.212746726168));
#68384=CARTESIAN_POINT('Ctrl Pts',(9.5858300487866,0.994210468353891,330.181338683185));
#68385=CARTESIAN_POINT('Ctrl Pts',(9.5780780793208,0.859444993842858,330.155482049344));
#68386=CARTESIAN_POINT('Ctrl Pts',(9.57032610985505,0.723764053976697,330.135295624946));
#68387=CARTESIAN_POINT('Ctrl Pts',(9.56257742332448,0.588140574570665,330.115117749437));
#68388=CARTESIAN_POINT('Ctrl Pts',(9.55482873679395,0.451602786725605,330.100605364723));
#68389=CARTESIAN_POINT('Ctrl Pts',(9.54708005026339,0.314662173250379,330.091826125816));
#68390=CARTESIAN_POINT('Ctrl Pts',(9.53933297589371,0.177750051094268,330.083048713481));
#68391=CARTESIAN_POINT('Ctrl Pts',(9.53158590152403,0.0404356598416378,
330.08000209935));
#68392=CARTESIAN_POINT('Ctrl Pts',(9.52383882715435,-0.0967650435309119,
330.082702003249));
#68393=CARTESIAN_POINT('Ctrl Pts',(9.51609168783409,-0.233966897178491,
330.085401929784));
#68394=CARTESIAN_POINT('Ctrl Pts',(9.50834454851381,-0.371054670245795,
330.093848462754));
#68395=CARTESIAN_POINT('Ctrl Pts',(9.50059740919355,-0.507513452040183,
330.108005196395));
#68396=CARTESIAN_POINT('Ctrl Pts',(9.49284852812469,-0.644002913144896,
330.12216511282));
#68397=CARTESIAN_POINT('Ctrl Pts',(9.48509964705582,-0.779862712868882,
330.142037744198));
#68398=CARTESIAN_POINT('Ctrl Pts',(9.47735076598696,-0.914584495363758,
330.167534970293));
#68399=CARTESIAN_POINT('Ctrl Pts',(9.46959366010778,-1.04944927413084,330.193059259631));
#68400=CARTESIAN_POINT('Ctrl Pts',(9.46183655422864,-1.18317323808522,330.224219996623));
#68401=CARTESIAN_POINT('Ctrl Pts',(9.45407944834946,-1.31525909789341,330.260878080498));
#68402=CARTESIAN_POINT('Ctrl Pts',(9.44631819729033,-1.44741554068276,330.297555753424));
#68403=CARTESIAN_POINT('Ctrl Pts',(9.43855694623125,-1.5779317633539,330.339736506579));
#68404=CARTESIAN_POINT('Ctrl Pts',(9.43079569517212,-1.70632797144456,330.387232076468));
#68405=CARTESIAN_POINT('Ctrl Pts',(9.42302202854694,-1.83492957317483,330.434803624363));
#68406=CARTESIAN_POINT('Ctrl Pts',(9.4152483619217,-1.96140402259827,330.487706827669));
#68407=CARTESIAN_POINT('Ctrl Pts',(9.40747469529651,-2.08529294175604,330.545705846089));
#68408=CARTESIAN_POINT('Ctrl Pts',(9.40006284732105,-2.20341555736534,330.601005349912));
#68409=CARTESIAN_POINT('Ctrl Pts',(9.3926509993456,-2.31918765281013,330.660936851974));
#68410=CARTESIAN_POINT('Ctrl Pts',(9.38523915137014,-2.43223616300396,330.725259035933));
#68411=CARTESIAN_POINT('Ctrl Pts',(9.37746407213797,-2.55082482358454,330.792733446946));
#68412=CARTESIAN_POINT('Ctrl Pts',(9.36968899290579,-2.66679096589698,330.865252999787));
#68413=CARTESIAN_POINT('Ctrl Pts',(9.36191391367362,-2.77967560314094,330.942588681955));
#68414=CARTESIAN_POINT('Ctrl Pts',(9.35414840220223,-2.89242132820501,331.019829197336));
#68415=CARTESIAN_POINT('Ctrl Pts',(9.3463828907308,-3.00209277381689,331.101873831063));
#68416=CARTESIAN_POINT('Ctrl Pts',(9.3386173792594,-3.10825557629554,331.188447778801));
#68417=CARTESIAN_POINT('Ctrl Pts',(9.33085956734618,-3.21431311762354,331.274935887873));
#68418=CARTESIAN_POINT('Ctrl Pts',(9.32310175543299,-3.31686863794535,331.365944128484));
#68419=CARTESIAN_POINT('Ctrl Pts',(9.31534394351976,-3.41551710710683,331.461154714662));
#68420=CARTESIAN_POINT('Ctrl Pts',(9.30759196963713,-3.51409133977126,331.556293651473));
#68421=CARTESIAN_POINT('Ctrl Pts',(9.29983999575445,-3.60876409347624,331.655628368866));
#68422=CARTESIAN_POINT('Ctrl Pts',(9.29208802187182,-3.69916405343823,331.758801399443));
#68423=CARTESIAN_POINT('Ctrl Pts',(9.28433933100309,-3.78952572839959,331.861930735538));
#68424=CARTESIAN_POINT('Ctrl Pts',(9.27659064013434,-3.87561795164439,331.968894858332));
#68425=CARTESIAN_POINT('Ctrl Pts',(9.26884194926561,-3.9571070376224,332.079300262728));
#68426=CARTESIAN_POINT('Ctrl Pts',(9.26109487060617,-4.0385791688059,332.189682695938));
#68427=CARTESIAN_POINT('Ctrl Pts',(9.25334779194675,-4.11544983575781,332.303504672284));
#68428=CARTESIAN_POINT('Ctrl Pts',(9.2456007132873,-4.18742660509345,332.420340819128));
#68429=CARTESIAN_POINT('Ctrl Pts',(9.23785356972949,-4.25940397738855,332.537177944725));
#68430=CARTESIAN_POINT('Ctrl Pts',(9.23010642617165,-4.32648716527949,332.657028958392));
#68431=CARTESIAN_POINT('Ctrl Pts',(9.22235928261384,-4.3884281350977,332.779441159171));
#68432=CARTESIAN_POINT('Ctrl Pts',(9.21461039736349,-4.45038303032262,332.901880880341));
#68433=CARTESIAN_POINT('Ctrl Pts',(9.20686151211319,-4.50719323060179,333.026882585701));
#68434=CARTESIAN_POINT('Ctrl Pts',(9.19911262686284,-4.55865773726159,333.153971100712));
#68435=CARTESIAN_POINT('Ctrl Pts',(9.1913555169137,-4.61017686856121,333.281194507999));
#68436=CARTESIAN_POINT('Ctrl Pts',(9.18359840696458,-4.65633882506793,333.410508786635));
#68437=CARTESIAN_POINT('Ctrl Pts',(9.17584129701544,-4.69699146744889,333.54142047964));
#68438=CARTESIAN_POINT('Ctrl Pts',(9.16808004194063,-4.73766583316658,333.672402127232));
#68439=CARTESIAN_POINT('Ctrl Pts',(9.16031878686583,-4.7728249184651,333.804982512447));
#68440=CARTESIAN_POINT('Ctrl Pts',(9.15255753179102,-4.80236739346133,333.938656285306));
#68441=CARTESIAN_POINT('Ctrl Pts',(9.14478386128284,-4.83195712661703,334.072543891857));
#68442=CARTESIAN_POINT('Ctrl Pts',(9.13701019077465,-4.85591222701698,334.207527996125));
#68443=CARTESIAN_POINT('Ctrl Pts',(9.12923652026646,-4.8741829628194,334.343095511158));
#68444=CARTESIAN_POINT('Ctrl Pts',(9.12182471920972,-4.89160318390869,334.472352269612));
#68445=CARTESIAN_POINT('Ctrl Pts',(9.11441291815298,-4.90385632254623,334.602139058645));
#68446=CARTESIAN_POINT('Ctrl Pts',(9.10700111709625,-4.91094341938446,334.732011578413));
#68447=CARTESIAN_POINT('Ctrl Pts',(9.10193987023375,-4.91578293765565,334.820696754684));
#68448=CARTESIAN_POINT('Ctrl Pts',(9.09687862337123,-4.91822036105881,334.90951420329));
#68449=CARTESIAN_POINT('Ctrl Pts',(9.09181737650877,-4.91824973135267,334.998374407977));
#68450=CARTESIAN_POINT('',(7.34181737656206,-4.91824863900072,334.996341111162));
#68451=CARTESIAN_POINT('Ctrl Pts',(9.09181737647953,-4.91824973135284,334.998374408491));
#68452=CARTESIAN_POINT('Ctrl Pts',(9.08410754254342,-4.91829447131967,335.13373580071));
#68453=CARTESIAN_POINT('Ctrl Pts',(9.07639770860732,-4.91274680624549,335.269324293168));
#68454=CARTESIAN_POINT('Ctrl Pts',(9.06868787467121,-4.9015766619707,335.4046347604));
#68455=CARTESIAN_POINT('Ctrl Pts',(9.06098726770942,-4.89041988590009,335.539783290785));
#68456=CARTESIAN_POINT('Ctrl Pts',(9.05328666074762,-4.87365404750714,335.674654064992));
#68457=CARTESIAN_POINT('Ctrl Pts',(9.04558605378583,-4.85130105419687,335.808740467671));
#68458=CARTESIAN_POINT('Ctrl Pts',(9.03789274498896,-4.82896924568837,335.942699791447));
#68459=CARTESIAN_POINT('Ctrl Pts',(9.03019943619208,-4.80106088196502,336.075875832535));
#68460=CARTESIAN_POINT('Ctrl Pts',(9.02250612739522,-4.76764975578662,336.207766065365));
#68461=CARTESIAN_POINT('Ctrl Pts',(9.01443350053801,-4.73259129633322,336.346159137041));
#68462=CARTESIAN_POINT('Ctrl Pts',(9.00636087368077,-4.69147366052708,336.483135933379));
#68463=CARTESIAN_POINT('Ctrl Pts',(8.99828824682356,-4.64444300410043,336.618126152116));
#68464=CARTESIAN_POINT('Ctrl Pts',(8.99060304167977,-4.599669444133,336.746637916843));
#68465=CARTESIAN_POINT('Ctrl Pts',(8.98291783653599,-4.54953734429063,336.873348920796));
#68466=CARTESIAN_POINT('Ctrl Pts',(8.9752326313922,-4.49422406301,336.997782053669));
#68467=CARTESIAN_POINT('Ctrl Pts',(8.96754842408633,-4.4389179635402,337.122199030292));
#68468=CARTESIAN_POINT('Ctrl Pts',(8.9598642167805,-4.37843218198699,337.24433836039));
#68469=CARTESIAN_POINT('Ctrl Pts',(8.95218000947463,-4.31299201024085,337.363743425607));
#68470=CARTESIAN_POINT('Ctrl Pts',(8.9444950684509,-4.24754559001375,337.483159892081));
#68471=CARTESIAN_POINT('Ctrl Pts',(8.9368101274272,-4.17714403006146,337.599841225438));
#68472=CARTESIAN_POINT('Ctrl Pts',(8.92912518640347,-4.10205807164927,337.713356342119));
#68473=CARTESIAN_POINT('Ctrl Pts',(8.92143777987631,-4.02694802395825,337.826907877024));
#68474=CARTESIAN_POINT('Ctrl Pts',(8.91375037334906,-3.94715080806605,337.937290843134));
#68475=CARTESIAN_POINT('Ctrl Pts',(8.90606296682191,-3.86297958756368,338.044104428));
#68476=CARTESIAN_POINT('Ctrl Pts',(8.89836717245813,-3.7787165266671,338.15103455866));
#68477=CARTESIAN_POINT('Ctrl Pts',(8.89067137809435,-3.69007018080346,338.254387221121));
#68478=CARTESIAN_POINT('Ctrl Pts',(8.88297558373057,-3.59739318926874,338.353795656313));
#68479=CARTESIAN_POINT('Ctrl Pts',(8.8752748898708,-3.50465719530665,338.453267379479));
#68480=CARTESIAN_POINT('Ctrl Pts',(8.86757419601105,-3.40788572869358,338.548789596827));
#68481=CARTESIAN_POINT('Ctrl Pts',(8.85987350215129,-3.30746624117089,338.640034357807));
#68482=CARTESIAN_POINT('Ctrl Pts',(8.85216184201642,-3.20690374994678,338.731409057097));
#68483=CARTESIAN_POINT('Ctrl Pts',(8.84445018188164,-3.10268317295261,338.818493887959));
#68484=CARTESIAN_POINT('Ctrl Pts',(8.83673852174678,-2.99522304385326,338.901002689062));
#68485=CARTESIAN_POINT('Ctrl Pts',(8.83408004210527,-2.95817776949094,338.929446365799));
#68486=CARTESIAN_POINT('Ctrl Pts',(8.83142156246372,-2.92074773267013,338.957346608124));
#68487=CARTESIAN_POINT('Ctrl Pts',(8.82876308282221,-2.88295077582512,338.984692947602));
#68488=CARTESIAN_POINT('Ctrl Pts',(8.82098803347039,-2.77240894573939,339.064670667089));
#68489=CARTESIAN_POINT('Ctrl Pts',(8.81321298411855,-2.65836184263739,339.140171372476));
#68490=CARTESIAN_POINT('Ctrl Pts',(8.80543793476673,-2.54120805372173,339.210872200649));
#68491=CARTESIAN_POINT('Ctrl Pts',(8.79767245314615,-2.42419843057469,339.281486026606));
#68492=CARTESIAN_POINT('Ctrl Pts',(8.78990697152558,-2.30409005972581,339.347311527713));
#68493=CARTESIAN_POINT('Ctrl Pts',(8.782141489905,-2.18131300429889,339.408067222693));
#68494=CARTESIAN_POINT('Ctrl Pts',(8.77438370778293,-2.05865768269373,339.468762678217));
#68495=CARTESIAN_POINT('Ctrl Pts',(8.76662592566089,-1.93333929029083,339.524398158843));
#68496=CARTESIAN_POINT('Ctrl Pts',(8.75886814353882,-1.80581485692351,339.574736688053));
#68497=CARTESIAN_POINT('Ctrl Pts',(8.75111619935774,-1.67838638914334,339.625037336156));
#68498=CARTESIAN_POINT('Ctrl Pts',(8.74336425517663,-1.54875554686997,339.670048824038));
#68499=CARTESIAN_POINT('Ctrl Pts',(8.73561231099555,-1.41740150757175,339.709581300799));
#68500=CARTESIAN_POINT('Ctrl Pts',(8.72786364958949,-1.28610309377204,339.74909703644));
#68501=CARTESIAN_POINT('Ctrl Pts',(8.72011498818342,-1.15308330785384,339.783138263336));
#68502=CARTESIAN_POINT('Ctrl Pts',(8.71236632677736,-1.01883853709875,339.811564308811));
#68503=CARTESIAN_POINT('Ctrl Pts',(8.7046192774313,-0.884621695119256,339.839984440427));
#68504=CARTESIAN_POINT('Ctrl Pts',(8.69687222808524,-0.74918075737672,339.862791633339));
#68505=CARTESIAN_POINT('Ctrl Pts',(8.68912517873918,-0.613024024494354,
339.879895962814));
#68506=CARTESIAN_POINT('Ctrl Pts',(8.68137806431856,-0.476866147907073,
339.897000435965));
#68507=CARTESIAN_POINT('Ctrl Pts',(8.67363094989797,-0.339992852016731,
339.908401901411));
#68508=CARTESIAN_POINT('Ctrl Pts',(8.66588383547736,-0.202918915392262,
339.914062166505));
#68509=CARTESIAN_POINT('Ctrl Pts',(8.65813497916096,-0.0658141584519695,
339.919723704278));
#68510=CARTESIAN_POINT('Ctrl Pts',(8.65038612284457,0.0714909385238468,
339.919641456873));
#68511=CARTESIAN_POINT('Ctrl Pts',(8.64263726652817,0.208480629353462,339.913829350892));
#68512=CARTESIAN_POINT('Ctrl Pts',(8.63488018503037,0.345615730681223,339.908011075533));
#68513=CARTESIAN_POINT('Ctrl Pts',(8.62712310353256,0.482434365936827,339.896450808678));
#68514=CARTESIAN_POINT('Ctrl Pts',(8.61936602203477,0.618424391671335,339.879214520216));
#68515=CARTESIAN_POINT('Ctrl Pts',(8.61160479519355,0.754487089758085,339.861969020772));
#68516=CARTESIAN_POINT('Ctrl Pts',(8.60384356835233,0.889719910813559,339.839041521031));
#68517=CARTESIAN_POINT('Ctrl Pts',(8.59608234151111,1.02362093744717,339.810549161886));
#68518=CARTESIAN_POINT('Ctrl Pts',(8.58830869858097,1.15773617339159,339.782011221845));
#68519=CARTESIAN_POINT('Ctrl Pts',(8.58053505565073,1.29051497866879,339.747890730042));
#68520=CARTESIAN_POINT('Ctrl Pts',(8.57276141272058,1.42146977119236,339.708354994272));
#68521=CARTESIAN_POINT('Ctrl Pts',(8.56534929132981,1.54633437169053,339.670657909979));
#68522=CARTESIAN_POINT('Ctrl Pts',(8.55793716993905,1.66954052761693,339.628038032801));
#68523=CARTESIAN_POINT('Ctrl Pts',(8.55052504854828,1.79068424137417,339.580680409087));
#68524=CARTESIAN_POINT('Ctrl Pts',(8.5427499581479,1.91776032070997,339.531003698992));
#68525=CARTESIAN_POINT('Ctrl Pts',(8.53497486774757,2.04296846105325,339.475956514327));
#68526=CARTESIAN_POINT('Ctrl Pts',(8.52719977734719,2.16582145814549,339.415699318787));
#68527=CARTESIAN_POINT('Ctrl Pts',(8.5194342548707,2.28852327395677,339.355516274958));
#68528=CARTESIAN_POINT('Ctrl Pts',(8.51166873239421,2.40887536554206,339.290136147524));
#68529=CARTESIAN_POINT('Ctrl Pts',(8.50390320991772,2.52640829426202,339.219768262972));
#68530=CARTESIAN_POINT('Ctrl Pts',(8.4961453871716,2.64382468583162,339.149470150124));
#68531=CARTESIAN_POINT('Ctrl Pts',(8.48838756442549,2.75842714409564,339.074194321471));
#68532=CARTESIAN_POINT('Ctrl Pts',(8.48062974167937,2.86976906229912,338.994196864398));
#68533=CARTESIAN_POINT('Ctrl Pts',(8.47287775714514,2.98102718924667,338.914259610056));
#68534=CARTESIAN_POINT('Ctrl Pts',(8.46512577261092,3.08902934403782,338.829608027117));
#68535=CARTESIAN_POINT('Ctrl Pts',(8.45737378807669,3.19335656356526,338.740542329721));
#68536=CARTESIAN_POINT('Ctrl Pts',(8.44962508686652,3.29763959568915,338.651514355768));
#68537=CARTESIAN_POINT('Ctrl Pts',(8.44187638565634,3.39825049167207,338.558076239086));
#68538=CARTESIAN_POINT('Ctrl Pts',(8.43412768444617,3.49480233025679,338.460569279025));
#68539=CARTESIAN_POINT('Ctrl Pts',(8.42638059563513,3.59133407771952,338.363082608834));
#68540=CARTESIAN_POINT('Ctrl Pts',(8.4186335068241,3.68380817296939,338.261529056925));
#68541=CARTESIAN_POINT('Ctrl Pts',(8.41088641801306,3.77187392275263,338.156287403479));
#68542=CARTESIAN_POINT('Ctrl Pts',(8.4031392645021,3.85994040801835,338.051044871105));
#68543=CARTESIAN_POINT('Ctrl Pts',(8.39539211099112,3.94359822354101,337.942114475523));
#68544=CARTESIAN_POINT('Ctrl Pts',(8.38764495748015,4.02253667302524,337.829908439626));
#68545=CARTESIAN_POINT('Ctrl Pts',(8.37989606248383,4.10149286711114,337.717677180895));
#68546=CARTESIAN_POINT('Ctrl Pts',(8.3721471674875,4.17572735928963,337.602169136254));
#68547=CARTESIAN_POINT('Ctrl Pts',(8.36439827249117,4.2449727577381,337.483825547127));
#68548=CARTESIAN_POINT('Ctrl Pts',(8.35664115317578,4.3142916500526,337.365356353583));
#68549=CARTESIAN_POINT('Ctrl Pts',(8.3488840338604,4.37861067327945,337.244045941661));
#68550=CARTESIAN_POINT('Ctrl Pts',(8.34112691454501,4.43770814948298,337.120360686891));
#68551=CARTESIAN_POINT('Ctrl Pts',(8.33336565029588,4.49683720379094,336.996609342228));
#68552=CARTESIAN_POINT('Ctrl Pts',(8.3256043860467,4.55073899806773,336.870480985421));
#68553=CARTESIAN_POINT('Ctrl Pts',(8.31784312179755,4.59924041896377,336.742461084521));
#68554=CARTESIAN_POINT('Ctrl Pts',(8.3100694425331,4.64781942333895,336.614236401387));
#68555=CARTESIAN_POINT('Ctrl Pts',(8.30229576326871,4.6909806689184,336.484114499033));
#68556=CARTESIAN_POINT('Ctrl Pts',(8.29452208400426,4.72860098635664,336.352595939047));
#68557=CARTESIAN_POINT('Ctrl Pts',(8.2871103940943,4.7644694750968,336.227201675809));
#68558=CARTESIAN_POINT('Ctrl Pts',(8.27969870418431,4.79530138581858,336.100538179217));
#68559=CARTESIAN_POINT('Ctrl Pts',(8.27228701427435,4.82103370919337,335.973045239093));
#68560=CARTESIAN_POINT('Ctrl Pts',(8.26451185432889,4.84802794835314,335.839300032072));
#68561=CARTESIAN_POINT('Ctrl Pts',(8.25673669438341,4.86949507726135,335.704219350032));
#68562=CARTESIAN_POINT('Ctrl Pts',(8.24896153443794,4.88530638429945,335.568299739594));
#68563=CARTESIAN_POINT('Ctrl Pts',(8.24119594181795,4.90109823554221,335.432547378083));
#68564=CARTESIAN_POINT('Ctrl Pts',(8.23343034919796,4.91124806756337,335.295958526694));
#68565=CARTESIAN_POINT('Ctrl Pts',(8.22566475657797,4.91567787271867,335.159041234163));
#68566=CARTESIAN_POINT('Ctrl Pts',(8.21790686316969,4.92010328593513,335.022259688545));
#68567=CARTESIAN_POINT('Ctrl Pts',(8.21014896976141,4.91881994560553,334.88515073796));
#68568=CARTESIAN_POINT('Ctrl Pts',(8.20239107635314,4.91180152206862,334.748228535564));
#68569=CARTESIAN_POINT('Ctrl Pts',(8.19463902071675,4.90478837985661,334.611409366368));
#68570=CARTESIAN_POINT('Ctrl Pts',(8.18688696508037,4.89204876439694,334.474777054429));
#68571=CARTESIAN_POINT('Ctrl Pts',(8.17913490944397,4.87360841273638,334.338846385622));
#68572=CARTESIAN_POINT('Ctrl Pts',(8.17138613671882,4.85517587036418,334.202973281974));
#68573=CARTESIAN_POINT('Ctrl Pts',(8.16363736399368,4.83104744590153,334.067801616982));
#68574=CARTESIAN_POINT('Ctrl Pts',(8.15588859126854,4.8013007654651,333.933841464864));
#68575=CARTESIAN_POINT('Ctrl Pts',(8.148141430702,4.77156027392707,333.799909183612));
#68576=CARTESIAN_POINT('Ctrl Pts',(8.14039427013551,4.7362039361131,333.667188295201));
#68577=CARTESIAN_POINT('Ctrl Pts',(8.13264710956898,4.69536050153297,333.536178691525));
#68578=CARTESIAN_POINT('Ctrl Pts',(8.12489988413112,4.65451672494779,333.405167990833));
#68579=CARTESIAN_POINT('Ctrl Pts',(8.11715265869318,4.60818587628597,333.27586897661));
#68580=CARTESIAN_POINT('Ctrl Pts',(8.10940543325532,4.55654647229255,333.148766003894));
#68581=CARTESIAN_POINT('Ctrl Pts',(8.10165646622969,4.50489545968457,333.021634458242));
#68582=CARTESIAN_POINT('Ctrl Pts',(8.09390749920413,4.44793366416211,332.896700298501));
#68583=CARTESIAN_POINT('Ctrl Pts',(8.0861585321785,4.38588743921164,332.774427167432));
#68584=CARTESIAN_POINT('Ctrl Pts',(8.0784013410826,4.32377536386944,332.652024266444));
#68585=CARTESIAN_POINT('Ctrl Pts',(8.0706441499867,4.25656825690343,332.532288384802));
#68586=CARTESIAN_POINT('Ctrl Pts',(8.0628869588908,4.18453834592537,332.415658324838));
#68587=CARTESIAN_POINT('Ctrl Pts',(8.05512562288319,4.11246994709544,332.298965945757));
#68588=CARTESIAN_POINT('Ctrl Pts',(8.04736428687552,4.03557382840571,332.185383018638));
#68589=CARTESIAN_POINT('Ctrl Pts',(8.0396029508679,3.95416455384308,332.07531783887));
#68590=CARTESIAN_POINT('Ctrl Pts',(8.03182920061177,3.87262506523414,331.965076609966));
#68591=CARTESIAN_POINT('Ctrl Pts',(8.0240554503557,3.78655824098585,331.858364676495));
#68592=CARTESIAN_POINT('Ctrl Pts',(8.01628170009957,3.69631836510102,331.755556502832));
#68593=CARTESIAN_POINT('Ctrl Pts',(8.00887079339987,3.61029047910769,331.657546950443));
#68594=CARTESIAN_POINT('Ctrl Pts',(8.00145988670013,3.52047050468999,331.563085172389));
#68595=CARTESIAN_POINT('Ctrl Pts',(7.99404898000043,3.42719405997353,331.472462057216));
#68596=CARTESIAN_POINT('Ctrl Pts',(7.98627410851617,3.32933661829125,331.377388255517));
#68597=CARTESIAN_POINT('Ctrl Pts',(7.97849923703191,3.22736533653725,331.286239256395));
#68598=CARTESIAN_POINT('Ctrl Pts',(7.97072436554765,3.12162808045917,331.199391997352));
#68599=CARTESIAN_POINT('Ctrl Pts',(7.96295906192474,3.01602094606957,331.112651613714));
#68600=CARTESIAN_POINT('Ctrl Pts',(7.95519375830186,2.90665735776875,331.030202682796));
#68601=CARTESIAN_POINT('Ctrl Pts',(7.94742845467894,2.79392229422256,330.952385730292));
#68602=CARTESIAN_POINT('Ctrl Pts',(7.93967085050097,2.68129900961734,330.874645934763));
#68603=CARTESIAN_POINT('Ctrl Pts',(7.93191324632298,2.56531122190909,330.801529198564));
#68604=CARTESIAN_POINT('Ctrl Pts',(7.92415564214502,2.44637701059868,330.733335895045));
#68605=CARTESIAN_POINT('Ctrl Pts',(7.91640387567222,2.32753229893818,330.665193907936));
#68606=CARTESIAN_POINT('Ctrl Pts',(7.90865210919945,2.20574591469231,330.601968172642));
#68607=CARTESIAN_POINT('Ctrl Pts',(7.90090034272663,2.08146464707327,330.543915621817));
#68608=CARTESIAN_POINT('Ctrl Pts',(7.89315185805154,1.95723599533002,330.485887648195));
#68609=CARTESIAN_POINT('Ctrl Pts',(7.88540337337647,1.83051491441665,330.433028668135));
#68610=CARTESIAN_POINT('Ctrl Pts',(7.87765488870139,1.7017723127771,330.385549430543));
#68611=CARTESIAN_POINT('Ctrl Pts',(7.86990801546764,1.5730564855533,330.33808006714));
#68612=CARTESIAN_POINT('Ctrl Pts',(7.86216114223388,1.4423203403539,330.295988355972));
#68613=CARTESIAN_POINT('Ctrl Pts',(7.85441426900013,1.31005388964136,330.259436545226));
#68614=CARTESIAN_POINT('Ctrl Pts',(7.84666732991003,1.17778631452862,330.222884423753));
#68615=CARTESIAN_POINT('Ctrl Pts',(7.83892039081992,1.04398878473043,330.191872400757));
#68616=CARTESIAN_POINT('Ctrl Pts',(7.83117345172982,0.909165179699443,330.166512466291));
#68617=CARTESIAN_POINT('Ctrl Pts',(7.82342476979832,0.774311243184096,330.14114682656));
#68618=CARTESIAN_POINT('Ctrl Pts',(7.81567608786683,0.638431156179882,330.121435877864));
#68619=CARTESIAN_POINT('Ctrl Pts',(7.80792740593532,0.502037267884032,330.107440174698));
#68620=CARTESIAN_POINT('Ctrl Pts',(7.80017049635155,0.365498554765905,330.093429610711));
#68621=CARTESIAN_POINT('Ctrl Pts',(7.79241358676781,0.228445340016672,330.085146454658));
#68622=CARTESIAN_POINT('Ctrl Pts',(7.78465667718405,0.0913939089992144,
330.082599241886));
#68623=CARTESIAN_POINT('Ctrl Pts',(7.77689562118348,-0.0457307821677491,
330.080050667515));
#68624=CARTESIAN_POINT('Ctrl Pts',(7.76913456518287,-0.182853297111027,
330.083244136836));
#68625=CARTESIAN_POINT('Ctrl Pts',(7.76137350918231,-0.319460094755516,
330.092136074588));
#68626=CARTESIAN_POINT('Ctrl Pts',(7.7536000335394,-0.45628549764744,330.101042241678));
#68627=CARTESIAN_POINT('Ctrl Pts',(7.74582655789653,-0.592593145221596,
330.115665057905));
#68628=CARTESIAN_POINT('Ctrl Pts',(7.73805308225363,-0.727876451581748,
330.135909238744));
#68629=CARTESIAN_POINT('Ctrl Pts',(7.73063903674461,-0.85690452551417,330.155217368715));
#68630=CARTESIAN_POINT('Ctrl Pts',(7.7232249912356,-0.985000584621647,330.179638587204));
#68631=CARTESIAN_POINT('Ctrl Pts',(7.71581094572659,-1.11173783880216,330.209047898353));
#68632=CARTESIAN_POINT('Ctrl Pts',(7.70803573266196,-1.24464896718422,330.239889853665));
#68633=CARTESIAN_POINT('Ctrl Pts',(7.70026051959734,-1.3764857036768,330.276315585869));
#68634=CARTESIAN_POINT('Ctrl Pts',(7.69248530653272,-1.5067427916735,330.318236526453));
#68635=CARTESIAN_POINT('Ctrl Pts',(7.68471966236776,-1.63683957319427,330.360105875232));
#68636=CARTESIAN_POINT('Ctrl Pts',(7.67695401820283,-1.76536020583765,330.407456857526));
#68637=CARTESIAN_POINT('Ctrl Pts',(7.66918837403787,-1.8918099704092,330.460149991645));
#68638=CARTESIAN_POINT('Ctrl Pts',(7.66143043069044,-2.01813434080322,330.512790872506));
#68639=CARTESIAN_POINT('Ctrl Pts',(7.65367248734299,-2.14239157140488,330.570763213374));
#68640=CARTESIAN_POINT('Ctrl Pts',(7.64591454399556,-2.26410279659415,330.633877969072));
#68641=CARTESIAN_POINT('Ctrl Pts',(7.63816244005857,-2.38572240964241,330.69694521824));
#68642=CARTESIAN_POINT('Ctrl Pts',(7.63041033612161,-2.50479948615676,330.765146998587));
#68643=CARTESIAN_POINT('Ctrl Pts',(7.62265823218462,-2.6208761551355,330.838246614473));
#68644=CARTESIAN_POINT('Ctrl Pts',(7.61490941379342,-2.73690362776522,330.911315248817));
#68645=CARTESIAN_POINT('Ctrl Pts',(7.60716059540217,-2.84993289204024,330.989277382153));
#68646=CARTESIAN_POINT('Ctrl Pts',(7.59941177701097,-2.95953186226359,331.071851044226));
#68647=CARTESIAN_POINT('Ctrl Pts',(7.59166457238506,-3.06910800745674,331.154407509547));
#68648=CARTESIAN_POINT('Ctrl Pts',(7.58391736775921,-3.17525496759558,331.241573358259));
#68649=CARTESIAN_POINT('Ctrl Pts',(7.5761701631333,-3.27757110396192,331.333024308647));
#68650=CARTESIAN_POINT('Ctrl Pts',(7.56842289527597,-3.3798880754159,331.424476005443));
#68651=CARTESIAN_POINT('Ctrl Pts',(7.56067562741865,-3.47837386931059,331.520212613203));
#68652=CARTESIAN_POINT('Ctrl Pts',(7.55292835956132,-3.57266160545297,331.619870991305));
#68653=CARTESIAN_POINT('Ctrl Pts',(7.54517935179048,-3.66697051712582,331.719551751098));
#68654=CARTESIAN_POINT('Ctrl Pts',(7.5374303440196,-3.75707922637368,331.823155749992));
#68655=CARTESIAN_POINT('Ctrl Pts',(7.52968133624876,-3.84265952213,331.930284889524));
#68656=CARTESIAN_POINT('Ctrl Pts',(7.52192410726055,-3.92833061328026,332.037527686439));
#68657=CARTESIAN_POINT('Ctrl Pts',(7.51416687827237,-4.00946344942378,332.148302789043));
#68658=CARTESIAN_POINT('Ctrl Pts',(7.50640964928417,-4.08577143287314,332.262180637657));
#68659=CARTESIAN_POINT('Ctrl Pts',(7.49864827687753,-4.16212017519473,332.376119312577));
#68660=CARTESIAN_POINT('Ctrl Pts',(7.4908869044709,-4.23363872595838,332.493163702452));
#68661=CARTESIAN_POINT('Ctrl Pts',(7.48312553206426,-4.30008579241826,332.612858353523));
#68662=CARTESIAN_POINT('Ctrl Pts',(7.47535174830598,-4.36663911558953,332.732744410486));
#68663=CARTESIAN_POINT('Ctrl Pts',(7.46757796454767,-4.42810457313419,332.855288848026));
#68664=CARTESIAN_POINT('Ctrl Pts',(7.45980418078938,-4.48428811884057,332.98001407685));
#68665=CARTESIAN_POINT('Ctrl Pts',(7.4523937576771,-4.53784554448783,333.098909423967));
#68666=CARTESIAN_POINT('Ctrl Pts',(7.44498333456483,-4.5866035606663,333.219786036243));
#68667=CARTESIAN_POINT('Ctrl Pts',(7.43757291145255,-4.63043647946362,333.342218026352));
#68668=CARTESIAN_POINT('Ctrl Pts',(7.42853293022947,-4.68390829299926,333.491572911345));
#68669=CARTESIAN_POINT('Ctrl Pts',(7.41949294900638,-4.73019051434829,333.643629749562));
#68670=CARTESIAN_POINT('Ctrl Pts',(7.4104529677833,-4.76904131470013,333.79774046014));
#68671=CARTESIAN_POINT('Ctrl Pts',(7.40145047453499,-4.80773100433867,333.951212087707));
#68672=CARTESIAN_POINT('Ctrl Pts',(7.3924479812867,-4.83905068851853,334.106720477118));
#68673=CARTESIAN_POINT('Ctrl Pts',(7.38344548803838,-4.86280821719862,334.263603839468));
#68674=CARTESIAN_POINT('Ctrl Pts',(7.37451337646857,-4.88638000902782,334.419260684445));
#68675=CARTESIAN_POINT('Ctrl Pts',(7.36558126489878,-4.90250734734599,334.576270960164));
#68676=CARTESIAN_POINT('Ctrl Pts',(7.35664915332899,-4.91104982362841,334.733968625273));
#68677=CARTESIAN_POINT('Ctrl Pts',(7.35170522774001,-4.91577808600577,334.821254315309));
#68678=CARTESIAN_POINT('Ctrl Pts',(7.34676130215096,-4.9181834765372,334.90875025729));
#68679=CARTESIAN_POINT('Ctrl Pts',(7.34181737656198,-4.91824863900072,334.996341111162));
#68680=CARTESIAN_POINT('Ctrl Pts',(7.34181737650883,-4.91824863900143,334.996341112105));
#68681=CARTESIAN_POINT('Ctrl Pts',(7.33405948590145,-4.91835089036512,335.133786599567));
#68682=CARTESIAN_POINT('Ctrl Pts',(7.32630159529412,-4.9126872523713,335.271288781228));
#68683=CARTESIAN_POINT('Ctrl Pts',(7.31854370468673,-4.90127022971028,335.408329766066));
#68684=CARTESIAN_POINT('Ctrl Pts',(7.31078659251573,-4.88985435264751,335.545357000041));
#68685=CARTESIAN_POINT('Ctrl Pts',(7.30302948034469,-4.8726862711426,335.681922741711));
#68686=CARTESIAN_POINT('Ctrl Pts',(7.2952723681737,-4.84983049454056,335.817512835816));
#68687=CARTESIAN_POINT('Ctrl Pts',(7.28751437646116,-4.82697212643223,335.953118303829));
#68688=CARTESIAN_POINT('Ctrl Pts',(7.27975638474862,-4.79842484400952,336.087747520506));
#68689=CARTESIAN_POINT('Ctrl Pts',(7.27199839303609,-4.76430448091855,336.220895521984));
#68690=CARTESIAN_POINT('Ctrl Pts',(7.26423786358946,-4.730172956639,336.354087077803));
#68691=CARTESIAN_POINT('Ctrl Pts',(7.25647733414284,-4.69046481973589,336.485796077464));
#68692=CARTESIAN_POINT('Ctrl Pts',(7.24871680469622,-4.64534596146615,336.615532098347));
#68693=CARTESIAN_POINT('Ctrl Pts',(7.24094709317594,-4.60017371963766,336.745421619802));
#68694=CARTESIAN_POINT('Ctrl Pts',(7.23317738165566,-4.54957809758052,336.873333132058));
#68695=CARTESIAN_POINT('Ctrl Pts',(7.22540767013538,-4.49377363385272,336.998795034562));
#68696=CARTESIAN_POINT('Ctrl Pts',(7.21763315266209,-4.43793465228857,337.124334541493));
#68697=CARTESIAN_POINT('Ctrl Pts',(7.20985863518881,-4.37688058228527,337.247421071832));
#68698=CARTESIAN_POINT('Ctrl Pts',(7.20208411771551,-4.31087180155181,337.367607943281));
#68699=CARTESIAN_POINT('Ctrl Pts',(7.19429674930069,-4.24475391115534,337.487993478435));
#68700=CARTESIAN_POINT('Ctrl Pts',(7.18650938088584,-4.17366514813585,337.605469445913));
#68701=CARTESIAN_POINT('Ctrl Pts',(7.17872201247101,-4.09790953495292,337.71961771318));
#68702=CARTESIAN_POINT('Ctrl Pts',(7.1722596340402,-4.03504344019951,337.814344103535));
#68703=CARTESIAN_POINT('Ctrl Pts',(7.16579725560938,-3.96896432051202,337.906779326875));
#68704=CARTESIAN_POINT('Ctrl Pts',(7.15933487717857,-3.89986615034613,337.996702699949));
#68705=CARTESIAN_POINT('Ctrl Pts',(7.15156122621795,-3.81674736325525,338.104872303908));
#68706=CARTESIAN_POINT('Ctrl Pts',(7.14378757525728,-3.72899314005567,338.209752401944));
#68707=CARTESIAN_POINT('Ctrl Pts',(7.13601392429661,-3.63689323404313,338.310919912452));
#68708=CARTESIAN_POINT('Ctrl Pts',(7.12824984273351,-3.54490670340889,338.411962885321));
#68709=CARTESIAN_POINT('Ctrl Pts',(7.12048576117038,-3.4485853946733,338.509302077618));
#68710=CARTESIAN_POINT('Ctrl Pts',(7.11272167960729,-3.34826104067228,338.602545081747));
#68711=CARTESIAN_POINT('Ctrl Pts',(7.10496529775928,-3.24803617930738,338.695695615883));
#68712=CARTESIAN_POINT('Ctrl Pts',(7.09720891591133,-3.14381645743581,338.784757781369));
#68713=CARTESIAN_POINT('Ctrl Pts',(7.08945253406333,-3.0359721560843,338.869374126391));
#68714=CARTESIAN_POINT('Ctrl Pts',(7.08170198893485,-2.92820900815613,338.953926797152));
#68715=CARTESIAN_POINT('Ctrl Pts',(7.07395144380637,-2.81682701609293,339.034040066058));
#68716=CARTESIAN_POINT('Ctrl Pts',(7.06620089867789,-2.70223113714075,339.109395325832));
#68717=CARTESIAN_POINT('Ctrl Pts',(7.0584536295921,-2.58768369619975,339.184718734034));
#68718=CARTESIAN_POINT('Ctrl Pts',(7.05070636050632,-2.46992539625358,339.255287918658));
#68719=CARTESIAN_POINT('Ctrl Pts',(7.04295909142053,-2.3493917231837,339.320826494264));
#68720=CARTESIAN_POINT('Ctrl Pts',(7.03521343011243,-2.22888306426368,339.38635146876));
#68721=CARTESIAN_POINT('Ctrl Pts',(7.02746776880427,-2.10560052116608,339.446847724117));
#68722=CARTESIAN_POINT('Ctrl Pts',(7.01972210749616,-1.98000547773249,339.502084114124));
#68723=CARTESIAN_POINT('Ctrl Pts',(7.01197637554554,-1.85440928883823,339.557321007902));
#68724=CARTESIAN_POINT('Ctrl Pts',(7.00423064359498,-1.7265009154913,339.60729778324));
#68725=CARTESIAN_POINT('Ctrl Pts',(6.99648491164436,-1.5967627089283,339.651831028087));
#68726=CARTESIAN_POINT('Ctrl Pts',(6.98873743093975,-1.46699521136894,339.696374327206));
#68727=CARTESIAN_POINT('Ctrl Pts',(6.98098995023512,-1.33539742830905,339.735471523376));
#68728=CARTESIAN_POINT('Ctrl Pts',(6.9732424695305,-1.20246750549885,339.768988882428));
#68729=CARTESIAN_POINT('Ctrl Pts',(6.96548674509676,-1.06939613822188,339.802541905722));
#68730=CARTESIAN_POINT('Ctrl Pts',(6.95773102066302,-0.934990179439701,
339.830503135968));
#68731=CARTESIAN_POINT('Ctrl Pts',(6.94997529622927,-0.799759167171889,
339.852789747869));
#68732=CARTESIAN_POINT('Ctrl Pts',(6.94221541850505,-0.664455736952739,
339.875088294538));
#68733=CARTESIAN_POINT('Ctrl Pts',(6.93445554078086,-0.528326760827144,
339.891706120434));
#68734=CARTESIAN_POINT('Ctrl Pts',(6.92669566305665,-0.391886567790598,
339.902612362862));
#68735=CARTESIAN_POINT('Ctrl Pts',(6.91892334207123,-0.255227587677649,
339.913536093867));
#68736=CARTESIAN_POINT('Ctrl Pts',(6.91115102108579,-0.118256784361598,
339.918729924733));
#68737=CARTESIAN_POINT('Ctrl Pts',(6.90337870010038,0.0185109458667954,
339.918215164812));
#68738=CARTESIAN_POINT('Ctrl Pts',(6.89595141436849,0.149207170741441,339.917723256535));
#68739=CARTESIAN_POINT('Ctrl Pts',(6.88852412863661,0.279717674553717,339.912018754077));
#68740=CARTESIAN_POINT('Ctrl Pts',(6.88109684290473,0.409599680461112,339.901164266199));
#68741=CARTESIAN_POINT('Ctrl Pts',(6.87332050122199,0.545585677612053,339.889799656087));
#68742=CARTESIAN_POINT('Ctrl Pts',(6.86554415953925,0.681313005923244,339.872753288523));
#68743=CARTESIAN_POINT('Ctrl Pts',(6.85776781785651,0.816268807056172,339.850040030466));
#68744=CARTESIAN_POINT('Ctrl Pts',(6.85000105068764,0.951058445712975,339.827354737797));
#68745=CARTESIAN_POINT('Ctrl Pts',(6.84223428351876,1.08507806565111,339.799016501738));
#68746=CARTESIAN_POINT('Ctrl Pts',(6.83446751634989,1.21781790235197,339.765092089269));
#68747=CARTESIAN_POINT('Ctrl Pts',(6.82670845668871,1.3504260120047,339.731201342373));
#68748=CARTESIAN_POINT('Ctrl Pts',(6.81894939702748,1.48175648970576,339.691735547248));
#68749=CARTESIAN_POINT('Ctrl Pts',(6.8111903373663,1.61130811837897,339.646812801281));
#68750=CARTESIAN_POINT('Ctrl Pts',(6.80343712487902,1.74076211783737,339.601923908785));
#68751=CARTESIAN_POINT('Ctrl Pts',(6.79568391239175,1.86843956884725,339.551586378364));
#68752=CARTESIAN_POINT('Ctrl Pts',(6.78793069990448,1.9938531633102,339.495968485839));
#68753=CARTESIAN_POINT('Ctrl Pts',(6.78018078853269,2.11921335993852,339.440374273961));
#68754=CARTESIAN_POINT('Ctrl Pts',(6.77243087716089,2.24231126072714,339.37950432975));
#68755=CARTESIAN_POINT('Ctrl Pts',(6.7646809657891,2.36267854936551,339.313575446757));
#68756=CARTESIAN_POINT('Ctrl Pts',(6.75693267779888,2.48302062454926,339.247660373952));
#68757=CARTESIAN_POINT('Ctrl Pts',(6.74918438980871,2.60063288282723,339.1766886578));
#68758=CARTESIAN_POINT('Ctrl Pts',(6.74143610181849,2.71507103704166,339.100923350456));
#68759=CARTESIAN_POINT('Ctrl Pts',(6.73368776118936,2.82950996870531,339.025157528392));
#68760=CARTESIAN_POINT('Ctrl Pts',(6.72593942056018,2.94077442746838,338.944598265858));
#68761=CARTESIAN_POINT('Ctrl Pts',(6.71819107993105,3.04844891825089,338.859552079622));
#68762=CARTESIAN_POINT('Ctrl Pts',(6.71044101096481,3.15614742679748,338.774486923069));
#68763=CARTESIAN_POINT('Ctrl Pts',(6.70269094199856,3.26025406733491,338.684933093379));
#68764=CARTESIAN_POINT('Ctrl Pts',(6.69494087303232,3.36038656790733,338.591237276584));
#68765=CARTESIAN_POINT('Ctrl Pts',(6.68718260700293,3.4606249762381,338.497442359958));
#68766=CARTESIAN_POINT('Ctrl Pts',(6.67942434097348,3.5568805622272,338.399496972382));
#68767=CARTESIAN_POINT('Ctrl Pts',(6.67166607494408,3.64880769520589,338.29778493324));
#68768=CARTESIAN_POINT('Ctrl Pts',(6.66390367701195,3.74078378680122,338.19601872423));
#68769=CARTESIAN_POINT('Ctrl Pts',(6.65614127907988,3.82842658239426,338.09048216683));
#68770=CARTESIAN_POINT('Ctrl Pts',(6.64837888114775,3.91143154575164,337.981591240495));
#68771=CARTESIAN_POINT('Ctrl Pts',(6.64060410176749,3.99456890655333,337.872526627193));
#68772=CARTESIAN_POINT('Ctrl Pts',(6.63282932238728,4.07305342871677,337.760097273816));
#68773=CARTESIAN_POINT('Ctrl Pts',(6.62505454300702,4.14662413498238,337.644747879417));
#68774=CARTESIAN_POINT('Ctrl Pts',(6.61765596488162,4.21663494704854,337.534979940748));
#68775=CARTESIAN_POINT('Ctrl Pts',(6.6102573867562,4.28219618884176,337.422568170264));
#68776=CARTESIAN_POINT('Ctrl Pts',(6.6028588086308,4.34312291699588,337.307913861123));
#68777=CARTESIAN_POINT('Ctrl Pts',(6.59508121422942,4.40717081535613,337.187386011345));
#68778=CARTESIAN_POINT('Ctrl Pts',(6.58730361982803,4.46629835475321,337.064000567731));
#68779=CARTESIAN_POINT('Ctrl Pts',(6.57952602542665,4.52024059322292,336.938197111204));
#68780=CARTESIAN_POINT('Ctrl Pts',(6.57175797883564,4.57411661195453,336.812548091574));
#68781=CARTESIAN_POINT('Ctrl Pts',(6.5639899322446,4.6228198430109,336.684487320884));
#68782=CARTESIAN_POINT('Ctrl Pts',(6.5562218856536,4.66613067559802,336.554479842501));
#68783=CARTESIAN_POINT('Ctrl Pts',(6.54846152154273,4.70939867442934,336.424600939541));
#68784=CARTESIAN_POINT('Ctrl Pts',(6.54070115743189,4.74728476526471,336.292779528521));
#68785=CARTESIAN_POINT('Ctrl Pts',(6.53294079332102,4.77961713734269,336.159501221612));
#68786=CARTESIAN_POINT('Ctrl Pts',(6.52518625299873,4.81192524549478,336.02632293381));
#68787=CARTESIAN_POINT('Ctrl Pts',(6.51743171267646,4.83868783911139,335.89169030443));
#68788=CARTESIAN_POINT('Ctrl Pts',(6.50967717235417,4.8597828370889,335.756104383558));
#68789=CARTESIAN_POINT('Ctrl Pts',(6.5019259026434,4.88086893788613,335.620575648394));
#68790=CARTESIAN_POINT('Ctrl Pts',(6.4941746329326,4.89629213753075,335.484094806573));
#68791=CARTESIAN_POINT('Ctrl Pts',(6.48642336322183,4.90598143576346,335.347173176447));
#68792=CARTESIAN_POINT('Ctrl Pts',(6.47867369856857,4.91566872763059,335.210279898719));
#68793=CARTESIAN_POINT('Ctrl Pts',(6.47092403391527,4.91962445223797,335.072946403604));
#68794=CARTESIAN_POINT('Ctrl Pts',(6.46317436926199,4.91782951458132,334.935688818913));
#68795=CARTESIAN_POINT('Ctrl Pts',(6.45542463505456,4.9160345608149,334.798430002318));
#68796=CARTESIAN_POINT('Ctrl Pts',(6.44767490084714,4.90848884696551,334.661247488054));
#68797=CARTESIAN_POINT('Ctrl Pts',(6.43992516663971,4.89522540931375,334.52465669826));
#68798=CARTESIAN_POINT('Ctrl Pts',(6.43217368857847,4.88195898710851,334.388035172655));
#68799=CARTESIAN_POINT('Ctrl Pts',(6.42442221051726,4.8629723185987,334.252006025156));
#68800=CARTESIAN_POINT('Ctrl Pts',(6.41667073245603,4.83835019667313,334.117078465064));
#68801=CARTESIAN_POINT('Ctrl Pts',(6.40891104105662,4.81370198555369,333.982007937958));
#68802=CARTESIAN_POINT('Ctrl Pts',(6.40115134965721,4.78340646312433,333.848041714744));
#68803=CARTESIAN_POINT('Ctrl Pts',(6.3933916582578,4.74759947504644,333.71567827744));
#68804=CARTESIAN_POINT('Ctrl Pts',(6.38562782385426,4.71177336913359,333.583244169508));
#68805=CARTESIAN_POINT('Ctrl Pts',(6.37786398945076,4.67043005160834,333.452414924919));
#68806=CARTESIAN_POINT('Ctrl Pts',(6.37010015504723,4.62375464775931,333.323671863917));
#68807=CARTESIAN_POINT('Ctrl Pts',(6.36232393501272,4.57700478272297,333.194723419343));
#68808=CARTESIAN_POINT('Ctrl Pts',(6.35454771497819,4.52490598174406,333.067868170361));
#68809=CARTESIAN_POINT('Ctrl Pts',(6.34677149494368,4.46769108994829,332.943566342598));
#68810=CARTESIAN_POINT('Ctrl Pts',(6.33938792141474,4.41336516312913,332.825540916234));
#68811=CARTESIAN_POINT('Ctrl Pts',(6.33200434788581,4.35442727196074,332.709817616591));
#68812=CARTESIAN_POINT('Ctrl Pts',(6.32462077435687,4.29111327678704,332.596766780297));
#68813=CARTESIAN_POINT('Ctrl Pts',(6.31685531416248,4.22452461110345,332.477868828548));
#68814=CARTESIAN_POINT('Ctrl Pts',(6.3090898539681,4.15288382142553,332.36154993445));
#68815=CARTESIAN_POINT('Ctrl Pts',(6.30132439377371,4.07641570313481,332.248269984585));
#68816=CARTESIAN_POINT('Ctrl Pts',(6.2935685171197,4.00004195597996,332.135129836218));
#68817=CARTESIAN_POINT('Ctrl Pts',(6.28581264046562,3.91885295049355,332.02502149187));
#68818=CARTESIAN_POINT('Ctrl Pts',(6.27805676381161,3.83311947643843,331.918380597503));
#68819=CARTESIAN_POINT('Ctrl Pts',(6.27030859261078,3.74747117847623,331.811845650722));
#68820=CARTESIAN_POINT('Ctrl Pts',(6.26256042141,3.65728764039709,331.708771602173));
#68821=CARTESIAN_POINT('Ctrl Pts',(6.25481225020917,3.5628828680657,331.609565111826));
#68822=CARTESIAN_POINT('Ctrl Pts',(6.24706991314045,3.4685491795939,331.510433320884));
#68823=CARTESIAN_POINT('Ctrl Pts',(6.2393275760717,3.37000085219638,331.415163574706));
#68824=CARTESIAN_POINT('Ctrl Pts',(6.23158523900298,3.26759183428722,331.324129128084));
#68825=CARTESIAN_POINT('Ctrl Pts',(6.22384614567352,3.16522572178886,331.233132821369));
#68826=CARTESIAN_POINT('Ctrl Pts',(6.21610705234402,3.05900242779361,331.146368545235));
#68827=CARTESIAN_POINT('Ctrl Pts',(6.20836795901457,2.94931222402584,331.06417220045));
#68828=CARTESIAN_POINT('Ctrl Pts',(6.2006304528915,2.83964451656158,330.981992713267));
#68829=CARTESIAN_POINT('Ctrl Pts',(6.19289294676851,2.72651162694693,330.904379529035));
#68830=CARTESIAN_POINT('Ctrl Pts',(6.18515544064545,2.61033599307547,330.831627527949));
#68831=CARTESIAN_POINT('Ctrl Pts',(6.17741783588129,2.4941588781465,330.758874599389));
#68832=CARTESIAN_POINT('Ctrl Pts',(6.16968023111711,2.37493927381613,330.690983185531));
#68833=CARTESIAN_POINT('Ctrl Pts',(6.16194262635295,2.25312725560259,330.628203958033));
#68834=CARTESIAN_POINT('Ctrl Pts',(6.15420323738419,2.13128714890814,330.56541025435));
#68835=CARTESIAN_POINT('Ctrl Pts',(6.14646384841544,2.00685378717366,330.507731262158));
#68836=CARTESIAN_POINT('Ctrl Pts',(6.13872445944668,1.88030003422444,330.455370769381));
#68837=CARTESIAN_POINT('Ctrl Pts',(6.1309767254356,1.75360982393633,330.402953818591));
#68838=CARTESIAN_POINT('Ctrl Pts',(6.12322899142452,1.62479501807467,330.355866972769));
#68839=CARTESIAN_POINT('Ctrl Pts',(6.11548125741345,1.49434708877615,330.314265282715));
#68840=CARTESIAN_POINT('Ctrl Pts',(6.10772932783854,1.36382851913112,330.272641064455));
#68841=CARTESIAN_POINT('Ctrl Pts',(6.09997739826369,1.2316754418383,330.236508023425));
#68842=CARTESIAN_POINT('Ctrl Pts',(6.09222546868878,1.09839153265352,330.205970473235));
#68843=CARTESIAN_POINT('Ctrl Pts',(6.08446094315674,0.964891053079382,330.175383303183));
#68844=CARTESIAN_POINT('Ctrl Pts',(6.07669641762463,0.830256455393671,330.150409863777));
#68845=CARTESIAN_POINT('Ctrl Pts',(6.06893189209259,0.694999476123359,330.131102918454));
#68846=CARTESIAN_POINT('Ctrl Pts',(6.06141550808936,0.564065088552856,330.112412991507));
#68847=CARTESIAN_POINT('Ctrl Pts',(6.0538991240861,0.432547813631449,330.099032887664));
#68848=CARTESIAN_POINT('Ctrl Pts',(6.04638274008286,0.300911661534685,330.090963920029));
#68849=CARTESIAN_POINT('Ctrl Pts',(6.03859686493552,0.164555849396764,330.082605649012));
#68850=CARTESIAN_POINT('Ctrl Pts',(6.03081098978817,0.0276383429979844,
330.079919834404));
#68851=CARTESIAN_POINT('Ctrl Pts',(6.02302511464083,-0.109330180294248,
330.082965327133));
#68852=CARTESIAN_POINT('Ctrl Pts',(6.0152488453941,-0.246129717313841,330.086007062456));
#68853=CARTESIAN_POINT('Ctrl Pts',(6.00747257614737,-0.382979760028109,
330.094766026414));
#68854=CARTESIAN_POINT('Ctrl Pts',(5.99969630690063,-0.519365263713141,
330.109249261581));
#68855=CARTESIAN_POINT('Ctrl Pts',(5.99192778607104,-0.655614870383523,
330.123718065387));
#68856=CARTESIAN_POINT('Ctrl Pts',(5.98415926524146,-0.791400474143886,
330.143899748102));
#68857=CARTESIAN_POINT('Ctrl Pts',(5.97639074441187,-0.926208128716363,
330.169749326919));
#68858=CARTESIAN_POINT('Ctrl Pts',(5.96862812115544,-1.06091344231262,330.195579281693));
#68859=CARTESIAN_POINT('Ctrl Pts',(5.96086549789901,-1.19464190332912,330.22706849442));
#68860=CARTESIAN_POINT('Ctrl Pts',(5.95310287464258,-1.32688612205344,330.264120326528));
#68861=CARTESIAN_POINT('Ctrl Pts',(5.94534366171854,-1.45907224228106,330.301155880755));
#68862=CARTESIAN_POINT('Ctrl Pts',(5.93758444879453,-1.58977504287365,330.343749088023));
#68863=CARTESIAN_POINT('Ctrl Pts',(5.92982523587048,-1.7184989556453,330.391752567196));
#68864=CARTESIAN_POINT('Ctrl Pts',(5.92206771428337,-1.8471948094488,330.439745582671));
#68865=CARTESIAN_POINT('Ctrl Pts',(5.91431019269621,-1.97391226858973,330.493146387989));
#68866=CARTESIAN_POINT('Ctrl Pts',(5.9065526711091,-2.09817287370277,330.55175836374));
#68867=CARTESIAN_POINT('Ctrl Pts',(5.89879517343114,-2.22243309583706,330.610370158845));
#68868=CARTESIAN_POINT('Ctrl Pts',(5.89103767575322,-2.34423612646736,330.67419292631));
#68869=CARTESIAN_POINT('Ctrl Pts',(5.88328017807527,-2.46312571868049,330.742982880411));
#68870=CARTESIAN_POINT('Ctrl Pts',(5.8755210372566,-2.58204049328334,330.811787405135));
#68871=CARTESIAN_POINT('Ctrl Pts',(5.8677618964379,-2.69804026419989,330.885561014991));
#68872=CARTESIAN_POINT('Ctrl Pts',(5.86000275561923,-2.81069584596198,330.96401537119));
#68873=CARTESIAN_POINT('Ctrl Pts',(5.85223560277196,-2.92346775500368,331.042550738749));
#68874=CARTESIAN_POINT('Ctrl Pts',(5.84446844992471,-3.03288825638894,331.125776284726));
#68875=CARTESIAN_POINT('Ctrl Pts',(5.83670129707744,-3.13855905018823,331.213361629231));
#68876=CARTESIAN_POINT('Ctrl Pts',(5.82893009938131,-3.24428487346845,331.300992584977));
#68877=CARTESIAN_POINT('Ctrl Pts',(5.82115890168517,-3.34625680853045,331.392987602795));
#68878=CARTESIAN_POINT('Ctrl Pts',(5.81338770398904,-3.44411254127841,331.488978515374));
#68879=CARTESIAN_POINT('Ctrl Pts',(5.80560436101053,-3.5421212086901,331.585119448166));
#68880=CARTESIAN_POINT('Ctrl Pts',(5.79782101803203,-3.63600055173004,331.685268470824));
#68881=CARTESIAN_POINT('Ctrl Pts',(5.79003767505353,-3.7254271888263,331.789022684095));
#68882=CARTESIAN_POINT('Ctrl Pts',(5.78274001863869,-3.80927353526954,331.886302554986));
#68883=CARTESIAN_POINT('Ctrl Pts',(5.77544236222388,-3.88920577385065,331.986751200925));
#68884=CARTESIAN_POINT('Ctrl Pts',(5.76814470580905,-3.96499237429082,332.090013997574));
#68885=CARTESIAN_POINT('Ctrl Pts',(5.76033139000508,-4.04613412847658,332.200573442298));
#68886=CARTESIAN_POINT('Ctrl Pts',(5.75251807420117,-4.12277500424751,332.314702062708));
#68887=CARTESIAN_POINT('Ctrl Pts',(5.74470475839726,-4.19458675120634,332.431999795735));
#68888=CARTESIAN_POINT('Ctrl Pts',(5.73690099457361,-4.26631070645083,332.549154129256));
#68889=CARTESIAN_POINT('Ctrl Pts',(5.72909723074999,-4.33321707948485,332.669469541798));
#68890=CARTESIAN_POINT('Ctrl Pts',(5.72129346692634,-4.39501868564208,332.792514141527));
#68891=CARTESIAN_POINT('Ctrl Pts',(5.71349761094548,-4.45675766594377,332.915434055608));
#68892=CARTESIAN_POINT('Ctrl Pts',(5.70570175496459,-4.51340200123606,333.041077311382));
#68893=CARTESIAN_POINT('Ctrl Pts',(5.69790589898372,-4.56470872838734,333.16898462937));
#68894=CARTESIAN_POINT('Ctrl Pts',(5.69011631244605,-4.61597419456453,333.296789084033));
#68895=CARTESIAN_POINT('Ctrl Pts',(5.68232672590839,-4.661910453602,333.426853620556));
#68896=CARTESIAN_POINT('Ctrl Pts',(5.67453713937073,-4.70232142528769,333.558696327702));
#68897=CARTESIAN_POINT('Ctrl Pts',(5.66675225035573,-4.74270802707204,333.690459526891));
#68898=CARTESIAN_POINT('Ctrl Pts',(5.65896736134076,-4.77757586349578,333.823998393796));
#68899=CARTESIAN_POINT('Ctrl Pts',(5.65118247232576,-4.80677787629,333.958813412251));
#68900=CARTESIAN_POINT('Ctrl Pts',(5.64340035908543,-4.83596947683462,334.093580361155));
#68901=CARTESIAN_POINT('Ctrl Pts',(5.63561824584508,-4.85949919536628,334.229622179123));
#68902=CARTESIAN_POINT('Ctrl Pts',(5.62783613260476,-4.87727056797979,334.366426903019));
#68903=CARTESIAN_POINT('Ctrl Pts',(5.6200540689251,-4.89504182741568,334.503230755669));
#68904=CARTESIAN_POINT('Ctrl Pts',(5.6122720052455,-4.9070547585848,334.640797123079));
#68905=CARTESIAN_POINT('Ctrl Pts',(5.60448994156584,-4.91326450350974,334.778606727629));
#68906=CARTESIAN_POINT('Ctrl Pts',(5.60026575321351,-4.91663522023254,334.853411271815));
#68907=CARTESIAN_POINT('Ctrl Pts',(5.59604156486116,-4.91829696519244,334.928287391275));
#68908=CARTESIAN_POINT('Ctrl Pts',(5.59181737650883,-4.91824899013982,335.003151743738));
#68909=CARTESIAN_POINT('Origin',(186.231676812499,0.,335.));
#68910=CARTESIAN_POINT('',(186.231676812499,-7.,335.));
#68911=CARTESIAN_POINT('Origin',(186.231676812499,0.,335.));
#68912=CARTESIAN_POINT('',(186.231676812499,5.77350269189626,335.));
#68913=CARTESIAN_POINT('',(186.231676812499,2.88675134594813,340.));
#68914=CARTESIAN_POINT('',(186.231676812499,5.05181485540923,336.25));
#68915=CARTESIAN_POINT('',(186.231676812499,2.88675134594813,330.));
#68916=CARTESIAN_POINT('',(186.231676812499,3.60843918243516,331.25));
#68917=CARTESIAN_POINT('',(186.231676812499,-2.88675134594813,330.));
#68918=CARTESIAN_POINT('',(186.231676812499,-1.44337567297406,330.));
#68919=CARTESIAN_POINT('',(186.231676812499,-5.77350269189625,335.));
#68920=CARTESIAN_POINT('',(186.231676812499,-5.05181485540922,333.75));
#68921=CARTESIAN_POINT('',(186.231676812499,-2.88675134594811,340.));
#68922=CARTESIAN_POINT('',(186.231676812499,-3.60843918243515,338.75));
#68923=CARTESIAN_POINT('',(186.231676812499,1.44337567297406,340.));
#68924=CARTESIAN_POINT('Origin',(185.231676812499,0.,335.));
#68925=CARTESIAN_POINT('',(185.231676812499,-7.,335.));
#68926=CARTESIAN_POINT('',(185.231676812499,-7.,335.));
#68927=CARTESIAN_POINT('Origin',(185.231676812499,0.,335.));
#68928=CARTESIAN_POINT('Origin',(185.231676812499,-5.77350269189625,335.));
#68929=CARTESIAN_POINT('',(205.231676812499,-2.88675134594813,330.));
#68930=CARTESIAN_POINT('',(185.231676812499,-2.88675134594813,330.));
#68931=CARTESIAN_POINT('',(205.231676812499,-5.77350269189625,335.));
#68932=CARTESIAN_POINT('',(205.231676812499,-5.77350269189625,335.));
#68933=CARTESIAN_POINT('',(185.231676812499,-5.77350269189625,335.));
#68934=CARTESIAN_POINT('Origin',(185.231676812499,-2.88675134594813,330.));
#68935=CARTESIAN_POINT('',(205.231676812499,2.88675134594813,330.));
#68936=CARTESIAN_POINT('',(185.231676812499,2.88675134594813,330.));
#68937=CARTESIAN_POINT('',(205.231676812499,-2.88675134594813,330.));
#68938=CARTESIAN_POINT('Origin',(185.231676812499,2.88675134594813,330.));
#68939=CARTESIAN_POINT('',(205.231676812499,5.77350269189626,335.));
#68940=CARTESIAN_POINT('',(185.231676812499,5.77350269189626,335.));
#68941=CARTESIAN_POINT('',(205.231676812499,2.88675134594813,330.));
#68942=CARTESIAN_POINT('Origin',(185.231676812499,4.44089209850063E-15,
335.));
#68943=CARTESIAN_POINT('',(185.23167683184,-3.96013600436147,338.142060500916));
#68944=CARTESIAN_POINT('Ctrl Pts',(185.231676812499,-3.96013605566283,338.142060549271));
#68945=CARTESIAN_POINT('Ctrl Pts',(185.231676812499,-4.28438313788062,337.798053387465));
#68946=CARTESIAN_POINT('Ctrl Pts',(185.231676812499,-4.5597175012955,337.407746480001));
#68947=CARTESIAN_POINT('Ctrl Pts',(185.231676812499,-5.00660837949084,336.559057380709));
#68948=CARTESIAN_POINT('Ctrl Pts',(185.231676812499,-5.17583108149262,336.097536688629));
#68949=CARTESIAN_POINT('Ctrl Pts',(185.231676812499,-5.43533327152918,334.920836850492));
#68950=CARTESIAN_POINT('Ctrl Pts',(185.231676812499,-5.44158388072912,334.250043530421));
#68951=CARTESIAN_POINT('Ctrl Pts',(185.231676812499,-5.19996495846416,332.894580477494));
#68952=CARTESIAN_POINT('Ctrl Pts',(185.231676812499,-4.93922833436616,332.223849290227));
#68953=CARTESIAN_POINT('Ctrl Pts',(185.231676812499,-4.3237022218484,331.228008604537));
#68954=CARTESIAN_POINT('Ctrl Pts',(185.231676812499,-4.03283623373639,330.863982759591));
#68955=CARTESIAN_POINT('Ctrl Pts',(185.231676812499,-3.36666521490454,330.20750410331));
#68956=CARTESIAN_POINT('Ctrl Pts',(185.231676812499,-2.99060132980376,329.917370541692));
#68957=CARTESIAN_POINT('Ctrl Pts',(185.231676812499,-2.58391981634258,329.677285566066));
#68958=CARTESIAN_POINT('',(185.229482559938,5.39695405107274,334.345551452481));
#68959=CARTESIAN_POINT('Ctrl Pts',(185.227994231758,2.5854165783574,329.675696584773));
#68960=CARTESIAN_POINT('Ctrl Pts',(185.227640459499,2.7081737407366,329.747941861091));
#68961=CARTESIAN_POINT('Ctrl Pts',(185.227524853352,2.82806177680362,329.8243971901));
#68962=CARTESIAN_POINT('Ctrl Pts',(185.227590200135,2.94476028939518,329.90515414262));
#68963=CARTESIAN_POINT('Ctrl Pts',(185.227662105192,3.07317079076938,329.99401595013));
#68964=CARTESIAN_POINT('Ctrl Pts',(185.227953107064,3.19772021473749,330.088086613307));
#68965=CARTESIAN_POINT('Ctrl Pts',(185.228386979994,3.31819273430149,330.187071053314));
#68966=CARTESIAN_POINT('Ctrl Pts',(185.228821913669,3.43895978855643,330.286297493335));
#68967=CARTESIAN_POINT('Ctrl Pts',(185.229400417846,3.55562982264465,330.390462569785));
#68968=CARTESIAN_POINT('Ctrl Pts',(185.230045706324,3.66793313993279,330.499263559958));
#68969=CARTESIAN_POINT('Ctrl Pts',(185.230688110766,3.77973453152617,330.60757827765));
#68970=CARTESIAN_POINT('Ctrl Pts',(185.231396703875,3.88720789030099,330.720488276194));
#68971=CARTESIAN_POINT('Ctrl Pts',(185.232095724413,3.99003858553928,330.837678118006));
#68972=CARTESIAN_POINT('Ctrl Pts',(185.232737549218,4.08445539794597,330.945279173165));
#68973=CARTESIAN_POINT('Ctrl Pts',(185.233371303873,4.17495751476312,331.056488543143));
#68974=CARTESIAN_POINT('Ctrl Pts',(185.233938343949,4.26126815979221,331.171042131527));
#68975=CARTESIAN_POINT('Ctrl Pts',(185.234525681538,4.35066834219649,331.289696229098));
#68976=CARTESIAN_POINT('Ctrl Pts',(185.234997494895,4.43522375791577,331.411591120723));
#68977=CARTESIAN_POINT('Ctrl Pts',(185.23535434099,4.51484630737464,331.536408496964));
#68978=CARTESIAN_POINT('Ctrl Pts',(185.235715534686,4.59543893075985,331.662746574099));
#68979=CARTESIAN_POINT('Ctrl Pts',(185.23595894267,4.67097812182971,331.792079505726));
#68980=CARTESIAN_POINT('Ctrl Pts',(185.236085142519,4.7413275791168,331.924105489045));
#68981=CARTESIAN_POINT('Ctrl Pts',(185.236210806957,4.81137857461677,332.05557134422));
#68982=CARTESIAN_POINT('Ctrl Pts',(185.236220255677,4.87628401583103,332.189708219156));
#68983=CARTESIAN_POINT('Ctrl Pts',(185.236114058936,4.93586070137055,332.326234669537));
#68984=CARTESIAN_POINT('Ctrl Pts',(185.236010030404,4.99422101533023,332.459973672234));
#68985=CARTESIAN_POINT('Ctrl Pts',(185.235795030449,5.0474680260653,332.596006376573));
#68986=CARTESIAN_POINT('Ctrl Pts',(185.235469595109,5.09538063730756,332.734073214484));
#68987=CARTESIAN_POINT('Ctrl Pts',(185.235167173811,5.13990497844604,332.862376281915));
#68988=CARTESIAN_POINT('Ctrl Pts',(185.234769384316,5.17982239323938,332.992436422879));
#68989=CARTESIAN_POINT('Ctrl Pts',(185.234276656793,5.21491522649548,333.124041555105));
#68990=CARTESIAN_POINT('Ctrl Pts',(185.233707355273,5.25546178082372,333.276099230379));
#68991=CARTESIAN_POINT('Ctrl Pts',(185.233047946604,5.28946248209387,333.429600643541));
#68992=CARTESIAN_POINT('Ctrl Pts',(185.232384613167,5.3168113587751,333.584078469419));
#68993=CARTESIAN_POINT('Ctrl Pts',(185.231733768864,5.343645315285,333.735647812088));
#68994=CARTESIAN_POINT('Ctrl Pts',(185.23107914619,5.36407628133255,333.888157544675));
#68995=CARTESIAN_POINT('Ctrl Pts',(185.230502150722,5.37797927517833,334.041209013612));
#68996=CARTESIAN_POINT('Ctrl Pts',(185.230120463025,5.38717623078736,334.142453938362));
#68997=CARTESIAN_POINT('Ctrl Pts',(185.229772744539,5.3935160662643,334.243936791883));
#68998=CARTESIAN_POINT('Ctrl Pts',(185.229482559938,5.39695405107274,334.345551452481));
#68999=CARTESIAN_POINT('',(185.231676812499,5.18549872251091,336.021916810612));
#69000=CARTESIAN_POINT('Ctrl Pts',(185.231676812499,5.4007694079033,334.346099854067));
#69001=CARTESIAN_POINT('Ctrl Pts',(185.231676812499,5.40584147874406,334.477371134359));
#69002=CARTESIAN_POINT('Ctrl Pts',(185.231676812499,5.40590729260707,334.608862633821));
#69003=CARTESIAN_POINT('Ctrl Pts',(185.231676812499,5.40076593664994,334.740348989421));
#69004=CARTESIAN_POINT('Ctrl Pts',(185.231676812499,5.39466110985939,334.89647539517));
#69005=CARTESIAN_POINT('Ctrl Pts',(185.231676812499,5.38121472107825,335.052595876397));
#69006=CARTESIAN_POINT('Ctrl Pts',(185.231676812499,5.36057609261863,335.208219833612));
#69007=CARTESIAN_POINT('Ctrl Pts',(185.231676812499,5.3582462039911,335.225788175849));
#69008=CARTESIAN_POINT('Ctrl Pts',(185.231676812499,5.35582407669609,335.24335377265));
#69009=CARTESIAN_POINT('Ctrl Pts',(185.231676812499,5.35331226641627,335.260899704573));
#69010=CARTESIAN_POINT('Ctrl Pts',(185.231676812499,5.3317196398837,335.411732256789));
#69011=CARTESIAN_POINT('Ctrl Pts',(185.231676812499,5.30346550590915,335.561410147836));
#69012=CARTESIAN_POINT('Ctrl Pts',(185.231676812499,5.26880078272557,335.709514464873));
#69013=CARTESIAN_POINT('Ctrl Pts',(185.231676812499,5.24423048589748,335.814490552864));
#69014=CARTESIAN_POINT('Ctrl Pts',(185.231676812499,5.21643836800517,335.918675990125));
#69015=CARTESIAN_POINT('Ctrl Pts',(185.231676812499,5.18549872286584,336.021916809428));
#69016=CARTESIAN_POINT('Ctrl Pts',(185.231676812499,5.18549872251113,336.021916810612));
#69017=CARTESIAN_POINT('Ctrl Pts',(185.231676812499,5.05958569114637,336.442069157206));
#69018=CARTESIAN_POINT('Ctrl Pts',(185.231676812498,4.88129210995362,336.847360621326));
#69019=CARTESIAN_POINT('Ctrl Pts',(185.231676812498,4.4356744775517,337.590470320891));
#69020=CARTESIAN_POINT('Ctrl Pts',(185.231676812498,4.17082293995955,337.929261543294));
#69021=CARTESIAN_POINT('Ctrl Pts',(185.231676812498,3.56527418889084,338.529985313398));
#69022=CARTESIAN_POINT('Ctrl Pts',(185.231676812499,3.22591379223974,338.791088436061));
#69023=CARTESIAN_POINT('Ctrl Pts',(185.231676812499,2.8570646345848,339.00329423554));
#69024=CARTESIAN_POINT('Ctrl Pts',(185.231676812499,-2.86416480220691,339.00656505702));
#69025=CARTESIAN_POINT('Ctrl Pts',(185.231676812499,-2.96718909511977,338.948123090184));
#69026=CARTESIAN_POINT('Ctrl Pts',(185.231676812499,-3.06770027579107,338.885880925931));
#69027=CARTESIAN_POINT('Ctrl Pts',(185.231676812499,-3.16545727640773,338.819900221475));
#69028=CARTESIAN_POINT('Ctrl Pts',(185.231676812499,-3.28283399218438,338.740677267162));
#69029=CARTESIAN_POINT('Ctrl Pts',(185.231676812499,-3.39624147032995,338.656066420927));
#69030=CARTESIAN_POINT('Ctrl Pts',(185.231676812499,-3.5055969172483,338.566518159339));
#69031=CARTESIAN_POINT('Ctrl Pts',(185.231676812499,-3.61495236416665,338.476969897751));
#69032=CARTESIAN_POINT('Ctrl Pts',(185.231676812499,-3.7202561302643,338.38248371036));
#69033=CARTESIAN_POINT('Ctrl Pts',(185.231676812499,-3.82140495863234,338.283461318034));
#69034=CARTESIAN_POINT('Ctrl Pts',(185.231676812499,-3.86855595085661,338.237301573764));
#69035=CARTESIAN_POINT('Ctrl Pts',(185.231676812499,-3.91480375207395,338.190155468001));
#69036=CARTESIAN_POINT('Ctrl Pts',(185.231676812499,-3.96013605261152,338.142060552508));
#69037=CARTESIAN_POINT('Origin',(185.231676812499,5.77350269189626,335.));
#69038=CARTESIAN_POINT('',(205.231676812499,2.88675134594813,340.));
#69039=CARTESIAN_POINT('',(185.231676812499,2.88675134594813,340.));
#69040=CARTESIAN_POINT('',(205.231676812499,5.77350269189626,335.));
#69041=CARTESIAN_POINT('Origin',(185.231676812499,-2.88675134594811,340.));
#69042=CARTESIAN_POINT('',(205.231676812499,-2.88675134594811,340.));
#69043=CARTESIAN_POINT('',(205.231676812499,-2.88675134594811,340.));
#69044=CARTESIAN_POINT('',(185.231676812499,-2.88675134594811,340.));
#69045=CARTESIAN_POINT('Origin',(185.231676812499,2.88675134594813,340.));
#69046=CARTESIAN_POINT('',(205.231676812499,2.88675134594813,340.));
#69047=CARTESIAN_POINT('Origin',(205.231676812499,4.44089209850063E-15,
335.));
#69048=CARTESIAN_POINT('Ctrl Pts',(185.811080378289,-2.14557563496124,330.580037935284));
#69049=CARTESIAN_POINT('Ctrl Pts',(185.764705644279,-2.88151516997222,330.937283427965));
#69050=CARTESIAN_POINT('Ctrl Pts',(185.671957904555,-4.15942683785613,332.026471253785));
#69051=CARTESIAN_POINT('Ctrl Pts',(185.486464153408,-5.4171251388755,335.17484951642));
#69052=CARTESIAN_POINT('Ctrl Pts',(185.254599124846,-3.7104720235285,339.469931545235));
#69053=CARTESIAN_POINT('Ctrl Pts',(184.976361090572,1.75984649753305,340.540119552943));
#69054=CARTESIAN_POINT('Ctrl Pts',(184.698123056299,5.60655848723213,336.517695725471));
#69055=CARTESIAN_POINT('Ctrl Pts',(184.419885022024,4.31271335213631,331.106893305836));
#69056=CARTESIAN_POINT('Ctrl Pts',(184.141646987751,-0.941219558116164,
329.266428853344));
#69057=CARTESIAN_POINT('Ctrl Pts',(183.863408953476,-5.33015269272146,332.688798752324));
#69058=CARTESIAN_POINT('Ctrl Pts',(183.585170919203,-4.82834868771287,338.231477647666));
#69059=CARTESIAN_POINT('Ctrl Pts',(183.306932884928,0.104711979366552,340.809019443882));
#69060=CARTESIAN_POINT('Ctrl Pts',(183.028694850655,4.94149341094068,338.055528588394));
#69061=CARTESIAN_POINT('Ctrl Pts',(182.750456816381,5.24363809821535,332.498120236651));
#69062=CARTESIAN_POINT('Ctrl Pts',(182.472218782107,0.733721161916883,329.236599179529));
#69063=CARTESIAN_POINT('Ctrl Pts',(182.193980747833,-4.44949313718591,331.264092910913));
#69064=CARTESIAN_POINT('Ctrl Pts',(181.915742713559,-5.54948793815025,336.719959177412));
#69065=CARTESIAN_POINT('Ctrl Pts',(181.637504679285,-1.556791794289,340.59745184479));
#69066=CARTESIAN_POINT('Ctrl Pts',(181.359266645011,3.86454508368571,339.338241573188));
#69067=CARTESIAN_POINT('Ctrl Pts',(181.081028610737,5.73944815949048,334.097893160242));
#69068=CARTESIAN_POINT('Ctrl Pts',(180.802790576463,2.34734321862604,329.685393757349));
#69069=CARTESIAN_POINT('Ctrl Pts',(180.524552542189,-3.19888333564474,330.150030653944));
#69070=CARTESIAN_POINT('Ctrl Pts',(180.246314507915,-5.80954219213952,335.065412519364));
#69071=CARTESIAN_POINT('Ctrl Pts',(179.968076473641,-3.08886975606896,339.920766447875));
#69072=CARTESIAN_POINT('Ctrl Pts',(179.689838439367,2.46641277265436,340.260405549321));
#69073=CARTESIAN_POINT('Ctrl Pts',(179.411600405093,5.75830475221954,335.772648168347));
#69074=CARTESIAN_POINT('Ctrl Pts',(179.13336237082,3.76588542763037,330.575842942801));
#69075=CARTESIAN_POINT('Ctrl Pts',(178.855124336545,-1.68243135602239,329.439021361301));
#69076=CARTESIAN_POINT('Ctrl Pts',(178.576886302272,-5.58680572404651,333.405427789685));
#69077=CARTESIAN_POINT('Ctrl Pts',(178.298648267998,-4.36425093644542,338.835149603303));
#69078=CARTESIAN_POINT('Ctrl Pts',(178.020410233724,0.863312517288815,340.745411230739));
#69079=CARTESIAN_POINT('Ctrl Pts',(177.74217219945,5.2986268174406,337.383193774887));
#69080=CARTESIAN_POINT('Ctrl Pts',(177.463934165176,4.87146949426853,331.833954567158));
#69081=CARTESIAN_POINT('Ctrl Pts',(177.185696130902,-0.0261634807241003,
329.190148522684));
#69082=CARTESIAN_POINT('Ctrl Pts',(176.907458096628,-4.89978661578628,331.877957425521));
#69083=CARTESIAN_POINT('Ctrl Pts',(176.629220062354,-5.27694789418978,337.430818717767));
#69084=CARTESIAN_POINT('Ctrl Pts',(176.35098202808,-0.811531977762798,340.752953551501));
#69085=CARTESIAN_POINT('Ctrl Pts',(176.072743993806,4.39861485648817,338.795687824499));
#69086=CARTESIAN_POINT('Ctrl Pts',(175.794505959532,5.57221776037641,333.355175405204));
#69087=CARTESIAN_POINT('Ctrl Pts',(175.516267925258,1.63227867137313,329.424094238988));
#69088=CARTESIAN_POINT('Ctrl Pts',(175.238029890984,-3.80557846195905,330.609939489414));
#69089=CARTESIAN_POINT('Ctrl Pts',(174.95979185671,-5.7511124109956,335.824478473221));
#69090=CARTESIAN_POINT('Ctrl Pts',(174.681553822436,-2.41893538674252,340.282405731434));
#69091=CARTESIAN_POINT('Ctrl Pts',(174.403315788163,3.1330629384969,339.892747218091));
#69092=CARTESIAN_POINT('Ctrl Pts',(174.125077753888,5.80989564901061,335.013086799536));
#69093=CARTESIAN_POINT('Ctrl Pts',(173.846839719615,3.15507287634666,330.121416818209));
#69094=CARTESIAN_POINT('Ctrl Pts',(173.56860168534,-2.39511370614138,329.706750615041));
#69095=CARTESIAN_POINT('Ctrl Pts',(173.290363651067,-5.74733979232378,334.149621244218));
#69096=CARTESIAN_POINT('Ctrl Pts',(173.012125616793,-3.82531698168697,339.372871906006));
#69097=CARTESIAN_POINT('Ctrl Pts',(172.733887582519,1.60714276145788,340.583202563136));
#69098=CARTESIAN_POINT('Ctrl Pts',(172.455649548245,5.56475131380112,336.669910636011));
#69099=CARTESIAN_POINT('Ctrl Pts',(172.177411513971,4.41566972106383,331.22416636606));
#69100=CARTESIAN_POINT('Ctrl Pts',(171.899173479697,-0.78560679951547,329.243448890762));
#69101=CARTESIAN_POINT('Ctrl Pts',(171.620935445424,-5.26594355571678,332.545433401856));
#69102=CARTESIAN_POINT('Ctrl Pts',(171.342697411149,-4.91380163603628,338.099937450725));
#69103=CARTESIAN_POINT('Ctrl Pts',(171.064459376875,-0.0523364825585829,
340.809674656063));
#69104=CARTESIAN_POINT('Ctrl Pts',(170.786221342601,4.85715708847794,338.187959180191));
#69105=CARTESIAN_POINT('Ctrl Pts',(170.507983308327,5.30930929093936,332.640700618857));
#69106=CARTESIAN_POINT('Ctrl Pts',(170.229745274054,0.88918672238244,329.258536276397));
#69107=CARTESIAN_POINT('Ctrl Pts',(169.951507239779,-4.34692937693034,331.145228449221));
#69108=CARTESIAN_POINT('Ctrl Pts',(169.673269205506,-5.59393254760659,336.569387577861));
#69109=CARTESIAN_POINT('Ctrl Pts',(169.395031171231,-1.70746638565333,340.553342890419));
#69110=CARTESIAN_POINT('Ctrl Pts',(169.116793136958,3.74591647625145,339.441077399649));
#69111=CARTESIAN_POINT('Ctrl Pts',(168.838555102684,5.76172707753682,334.253300729414));
#69112=CARTESIAN_POINT('Ctrl Pts',(168.56031706841,2.49008578271897,329.750758958534));
#69113=CARTESIAN_POINT('Ctrl Pts',(168.282079034136,-3.06667048129415,330.065368212736));
#69114=CARTESIAN_POINT('Ctrl Pts',(168.003840999862,-5.80918850860578,334.908416223065));
#69115=CARTESIAN_POINT('Ctrl Pts',(167.725602965588,-3.22069998505172,339.835509313713));
#69116=CARTESIAN_POINT('Ctrl Pts',(167.447364931314,2.32337737733045,340.325126879166));
#69117=CARTESIAN_POINT('Ctrl Pts',(167.16912689704,5.73532561353033,335.927954106353));
#69118=CARTESIAN_POINT('Ctrl Pts',(166.890888862766,3.88405018746073,330.67921154672));
#69119=CARTESIAN_POINT('Ctrl Pts',(166.612650828492,-1.5315607671548,329.395592775929));
#69120=CARTESIAN_POINT('Ctrl Pts',(166.334412794218,-5.54168101155223,333.255055793753));
#69121=CARTESIAN_POINT('Ctrl Pts',(166.056174759944,-4.46628238672583,338.715828354316));
#69122=CARTESIAN_POINT('Ctrl Pts',(165.77793672567,0.707757662178901,340.76664007966));
#69123=CARTESIAN_POINT('Ctrl Pts',(165.499698691397,5.23229895098799,337.525491319368));
#69124=CARTESIAN_POINT('Ctrl Pts',(165.221460657123,4.95523672108138,331.966736451483));
#69125=CARTESIAN_POINT('Ctrl Pts',(164.943222622848,0.130826891412531,329.191562771176));
#69126=CARTESIAN_POINT('Ctrl Pts',(164.664984588575,-4.81364084550388,331.746706203367));
#69127=CARTESIAN_POINT('Ctrl Pts',(164.3867465543,-5.34070142772378,337.287349334192));
#69128=CARTESIAN_POINT('Ctrl Pts',(164.108508520027,-0.96667913834544,340.728925742249));
#69129=CARTESIAN_POINT('Ctrl Pts',(163.830270485753,4.29445032813183,338.913151555451));
#69130=CARTESIAN_POINT('Ctrl Pts',(163.552032451479,5.61462611446546,333.506335944236));
#69131=CARTESIAN_POINT('Ctrl Pts',(163.273794417205,1.78234238729975,329.470233790553));
#69132=CARTESIAN_POINT('Ctrl Pts',(162.995556382931,-3.68557064136043,330.508716468062));
#69133=CARTESIAN_POINT('Ctrl Pts',(162.717318348657,-5.77128989137762,335.668783751595));
#69134=CARTESIAN_POINT('Ctrl Pts',(162.439080314383,-2.56078159217679,340.215118057522));
#69135=CARTESIAN_POINT('Ctrl Pts',(162.160842280109,2.99971817709032,339.975615497076));
#69136=CARTESIAN_POINT('Ctrl Pts',(161.882604245835,5.80742085100939,335.17006403493));
#69137=CARTESIAN_POINT('Ctrl Pts',(161.604366211561,3.28573912734839,330.208447318068));
#69138=CARTESIAN_POINT('Ctrl Pts',(161.326128177287,-2.2512168960502,329.643967774215));
#69139=CARTESIAN_POINT('Ctrl Pts',(161.047890143014,-5.72226440185046,333.994639949058));
#69140=CARTESIAN_POINT('Ctrl Pts',(160.769652108739,-3.94207432655665,339.267916203561));
#69141=CARTESIAN_POINT('Ctrl Pts',(160.491414074466,1.45569917329649,340.624588752396));
#69142=CARTESIAN_POINT('Ctrl Pts',(160.213176040192,5.51759902790003,336.819659221952));
#69143=CARTESIAN_POINT('Ctrl Pts',(159.934938005918,4.51607969422787,331.344855281648));
#69144=CARTESIAN_POINT('Ctrl Pts',(159.656699971644,-0.629779317610128,
329.224323699529));
#69145=CARTESIAN_POINT('Ctrl Pts',(159.37846193737,-5.19769914520483,332.404045009509));
#69146=CARTESIAN_POINT('Ctrl Pts',(159.100223903096,-4.99576718515871,337.966035898031));
#69147=CARTESIAN_POINT('Ctrl Pts',(158.821985868822,-0.209293416695222,
340.806139421548));
#69148=CARTESIAN_POINT('Ctrl Pts',(158.543747834548,4.7692458311037,338.318034496387));
#69149=CARTESIAN_POINT('Ctrl Pts',(158.265509800274,5.37111857365183,332.785018288002));
#69150=CARTESIAN_POINT('Ctrl Pts',(157.987271766,1.04399507873988,329.284658103641));
#69151=CARTESIAN_POINT('Ctrl Pts',(157.709033731726,-4.24118729058956,331.02918281926));
#69152=CARTESIAN_POINT('Ctrl Pts',(157.430795697452,-5.63429468316675,336.417667852479));
#69153=CARTESIAN_POINT('Ctrl Pts',(157.152557663178,-1.85689300705504,340.505180022221));
#69154=CARTESIAN_POINT('Ctrl Pts',(156.874319628904,3.62455197393519,339.540669741894));
#69155=CARTESIAN_POINT('Ctrl Pts',(156.596081594631,5.77979910674458,334.409253859607));
#69156=CARTESIAN_POINT('Ctrl Pts',(156.317843560356,2.63100990898947,329.819956990959));
#69157=CARTESIAN_POINT('Ctrl Pts',(156.039605526083,-2.9322182486027,329.984309134399));
#69158=CARTESIAN_POINT('Ctrl Pts',(155.761367491809,-5.80459299892257,334.751486753724));
#69159=CARTESIAN_POINT('Ctrl Pts',(155.483129457535,-3.35017842978342,339.746721311109));
#69160=CARTESIAN_POINT('Ctrl Pts',(155.204891423261,2.1786454358154,340.385959782779));
#69161=CARTESIAN_POINT('Ctrl Pts',(154.926653388987,5.70815854172035,336.08258245843));
#69162=CARTESIAN_POINT('Ctrl Pts',(154.648415354713,3.9993788061705,330.78573519087));
#69163=CARTESIAN_POINT('Ctrl Pts',(154.370177320439,-1.37957182906757,329.356256536203));
#69164=CARTESIAN_POINT('Ctrl Pts',(154.091939286165,-5.49250975921714,333.105957956745));
#69165=CARTESIAN_POINT('Ctrl Pts',(153.813701251891,-4.56505255264437,338.593793804367));
#69166=CARTESIAN_POINT('Ctrl Pts',(153.535463217617,0.551686001424929,340.783658122032));
#69167=CARTESIAN_POINT('Ctrl Pts',(153.257225183343,5.1621504548586,337.665944747762));
#69168=CARTESIAN_POINT('Ctrl Pts',(152.978987149069,5.03538562908436,332.101733227751));
#69169=CARTESIAN_POINT('Ctrl Pts',(152.700749114795,0.287721733669453,329.197218346285));
#69170=CARTESIAN_POINT('Ctrl Pts',(152.422511080521,-4.72398014996808,331.617830539517));
#69171=CARTESIAN_POINT('Ctrl Pts',(152.144273046247,-5.40055517581262,337.142209725895));
#69172=CARTESIAN_POINT('Ctrl Pts',(151.866035011973,-1.12112042887766,340.700714665783));
#69173=CARTESIAN_POINT('Ctrl Pts',(151.5877969777,4.18714998792789,339.027757899293));
#69174=CARTESIAN_POINT('Ctrl Pts',(151.309558943426,5.65293466304457,333.65858715823));
#69175=CARTESIAN_POINT('Ctrl Pts',(151.031320909152,1.93110463506422,329.52041118284));
#69176=CARTESIAN_POINT('Ctrl Pts',(150.753082874878,-3.56287161345692,330.410772986358));
#69177=CARTESIAN_POINT('Ctrl Pts',(150.474844840604,-5.78725317020745,335.512600683417));
#69178=CARTESIAN_POINT('Ctrl Pts',(150.19660680633,-2.70075791237538,340.144022299277));
#69179=CARTESIAN_POINT('Ctrl Pts',(149.918368772056,2.86418301852214,340.054850576735));
#69180=CARTESIAN_POINT('Ctrl Pts',(149.640130737782,5.80070546859394,335.326917089396));
#69181=CARTESIAN_POINT('Ctrl Pts',(149.361892703508,3.41400612840946,330.298976614406));
#69182=CARTESIAN_POINT('Ctrl Pts',(149.083654669234,-2.10567624516853,329.585095913385));
#69183=CARTESIAN_POINT('Ctrl Pts',(148.80541663496,-5.69301060828579,333.840392768796));
#69184=CARTESIAN_POINT('Ctrl Pts',(148.527178600686,-4.05595316487803,339.159844064509));
#69185=CARTESIAN_POINT('Ctrl Pts',(148.248940566412,1.30319263216773,340.661867861419));
#69186=CARTESIAN_POINT('Ctrl Pts',(147.970702532138,5.46641778576486,336.968079090938));
#69187=CARTESIAN_POINT('Ctrl Pts',(147.692464497864,4.61319202155985,331.468213187502));
#69188=CARTESIAN_POINT('Ctrl Pts',(147.414226463591,-0.473491970228016,
329.209415912808));
#69189=CARTESIAN_POINT('Ctrl Pts',(147.135988429316,-5.12565936966766,332.264552186048));
#69190=CARTESIAN_POINT('Ctrl Pts',(146.857750395043,-5.07408482017158,337.829968543009));
#69191=CARTESIAN_POINT('Ctrl Pts',(146.579512360768,-0.366097524573219,
340.798364538318));
#69192=CARTESIAN_POINT('Ctrl Pts',(146.301274326495,4.67785206573538,338.445686980533));
#69193=CARTESIAN_POINT('Ctrl Pts',(146.023036292221,5.42900586030193,332.930953338969));
#69194=CARTESIAN_POINT('Ctrl Pts',(145.744798257947,1.19804110886455,329.314953279156));
#69195=CARTESIAN_POINT('Ctrl Pts',(145.466560223673,-4.13234828512005,330.916036683908));
#69196=CARTESIAN_POINT('Ctrl Pts',(145.188322189399,-5.67054265121069,336.26491294464));
#69197=CARTESIAN_POINT('Ctrl Pts',(144.910084155125,-2.00496372335765,340.452997266158));
#69198=CARTESIAN_POINT('Ctrl Pts',(144.631846120851,3.50054082020459,339.636946482633));
#69199=CARTESIAN_POINT('Ctrl Pts',(144.353608086577,5.79365072096298,334.565638353212));
#69200=CARTESIAN_POINT('Ctrl Pts',(144.075370052303,2.77001286923813,329.892937495882));
#69201=CARTESIAN_POINT('Ctrl Pts',(143.797132018029,-2.79562490726363,329.906912518462));
#69202=CARTESIAN_POINT('Ctrl Pts',(143.518893983755,-5.79575896972554,334.594738749002));
#69203=CARTESIAN_POINT('Ctrl Pts',(143.240655949481,-3.4772105709325,339.654467247936));
#69204=CARTESIAN_POINT('Ctrl Pts',(142.962417915208,2.03232264526139,340.442859853265));
#69205=CARTESIAN_POINT('Ctrl Pts',(142.684179880933,5.67682336693198,336.236420307731));
#69206=CARTESIAN_POINT('Ctrl Pts',(142.40594184666,4.11178707454463,330.895336095327));
#69207=CARTESIAN_POINT('Ctrl Pts',(142.127703812386,-1.22657552627459,329.321041363502));
#69208=CARTESIAN_POINT('Ctrl Pts',(141.849465778112,-5.43932787085671,332.958243151098));
#69209=CARTESIAN_POINT('Ctrl Pts',(141.571227743838,-4.6604893127014,338.46913506265));
#69210=CARTESIAN_POINT('Ctrl Pts',(141.292989709564,0.395211499010483,340.796452931557));
#69211=CARTESIAN_POINT('Ctrl Pts',(141.01475167529,5.08823255139261,337.80445150068));
#69212=CARTESIAN_POINT('Ctrl Pts',(140.736513641016,5.11185769355109,332.238846321264));
#69213=CARTESIAN_POINT('Ctrl Pts',(140.458275606742,0.444406481233616,329.207111118263));
#69214=CARTESIAN_POINT('Ctrl Pts',(140.180037572468,-4.63086999948305,331.491424539133));
#69215=CARTESIAN_POINT('Ctrl Pts',(139.901799538194,-5.45646543320326,336.995505873951));
#69216=CARTESIAN_POINT('Ctrl Pts',(139.62356150392,-1.27474307617062,340.668340921863));
#69217=CARTESIAN_POINT('Ctrl Pts',(139.345323469646,4.07679218668677,339.139423170357));
#69218=CARTESIAN_POINT('Ctrl Pts',(139.067085435372,5.68711543317582,333.811817873199));
#69219=CARTESIAN_POINT('Ctrl Pts',(138.788847401098,2.0784567883257,329.574589776268));
#69220=CARTESIAN_POINT('Ctrl Pts',(138.510609366824,-3.43757097319903,330.316180562732));
#69221=CARTESIAN_POINT('Ctrl Pts',(138.232371332551,-5.79899059108342,335.356043313715));
#69222=CARTESIAN_POINT('Ctrl Pts',(137.954133298277,-2.83876213649137,340.069170370893));
#69223=CARTESIAN_POINT('Ctrl Pts',(137.675895264003,2.72655643069835,340.130394599535));
#69224=CARTESIAN_POINT('Ctrl Pts',(137.397657229729,5.78975440534314,335.483531428683));
#69225=CARTESIAN_POINT('Ctrl Pts',(137.119419195455,3.53978021883948,330.392938602642));
#69226=CARTESIAN_POINT('Ctrl Pts',(136.841181161181,-1.95859802742279,329.530178020841));
#69227=CARTESIAN_POINT('Ctrl Pts',(136.562943126907,-5.65959977277867,333.686992334875));
#69228=CARTESIAN_POINT('Ctrl Pts',(136.284705092633,-4.16687034221126,339.048734403232));
#69229=CARTESIAN_POINT('Ctrl Pts',(136.006467058359,1.14973449849797,340.695012668966));
#69230=CARTESIAN_POINT('Ctrl Pts',(135.728229024085,5.41124495998901,337.115061866638));
#69231=CARTESIAN_POINT('Ctrl Pts',(135.449990989811,4.70693579154281,331.594150007559));
#69232=CARTESIAN_POINT('Ctrl Pts',(135.171752955537,-0.316858878543813,
329.198736416279));
#69233=CARTESIAN_POINT('Ctrl Pts',(134.893514921263,-5.04987683262017,332.12705678927));
#69234=CARTESIAN_POINT('Ctrl Pts',(134.615276886989,-5.14869735346086,337.691834742175));
#69235=CARTESIAN_POINT('Ctrl Pts',(134.337038852715,-0.522634307678893,
340.786355683602));
#69236=CARTESIAN_POINT('Ctrl Pts',(134.058800818442,4.58304252819027,338.570823420658));
#69237=CARTESIAN_POINT('Ctrl Pts',(133.780562784167,5.48292888153603,333.078399209843));
#69238=CARTESIAN_POINT('Ctrl Pts',(133.502324749894,1.35121232819393,329.349399681374));
#69239=CARTESIAN_POINT('Ctrl Pts',(133.22408671562,-4.02049183487047,330.805872662585));
#69240=CARTESIAN_POINT('Ctrl Pts',(132.945848681346,-5.70264998343651,336.111234396122));
#69241=CARTESIAN_POINT('Ctrl Pts',(132.667610647072,-2.15157041317865,340.396832726132));
#69242=CARTESIAN_POINT('Ctrl Pts',(132.389372612798,3.37397356812602,339.72983732049));
#69243=CARTESIAN_POINT('Ctrl Pts',(132.111134578524,5.80327180572966,334.722340018119));
#69244=CARTESIAN_POINT('Ctrl Pts',(131.83289654425,2.90699316336665,329.969647182866));
#69245=CARTESIAN_POINT('Ctrl Pts',(131.554658509976,-2.65699019786919,329.83323488001));
#69246=CARTESIAN_POINT('Ctrl Pts',(131.276420475702,-5.7826928716315,334.438286666443));
#69247=CARTESIAN_POINT('Ctrl Pts',(130.998182441428,-3.60170364950447,339.558814488204));
#69248=CARTESIAN_POINT('Ctrl Pts',(130.719944407154,1.8845158507141,340.495785542134));
#69249=CARTESIAN_POINT('Ctrl Pts',(130.44170637288,5.64134297014069,336.389355321708));
#69250=CARTESIAN_POINT('Ctrl Pts',(130.163468338606,4.22119291195493,331.007934229403));
#69251=CARTESIAN_POINT('Ctrl Pts',(129.885230304332,-1.07268357682663,329.289972971979));
#69252=CARTESIAN_POINT('Ctrl Pts',(129.606992270059,-5.38217417993802,332.812019238311));
#69253=CARTESIAN_POINT('Ctrl Pts',(129.328754235784,-4.75252297888098,338.341943155101));
#69254=CARTESIAN_POINT('Ctrl Pts',(129.050516201511,0.23844841277096,340.805015165454));
#69255=CARTESIAN_POINT('Ctrl Pts',(128.772278167236,5.0105992155158,337.940910440355));
#69256=CARTESIAN_POINT('Ctrl Pts',(128.494040132963,5.18459707450497,332.377975611908));
#69257=CARTESIAN_POINT('Ctrl Pts',(128.215802098689,0.600766722748434,329.221233863396));
#69258=CARTESIAN_POINT('Ctrl Pts',(127.937564064415,-4.53437838317207,331.367580503998));
#69259=CARTESIAN_POINT('Ctrl Pts',(127.659326030141,-5.50839137417084,336.847344901656));
#69260=CARTESIAN_POINT('Ctrl Pts',(127.381087995867,-1.42743490481644,340.631828149831));
#69261=CARTESIAN_POINT('Ctrl Pts',(127.102849961593,3.96345750778334,339.248065830553));
#69262=CARTESIAN_POINT('Ctrl Pts',(126.824611927319,5.71714346602729,333.965916199926));
#69263=CARTESIAN_POINT('Ctrl Pts',(126.546373893045,2.22429125039721,329.632730009574));
#69264=CARTESIAN_POINT('Ctrl Pts',(126.268135858771,-3.30976021523733,330.225008268662));
#69265=CARTESIAN_POINT('Ctrl Pts',(125.989897824497,-5.80649358332928,335.199225960836));
#69266=CARTESIAN_POINT('Ctrl Pts',(125.711659790223,-2.97469349370475,339.990616929322));
#69267=CARTESIAN_POINT('Ctrl Pts',(125.433421755949,2.58693890868864,340.202192403153));
#69268=CARTESIAN_POINT('Ctrl Pts',(125.155183721675,5.77457565773415,335.639792692846));
#69269=CARTESIAN_POINT('Ctrl Pts',(124.876945687402,3.66296955827404,330.490264671638));
#69270=CARTESIAN_POINT('Ctrl Pts',(124.598707653127,-1.81008963947211,329.479254197684));
#69271=CARTESIAN_POINT('Ctrl Pts',(124.320469618854,-5.62205629195399,333.53455066044));
#69272=CARTESIAN_POINT('Ctrl Pts',(124.04223158458,-4.27474486672454,338.934668352114));
#69273=CARTESIAN_POINT('Ctrl Pts',(123.763993550306,0.995436827567214,340.723998972662));
#69274=CARTESIAN_POINT('Ctrl Pts',(123.485755516032,5.35212083782403,337.260500222085));
#69275=CARTESIAN_POINT('Ctrl Pts',(123.207517481758,4.79724255238381,331.722573782628));
#69276=CARTESIAN_POINT('Ctrl Pts',(122.929279447484,-0.159994416194986,
329.192293008123));
#69277=CARTESIAN_POINT('Ctrl Pts',(122.65104141321,-4.9704068705453,331.991659218448));
#69278=CARTESIAN_POINT('Ctrl Pts',(122.372803378936,-5.21955030288149,337.551735360966));
#69279=CARTESIAN_POINT('Ctrl Pts',(122.094565344662,-0.678789462699493,
340.770121626278));
#69280=CARTESIAN_POINT('Ctrl Pts',(121.816327310388,4.48488644848576,338.693352442011));
#69281=CARTESIAN_POINT('Ctrl Pts',(121.538089276114,5.53284826271111,333.227248235502));
#69282=CARTESIAN_POINT('Ctrl Pts',(121.25985124184,1.50339689095296,329.387972157501));
#69283=CARTESIAN_POINT('Ctrl Pts',(120.981613207566,-3.90569961753098,330.698771197166));
#69284=CARTESIAN_POINT('Ctrl Pts',(120.703375173292,-5.7305932350386,335.956744423159));
#69285=CARTESIAN_POINT('Ctrl Pts',(120.425137139018,-2.2966060241688,340.336727413544));
#69286=CARTESIAN_POINT('Ctrl Pts',(120.146899104744,3.24494263723136,339.819274426487));
#69287=CARTESIAN_POINT('Ctrl Pts',(119.868661070471,5.80865533571912,334.879244430617));
#69288=CARTESIAN_POINT('Ctrl Pts',(119.590423036197,3.04185076822965,330.050030038421));
#69289=CARTESIAN_POINT('Ctrl Pts',(119.312185001923,-2.51641535162041,329.763330018529));
#69290=CARTESIAN_POINT('Ctrl Pts',(119.033946967649,-5.76540424551814,334.28224474751));
#69291=CARTESIAN_POINT('Ctrl Pts',(118.755708933375,-3.72356676053103,339.459832877652));
#69292=CARTESIAN_POINT('Ctrl Pts',(118.477470899101,1.7353329808401,340.544698202998));
#69293=CARTESIAN_POINT('Ctrl Pts',(118.199232864827,5.60174325916709,336.541275827064));
#69294=CARTESIAN_POINT('Ctrl Pts',(117.920994830553,4.32751643015142,331.123447373827));
#69295=CARTESIAN_POINT('Ctrl Pts',(117.642756796279,-0.918008352776408,
329.263074047807));
#69296=CARTESIAN_POINT('Ctrl Pts',(117.364518762005,-5.32109042014236,332.667392991226));
#69297=CARTESIAN_POINT('Ctrl Pts',(117.086280727731,-4.84108634810961,338.212310957373));
#69298=CARTESIAN_POINT('Ctrl Pts',(116.808042693457,0.0815112112657543,
340.809338571572));
#69299=CARTESIAN_POINT('Ctrl Pts',(116.529804659183,4.92930713516613,338.075221924337));
#69300=CARTESIAN_POINT('Ctrl Pts',(116.251566624909,5.25355065757865,332.519019507338));
#69301=CARTESIAN_POINT('Ctrl Pts',(115.973328590636,0.756688283811837,329.239576269243));
#69302=CARTESIAN_POINT('Ctrl Pts',(115.695090556361,-4.43457575930834,331.246388865151));
#69303=CARTESIAN_POINT('Ctrl Pts',(115.416852522088,-5.55629508234218,336.697834996298));
#69304=CARTESIAN_POINT('Ctrl Pts',(115.138614487814,-1.57908441909158,340.591203011347));
#69305=CARTESIAN_POINT('Ctrl Pts',(114.86037645354,3.84722870831154,339.353606548904));
#69306=CARTESIAN_POINT('Ctrl Pts',(114.582138419266,5.74299683509981,334.120769615659));
#69307=CARTESIAN_POINT('Ctrl Pts',(114.303900384992,2.36850153281131,329.694789428705));
#69308=CARTESIAN_POINT('Ctrl Pts',(114.025662350718,-3.17953266711279,330.137322678249));
#69309=CARTESIAN_POINT('Ctrl Pts',(113.747424316444,-5.80975666825273,335.042263132965));
#69310=CARTESIAN_POINT('Ctrl Pts',(113.46918628217,-3.108452726805,339.908419334362));
#69311=CARTESIAN_POINT('Ctrl Pts',(113.190948247896,2.44543240134464,340.270191560766));
#69312=CARTESIAN_POINT('Ctrl Pts',(112.912710213622,5.75518030930339,335.795586779756));
#69313=CARTESIAN_POINT('Ctrl Pts',(112.634472179348,3.78348419373652,330.590883753805));
#69314=CARTESIAN_POINT('Ctrl Pts',(112.356234145074,-1.66025952228718,329.432361628538));
#69315=CARTESIAN_POINT('Ctrl Pts',(112.0779961108,-5.58040758009832,333.383179058555));
#69316=CARTESIAN_POINT('Ctrl Pts',(111.799758076526,-4.37949796833411,338.817729202297));
#69317=CARTESIAN_POINT('Ctrl Pts',(111.521520042252,0.840412287686272,340.748805606682));
#69318=CARTESIAN_POINT('Ctrl Pts',(111.243282007978,5.28908859176198,337.404287958046));
#69319=CARTESIAN_POINT('Ctrl Pts',(110.965043973705,4.88404636199737,331.853390737543));
#69320=CARTESIAN_POINT('Ctrl Pts',(110.686805939431,-0.00301312576609244,
329.19009039332));
#69321=CARTESIAN_POINT('Ctrl Pts',(110.408567905157,-4.88730751248768,331.858458341022));
#69322=CARTESIAN_POINT('Ctrl Pts',(110.130329870883,-5.28659193153996,337.409772700089));
#69323=CARTESIAN_POINT('Ctrl Pts',(109.852091836609,-0.834448964987024,
340.74967422047));
#69324=CARTESIAN_POINT('Ctrl Pts',(109.573853802335,4.38345550028797,338.81318457378));
#69325=CARTESIAN_POINT('Ctrl Pts',(109.295615768061,5.57872755264583,333.377391726243));
#69326=CARTESIAN_POINT('Ctrl Pts',(109.017377733787,1.65448367182431,329.430642541875));
#69327=CARTESIAN_POINT('Ctrl Pts',(108.739139699513,-3.78805545449141,330.594810493246));
#69328=CARTESIAN_POINT('Ctrl Pts',(108.460901665239,-5.75435200182722,335.801555834477));
#69329=CARTESIAN_POINT('Ctrl Pts',(108.182663630965,-2.43996465118251,340.272725217351));
#69330=CARTESIAN_POINT('Ctrl Pts',(107.904425596691,3.11354224603317,339.905192493561));
#69331=CARTESIAN_POINT('Ctrl Pts',(107.626187562417,5.80979737987243,335.036237018951));
#69332=CARTESIAN_POINT('Ctrl Pts',(107.347949528143,3.17448721067152,330.134027366908));
#69333=CARTESIAN_POINT('Ctrl Pts',(107.069711493869,-2.37400301640822,329.697248978614));
#69334=CARTESIAN_POINT('Ctrl Pts',(106.791473459595,-5.74390571555722,334.126726934171));
#69335=CARTESIAN_POINT('Ctrl Pts',(106.513235425322,-3.84271091944876,339.357594692747));
#69336=CARTESIAN_POINT('Ctrl Pts',(106.234997391047,1.58488296911764,340.589562119784));
#69337=CARTESIAN_POINT('Ctrl Pts',(105.956759356774,5.55805314975906,336.692070891295));
#69338=CARTESIAN_POINT('Ctrl Pts',(105.6785213225,4.43067999159659,331.241791180792));
#69339=CARTESIAN_POINT('Ctrl Pts',(105.400283288226,-0.762662798124573,
329.240364232604));
#69340=CARTESIAN_POINT('Ctrl Pts',(105.122045253952,-5.25612119489127,332.524470016072));
#69341=CARTESIAN_POINT('Ctrl Pts',(104.843807219678,-4.92611475132793,338.080333127028));
#69342=CARTESIAN_POINT('Ctrl Pts',(104.565569185404,-0.0754855098054712,
340.809419992954));
#69343=CARTESIAN_POINT('Ctrl Pts',(104.28733115113,4.84441566990115,338.207287878244));
#69344=CARTESIAN_POINT('Ctrl Pts',(104.009093116856,5.31866809279759,332.661875017163));
#69345=CARTESIAN_POINT('Ctrl Pts',(103.730855082582,0.912057310346108,329.262124942162));
#69346=CARTESIAN_POINT('Ctrl Pts',(103.452617048308,-4.33153500386603,331.127938116843));
#69347=CARTESIAN_POINT('Ctrl Pts',(103.174379014034,-5.6001415783824,336.547085330158));
#69348=CARTESIAN_POINT('Ctrl Pts',(102.89614097976,-1.72958088437146,340.546495170927));
#69349=CARTESIAN_POINT('Ctrl Pts',(102.617902945486,3.72819065865516,339.455968259473));
#69350=CARTESIAN_POINT('Ctrl Pts',(102.339664911213,5.76465666223787,334.276265046283));
#69351=CARTESIAN_POINT('Ctrl Pts',(102.061426876938,2.51098233307774,329.760722717809));
#69352=CARTESIAN_POINT('Ctrl Pts',(101.783188842665,-3.04698342110933,330.053187819595));
#69353=CARTESIAN_POINT('Ctrl Pts',(101.504950808391,-5.80877746314596,334.885269444511));
#69354=CARTESIAN_POINT('Ctrl Pts',(101.226712774117,-3.23994216466833,339.822637606779));
#69355=CARTESIAN_POINT('Ctrl Pts',(100.948474739843,2.30214023685744,340.33434241932));
#69356=CARTESIAN_POINT('Ctrl Pts',(100.670236705569,5.73158252255335,335.950799928416));
#69357=CARTESIAN_POINT('Ctrl Pts',(100.391998671295,3.90123612532141,330.694722376988));
#69358=CARTESIAN_POINT('Ctrl Pts',(100.113760637021,-1.50921708196717,329.389534554406));
#69359=CARTESIAN_POINT('Ctrl Pts',(99.8355226027465,-5.53468404914209,333.23298806091));
#69360=CARTESIAN_POINT('Ctrl Pts',(99.5572845684727,-4.48105315622197,338.698002342863));
#69361=CARTESIAN_POINT('Ctrl Pts',(99.2790465341986,0.684774077926888,340.769414457197));
#69362=CARTESIAN_POINT('Ctrl Pts',(99.0008084999249,5.22219424801106,337.546320080579));
#69363=CARTESIAN_POINT('Ctrl Pts',(98.7225704656507,4.96728383615623,331.986505349636));
#69364=CARTESIAN_POINT('Ctrl Pts',(98.444332431377,0.153970364850074,329.192130180225));
#69365=CARTESIAN_POINT('Ctrl Pts',(98.1660943971029,-4.80063943768013,331.727551420403));
#69366=CARTESIAN_POINT('Ctrl Pts',(97.8878563628291,-5.34977328557324,337.266050420816));
#69367=CARTESIAN_POINT('Ctrl Pts',(97.6096183285551,-0.989499151820034,
340.725028396896));
#69368=CARTESIAN_POINT('Ctrl Pts',(97.331380294281,4.27882374857487,338.930232314425));
#69369=CARTESIAN_POINT('Ctrl Pts',(97.0531422600072,5.62053325023763,333.528720047139));
#69370=CARTESIAN_POINT('Ctrl Pts',(96.7749042257333,1.80436234709209,329.477379676539));
#69371=CARTESIAN_POINT('Ctrl Pts',(96.4966661914593,-3.66764524963526,330.494066463036));
#69372=CARTESIAN_POINT('Ctrl Pts',(96.2184281571854,-5.77390893512749,335.645781948935));
#69373=CARTESIAN_POINT('Ctrl Pts',(95.9401901229113,-2.58154161360941,340.204872872023));
#69374=CARTESIAN_POINT('Ctrl Pts',(95.6619520886377,2.97986834322628,339.987528784253));
#69375=CARTESIAN_POINT('Ctrl Pts',(95.3837140543634,5.80669710426784,335.193203146979));
#69376=CARTESIAN_POINT('Ctrl Pts',(95.1054760200898,3.30480563943159,330.221577833395));
#69377=CARTESIAN_POINT('Ctrl Pts',(94.8272379858156,-2.22985718185977,329.63504001271));
#69378=CARTESIAN_POINT('Ctrl Pts',(94.5489999515418,-5.71821297999646,333.971846785681));
#69379=CARTESIAN_POINT('Ctrl Pts',(94.2707619172678,-3.95904912707566,339.252174587916));
#69380=CARTESIAN_POINT('Ctrl Pts',(93.9925238829939,1.43327567429316,340.630344532814));
#69381=CARTESIAN_POINT('Ctrl Pts',(93.71428584872,5.51030454447741,336.841630403699));
#69382=CARTESIAN_POINT('Ctrl Pts',(93.4360478144461,4.5306082661565,331.362879235528));
#69383=CARTESIAN_POINT('Ctrl Pts',(93.1578097801719,-0.606760346347846,
329.221860109099));
#69384=CARTESIAN_POINT('Ctrl Pts',(92.8795717458984,-5.1873139447767,332.383354675345));
#69385=CARTESIAN_POINT('Ctrl Pts',(92.601333711624,-5.00754610071247,337.946106034405));
#69386=CARTESIAN_POINT('Ctrl Pts',(92.3230956773503,-0.232427111283864,
340.805259370145));
#69387=CARTESIAN_POINT('Ctrl Pts',(92.0448576430763,4.75598680755151,338.33701186739));
#69388=CARTESIAN_POINT('Ctrl Pts',(91.7666196088024,5.37990183134708,332.806437828148));
#69389=CARTESIAN_POINT('Ctrl Pts',(91.4883815745285,1.06676035173629,329.288863417088));
#69390=CARTESIAN_POINT('Ctrl Pts',(91.2101435402544,-4.22533135730589,331.01231475193));
#69391=CARTESIAN_POINT('Ctrl Pts',(90.9319055059806,-5.63989884553708,336.395205980787));
#69392=CARTESIAN_POINT('Ctrl Pts',(90.6536674717066,-1.87881440798938,340.497737274284));
#69393=CARTESIAN_POINT('Ctrl Pts',(90.3754294374327,3.60643028051496,339.555076217639));
#69394=CARTESIAN_POINT('Ctrl Pts',(90.0971914031586,5.78210713141441,334.432288948882));
#69395=CARTESIAN_POINT('Ctrl Pts',(89.8189533688849,2.65162961157622,329.830481732335));
#69396=CARTESIAN_POINT('Ctrl Pts',(89.5407153346108,-2.91220926481656,329.972665128059));
#69397=CARTESIAN_POINT('Ctrl Pts',(89.262477300337,-5.80355668302547,334.728359532423));
#69398=CARTESIAN_POINT('Ctrl Pts',(88.984239266063,-3.36906579357812,339.733334384476));
#69399=CARTESIAN_POINT('Ctrl Pts',(88.7060012317891,2.15716704730625,340.394598135795));
#69400=CARTESIAN_POINT('Ctrl Pts',(88.4277631975151,5.70379952861112,336.105318802034));
#69401=CARTESIAN_POINT('Ctrl Pts',(88.1495251632412,4.01613937045259,330.801704718125));
#69402=CARTESIAN_POINT('Ctrl Pts',(87.8712871289672,-1.35707260985033,329.350804247655));
#69403=CARTESIAN_POINT('Ctrl Pts',(87.5930490946932,-5.48491908645251,333.084087337121));
#69404=CARTESIAN_POINT('Ctrl Pts',(87.3148110604194,-4.57933627469021,338.575575198485));
#69405=CARTESIAN_POINT('Ctrl Pts',(87.0365730261455,0.528635845462655,340.785810475604));
#69406=CARTESIAN_POINT('Ctrl Pts',(86.7583349918715,5.15148665288674,337.686492877684));
#69407=CARTESIAN_POINT('Ctrl Pts',(86.4800969575976,5.04689419477502,332.121820418482));
#69408=CARTESIAN_POINT('Ctrl Pts',(86.2018589233236,0.310841426154469,329.19841087938));
#69409=CARTESIAN_POINT('Ctrl Pts',(85.9236208890498,-4.71046593123611,331.599034044954));
#69410=CARTESIAN_POINT('Ctrl Pts',(85.6453828547757,-5.40904822989449,337.120673469299));
#69411=CARTESIAN_POINT('Ctrl Pts',(85.3671448205018,-1.1438268053997,340.696202151958));
#69412=CARTESIAN_POINT('Ctrl Pts',(85.0889067862279,4.17106759555441,339.04441019557));
#69413=CARTESIAN_POINT('Ctrl Pts',(84.8106687519538,5.65823482892504,333.681122698105));
#69414=CARTESIAN_POINT('Ctrl Pts',(84.53243071768,1.95292347520033,329.528149433992));
#69415=CARTESIAN_POINT('Ctrl Pts',(84.2541926834061,-3.54455692661247,330.396612669922));
#69416=CARTESIAN_POINT('Ctrl Pts',(83.9759546491321,-5.7892497544475,335.48953651278));
#69417=CARTESIAN_POINT('Ctrl Pts',(83.6977166148583,-2.72123353181235,340.133219923406));
#69418=CARTESIAN_POINT('Ctrl Pts',(83.419478580584,2.8440185376259,340.066223176525));
#69419=CARTESIAN_POINT('Ctrl Pts',(83.1412405463105,5.79935677272967,335.350028197878));
#69420=CARTESIAN_POINT('Ctrl Pts',(82.8630025120362,3.43271089586507,330.312617508446));
#69421=CARTESIAN_POINT('Ctrl Pts',(82.5847644777625,-2.08408310340512,329.576748545861));
#69422=CARTESIAN_POINT('Ctrl Pts',(82.3065264434884,-5.68834479969662,333.817717395679));
#69423=CARTESIAN_POINT('Ctrl Pts',(82.0282884092145,-4.07249643313815,339.14364954102));
#69424=CARTESIAN_POINT('Ctrl Pts',(81.7500503749407,1.28062180016229,340.667015662733));
#69425=CARTESIAN_POINT('Ctrl Pts',(81.4718123406666,5.45853230940055,336.989845155771));
#69426=CARTESIAN_POINT('Ctrl Pts',(81.1935743063928,4.627228286107,331.486623119424));
#69427=CARTESIAN_POINT('Ctrl Pts',(80.9153362721188,-0.450414837569424,
329.207575189023));
#69428=CARTESIAN_POINT('Ctrl Pts',(80.6370982378449,-5.11471891292048,332.244150011606));
#69429=CARTESIAN_POINT('Ctrl Pts',(80.358860203571,-5.08532093501182,337.809727692259));
#69430=CARTESIAN_POINT('Ctrl Pts',(80.080622169297,-0.389198994256777,340.796859741237));
#69431=CARTESIAN_POINT('Ctrl Pts',(79.802384135023,4.66408511895998,338.464299167193));
#69432=CARTESIAN_POINT('Ctrl Pts',(79.5241461007491,5.43720716029067,332.952602380386));
#69433=CARTESIAN_POINT('Ctrl Pts',(79.2459080664751,1.22068444366876,329.319772169561));
#69434=CARTESIAN_POINT('Ctrl Pts',(78.9676700322012,-4.11604236963513,330.899603198703));
#69435=CARTESIAN_POINT('Ctrl Pts',(78.6894319979273,-5.67553785301064,336.24230785064));
#69436=CARTESIAN_POINT('Ctrl Pts',(78.4111939636534,-2.02667601947968,340.444964924476));
#69437=CARTESIAN_POINT('Ctrl Pts',(78.1329559293794,3.48203648343876,339.650858054674));
#69438=CARTESIAN_POINT('Ctrl Pts',(77.8547178951055,5.79533550027971,334.588727394648));
#69439=CARTESIAN_POINT('Ctrl Pts',(77.5764798608315,2.79034066752573,329.904015534182));
#69440=CARTESIAN_POINT('Ctrl Pts',(77.2982418265576,-2.77530861045587,329.895813401389));
#69441=CARTESIAN_POINT('Ctrl Pts',(77.0200037922837,-5.79409814011006,334.571647972472));
#69442=CARTESIAN_POINT('Ctrl Pts',(76.7417657580097,-3.49572932733361,339.640574876751));
#69443=CARTESIAN_POINT('Ctrl Pts',(76.4635277237358,2.0106186922566,340.45091471141));
#69444=CARTESIAN_POINT('Ctrl Pts',(76.1852896894618,5.67185161464618,336.259030570777));
#69445=CARTESIAN_POINT('Ctrl Pts',(75.9070516551879,4.12811002666756,330.911752658603));
#69446=CARTESIAN_POINT('Ctrl Pts',(75.628813620914,-1.20393720197976,329.316198989197));
#69447=CARTESIAN_POINT('Ctrl Pts',(75.35057558664,-5.43114903045424,332.93658561464));
#69448=CARTESIAN_POINT('Ctrl Pts',(75.0723375523661,-4.67427555730914,338.450537165582));
#69449=CARTESIAN_POINT('Ctrl Pts',(74.7940995180922,0.372111602584409,340.797981689513));
#69450=CARTESIAN_POINT('Ctrl Pts',(74.5158614838182,5.07701743714451,337.82470399505));
#69451=CARTESIAN_POINT('Ctrl Pts',(74.2376234495443,5.12281930629161,332.25923713689));
#69452=CARTESIAN_POINT('Ctrl Pts',(73.9593854152703,0.467485510743936,329.208927904614));
#69453=CARTESIAN_POINT('Ctrl Pts',(73.6811473809965,-4.61685283793864,331.473000058189));
#69454=CARTESIAN_POINT('Ctrl Pts',(73.4029093467224,-5.46437348188109,336.973747999931));
#69455=CARTESIAN_POINT('Ctrl Pts',(73.1246713124486,-1.29731923552167,340.663216534608));
#69456=CARTESIAN_POINT('Ctrl Pts',(72.8464332781745,4.06026572487547,339.155634844415));
#69457=CARTESIAN_POINT('Ctrl Pts',(72.5681952439007,5.69180475897825,333.834488394571));
#69458=CARTESIAN_POINT('Ctrl Pts',(72.2899572096266,2.10005857666722,329.582914742107));
#69459=CARTESIAN_POINT('Ctrl Pts',(72.0117191753529,-3.41888036463754,330.302520274763));
#69460=CARTESIAN_POINT('Ctrl Pts',(71.7334811410787,-5.80036325790589,335.332933616582));
#69461=CARTESIAN_POINT('Ctrl Pts',(71.455243106805,-2.85893840261536,340.057818692555));
#69462=CARTESIAN_POINT('Ctrl Pts',(71.1770050725308,2.70609202689364,340.141218207653));
#69463=CARTESIAN_POINT('Ctrl Pts',(70.8987670382572,5.78778174517512,335.506597657843));
#69464=CARTESIAN_POINT('Ctrl Pts',(70.620529003983,3.55810958342815,330.407079914801));
#69465=CARTESIAN_POINT('Ctrl Pts',(70.3422909697092,-1.93678722541939,329.522417142556));
#69466=CARTESIAN_POINT('Ctrl Pts',(70.0640529354351,-5.65432298443225,333.664451309597));
#69467=CARTESIAN_POINT('Ctrl Pts',(69.7858149011614,-4.18296999830208,339.032098797155));
#69468=CARTESIAN_POINT('Ctrl Pts',(69.5075768668872,1.12703281473394,340.699548732244));
#69469=CARTESIAN_POINT('Ctrl Pts',(69.2293388326135,5.4027742486657,337.136606920955));
#69470=CARTESIAN_POINT('Ctrl Pts',(68.9511007983393,4.72046949941413,331.61293247457));
#69471=CARTESIAN_POINT('Ctrl Pts',(68.6728627640656,-0.293740435434174,
329.197519903239));
#69472=CARTESIAN_POINT('Ctrl Pts',(68.3946247297915,-5.03838910828626,332.106957672239));
#69473=CARTESIAN_POINT('Ctrl Pts',(68.1163866955177,-5.15938246296538,337.67129768419));
#69474=CARTESIAN_POINT('Ctrl Pts',(67.8381486612436,-0.545686683741498,
340.78422723965));
#69475=CARTESIAN_POINT('Ctrl Pts',(67.5599106269698,4.56877771082971,338.589056832337));
#69476=CARTESIAN_POINT('Ctrl Pts',(67.2816725926958,5.49054223522097,333.10026194438));
#69477=CARTESIAN_POINT('Ctrl Pts',(67.0034345584219,1.37371719062049,329.354828629979));
#69478=CARTESIAN_POINT('Ctrl Pts',(66.7251965241479,-4.00374784377992,330.789885759252));
#69479=CARTESIAN_POINT('Ctrl Pts',(66.446958489874,-5.7070325771648,336.088502586077));
#69480=CARTESIAN_POINT('Ctrl Pts',(66.1687204556001,-2.1730577501483,340.388216655929));
#69481=CARTESIAN_POINT('Ctrl Pts',(65.8904824213261,3.35510009989947,339.743243830584));
#69482=CARTESIAN_POINT('Ctrl Pts',(65.6122443870522,5.8043321094658,334.745466152075));
#69483=CARTESIAN_POINT('Ctrl Pts',(65.3340063527783,2.92701421397687,329.981270428894));
#69484=CARTESIAN_POINT('Ctrl Pts',(65.0557683185043,-2.63638142301966,329.822688756789));
#69485=CARTESIAN_POINT('Ctrl Pts',(64.7775302842304,-5.78040874103706,334.415249195591));
#69486=CARTESIAN_POINT('Ctrl Pts',(64.4992922499564,-3.61984027609792,339.54442681669));
#69487=CARTESIAN_POINT('Ctrl Pts',(64.2210542156825,1.86260218146139,340.503251023743));
#69488=CARTESIAN_POINT('Ctrl Pts',(63.9428161814086,5.63576210905672,336.411822994159));
#69489=CARTESIAN_POINT('Ctrl Pts',(63.6645781471346,4.23706633288306,331.024785841308));
#69490=CARTESIAN_POINT('Ctrl Pts',(63.3863401128608,-1.04992267798081,329.285744047825));
#69491=CARTESIAN_POINT('Ctrl Pts',(63.1081020785866,-5.37341314409502,332.790590599372));
#69492=CARTESIAN_POINT('Ctrl Pts',(62.8298640443129,-4.76580167932123,338.322979547047));
#69493=CARTESIAN_POINT('Ctrl Pts',(62.5516260100388,0.21531564344817,340.805919211494));
#69494=CARTESIAN_POINT('Ctrl Pts',(62.2733879757649,4.99884097827888,337.960852510781));
#69495=CARTESIAN_POINT('Ctrl Pts',(61.995149941491,5.19500373011495,332.398655163035));
#69496=CARTESIAN_POINT('Ctrl Pts',(61.716911907217,0.623788236953903,329.223673576385));
#69497=CARTESIAN_POINT('Ctrl Pts',(61.4386738729432,-4.51986851416046,331.349541490248));
#69498=CARTESIAN_POINT('Ctrl Pts',(61.1604358386692,-5.51570864297967,336.825381297832));
#69499=CARTESIAN_POINT('Ctrl Pts',(60.8821978043952,-1.44986436186256,340.626095630978));
#69500=CARTESIAN_POINT('Ctrl Pts',(60.6039597701214,3.94649904417292,339.263825044612));
#69501=CARTESIAN_POINT('Ctrl Pts',(60.3257217358473,5.72121852760133,333.988705148759));
#69502=CARTESIAN_POINT('Ctrl Pts',(60.0474837015735,2.2456602132971,329.641635611203));
#69503=CARTESIAN_POINT('Ctrl Pts',(59.7692456672994,-3.2907073328593,330.211857983917));
#69504=CARTESIAN_POINT('Ctrl Pts',(59.4910076330256,-5.80724133041153,335.17608761193));
#69505=CARTESIAN_POINT('Ctrl Pts',(59.2127695987516,-2.99455567378668,339.978724237523));
#69506=CARTESIAN_POINT('Ctrl Pts',(58.9345315644777,2.56618952510292,340.212459116192));
#69507=CARTESIAN_POINT('Ctrl Pts',(58.6562935302037,5.77198047370087,335.6627971997));
#69508=CARTESIAN_POINT('Ctrl Pts',(58.3780554959298,3.68091013587568,330.504896075916));
#69509=CARTESIAN_POINT('Ctrl Pts',(58.0998174616558,-1.78807710349808,329.472085475637));
#69510=CARTESIAN_POINT('Ctrl Pts',(57.821579427382,-5.61617237696643,333.512160442483));
#69511=CARTESIAN_POINT('Ctrl Pts',(57.543341393108,-4.2903891546611,338.917603810785));
#69512=CARTESIAN_POINT('Ctrl Pts',(57.265103358834,0.972620868836612,340.727919985669));
#69513=CARTESIAN_POINT('Ctrl Pts',(56.9868653245601,5.34307107686344,337.281808533663));
#69514=CARTESIAN_POINT('Ctrl Pts',(56.7086272902862,4.81026382125253,331.741715069755));
#69515=CARTESIAN_POINT('Ctrl Pts',(56.4303892560122,-0.136851543744224,
329.191701594125));
#69516=CARTESIAN_POINT('Ctrl Pts',(56.1521512217384,-4.95838026697236,331.971877835222));
#69517=CARTESIAN_POINT('Ctrl Pts',(55.8739131874643,-5.22967660477275,337.530917091927));
#69518=CARTESIAN_POINT('Ctrl Pts',(55.5956751531904,-0.701775912273333,
340.767371089645));
#69519=CARTESIAN_POINT('Ctrl Pts',(55.3174371189165,4.47013417672383,338.711193764654));
#69520=CARTESIAN_POINT('Ctrl Pts',(55.0391990846425,5.53986811081383,333.24930869897));
#69521=CARTESIAN_POINT('Ctrl Pts',(54.7609610503686,1.52574684792925,329.39400720008));
#69522=CARTESIAN_POINT('Ctrl Pts',(54.4827230160947,-3.88852977731343,330.683242549359));
#69523=CARTESIAN_POINT('Ctrl Pts',(54.2044849818207,-5.73436002052102,335.933902495856));
#69524=CARTESIAN_POINT('Ctrl Pts',(53.9262469475468,-2.31785271191163,340.327533906283));
#69525=CARTESIAN_POINT('Ctrl Pts',(53.6480089132729,3.22571381896912,339.832166085187));
#69526=CARTESIAN_POINT('Ctrl Pts',(53.3697708789989,5.80909038963983,334.902390770369));
#69527=CARTESIAN_POINT('Ctrl Pts',(53.0915328447249,3.06155045177167,330.062190004873));
#69528=CARTESIAN_POINT('Ctrl Pts',(52.8132948104511,-2.49552914727676,329.753344589951));
#69529=CARTESIAN_POINT('Ctrl Pts',(52.535056776177,-5.76249848181913,334.259277404323));
#69530=CARTESIAN_POINT('Ctrl Pts',(52.2568187419033,-3.74130801393427,339.444960411701));
#69531=CARTESIAN_POINT('Ctrl Pts',(51.9785807076291,1.71322559672231,340.551568856769));
#69532=CARTESIAN_POINT('Ctrl Pts',(51.7003426733553,5.59555736443519,336.563584503002));
#69533=CARTESIAN_POINT('Ctrl Pts',(51.4221046390813,4.3429287290972,331.1407217293));
#69534=CARTESIAN_POINT('Ctrl Pts',(51.1438666048075,-0.895141499410306,
329.259461661765));
#69535=CARTESIAN_POINT('Ctrl Pts',(50.8656285705334,-5.31175358617586,332.646208897021));
#69536=CARTESIAN_POINT('Ctrl Pts',(50.5873905362596,-4.85384780826223,338.192995485581));
#69537=CARTESIAN_POINT('Ctrl Pts',(50.3091525019856,0.0583624606174229,
340.809617245559));
#69538=CARTESIAN_POINT('Ctrl Pts',(50.0309144677117,4.91701436081699,338.094839009098));
#69539=CARTESIAN_POINT('Ctrl Pts',(49.7526764334377,5.26339475710779,332.539972693736));
#69540=CARTESIAN_POINT('Ctrl Pts',(49.4744383991637,0.779635472380057,329.242637127389));
#69541=CARTESIAN_POINT('Ctrl Pts',(49.1962003648898,-4.41958377795016,331.2287484907));
#69542=CARTESIAN_POINT('Ctrl Pts',(48.9179623306159,-5.56301622820511,336.675681700515));
#69543=CARTESIAN_POINT('Ctrl Pts',(48.639724296342,-1.60135079582141,340.584866546789));
#69544=CARTESIAN_POINT('Ctrl Pts',(48.361486262068,3.8298506259886,339.368901795568));
#69545=CARTESIAN_POINT('Ctrl Pts',(48.0832482277942,5.74645465683156,334.143660351442));
#69546=CARTESIAN_POINT('Ctrl Pts',(47.80501019352,2.3896220666319,329.704269163243));
#69547=CARTESIAN_POINT('Ctrl Pts',(47.5267721592463,-3.16013142335197,330.124691999078));
#69548=CARTESIAN_POINT('Ctrl Pts',(47.2485341249722,-5.80987894958908,335.01911302793));
#69549=CARTESIAN_POINT('Ctrl Pts',(46.9702960906984,-3.12798631746102,339.89599431316));
#69550=CARTESIAN_POINT('Ctrl Pts',(46.6920580564244,2.42441318919865,340.27989388196));
#69551=CARTESIAN_POINT('Ctrl Pts',(46.4138200221505,5.75196449641075,335.81851276639));
#69552=CARTESIAN_POINT('Ctrl Pts',(46.1355819878765,3.80102288412349,330.605994566335));
#69553=CARTESIAN_POINT('Ctrl Pts',(45.8573439536026,-1.63806132591808,329.425790297338));
#69554=CARTESIAN_POINT('Ctrl Pts',(45.5791059193286,-5.57392083491017,333.360955997275));
#69555=CARTESIAN_POINT('Ctrl Pts',(45.3008678850548,-4.39467546464187,338.800248186262));
#69556=CARTESIAN_POINT('Ctrl Pts',(45.0226298507807,0.817498714224755,340.752108706288));
#69557=CARTESIAN_POINT('Ctrl Pts',(44.7443918165069,5.27946638930855,337.425343967539));
#69558=CARTESIAN_POINT('Ctrl Pts',(44.4661537822328,4.89654568372007,331.872876867797));
#69559=CARTESIAN_POINT('Ctrl Pts',(44.187915747959,0.0201372770774963,329.190124510216));
#69560=CARTESIAN_POINT('Ctrl Pts',(43.909677713685,-4.87475081151337,331.839009135989));
#69561=CARTESIAN_POINT('Ctrl Pts',(43.6314396794111,-5.29615203158245,337.388688421515));
#69562=CARTESIAN_POINT('Ctrl Pts',(43.3532016451371,-0.857352703344343,
340.7463035996));
#69563=CARTESIAN_POINT('Ctrl Pts',(43.0749636108633,4.36822654624751,338.830620779635));
#69564=CARTESIAN_POINT('Ctrl Pts',(42.7967255765892,5.58514876926659,333.399633810069));
#69565=CARTESIAN_POINT('Ctrl Pts',(42.5184875423154,1.67666240339047,329.437279271636));
#69566=CARTESIAN_POINT('Ctrl Pts',(42.2402495080414,-3.77047230258058,330.579751439999));
#69567=CARTESIAN_POINT('Ctrl Pts',(41.9620114737676,-5.7575002285534,335.778620469114));
#69568=CARTESIAN_POINT('Ctrl Pts',(41.6837734394935,-2.46095517534683,340.262960986141));
#69569=CARTESIAN_POINT('Ctrl Pts',(41.4055354052196,3.09397211863666,339.917559887364));
#69570=CARTESIAN_POINT('Ctrl Pts',(41.1272973709457,5.80960686630092,335.059386663018));
#69571=CARTESIAN_POINT('Ctrl Pts',(40.8490593366717,3.19385114241758,330.146715174566));
#69572=CARTESIAN_POINT('Ctrl Pts',(40.5708213023978,-2.35285463369676,329.687831536048));
#69573=CARTESIAN_POINT('Ctrl Pts',(40.2925832681238,-5.74038044054507,334.103846489421));
#69574=CARTESIAN_POINT('Ctrl Pts',(40.0143452338499,-3.86004384498157,339.342248292249));
#69575=CARTESIAN_POINT('Ctrl Pts',(39.736107199576,1.56259801296774,340.595832928758));
#69576=CARTESIAN_POINT('Ctrl Pts',(39.457869165302,5.55126673832543,336.714204280906));
#69577=CARTESIAN_POINT('Ctrl Pts',(39.1796311310281,4.44561991448462,331.259475666079));
#69578=CARTESIAN_POINT('Ctrl Pts',(38.9013930967542,-0.739706687636357,
329.237371022444));
#69579=CARTESIAN_POINT('Ctrl Pts',(38.6231550624802,-5.24621538056624,332.503545935245));
#69580=CARTESIAN_POINT('Ctrl Pts',(38.3449170282063,-4.9383496527626,338.060679895673));
#69581=CARTESIAN_POINT('Ctrl Pts',(38.0666789939323,-0.0986333385400925,
340.809073091401));
#69582=CARTESIAN_POINT('Ctrl Pts',(37.7884409596584,4.83159733463496,338.226565652931));
#69583=CARTESIAN_POINT('Ctrl Pts',(37.5102029253845,5.32794244807527,332.683086538794));
#69584=CARTESIAN_POINT('Ctrl Pts',(37.2319648911105,0.93491341721853,329.265804710423));
#69585=CARTESIAN_POINT('Ctrl Pts',(36.9537268568366,-4.31607185732023,331.11070926271));
#69586=CARTESIAN_POINT('Ctrl Pts',(36.6754888225627,-5.60626169351242,336.524758518774));
#69587=CARTESIAN_POINT('Ctrl Pts',(36.3972507882887,-1.7516679218552,340.539559387556));
#69588=CARTESIAN_POINT('Ctrl Pts',(36.1190127540148,3.71040564711238,339.470788370142));
#69589=CARTESIAN_POINT('Ctrl Pts',(35.8407747197408,5.76749471922252,334.299240854176));
#69590=CARTESIAN_POINT('Ctrl Pts',(35.5625366854669,2.53183901558466,329.770769663146));
#69591=CARTESIAN_POINT('Ctrl Pts',(35.2842986511929,-3.02724798277262,330.041085968933));
#69592=CARTESIAN_POINT('Ctrl Pts',(35.0060606169191,-5.80827418944645,334.862124487579));
#69593=CARTESIAN_POINT('Ctrl Pts',(34.7278225826451,-3.25913290245178,339.809689328935));
#69594=CARTESIAN_POINT('Ctrl Pts',(34.4495845483711,2.28086654440011,340.343473264026));
#69595=CARTESIAN_POINT('Ctrl Pts',(34.1713465140972,5.72774842899101,335.973630654255));
#69596=CARTESIAN_POINT('Ctrl Pts',(33.8931084798233,3.91836012172512,330.710301563841));
#69597=CARTESIAN_POINT('Ctrl Pts',(33.6148704455493,-1.48684943434735,329.383565412443));
#69598=CARTESIAN_POINT('Ctrl Pts',(33.3366324112754,-5.52759921038091,333.21094838361));
#69599=CARTESIAN_POINT('Ctrl Pts',(33.0583943770014,-4.49575277827853,338.680117616777));
#69600=CARTESIAN_POINT('Ctrl Pts',(32.7801563427275,0.661779621247826,340.772097231476));
#69601=CARTESIAN_POINT('Ctrl Pts',(32.5019183084535,5.21200663020625,337.567108412865));
#69602=CARTESIAN_POINT('Ctrl Pts',(32.2236802741797,4.97925208371616,332.006322094225));
#69603=CARTESIAN_POINT('Ctrl Pts',(31.9454422399056,0.177111393640036,329.192789803102));
#69604=CARTESIAN_POINT('Ctrl Pts',(31.6672042056318,-4.78756180821967,331.70844859539));
#69605=CARTESIAN_POINT('Ctrl Pts',(31.3889661713578,-5.35876020297263,337.244715528469));
#69606=CARTESIAN_POINT('Ctrl Pts',(31.1107281370839,-1.01230345462855,340.72104015302));
#69607=CARTESIAN_POINT('Ctrl Pts',(30.8324901028099,4.26312923245365,338.947250671558));
#69608=CARTESIAN_POINT('Ctrl Pts',(30.554252068536,5.62635114659746,333.551127510132));
#69609=CARTESIAN_POINT('Ctrl Pts',(30.276014034262,1.82635365831559,329.484613247335));
#69610=CARTESIAN_POINT('Ctrl Pts',(29.9977759999882,-3.6496616252667,330.479488000484));
#69611=CARTESIAN_POINT('Ctrl Pts',(29.7195379657141,-5.77643630425902,335.622769892941));
#69612=CARTESIAN_POINT('Ctrl Pts',(29.4412999314403,-2.60226064689294,340.194545046715));
#69613=CARTESIAN_POINT('Ctrl Pts',(29.1630618971662,2.95997119682261,339.999362882477));
#69614=CARTESIAN_POINT('Ctrl Pts',(28.8848238628924,5.80588116231729,335.216339191467));
#69615=CARTESIAN_POINT('Ctrl Pts',(28.6065858286184,3.32381967981889,330.234784217607));
#69616=CARTESIAN_POINT('Ctrl Pts',(28.3283477943445,-2.20846206335126,329.626197432781));
#69617=CARTESIAN_POINT('Ctrl Pts',(28.0501097600705,-5.71407076783057,333.949069946695));
#69618=CARTESIAN_POINT('Ctrl Pts',(27.7718717257966,-3.97596106821805,339.236365458825));
#69619=CARTESIAN_POINT('Ctrl Pts',(27.4936336915227,1.410829418609,340.636010918044));
#69620=CARTESIAN_POINT('Ctrl Pts',(27.2153956572488,5.50292257178667,336.863572345158));
#69621=CARTESIAN_POINT('Ctrl Pts',(26.9371576229748,4.54506490383972,331.380960937403));
#69622=CARTESIAN_POINT('Ctrl Pts',(26.6589195887009,-0.583731741312921,
329.219488260466));
#69623=CARTESIAN_POINT('Ctrl Pts',(26.3806815544269,-5.17684638332907,332.362705886685));
#69624=CARTESIAN_POINT('Ctrl Pts',(26.102443520153,-5.01924550949151,337.926129394297));
#69625=CARTESIAN_POINT('Ctrl Pts',(25.824205485879,-0.255557115535859,340.804287146361));
#69626=CARTESIAN_POINT('Ctrl Pts',(25.5459674516051,4.74265227133019,338.355936255349));
#69627=CARTESIAN_POINT('Ctrl Pts',(25.2677294173311,5.38859967022931,332.82789219634));
#69628=CARTESIAN_POINT('Ctrl Pts',(24.9894913830572,1.08950868735974,329.293159408492));
#69629=CARTESIAN_POINT('Ctrl Pts',(24.7112533487833,-4.20940833677799,330.995509998641));
#69630=CARTESIAN_POINT('Ctrl Pts',(24.4330153145093,-5.64541346101978,336.372721956863));
#69631=CARTESIAN_POINT('Ctrl Pts',(24.1547772802354,-1.90070597824981,340.490207236613));
#69632=CARTESIAN_POINT('Ctrl Pts',(23.8765392459615,3.58825132638577,339.56941037065));
#69633=CARTESIAN_POINT('Ctrl Pts',(23.5983012116875,5.78432335129987,334.455333051928));
#69634=CARTESIAN_POINT('Ctrl Pts',(23.3200631774136,2.67220721319882,329.841088552181));
#69635=CARTESIAN_POINT('Ctrl Pts',(23.0418251431397,-2.89215404274099,329.961100942688));
#69636=CARTESIAN_POINT('Ctrl Pts',(22.7635871088657,-5.80242822178108,334.705236624064));
#69637=CARTESIAN_POINT('Ctrl Pts',(22.4853490745917,-3.38789966539284,339.719872304835));
#69638=CARTESIAN_POINT('Ctrl Pts',(22.2071110403179,2.13565440860932,340.40315083666));
#69639=CARTESIAN_POINT('Ctrl Pts',(21.9288730060438,5.6993499540381,336.128037596058));
#69640=CARTESIAN_POINT('Ctrl Pts',(21.65063497177,4.03283616891361,330.817740903362));
#69641=CARTESIAN_POINT('Ctrl Pts',(21.372396937496,-1.3345518438582,329.345441653607));
#69642=CARTESIAN_POINT('Ctrl Pts',(21.0941589032221,-5.47724132747451,333.062247137192));
#69643=CARTESIAN_POINT('Ctrl Pts',(20.8159208689482,-4.5935472888171,338.557299821791));
#69644=CARTESIAN_POINT('Ctrl Pts',(20.5376828346742,0.505577296140925,340.787870965592));
#69645=CARTESIAN_POINT('Ctrl Pts',(20.2594448004003,5.14074105873908,337.706998353104));
#69646=CARTESIAN_POINT('Ctrl Pts',(19.9812067661263,5.05832262894602,332.141953307203));
#69647=CARTESIAN_POINT('Ctrl Pts',(19.7029687318525,0.33395618328883,329.199695526581));
#69648=CARTESIAN_POINT('Ctrl Pts',(19.4247306975784,-4.69687692258734,331.580291548863));
#69649=CARTESIAN_POINT('Ctrl Pts',(19.1464926633046,-5.41745540239484,337.099103541939));
#69650=CARTESIAN_POINT('Ctrl Pts',(18.8682546290305,-1.16651502093527,340.691599197295));
#69651=CARTESIAN_POINT('Ctrl Pts',(18.5900165947567,4.15491897750313,339.06099827716));
#69652=CARTESIAN_POINT('Ctrl Pts',(18.3117785604827,5.66344515679048,333.703679178312));
#69653=CARTESIAN_POINT('Ctrl Pts',(18.0335405262088,1.97471130800469,329.535974563863));
#69654=CARTESIAN_POINT('Ctrl Pts',(17.7553024919348,-3.52618596144585,330.382525443273));
#69655=CARTESIAN_POINT('Ctrl Pts',(17.4770644576609,-5.79115442049705,335.46646456958));
#69656=CARTESIAN_POINT('Ctrl Pts',(17.198826423387,-2.74166594515719,340.122336045387));
#69657=CARTESIAN_POINT('Ctrl Pts',(16.920588389113,2.82380890113031,340.0775153379));
#69658=CARTESIAN_POINT('Ctrl Pts',(16.6423503548391,5.79791599820176,335.373133748825));
#69659=CARTESIAN_POINT('Ctrl Pts',(16.3641123205652,3.45136116082296,330.326332825898));
#69660=CARTESIAN_POINT('Ctrl Pts',(16.0858742862912,-2.06245687183517,329.56848728543));
#69661=CARTESIAN_POINT('Ctrl Pts',(15.8076362520173,-5.68358867502499,333.795060794126));
#69662=CARTESIAN_POINT('Ctrl Pts',(15.5293982177433,-4.08897504077325,339.12738922718));
#69663=CARTESIAN_POINT('Ctrl Pts',(15.2511601834694,1.25803063521879,340.672073486614));
#69664=CARTESIAN_POINT('Ctrl Pts',(14.9729221491955,5.45056016578104,337.011579627053));
#69665=CARTESIAN_POINT('Ctrl Pts',(14.6946841149215,4.64119108232566,331.505088834606));
#69666=CARTESIAN_POINT('Ctrl Pts',(14.4164460806476,-0.427330553480647,
329.205826433848));
#69667=CARTESIAN_POINT('Ctrl Pts',(14.1382080463736,-5.10369724780541,332.223791592866));
#69668=CARTESIAN_POINT('Ctrl Pts',(13.8599700120997,-5.09647630815562,337.789442230377));
#69669=CARTESIAN_POINT('Ctrl Pts',(13.5817319778257,-0.412294284588803,
340.795262905107));
#69670=CARTESIAN_POINT('Ctrl Pts',(13.3034939435518,4.65024411888873,338.48285634988));
#69671=CARTESIAN_POINT('Ctrl Pts',(13.0252559092779,5.4453221312027,332.974283929017));
#69672=CARTESIAN_POINT('Ctrl Pts',(12.747017875004,1.24330839795111,329.324681247404));
#69673=CARTESIAN_POINT('Ctrl Pts',(12.46877984073,-4.0996711035725,330.88323481667));
#69674=CARTESIAN_POINT('Ctrl Pts',(12.1905418064561,-5.68044293934458,336.219683032856));
#69675=CARTESIAN_POINT('Ctrl Pts',(11.9123037721821,-2.04835614241469,340.436846129389));
#69676=CARTESIAN_POINT('Ctrl Pts',(11.6340657379082,3.46347687072457,339.664695786162));
#69677=CARTESIAN_POINT('Ctrl Pts',(11.3558277036343,5.7969282464423,334.611822960457));
#69678=CARTESIAN_POINT('Ctrl Pts',(11.0775896693603,2.81062419710516,329.915174493934));
#69679=CARTESIAN_POINT('Ctrl Pts',(10.7993516350864,-2.75494831436375,329.884795305649));
#69680=CARTESIAN_POINT('Ctrl Pts',(10.5211136008124,-5.79234519187351,334.548564034518));
#69681=CARTESIAN_POINT('Ctrl Pts',(10.2428755665385,-3.51419281376853,339.626608754597));
#69682=CARTESIAN_POINT('Ctrl Pts',(9.96463753226452,1.98888325600979,340.458883156817));
#69683=CARTESIAN_POINT('Ctrl Pts',(9.6863994979906,5.66678897707144,336.281620591485));
#69684=CARTESIAN_POINT('Ctrl Pts',(9.40816146371663,4.1443690044055,330.928234608818));
#69685=CARTESIAN_POINT('Ctrl Pts',(9.12992342944273,-1.18128272534144,329.311445959609));
#69686=CARTESIAN_POINT('Ctrl Pts',(8.85168539516876,-5.42287836274404,332.914962537737));
#69687=CARTESIAN_POINT('Ctrl Pts',(8.57344736089482,-4.68799815077282,338.431881276968));
#69688=CARTESIAN_POINT('Ctrl Pts',(8.2952093266209,0.349025745286411,340.799424444239));
#69689=CARTESIAN_POINT('Ctrl Pts',(8.01697129234695,5.06568404854495,337.844900210057));
#69690=CARTESIAN_POINT('Ctrl Pts',(7.73873325807302,5.13377070045174,332.279693051656));
#69691=CARTESIAN_POINT('Ctrl Pts',(7.46049522379906,0.490422830949281,329.210795885065));
#69692=CARTESIAN_POINT('Ctrl Pts',(7.18225718952515,-4.60250880545255,331.454708526691));
#69693=CARTESIAN_POINT('Ctrl Pts',(6.90401915525119,-5.47267361015814,336.951813491864));
#69694=CARTESIAN_POINT('Ctrl Pts',(6.62578112097724,-1.31897021806641,340.658276570979));
#69695=CARTESIAN_POINT('Ctrl Pts',(6.34754308670334,4.04196323422092,339.17126259052));
#69696=CARTESIAN_POINT('Ctrl Pts',(6.06930505242936,5.69966438415706,333.858154886264));
#69697=CARTESIAN_POINT('Ctrl Pts',(5.79106701815547,2.11523392583091,329.589484673758));
#69698=CARTESIAN_POINT('Ctrl Pts',(5.55920198959383,-2.46923262374946,330.175198721871));
#69699=CARTESIAN_POINT('Ctrl Pts',(5.37370996674454,-4.61534172680647,332.799716245588));
#69700=CARTESIAN_POINT('Ctrl Pts',(5.28096395531991,-4.94983430610851,334.445130104656));
#69701=CARTESIAN_POINT('Ctrl Pts',(5.23459094960758,-4.90621187798767,335.262000892055));
#69702=CARTESIAN_POINT('Ctrl Pts',(185.617269906516,-2.29216991494913,330.278048508348));
#69703=CARTESIAN_POINT('Ctrl Pts',(185.570895172505,-3.07839177256439,330.659702437128));
#69704=CARTESIAN_POINT('Ctrl Pts',(185.478147432782,-4.44361545955773,331.823307916884));
#69705=CARTESIAN_POINT('Ctrl Pts',(185.292653681635,-5.78724472188837,335.186795932361));
#69706=CARTESIAN_POINT('Ctrl Pts',(185.060788653073,-3.96398626270871,339.775335086267));
#69707=CARTESIAN_POINT('Ctrl Pts',(184.782550618799,1.88008622527413,340.918642604601));
#69708=CARTESIAN_POINT('Ctrl Pts',(184.504312584525,5.9896209117165,336.621390747211));
#69709=CARTESIAN_POINT('Ctrl Pts',(184.226074550251,4.6073751195171,330.840900737945));
#69710=CARTESIAN_POINT('Ctrl Pts',(183.947836515977,-1.00552743017874,328.874688417676));
#69711=CARTESIAN_POINT('Ctrl Pts',(183.669598481703,-5.69432997152738,332.530888270267));
#69712=CARTESIAN_POINT('Ctrl Pts',(183.391360447429,-5.15824071662504,338.45226508174));
#69713=CARTESIAN_POINT('Ctrl Pts',(183.113122413155,0.111866319196326,341.205914807967));
#69714=CARTESIAN_POINT('Ctrl Pts',(182.834884378881,5.27911593835755,338.264294481376));
#69715=CARTESIAN_POINT('Ctrl Pts',(182.556646344607,5.60190435506298,332.327181838327));
#69716=CARTESIAN_POINT('Ctrl Pts',(182.278408310334,0.783851916427845,328.842820661638));
#69717=CARTESIAN_POINT('Ctrl Pts',(182.000170276059,-4.75350024470837,331.008840846666));
#69718=CARTESIAN_POINT('Ctrl Pts',(181.721932241786,-5.9286510752286,336.837473644445));
#69719=CARTESIAN_POINT('Ctrl Pts',(181.443694207511,-1.66315801529447,340.979892067162));
#69720=CARTESIAN_POINT('Ctrl Pts',(181.165456173238,4.12858620849688,339.634647530392));
#69721=CARTESIAN_POINT('Ctrl Pts',(180.887218138964,6.13159013610263,334.036257625006));
#69722=CARTESIAN_POINT('Ctrl Pts',(180.60898010469,2.50772306420635,329.322278673983));
#69723=CARTESIAN_POINT('Ctrl Pts',(180.330742070416,-3.41744379639589,329.818661415471));
#69724=CARTESIAN_POINT('Ctrl Pts',(180.052504036142,-6.20647327246837,335.069881763432));
#69725=CARTESIAN_POINT('Ctrl Pts',(179.774266001868,-3.29991365053048,340.256972826555));
#69726=CARTESIAN_POINT('Ctrl Pts',(179.496027967594,2.63492792479757,340.619817425265));
#69727=CARTESIAN_POINT('Ctrl Pts',(179.21778993332,6.15173508641257,335.825438571107));
#69728=CARTESIAN_POINT('Ctrl Pts',(178.939551899046,4.02318573146549,330.273566897255));
#69729=CARTESIAN_POINT('Ctrl Pts',(178.661313864772,-1.79738177270635,329.059073133759));
#69730=CARTESIAN_POINT('Ctrl Pts',(178.383075830499,-5.96851856101238,333.296480260058));
#69731=CARTESIAN_POINT('Ctrl Pts',(178.104837796224,-4.66243395702323,339.09718231172));
#69732=CARTESIAN_POINT('Ctrl Pts',(177.826599761951,0.922297469772181,341.137960628148));
#69733=CARTESIAN_POINT('Ctrl Pts',(177.548361727676,5.66065012278018,337.546023073378));
#69734=CARTESIAN_POINT('Ctrl Pts',(177.270123693403,5.204307708571,331.617637722823));
#69735=CARTESIAN_POINT('Ctrl Pts',(176.991885659128,-0.02795107401978,328.793196310758));
#69736=CARTESIAN_POINT('Ctrl Pts',(176.713647624855,-5.23455956870826,331.664647031874));
#69737=CARTESIAN_POINT('Ctrl Pts',(176.43540959058,-5.63749000907656,337.596901942197));
#69738=CARTESIAN_POINT('Ctrl Pts',(176.157171556307,-0.866979077378676,
341.14601827033));
#69739=CARTESIAN_POINT('Ctrl Pts',(175.878933522033,4.69914575706443,339.055024346885));
#69740=CARTESIAN_POINT('Ctrl Pts',(175.600695487759,5.95293388951394,333.242794432354));
#69741=CARTESIAN_POINT('Ctrl Pts',(175.322457453485,1.74380245672373,329.043126130946));
#69742=CARTESIAN_POINT('Ctrl Pts',(175.044219419211,-4.06559075212348,330.309993055851));
#69743=CARTESIAN_POINT('Ctrl Pts',(174.765981384937,-6.14405133576617,335.880810129014));
#69744=CARTESIAN_POINT('Ctrl Pts',(174.487743350663,-2.58420669462633,340.643320747517));
#69745=CARTESIAN_POINT('Ctrl Pts',(174.209505316389,3.34712628734432,340.227039211301));
#69746=CARTESIAN_POINT('Ctrl Pts',(173.931267282115,6.20685087892184,335.013980941847));
#69747=CARTESIAN_POINT('Ctrl Pts',(173.653029247841,3.37064003188176,329.788092568417));
#69748=CARTESIAN_POINT('Ctrl Pts',(173.374791213568,-2.55875742185098,329.345094717325));
#69749=CARTESIAN_POINT('Ctrl Pts',(173.096553179293,-6.14002095674867,334.091519977878));
#69750=CARTESIAN_POINT('Ctrl Pts',(172.818315145019,-4.08667788619891,339.671643945589));
#69751=CARTESIAN_POINT('Ctrl Pts',(172.540077110746,1.71694916124885,340.964669217786));
#69752=CARTESIAN_POINT('Ctrl Pts',(172.261839076472,5.94495730554663,336.784005587194));
#69753=CARTESIAN_POINT('Ctrl Pts',(171.983601042198,4.71736587797027,330.966186361113));
#69754=CARTESIAN_POINT('Ctrl Pts',(171.705363007924,-0.839282587613181,
328.850138372448));
#69755=CARTESIAN_POINT('Ctrl Pts',(171.42712497365,-5.62573381033469,332.377727627579));
#69756=CARTESIAN_POINT('Ctrl Pts',(171.148886939376,-5.24953215100701,338.311737534204));
#69757=CARTESIAN_POINT('Ctrl Pts',(170.870648905102,-0.0559123196677501,
341.206614786856));
#69758=CARTESIAN_POINT('Ctrl Pts',(170.592410870828,5.18901742216613,338.405773259095));
#69759=CARTESIAN_POINT('Ctrl Pts',(170.314172836554,5.67206246544976,332.479503880593));
#69760=CARTESIAN_POINT('Ctrl Pts',(170.03593480228,0.949939503694936,328.86625658841));
#69761=CARTESIAN_POINT('Ctrl Pts',(169.757696768006,-4.64392891951665,330.881855091139));
#69762=CARTESIAN_POINT('Ctrl Pts',(169.479458733732,-5.9761323175663,336.67661439301));
#69763=CARTESIAN_POINT('Ctrl Pts',(169.201220699458,-1.82412729535379,340.932769413205));
#69764=CARTESIAN_POINT('Ctrl Pts',(168.922982665185,4.00185242173016,339.744509510434));
#69765=CARTESIAN_POINT('Ctrl Pts',(168.64474463091,6.15539123863725,334.202283258784));
#69766=CARTESIAN_POINT('Ctrl Pts',(168.366506596637,2.66021836927275,329.392109886269));
#69767=CARTESIAN_POINT('Ctrl Pts',(168.088268562362,-3.27619763281457,329.728214498801));
#69768=CARTESIAN_POINT('Ctrl Pts',(167.810030528089,-6.20609542386578,334.902158854359));
#69769=CARTESIAN_POINT('Ctrl Pts',(167.531792493814,-3.44075104625367,340.165890585137));
#69770=CARTESIAN_POINT('Ctrl Pts',(167.253554459541,2.48211978110324,340.688960774356));
#69771=CARTESIAN_POINT('Ctrl Pts',(166.975316425266,6.12718592136962,335.991355629872));
#69772=CARTESIAN_POINT('Ctrl Pts',(166.697078390993,4.14942397871105,330.383998056239));
#69773=CARTESIAN_POINT('Ctrl Pts',(166.418840356719,-1.63620310381311,329.012677334318));
#69774=CARTESIAN_POINT('Ctrl Pts',(166.140602322445,-5.92031074828621,333.135834249957));
#69775=CARTESIAN_POINT('Ctrl Pts',(165.862364288171,-4.77143660270046,338.969708559367));
#69776=CARTESIAN_POINT('Ctrl Pts',(165.584126253897,0.756114486894692,341.16063991665));
#69777=CARTESIAN_POINT('Ctrl Pts',(165.305888219623,5.5897904720981,337.698042953318));
#69778=CARTESIAN_POINT('Ctrl Pts',(165.027650185349,5.29379824622925,331.759491794775));
#69779=CARTESIAN_POINT('Ctrl Pts',(164.749412151075,0.139765506129893,328.794707186344));
#69780=CARTESIAN_POINT('Ctrl Pts',(164.471174116801,-5.14252797600939,331.524428203033));
#69781=CARTESIAN_POINT('Ctrl Pts',(164.192936082527,-5.70559943815337,337.443630158443));
#69782=CARTESIAN_POINT('Ctrl Pts',(163.914698048254,-1.03272651041366,341.120348785372));
#69783=CARTESIAN_POINT('Ctrl Pts',(163.63646001398,4.58786429291437,339.180513668164));
#69784=CARTESIAN_POINT('Ctrl Pts',(163.358221979706,5.99823975140083,333.404282861963));
#69785=CARTESIAN_POINT('Ctrl Pts',(163.079983945431,1.90411912390037,329.092418120592));
#69786=CARTESIAN_POINT('Ctrl Pts',(162.801745911158,-3.93738351885127,330.201854074189));
#69787=CARTESIAN_POINT('Ctrl Pts',(162.523507876884,-6.16560742203855,335.714477723383));
#69788=CARTESIAN_POINT('Ctrl Pts',(162.24526984261,-2.7357443982375,340.571435711504));
#69789=CARTESIAN_POINT('Ctrl Pts',(161.967031808336,3.20467088030497,340.315569381432));
#69790=CARTESIAN_POINT('Ctrl Pts',(161.688793774062,6.20420699285626,335.181683487698));
#69791=CARTESIAN_POINT('Ctrl Pts',(161.410555739788,3.51023392200846,329.881069338944));
#69792=CARTESIAN_POINT('Ctrl Pts',(161.132317705514,-2.40502900809874,329.278022302551));
#69793=CARTESIAN_POINT('Ctrl Pts',(160.85407967124,-6.1132323156437,333.925949742852));
#69794=CARTESIAN_POINT('Ctrl Pts',(160.575841636966,-4.21141255828351,339.559517251183));
#69795=CARTESIAN_POINT('Ctrl Pts',(160.297603602692,1.55515834346599,341.008883076468));
#69796=CARTESIAN_POINT('Ctrl Pts',(160.019365568419,5.89458338751627,336.943985593446));
#69797=CARTESIAN_POINT('Ctrl Pts',(159.741127534144,4.82463626075106,331.0951212245));
#69798=CARTESIAN_POINT('Ctrl Pts',(159.462889499871,-0.672808350990864,
328.829706471913));
#69799=CARTESIAN_POINT('Ctrl Pts',(159.184651465596,-5.55282666966348,332.22667901667));
#69800=CARTESIAN_POINT('Ctrl Pts',(158.906413431323,-5.33709791317324,338.168687293676));
#69801=CARTESIAN_POINT('Ctrl Pts',(158.628175397049,-0.223593177199989,
341.202838011026));
#69802=CARTESIAN_POINT('Ctrl Pts',(158.349937362775,5.0950997172598,338.544735839393));
#69803=CARTESIAN_POINT('Ctrl Pts',(158.071699328501,5.73809480473883,332.633681908167));
#69804=CARTESIAN_POINT('Ctrl Pts',(157.793461294227,1.11532498404952,328.894163163016));
#69805=CARTESIAN_POINT('Ctrl Pts',(157.515223259953,-4.53096211233226,330.757880761163));
#69806=CARTESIAN_POINT('Ctrl Pts',(157.236985225679,-6.01925215511788,336.514528571211));
#69807=CARTESIAN_POINT('Ctrl Pts',(156.958747191405,-1.98376333916801,340.881315865866));
#69808=CARTESIAN_POINT('Ctrl Pts',(156.680509157131,3.87219581283742,339.850906398494));
#69809=CARTESIAN_POINT('Ctrl Pts',(156.402271122857,6.1746980209185,334.368891728486));
#69810=CARTESIAN_POINT('Ctrl Pts',(156.124033088583,2.8107709935961,329.466035804104));
#69811=CARTESIAN_POINT('Ctrl Pts',(155.845795054309,-3.13255908763759,329.641617141117));
#69812=CARTESIAN_POINT('Ctrl Pts',(155.567557020035,-6.20118593064259,334.734507338127));
#69813=CARTESIAN_POINT('Ctrl Pts',(155.289318985761,-3.5790759744512,340.071036232271));
#69814=CARTESIAN_POINT('Ctrl Pts',(155.011080951487,2.32749917641929,340.753950024433));
#69815=CARTESIAN_POINT('Ctrl Pts',(154.732842917213,6.09816268692131,336.156548807336));
#69816=CARTESIAN_POINT('Ctrl Pts',(154.45460488294,4.27263230836939,330.497799820378));
#69817=CARTESIAN_POINT('Ctrl Pts',(154.176366848666,-1.47382967562362,328.970653485895));
#69818=CARTESIAN_POINT('Ctrl Pts',(153.898128814392,-5.86777991998716,332.976549454396));
#69819=CARTESIAN_POINT('Ctrl Pts',(153.619890780118,-4.87695514006821,338.839336122517));
#69820=CARTESIAN_POINT('Ctrl Pts',(153.341652745844,0.589379388151474,341.178820699513));
#69821=CARTESIAN_POINT('Ctrl Pts',(153.06341471157,5.51484915109007,337.848092719809));
#69822=CARTESIAN_POINT('Ctrl Pts',(152.785176677296,5.37942324711333,331.903712088916));
#69823=CARTESIAN_POINT('Ctrl Pts',(152.506938643022,0.307380029417682,328.80074917289));
#69824=CARTESIAN_POINT('Ctrl Pts',(152.228700608748,-5.04674130435279,331.386747240111));
#69825=CARTESIAN_POINT('Ctrl Pts',(151.950462574474,-5.76954263289824,337.288574033559));
#69826=CARTESIAN_POINT('Ctrl Pts',(151.6722245402,-1.19771984554265,341.090210215707));
#69827=CARTESIAN_POINT('Ctrl Pts',(151.393986505926,4.47323276575143,339.302950374257));
#69828=CARTESIAN_POINT('Ctrl Pts',(151.115748471652,6.0391656927229,333.566936485794));
#69829=CARTESIAN_POINT('Ctrl Pts',(150.837510437378,2.06304540142216,329.146023832335));
#69830=CARTESIAN_POINT('Ctrl Pts',(150.559272403104,-3.8063012042635,330.097218703396));
#69831=CARTESIAN_POINT('Ctrl Pts',(150.281034368831,-6.18266137571024,335.547623605416));
#69832=CARTESIAN_POINT('Ctrl Pts',(150.002796334556,-2.8852844586,340.495482407657));
#69833=CARTESIAN_POINT('Ctrl Pts',(149.724558300283,3.05987541943865,340.400218117578));
#69834=CARTESIAN_POINT('Ctrl Pts',(149.446320266009,6.19703278874562,335.349253368086));
#69835=CARTESIAN_POINT('Ctrl Pts',(149.168082231735,3.64726463587476,329.977783957673));
#69836=CARTESIAN_POINT('Ctrl Pts',(148.889844197461,-2.24954443980059,329.215128081515));
#69837=CARTESIAN_POINT('Ctrl Pts',(148.611606163187,-6.08197978629243,333.761163780382));
#69838=CARTESIAN_POINT('Ctrl Pts',(148.333368128913,-4.33307205277822,339.444061192799));
#69839=CARTESIAN_POINT('Ctrl Pts',(148.055130094639,1.39223194753191,341.048709242821));
#69840=CARTESIAN_POINT('Ctrl Pts',(147.776892060365,5.83990523890187,337.102546099508));
#69841=CARTESIAN_POINT('Ctrl Pts',(147.498654026091,4.92838368939162,331.226907434206));
#69842=CARTESIAN_POINT('Ctrl Pts',(147.220415991817,-0.505842829049313,
328.81378012578));
#69843=CARTESIAN_POINT('Ctrl Pts',(146.942177957543,-5.4758648494996,332.077655487468));
#69844=CARTESIAN_POINT('Ctrl Pts',(146.66393992327,-5.4207665211968,338.023323274573));
#69845=CARTESIAN_POINT('Ctrl Pts',(146.385701888995,-0.391110766774394,
341.194531916781));
#69846=CARTESIAN_POINT('Ctrl Pts',(146.107463854722,4.99746156553142,338.6811100501));
#69847=CARTESIAN_POINT('Ctrl Pts',(145.829225820447,5.79993718156084,332.789587823537));
#69848=CARTESIAN_POINT('Ctrl Pts',(145.550987786174,1.27989605300435,328.926528225684));
#69849=CARTESIAN_POINT('Ctrl Pts',(145.2727497519,-4.41468679215945,330.637004030825));
#69850=CARTESIAN_POINT('Ctrl Pts',(144.994511717626,-6.05797672882878,336.351336839162));
#69851=CARTESIAN_POINT('Ctrl Pts',(144.716273683352,-2.14195083704191,340.825567775901));
#69852=CARTESIAN_POINT('Ctrl Pts',(144.438035649078,3.73971172275569,339.953761149933));
#69853=CARTESIAN_POINT('Ctrl Pts',(144.159797614804,6.18949603263506,334.535961034068));
#69854=CARTESIAN_POINT('Ctrl Pts',(143.88155958053,2.95927119017693,329.544002628035));
#69855=CARTESIAN_POINT('Ctrl Pts',(143.603321546256,-2.98663314473539,329.558932479864));
#69856=CARTESIAN_POINT('Ctrl Pts',(143.325083511982,-6.191748325357,334.567049684898));
#69857=CARTESIAN_POINT('Ctrl Pts',(143.046845477708,-3.71478745785397,339.972479003764));
#69858=CARTESIAN_POINT('Ctrl Pts',(142.768607443434,2.17117902954865,340.814737734546));
#69859=CARTESIAN_POINT('Ctrl Pts',(142.49036940916,6.06468656808442,336.320897471724));
#69860=CARTESIAN_POINT('Ctrl Pts',(142.212131374886,4.39272075771613,330.614889095514));
#69861=CARTESIAN_POINT('Ctrl Pts',(141.933893340612,-1.31038005555615,328.933032272222));
#69862=CARTESIAN_POINT('Ctrl Pts',(141.655655306338,-5.81096443302246,332.818742184414));
#69863=CARTESIAN_POINT('Ctrl Pts',(141.377417272064,-4.97891251999851,338.706160198657));
#69864=CARTESIAN_POINT('Ctrl Pts',(141.099179237791,0.422213923999755,341.192489701428));
#69865=CARTESIAN_POINT('Ctrl Pts',(140.820941203517,5.43588088181075,337.996062806197));
#69866=CARTESIAN_POINT('Ctrl Pts',(140.542703169243,5.46112018785431,332.050193295534));
#69867=CARTESIAN_POINT('Ctrl Pts',(140.264465134969,0.474770103505825,328.811317858483));
#69868=CARTESIAN_POINT('Ctrl Pts',(139.986227100695,-4.94726949723473,331.251704677905));
#69869=CARTESIAN_POINT('Ctrl Pts',(139.707989066421,-5.82927290194103,337.131846789665));
#69870=CARTESIAN_POINT('Ctrl Pts',(139.429751032147,-1.36183860446307,341.055624568556));
#69871=CARTESIAN_POINT('Ctrl Pts',(139.151512997873,4.35533487962575,339.422245061756));
#69872=CARTESIAN_POINT('Ctrl Pts',(138.873274963599,6.07568182931952,333.730636534013));
#69873=CARTESIAN_POINT('Ctrl Pts',(138.595036929325,2.22046524116368,329.203904123231));
#69874=CARTESIAN_POINT('Ctrl Pts',(138.316798895051,-3.67243952479488,329.996163348326));
#69875=CARTESIAN_POINT('Ctrl Pts',(138.038560860777,-6.19520074396771,335.380369612154));
#69876=CARTESIAN_POINT('Ctrl Pts',(137.760322826503,-3.03271768141446,340.415516297154));
#69877=CARTESIAN_POINT('Ctrl Pts',(137.482084792229,2.91284563453323,340.480923609145));
#69878=CARTESIAN_POINT('Ctrl Pts',(137.203846757955,6.18533350520087,335.516568223324));
#69879=CARTESIAN_POINT('Ctrl Pts',(136.925608723682,3.78163211351856,330.078165803492));
#69880=CARTESIAN_POINT('Ctrl Pts',(136.647370689407,-2.09241725194123,329.156457979643));
#69881=CARTESIAN_POINT('Ctrl Pts',(136.369132655134,-6.04628618932257,333.597282417335));
#69882=CARTESIAN_POINT('Ctrl Pts',(136.09089462086,-4.45156753380044,339.325360076563));
#69883=CARTESIAN_POINT('Ctrl Pts',(135.812656586586,1.22828894246125,341.084118635737));
#69884=CARTESIAN_POINT('Ctrl Pts',(135.534418552312,5.78096278574133,337.259571324341));
#69885=CARTESIAN_POINT('Ctrl Pts',(135.256180518038,5.02853240741745,331.361448759813));
#69886=CARTESIAN_POINT('Ctrl Pts',(134.977942483764,-0.338507940176758,
328.802370963477));
#69887=CARTESIAN_POINT('Ctrl Pts',(134.69970444949,-5.39490454743976,331.930765857103));
#69888=CARTESIAN_POINT('Ctrl Pts',(134.421466415216,-5.50047688017788,337.875751621844));
#69889=CARTESIAN_POINT('Ctrl Pts',(134.143228380942,-0.558342766882442,
341.181702569242));
#69890=CARTESIAN_POINT('Ctrl Pts',(133.864990346668,4.89617426245531,338.814796310628));
#69891=CARTESIAN_POINT('Ctrl Pts',(133.586752312394,5.85754443855144,332.947107784052));
#69892=CARTESIAN_POINT('Ctrl Pts',(133.30851427812,1.44353254060325,328.963328143411));
#69893=CARTESIAN_POINT('Ctrl Pts',(133.030276243846,-4.29518786335118,330.519313164433));
#69894=CARTESIAN_POINT('Ctrl Pts',(132.752038209572,-6.09227776197722,336.187158359625));
#69895=CARTESIAN_POINT('Ctrl Pts',(132.473800175299,-2.29857428030914,340.765565850617));
#69896=CARTESIAN_POINT('Ctrl Pts',(132.195562141024,3.60449689149788,340.052998660112));
#69897=CARTESIAN_POINT('Ctrl Pts',(131.917324106751,6.1997744682642,334.703369181358));
#69898=CARTESIAN_POINT('Ctrl Pts',(131.639086072476,3.10561052402562,329.625953426611));
#69899=CARTESIAN_POINT('Ctrl Pts',(131.360848038203,-2.83852635937508,329.480220891463));
#69900=CARTESIAN_POINT('Ctrl Pts',(131.082610003929,-6.17778949935765,334.399908172415));
#69901=CARTESIAN_POINT('Ctrl Pts',(130.804371969655,-3.84778639980326,339.870290866201));
#69902=CARTESIAN_POINT('Ctrl Pts',(130.526133935381,2.01327348561643,340.871279517449));
#69903=CARTESIAN_POINT('Ctrl Pts',(130.247895901107,6.02678200915386,336.484281615479));
#69904=CARTESIAN_POINT('Ctrl Pts',(129.969657866833,4.50960163804743,330.735180382943));
#69905=CARTESIAN_POINT('Ctrl Pts',(129.691419832559,-1.14597359468405,328.899841164347));
#69906=CARTESIAN_POINT('Ctrl Pts',(129.413181798285,-5.74990577411651,332.662527671032));
#69907=CARTESIAN_POINT('Ctrl Pts',(129.134943764011,-5.07723429311236,338.570278032976));
#69908=CARTESIAN_POINT('Ctrl Pts',(128.856705729737,0.254740158825682,341.201636941275));
#69909=CARTESIAN_POINT('Ctrl Pts',(128.578467695463,5.35294332696797,338.141845164577));
#69910=CARTESIAN_POINT('Ctrl Pts',(128.300229661189,5.53882941326574,332.198828453905));
#69911=CARTESIAN_POINT('Ctrl Pts',(128.021991626915,0.641813499997803,328.826405525861));
#69912=CARTESIAN_POINT('Ctrl Pts',(127.743753592642,-4.84418518906642,331.119399124628));
#69913=CARTESIAN_POINT('Ctrl Pts',(127.465515558368,-5.88474663018062,336.97356286915));
#69914=CARTESIAN_POINT('Ctrl Pts',(127.187277524094,-1.52496294749595,341.016617098393));
#69915=CARTESIAN_POINT('Ctrl Pts',(126.90903948982,4.23425672368954,339.538310621564));
#69916=CARTESIAN_POINT('Ctrl Pts',(126.630801455546,6.10776149707195,333.89526347268));
#69917=CARTESIAN_POINT('Ctrl Pts',(126.352563421272,2.37626369500335,329.266016729034));
#69918=CARTESIAN_POINT('Ctrl Pts',(126.074325386998,-3.53589622637518,329.898761799698));
#69919=CARTESIAN_POINT('Ctrl Pts',(125.796087352724,-6.20321637055196,335.212837872628));
#69920=CARTESIAN_POINT('Ctrl Pts',(125.51784931845,-3.17793641079674,340.331595771327));
#69921=CARTESIAN_POINT('Ctrl Pts',(125.239611284176,2.76368888688211,340.557626924905));
#69922=CARTESIAN_POINT('Ctrl Pts',(124.961373249902,6.16911768505035,335.683505879936));
#69923=CARTESIAN_POINT('Ctrl Pts',(124.683135215628,3.91323823967566,330.182141577479));
#69924=CARTESIAN_POINT('Ctrl Pts',(124.404897181354,-1.93376217894764,329.102054837896));
#69925=CARTESIAN_POINT('Ctrl Pts',(124.12665914708,-6.00617758823367,333.434425320048));
#69926=CARTESIAN_POINT('Ctrl Pts',(123.848421112806,-4.56681247583354,339.203500578147));
#69927=CARTESIAN_POINT('Ctrl Pts',(123.570183078532,1.06344903959737,341.115085399248));
#69928=CARTESIAN_POINT('Ctrl Pts',(123.291945044258,5.71779906787188,337.414946607972));
#69929=CARTESIAN_POINT('Ctrl Pts',(123.013707009985,5.12500928613626,331.498646959113));
#69930=CARTESIAN_POINT('Ctrl Pts',(122.73546897571,-0.170925872473485,328.795487315991));
#69931=CARTESIAN_POINT('Ctrl Pts',(122.457230941437,-5.31000488077602,331.786117384526));
#69932=CARTESIAN_POINT('Ctrl Pts',(122.178992907162,-5.5761707855341,337.726080092452));
#69933=CARTESIAN_POINT('Ctrl Pts',(121.900754872889,-0.725167064553412,
341.164359336411));
#69934=CARTESIAN_POINT('Ctrl Pts',(121.622516838615,4.79131176811961,338.94569700314));
#69935=CARTESIAN_POINT('Ctrl Pts',(121.344278804341,5.91087451083504,333.106126768479));
#69936=CARTESIAN_POINT('Ctrl Pts',(121.066040770067,1.60611495932192,329.004536044862));
#69937=CARTESIAN_POINT('Ctrl Pts',(120.787802735793,-4.17255258414297,330.404894099973));
#69938=CARTESIAN_POINT('Ctrl Pts',(120.509564701519,-6.12213020791506,336.022113015885));
#69939=CARTESIAN_POINT('Ctrl Pts',(120.231326667245,-2.45351930237723,340.701353903483));
#69940=CARTESIAN_POINT('Ctrl Pts',(119.953088632971,3.46665005306664,340.148546465701));
#69941=CARTESIAN_POINT('Ctrl Pts',(119.674850598697,6.20552582248217,334.870993928765));
#69942=CARTESIAN_POINT('Ctrl Pts',(119.396612564423,3.24968213801681,329.711828359275));
#69943=CARTESIAN_POINT('Ctrl Pts',(119.118374530149,-2.68834687927684,329.405539851193));
#69944=CARTESIAN_POINT('Ctrl Pts',(118.840136495875,-6.15931964539302,334.233204847575));
#69945=CARTESIAN_POINT('Ctrl Pts',(118.561898461601,-3.97797568434098,339.764546437459));
#69946=CARTESIAN_POINT('Ctrl Pts',(118.283660427328,1.85389784740593,340.923534086277));
#69947=CARTESIAN_POINT('Ctrl Pts',(118.005422393054,5.98447668807579,336.646581935339));
#69948=CARTESIAN_POINT('Ctrl Pts',(117.72718435878,4.62318960282962,330.85858584585));
#69949=CARTESIAN_POINT('Ctrl Pts',(117.448946324506,-0.980730342766608,
328.871104398451));
#69950=CARTESIAN_POINT('Ctrl Pts',(117.170708290232,-5.68464852836201,332.508019982243));
#69951=CARTESIAN_POINT('Ctrl Pts',(116.892470255958,-5.17184866475443,338.431788846766));
#69952=CARTESIAN_POINT('Ctrl Pts',(116.614232221684,0.087080382136921,341.206255739731));
#69953=CARTESIAN_POINT('Ctrl Pts',(116.33599418741,5.26609704764564,338.285333344531));
#69954=CARTESIAN_POINT('Ctrl Pts',(116.057756153136,5.61249417999503,332.349509030494));
#69955=CARTESIAN_POINT('Ctrl Pts',(115.779518118862,0.80838824364127,328.846001157991));
#69956=CARTESIAN_POINT('Ctrl Pts',(115.501280084588,-4.73756365211115,330.989927189924));
#69957=CARTESIAN_POINT('Ctrl Pts',(115.223042050314,-5.93592331064607,336.813837851088));
#69958=CARTESIAN_POINT('Ctrl Pts',(114.94480401604,-1.68697376108552,340.973216288509));
#69959=CARTESIAN_POINT('Ctrl Pts',(114.666565981766,4.1100867093313,339.651062302496));
#69960=CARTESIAN_POINT('Ctrl Pts',(114.388327947492,6.13538127137518,334.060697091047));
#69961=CARTESIAN_POINT('Ctrl Pts',(114.110089913219,2.53032699875718,329.332316295059));
#69962=CARTESIAN_POINT('Ctrl Pts',(113.831851878945,-3.39677101305501,329.805085180218));
#69963=CARTESIAN_POINT('Ctrl Pts',(113.553613844671,-6.20670240244458,335.045150718677));
#69964=CARTESIAN_POINT('Ctrl Pts',(113.275375810397,-3.32083460788806,340.243782109027));
#69965=CARTESIAN_POINT('Ctrl Pts',(112.997137776123,2.61251409088887,340.630272056021));
#69966=CARTESIAN_POINT('Ctrl Pts',(112.718899741849,6.14839716910185,335.849944439884));
#69967=CARTESIAN_POINT('Ctrl Pts',(112.440661707575,4.04198691542352,330.289635356424));
#69968=CARTESIAN_POINT('Ctrl Pts',(112.162423673301,-1.77369507090989,329.051958381506));
#69969=CARTESIAN_POINT('Ctrl Pts',(111.884185639027,-5.96168327036564,333.27271140693));
#69970=CARTESIAN_POINT('Ctrl Pts',(111.605947604753,-4.67872272690766,339.078571679476));
#69971=CARTESIAN_POINT('Ctrl Pts',(111.327709570479,0.897832605199222,341.141586921387));
#69972=CARTESIAN_POINT('Ctrl Pts',(111.049471536205,5.65046020750232,337.568558495216));
#69973=CARTESIAN_POINT('Ctrl Pts',(110.771233501931,5.21774387803648,331.638401849845));
#69974=CARTESIAN_POINT('Ctrl Pts',(110.492995467657,-0.00321899453002624,
328.793134209766));
#69975=CARTESIAN_POINT('Ctrl Pts',(110.214757433383,-5.22122784332861,331.643815692195));
#69976=CARTESIAN_POINT('Ctrl Pts',(109.93651939911,-5.64779296550117,337.574417976698));
#69977=CARTESIAN_POINT('Ctrl Pts',(109.658281364835,-0.891461844520826,
341.142514882332));
#69978=CARTESIAN_POINT('Ctrl Pts',(109.380043330562,4.68295065322101,339.073716543821));
#69979=CARTESIAN_POINT('Ctrl Pts',(109.101805296288,5.95988845674028,333.266528661003));
#69980=CARTESIAN_POINT('Ctrl Pts',(108.823567262014,1.76752459131841,329.050121839987));
#69981=CARTESIAN_POINT('Ctrl Pts',(108.54532922774,-4.04687050293616,330.293830386358));
#69982=CARTESIAN_POINT('Ctrl Pts',(108.267091193466,-6.14751226835692,335.856321324217));
#69983=CARTESIAN_POINT('Ctrl Pts',(107.988853159192,-2.60667276223889,340.632978822125));
#69984=CARTESIAN_POINT('Ctrl Pts',(107.710615124918,3.32627186335888,340.2403347976));
#69985=CARTESIAN_POINT('Ctrl Pts',(107.432377090644,6.20674589564442,335.038712876532));
#69986=CARTESIAN_POINT('Ctrl Pts',(107.15413905637,3.39138083091633,329.801564720073));
#69987=CARTESIAN_POINT('Ctrl Pts',(106.875901022096,-2.53620436564467,329.334943891222));
#69988=CARTESIAN_POINT('Ctrl Pts',(106.597662987822,-6.13635225016862,334.067061437308));
#69989=CARTESIAN_POINT('Ctrl Pts',(106.319424953548,-4.10526024712359,339.655322932224));
#69990=CARTESIAN_POINT('Ctrl Pts',(106.041186919274,1.69316849116485,340.971463284693));
#69991=CARTESIAN_POINT('Ctrl Pts',(105.762948885,5.93780149623726,336.807679919453));
#69992=CARTESIAN_POINT('Ctrl Pts',(105.484710850726,4.73340171001917,330.985015373441));
#69993=CARTESIAN_POINT('Ctrl Pts',(105.206472816452,-0.814770960588805,
328.846842958148));
#69994=CARTESIAN_POINT('Ctrl Pts',(104.928234782179,-5.61524034666409,332.355331939712));
#69995=CARTESIAN_POINT('Ctrl Pts',(104.649996747905,-5.26268654741741,338.290793764967));
#69996=CARTESIAN_POINT('Ctrl Pts',(104.371758713631,-0.0806429807318726,
341.206342724146));
#69997=CARTESIAN_POINT('Ctrl Pts',(104.093520679357,5.17540545908285,338.426422570846));
#69998=CARTESIAN_POINT('Ctrl Pts',(103.815282645083,5.68206069795661,332.502124998195));
#69999=CARTESIAN_POINT('Ctrl Pts',(103.537044610809,0.974372701394095,328.870090446125));
#70000=CARTESIAN_POINT('Ctrl Pts',(103.258806576535,-4.62748274152016,330.86338341433));
#70001=CARTESIAN_POINT('Ctrl Pts',(102.980568542261,-5.98276557407492,336.652788366844));
#70002=CARTESIAN_POINT('Ctrl Pts',(102.702330507987,-1.84775274477625,340.925453830221));
#70003=CARTESIAN_POINT('Ctrl Pts',(102.424092473713,3.98291550561775,339.76041777316));
#70004=CARTESIAN_POINT('Ctrl Pts',(102.145854439439,6.15852098424286,334.226816589321));
#70005=CARTESIAN_POINT('Ctrl Pts',(101.867616405165,2.682542655249,329.402754409294));
#70006=CARTESIAN_POINT('Ctrl Pts',(101.589378370891,-3.25516547420216,329.715201892649));
#70007=CARTESIAN_POINT('Ctrl Pts',(101.311140336617,-6.20565629414165,334.877430595626));
#70008=CARTESIAN_POINT('Ctrl Pts',(101.032902302343,-3.4613079282841,340.152139431878));
#70009=CARTESIAN_POINT('Ctrl Pts',(100.75466426807,2.4594316345385,340.698805956947));
#70010=CARTESIAN_POINT('Ctrl Pts',(100.476426233796,6.12318708749654,336.015762369565));
#70011=CARTESIAN_POINT('Ctrl Pts',(100.198188199522,4.16778412835227,330.400568648261));
#70012=CARTESIAN_POINT('Ctrl Pts',(99.9199501652471,-1.61233280898796,329.006205190952));
#70013=CARTESIAN_POINT('Ctrl Pts',(99.6417121309733,-5.91283572551321,333.112258761641));
#70014=CARTESIAN_POINT('Ctrl Pts',(99.3634740966994,-4.78721657004721,338.950664603756));
#70015=CARTESIAN_POINT('Ctrl Pts',(99.0852360624254,0.73156057255035,341.163603850719));
#70016=CARTESIAN_POINT('Ctrl Pts',(98.8069980281515,5.5789953755348,337.720294818521));
#70017=CARTESIAN_POINT('Ctrl Pts',(98.5287599938776,5.30666846822774,331.780611382852));
#70018=CARTESIAN_POINT('Ctrl Pts',(98.2505219596036,0.164490233926267,328.795313363042));
#70019=CARTESIAN_POINT('Ctrl Pts',(97.9722839253297,-5.12863826017746,331.503964688944));
#70020=CARTESIAN_POINT('Ctrl Pts',(97.6940458910556,-5.71529112149298,337.420876018406));
#70021=CARTESIAN_POINT('Ctrl Pts',(97.4158078567819,-1.05710567817306,341.116185157848));
#70022=CARTESIAN_POINT('Ctrl Pts',(97.1375698225077,4.57117004315204,339.198761452678));
#70023=CARTESIAN_POINT('Ctrl Pts',(96.8593317882339,6.00455048623575,333.428196336003));
#70024=CARTESIAN_POINT('Ctrl Pts',(96.5810937539601,1.92764357512081,329.100052241994));
#70025=CARTESIAN_POINT('Ctrl Pts',(96.3028557196859,-3.91823339290997,330.18620312242));
#70026=CARTESIAN_POINT('Ctrl Pts',(96.0246176854122,-6.16840540929736,335.689904345876));
#70027=CARTESIAN_POINT('Ctrl Pts',(95.7463796511382,-2.75792282708715,340.560490534093));
#70028=CARTESIAN_POINT('Ctrl Pts',(95.4681416168641,3.18346482666672,340.328296631878));
#70029=CARTESIAN_POINT('Ctrl Pts',(95.1899035825903,6.20343379685237,335.206403556118));
#70030=CARTESIAN_POINT('Ctrl Pts',(94.9116655483162,3.53060313419934,329.89509698342));
#70031=CARTESIAN_POINT('Ctrl Pts',(94.6334275140424,-2.38220991309158,329.268484560793));
#70032=CARTESIAN_POINT('Ctrl Pts',(94.3551894797685,-6.10890408449904,333.901599259696));
#70033=CARTESIAN_POINT('Ctrl Pts',(94.0769514454943,-4.22954714483822,339.542700105609));
#70034=CARTESIAN_POINT('Ctrl Pts',(93.7987134112207,1.53120278162712,341.015032114749));
#70035=CARTESIAN_POINT('Ctrl Pts',(93.5204753769465,5.88679051590925,336.967457933911));
#70036=CARTESIAN_POINT('Ctrl Pts',(93.2422373426728,4.84015748262706,331.114376646755));
#70037=CARTESIAN_POINT('Ctrl Pts',(92.9639993083986,-0.648216631854655,
328.827074559167));
#70038=CARTESIAN_POINT('Ctrl Pts',(92.6857612741249,-5.54173191094504,332.204575036399));
#70039=CARTESIAN_POINT('Ctrl Pts',(92.4075232398509,-5.34968161119029,338.147395742324));
#70040=CARTESIAN_POINT('Ctrl Pts',(92.1292852055768,-0.248307458017522,
341.201897831003));
#70041=CARTESIAN_POINT('Ctrl Pts',(91.8510471713032,5.08093478436595,338.565009820033));
#70042=CARTESIAN_POINT('Ctrl Pts',(91.5728091370289,5.74747816961128,332.656564916677));
#70043=CARTESIAN_POINT('Ctrl Pts',(91.2945711027553,1.13964567124306,328.898655800242));
#70044=CARTESIAN_POINT('Ctrl Pts',(91.0163330684812,-4.51402283848238,330.739860200232));
#70045=CARTESIAN_POINT('Ctrl Pts',(90.7380950342073,-6.02523921620042,336.490532014909));
#70046=CARTESIAN_POINT('Ctrl Pts',(90.4598569999334,-2.00718249759639,340.873364599721));
#70047=CARTESIAN_POINT('Ctrl Pts',(90.1816189656593,3.85283597308675,339.866297182088));
#70048=CARTESIAN_POINT('Ctrl Pts',(89.9033809313856,6.17716373903393,334.393500666882));
#70049=CARTESIAN_POINT('Ctrl Pts',(89.6251428971114,2.832799516457,329.477279637762));
#70050=CARTESIAN_POINT('Ctrl Pts',(89.3469048628377,-3.11118301032018,329.62917756985));
#70051=CARTESIAN_POINT('Ctrl Pts',(89.0686668285635,-6.20007880951249,334.709799972876));
#70052=CARTESIAN_POINT('Ctrl Pts',(88.7904287942898,-3.59925379822841,340.056734657449));
#70053=CARTESIAN_POINT('Ctrl Pts',(88.5121907600156,2.30455329879092,340.763178584161));
#70054=CARTESIAN_POINT('Ctrl Pts',(88.2339527257419,6.09350584866075,336.180838588566));
#70055=CARTESIAN_POINT('Ctrl Pts',(87.9557146914679,4.2905380212135,330.514860449392));
#70056=CARTESIAN_POINT('Ctrl Pts',(87.677476657194,-1.44979322006398,328.96482867526));
#70057=CARTESIAN_POINT('Ctrl Pts',(87.39923862292,-5.8596706222016,332.953184546859));
#70058=CARTESIAN_POINT('Ctrl Pts',(87.1210005886461,-4.89221478294142,338.819872748859));
#70059=CARTESIAN_POINT('Ctrl Pts',(86.8427625543722,0.564754353652266,341.18112011046));
#70060=CARTESIAN_POINT('Ctrl Pts',(86.5645245200982,5.50345675565987,337.870044779876));
#70061=CARTESIAN_POINT('Ctrl Pts',(86.2862864858242,5.39171812388697,331.92517171659));
#70062=CARTESIAN_POINT('Ctrl Pts',(86.0080484515503,0.332079351452054,328.802023184599));
#70063=CARTESIAN_POINT('Ctrl Pts',(85.7298104172765,-5.03230374032721,331.366666494113));
#70064=CARTESIAN_POINT('Ctrl Pts',(85.4515723830023,-5.77861596628966,337.265566334065));
#70065=CARTESIAN_POINT('Ctrl Pts',(85.1733343487285,-1.22197761221993,341.08538938895));
#70066=CARTESIAN_POINT('Ctrl Pts',(84.8950963144546,4.45605156022403,339.320740421795));
#70067=CARTESIAN_POINT('Ctrl Pts',(84.6168582801807,6.04482798706362,333.591011743583));
#70068=CARTESIAN_POINT('Ctrl Pts',(84.3386202459067,2.08635499168976,329.154290791653));
#70069=CARTESIAN_POINT('Ctrl Pts',(84.0603822116327,-3.78673518500859,330.082090897696));
#70070=CARTESIAN_POINT('Ctrl Pts',(83.7821441773588,-6.18479437454427,335.522983598705));
#70071=CARTESIAN_POINT('Ctrl Pts',(83.5039061430849,-2.907159053976,340.483941970407));
#70072=CARTESIAN_POINT('Ctrl Pts',(83.225668108811,3.03833322082874,340.412367738718));
#70073=CARTESIAN_POINT('Ctrl Pts',(82.947430074537,6.19559194460378,335.373943519624));
#70074=CARTESIAN_POINT('Ctrl Pts',(82.6691920402631,3.66724738760314,329.992356851969));
#70075=CARTESIAN_POINT('Ctrl Pts',(82.3909540059891,-2.2264759685182,329.206210388569));
#70076=CARTESIAN_POINT('Ctrl Pts',(82.1127159717152,-6.07699519106181,333.736939135386));
#70077=CARTESIAN_POINT('Ctrl Pts',(81.8344779374412,-4.35074562306998,339.42676019491));
#70078=CARTESIAN_POINT('Ctrl Pts',(81.5562399031674,1.36811898631292,341.054208762439));
#70079=CARTESIAN_POINT('Ctrl Pts',(81.2780018688933,5.83148099535957,337.125799308652));
#70080=CARTESIAN_POINT('Ctrl Pts',(80.9997638346196,4.9433789674834,331.246575206061));
#70081=CARTESIAN_POINT('Ctrl Pts',(80.7215258003455,-0.481188974698351,
328.811813636409));
#70082=CARTESIAN_POINT('Ctrl Pts',(80.4432877660716,-5.46417689713705,332.055859355143));
#70083=CARTESIAN_POINT('Ctrl Pts',(80.1650497317976,-5.43277033219188,338.001699488218));
#70084=CARTESIAN_POINT('Ctrl Pts',(79.8868116975237,-0.415790620952878,
341.192924305967));
#70085=CARTESIAN_POINT('Ctrl Pts',(79.6085736632497,4.98275400607507,338.700993895544));
#70086=CARTESIAN_POINT('Ctrl Pts',(79.3303356289758,5.8086988270565,332.81271601376));
#70087=CARTESIAN_POINT('Ctrl Pts',(79.0520975947017,1.30408647070233,328.931676361891));
#70088=CARTESIAN_POINT('Ctrl Pts',(78.7738595604281,-4.39726679153062,330.619447744404));
#70089=CARTESIAN_POINT('Ctrl Pts',(78.4956215261539,-6.06331322272737,336.327187275032));
#70090=CARTESIAN_POINT('Ctrl Pts',(78.21738349188,-2.16514660378369,340.816986632616));
#70091=CARTESIAN_POINT('Ctrl Pts',(77.939145457606,3.71994309594081,339.96862321603));
#70092=CARTESIAN_POINT('Ctrl Pts',(77.6609074233321,6.1912959227905,334.560627610852));
#70093=CARTESIAN_POINT('Ctrl Pts',(77.3826693890583,2.98098786467339,329.555837562069));
#70094=CARTESIAN_POINT('Ctrl Pts',(77.1044313547843,-2.96492875754574,329.54707502687));
#70095=CARTESIAN_POINT('Ctrl Pts',(76.8261933205103,-6.18997402124187,334.542381254471));
#70096=CARTESIAN_POINT('Ctrl Pts',(76.5479552862364,-3.73457148951113,339.957637450403));
#70097=CARTESIAN_POINT('Ctrl Pts',(76.2697172519624,2.14799217595916,340.823342932708));
#70098=CARTESIAN_POINT('Ctrl Pts',(75.9914792176885,6.05937512586425,336.345052558068));
#70099=CARTESIAN_POINT('Ctrl Pts',(75.7132411834145,4.41015895899399,330.632427303832));
#70100=CARTESIAN_POINT('Ctrl Pts',(75.4350031491406,-1.28619499070553,328.927859047602));
#70101=CARTESIAN_POINT('Ctrl Pts',(75.1567651148666,-5.80222678164153,332.795604918733));
#70102=CARTESIAN_POINT('Ctrl Pts',(74.8785270805928,-4.99364069579202,338.686291619127));
#70103=CARTESIAN_POINT('Ctrl Pts',(74.6002890463187,0.397535750569984,341.194122910221));
#70104=CARTESIAN_POINT('Ctrl Pts',(74.3220510120449,5.42389950625196,338.017699031711));
#70105=CARTESIAN_POINT('Ctrl Pts',(74.0438129777708,5.47283074167201,332.071977292964));
#70106=CARTESIAN_POINT('Ctrl Pts',(73.7655749434971,0.499425984308978,328.81325877492));
#70107=CARTESIAN_POINT('Ctrl Pts',(73.4873369092229,-4.93229462733895,331.232021362981));
#70108=CARTESIAN_POINT('Ctrl Pts',(73.2090988749492,-5.83772126002729,337.108602330961));
#70109=CARTESIAN_POINT('Ctrl Pts',(72.9308608406751,-1.38595725701314,341.050150062737));
#70110=CARTESIAN_POINT('Ctrl Pts',(72.6526228064015,4.33767926406639,339.439564382009));
#70111=CARTESIAN_POINT('Ctrl Pts',(72.3743847721271,6.08069154855318,333.754855995773));
#70112=CARTESIAN_POINT('Ctrl Pts',(72.0961467378534,2.24354294979286,329.212797883922));
#70113=CARTESIAN_POINT('Ctrl Pts',(71.8179087035794,-3.65247189935271,329.981569735032));
#70114=CARTESIAN_POINT('Ctrl Pts',(71.5396706693055,-6.19666719685916,335.355680968395));
#70115=CARTESIAN_POINT('Ctrl Pts',(71.2614326350313,-3.05427247046587,340.403389026903));
#70116=CARTESIAN_POINT('Ctrl Pts',(70.9831946007578,2.89098302108621,340.492486729315));
#70117=CARTESIAN_POINT('Ctrl Pts',(70.7049565664835,6.18322606502682,335.541210429205));
#70118=CARTESIAN_POINT('Ctrl Pts',(70.4267185322099,3.8012138133597,330.093273306468));
#70119=CARTESIAN_POINT('Ctrl Pts',(70.1484804979358,-2.06911624900363,329.148166847215));
#70120=CARTESIAN_POINT('Ctrl Pts',(69.8702424636618,-6.04064886976221,333.57320129936));
#70121=CARTESIAN_POINT('Ctrl Pts',(69.592004429388,-4.46876718257118,339.307587859566));
#70122=CARTESIAN_POINT('Ctrl Pts',(69.313766395114,1.20403618916992,341.088964620942));
#70123=CARTESIAN_POINT('Ctrl Pts',(69.0355283608399,5.7719133216548,337.282588422648));
#70124=CARTESIAN_POINT('Ctrl Pts',(68.7572903265662,5.04299079215806,331.381514519843));
#70125=CARTESIAN_POINT('Ctrl Pts',(68.479052292292,-0.313809952880065,328.801071333416));
#70126=CARTESIAN_POINT('Ctrl Pts',(68.2008142580184,-5.38263193598747,331.90929348828));
#70127=CARTESIAN_POINT('Ctrl Pts',(67.9225762237442,-5.51189203895631,337.853811390193));
#70128=CARTESIAN_POINT('Ctrl Pts',(67.6443381894704,-0.582970173168094,
341.179428701516));
#70129=CARTESIAN_POINT('Ctrl Pts',(67.3661001551964,4.88093481591085,338.834275501673));
#70130=CARTESIAN_POINT('Ctrl Pts',(67.0878621209226,5.86567796690818,332.97046426776));
#70131=CARTESIAN_POINT('Ctrl Pts',(66.8096240866486,1.46757502493876,328.969128019425));
#70132=CARTESIAN_POINT('Ctrl Pts',(66.5313860523745,-4.2772998560451,330.502233972139));
#70133=CARTESIAN_POINT('Ctrl Pts',(66.2531480181009,-6.09695979197876,336.162873421702));
#70134=CARTESIAN_POINT('Ctrl Pts',(65.9749099838266,-2.32152971779252,340.756361096154));
#70135=CARTESIAN_POINT('Ctrl Pts',(65.696671949553,3.58433391268944,340.067321156415));
#70136=CARTESIAN_POINT('Ctrl Pts',(65.4184339152789,6.20090721617813,334.728075384972));
#70137=CARTESIAN_POINT('Ctrl Pts',(65.1401958810049,3.12699949262064,329.63837081914));
#70138=CARTESIAN_POINT('Ctrl Pts',(64.8619578467309,-2.81650951087796,329.468954215065));
#70139=CARTESIAN_POINT('Ctrl Pts',(64.583719812457,-6.17534930785609,334.375296689724));
#70140=CARTESIAN_POINT('Ctrl Pts',(64.305481778183,-3.86716219302106,339.854920171618));
#70141=CARTESIAN_POINT('Ctrl Pts',(64.0272437439093,1.98986258712899,340.879255070521));
#70142=CARTESIAN_POINT('Ctrl Pts',(63.749005709635,6.02081984139441,336.508284368871));
#70143=CARTESIAN_POINT('Ctrl Pts',(63.4707676753615,4.52655959436737,330.753183364147));
#70144=CARTESIAN_POINT('Ctrl Pts',(63.1925296410872,-1.12165758050052,328.895323303236));
#70145=CARTESIAN_POINT('Ctrl Pts',(62.9142916068136,-5.74054614938183,332.639634942063));
#70146=CARTESIAN_POINT('Ctrl Pts',(62.6360535725393,-5.09142024729771,338.550018755629));
#70147=CARTESIAN_POINT('Ctrl Pts',(62.3578155382655,0.230026866491849,341.202602755343));
#70148=CARTESIAN_POINT('Ctrl Pts',(62.0795775039915,5.34038172009283,338.163149756747));
#70149=CARTESIAN_POINT('Ctrl Pts',(61.8013394697177,5.5499470930696,332.220920914397));
#70150=CARTESIAN_POINT('Ctrl Pts',(61.5231014354438,0.666407935821213,328.829011929764));
#70151=CARTESIAN_POINT('Ctrl Pts',(61.2448634011698,-4.82868394796529,331.100127613554));
#70152=CARTESIAN_POINT('Ctrl Pts',(60.9666253668957,-5.89256384396229,336.950098624361));
#70153=CARTESIAN_POINT('Ctrl Pts',(60.6883873326221,-1.54892487445486,341.010492911002));
#70154=CARTESIAN_POINT('Ctrl Pts',(60.4101492983478,4.21613959024611,339.555146567945));
#70155=CARTESIAN_POINT('Ctrl Pts',(60.1319112640742,6.11211498309658,333.919609453339));
#70156=CARTESIAN_POINT('Ctrl Pts',(59.8536732298,2.39909267062866,329.275530796865));
#70157=CARTESIAN_POINT('Ctrl Pts',(59.5754351955263,-3.51554157512524,329.884713035079));
#70158=CARTESIAN_POINT('Ctrl Pts',(59.2971971612521,-6.20401520669551,335.188118619492));
#70159=CARTESIAN_POINT('Ctrl Pts',(59.0189591269783,-3.19915565419569,340.31889052342));
#70160=CARTESIAN_POINT('Ctrl Pts',(58.7407210927044,2.74152182269945,340.568595100703));
#70161=CARTESIAN_POINT('Ctrl Pts',(58.4624830584305,6.16634518769909,335.708082146398));
#70162=CARTESIAN_POINT('Ctrl Pts',(58.1842450241564,3.93240458905305,330.197772657621));
#70163=CARTESIAN_POINT('Ctrl Pts',(57.9060069898825,-1.91024565877038,329.094396320183));
#70164=CARTESIAN_POINT('Ctrl Pts',(57.6277689556085,-5.99989166071994,333.410505313149));
#70165=CARTESIAN_POINT('Ctrl Pts',(57.3495309213347,-4.58352564388255,339.185270119332));
#70166=CARTESIAN_POINT('Ctrl Pts',(57.0712928870607,1.03907420361824,341.119274311492));
#70167=CARTESIAN_POINT('Ctrl Pts',(56.7930548527868,5.70813099116869,337.437710788336));
#70168=CARTESIAN_POINT('Ctrl Pts',(56.5148168185127,5.13892021999894,331.519096055276));
#70169=CARTESIAN_POINT('Ctrl Pts',(56.2365787842391,-0.146201786725707,
328.794855494232));
#70170=CARTESIAN_POINT('Ctrl Pts',(55.9583407499648,-5.29715657170701,331.764984458348));
#70171=CARTESIAN_POINT('Ctrl Pts',(55.6801027156911,-5.58698895673563,337.703839436287));
#70172=CARTESIAN_POINT('Ctrl Pts',(55.401864681417,-0.74972403998978,341.16142087215));
#70173=CARTESIAN_POINT('Ctrl Pts',(55.1236266471431,4.775551562346,338.964757316064));
#70174=CARTESIAN_POINT('Ctrl Pts',(54.8453886128692,5.91837398294238,333.129694490748));
#70175=CARTESIAN_POINT('Ctrl Pts',(54.5671505785953,1.62999195444933,329.010983425608));
#70176=CARTESIAN_POINT('Ctrl Pts',(54.2889125443213,-4.15420963200005,330.388304473048));
#70177=CARTESIAN_POINT('Ctrl Pts',(54.0106745100473,-6.12615435519665,335.997710437058));
#70178=CARTESIAN_POINT('Ctrl Pts',(53.7324364757735,-2.47621764851933,340.691532259161));
#70179=CARTESIAN_POINT('Ctrl Pts',(53.4541984414994,3.44610744529158,340.16231893391));
#70180=CARTESIAN_POINT('Ctrl Pts',(53.1759604072256,6.20599060102094,334.895721718714));
#70181=CARTESIAN_POINT('Ctrl Pts',(52.8977223729516,3.2707277824645,329.724819143107));
#70182=CARTESIAN_POINT('Ctrl Pts',(52.6194843386776,-2.66603364619667,329.394872178331));
#70183=CARTESIAN_POINT('Ctrl Pts',(52.3412463044037,-6.15621534833528,334.208668283948));
#70184=CARTESIAN_POINT('Ctrl Pts',(52.0630082701298,-3.99692909089618,339.74865782535));
#70185=CARTESIAN_POINT('Ctrl Pts',(51.7847702358559,1.83027999868166,340.930874170501));
#70186=CARTESIAN_POINT('Ctrl Pts',(51.506532201582,5.97786814835784,336.670414828945));
#70187=CARTESIAN_POINT('Ctrl Pts',(51.2282941673079,4.63965493147527,330.877040454146));
#70188=CARTESIAN_POINT('Ctrl Pts',(50.9500561330343,-0.95630113482762,328.867245199796));
#70189=CARTESIAN_POINT('Ctrl Pts',(50.67181809876,-5.67467376468082,332.485388506279));
#70190=CARTESIAN_POINT('Ctrl Pts',(50.3935800644862,-5.1854820387339,338.411153664947));
#70191=CARTESIAN_POINT('Ctrl Pts',(50.1153420302121,0.0623500165696838,
341.206553453837));
#70192=CARTESIAN_POINT('Ctrl Pts',(49.8371039959383,5.25296438195201,338.306290746721));
#70193=CARTESIAN_POINT('Ctrl Pts',(49.5588659616644,5.62301086764414,332.371893822109));
#70194=CARTESIAN_POINT('Ctrl Pts',(49.2806279273904,0.832903275603628,328.849271146165));
#70195=CARTESIAN_POINT('Ctrl Pts',(49.0023898931164,-4.72154735882616,330.971081554776));
#70196=CARTESIAN_POINT('Ctrl Pts',(48.7241518588426,-5.94310367198592,336.790170953829));
#70197=CARTESIAN_POINT('Ctrl Pts',(48.4459138245685,-1.71076146543087,340.966446891435));
#70198=CARTESIAN_POINT('Ctrl Pts',(48.1676757902947,4.09152128715226,339.667402581381));
#70199=CARTESIAN_POINT('Ctrl Pts',(47.8894377560206,6.13907534527108,334.085151813145));
#70200=CARTESIAN_POINT('Ctrl Pts',(47.611199721747,2.5528905716382,329.342443722848));
#70201=CARTESIAN_POINT('Ctrl Pts',(47.3329616874728,-3.37604419898399,329.7915915227));
#70202=CARTESIAN_POINT('Ctrl Pts',(47.0547236531989,-6.20683303852926,335.020418906187));
#70203=CARTESIAN_POINT('Ctrl Pts',(46.7764856189251,-3.34170281132171,340.230508160849));
#70204=CARTESIAN_POINT('Ctrl Pts',(46.498247584651,2.59005876238313,340.640637278474));
#70205=CARTESIAN_POINT('Ctrl Pts',(46.2200095503771,6.14496163905365,335.874436821312));
#70206=CARTESIAN_POINT('Ctrl Pts',(45.9417715161031,4.06072391904974,330.305778599899));
#70207=CARTESIAN_POINT('Ctrl Pts',(45.6635334818292,-1.7499802052793,329.044938070764));
#70208=CARTESIAN_POINT('Ctrl Pts',(45.3852954475554,-5.95475332488903,333.248969977519));
#70209=CARTESIAN_POINT('Ctrl Pts',(45.1070574132813,-4.69493721026309,339.059896290744));
#70210=CARTESIAN_POINT('Ctrl Pts',(44.8288193790074,0.873353485061651,341.145115701924));
#70211=CARTESIAN_POINT('Ctrl Pts',(44.5505813447335,5.64018057782164,337.591053135208));
#70212=CARTESIAN_POINT('Ctrl Pts',(44.2723433104595,5.23109720324356,331.659219350193));
#70213=CARTESIAN_POINT('Ctrl Pts',(43.9941052761856,0.0215131361170371,
328.793170657663));
#70214=CARTESIAN_POINT('Ctrl Pts',(43.7158672419116,-5.20781321849073,331.623037639946));
#70215=CARTESIAN_POINT('Ctrl Pts',(43.4376292076377,-5.65800624968665,337.551893136167));
#70216=CARTESIAN_POINT('Ctrl Pts',(43.1593911733638,-0.915930457580677,
341.138913967208));
#70217=CARTESIAN_POINT('Ctrl Pts',(42.8811531390898,4.66668119633548,339.092344060764));
#70218=CARTESIAN_POINT('Ctrl Pts',(42.602915104816,5.96674839647658,333.290290412657));
#70219=CARTESIAN_POINT('Ctrl Pts',(42.3246770705419,1.79121866223313,329.057212017582));
#70220=CARTESIAN_POINT('Ctrl Pts',(42.0464390362682,-4.02808599999753,330.277742438566));
#70221=CARTESIAN_POINT('Ctrl Pts',(41.768201001994,-6.15087559448237,335.831818923268));
#70222=CARTESIAN_POINT('Ctrl Pts',(41.4899629677202,-2.62909744268569,340.622547459718));
#70223=CARTESIAN_POINT('Ctrl Pts',(41.2117249334461,3.305364626849,340.253547181046));
#70224=CARTESIAN_POINT('Ctrl Pts',(40.9334868991725,6.20654236542629,335.06344419656));
#70225=CARTESIAN_POINT('Ctrl Pts',(40.6552488648983,3.41206778366701,329.815119409323));
#70226=CARTESIAN_POINT('Ctrl Pts',(40.3770108306245,-2.51361104112554,329.324883011441));
#70227=CARTESIAN_POINT('Ctrl Pts',(40.0987727963505,-6.13258611431534,334.042617709367));
#70228=CARTESIAN_POINT('Ctrl Pts',(39.8205347620765,-4.12377742722061,339.638928004471));
#70229=CARTESIAN_POINT('Ctrl Pts',(39.5422967278027,1.6693609379794,340.978162540334));
#70230=CARTESIAN_POINT('Ctrl Pts',(39.2640586935287,5.9305514101228,336.83132555047));
#70231=CARTESIAN_POINT('Ctrl Pts',(38.9858206592547,4.74936238799182,331.003908133258));
#70232=CARTESIAN_POINT('Ctrl Pts',(38.7075826249808,-0.79024639712531,328.843645239938));
#70233=CARTESIAN_POINT('Ctrl Pts',(38.4293445907068,-5.60465772761824,332.332978242278));
#70234=CARTESIAN_POINT('Ctrl Pts',(38.1511065564329,-5.27575738608837,338.269797746504));
#70235=CARTESIAN_POINT('Ctrl Pts',(37.872868522159,-0.105372361396576,341.205972120898));
#70236=CARTESIAN_POINT('Ctrl Pts',(37.594630487885,5.16171132405535,338.447017479942));
#70237=CARTESIAN_POINT('Ctrl Pts',(37.3163924536112,5.69196871415593,332.524785775537));
#70238=CARTESIAN_POINT('Ctrl Pts',(37.0381544193371,0.99879042859613,328.874021630821));
#70239=CARTESIAN_POINT('Ctrl Pts',(36.7599163850632,-4.61096309116378,330.844977416206));
#70240=CARTESIAN_POINT('Ctrl Pts',(36.4816783507893,-5.98930383986636,336.628936098708));
#70241=CARTESIAN_POINT('Ctrl Pts',(36.2034403165153,-1.87134885670335,340.918044166481));
#70242=CARTESIAN_POINT('Ctrl Pts',(35.9252022822415,3.96391535119249,339.776250452865));
#70243=CARTESIAN_POINT('Ctrl Pts',(35.6469642479676,6.16155294859364,334.251362195994));
#70244=CARTESIAN_POINT('Ctrl Pts',(35.3687262136935,2.70482434944287,329.413487801986));
#70245=CARTESIAN_POINT('Ctrl Pts',(35.0904881794196,-3.23408163204968,329.702273195308));
#70246=CARTESIAN_POINT('Ctrl Pts',(34.8122501451456,-6.20511863477687,334.852704282978));
#70247=CARTESIAN_POINT('Ctrl Pts',(34.5340121108717,-3.48180985377025,340.138306476077));
#70248=CARTESIAN_POINT('Ctrl Pts',(34.2557740765978,2.43670443861214,340.70856065736));
#70249=CARTESIAN_POINT('Ctrl Pts',(33.9775360423238,6.11909103337872,336.0401529816));
#70250=CARTESIAN_POINT('Ctrl Pts',(33.69929800805,4.18607810444926,330.41721226726));
#70251=CARTESIAN_POINT('Ctrl Pts',(33.421059973776,-1.58843691452174,328.999828213418));
#70252=CARTESIAN_POINT('Ctrl Pts',(33.1428219395021,-5.90526682232657,333.088713245733));
#70253=CARTESIAN_POINT('Ctrl Pts',(32.864583905228,-4.80292052887772,338.931557921892));
#70254=CARTESIAN_POINT('Ctrl Pts',(32.5863458709542,0.706995042931406,341.166469922831));
#70255=CARTESIAN_POINT('Ctrl Pts',(32.3081078366801,5.56811169907211,337.742503492534));
#70256=CARTESIAN_POINT('Ctrl Pts',(32.0298698024063,5.31945443416831,331.801782086425));
#70257=CARTESIAN_POINT('Ctrl Pts',(31.7516317681322,0.189212350046987,328.796018053983));
#70258=CARTESIAN_POINT('Ctrl Pts',(31.4733937338585,-5.11466711494274,331.483556682778));
#70259=CARTESIAN_POINT('Ctrl Pts',(31.1951556995843,-5.72489206091239,337.39808344117));
#70260=CARTESIAN_POINT('Ctrl Pts',(30.9169176653106,-1.08146806185105,341.111924421253));
#70261=CARTESIAN_POINT('Ctrl Pts',(30.6386796310364,4.55440321512858,339.216942571809));
#70262=CARTESIAN_POINT('Ctrl Pts',(30.3604415967627,6.01076588446597,333.452134766186));
#70263=CARTESIAN_POINT('Ctrl Pts',(30.0822035624886,1.95113742038797,329.107780039181));
#70264=CARTESIAN_POINT('Ctrl Pts',(29.8039655282148,-3.89902105563896,330.170628601195));
#70265=CARTESIAN_POINT('Ctrl Pts',(29.5257274939408,-6.17110545836244,335.665320014488));
#70266=CARTESIAN_POINT('Ctrl Pts',(29.2474894596669,-2.78005746731399,340.549457070591));
#70267=CARTESIAN_POINT('Ctrl Pts',(28.9692514253929,3.16220822790757,340.340939282866));
#70268=CARTESIAN_POINT('Ctrl Pts',(28.691013391119,6.20256210649528,335.231120347389));
#70269=CARTESIAN_POINT('Ctrl Pts',(28.412775356845,3.5509162896189,329.909205680443));
#70270=CARTESIAN_POINT('Ctrl Pts',(28.1345373225713,-2.35935299480223,329.259037820555));
#70271=CARTESIAN_POINT('Ctrl Pts',(27.8562992882971,-6.10447885988647,333.877266216279));
#70272=CARTESIAN_POINT('Ctrl Pts',(27.5780612540233,-4.24761457721317,339.525810833801));
#70273=CARTESIAN_POINT('Ctrl Pts',(27.2998232197493,1.50722290828026,341.021085650003));
#70274=CARTESIAN_POINT('Ctrl Pts',(27.0215851854754,5.87890417741855,336.990899036275));
#70275=CARTESIAN_POINT('Ctrl Pts',(26.7433471512014,4.85560185542327,331.133693762579));
#70276=CARTESIAN_POINT('Ctrl Pts',(26.4651091169276,-0.62361462072805,328.824540656379));
#70277=CARTESIAN_POINT('Ctrl Pts',(26.1868710826535,-5.53054916397395,332.182515440188));
#70278=CARTESIAN_POINT('Ctrl Pts',(25.9086330483796,-5.36218037021281,338.126054218534));
#70279=CARTESIAN_POINT('Ctrl Pts',(25.6303950141058,-0.273017796359905,
341.200859181014));
#70280=CARTESIAN_POINT('Ctrl Pts',(25.3521569798317,5.06668917947642,338.585227197611));
#70281=CARTESIAN_POINT('Ctrl Pts',(25.0739189455577,5.75677027951692,332.679485132825));
#70282=CARTESIAN_POINT('Ctrl Pts',(24.7956809112839,1.1639482638348,328.903245310903));
#70283=CARTESIAN_POINT('Ctrl Pts',(24.5174428770099,-4.49701189372031,330.721907279214));
#70284=CARTESIAN_POINT('Ctrl Pts',(24.239204842736,-6.03113061219504,336.466511792845));
#70285=CARTESIAN_POINT('Ctrl Pts',(23.960966808462,-2.0305697872003,340.865320079861));
#70286=CARTESIAN_POINT('Ctrl Pts',(23.6827287741881,3.83341496034723,339.881610701572));
#70287=CARTESIAN_POINT('Ctrl Pts',(23.4044907399142,6.17953137989617,334.418119234905));
#70288=CARTESIAN_POINT('Ctrl Pts',(23.1262527056403,2.85478306184805,329.488611157822));
#70289=CARTESIAN_POINT('Ctrl Pts',(22.8480146713663,-3.0897575355291,329.616823273238));
#70290=CARTESIAN_POINT('Ctrl Pts',(22.5697766370923,-6.19887324729767,334.685097215247));
#70291=CARTESIAN_POINT('Ctrl Pts',(22.2915386028184,-3.61937447524032,340.042352794865));
#70292=CARTESIAN_POINT('Ctrl Pts',(22.0133005685444,2.28157083086538,340.772315639642));
#70293=CARTESIAN_POINT('Ctrl Pts',(21.7350625342706,6.08875226141619,336.205109621158));
#70294=CARTESIAN_POINT('Ctrl Pts',(21.4568244999966,4.30837561150147,330.531992290727));
#70295=CARTESIAN_POINT('Ctrl Pts',(21.1785864657227,-1.4257337455679,328.95909968741));
#70296=CARTESIAN_POINT('Ctrl Pts',(20.9003484314487,-5.85146828812547,332.929852137414));
#70297=CARTESIAN_POINT('Ctrl Pts',(20.6221103971749,-4.90739675020082,338.800348725582));
#70298=CARTESIAN_POINT('Ctrl Pts',(20.3438723629008,0.540120352325815,341.183321381337));
#70299=CARTESIAN_POINT('Ctrl Pts',(20.0656343286271,5.49197697968639,337.891951271115));
#70300=CARTESIAN_POINT('Ctrl Pts',(19.787396294353,5.40392739423611,331.94668016452));
#70301=CARTESIAN_POINT('Ctrl Pts',(19.5091582600792,0.356773400932937,328.803395604019));
#70302=CARTESIAN_POINT('Ctrl Pts',(19.2309202258051,-5.01778627643961,331.346643435978));
#70303=CARTESIAN_POINT('Ctrl Pts',(18.9526821915312,-5.78759755032758,337.242522663286));
#70304=CARTESIAN_POINT('Ctrl Pts',(18.6744441572573,-1.24621597707973,341.080471942077));
#70305=CARTESIAN_POINT('Ctrl Pts',(18.3962061229834,4.43879960421651,339.338461867242));
#70306=CARTESIAN_POINT('Ctrl Pts',(18.1179680887094,6.05039430529802,333.615109372432));
#70307=CARTESIAN_POINT('Ctrl Pts',(17.8397300544354,2.1096314560811,329.162650565589));
#70308=CARTESIAN_POINT('Ctrl Pts',(17.5614920201615,-3.76710904227219,330.067041175568));
#70309=CARTESIAN_POINT('Ctrl Pts',(17.2832539858876,-6.18682917497063,335.498335288377));
#70310=CARTESIAN_POINT('Ctrl Pts',(17.0050159516137,-2.92898749124742,340.472314462457));
#70311=CARTESIAN_POINT('Ctrl Pts',(16.7267779173396,3.01674278140895,340.424431425571));
#70312=CARTESIAN_POINT('Ctrl Pts',(16.4485398830658,6.19405273061698,335.398627733914));
#70313=CARTESIAN_POINT('Ctrl Pts',(16.1703018487919,3.68717191300587,330.00700925458));
#70314=CARTESIAN_POINT('Ctrl Pts',(15.8920638145178,-2.20337214660178,329.197384685895));
#70315=CARTESIAN_POINT('Ctrl Pts',(15.6138257802439,-6.07191410899394,333.712734544503));
#70316=CARTESIAN_POINT('Ctrl Pts',(15.3355877459701,-4.36835011486507,339.409388911613));
#70317=CARTESIAN_POINT('Ctrl Pts',(15.057349711696,1.3439843029285,341.059612157009));
#70318=CARTESIAN_POINT('Ctrl Pts',(14.7791116774222,5.82296416310975,337.149018765648));
#70319=CARTESIAN_POINT('Ctrl Pts',(14.5008736431483,4.95829575759767,331.266302572513));
#70320=CARTESIAN_POINT('Ctrl Pts',(14.2226356088742,-0.456527480302993,
328.809945399307));
#70321=CARTESIAN_POINT('Ctrl Pts',(13.9443975746004,-5.4524021879272,332.034109968084));
#70322=CARTESIAN_POINT('Ctrl Pts',(13.6661595403263,-5.44468788489596,337.980028042719));
#70323=CARTESIAN_POINT('Ctrl Pts',(13.3879215060525,-0.440463873581898,
341.191218367626));
#70324=CARTESIAN_POINT('Ctrl Pts',(13.1096834717786,4.96796733370652,338.720818978924));
#70325=CARTESIAN_POINT('Ctrl Pts',(12.8314454375045,5.81736824512882,332.835878932219));
#70326=CARTESIAN_POINT('Ctrl Pts',(12.5532074032307,1.32825618372396,328.936920847501));
#70327=CARTESIAN_POINT('Ctrl Pts',(12.2749693689567,-4.37977697531212,330.601961009263));
#70328=CARTESIAN_POINT('Ctrl Pts',(11.9967313346828,-6.0685534441121,336.303016639511));
#70329=CARTESIAN_POINT('Ctrl Pts',(11.7184933004087,-2.18830799913804,340.808313129084));
#70330=CARTESIAN_POINT('Ctrl Pts',(11.4402552661348,3.70011541650439,339.983406396494));
#70331=CARTESIAN_POINT('Ctrl Pts',(11.162017231861,6.19299749171987,334.585301157778));
#70332=CARTESIAN_POINT('Ctrl Pts',(10.883779197587,3.00265724584708,329.567758946434));
#70333=CARTESIAN_POINT('Ctrl Pts',(10.6055411633131,-2.94317736486522,329.535304130909));
#70334=CARTESIAN_POINT('Ctrl Pts',(10.327303129039,-6.18810130459427,334.517720129862));
#70335=CARTESIAN_POINT('Ctrl Pts',(10.0490650947653,-3.75429647493768,339.942717107111));
#70336=CARTESIAN_POINT('Ctrl Pts',(9.77082706049122,2.12477168806704,340.831855814069));
#70337=CARTESIAN_POINT('Ctrl Pts',(9.49258902621731,6.05396658870994,336.36918601904));
#70338=CARTESIAN_POINT('Ctrl Pts',(9.21435099194333,4.42752881490187,330.650035366585));
#70339=CARTESIAN_POINT('Ctrl Pts',(8.93611295766945,-1.26199266991894,328.922781272086));
#70340=CARTESIAN_POINT('Ctrl Pts',(8.65787492339546,-5.79339102894519,332.772504467024));
#70341=CARTESIAN_POINT('Ctrl Pts',(8.37963688912154,-5.00830087154158,338.666361085838));
#70342=CARTESIAN_POINT('Ctrl Pts',(8.1013988548476,0.372872575477468,341.1956642397));
#70343=CARTESIAN_POINT('Ctrl Pts',(7.82316082057367,5.4117917753666,338.039275132633));
#70344=CARTESIAN_POINT('Ctrl Pts',(7.54492278629972,5.48453037873516,332.093830837367));
#70345=CARTESIAN_POINT('Ctrl Pts',(7.26668475202578,0.52393047366258,328.815254383241));
#70346=CARTESIAN_POINT('Ctrl Pts',(6.98844671775185,-4.91697055337583,331.212480081138));
#70347=CARTESIAN_POINT('Ctrl Pts',(6.71020868347791,-5.84658848615386,337.085169169869));
#70348=CARTESIAN_POINT('Ctrl Pts',(6.43197064920395,-1.40908752098961,341.044872581102));
#70349=CARTESIAN_POINT('Ctrl Pts',(6.15373261493005,4.31812627429368,339.456259878022));
#70350=CARTESIAN_POINT('Ctrl Pts',(5.87549458065607,6.08908817465391,333.780139476516));
#70351=CARTESIAN_POINT('Ctrl Pts',(5.59725654638217,2.25975513930278,329.219816699493));
#70352=CARTESIAN_POINT('Ctrl Pts',(5.36539151782054,-2.6379404393598,329.845549066121));
#70353=CARTESIAN_POINT('Ctrl Pts',(5.17989949497124,-4.93068027107053,332.649384088804));
#70354=CARTESIAN_POINT('Ctrl Pts',(5.08715348354661,-5.28802671673104,334.407219181606));
#70355=CARTESIAN_POINT('Ctrl Pts',(5.04078047783429,-5.24142383043492,335.279901837379));
#70356=CARTESIAN_POINT('Ctrl Pts',(185.423459434742,-2.43876419493702,329.976059081413));
#70357=CARTESIAN_POINT('Ctrl Pts',(185.377084700732,-3.27526837515656,330.38212144629));
#70358=CARTESIAN_POINT('Ctrl Pts',(185.284336961008,-4.72780408125933,331.620144579983));
#70359=CARTESIAN_POINT('Ctrl Pts',(185.098843209861,-6.15736430490123,335.198742348302));
#70360=CARTESIAN_POINT('Ctrl Pts',(184.866978181299,-4.21750050188893,340.080738627298));
#70361=CARTESIAN_POINT('Ctrl Pts',(184.588740147026,2.00032595301521,341.297165656258));
#70362=CARTESIAN_POINT('Ctrl Pts',(184.31050211275,6.37268333620086,336.725085768952));
#70363=CARTESIAN_POINT('Ctrl Pts',(184.032264078478,4.90203688689787,330.574908170056));
#70364=CARTESIAN_POINT('Ctrl Pts',(183.754026044204,-1.06983530224133,328.482947982007));
#70365=CARTESIAN_POINT('Ctrl Pts',(183.47578800993,-6.0585072503333,332.372977788209));
#70366=CARTESIAN_POINT('Ctrl Pts',(183.197549975656,-5.4881327455372,338.673052515815));
#70367=CARTESIAN_POINT('Ctrl Pts',(182.919311941382,0.119020659026097,341.60281017205));
#70368=CARTESIAN_POINT('Ctrl Pts',(182.641073907107,5.61673846577441,338.473060374359));
#70369=CARTESIAN_POINT('Ctrl Pts',(182.362835872834,5.9601706119106,332.156243440002));
#70370=CARTESIAN_POINT('Ctrl Pts',(182.084597838559,0.833982670938808,328.449042143749));
#70371=CARTESIAN_POINT('Ctrl Pts',(181.806359804286,-5.05750735223084,330.753588782418));
#70372=CARTESIAN_POINT('Ctrl Pts',(181.528121770012,-6.30781421230692,336.954988111478));
#70373=CARTESIAN_POINT('Ctrl Pts',(181.249883735738,-1.76952423629996,341.362332289535));
#70374=CARTESIAN_POINT('Ctrl Pts',(180.971645701464,4.39262733330804,339.931053487594));
#70375=CARTESIAN_POINT('Ctrl Pts',(180.69340766719,6.52373211271479,333.974622089771));
#70376=CARTESIAN_POINT('Ctrl Pts',(180.415169632916,2.66810290978665,328.959163590617));
#70377=CARTESIAN_POINT('Ctrl Pts',(180.136931598643,-3.63600425714706,329.487292176997));
#70378=CARTESIAN_POINT('Ctrl Pts',(179.858693564369,-6.60340435279722,335.074351007501));
#70379=CARTESIAN_POINT('Ctrl Pts',(179.580455530094,-3.51095754499201,340.593179205234));
#70380=CARTESIAN_POINT('Ctrl Pts',(179.302217495821,2.80344307694077,340.97922930121));
#70381=CARTESIAN_POINT('Ctrl Pts',(179.023979461547,6.54516542060559,335.878228973867));
#70382=CARTESIAN_POINT('Ctrl Pts',(178.745741427273,4.28048603530062,329.971290851712));
#70383=CARTESIAN_POINT('Ctrl Pts',(178.467503392998,-1.91233218939032,328.679124906215));
#70384=CARTESIAN_POINT('Ctrl Pts',(178.189265358724,-6.35023139797826,333.187532730431));
#70385=CARTESIAN_POINT('Ctrl Pts',(177.911027324451,-4.96061697760105,339.359215020136));
#70386=CARTESIAN_POINT('Ctrl Pts',(177.632789290177,0.981282422255545,341.530510025558));
#70387=CARTESIAN_POINT('Ctrl Pts',(177.354551255903,6.02267342811975,337.708852371867));
#70388=CARTESIAN_POINT('Ctrl Pts',(177.07631322163,5.53714592287347,331.401320878489));
#70389=CARTESIAN_POINT('Ctrl Pts',(176.798075187355,-0.029738667315452,
328.396244098834));
#70390=CARTESIAN_POINT('Ctrl Pts',(176.51983715308,-5.56933252163025,331.451336638226));
#70391=CARTESIAN_POINT('Ctrl Pts',(176.241599118807,-5.99803212396333,337.762985166628));
#70392=CARTESIAN_POINT('Ctrl Pts',(175.963361084532,-0.922426176994555,
341.539082989158));
#70393=CARTESIAN_POINT('Ctrl Pts',(175.685123050259,4.99967665764068,339.314360869272));
#70394=CARTESIAN_POINT('Ctrl Pts',(175.406885015986,6.33365001865148,333.130413459503));
#70395=CARTESIAN_POINT('Ctrl Pts',(175.128646981712,1.85532624207433,328.662158022904));
#70396=CARTESIAN_POINT('Ctrl Pts',(174.850408947438,-4.32560304228792,330.010046622287));
#70397=CARTESIAN_POINT('Ctrl Pts',(174.572170913164,-6.53699026053673,335.937141784809));
#70398=CARTESIAN_POINT('Ctrl Pts',(174.29393287889,-2.74947800251017,341.004235763601));
#70399=CARTESIAN_POINT('Ctrl Pts',(174.015694844616,3.56118963619175,340.561331204512));
#70400=CARTESIAN_POINT('Ctrl Pts',(173.737456810342,6.60380610883307,335.014875084156));
#70401=CARTESIAN_POINT('Ctrl Pts',(173.459218776068,3.58620718741687,329.454768318626));
#70402=CARTESIAN_POINT('Ctrl Pts',(173.180980741794,-2.72240113756057,328.983438819608));
#70403=CARTESIAN_POINT('Ctrl Pts',(172.90274270752,-6.53270212117353,334.033418711538));
#70404=CARTESIAN_POINT('Ctrl Pts',(172.624504673246,-4.34803879071085,339.970415985173));
#70405=CARTESIAN_POINT('Ctrl Pts',(172.346266638971,1.82675556103984,341.346135872435));
#70406=CARTESIAN_POINT('Ctrl Pts',(172.068028604698,6.32516329729214,336.898100538374));
#70407=CARTESIAN_POINT('Ctrl Pts',(171.789790570425,5.0190620348767,330.708206356167));
#70408=CARTESIAN_POINT('Ctrl Pts',(171.51155253615,-0.892958375710887,328.456827854133));
#70409=CARTESIAN_POINT('Ctrl Pts',(171.233314501877,-5.98552406495261,332.2100218533));
#70410=CARTESIAN_POINT('Ctrl Pts',(170.955076467602,-5.58526266597773,338.523537617683));
#70411=CARTESIAN_POINT('Ctrl Pts',(170.676838433328,-0.0594881567769249,
341.603554917649));
#70412=CARTESIAN_POINT('Ctrl Pts',(170.398600399054,5.52087775585432,338.623587337999));
#70413=CARTESIAN_POINT('Ctrl Pts',(170.120362364781,6.03481563996016,332.318307142329));
#70414=CARTESIAN_POINT('Ctrl Pts',(169.842124330507,1.01069228500742,328.473976900422));
#70415=CARTESIAN_POINT('Ctrl Pts',(169.563886296233,-4.94092846210296,330.618481733055));
#70416=CARTESIAN_POINT('Ctrl Pts',(169.285648261959,-6.35833208752602,336.783841208159));
#70417=CARTESIAN_POINT('Ctrl Pts',(169.007410227685,-1.94078820505423,341.312195935989));
#70418=CARTESIAN_POINT('Ctrl Pts',(168.729172193411,4.25778836720887,340.04794162122));
#70419=CARTESIAN_POINT('Ctrl Pts',(168.450934159137,6.54905539973767,334.151265788155));
#70420=CARTESIAN_POINT('Ctrl Pts',(168.172696124863,2.83035095582653,329.033460814003));
#70421=CARTESIAN_POINT('Ctrl Pts',(167.894458090589,-3.48572478433498,329.391060784866));
#70422=CARTESIAN_POINT('Ctrl Pts',(167.616220056316,-6.60300233912578,334.895901485651));
#70423=CARTESIAN_POINT('Ctrl Pts',(167.337982022041,-3.66080210745563,340.496271856563));
#70424=CARTESIAN_POINT('Ctrl Pts',(167.059743987767,2.64086218487603,341.052794669545));
#70425=CARTESIAN_POINT('Ctrl Pts',(166.781505953493,6.51904622920892,336.054757153391));
#70426=CARTESIAN_POINT('Ctrl Pts',(166.503267919219,4.41479776996139,330.088784565758));
#70427=CARTESIAN_POINT('Ctrl Pts',(166.225029884946,-1.74084544047143,328.62976189271));
#70428=CARTESIAN_POINT('Ctrl Pts',(165.946791850672,-6.2989404850202,333.01661270616));
#70429=CARTESIAN_POINT('Ctrl Pts',(165.668553816398,-5.07659081867508,339.22358876442));
#70430=CARTESIAN_POINT('Ctrl Pts',(165.390315782124,0.804471311610485,341.55463975364));
#70431=CARTESIAN_POINT('Ctrl Pts',(165.11207774785,5.94728199320819,337.870594587267));
#70432=CARTESIAN_POINT('Ctrl Pts',(164.833839713576,5.63235977137711,331.552247138068));
#70433=CARTESIAN_POINT('Ctrl Pts',(164.555601679302,0.148704120847259,328.397851601514));
#70434=CARTESIAN_POINT('Ctrl Pts',(164.277363645027,-5.47141510651493,331.3021502027));
#70435=CARTESIAN_POINT('Ctrl Pts',(163.999125610754,-6.07049744858296,337.599910982695));
#70436=CARTESIAN_POINT('Ctrl Pts',(163.72088757648,-1.09877388248187,341.511771828493));
#70437=CARTESIAN_POINT('Ctrl Pts',(163.442649542206,4.8812782576969,339.447875780879));
#70438=CARTESIAN_POINT('Ctrl Pts',(163.164411507932,6.38185338833623,333.30222977969));
#70439=CARTESIAN_POINT('Ctrl Pts',(162.886173473658,2.02589586050099,328.714602450632));
#70440=CARTESIAN_POINT('Ctrl Pts',(162.607935439384,-4.18919639634211,329.894991680314));
#70441=CARTESIAN_POINT('Ctrl Pts',(162.329697405111,-6.5599249526995,335.760171695172));
#70442=CARTESIAN_POINT('Ctrl Pts',(162.051459370836,-2.91070720429822,340.927753365486));
#70443=CARTESIAN_POINT('Ctrl Pts',(161.773221336563,3.40962358351962,340.655523265791));
#70444=CARTESIAN_POINT('Ctrl Pts',(161.494983302289,6.60099313470312,335.193302940465));
#70445=CARTESIAN_POINT('Ctrl Pts',(161.216745268015,3.73472871666854,329.553691359822));
#70446=CARTESIAN_POINT('Ctrl Pts',(160.938507233741,-2.55884112014728,328.912076830886));
#70447=CARTESIAN_POINT('Ctrl Pts',(160.660269199467,-6.50420022943695,333.857259536647));
#70448=CARTESIAN_POINT('Ctrl Pts',(160.382031165193,-4.48075079001036,339.851118298805));
#70449=CARTESIAN_POINT('Ctrl Pts',(160.103793130919,1.65461751363549,341.393177400539));
#70450=CARTESIAN_POINT('Ctrl Pts',(159.825555096645,6.27156774713252,337.068311964941));
#70451=CARTESIAN_POINT('Ctrl Pts',(159.547317062371,5.13319282727425,330.845387167351));
#70452=CARTESIAN_POINT('Ctrl Pts',(159.269079028097,-0.715837384371603,
328.435089244298));
#70453=CARTESIAN_POINT('Ctrl Pts',(158.990840993823,-5.90795419412213,332.049313023829));
#70454=CARTESIAN_POINT('Ctrl Pts',(158.712602959549,-5.67842864118778,338.371338689323));
#70455=CARTESIAN_POINT('Ctrl Pts',(158.434364925275,-0.237892937704753,
341.599536600503));
#70456=CARTESIAN_POINT('Ctrl Pts',(158.156126891001,5.42095360341592,338.771437182402));
#70457=CARTESIAN_POINT('Ctrl Pts',(157.877888856727,6.10507103582582,332.482345528331));
#70458=CARTESIAN_POINT('Ctrl Pts',(157.599650822454,1.18665488935917,328.503668222393));
#70459=CARTESIAN_POINT('Ctrl Pts',(157.321412788179,-4.82073693407496,330.486578703064));
#70460=CARTESIAN_POINT('Ctrl Pts',(157.043174753906,-6.40420962706899,336.611389289944));
#70461=CARTESIAN_POINT('Ctrl Pts',(156.764936719632,-2.11063367128099,341.257451709509));
#70462=CARTESIAN_POINT('Ctrl Pts',(156.486698685358,4.11983965173963,340.161143055094));
#70463=CARTESIAN_POINT('Ctrl Pts',(156.208460651084,6.56959693509242,334.328529597365));
#70464=CARTESIAN_POINT('Ctrl Pts',(155.93022261681,2.99053207820273,329.112114617248));
#70465=CARTESIAN_POINT('Ctrl Pts',(155.651984582536,-3.33289992667248,329.298925147836));
#70466=CARTESIAN_POINT('Ctrl Pts',(155.373746548262,-6.59777886236264,334.717527922529));
#70467=CARTESIAN_POINT('Ctrl Pts',(155.095508513988,-3.80797351911897,340.395351153436));
#70468=CARTESIAN_POINT('Ctrl Pts',(154.817270479714,2.47635291702316,341.121940266087));
#70469=CARTESIAN_POINT('Ctrl Pts',(154.53903244544,6.48816683212228,336.230515156241));
#70470=CARTESIAN_POINT('Ctrl Pts',(154.260794411166,4.54588581056825,330.209864449886));
#70471=CARTESIAN_POINT('Ctrl Pts',(153.982556376892,-1.56808752217966,328.585050435586));
#70472=CARTESIAN_POINT('Ctrl Pts',(153.704318342618,-6.24305008075718,332.847140952048));
#70473=CARTESIAN_POINT('Ctrl Pts',(153.426080308345,-5.18885772749205,339.084878440669));
#70474=CARTESIAN_POINT('Ctrl Pts',(153.14784227407,0.62707277487803,341.573983276994));
#70475=CARTESIAN_POINT('Ctrl Pts',(152.869604239797,5.86754784732152,338.030240691857));
#70476=CARTESIAN_POINT('Ctrl Pts',(152.591366205523,5.72346086514233,331.705690950081));
#70477=CARTESIAN_POINT('Ctrl Pts',(152.313128171249,0.327038325165903,328.404279999495));
#70478=CARTESIAN_POINT('Ctrl Pts',(152.034890136975,-5.36950245873749,331.155663940705));
#70479=CARTESIAN_POINT('Ctrl Pts',(151.756652102701,-6.13853008998387,337.434938341222));
#70480=CARTESIAN_POINT('Ctrl Pts',(151.478414068427,-1.27431926220765,341.479705765631));
#70481=CARTESIAN_POINT('Ctrl Pts',(151.200176034153,4.75931554357499,339.578142849221));
#70482=CARTESIAN_POINT('Ctrl Pts',(150.921937999879,6.4253967224012,333.475285813359));
#70483=CARTESIAN_POINT('Ctrl Pts',(150.643699965605,2.19498616778012,328.771636481832));
#70484=CARTESIAN_POINT('Ctrl Pts',(150.365461931331,-4.04973079507009,329.783664420433));
#70485=CARTESIAN_POINT('Ctrl Pts',(150.087223897057,-6.57806958121304,335.582646527415));
#70486=CARTESIAN_POINT('Ctrl Pts',(149.808985862783,-3.06981100482464,340.846942516038));
#70487=CARTESIAN_POINT('Ctrl Pts',(149.53074782851,3.25556782035516,340.745585658421));
#70488=CARTESIAN_POINT('Ctrl Pts',(149.252509794235,6.5933601088973,335.371589646777));
#70489=CARTESIAN_POINT('Ctrl Pts',(148.974271759962,3.88052314334006,329.656591300939));
#70490=CARTESIAN_POINT('Ctrl Pts',(148.696033725687,-2.39341263443264,328.845160249647));
#70491=CARTESIAN_POINT('Ctrl Pts',(148.417795691414,-6.47094896429908,333.681934791966));
#70492=CARTESIAN_POINT('Ctrl Pts',(148.13955765714,-4.61019094067841,339.72827832109));
#70493=CARTESIAN_POINT('Ctrl Pts',(147.861319622866,1.4812712628961,341.435550624221));
#70494=CARTESIAN_POINT('Ctrl Pts',(147.583081588592,6.21339269203886,337.237013108077));
#70495=CARTESIAN_POINT('Ctrl Pts',(147.304843554318,5.24357535722337,330.98560168091));
#70496=CARTESIAN_POINT('Ctrl Pts',(147.026605520044,-0.538193687870606,
328.418144338751));
#70497=CARTESIAN_POINT('Ctrl Pts',(146.74836748577,-5.82607032933153,331.890758788889));
#70498=CARTESIAN_POINT('Ctrl Pts',(146.470129451496,-5.76744822222202,338.216678006139));
#70499=CARTESIAN_POINT('Ctrl Pts',(146.191891417222,-0.416124008975574,
341.590699295245));
#70500=CARTESIAN_POINT('Ctrl Pts',(145.913653382948,5.31707106532745,338.916533119666));
#70501=CARTESIAN_POINT('Ctrl Pts',(145.635415348674,6.17086850281975,332.648222308105));
#70502=CARTESIAN_POINT('Ctrl Pts',(145.3571773144,1.36175099714417,328.538103172212));
#70503=CARTESIAN_POINT('Ctrl Pts',(145.078939280126,-4.69702529919884,330.357971377741));
#70504=CARTESIAN_POINT('Ctrl Pts',(144.800701245853,-6.44541080644686,336.437760733685));
#70505=CARTESIAN_POINT('Ctrl Pts',(144.522463211578,-2.27893795072618,341.198138285642));
#70506=CARTESIAN_POINT('Ctrl Pts',(144.244225177305,3.97888262530681,340.270575817235));
#70507=CARTESIAN_POINT('Ctrl Pts',(143.96598714303,6.58534134430714,334.506283714924));
#70508=CARTESIAN_POINT('Ctrl Pts',(143.687749108757,3.14852951111574,329.195067760186));
#70509=CARTESIAN_POINT('Ctrl Pts',(143.409511074483,-3.17764138220717,329.210952441267));
#70510=CARTESIAN_POINT('Ctrl Pts',(143.131273040209,-6.58773768098847,334.539360620795));
#70511=CARTESIAN_POINT('Ctrl Pts',(142.853035005935,-3.95236434477544,340.290490759593));
#70512=CARTESIAN_POINT('Ctrl Pts',(142.574796971661,2.31003541383591,341.186615615829));
#70513=CARTESIAN_POINT('Ctrl Pts',(142.296558937387,6.45254976923686,336.405374635716));
#70514=CARTESIAN_POINT('Ctrl Pts',(142.018320903113,4.67365444088762,330.334442095702));
#70515=CARTESIAN_POINT('Ctrl Pts',(141.740082868839,-1.39418458483772,328.545023180941));
#70516=CARTESIAN_POINT('Ctrl Pts',(141.461844834565,-6.18260099518822,332.679241217728));
#70517=CARTESIAN_POINT('Ctrl Pts',(141.183606800291,-5.29733572729561,338.943185334664));
#70518=CARTESIAN_POINT('Ctrl Pts',(140.905368766017,0.449216348989023,341.588526471297));
#70519=CARTESIAN_POINT('Ctrl Pts',(140.627130731743,5.78352921222887,338.187674111713));
#70520=CARTESIAN_POINT('Ctrl Pts',(140.34889269747,5.81038268215753,331.861540269802));
#70521=CARTESIAN_POINT('Ctrl Pts',(140.070654663195,0.505133725778029,328.415524598705));
#70522=CARTESIAN_POINT('Ctrl Pts',(139.792416628922,-5.26366899498638,331.011984816678));
#70523=CARTESIAN_POINT('Ctrl Pts',(139.514178594648,-6.20208037067882,337.268187705379));
#70524=CARTESIAN_POINT('Ctrl Pts',(139.235940560374,-1.4489341327555,341.44290821525));
#70525=CARTESIAN_POINT('Ctrl Pts',(138.9577025261,4.63387757256473,339.705066953155));
#70526=CARTESIAN_POINT('Ctrl Pts',(138.679464491826,6.46424822546323,333.649455194825));
#70527=CARTESIAN_POINT('Ctrl Pts',(138.401226457552,2.36247369400165,328.833218470195));
#70528=CARTESIAN_POINT('Ctrl Pts',(138.122988423278,-3.90730807639073,329.676146133921));
#70529=CARTESIAN_POINT('Ctrl Pts',(137.844750389004,-6.59141089685199,335.404695910594));
#70530=CARTESIAN_POINT('Ctrl Pts',(137.56651235473,-3.22667322633757,340.761862223415));
#70531=CARTESIAN_POINT('Ctrl Pts',(137.288274320456,3.09913483836811,340.831452618757));
#70532=CARTESIAN_POINT('Ctrl Pts',(137.010036286182,6.58091260505858,335.549605017963));
#70533=CARTESIAN_POINT('Ctrl Pts',(136.731798251908,4.02348400819764,329.763393004342));
#70534=CARTESIAN_POINT('Ctrl Pts',(136.453560217634,-2.22623647645968,328.782737938444));
#70535=CARTESIAN_POINT('Ctrl Pts',(136.17532218336,-6.43297260586646,333.507572499797));
#70536=CARTESIAN_POINT('Ctrl Pts',(135.897084149086,-4.73626472538963,339.601985749893));
#70537=CARTESIAN_POINT('Ctrl Pts',(135.618846114812,1.30684338642453,341.47322460251));
#70538=CARTESIAN_POINT('Ctrl Pts',(135.340608080539,6.15068061149365,337.404080782043));
#70539=CARTESIAN_POINT('Ctrl Pts',(135.062370046264,5.35012902329207,331.128747512067));
#70540=CARTESIAN_POINT('Ctrl Pts',(134.784132011991,-0.360157001809702,
328.406005510677));
#70541=CARTESIAN_POINT('Ctrl Pts',(134.505893977717,-5.73993226225935,331.734474924936));
#70542=CARTESIAN_POINT('Ctrl Pts',(134.227655943443,-5.8522564068949,338.059668501513));
#70543=CARTESIAN_POINT('Ctrl Pts',(133.949417909169,-0.594051226085983,
341.577049454882));
#70544=CARTESIAN_POINT('Ctrl Pts',(133.671179874895,5.20930599672032,339.058769200599));
#70545=CARTESIAN_POINT('Ctrl Pts',(133.392941840621,6.23215999556685,332.815816358259));
#70546=CARTESIAN_POINT('Ctrl Pts',(133.114703806347,1.53585275301256,328.577256605449));
#70547=CARTESIAN_POINT('Ctrl Pts',(132.836465772073,-4.56988389183189,330.23275366628));
#70548=CARTESIAN_POINT('Ctrl Pts',(132.558227737799,-6.48190554051795,336.263082323126));
#70549=CARTESIAN_POINT('Ctrl Pts',(132.279989703525,-2.44557814743964,341.134298975103));
#70550=CARTESIAN_POINT('Ctrl Pts',(132.001751669251,3.83502021486974,340.376159999734));
#70551=CARTESIAN_POINT('Ctrl Pts',(131.723513634977,6.59627713079875,334.684398344598));
#70552=CARTESIAN_POINT('Ctrl Pts',(131.445275600703,3.3042278846846,329.282259670354));
#70553=CARTESIAN_POINT('Ctrl Pts',(131.16703756643,-3.02006252088097,329.127206902916));
#70554=CARTESIAN_POINT('Ctrl Pts',(130.888799532155,-6.57288612708381,334.361529678387));
#70555=CARTESIAN_POINT('Ctrl Pts',(130.610561497882,-4.09386915010205,340.181767244197));
#70556=CARTESIAN_POINT('Ctrl Pts',(130.332323463607,2.14203112051876,341.246773492765));
#70557=CARTESIAN_POINT('Ctrl Pts',(130.054085429334,6.41222104816702,336.579207909249));
#70558=CARTESIAN_POINT('Ctrl Pts',(129.77584739506,4.79801036413993,330.462426536485));
#70559=CARTESIAN_POINT('Ctrl Pts',(129.497609360786,-1.21926361254148,328.509709356714));
#70560=CARTESIAN_POINT('Ctrl Pts',(129.219371326512,-6.117637368295,332.513036103753));
#70561=CARTESIAN_POINT('Ctrl Pts',(128.941133292238,-5.40194560734373,338.798612910852));
#70562=CARTESIAN_POINT('Ctrl Pts',(128.662895257964,0.271031904880399,341.598258717095));
#70563=CARTESIAN_POINT('Ctrl Pts',(128.38465722369,5.69528743842016,338.342779888799));
#70564=CARTESIAN_POINT('Ctrl Pts',(128.106419189416,5.89306175202652,332.019681295903));
#70565=CARTESIAN_POINT('Ctrl Pts',(127.828181155142,0.68286027724717,328.431577188323));
#70566=CARTESIAN_POINT('Ctrl Pts',(127.549943120868,-5.15399199496077,330.871217745259));
#70567=CARTESIAN_POINT('Ctrl Pts',(127.271705086593,-6.26110188619041,337.099780836643));
#70568=CARTESIAN_POINT('Ctrl Pts',(126.99346705232,-1.62249099017548,341.401406046955));
#70569=CARTESIAN_POINT('Ctrl Pts',(126.715229018046,4.50505593959574,339.828555412574));
#70570=CARTESIAN_POINT('Ctrl Pts',(126.436990983773,6.49837952811661,333.824610745435));
#70571=CARTESIAN_POINT('Ctrl Pts',(126.158752949498,2.52823613960948,328.899303448494));
#70572=CARTESIAN_POINT('Ctrl Pts',(125.880514915225,-3.76203223751303,329.572515330735));
#70573=CARTESIAN_POINT('Ctrl Pts',(125.602276880951,-6.59993915777462,335.226449784418));
#70574=CARTESIAN_POINT('Ctrl Pts',(125.324038846677,-3.38117932788874,340.672574613335));
#70575=CARTESIAN_POINT('Ctrl Pts',(125.045800812403,2.94043886507557,340.913061446657));
#70576=CARTESIAN_POINT('Ctrl Pts',(124.767562778129,6.56365971236653,335.727219067027));
#70577=CARTESIAN_POINT('Ctrl Pts',(124.489324743855,4.16350692107729,329.874018483321));
#70578=CARTESIAN_POINT('Ctrl Pts',(124.211086709581,-2.05743471842317,328.72485547811));
#70579=CARTESIAN_POINT('Ctrl Pts',(123.932848675307,-6.39029888451334,333.334299979654));
#70580=CARTESIAN_POINT('Ctrl Pts',(123.654610641033,-4.85888008494255,339.472332804179));
#70581=CARTESIAN_POINT('Ctrl Pts',(123.376372606759,1.13146125162753,341.506171825833));
#70582=CARTESIAN_POINT('Ctrl Pts',(123.098134572485,6.08347729791972,337.569392993857));
#70583=CARTESIAN_POINT('Ctrl Pts',(122.819896538211,5.45277601988872,331.274720135599));
#70584=CARTESIAN_POINT('Ctrl Pts',(122.541658503937,-0.181857328751986,
328.39868162386));
#70585=CARTESIAN_POINT('Ctrl Pts',(122.263420469663,-5.64960289100673,331.580575550605));
#70586=CARTESIAN_POINT('Ctrl Pts',(121.985182435389,-5.93279126818671,337.900424823939));
#70587=CARTESIAN_POINT('Ctrl Pts',(121.706944401116,-0.771544666407324,
341.558597046544));
#70588=CARTESIAN_POINT('Ctrl Pts',(121.428706366841,5.09773708775345,339.198041564269));
#70589=CARTESIAN_POINT('Ctrl Pts',(121.150468332568,6.28890075895896,332.985005301457));
#70590=CARTESIAN_POINT('Ctrl Pts',(120.872230298294,1.70883302769088,328.621099932225));
#70591=CARTESIAN_POINT('Ctrl Pts',(120.59399226402,-4.43940555075498,330.111017002779));
#70592=CARTESIAN_POINT('Ctrl Pts',(120.315754229746,-6.51366718079151,336.087481608612));
#70593=CARTESIAN_POINT('Ctrl Pts',(120.037516195472,-2.61043258058566,341.065980393425));
#70594=CARTESIAN_POINT('Ctrl Pts',(119.759278161198,3.68835746890191,340.477818504914));
#70595=CARTESIAN_POINT('Ctrl Pts',(119.481040126924,6.60239630924522,334.862743426914));
#70596=CARTESIAN_POINT('Ctrl Pts',(119.20280209265,3.45751350780396,329.37362668013));
#70597=CARTESIAN_POINT('Ctrl Pts',(118.924564058376,-2.86027840693326,329.047749683857));
#70598=CARTESIAN_POINT('Ctrl Pts',(118.646326024102,-6.55323504526792,334.184164947638));
#70599=CARTESIAN_POINT('Ctrl Pts',(118.368087989828,-4.23238460815091,340.069259997266));
#70600=CARTESIAN_POINT('Ctrl Pts',(118.089849955554,1.97246271397175,341.302369969558));
#70601=CARTESIAN_POINT('Ctrl Pts',(117.81161192128,6.3672101169845,336.751888043614));
#70602=CARTESIAN_POINT('Ctrl Pts',(117.533373887006,4.91886277550783,330.593724317872));
#70603=CARTESIAN_POINT('Ctrl Pts',(117.255135852733,-1.04345233275681,328.479134749095));
#70604=CARTESIAN_POINT('Ctrl Pts',(116.976897818459,-6.04820663658166,332.34864697326));
#70605=CARTESIAN_POINT('Ctrl Pts',(116.698659784185,-5.50261098139925,338.651266736158));
#70606=CARTESIAN_POINT('Ctrl Pts',(116.420421749911,0.0926495530080822,
341.603172907892));
#70607=CARTESIAN_POINT('Ctrl Pts',(116.142183715637,5.60288696012516,338.495444764725));
#70608=CARTESIAN_POINT('Ctrl Pts',(115.863945681363,5.97143770241139,332.179998553651));
#70609=CARTESIAN_POINT('Ctrl Pts',(115.585707647089,0.860088203470714,328.452426046737));
#70610=CARTESIAN_POINT('Ctrl Pts',(115.307469612815,-5.04055154491398,330.7334655147));
#70611=CARTESIAN_POINT('Ctrl Pts',(115.029231578541,-6.31555153894996,336.929840705875));
#70612=CARTESIAN_POINT('Ctrl Pts',(114.750993544267,-1.79486310307947,341.355229565673));
#70613=CARTESIAN_POINT('Ctrl Pts',(114.472755509993,4.37294471035107,339.948518056085));
#70614=CARTESIAN_POINT('Ctrl Pts',(114.194517475719,6.52776570765055,334.000624566437));
#70615=CARTESIAN_POINT('Ctrl Pts',(113.916279441445,2.69215246470304,328.96984316141));
#70616=CARTESIAN_POINT('Ctrl Pts',(113.638041407171,-3.61400935899722,329.47284768219));
#70617=CARTESIAN_POINT('Ctrl Pts',(113.359803372898,-6.60364813663642,335.048038304389));
#70618=CARTESIAN_POINT('Ctrl Pts',(113.081565338623,-3.53321648897111,340.579144883695));
#70619=CARTESIAN_POINT('Ctrl Pts',(112.80332730435,2.7795957804331,340.990352551276));
#70620=CARTESIAN_POINT('Ctrl Pts',(112.525089270076,6.54161402890032,335.904302100012));
#70621=CARTESIAN_POINT('Ctrl Pts',(112.246851235802,4.30048963711052,329.988386959043));
#70622=CARTESIAN_POINT('Ctrl Pts',(111.968613201528,-1.88713061953261,328.671555134473));
#70623=CARTESIAN_POINT('Ctrl Pts',(111.690375167254,-6.34295896063294,333.162243755305));
#70624=CARTESIAN_POINT('Ctrl Pts',(111.41213713298,-4.97794748548122,339.339414156655));
#70625=CARTESIAN_POINT('Ctrl Pts',(111.133899098706,0.955252922712176,341.534368236092));
#70626=CARTESIAN_POINT('Ctrl Pts',(110.855661064432,6.01183182324263,337.732829032383));
#70627=CARTESIAN_POINT('Ctrl Pts',(110.577423030158,5.55144139407559,331.423412962147));
#70628=CARTESIAN_POINT('Ctrl Pts',(110.299184995884,-0.0034248632939677,
328.396178026211));
#70629=CARTESIAN_POINT('Ctrl Pts',(110.02094696161,-5.55514817416955,331.429173043368));
#70630=CARTESIAN_POINT('Ctrl Pts',(109.742708927336,-6.00899399946238,337.739063253307));
#70631=CARTESIAN_POINT('Ctrl Pts',(109.464470893062,-0.948474724054632,
341.535355544193));
#70632=CARTESIAN_POINT('Ctrl Pts',(109.186232858788,4.98244580615406,339.334248513863));
#70633=CARTESIAN_POINT('Ctrl Pts',(108.907994824514,6.34104936083474,333.155665595764));
#70634=CARTESIAN_POINT('Ctrl Pts',(108.62975679024,1.8805655108125,328.669601138101));
#70635=CARTESIAN_POINT('Ctrl Pts',(108.351518755967,-4.30568555138091,329.992850279468));
#70636=CARTESIAN_POINT('Ctrl Pts',(108.073280721693,-6.54067253488663,335.91108681396));
#70637=CARTESIAN_POINT('Ctrl Pts',(107.795042687419,-2.77338087329526,340.993232426899));
#70638=CARTESIAN_POINT('Ctrl Pts',(107.516804653145,3.53900148068459,340.575477101639));
#70639=CARTESIAN_POINT('Ctrl Pts',(107.238566618871,6.60369441141642,335.041188734113));
#70640=CARTESIAN_POINT('Ctrl Pts',(106.960328584597,3.60827445116114,329.469102073235));
#70641=CARTESIAN_POINT('Ctrl Pts',(106.682090550323,-2.69840571488112,328.972638803831));
#70642=CARTESIAN_POINT('Ctrl Pts',(106.403852516049,-6.52879878478004,334.007395940445));
#70643=CARTESIAN_POINT('Ctrl Pts',(106.125614481775,-4.36780957479843,339.953051171701));
#70644=CARTESIAN_POINT('Ctrl Pts',(105.847376447501,1.80145401321206,341.353364449603));
#70645=CARTESIAN_POINT('Ctrl Pts',(105.569138413227,6.31754984271549,336.923288947608));
#70646=CARTESIAN_POINT('Ctrl Pts',(105.290900378953,5.03612342844174,330.728239566094));
#70647=CARTESIAN_POINT('Ctrl Pts',(105.012662344679,-0.866879123053034,
328.453321683692));
#70648=CARTESIAN_POINT('Ctrl Pts',(104.734424310405,-5.97435949843692,332.186193863354));
#70649=CARTESIAN_POINT('Ctrl Pts',(104.456186276131,-5.5992583435069,338.501254402905));
#70650=CARTESIAN_POINT('Ctrl Pts',(104.177948241857,-0.0858004516582664,
341.60326545534));
#70651=CARTESIAN_POINT('Ctrl Pts',(103.899710207583,5.50639524826456,338.645557263449));
#70652=CARTESIAN_POINT('Ctrl Pts',(103.62147217331,6.04545330311564,332.342374979226));
#70653=CARTESIAN_POINT('Ctrl Pts',(103.343234139036,1.03668809244208,328.478055950089));
#70654=CARTESIAN_POINT('Ctrl Pts',(103.064996104762,-4.9234304791743,330.598828711817));
#70655=CARTESIAN_POINT('Ctrl Pts',(102.786758070488,-6.36538956976742,336.758491403529));
#70656=CARTESIAN_POINT('Ctrl Pts',(102.508520036214,-1.96592460518105,341.304412489514));
#70657=CARTESIAN_POINT('Ctrl Pts',(102.23028200194,4.23764035258036,340.064867286846));
#70658=CARTESIAN_POINT('Ctrl Pts',(101.952043967666,6.55238530624785,334.17736813236));
#70659=CARTESIAN_POINT('Ctrl Pts',(101.673805933392,2.85410297742028,329.044786100778));
#70660=CARTESIAN_POINT('Ctrl Pts',(101.395567899118,-3.46334752729499,329.377215965702));
#70661=CARTESIAN_POINT('Ctrl Pts',(101.117329864844,-6.60253512513736,334.869591746742));
#70662=CARTESIAN_POINT('Ctrl Pts',(100.83909183057,-3.68267369189987,340.481641256976));
#70663=CARTESIAN_POINT('Ctrl Pts',(100.560853796296,2.61672303221954,341.063269494575));
#70664=CARTESIAN_POINT('Ctrl Pts',(100.282615762022,6.51479165243972,336.080724810714));
#70665=CARTESIAN_POINT('Ctrl Pts',(100.004377727748,4.43433213138313,330.106414919533));
#70666=CARTESIAN_POINT('Ctrl Pts',(99.726139693474,-1.71544853600877,328.622875827498));
#70667=CARTESIAN_POINT('Ctrl Pts',(99.4479016591999,-6.29098740188432,332.991529462371));
#70668=CARTESIAN_POINT('Ctrl Pts',(99.169663624926,-5.09337998387248,339.203326864648));
#70669=CARTESIAN_POINT('Ctrl Pts',(98.8914255906521,0.778347067173814,341.557793244242));
#70670=CARTESIAN_POINT('Ctrl Pts',(98.6131875563781,5.93579650305857,337.894269556463));
#70671=CARTESIAN_POINT('Ctrl Pts',(98.3349495221042,5.64605310029925,331.574717416068));
#70672=CARTESIAN_POINT('Ctrl Pts',(98.0567114878303,0.175010103002464,328.398496545858));
#70673=CARTESIAN_POINT('Ctrl Pts',(97.7784734535562,-5.4566370826748,331.280377957486));
#70674=CARTESIAN_POINT('Ctrl Pts',(97.5002354192825,-6.08080895741272,337.575701615994));
#70675=CARTESIAN_POINT('Ctrl Pts',(97.2219973850083,-1.12471220452607,341.507341918801));
#70676=CARTESIAN_POINT('Ctrl Pts',(96.9437593507347,4.86351633772921,339.467290590932));
#70677=CARTESIAN_POINT('Ctrl Pts',(96.6655213164605,6.38856772223389,333.327672624866));
#70678=CARTESIAN_POINT('Ctrl Pts',(96.3872832821866,2.05092480314952,328.722724807449));
#70679=CARTESIAN_POINT('Ctrl Pts',(96.1090452479129,-4.16882153618468,329.878339781806));
#70680=CARTESIAN_POINT('Ctrl Pts',(95.8308072136387,-6.56290188346721,335.734026742819));
#70681=CARTESIAN_POINT('Ctrl Pts',(95.5525691793649,-2.9343040405649,340.916108196163));
#70682=CARTESIAN_POINT('Ctrl Pts',(95.2743311450908,3.38706131010718,340.669064479504));
#70683=CARTESIAN_POINT('Ctrl Pts',(94.996093110817,6.60017048943689,335.219603965257));
#70684=CARTESIAN_POINT('Ctrl Pts',(94.7178550765429,3.75640062896709,329.568616133444));
#70685=CARTESIAN_POINT('Ctrl Pts',(94.4396170422691,-2.5345626443234,328.901929108874));
#70686=CARTESIAN_POINT('Ctrl Pts',(94.161379007995,-6.49959518900162,333.831351733713));
#70687=CARTESIAN_POINT('Ctrl Pts',(93.8831409737213,-4.5000451626008,339.833225623302));
#70688=CARTESIAN_POINT('Ctrl Pts',(93.6049029394472,1.62912988896106,341.399719696681));
#70689=CARTESIAN_POINT('Ctrl Pts',(93.3266649051734,6.26327648734109,337.093285464125));
#70690=CARTESIAN_POINT('Ctrl Pts',(93.0484268708992,5.14970669909762,330.865874057982));
#70691=CARTESIAN_POINT('Ctrl Pts',(92.7701888366256,-0.689672917361457,
328.432289009233));
#70692=CARTESIAN_POINT('Ctrl Pts',(92.4919508023513,-5.89614987711338,332.025795397454));
#70693=CARTESIAN_POINT('Ctrl Pts',(92.2137127680778,-5.69181712166809,338.348685450244));
#70694=CARTESIAN_POINT('Ctrl Pts',(91.9354747338034,-0.264187804751184,
341.598536291861));
#70695=CARTESIAN_POINT('Ctrl Pts',(91.6572366995299,5.4058827611804,338.793007772674));
#70696=CARTESIAN_POINT('Ctrl Pts',(91.3789986652556,6.11505450787548,332.506692005207));
#70697=CARTESIAN_POINT('Ctrl Pts',(91.1007606309819,1.21253099074983,328.508448183395));
#70698=CARTESIAN_POINT('Ctrl Pts',(90.8225225967078,-4.80271431965887,330.467405648535));
#70699=CARTESIAN_POINT('Ctrl Pts',(90.544284562434,-6.41057958686376,336.58585804903));
#70700=CARTESIAN_POINT('Ctrl Pts',(90.26604652816,-2.1355505872034,341.248991925158));
#70701=CARTESIAN_POINT('Ctrl Pts',(89.9878084938861,4.09924166565854,340.177518146537));
#70702=CARTESIAN_POINT('Ctrl Pts',(89.7095704596121,6.57222034665343,334.354712384882));
#70703=CARTESIAN_POINT('Ctrl Pts',(89.4313324253382,3.01396942133779,329.124077543191));
#70704=CARTESIAN_POINT('Ctrl Pts',(89.1530943910642,-3.31015675582382,329.285690011641));
#70705=CARTESIAN_POINT('Ctrl Pts',(88.8748563567904,-6.59660093599952,334.69124041333));
#70706=CARTESIAN_POINT('Ctrl Pts',(88.5966183225163,-3.82944180287868,340.380134930423));
#70707=CARTESIAN_POINT('Ctrl Pts',(88.3183802882425,2.45193955027557,341.131759032528));
#70708=CARTESIAN_POINT('Ctrl Pts',(88.0401422539686,6.48321216871036,336.256358375097));
#70709=CARTESIAN_POINT('Ctrl Pts',(87.7619042196945,4.56493667197442,330.228016180658));
#70710=CARTESIAN_POINT('Ctrl Pts',(87.4836661854207,-1.54251383027763,328.578853102865));
#70711=CARTESIAN_POINT('Ctrl Pts',(87.2054281511466,-6.23442215795071,332.822281756599));
#70712=CARTESIAN_POINT('Ctrl Pts',(86.9271901168728,-5.20509329119263,339.064170299233));
#70713=CARTESIAN_POINT('Ctrl Pts',(86.6489520825988,0.600872861841872,341.576429745317));
#70714=CARTESIAN_POINT('Ctrl Pts',(86.3707140483249,5.855426858433,338.053596682067));
#70715=CARTESIAN_POINT('Ctrl Pts',(86.092476014051,5.73654205299892,331.728523014697));
#70716=CARTESIAN_POINT('Ctrl Pts',(85.8142379797769,0.353317276749643,328.405635489819));
#70717=CARTESIAN_POINT('Ctrl Pts',(85.535999945503,-5.35414154941832,331.134298943272));
#70718=CARTESIAN_POINT('Ctrl Pts',(85.2577619112292,-6.14818370268483,337.410459198831));
#70719=CARTESIAN_POINT('Ctrl Pts',(84.9795238769551,-1.30012841904015,341.474576625942));
#70720=CARTESIAN_POINT('Ctrl Pts',(84.7012858426813,4.74103552489365,339.597070648021));
#70721=CARTESIAN_POINT('Ctrl Pts',(84.4230478084072,6.43142114520221,333.500900789061));
#70722=CARTESIAN_POINT('Ctrl Pts',(84.1448097741333,2.21978650817918,328.780432149313));
#70723=CARTESIAN_POINT('Ctrl Pts',(83.8665717398596,-4.02891344340471,329.767569125469));
#70724=CARTESIAN_POINT('Ctrl Pts',(83.5883337055854,-6.58033899464105,335.556430684628));
#70725=CARTESIAN_POINT('Ctrl Pts',(83.3100956713115,-3.09308457613965,340.834664017408));
#70726=CARTESIAN_POINT('Ctrl Pts',(83.0318576370376,3.2326479040316,340.758512300912));
#70727=CARTESIAN_POINT('Ctrl Pts',(82.7536196027636,6.5918271164779,335.397858841371));
#70728=CARTESIAN_POINT('Ctrl Pts',(82.4753815684898,3.90178387934119,329.67209619549));
#70729=CARTESIAN_POINT('Ctrl Pts',(82.1971435342158,-2.36886883363129,328.835672231278));
#70730=CARTESIAN_POINT('Ctrl Pts',(81.918905499942,-6.46564558242699,333.656160875092));
#70731=CARTESIAN_POINT('Ctrl Pts',(81.6406674656679,-4.62899481300182,339.709870848802));
#70732=CARTESIAN_POINT('Ctrl Pts',(81.3624294313939,1.45561617246357,341.441401862146));
#70733=CARTESIAN_POINT('Ctrl Pts',(81.0841913971202,6.20442968131859,337.261753461534));
#70734=CARTESIAN_POINT('Ctrl Pts',(80.8059533628462,5.25952964885982,331.006527292699));
#70735=CARTESIAN_POINT('Ctrl Pts',(80.5277153285721,-0.511963111827283,
328.416052083794));
#70736=CARTESIAN_POINT('Ctrl Pts',(80.2494772942983,-5.81363488135362,331.867568698678));
#70737=CARTESIAN_POINT('Ctrl Pts',(79.9712392600242,-5.78021972937194,338.193671284176));
#70738=CARTESIAN_POINT('Ctrl Pts',(79.6930012257504,-0.442382247648974,
341.588988870696));
#70739=CARTESIAN_POINT('Ctrl Pts',(79.4147631914764,5.30142289319017,338.937688623895));
#70740=CARTESIAN_POINT('Ctrl Pts',(79.1365251572024,6.18019049382234,332.672829647134));
#70741=CARTESIAN_POINT('Ctrl Pts',(78.8582871229286,1.38748849773591,328.54358055422));
#70742=CARTESIAN_POINT('Ctrl Pts',(78.5800490886545,-4.67849121342611,330.339292290103));
#70743=CARTESIAN_POINT('Ctrl Pts',(78.3018110543807,-6.4510885924441,336.412066699426));
#70744=CARTESIAN_POINT('Ctrl Pts',(78.0235730201066,-2.30361718808769,341.189008340755));
#70745=CARTESIAN_POINT('Ctrl Pts',(77.7453349858328,3.95784970844284,340.286388377386));
#70746=CARTESIAN_POINT('Ctrl Pts',(77.4670969515588,6.58725634530131,334.532527827055));
#70747=CARTESIAN_POINT('Ctrl Pts',(77.1888589172849,3.17163506182105,329.207659589957));
#70748=CARTESIAN_POINT('Ctrl Pts',(76.910620883011,-3.15454890463561,329.198336652351));
#70749=CARTESIAN_POINT('Ctrl Pts',(76.6323828487369,-6.58584990237367,334.513114536472));
#70750=CARTESIAN_POINT('Ctrl Pts',(76.3541448144631,-3.97341365168864,340.274700024055));
#70751=CARTESIAN_POINT('Ctrl Pts',(76.0759067801891,2.2853656596617,341.195771154007));
#70752=CARTESIAN_POINT('Ctrl Pts',(75.7976687459152,6.44689863708233,336.431074545359));
#70753=CARTESIAN_POINT('Ctrl Pts',(75.5194307116413,4.69220789132043,330.353101949061));
#70754=CARTESIAN_POINT('Ctrl Pts',(75.2411926773673,-1.3684527794313,328.539519106006));
#70755=CARTESIAN_POINT('Ctrl Pts',(74.9629546430933,-6.17330453282882,332.654624222828));
#70756=CARTESIAN_POINT('Ctrl Pts',(74.6847166088195,-5.31300583427489,338.92204607267));
#70757=CARTESIAN_POINT('Ctrl Pts',(74.4064785745454,0.422959898555554,341.590264130928));
#70758=CARTESIAN_POINT('Ctrl Pts',(74.1282405402716,5.77078157535943,338.210694068373));
#70759=CARTESIAN_POINT('Ctrl Pts',(73.8500025059976,5.82284217705239,331.884717449037));
#70760=CARTESIAN_POINT('Ctrl Pts',(73.5717644717237,0.531366457874022,328.417589645226));
#70761=CARTESIAN_POINT('Ctrl Pts',(73.2935264374498,-5.24773641673927,330.991042667773));
#70762=CARTESIAN_POINT('Ctrl Pts',(73.0152884031758,-6.21106903817348,337.243456661992));
#70763=CARTESIAN_POINT('Ctrl Pts',(72.7370503689018,-1.47459527850462,341.437083590866));
#70764=CARTESIAN_POINT('Ctrl Pts',(72.4588123346279,4.61509280325731,339.723493919602));
#70765=CARTESIAN_POINT('Ctrl Pts',(72.180574300354,6.46957833812812,333.675223596974));
#70766=CARTESIAN_POINT('Ctrl Pts',(71.90233626608,2.3870273229185,328.842681025737));
#70767=CARTESIAN_POINT('Ctrl Pts',(71.6240982318062,-3.88606343406789,329.660619195301));
#70768=CARTESIAN_POINT('Ctrl Pts',(71.3458601975322,-6.59297113581244,335.378428320206));
#70769=CARTESIAN_POINT('Ctrl Pts',(71.0676221632582,-3.24960653831636,340.748959361252));
#70770=CARTESIAN_POINT('Ctrl Pts',(70.7893841289843,3.07587401527876,340.843755250977));
#70771=CARTESIAN_POINT('Ctrl Pts',(70.5111460947104,6.57867038487854,335.575823200567));
#70772=CARTESIAN_POINT('Ctrl Pts',(70.2329080604365,4.04431804329124,329.779466698133));
#70773=CARTESIAN_POINT('Ctrl Pts',(69.9546700261624,-2.20144527258785,328.773916551877));
#70774=CARTESIAN_POINT('Ctrl Pts',(69.6764319918886,-6.42697475509217,333.481951289123));
#70775=CARTESIAN_POINT('Ctrl Pts',(69.3981939576146,-4.75456436684029,339.583076921977));
#70776=CARTESIAN_POINT('Ctrl Pts',(69.1199559233406,1.28103956360592,341.478380509639));
#70777=CARTESIAN_POINT('Ctrl Pts',(68.8417178890667,6.14105239464392,337.428569924345));
#70778=CARTESIAN_POINT('Ctrl Pts',(68.5634798547928,5.36551208490198,331.150096565112));
#70779=CARTESIAN_POINT('Ctrl Pts',(68.2852418205188,-0.333879470325961,
328.404622763596));
#70780=CARTESIAN_POINT('Ctrl Pts',(68.007003786245,-5.72687476368866,331.711629304318));
#70781=CARTESIAN_POINT('Ctrl Pts',(67.728765751971,-5.86440161494724,338.036325096198));
#70782=CARTESIAN_POINT('Ctrl Pts',(67.450527717697,-0.620253662594679,341.574630163379));
#70783=CARTESIAN_POINT('Ctrl Pts',(67.1722896834231,5.19309192099196,339.079494171012));
#70784=CARTESIAN_POINT('Ctrl Pts',(66.8940516491492,6.24081369859539,332.840666591141));
#70785=CARTESIAN_POINT('Ctrl Pts',(66.6158136148752,1.56143285925702,328.583427408871));
#70786=CARTESIAN_POINT('Ctrl Pts',(66.3375755806014,-4.55085186831029,330.214582185024));
#70787=CARTESIAN_POINT('Ctrl Pts',(66.0593375463273,-6.48688700679271,336.237244257329));
#70788=CARTESIAN_POINT('Ctrl Pts',(65.7810995120535,-2.47000168543674,341.124505536378));
#70789=CARTESIAN_POINT('Ctrl Pts',(65.5028614777794,3.81356772547941,340.391398482247));
#70790=CARTESIAN_POINT('Ctrl Pts',(65.2246234435056,6.59748232289047,334.710684617869));
#70791=CARTESIAN_POINT('Ctrl Pts',(64.9463854092316,3.32698477126441,329.295471209385));
#70792=CARTESIAN_POINT('Ctrl Pts',(64.6681473749577,-2.99663759873627,329.115219673341));
#70793=CARTESIAN_POINT('Ctrl Pts',(64.3899093406837,-6.57028987467513,334.335344183859));
#70794=CARTESIAN_POINT('Ctrl Pts',(64.1116713064098,-4.1144841099442,340.165413526544));
#70795=CARTESIAN_POINT('Ctrl Pts',(63.8334332721358,2.1171229927966,341.255259117299));
#70796=CARTESIAN_POINT('Ctrl Pts',(63.5551952378619,6.40587757373213,336.604745743583));
#70797=CARTESIAN_POINT('Ctrl Pts',(63.2769572035879,4.81605285585167,330.481580886987));
#70798=CARTESIAN_POINT('Ctrl Pts',(62.9987191693141,-1.19339248302022,328.504902558648));
#70799=CARTESIAN_POINT('Ctrl Pts',(62.72048113504,-6.10767915466864,332.488679284755));
#70800=CARTESIAN_POINT('Ctrl Pts',(62.4422431007662,-5.41703881527419,338.777057964211));
#70801=CARTESIAN_POINT('Ctrl Pts',(62.1640050664922,0.244738089535523,341.599286299194));
#70802=CARTESIAN_POINT('Ctrl Pts',(61.8857670322182,5.68192246190678,338.365447002713));
#70803=CARTESIAN_POINT('Ctrl Pts',(61.6075289979444,5.90489045602424,332.043186665759));
#70804=CARTESIAN_POINT('Ctrl Pts',(61.3292909636703,0.709027634688525,328.434350283145));
#70805=CARTESIAN_POINT('Ctrl Pts',(61.0510529293965,-5.13749938177011,330.850713736857));
#70806=CARTESIAN_POINT('Ctrl Pts',(60.7728148951225,-6.2694190449449,337.074815950891));
#70807=CARTESIAN_POINT('Ctrl Pts',(60.4945768608485,-1.64798538704716,341.394890191025));
#70808=CARTESIAN_POINT('Ctrl Pts',(60.2163388265747,4.48578013631931,339.84646809128));
#70809=CARTESIAN_POINT('Ctrl Pts',(59.9381007923006,6.50301143859184,333.850513757919));
#70810=CARTESIAN_POINT('Ctrl Pts',(59.6598627580269,2.5525251279602,328.909425982527));
#70811=CARTESIAN_POINT('Ctrl Pts',(59.3816247237527,-3.7403758173912,329.557568086244));
#70812=CARTESIAN_POINT('Ctrl Pts',(59.103386689479,-6.60078908297948,335.200149627053));
#70813=CARTESIAN_POINT('Ctrl Pts',(58.8251486552049,-3.4037556346047,340.659056809318));
#70814=CARTESIAN_POINT('Ctrl Pts',(58.5469106209311,2.91685412029599,340.924731085214));
#70815=CARTESIAN_POINT('Ctrl Pts',(58.2686725866571,6.56070990169731,335.753367093097));
#70816=CARTESIAN_POINT('Ctrl Pts',(57.9904345523832,4.18389904223041,329.890649239325));
#70817=CARTESIAN_POINT('Ctrl Pts',(57.7121965181092,-2.03241421404269,328.716707164732));
#70818=CARTESIAN_POINT('Ctrl Pts',(57.4339584838352,-6.38361094447344,333.308850183812));
#70819=CARTESIAN_POINT('Ctrl Pts',(57.1557204495613,-4.87666213310401,339.452936427881));
#70820=CARTESIAN_POINT('Ctrl Pts',(56.8774824152874,1.10552753839988,341.510628637314));
#70821=CARTESIAN_POINT('Ctrl Pts',(56.5992443810134,6.07319090547391,337.593613043008));
#70822=CARTESIAN_POINT('Ctrl Pts',(56.3210063467396,5.46757661874537,331.296477040796));
#70823=CARTESIAN_POINT('Ctrl Pts',(56.0427683124655,-0.155552029707196,
328.398009394339));
#70824=CARTESIAN_POINT('Ctrl Pts',(55.7645302781917,-5.63593287644166,331.558091081473));
#70825=CARTESIAN_POINT('Ctrl Pts',(55.4862922439177,-5.94430130869852,337.876761780648));
#70826=CARTESIAN_POINT('Ctrl Pts',(55.2080542096437,-0.797672167706236,
341.555470654657));
#70827=CARTESIAN_POINT('Ctrl Pts',(54.9298161753698,5.08096894796816,339.218320867475));
#70828=CARTESIAN_POINT('Ctrl Pts',(54.6515781410958,6.29687985507091,333.010080282526));
#70829=CARTESIAN_POINT('Ctrl Pts',(54.373340106822,1.73423706096941,328.627959651136));
#70830=CARTESIAN_POINT('Ctrl Pts',(54.0951020725479,-4.41988948668667,330.093366396737));
#70831=CARTESIAN_POINT('Ctrl Pts',(53.8168640382742,-6.51794868987227,336.06151837826));
#70832=CARTESIAN_POINT('Ctrl Pts',(53.5386260040001,-2.63458258512705,341.055530612038));
#70833=CARTESIAN_POINT('Ctrl Pts',(53.2603879697263,3.66650107161404,340.492471782635));
#70834=CARTESIAN_POINT('Ctrl Pts',(52.9821499354522,6.60289081240205,334.889052667058));
#70835=CARTESIAN_POINT('Ctrl Pts',(52.7039119011784,3.47990511315732,329.387448281342));
#70836=CARTESIAN_POINT('Ctrl Pts',(52.4256738669043,-2.83653814511659,329.036399766711));
#70837=CARTESIAN_POINT('Ctrl Pts',(52.1474358326305,-6.54993221485141,334.158059163574));
#70838=CARTESIAN_POINT('Ctrl Pts',(51.8691977983565,-4.25255016785809,340.052355238999));
#70839=CARTESIAN_POINT('Ctrl Pts',(51.5909597640826,1.947334400641,341.310179484236));
#70840=CARTESIAN_POINT('Ctrl Pts',(51.3127217298086,6.36017893228049,336.777245154886));
#70841=CARTESIAN_POINT('Ctrl Pts',(51.0344836955347,4.93638113385334,330.613359178993));
#70842=CARTESIAN_POINT('Ctrl Pts',(50.7562456612607,-1.01746077024492,328.475028737825));
#70843=CARTESIAN_POINT('Ctrl Pts',(50.4780076269868,-6.03759394318577,332.324568115538));
#70844=CARTESIAN_POINT('Ctrl Pts',(50.1997695927128,-5.51711626920556,338.629311844311));
#70845=CARTESIAN_POINT('Ctrl Pts',(49.9215315584389,0.0663375725219412,
341.603489662116));
#70846=CARTESIAN_POINT('Ctrl Pts',(49.643293524165,5.58891440308703,338.517742484343));
#70847=CARTESIAN_POINT('Ctrl Pts',(49.3650554898911,5.98262697818051,332.203814950485));
#70848=CARTESIAN_POINT('Ctrl Pts',(49.0868174556171,0.886171078827202,328.455905164941));
#70849=CARTESIAN_POINT('Ctrl Pts',(48.8085794213432,-5.02351093970216,330.713414618851));
#70850=CARTESIAN_POINT('Ctrl Pts',(48.5303413870692,-6.32319111576674,336.904660207144));
#70851=CARTESIAN_POINT('Ctrl Pts',(48.2521033527954,-1.82017213504033,341.348027236081));
#70852=CARTESIAN_POINT('Ctrl Pts',(47.9738653185213,4.35319194831591,339.965903367194));
#70853=CARTESIAN_POINT('Ctrl Pts',(47.6956272842475,6.53169603371061,334.026643274848));
#70854=CARTESIAN_POINT('Ctrl Pts',(47.4173892499734,2.7161590766445,328.980618282452));
#70855=CARTESIAN_POINT('Ctrl Pts',(47.1391512156996,-3.591956974616,329.458491046321));
#70856=CARTESIAN_POINT('Ctrl Pts',(46.8609131814255,-6.60378712746943,335.021724784445));
#70857=CARTESIAN_POINT('Ctrl Pts',(46.5826751471518,-3.55541930518241,340.565022008539));
#70858=CARTESIAN_POINT('Ctrl Pts',(46.3044371128777,2.75570433556762,341.001380674989));
#70859=CARTESIAN_POINT('Ctrl Pts',(46.0261990786039,6.53795878169654,335.930360876233));
#70860=CARTESIAN_POINT('Ctrl Pts',(45.7479610443298,4.320424953976,330.005562633464));
#70861=CARTESIAN_POINT('Ctrl Pts',(45.4697230100559,-1.86189908464054,328.664085844189));
#70862=CARTESIAN_POINT('Ctrl Pts',(45.191484975782,-6.33558581486789,333.136983957762));
#70863=CARTESIAN_POINT('Ctrl Pts',(44.9132469415081,-4.99519895588432,339.319544395225));
#70864=CARTESIAN_POINT('Ctrl Pts',(44.6350089072341,0.929208255898556,341.538122697561));
#70865=CARTESIAN_POINT('Ctrl Pts',(44.3567708729602,6.0008947663347,337.756762302877));
#70866=CARTESIAN_POINT('Ctrl Pts',(44.0785328386862,5.56564872276705,331.445561832588));
#70867=CARTESIAN_POINT('Ctrl Pts',(43.8002948044123,0.0228889951565719,
328.396216805112));
#70868=CARTESIAN_POINT('Ctrl Pts',(43.5220567701384,-5.54087562546809,331.407066143903));
#70869=CARTESIAN_POINT('Ctrl Pts',(43.2438187358644,-6.01986046779084,337.715097850819));
#70870=CARTESIAN_POINT('Ctrl Pts',(42.9655807015905,-0.974508211817014,
341.531524334815));
#70871=CARTESIAN_POINT('Ctrl Pts',(42.6873426673165,4.96513584642345,339.354067341895));
#70872=CARTESIAN_POINT('Ctrl Pts',(42.4091046330427,6.34834802368656,333.180947015245));
#70873=CARTESIAN_POINT('Ctrl Pts',(42.1308665987686,1.9057749210758,328.677144763527));
#70874=CARTESIAN_POINT('Ctrl Pts',(41.8526285644948,-4.28569969741449,329.97573343713));
#70875=CARTESIAN_POINT('Ctrl Pts',(41.5743905302207,-6.54425096041135,335.885017377426));
#70876=CARTESIAN_POINT('Ctrl Pts',(41.2961524959469,-2.79723971002455,340.982133933291));
#70877=CARTESIAN_POINT('Ctrl Pts',(41.0179144616729,3.51675713506133,340.58953447473));
#70878=CARTESIAN_POINT('Ctrl Pts',(40.7396764273991,6.60347786455166,335.0675017301));
#70879=CARTESIAN_POINT('Ctrl Pts',(40.461438393125,3.63028442491644,329.483523644082));
#70880=CARTESIAN_POINT('Ctrl Pts',(40.1832003588512,-2.67436744855432,328.961934486832));
#70881=CARTESIAN_POINT('Ctrl Pts',(39.9049623245772,-6.52479178808562,333.981388929316));
#70882=CARTESIAN_POINT('Ctrl Pts',(39.6267242903033,-4.38751100945966,339.935607716691));
#70883=CARTESIAN_POINT('Ctrl Pts',(39.3484862560292,1.77612386299106,341.36049215191));
#70884=CARTESIAN_POINT('Ctrl Pts',(39.0702482217554,6.30983608192015,336.948446820032));
#70885=CARTESIAN_POINT('Ctrl Pts',(38.7920101874814,5.05310486149901,330.748340600438));
#70886=CARTESIAN_POINT('Ctrl Pts',(38.5137721532075,-0.840786106614272,
328.449919457434));
#70887=CARTESIAN_POINT('Ctrl Pts',(38.2355341189336,-5.96310007467022,332.162410549312));
#70888=CARTESIAN_POINT('Ctrl Pts',(37.9572960846596,-5.61316511941414,338.478915597335));
#70889=CARTESIAN_POINT('Ctrl Pts',(37.6790580503857,-0.11211138425306,341.602871150394));
#70890=CARTESIAN_POINT('Ctrl Pts',(37.4008200161118,5.49182531347575,338.667469306956));
#70891=CARTESIAN_POINT('Ctrl Pts',(37.1225819818378,6.05599498023661,332.366485012281));
#70892=CARTESIAN_POINT('Ctrl Pts',(36.8443439475639,1.06266743997372,328.48223855122));
#70893=CARTESIAN_POINT('Ctrl Pts',(36.5661059132899,-4.90585432500734,330.579245569702));
#70894=CARTESIAN_POINT('Ctrl Pts',(36.287867879016,-6.37234598622031,336.733113678641));
#70895=CARTESIAN_POINT('Ctrl Pts',(36.009629844742,-1.99102979155148,341.296528945406));
#70896=CARTESIAN_POINT('Ctrl Pts',(35.7313918104681,4.21742505527259,340.081712535589));
#70897=CARTESIAN_POINT('Ctrl Pts',(35.4531537761941,6.55561117796478,334.203483537813));
#70898=CARTESIAN_POINT('Ctrl Pts',(35.1749157419203,2.87780968330108,329.056205940826));
#70899=CARTESIAN_POINT('Ctrl Pts',(34.8966777076463,-3.44091528132674,329.363460421683));
#70900=CARTESIAN_POINT('Ctrl Pts',(34.6184396733724,-6.6019630801073,334.843284078378));
#70901=CARTESIAN_POINT('Ctrl Pts',(34.3402016390984,-3.70448680508874,340.466923623218));
#70902=CARTESIAN_POINT('Ctrl Pts',(34.0619636048245,2.59254233282417,341.073648050696));
#70903=CARTESIAN_POINT('Ctrl Pts',(33.7837255705505,6.51043363776641,336.106675308945));
#70904=CARTESIAN_POINT('Ctrl Pts',(33.5054875362766,4.45379608717343,330.124122970679));
#70905=CARTESIAN_POINT('Ctrl Pts',(33.2272495020026,-1.69002439469614,328.616091014393));
#70906=CARTESIAN_POINT('Ctrl Pts',(32.9490114677288,-6.28293443427222,332.966478107856));
#70907=CARTESIAN_POINT('Ctrl Pts',(32.6707734334547,-5.11008827947693,339.182998227008));
#70908=CARTESIAN_POINT('Ctrl Pts',(32.3925353991809,0.752210464614984,341.560842614186));
#70909=CARTESIAN_POINT('Ctrl Pts',(32.1142973649069,5.92421676793797,337.917898572204));
#70910=CARTESIAN_POINT('Ctrl Pts',(31.836059330633,5.65965678462045,331.597242078624));
#70911=CARTESIAN_POINT('Ctrl Pts',(31.557821296359,0.201313306453949,328.399246304865));
#70912=CARTESIAN_POINT('Ctrl Pts',(31.2795832620851,-5.44177242166582,331.258664770167));
#70913=CARTESIAN_POINT('Ctrl Pts',(31.0013452278111,-6.09102391885213,337.551451353869));
#70914=CARTESIAN_POINT('Ctrl Pts',(30.7231071935373,-1.15063266907353,341.502808689487));
#70915=CARTESIAN_POINT('Ctrl Pts',(30.4448691592632,4.8456771978035,339.486634472059));
#70916=CARTESIAN_POINT('Ctrl Pts',(30.1666311249894,6.39518062233446,333.353142022241));
#70917=CARTESIAN_POINT('Ctrl Pts',(29.8883930907154,2.07592118246034,328.730946831028));
#70918=CARTESIAN_POINT('Ctrl Pts',(29.6101550564415,-4.14838048601121,329.861769201907));
#70919=CARTESIAN_POINT('Ctrl Pts',(29.3319170221675,-6.56577461246588,335.707870136034));
#70920=CARTESIAN_POINT('Ctrl Pts',(29.0536789878936,-2.95785428773503,340.904369094469));
#70921=CARTESIAN_POINT('Ctrl Pts',(28.7754409536196,3.36444525899253,340.682515683255));
#70922=CARTESIAN_POINT('Ctrl Pts',(28.4972029193457,6.59924305067326,335.245901503312));
#70923=CARTESIAN_POINT('Ctrl Pts',(28.2189648850717,3.77801289941892,329.58362714328));
#70924=CARTESIAN_POINT('Ctrl Pts',(27.9407268507979,-2.51024392625319,328.891878208328));
#70925=CARTESIAN_POINT('Ctrl Pts',(27.6624888165239,-6.49488695194235,333.805462485863));
#70926=CARTESIAN_POINT('Ctrl Pts',(27.38425078225,-4.51926808620829,339.815256208777));
#70927=CARTESIAN_POINT('Ctrl Pts',(27.106012747976,1.60361639795151,341.406160381961));
#70928=CARTESIAN_POINT('Ctrl Pts',(26.8277747137021,6.25488578305044,337.118225727392));
#70929=CARTESIAN_POINT('Ctrl Pts',(26.5495366794281,5.16613880700681,330.886426587756));
#70930=CARTESIAN_POINT('Ctrl Pts',(26.2712986451542,-0.663497500143172,
328.429593052291));
#70931=CARTESIAN_POINT('Ctrl Pts',(25.9930606108802,-5.88425194461882,332.002324993692));
#70932=CARTESIAN_POINT('Ctrl Pts',(25.7148225766064,-5.70511523093411,338.325979042772));
#70933=CARTESIAN_POINT('Ctrl Pts',(25.4365845423323,-0.290478477183944,
341.597431215669));
#70934=CARTESIAN_POINT('Ctrl Pts',(25.1583465080585,5.39072608762264,338.814518139873));
#70935=CARTESIAN_POINT('Ctrl Pts',(24.8801084737845,6.12494088880454,332.53107806931));
#70936=CARTESIAN_POINT('Ctrl Pts',(24.6018704395106,1.23838784030986,328.513331213315));
#70937=CARTESIAN_POINT('Ctrl Pts',(24.3236324052366,-4.78461545066262,330.448304559785));
#70938=CARTESIAN_POINT('Ctrl Pts',(24.0453943709627,-6.41684776337031,336.560301628827));
#70939=CARTESIAN_POINT('Ctrl Pts',(23.7671563366888,-2.16043359615079,341.240432923108));
#70940=CARTESIAN_POINT('Ctrl Pts',(23.4889183024148,4.0785785943087,340.193811032492));
#70941=CARTESIAN_POINT('Ctrl Pts',(23.2106802681409,6.57473940849246,334.380905417883));
#70942=CARTESIAN_POINT('Ctrl Pts',(22.9324422338669,3.03735891049729,329.136133763461));
#70943=CARTESIAN_POINT('Ctrl Pts',(22.654204199593,-3.28736102831721,329.272545603789));
#70944=CARTESIAN_POINT('Ctrl Pts',(22.3759661653191,-6.59531827281427,334.664957806429));
#70945=CARTESIAN_POINT('Ctrl Pts',(22.0977281310451,-3.85084928508779,340.364833284896));
#70946=CARTESIAN_POINT('Ctrl Pts',(21.8194900967712,2.42748725312145,341.141480442623));
#70947=CARTESIAN_POINT('Ctrl Pts',(21.5412520624972,6.47815456879428,336.282181646259));
#70948=CARTESIAN_POINT('Ctrl Pts',(21.2630140282234,4.58391505408935,330.246243678092));
#70949=CARTESIAN_POINT('Ctrl Pts',(20.9847759939494,-1.5169156472776,328.572757721213));
#70950=CARTESIAN_POINT('Ctrl Pts',(20.7065379596755,-6.22569524877642,332.797457137636));
#70951=CARTESIAN_POINT('Ctrl Pts',(20.4282999254015,-5.22124621158455,339.043397629371));
#70952=CARTESIAN_POINT('Ctrl Pts',(20.1500618911275,0.574663408510707,341.578771797085));
#70953=CARTESIAN_POINT('Ctrl Pts',(19.8718238568537,5.8432129006337,338.076904189125));
#70954=CARTESIAN_POINT('Ctrl Pts',(19.5935858225797,5.74953215952618,331.751407021838));
#70955=CARTESIAN_POINT('Ctrl Pts',(19.3153477883058,0.379590618577057,328.407095681455));
#70956=CARTESIAN_POINT('Ctrl Pts',(19.0371097540318,-5.33869563029188,331.112995323094));
#70957=CARTESIAN_POINT('Ctrl Pts',(18.7588717197579,-6.1577396982603,337.385941784633));
#70958=CARTESIAN_POINT('Ctrl Pts',(18.4806336854839,-1.3259169332242,341.469344686858));
#70959=CARTESIAN_POINT('Ctrl Pts',(18.20239565121,4.7226802309299,339.615925457325));
#70960=CARTESIAN_POINT('Ctrl Pts',(17.924157616936,6.43734345380558,333.526539566552));
#70961=CARTESIAN_POINT('Ctrl Pts',(17.6459195826621,2.2445516041575,328.789326567315));
#70962=CARTESIAN_POINT('Ctrl Pts',(17.3676815483882,-4.00803212309852,329.751556907862));
#70963=CARTESIAN_POINT('Ctrl Pts',(17.0894435141142,-6.58250392944424,335.530206007173));
#70964=CARTESIAN_POINT('Ctrl Pts',(16.8112054798403,-3.11630903733763,340.822292879527));
#70965=CARTESIAN_POINT('Ctrl Pts',(16.5329674455664,3.20967666168759,340.771347513243));
#70966=CARTESIAN_POINT('Ctrl Pts',(16.2547294112924,6.59018946303222,335.424121719004));
#70967=CARTESIAN_POINT('Ctrl Pts',(15.9764913770185,3.92298266518878,329.687685683262));
#70968=CARTESIAN_POINT('Ctrl Pts',(15.6982533427445,-2.34428742136838,328.82628208636));
#70969=CARTESIAN_POINT('Ctrl Pts',(15.4200153084707,-6.46023954296288,333.630408294877));
#70970=CARTESIAN_POINT('Ctrl Pts',(15.1417772741966,-4.6477251889569,339.691388596047));
#70971=CARTESIAN_POINT('Ctrl Pts',(14.8635392399228,1.42993797063821,341.447150827403));
#70972=CARTESIAN_POINT('Ctrl Pts',(14.5853012056488,6.19536816043845,337.286457904246));
#70973=CARTESIAN_POINT('Ctrl Pts',(14.3070631713749,5.27540043286967,331.027516310419));
#70974=CARTESIAN_POINT('Ctrl Pts',(14.0288251371009,-0.485724407125341,
328.414064364768));
#70975=CARTESIAN_POINT('Ctrl Pts',(13.750587102827,-5.80110712804899,331.844428343299));
#70976=CARTESIAN_POINT('Ctrl Pts',(13.472349068553,-5.7928994616363,338.170613855061));
#70977=CARTESIAN_POINT('Ctrl Pts',(13.1941110342791,-0.468633462574989,
341.587173830145));
#70978=CARTESIAN_POINT('Ctrl Pts',(12.9158730000052,5.28569054852431,338.958781607969));
#70979=CARTESIAN_POINT('Ctrl Pts',(12.6376349657312,6.18941435905494,332.697473935422));
#70980=CARTESIAN_POINT('Ctrl Pts',(12.3593969314573,1.4132039694968,328.549160447597));
#70981=CARTESIAN_POINT('Ctrl Pts',(12.0811588971833,-4.65988284705173,330.320687201855));
#70982=CARTESIAN_POINT('Ctrl Pts',(11.8029208629094,-6.45666394887963,336.386350246169));
#70983=CARTESIAN_POINT('Ctrl Pts',(11.5246828286355,-2.3282598558614,341.17978012878));
#70984=CARTESIAN_POINT('Ctrl Pts',(11.2464447943615,3.93675396228422,340.302117006826));
#70985=CARTESIAN_POINT('Ctrl Pts',(10.9682067600876,6.58906673699744,334.558779355101));
#70986=CARTESIAN_POINT('Ctrl Pts',(10.6899687258136,3.194690294589,329.220343398933));
#70987=CARTESIAN_POINT('Ctrl Pts',(10.4117306915397,-3.13140641536669,329.185812956169));
#70988=CARTESIAN_POINT('Ctrl Pts',(10.1334926572658,-6.58385741731503,334.486876225204));
#70989=CARTESIAN_POINT('Ctrl Pts',(9.8552546229919,-3.99440013610684,340.258825459627));
#70990=CARTESIAN_POINT('Ctrl Pts',(9.57701658871792,2.2606601201243,341.204828471322));
#70991=CARTESIAN_POINT('Ctrl Pts',(9.29877855444402,6.44114420034843,336.456751446593));
#70992=CARTESIAN_POINT('Ctrl Pts',(9.02054052017004,4.71068862539824,330.371836124353));
#70993=CARTESIAN_POINT('Ctrl Pts',(8.74230248589616,-1.34270261449642,328.534116584563));
#70994=CARTESIAN_POINT('Ctrl Pts',(8.46406445162217,-6.16390369514632,332.630046396311));
#70995=CARTESIAN_POINT('Ctrl Pts',(8.18582641734826,-5.32860359231034,338.900840894707));
#70996=CARTESIAN_POINT('Ctrl Pts',(7.9075883830743,0.396719405668529,341.591904035162));
#70997=CARTESIAN_POINT('Ctrl Pts',(7.62935034880038,5.75789950218825,338.233650055209));
#70998=CARTESIAN_POINT('Ctrl Pts',(7.35111231452643,5.83529005701858,331.907968623078));
#70999=CARTESIAN_POINT('Ctrl Pts',(7.07287428025249,0.55743811637587,328.419712881418));
#71000=CARTESIAN_POINT('Ctrl Pts',(6.79463624597856,-5.2314323012991,330.970251635584));
#71001=CARTESIAN_POINT('Ctrl Pts',(6.51639821170462,-6.22050336214957,337.218524847874));
#71002=CARTESIAN_POINT('Ctrl Pts',(6.23816017743065,-1.49920482391282,341.431468591223));
#71003=CARTESIAN_POINT('Ctrl Pts',(5.95992214315676,4.59428931436643,339.741257165524));
#71004=CARTESIAN_POINT('Ctrl Pts',(5.68168410888278,6.47851196515078,333.702124066768));
#71005=CARTESIAN_POINT('Ctrl Pts',(5.40344607460889,2.40427635277464,328.850148725226));
#71006=CARTESIAN_POINT('Ctrl Pts',(5.17158104604725,-2.80664825497015,329.515899410373));
#71007=CARTESIAN_POINT('Ctrl Pts',(4.98608902319796,-5.24601881533458,332.499051932022));
#71008=CARTESIAN_POINT('Ctrl Pts',(4.89334301177332,-5.62621912735357,334.369308258557));
#71009=CARTESIAN_POINT('Ctrl Pts',(4.846970006061,-5.57663578288216,335.297802782702));
#71010=CARTESIAN_POINT('Ctrl Pts',(185.229648962969,-2.58535847492491,329.674069654478));
#71011=CARTESIAN_POINT('Ctrl Pts',(185.183274228959,-3.47214497774874,330.104540455452));
#71012=CARTESIAN_POINT('Ctrl Pts',(185.090526489235,-5.01199270296094,331.416981243083));
#71013=CARTESIAN_POINT('Ctrl Pts',(184.905032738087,-6.52748388791409,335.210688764241));
#71014=CARTESIAN_POINT('Ctrl Pts',(184.673167709526,-4.47101474106914,340.386142168329));
#71015=CARTESIAN_POINT('Ctrl Pts',(184.394929675251,2.12056568075629,341.675688707916));
#71016=CARTESIAN_POINT('Ctrl Pts',(184.116691640978,6.75574576068523,336.828780790692));
#71017=CARTESIAN_POINT('Ctrl Pts',(183.838453606705,5.19669865427865,330.308915602165));
#71018=CARTESIAN_POINT('Ctrl Pts',(183.560215572429,-1.13414317430391,328.091207546338));
#71019=CARTESIAN_POINT('Ctrl Pts',(183.281977538157,-6.42268452913922,332.215067306152));
#71020=CARTESIAN_POINT('Ctrl Pts',(183.003739503882,-5.81802477444936,338.89383994989));
#71021=CARTESIAN_POINT('Ctrl Pts',(182.725501469609,0.126174998855868,341.999705536135));
#71022=CARTESIAN_POINT('Ctrl Pts',(182.447263435334,5.95436099319128,338.681826267342));
#71023=CARTESIAN_POINT('Ctrl Pts',(182.169025401061,6.31843686875824,331.985305041678));
#71024=CARTESIAN_POINT('Ctrl Pts',(181.890787366786,0.884113425449771,328.05526362586));
#71025=CARTESIAN_POINT('Ctrl Pts',(181.612549332511,-5.3615144597533,330.49833671817));
#71026=CARTESIAN_POINT('Ctrl Pts',(181.334311298238,-6.68697734938525,337.072502578512));
#71027=CARTESIAN_POINT('Ctrl Pts',(181.056073263964,-1.87589045730543,341.744772511905));
#71028=CARTESIAN_POINT('Ctrl Pts',(180.77783522969,4.6566684581192,340.227459444797));
#71029=CARTESIAN_POINT('Ctrl Pts',(180.499597195416,6.91587408932694,333.912986554537));
#71030=CARTESIAN_POINT('Ctrl Pts',(180.221359161143,2.82848275536695,328.59604850725));
#71031=CARTESIAN_POINT('Ctrl Pts',(179.943121126868,-3.85456471789821,329.155922938523));
#71032=CARTESIAN_POINT('Ctrl Pts',(179.664883092594,-7.00033543312608,335.078820251569));
#71033=CARTESIAN_POINT('Ctrl Pts',(179.38664505832,-3.72200143945353,340.929385583913));
#71034=CARTESIAN_POINT('Ctrl Pts',(179.108407024047,2.97195822908398,341.338641177155));
#71035=CARTESIAN_POINT('Ctrl Pts',(178.830168989773,6.93859575479861,335.931019376625));
#71036=CARTESIAN_POINT('Ctrl Pts',(178.5519309555,4.53778633913574,329.669014806167));
#71037=CARTESIAN_POINT('Ctrl Pts',(178.273692921225,-2.02728260607429,328.29917667867));
#71038=CARTESIAN_POINT('Ctrl Pts',(177.995454886951,-6.73194423494412,333.078585200804));
#71039=CARTESIAN_POINT('Ctrl Pts',(177.717216852677,-5.25879999817888,339.621247728553));
#71040=CARTESIAN_POINT('Ctrl Pts',(177.438978818404,1.04026737473892,341.923059422968));
#71041=CARTESIAN_POINT('Ctrl Pts',(177.16074078413,6.38469673345932,337.871681670357));
#71042=CARTESIAN_POINT('Ctrl Pts',(176.882502749856,5.86998413717594,331.185004034154));
#71043=CARTESIAN_POINT('Ctrl Pts',(176.604264715582,-0.0315262606111309,
327.999291886908));
#71044=CARTESIAN_POINT('Ctrl Pts',(176.326026681307,-5.90410547455225,331.238026244579));
#71045=CARTESIAN_POINT('Ctrl Pts',(176.047788647034,-6.35857423885009,337.929068391057));
#71046=CARTESIAN_POINT('Ctrl Pts',(175.76955061276,-0.977873276610438,341.932147707987));
#71047=CARTESIAN_POINT('Ctrl Pts',(175.491312578485,5.30020755821694,339.573697391659));
#71048=CARTESIAN_POINT('Ctrl Pts',(175.213074544211,6.714366147789,333.018032486652));
#71049=CARTESIAN_POINT('Ctrl Pts',(174.934836509937,1.96685002742494,328.281189914862));
#71050=CARTESIAN_POINT('Ctrl Pts',(174.656598475665,-4.58561533245236,329.710100188722));
#71051=CARTESIAN_POINT('Ctrl Pts',(174.37836044139,-6.92992918530729,335.993473440603));
#71052=CARTESIAN_POINT('Ctrl Pts',(174.100122407116,-2.914749310394,341.365150779684));
#71053=CARTESIAN_POINT('Ctrl Pts',(173.821884372842,3.77525298503917,340.895623197721));
#71054=CARTESIAN_POINT('Ctrl Pts',(173.543646338568,7.0007613387443,335.015769226465));
#71055=CARTESIAN_POINT('Ctrl Pts',(173.265408304295,3.80177434295197,329.121444068835));
#71056=CARTESIAN_POINT('Ctrl Pts',(172.98717027002,-2.88604485327017,328.621782921892));
#71057=CARTESIAN_POINT('Ctrl Pts',(172.708932235747,-6.92538328559842,333.975317445198));
#71058=CARTESIAN_POINT('Ctrl Pts',(172.430694201473,-4.60939969522278,340.269188024757));
#71059=CARTESIAN_POINT('Ctrl Pts',(172.152456167198,1.93656196083081,341.727602527083));
#71060=CARTESIAN_POINT('Ctrl Pts',(171.874218132924,6.70536928903767,337.012195489557));
#71061=CARTESIAN_POINT('Ctrl Pts',(171.59598009865,5.32075819178314,330.450226351219));
#71062=CARTESIAN_POINT('Ctrl Pts',(171.317742064377,-0.946634163808588,
328.06351733582));
#71063=CARTESIAN_POINT('Ctrl Pts',(171.039504030103,-6.34531431957053,332.042316079022));
#71064=CARTESIAN_POINT('Ctrl Pts',(170.76126599583,-5.92099318094844,338.735337701162));
#71065=CARTESIAN_POINT('Ctrl Pts',(170.483027961555,-0.0630639938860975,
342.000495048441));
#71066=CARTESIAN_POINT('Ctrl Pts',(170.204789927282,5.85273808954251,338.841401416901));
#71067=CARTESIAN_POINT('Ctrl Pts',(169.926551893006,6.39756881447056,332.157110404065));
#71068=CARTESIAN_POINT('Ctrl Pts',(169.648313858733,1.07144506631992,328.081697212435));
#71069=CARTESIAN_POINT('Ctrl Pts',(169.370075824459,-5.23792800468925,330.355108374972));
#71070=CARTESIAN_POINT('Ctrl Pts',(169.091837790186,-6.74053185748574,336.891068023309));
#71071=CARTESIAN_POINT('Ctrl Pts',(168.813599755911,-2.05744911475468,341.691622458773));
#71072=CARTESIAN_POINT('Ctrl Pts',(168.535361721638,4.51372431268757,340.351373732007));
#71073=CARTESIAN_POINT('Ctrl Pts',(168.257123687364,6.9427195608381,334.100248317525));
#71074=CARTESIAN_POINT('Ctrl Pts',(167.978885653089,3.00048354238029,328.674811741737));
#71075=CARTESIAN_POINT('Ctrl Pts',(167.700647618815,-3.69525193585539,329.053907070932));
#71076=CARTESIAN_POINT('Ctrl Pts',(167.422409584541,-6.99990925438579,334.889644116945));
#71077=CARTESIAN_POINT('Ctrl Pts',(167.144171550268,-3.88085316865759,340.826653127987));
#71078=CARTESIAN_POINT('Ctrl Pts',(166.865933515994,2.79960458864882,341.416628564735));
#71079=CARTESIAN_POINT('Ctrl Pts',(166.587695481719,6.91090653704819,336.118158676908));
#71080=CARTESIAN_POINT('Ctrl Pts',(166.309457447446,4.68017156121173,329.793571075277));
#71081=CARTESIAN_POINT('Ctrl Pts',(166.031219413172,-1.84548777712974,328.2468464511));
#71082=CARTESIAN_POINT('Ctrl Pts',(165.752981378897,-6.67757022175417,332.897391162365));
#71083=CARTESIAN_POINT('Ctrl Pts',(165.474743344624,-5.38174503464973,339.477468969471));
#71084=CARTESIAN_POINT('Ctrl Pts',(165.196505310349,0.852828136326283,341.948639590629));
#71085=CARTESIAN_POINT('Ctrl Pts',(164.918267276077,6.30477351431828,338.043146221218));
#71086=CARTESIAN_POINT('Ctrl Pts',(164.640029241802,5.97092129652498,331.345002481359));
#71087=CARTESIAN_POINT('Ctrl Pts',(164.361791207529,0.157642735564626,328.000996016683));
#71088=CARTESIAN_POINT('Ctrl Pts',(164.083553173255,-5.80030223702046,331.079872202367));
#71089=CARTESIAN_POINT('Ctrl Pts',(163.80531513898,-6.43539545901254,337.756191806947));
#71090=CARTESIAN_POINT('Ctrl Pts',(163.527077104706,-1.1648212545501,341.903194871616));
#71091=CARTESIAN_POINT('Ctrl Pts',(163.248839070432,5.17469222247944,339.715237893593));
#71092=CARTESIAN_POINT('Ctrl Pts',(162.970601036159,6.76546702527161,333.200176697417));
#71093=CARTESIAN_POINT('Ctrl Pts',(162.692363001885,2.14767259710162,328.336786780673));
#71094=CARTESIAN_POINT('Ctrl Pts',(162.414124967611,-4.44100927383294,329.588129286439));
#71095=CARTESIAN_POINT('Ctrl Pts',(162.135886933336,-6.95424248336044,335.805865666961));
#71096=CARTESIAN_POINT('Ctrl Pts',(161.857648899064,-3.08567001035892,341.284071019469));
#71097=CARTESIAN_POINT('Ctrl Pts',(161.579410864788,3.61457628673427,340.995477150148));
#71098=CARTESIAN_POINT('Ctrl Pts',(161.301172830515,6.99777927655,335.204922393233));
#71099=CARTESIAN_POINT('Ctrl Pts',(161.022934796242,3.9592235113286,329.226313380698));
#71100=CARTESIAN_POINT('Ctrl Pts',(160.744696761967,-2.71265323219581,328.546131359222));
#71101=CARTESIAN_POINT('Ctrl Pts',(160.466458727693,-6.89516814323021,333.788569330442));
#71102=CARTESIAN_POINT('Ctrl Pts',(160.188220693419,-4.75008902173721,340.142719346428));
#71103=CARTESIAN_POINT('Ctrl Pts',(159.909982659145,1.75407668380499,341.77747172461));
#71104=CARTESIAN_POINT('Ctrl Pts',(159.631744624871,6.64855210674876,337.192638336435));
#71105=CARTESIAN_POINT('Ctrl Pts',(159.353506590598,5.44174939379744,330.595653110203));
#71106=CARTESIAN_POINT('Ctrl Pts',(159.075268556323,-0.758866417752336,
328.040472016683));
#71107=CARTESIAN_POINT('Ctrl Pts',(158.79703052205,-6.26308171858079,331.871947030989));
#71108=CARTESIAN_POINT('Ctrl Pts',(158.518792487775,-6.01975936920231,338.573990084969));
#71109=CARTESIAN_POINT('Ctrl Pts',(158.240554453501,-0.252192698209519,
341.996235189982));
#71110=CARTESIAN_POINT('Ctrl Pts',(157.962316419228,5.74680748957203,338.998138525409));
#71111=CARTESIAN_POINT('Ctrl Pts',(157.684078384953,6.47204726691282,332.331009148498));
#71112=CARTESIAN_POINT('Ctrl Pts',(157.405840350679,1.2579847946688,328.113173281769));
#71113=CARTESIAN_POINT('Ctrl Pts',(157.127602316405,-5.11051175581766,330.215276644966));
#71114=CARTESIAN_POINT('Ctrl Pts',(156.849364282132,-6.78916709902012,336.708250008677));
#71115=CARTESIAN_POINT('Ctrl Pts',(156.571126247859,-2.23750400339395,341.633587553154));
#71116=CARTESIAN_POINT('Ctrl Pts',(156.292888213583,4.36748349064183,340.471379711693));
#71117=CARTESIAN_POINT('Ctrl Pts',(156.014650179311,6.96449584926633,334.288167466244));
#71118=CARTESIAN_POINT('Ctrl Pts',(155.736412145036,3.17029316280935,328.758193430391));
#71119=CARTESIAN_POINT('Ctrl Pts',(155.458174110763,-3.53324076570739,328.956233154555));
#71120=CARTESIAN_POINT('Ctrl Pts',(155.179936076489,-6.99437179408267,334.70054850693));
#71121=CARTESIAN_POINT('Ctrl Pts',(154.901698042215,-4.03687106378675,340.719666074599));
#71122=CARTESIAN_POINT('Ctrl Pts',(154.623460007941,2.62520665762704,341.489930507742));
#71123=CARTESIAN_POINT('Ctrl Pts',(154.345221973666,6.87817097732325,336.304481505147));
#71124=CARTESIAN_POINT('Ctrl Pts',(154.066983939393,4.81913931276712,329.921929079394));
#71125=CARTESIAN_POINT('Ctrl Pts',(153.788745905119,-1.6623453687357,328.199447385277));
#71126=CARTESIAN_POINT('Ctrl Pts',(153.510507870844,-6.61832024152719,332.7177324497));
#71127=CARTESIAN_POINT('Ctrl Pts',(153.23226983657,-5.50076031491589,339.330420758819));
#71128=CARTESIAN_POINT('Ctrl Pts',(152.954031802296,0.664766161604575,341.969145854475));
#71129=CARTESIAN_POINT('Ctrl Pts',(152.675793768022,6.22024654355298,338.212388663904));
#71130=CARTESIAN_POINT('Ctrl Pts',(152.397555733748,6.0674984831713,331.507669811247));
#71131=CARTESIAN_POINT('Ctrl Pts',(152.119317699474,0.346696620914136,328.0078108261));
#71132=CARTESIAN_POINT('Ctrl Pts',(151.841079665202,-5.6922636131222,330.924580641298));
#71133=CARTESIAN_POINT('Ctrl Pts',(151.562841630926,-6.50751754706949,337.581302648885));
#71134=CARTESIAN_POINT('Ctrl Pts',(151.284603596654,-1.35091867887267,341.869201315556));
#71135=CARTESIAN_POINT('Ctrl Pts',(151.00636556238,5.04539832139854,339.853335324186));
#71136=CARTESIAN_POINT('Ctrl Pts',(150.728127528106,6.81162775207952,333.383635140922));
#71137=CARTESIAN_POINT('Ctrl Pts',(150.449889493832,2.32692693413808,328.397249131329));
#71138=CARTESIAN_POINT('Ctrl Pts',(150.171651459557,-4.29316038587669,329.470110137471));
#71139=CARTESIAN_POINT('Ctrl Pts',(149.893413425284,-6.97347778671582,335.617669449416));
#71140=CARTESIAN_POINT('Ctrl Pts',(149.61517539101,-3.25433755104927,341.198402624417));
#71141=CARTESIAN_POINT('Ctrl Pts',(149.336937356736,3.45126022127169,341.090953199264));
#71142=CARTESIAN_POINT('Ctrl Pts',(149.058699322462,6.98968742904898,335.393925925467));
#71143=CARTESIAN_POINT('Ctrl Pts',(148.780461288187,4.11378165080535,329.335398644207));
#71144=CARTESIAN_POINT('Ctrl Pts',(148.502223253914,-2.5372808290647,328.475192417778));
#71145=CARTESIAN_POINT('Ctrl Pts',(148.22398521964,-6.85991814230574,333.602705803552));
#71146=CARTESIAN_POINT('Ctrl Pts',(147.945747185366,-4.88730982857861,340.012495449378));
#71147=CARTESIAN_POINT('Ctrl Pts',(147.667509151092,1.57031057826028,341.822392005622));
#71148=CARTESIAN_POINT('Ctrl Pts',(147.389271116818,6.58688014517586,337.371480116646));
#71149=CARTESIAN_POINT('Ctrl Pts',(147.111033082543,5.55876702505512,330.744295927614));
#71150=CARTESIAN_POINT('Ctrl Pts',(146.83279504827,-0.570544546691902,328.022508551721));
#71151=CARTESIAN_POINT('Ctrl Pts',(146.554557013996,-6.17627580916347,331.703862090309));
#71152=CARTESIAN_POINT('Ctrl Pts',(146.276318979723,-6.11412992324723,338.410032737704));
#71153=CARTESIAN_POINT('Ctrl Pts',(145.998080945448,-0.44113725117675,341.986866673709));
#71154=CARTESIAN_POINT('Ctrl Pts',(145.719842911175,5.63668056512349,339.151956189233));
#71155=CARTESIAN_POINT('Ctrl Pts',(145.4416048769,6.54179982407865,332.506856792673));
#71156=CARTESIAN_POINT('Ctrl Pts',(145.163366842627,1.44360594128398,328.149678118741));
#71157=CARTESIAN_POINT('Ctrl Pts',(144.885128808353,-4.97936380623825,330.078938724656));
#71158=CARTESIAN_POINT('Ctrl Pts',(144.606890774078,-6.83284488406494,336.524184628209));
#71159=CARTESIAN_POINT('Ctrl Pts',(144.328652739805,-2.41592506441045,341.570708795382));
#71160=CARTESIAN_POINT('Ctrl Pts',(144.05041470553,4.21805352785792,340.587390484536));
#71161=CARTESIAN_POINT('Ctrl Pts',(143.772176671257,6.98118665597922,334.47660639578));
#71162=CARTESIAN_POINT('Ctrl Pts',(143.493938636982,3.33778783205454,328.846132892339));
#71163=CARTESIAN_POINT('Ctrl Pts',(143.215700602708,-3.36864961967894,328.86297240267));
#71164=CARTESIAN_POINT('Ctrl Pts',(142.937462568435,-6.98372703661993,334.511671556691));
#71165=CARTESIAN_POINT('Ctrl Pts',(142.659224534161,-4.18994123169692,340.608502515421));
#71166=CARTESIAN_POINT('Ctrl Pts',(142.380986499886,2.44889179812317,341.558493497111));
#71167=CARTESIAN_POINT('Ctrl Pts',(142.102748465614,6.8404129703893,336.489851799707));
#71168=CARTESIAN_POINT('Ctrl Pts',(141.82451043134,4.95458812405912,330.053995095889));
#71169=CARTESIAN_POINT('Ctrl Pts',(141.546272397066,-1.47798911411928,328.15701408966));
#71170=CARTESIAN_POINT('Ctrl Pts',(141.268034362791,-6.55423755735398,332.539740251045));
#71171=CARTESIAN_POINT('Ctrl Pts',(140.989796328518,-5.61575893459271,339.18021047067));
#71172=CARTESIAN_POINT('Ctrl Pts',(140.711558294244,0.476218773978294,341.984563241168));
#71173=CARTESIAN_POINT('Ctrl Pts',(140.433320259969,6.13117754264699,338.37928541723));
#71174=CARTESIAN_POINT('Ctrl Pts',(140.155082225696,6.15964517646074,331.672887244071));
#71175=CARTESIAN_POINT('Ctrl Pts',(139.876844191421,0.535497348050235,328.019731338925));
#71176=CARTESIAN_POINT('Ctrl Pts',(139.598606157147,-5.58006849273806,330.772264955451));
#71177=CARTESIAN_POINT('Ctrl Pts',(139.320368122873,-6.5748878394166,337.404528621092));
#71178=CARTESIAN_POINT('Ctrl Pts',(139.042130088599,-1.53602966104794,341.830191861942));
#71179=CARTESIAN_POINT('Ctrl Pts',(138.763892054326,4.9124202655037,339.987888844554));
#71180=CARTESIAN_POINT('Ctrl Pts',(138.485654020052,6.85281462160694,333.568273855638));
#71181=CARTESIAN_POINT('Ctrl Pts',(138.207415985779,2.50448214683961,328.462532817158));
#71182=CARTESIAN_POINT('Ctrl Pts',(137.929177951504,-4.14217662798657,329.356128919516));
#71183=CARTESIAN_POINT('Ctrl Pts',(137.650939917231,-6.98762104973629,335.429022209032));
#71184=CARTESIAN_POINT('Ctrl Pts',(137.372701882957,-3.42062877126065,341.108208149678));
#71185=CARTESIAN_POINT('Ctrl Pts',(137.094463848682,3.28542404220298,341.181981628368));
#71186=CARTESIAN_POINT('Ctrl Pts',(136.816225814409,6.97649170491632,335.582641812605));
#71187=CARTESIAN_POINT('Ctrl Pts',(136.537987780135,4.26533590287672,329.448620205192));
#71188=CARTESIAN_POINT('Ctrl Pts',(136.259749745861,-2.3600557009781,328.409017897245));
#71189=CARTESIAN_POINT('Ctrl Pts',(135.981511711587,-6.81965902241038,333.417862582258));
#71190=CARTESIAN_POINT('Ctrl Pts',(135.703273677312,-5.0209619169788,339.878611423224));
#71191=CARTESIAN_POINT('Ctrl Pts',(135.425035643039,1.38539783038779,341.862330569284));
#71192=CARTESIAN_POINT('Ctrl Pts',(135.146797608765,6.52039843724598,337.548590239744));
#71193=CARTESIAN_POINT('Ctrl Pts',(134.868559574491,5.6717256391667,330.896046264323));
#71194=CARTESIAN_POINT('Ctrl Pts',(134.590321540217,-0.381806063442646,
328.009640057873));
#71195=CARTESIAN_POINT('Ctrl Pts',(134.312083505942,-6.08495997707894,331.538183992771));
#71196=CARTESIAN_POINT('Ctrl Pts',(134.033845471669,-6.20403593361193,338.243585381181));
#71197=CARTESIAN_POINT('Ctrl Pts',(133.755607437395,-0.62975968528953,341.972396340524));
#71198=CARTESIAN_POINT('Ctrl Pts',(133.477369403122,5.52243773098536,339.302742090568));
#71199=CARTESIAN_POINT('Ctrl Pts',(133.199131368848,6.60677555258225,332.684524932468));
#71200=CARTESIAN_POINT('Ctrl Pts',(132.920893334573,1.62817296542187,328.191185067485));
#71201=CARTESIAN_POINT('Ctrl Pts',(132.6426553003,-4.8445799203126,329.946194168128));
#71202=CARTESIAN_POINT('Ctrl Pts',(132.364417266025,-6.87153331905868,336.339006286627));
#71203=CARTESIAN_POINT('Ctrl Pts',(132.086179231752,-2.59258201457014,341.503032099589));
#71204=CARTESIAN_POINT('Ctrl Pts',(131.807941197478,4.0655435382416,340.699321339354));
#71205=CARTESIAN_POINT('Ctrl Pts',(131.529703163203,6.99277979333328,334.66542750784));
#71206=CARTESIAN_POINT('Ctrl Pts',(131.25146512893,3.50284524534358,328.938565914098));
#71207=CARTESIAN_POINT('Ctrl Pts',(130.973227094655,-3.20159868238686,328.774192914369));
#71208=CARTESIAN_POINT('Ctrl Pts',(130.694989060382,-6.96798275480997,334.32315118436));
#71209=CARTESIAN_POINT('Ctrl Pts',(130.416751026107,-4.33995190040084,340.493243622194));
#71210=CARTESIAN_POINT('Ctrl Pts',(130.138512991833,2.27078875542109,341.622267468082));
#71211=CARTESIAN_POINT('Ctrl Pts',(129.86027495756,6.79766008718017,336.674134203019));
#71212=CARTESIAN_POINT('Ctrl Pts',(129.582036923286,5.08641909023244,330.189672690026));
#71213=CARTESIAN_POINT('Ctrl Pts',(129.303798889013,-1.2925536303989,328.119577549082));
#71214=CARTESIAN_POINT('Ctrl Pts',(129.025560854738,-6.48536896247348,332.363544536476));
#71215=CARTESIAN_POINT('Ctrl Pts',(128.747322820465,-5.72665692157511,339.026947788727));
#71216=CARTESIAN_POINT('Ctrl Pts',(128.469084786191,0.287323650935115,341.994880492916));
#71217=CARTESIAN_POINT('Ctrl Pts',(128.190846751916,6.03763154987234,338.543714613022));
#71218=CARTESIAN_POINT('Ctrl Pts',(127.912608717642,6.24729409078729,331.840534137901));
#71219=CARTESIAN_POINT('Ctrl Pts',(127.634370683369,0.723907054496541,328.036748850787));
#71220=CARTESIAN_POINT('Ctrl Pts',(127.356132649094,-5.46379880085513,330.623036365888));
#71221=CARTESIAN_POINT('Ctrl Pts',(127.077894614821,-6.63745714220019,337.225998804136));
#71222=CARTESIAN_POINT('Ctrl Pts',(126.799656580547,-1.72001903285498,341.786194995516));
#71223=CARTESIAN_POINT('Ctrl Pts',(126.521418546272,4.77585515550195,340.118800203585));
#71224=CARTESIAN_POINT('Ctrl Pts',(126.243180511998,6.88899755916128,333.753958018191));
#71225=CARTESIAN_POINT('Ctrl Pts',(125.964942477725,2.6802085842156,328.532590167953));
#71226=CARTESIAN_POINT('Ctrl Pts',(125.68670444345,-3.98816824865087,329.246268861772));
#71227=CARTESIAN_POINT('Ctrl Pts',(125.408466409176,-6.99666194499731,335.24006169621));
#71228=CARTESIAN_POINT('Ctrl Pts',(125.130228374903,-3.58442224498074,341.013553455341));
#71229=CARTESIAN_POINT('Ctrl Pts',(124.851990340629,3.11718884326904,341.268495968409));
#71230=CARTESIAN_POINT('Ctrl Pts',(124.573752306356,6.95820173968273,335.770932254116));
#71231=CARTESIAN_POINT('Ctrl Pts',(124.29551427208,4.4137756024789,329.565895389163));
#71232=CARTESIAN_POINT('Ctrl Pts',(124.017276237808,-2.18110725789871,328.347656118321));
#71233=CARTESIAN_POINT('Ctrl Pts',(123.739038203534,-6.77442018079302,333.234174639263));
#71234=CARTESIAN_POINT('Ctrl Pts',(123.460800169259,-5.15094769405156,339.741165030212));
#71235=CARTESIAN_POINT('Ctrl Pts',(123.182562134986,1.19947346365769,341.897258252417));
#71236=CARTESIAN_POINT('Ctrl Pts',(122.904324100712,6.44915552796757,337.723839379744));
#71237=CARTESIAN_POINT('Ctrl Pts',(122.626086066438,5.78054275364118,331.050793312083));
#71238=CARTESIAN_POINT('Ctrl Pts',(122.347848032164,-0.192788785030493,
328.001875931728));
#71239=CARTESIAN_POINT('Ctrl Pts',(122.06960999789,-5.98920090123743,331.375033716685));
#71240=CARTESIAN_POINT('Ctrl Pts',(121.791371963616,-6.28941175083933,338.074769555423));
#71241=CARTESIAN_POINT('Ctrl Pts',(121.513133929341,-0.817922268261233,
341.952834756677));
#71242=CARTESIAN_POINT('Ctrl Pts',(121.234895895067,5.40416240738729,339.450386125398));
#71243=CARTESIAN_POINT('Ctrl Pts',(120.956657860793,6.66692700708289,332.863883834436));
#71244=CARTESIAN_POINT('Ctrl Pts',(120.67841982652,1.81155109605984,328.237663819586));
#71245=CARTESIAN_POINT('Ctrl Pts',(120.400181792245,-4.70625851736698,329.817139905586));
#71246=CARTESIAN_POINT('Ctrl Pts',(120.121943757973,-6.90520415366798,336.152850201338));
#71247=CARTESIAN_POINT('Ctrl Pts',(119.843705723699,-2.7673458587941,341.430606883365));
#71248=CARTESIAN_POINT('Ctrl Pts',(119.565467689425,3.91006488473719,340.807090544128));
#71249=CARTESIAN_POINT('Ctrl Pts',(119.287229655151,6.99926679600826,334.854492925062));
#71250=CARTESIAN_POINT('Ctrl Pts',(119.008991620877,3.66534487759111,329.035425000985));
#71251=CARTESIAN_POINT('Ctrl Pts',(118.730753586603,-3.03220993458969,328.689959516521));
#71252=CARTESIAN_POINT('Ctrl Pts',(118.452515552329,-6.9471504451428,334.135125047702));
#71253=CARTESIAN_POINT('Ctrl Pts',(118.174277518055,-4.48679353196085,340.373973557072));
#71254=CARTESIAN_POINT('Ctrl Pts',(117.896039483781,2.09102758053759,341.681205852838));
#71255=CARTESIAN_POINT('Ctrl Pts',(117.617801449507,6.74994354589319,336.85719415189));
#71256=CARTESIAN_POINT('Ctrl Pts',(117.339563415233,5.21453594818604,330.328862789894));
#71257=CARTESIAN_POINT('Ctrl Pts',(117.061325380959,-1.10617432274702,328.08716509974));
#71258=CARTESIAN_POINT('Ctrl Pts',(116.783087346685,-6.41176474480132,332.189273964279));
#71259=CARTESIAN_POINT('Ctrl Pts',(116.50484931241,-5.83337329804406,338.87074462555));
#71260=CARTESIAN_POINT('Ctrl Pts',(116.226611278137,0.0982187238792476,
342.000090076052));
#71261=CARTESIAN_POINT('Ctrl Pts',(115.948373243863,5.93967687260467,338.705556184921));
#71262=CARTESIAN_POINT('Ctrl Pts',(115.67013520959,6.33038122482778,332.010488076808));
#71263=CARTESIAN_POINT('Ctrl Pts',(115.391897175315,0.911788163300145,328.058850935484));
#71264=CARTESIAN_POINT('Ctrl Pts',(115.113659141041,-5.34353943771679,330.477003839475));
#71265=CARTESIAN_POINT('Ctrl Pts',(114.835421106768,-6.69517976725385,337.045843560665));
#71266=CARTESIAN_POINT('Ctrl Pts',(114.557183072494,-1.90275244507342,341.737242842834));
#71267=CARTESIAN_POINT('Ctrl Pts',(114.27894503822,4.63580271137082,340.245973809676));
#71268=CARTESIAN_POINT('Ctrl Pts',(114.000707003946,6.92015014392593,333.940552041823));
#71269=CARTESIAN_POINT('Ctrl Pts',(113.722468969672,2.8539779306489,328.607370027764));
#71270=CARTESIAN_POINT('Ctrl Pts',(113.444230935398,-3.83124770493942,329.140610184161));
#71271=CARTESIAN_POINT('Ctrl Pts',(113.165992901124,-7.00059387082826,335.050925890101));
#71272=CARTESIAN_POINT('Ctrl Pts',(112.88775486685,-3.74559837005416,340.914507658361));
#71273=CARTESIAN_POINT('Ctrl Pts',(112.609516832576,2.94667746997732,341.350433046532));
#71274=CARTESIAN_POINT('Ctrl Pts',(112.331278798301,6.93483088869879,335.95865976014));
#71275=CARTESIAN_POINT('Ctrl Pts',(112.053040764028,4.55899235879751,329.687138561661));
#71276=CARTESIAN_POINT('Ctrl Pts',(111.774802729754,-2.00056616815533,328.291151887441));
#71277=CARTESIAN_POINT('Ctrl Pts',(111.496564695481,-6.72423465090026,333.05177610368));
#71278=CARTESIAN_POINT('Ctrl Pts',(111.218326661206,-5.27717224405479,339.600256633835));
#71279=CARTESIAN_POINT('Ctrl Pts',(110.940088626933,1.01267324022512,341.927149550796));
#71280=CARTESIAN_POINT('Ctrl Pts',(110.661850592658,6.37320343898297,337.897099569552));
#71281=CARTESIAN_POINT('Ctrl Pts',(110.383612558385,5.88513891011469,331.208424074449));
#71282=CARTESIAN_POINT('Ctrl Pts',(110.105374524111,-0.00363073205790497,
327.999221842656));
#71283=CARTESIAN_POINT('Ctrl Pts',(109.827136489837,-5.88906850501048,331.214530394541));
#71284=CARTESIAN_POINT('Ctrl Pts',(109.548898455563,-6.37019503342358,337.903708529916));
#71285=CARTESIAN_POINT('Ctrl Pts',(109.270660421289,-1.00548760358844,341.928196206054));
#71286=CARTESIAN_POINT('Ctrl Pts',(108.992422387014,5.28194095908712,339.594780483906));
#71287=CARTESIAN_POINT('Ctrl Pts',(108.714184352741,6.72221026492919,333.044802530524));
#71288=CARTESIAN_POINT('Ctrl Pts',(108.435946318467,1.99360643030661,328.289080436214));
#71289=CARTESIAN_POINT('Ctrl Pts',(108.157708284192,-4.56450059982566,329.69187017258));
#71290=CARTESIAN_POINT('Ctrl Pts',(107.879470249919,-6.93383280141635,335.9658523037));
#71291=CARTESIAN_POINT('Ctrl Pts',(107.601232215645,-2.94008898435164,341.353486031673));
#71292=CARTESIAN_POINT('Ctrl Pts',(107.32299418137,3.75173109801029,340.910619405679));
#71293=CARTESIAN_POINT('Ctrl Pts',(107.044756147098,7.00064292718842,335.043664591693));
#71294=CARTESIAN_POINT('Ctrl Pts',(106.766518112823,3.82516807140595,329.1366394264));
#71295=CARTESIAN_POINT('Ctrl Pts',(106.48828007855,-2.86060706411756,328.610333716438));
#71296=CARTESIAN_POINT('Ctrl Pts',(106.210042044276,-6.92124531939146,333.947730443583));
#71297=CARTESIAN_POINT('Ctrl Pts',(105.931804010002,-4.63035890247325,340.250779411178));
#71298=CARTESIAN_POINT('Ctrl Pts',(105.653565975728,1.90973953525927,341.735265614511));
#71299=CARTESIAN_POINT('Ctrl Pts',(105.375327941454,6.69729818919371,337.038897975766));
#71300=CARTESIAN_POINT('Ctrl Pts',(105.09708990718,5.3388451468643,330.471463758743));
#71301=CARTESIAN_POINT('Ctrl Pts',(104.818851872906,-0.918987285517264,
328.059800409238));
#71302=CARTESIAN_POINT('Ctrl Pts',(104.540613838632,-6.33347865020975,332.017055786995));
#71303=CARTESIAN_POINT('Ctrl Pts',(104.262375804358,-5.93583013959639,338.711715040844));
#71304=CARTESIAN_POINT('Ctrl Pts',(103.984137770084,-0.0909579225846602,
342.000188186533));
#71305=CARTESIAN_POINT('Ctrl Pts',(103.70589973581,5.83738503744626,338.864691956051));
#71306=CARTESIAN_POINT('Ctrl Pts',(103.427661701535,6.40884590827468,332.182624960259));
#71307=CARTESIAN_POINT('Ctrl Pts',(103.149423667262,1.09900348349006,328.086021454053));
#71308=CARTESIAN_POINT('Ctrl Pts',(102.871185632988,-5.21937821682842,330.334274009303));
#71309=CARTESIAN_POINT('Ctrl Pts',(102.592947598715,-6.74801356545994,336.864194440215));
#71310=CARTESIAN_POINT('Ctrl Pts',(102.31470956444,-2.08409646558584,341.683371148806));
#71311=CARTESIAN_POINT('Ctrl Pts',(102.036471530166,4.49236519954295,340.369316800534));
#71312=CARTESIAN_POINT('Ctrl Pts',(101.758233495893,6.94624962825285,334.127919675399));
#71313=CARTESIAN_POINT('Ctrl Pts',(101.479995461619,3.02566329959154,328.686817792265));
#71314=CARTESIAN_POINT('Ctrl Pts',(101.201757427344,-3.67152958038781,329.039230038754));
#71315=CARTESIAN_POINT('Ctrl Pts',(100.923519393071,-6.99941395613305,334.861752897858));
#71316=CARTESIAN_POINT('Ctrl Pts',(100.645281358797,-3.90403945551564,340.811143082075));
#71317=CARTESIAN_POINT('Ctrl Pts',(100.367043324523,2.77401442990058,341.427733032202));
#71318=CARTESIAN_POINT('Ctrl Pts',(100.088805290249,6.90639621738289,336.145687251863));
#71319=CARTESIAN_POINT('Ctrl Pts',(99.8105672559745,4.70088013441401,329.812261190805));
#71320=CARTESIAN_POINT('Ctrl Pts',(99.5323292217006,-1.81856426302957,328.239546464046));
#71321=CARTESIAN_POINT('Ctrl Pts',(99.2540911874266,-6.66913907825543,332.870800163102));
#71322=CARTESIAN_POINT('Ctrl Pts',(98.9758531531527,-5.39954339769772,339.455989125541));
#71323=CARTESIAN_POINT('Ctrl Pts',(98.6976151188788,0.825133561797275,341.951982637763));
#71324=CARTESIAN_POINT('Ctrl Pts',(98.4193770846049,6.29259763058232,338.068244294405));
#71325=CARTESIAN_POINT('Ctrl Pts',(98.1411390503309,5.98543773237075,331.368823449284));
#71326=CARTESIAN_POINT('Ctrl Pts',(97.862901016057,0.185529972078658,328.001679728676));
#71327=CARTESIAN_POINT('Ctrl Pts',(97.5846629817831,-5.78463590517213,331.056791226025));
#71328=CARTESIAN_POINT('Ctrl Pts',(97.306424947509,-6.44632679333245,337.730527213584));
#71329=CARTESIAN_POINT('Ctrl Pts',(97.0281869132352,-1.19231873087909,341.898498679754));
#71330=CARTESIAN_POINT('Ctrl Pts',(96.7499488789612,5.15586263230639,339.735819729186));
#71331=CARTESIAN_POINT('Ctrl Pts',(96.4717108446873,6.772584958232,333.22714891373));
#71332=CARTESIAN_POINT('Ctrl Pts',(96.1934728104133,2.17420603117824,328.345397372904));
#71333=CARTESIAN_POINT('Ctrl Pts',(95.9152347761393,-4.4194096794594,329.570476441191));
#71334=CARTESIAN_POINT('Ctrl Pts',(95.6369967418656,-6.95739835763707,335.77814913976));
#71335=CARTESIAN_POINT('Ctrl Pts',(95.3587587075914,-3.11068525404265,341.271725858234));
#71336=CARTESIAN_POINT('Ctrl Pts',(95.0805206733176,3.59065779354763,341.009832327129));
#71337=CARTESIAN_POINT('Ctrl Pts',(94.8022826390436,6.9969071820214,335.232804374397));
#71338=CARTESIAN_POINT('Ctrl Pts',(94.5240446047697,3.98219812373486,329.242135283468));
#71339=CARTESIAN_POINT('Ctrl Pts',(94.2458065704957,-2.68691537555521,328.535373656956));
#71340=CARTESIAN_POINT('Ctrl Pts',(93.9675685362218,-6.8902862935042,333.761104207728));
#71341=CARTESIAN_POINT('Ctrl Pts',(93.6893305019479,-4.77054318036337,340.123751140995));
#71342=CARTESIAN_POINT('Ctrl Pts',(93.411092467674,1.72705699629501,341.784407278614));
#71343=CARTESIAN_POINT('Ctrl Pts',(93.1328544333999,6.63976245877293,337.219112994336));
#71344=CARTESIAN_POINT('Ctrl Pts',(92.8546163991262,5.45925591556819,330.61737146921));
#71345=CARTESIAN_POINT('Ctrl Pts',(92.576378364852,-0.731129202868262,328.037503459299));
#71346=CARTESIAN_POINT('Ctrl Pts',(92.2981403305784,-6.25056784328173,331.847015758509));
#71347=CARTESIAN_POINT('Ctrl Pts',(92.0199022963041,-6.0339526321459,338.549975158163));
#71348=CARTESIAN_POINT('Ctrl Pts',(91.7416642620304,-0.28006815148484,341.995174752719));
#71349=CARTESIAN_POINT('Ctrl Pts',(91.4634262277564,5.73083073799484,339.021005725314));
#71350=CARTESIAN_POINT('Ctrl Pts',(91.1851881934825,6.48263084613968,332.356819093736));
#71351=CARTESIAN_POINT('Ctrl Pts',(90.9069501592086,1.28541631025659,328.118240566549));
#71352=CARTESIAN_POINT('Ctrl Pts',(90.6287121249346,-5.09140580083534,330.194951096839));
#71353=CARTESIAN_POINT('Ctrl Pts',(90.3504740906606,-6.79591995752712,336.681184083152));
#71354=CARTESIAN_POINT('Ctrl Pts',(90.0722360563868,-2.2639186768104,341.624619250595));
#71355=CARTESIAN_POINT('Ctrl Pts',(89.7939980221127,4.34564735823031,340.488739110985));
#71356=CARTESIAN_POINT('Ctrl Pts',(89.5157599878389,6.96727695427295,334.315924102882));
#71357=CARTESIAN_POINT('Ctrl Pts',(89.2375219535649,3.19513932621856,328.77087544862));
#71358=CARTESIAN_POINT('Ctrl Pts',(88.9592839192909,-3.50913050132744,328.942202453431));
#71359=CARTESIAN_POINT('Ctrl Pts',(88.6810458850171,-6.99312306248656,334.672680853784));
#71360=CARTESIAN_POINT('Ctrl Pts',(88.402807850743,-4.05962980752896,340.703535203396));
#71361=CARTESIAN_POINT('Ctrl Pts',(88.1245698164692,2.59932580176022,341.500339480894));
#71362=CARTESIAN_POINT('Ctrl Pts',(87.8463317821953,6.87291848876,336.331878161628));
#71363=CARTESIAN_POINT('Ctrl Pts',(87.5680937479212,4.83933532273533,329.941171911925));
#71364=CARTESIAN_POINT('Ctrl Pts',(87.2898557136474,-1.63523444049127,328.192877530469));
#71365=CARTESIAN_POINT('Ctrl Pts',(87.0116176793733,-6.60917369369981,332.691378966339));
#71366=CARTESIAN_POINT('Ctrl Pts',(86.7333796450995,-5.51797179944384,339.308467849607));
#71367=CARTESIAN_POINT('Ctrl Pts',(86.4551416108254,0.636991370031486,341.971739380174));
#71368=CARTESIAN_POINT('Ctrl Pts',(86.1769035765517,6.20739696120613,338.237148584259));
#71369=CARTESIAN_POINT('Ctrl Pts',(85.8986655422775,6.08136598211088,331.531874312804));
#71370=CARTESIAN_POINT('Ctrl Pts',(85.6204275080038,0.374555202047226,328.009247795038));
#71371=CARTESIAN_POINT('Ctrl Pts',(85.3421894737298,-5.67597935850943,330.901931392432));
#71372=CARTESIAN_POINT('Ctrl Pts',(85.0639514394557,-6.51775143908,337.555352063598));
#71373=CARTESIAN_POINT('Ctrl Pts',(84.7857134051819,-1.37827922586039,341.863763862935));
#71374=CARTESIAN_POINT('Ctrl Pts',(84.5074753709079,5.02601948956327,339.873400874245));
#71375=CARTESIAN_POINT('Ctrl Pts',(84.229237336634,6.81801430334078,333.41078983454));
#71376=CARTESIAN_POINT('Ctrl Pts',(83.9509993023601,2.35321802466861,328.406573506974));
#71377=CARTESIAN_POINT('Ctrl Pts',(83.6727612680862,-4.27109170180083,329.453047353243));
#71378=CARTESIAN_POINT('Ctrl Pts',(83.3945232338121,-6.97588361473783,335.589877770553));
#71379=CARTESIAN_POINT('Ctrl Pts',(83.1162851995383,-3.27901009830331,341.185386064409));
#71380=CARTESIAN_POINT('Ctrl Pts',(82.8380471652642,3.42696258723445,341.104656863105));
#71381=CARTESIAN_POINT('Ctrl Pts',(82.5598091309904,6.98806228835202,335.421774163117));
#71382=CARTESIAN_POINT('Ctrl Pts',(82.2815710967164,4.13632037107925,329.351835539013));
#71383=CARTESIAN_POINT('Ctrl Pts',(82.0033330624425,-2.51126169874435,328.465134073986));
#71384=CARTESIAN_POINT('Ctrl Pts',(81.7250950281686,-6.85429597379216,333.575382614799));
#71385=CARTESIAN_POINT('Ctrl Pts',(81.4468569938946,-4.90724400293366,339.992981502693));
#71386=CARTESIAN_POINT('Ctrl Pts',(81.1686189596206,1.5431133586142,341.828594961853));
#71387=CARTESIAN_POINT('Ctrl Pts',(80.8903809253469,6.57737836727761,337.397707614416));
#71388=CARTESIAN_POINT('Ctrl Pts',(80.6121428910727,5.57568033023622,330.766479379337));
#71389=CARTESIAN_POINT('Ctrl Pts',(80.3339048567989,-0.542737248956215,
328.020290531178));
#71390=CARTESIAN_POINT('Ctrl Pts',(80.0556668225249,-6.16309286557018,331.679278042214));
#71391=CARTESIAN_POINT('Ctrl Pts',(79.7774287882509,-6.12766912655199,338.385643080134));
#71392=CARTESIAN_POINT('Ctrl Pts',(79.4991907539772,-0.46897387434508,341.985053435425));
#71393=CARTESIAN_POINT('Ctrl Pts',(79.220952719703,5.62009178030527,339.174383352245));
#71394=CARTESIAN_POINT('Ctrl Pts',(78.9427146854293,6.55168216058818,332.532943280508));
#71395=CARTESIAN_POINT('Ctrl Pts',(78.6644766511551,1.47089052476949,328.15548474655));
#71396=CARTESIAN_POINT('Ctrl Pts',(78.3862386168814,-4.9597156353216,330.059136835804));
#71397=CARTESIAN_POINT('Ctrl Pts',(78.1080005826073,-6.83886396216083,336.49694612382));
#71398=CARTESIAN_POINT('Ctrl Pts',(77.8297625483334,-2.44208777239169,341.561030048895));
#71399=CARTESIAN_POINT('Ctrl Pts',(77.5515245140595,4.19575632094487,340.604153538743));
#71400=CARTESIAN_POINT('Ctrl Pts',(77.2732864797855,6.98321676781211,334.504428043259));
#71401=CARTESIAN_POINT('Ctrl Pts',(76.9950484455116,3.36228225896871,328.859481617845));
#71402=CARTESIAN_POINT('Ctrl Pts',(76.7168104112377,-3.34416905172548,328.849598277832));
#71403=CARTESIAN_POINT('Ctrl Pts',(76.4385723769637,-6.98172578350548,334.483847818472));
#71404=CARTESIAN_POINT('Ctrl Pts',(76.1603343426898,-4.21225581386615,340.591762597706));
#71405=CARTESIAN_POINT('Ctrl Pts',(75.8820963084158,2.42273914336425,341.568199375306));
#71406=CARTESIAN_POINT('Ctrl Pts',(75.6038582741419,6.83442214830042,336.517096532651));
#71407=CARTESIAN_POINT('Ctrl Pts',(75.3256202398679,4.97425682364685,330.07377659429));
#71408=CARTESIAN_POINT('Ctrl Pts',(75.0473822055941,-1.45071056815708,328.151179164411));
#71409=CARTESIAN_POINT('Ctrl Pts',(74.76914417132,-6.54438228401613,332.513643526922));
#71410=CARTESIAN_POINT('Ctrl Pts',(74.4909061370462,-5.63237097275777,339.157800526215));
#71411=CARTESIAN_POINT('Ctrl Pts',(74.2126681027722,0.448384046541121,341.986405351636));
#71412=CARTESIAN_POINT('Ctrl Pts',(73.9344300684983,6.1176636444669,338.403689105034));
#71413=CARTESIAN_POINT('Ctrl Pts',(73.6561920342243,6.17285361243278,331.697457605112));
#71414=CARTESIAN_POINT('Ctrl Pts',(73.3779539999505,0.563306931439073,328.021920515531));
#71415=CARTESIAN_POINT('Ctrl Pts',(73.0997159656764,-5.56317820613959,330.750063972565));
#71416=CARTESIAN_POINT('Ctrl Pts',(72.8214779314026,-6.58441681631968,337.378310993021));
#71417=CARTESIAN_POINT('Ctrl Pts',(72.5432398971284,-1.56323329999609,341.824017118996));
#71418=CARTESIAN_POINT('Ctrl Pts',(72.2650018628548,4.89250634244821,340.007423457194));
#71419=CARTESIAN_POINT('Ctrl Pts',(71.9867638285806,6.85846512770305,333.595591198175));
#71420=CARTESIAN_POINT('Ctrl Pts',(71.7085257943068,2.53051169604413,328.47256416755));
#71421=CARTESIAN_POINT('Ctrl Pts',(71.4302877600328,-4.11965496878306,329.339668655569));
#71422=CARTESIAN_POINT('Ctrl Pts',(71.1520497257589,-6.98927507476571,335.401175672019));
#71423=CARTESIAN_POINT('Ctrl Pts',(70.8738116914849,-3.44494060616687,341.094529695599));
#71424=CARTESIAN_POINT('Ctrl Pts',(70.595573657211,3.26076500947132,341.19502377264));
#71425=CARTESIAN_POINT('Ctrl Pts',(70.3173356229371,6.97411470473025,335.610435971929));
#71426=CARTESIAN_POINT('Ctrl Pts',(70.0390975886631,4.2874222732228,329.465660089801));
#71427=CARTESIAN_POINT('Ctrl Pts',(69.7608595543893,-2.33377429617208,328.399666256538));
#71428=CARTESIAN_POINT('Ctrl Pts',(69.4826215201152,-6.81330064042213,333.390701278884));
#71429=CARTESIAN_POINT('Ctrl Pts',(69.2043834858414,-5.04036155110939,339.858565984389));
#71430=CARTESIAN_POINT('Ctrl Pts',(68.9261454515673,1.3580429380419,341.867796398335));
#71431=CARTESIAN_POINT('Ctrl Pts',(68.6479074172935,6.51019146763303,337.57455142604));
#71432=CARTESIAN_POINT('Ctrl Pts',(68.3696693830195,5.6880333776459,330.918678610382));
#71433=CARTESIAN_POINT('Ctrl Pts',(68.0914313487456,-0.353948987771852,
328.008174193774));
#71434=CARTESIAN_POINT('Ctrl Pts',(67.8131933144717,-6.07111759138985,331.513965120359));
#71435=CARTESIAN_POINT('Ctrl Pts',(67.5349552801977,-6.21691119093816,338.2188388022));
#71436=CARTESIAN_POINT('Ctrl Pts',(67.2567172459238,-0.657537152021269,
341.969831625245));
#71437=CARTESIAN_POINT('Ctrl Pts',(66.9784792116499,5.50524902607308,339.324712840349));
#71438=CARTESIAN_POINT('Ctrl Pts',(66.7002411773758,6.61594943028259,332.710868914521));
#71439=CARTESIAN_POINT('Ctrl Pts',(66.422003143102,1.6552906935753,328.197726798318));
#71440=CARTESIAN_POINT('Ctrl Pts',(66.1437651088279,-4.82440388057547,329.92693039791));
#71441=CARTESIAN_POINT('Ctrl Pts',(65.8655270745542,-6.87681422160667,336.311615092955));
#71442=CARTESIAN_POINT('Ctrl Pts',(65.58728904028,-2.61847365308096,341.492649976603));
#71443=CARTESIAN_POINT('Ctrl Pts',(65.3090510060063,4.04280153826938,340.715475808078));
#71444=CARTESIAN_POINT('Ctrl Pts',(65.0308129717322,6.99405742960281,334.693293850764));
#71445=CARTESIAN_POINT('Ctrl Pts',(64.7525749374583,3.52697004990818,328.952571599629));
#71446=CARTESIAN_POINT('Ctrl Pts',(64.4743369031844,-3.17676568659459,328.761485131617));
#71447=CARTESIAN_POINT('Ctrl Pts',(64.1960988689105,-6.96523044149417,334.295391677991));
#71448=CARTESIAN_POINT('Ctrl Pts',(63.9178608346364,-4.36180602686735,340.475906881471));
#71449=CARTESIAN_POINT('Ctrl Pts',(63.6396228003626,2.2443833984642,341.631263164078));
#71450=CARTESIAN_POINT('Ctrl Pts',(63.3613847660885,6.79093530606982,336.701207118295));
#71451=CARTESIAN_POINT('Ctrl Pts',(63.0831467318148,5.10554611733597,330.209978409827));
#71452=CARTESIAN_POINT('Ctrl Pts',(62.8049086975407,-1.26512738553993,328.11448181406));
#71453=CARTESIAN_POINT('Ctrl Pts',(62.5266706632668,-6.47481215995544,332.337723627447));
#71454=CARTESIAN_POINT('Ctrl Pts',(62.2484326289928,-5.74265738325067,339.004097172791));
#71455=CARTESIAN_POINT('Ctrl Pts',(61.970194594719,0.259449312579205,341.995969843042));
#71456=CARTESIAN_POINT('Ctrl Pts',(61.6919565604449,6.02346320372072,338.567744248679));
#71457=CARTESIAN_POINT('Ctrl Pts',(61.4137185261711,6.25983381897889,331.865452417122));
#71458=CARTESIAN_POINT('Ctrl Pts',(61.1354804918971,0.751647333555837,328.039688636525));
#71459=CARTESIAN_POINT('Ctrl Pts',(60.8572424576232,-5.44631481557494,330.601299860162));
#71460=CARTESIAN_POINT('Ctrl Pts',(60.5790044233492,-6.64627424592751,337.199533277421));
#71461=CARTESIAN_POINT('Ctrl Pts',(60.3007663890754,-1.74704589963946,341.779287471048));
#71462=CARTESIAN_POINT('Ctrl Pts',(60.0225283548013,4.75542068239251,340.137789614614));
#71463=CARTESIAN_POINT('Ctrl Pts',(59.7442903205275,6.89390789408709,333.781418062499));
#71464=CARTESIAN_POINT('Ctrl Pts',(59.4660522862535,2.70595758529176,328.543321168189));
#71465=CARTESIAN_POINT('Ctrl Pts',(59.1878142519796,-3.96521005965715,329.230423137408));
#71466=CARTESIAN_POINT('Ctrl Pts',(58.9095762177056,-6.99756295926346,335.212180634613));
#71467=CARTESIAN_POINT('Ctrl Pts',(58.6313381834317,-3.60835561501372,340.999223095215));
#71468=CARTESIAN_POINT('Ctrl Pts',(58.3531001491577,3.09218641789253,341.280867069725));
#71469=CARTESIAN_POINT('Ctrl Pts',(58.0748621148839,6.95507461569553,335.798652039796));
#71470=CARTESIAN_POINT('Ctrl Pts',(57.7966240806098,4.43539349540778,329.583525821029));
#71471=CARTESIAN_POINT('Ctrl Pts',(57.518386046336,-2.15458276931499,328.339018009277));
#71472=CARTESIAN_POINT('Ctrl Pts',(57.240148012062,-6.76733022822695,333.207195054478));
#71473=CARTESIAN_POINT('Ctrl Pts',(56.961909977788,-5.16979862232547,339.720602736427));
#71474=CARTESIAN_POINT('Ctrl Pts',(56.6836719435141,1.17198087318151,341.901982963139));
#71475=CARTESIAN_POINT('Ctrl Pts',(56.4054339092402,6.43825081977916,337.74951529768));
#71476=CARTESIAN_POINT('Ctrl Pts',(56.1271958749663,5.7962330174918,331.073858026319));
#71477=CARTESIAN_POINT('Ctrl Pts',(55.8489578406922,-0.164902272688679,
328.001163294445));
#71478=CARTESIAN_POINT('Ctrl Pts',(55.5707198064184,-5.97470918117631,331.351197704598));
#71479=CARTESIAN_POINT('Ctrl Pts',(55.2924817721444,-6.3016136606614,338.049684125008));
#71480=CARTESIAN_POINT('Ctrl Pts',(55.0142437378705,-0.845620295422691,
341.949520437162));
#71481=CARTESIAN_POINT('Ctrl Pts',(54.7360057035965,5.38638633359033,339.471884418886));
#71482=CARTESIAN_POINT('Ctrl Pts',(54.4577676693226,6.67538572719945,332.890466074303));
#71483=CARTESIAN_POINT('Ctrl Pts',(54.1795296350486,1.83848216748947,328.244935876664));
#71484=CARTESIAN_POINT('Ctrl Pts',(53.9012916007747,-4.68556934137328,329.798428320426));
#71485=CARTESIAN_POINT('Ctrl Pts',(53.6230535665008,-6.9097430245479,336.125326319462));
#71486=CARTESIAN_POINT('Ctrl Pts',(53.3448155322269,-2.79294752173477,341.419528964915));
#71487=CARTESIAN_POINT('Ctrl Pts',(53.0665774979529,3.88689469793651,340.82262463136));
#71488=CARTESIAN_POINT('Ctrl Pts',(52.788339463679,6.99979102378316,334.882383615403));
#71489=CARTESIAN_POINT('Ctrl Pts',(52.510101429405,3.68908244385015,329.050077419576));
#71490=CARTESIAN_POINT('Ctrl Pts',(52.2318633951311,-3.00704264403653,328.677927355091));
#71491=CARTESIAN_POINT('Ctrl Pts',(51.9536253608571,-6.94364908136755,334.107450043199));
#71492=CARTESIAN_POINT('Ctrl Pts',(51.6753873265832,-4.50817124482002,340.356052652648));
#71493=CARTESIAN_POINT('Ctrl Pts',(51.3971492923092,2.06438880260035,341.689484797969));
#71494=CARTESIAN_POINT('Ctrl Pts',(51.1189112580354,6.74248971620314,336.884075480828));
#71495=CARTESIAN_POINT('Ctrl Pts',(50.8406732237614,5.23310733623141,330.349677903839));
#71496=CARTESIAN_POINT('Ctrl Pts',(50.5624351894875,-1.07862040566223,328.082812275856));
#71497=CARTESIAN_POINT('Ctrl Pts',(50.2841971552135,-6.40051412169072,332.163747724796));
#71498=CARTESIAN_POINT('Ctrl Pts',(50.0059591209396,-5.84875049967723,338.847470023676));
#71499=CARTESIAN_POINT('Ctrl Pts',(49.7277210866656,0.0703251284742021,
342.000425870393));
#71500=CARTESIAN_POINT('Ctrl Pts',(49.4494830523918,5.92486442422205,338.729194221966));
#71501=CARTESIAN_POINT('Ctrl Pts',(49.1712450181177,6.34224308871686,332.035736078859));
#71502=CARTESIAN_POINT('Ctrl Pts',(48.8930069838439,0.939438882050772,328.062539183717));
#71503=CARTESIAN_POINT('Ctrl Pts',(48.6147689495699,-5.32547452057817,330.455747682926));
#71504=CARTESIAN_POINT('Ctrl Pts',(48.336530915296,-6.70327855954755,337.019149460459));
#71505=CARTESIAN_POINT('Ctrl Pts',(48.058292881022,-1.9295828046498,341.729607580726));
#71506=CARTESIAN_POINT('Ctrl Pts',(47.7800548467481,4.61486260947957,340.264404153007));
#71507=CARTESIAN_POINT('Ctrl Pts',(47.5018168124742,6.92431672215013,333.968134736551));
#71508=CARTESIAN_POINT('Ctrl Pts',(47.2235787782002,2.8794275816508,328.618792842057));
#71509=CARTESIAN_POINT('Ctrl Pts',(46.9453407439263,-3.80786975024803,329.125390569943));
#71510=CARTESIAN_POINT('Ctrl Pts',(46.6671027096523,-7.00074121640962,335.023030662701));
#71511=CARTESIAN_POINT('Ctrl Pts',(46.3888646753784,-3.76913579904309,340.899535856229));
#71512=CARTESIAN_POINT('Ctrl Pts',(46.1106266411045,2.92134990875209,341.362124071503));
#71513=CARTESIAN_POINT('Ctrl Pts',(45.8323886068305,6.93095592433945,335.986284931156));
#71514=CARTESIAN_POINT('Ctrl Pts',(45.5541505725566,4.58012598890224,329.705346667029));
#71515=CARTESIAN_POINT('Ctrl Pts',(45.2759125382826,-1.97381796400176,328.283233617615));
#71516=CARTESIAN_POINT('Ctrl Pts',(44.9976745040087,-6.71641830484675,333.024997938006));
#71517=CARTESIAN_POINT('Ctrl Pts',(44.7194364697347,-5.29546070150554,339.579192499707));
#71518=CARTESIAN_POINT('Ctrl Pts',(44.4411984354609,0.985063026735457,341.931129693197));
#71519=CARTESIAN_POINT('Ctrl Pts',(44.1629604011869,6.36160895484778,337.922471470547));
#71520=CARTESIAN_POINT('Ctrl Pts',(43.884722366913,5.90020024229054,331.231904314985));
#71521=CARTESIAN_POINT('Ctrl Pts',(43.606484332639,0.0242648541961058,327.999262952559));
#71522=CARTESIAN_POINT('Ctrl Pts',(43.3282462983651,-5.87393803244544,331.191094647862));
#71523=CARTESIAN_POINT('Ctrl Pts',(43.0500082640912,-6.38171468589505,337.87830256547));
#71524=CARTESIAN_POINT('Ctrl Pts',(42.7717702298172,-1.03308596605334,341.924134702423));
#71525=CARTESIAN_POINT('Ctrl Pts',(42.4935321955433,5.2635904965114,339.615790623024));
#71526=CARTESIAN_POINT('Ctrl Pts',(42.2152941612694,6.72994765089654,333.071603617833));
#71527=CARTESIAN_POINT('Ctrl Pts',(41.9370561269954,2.02033117991846,328.297077509473));
#71528=CARTESIAN_POINT('Ctrl Pts',(41.6588180927215,-4.54331339483144,329.673724435696));
#71529=CARTESIAN_POINT('Ctrl Pts',(41.3805800584475,-6.93762632634033,335.938215831582));
#71530=CARTESIAN_POINT('Ctrl Pts',(41.1023420241736,-2.96538197736341,341.341720406868));
#71531=CARTESIAN_POINT('Ctrl Pts',(40.8241039898996,3.72814964327367,340.925521768411));
#71532=CARTESIAN_POINT('Ctrl Pts',(40.5458659556258,7.00041336367703,335.071559263642));
#71533=CARTESIAN_POINT('Ctrl Pts',(40.2676279213517,3.84850106616587,329.15192787884));
#71534=CARTESIAN_POINT('Ctrl Pts',(39.9893898870779,-2.8351238559831,328.598985962225));
#71535=CARTESIAN_POINT('Ctrl Pts',(39.7111518528039,-6.91699746185588,333.920160149263));
#71536=CARTESIAN_POINT('Ctrl Pts',(39.43291381853,-4.65124459169871,340.232287428912));
#71537=CARTESIAN_POINT('Ctrl Pts',(39.154675784256,1.88288678800273,341.742821763484));
#71538=CARTESIAN_POINT('Ctrl Pts',(38.8764377499821,6.68912075371751,337.065568089594));
#71539=CARTESIAN_POINT('Ctrl Pts',(38.5981997157081,5.35684733500621,330.492773067617));
#71540=CARTESIAN_POINT('Ctrl Pts',(38.3199616814342,-0.891325816103229,
328.056193674929));
#71541=CARTESIAN_POINT('Ctrl Pts',(38.0417236471602,-6.32154242172221,331.991842856344));
#71542=CARTESIAN_POINT('Ctrl Pts',(37.7634856128864,-5.95057285273992,338.688033448167));
#71543=CARTESIAN_POINT('Ctrl Pts',(37.4852475786124,-0.118850407109541,
341.999770179891));
#71544=CARTESIAN_POINT('Ctrl Pts',(37.2070095443385,5.82193930289614,338.887921133968));
#71545=CARTESIAN_POINT('Ctrl Pts',(36.9287715100645,6.42002124631727,332.208184249024));
#71546=CARTESIAN_POINT('Ctrl Pts',(36.6505334757906,1.12654445135132,328.090455471618));
#71547=CARTESIAN_POINT('Ctrl Pts',(36.3722954415166,-5.2007455588509,330.313513723198));
#71548=CARTESIAN_POINT('Ctrl Pts',(36.0940574072427,-6.75538813257426,336.837291258574));
#71549=CARTESIAN_POINT('Ctrl Pts',(35.8158193729687,-2.11071072639963,341.675013724332));
#71550=CARTESIAN_POINT('Ctrl Pts',(35.5375813386949,4.4709347593527,340.38717461831));
#71551=CARTESIAN_POINT('Ctrl Pts',(35.2593433044208,6.94966940733592,334.155604879633));
#71552=CARTESIAN_POINT('Ctrl Pts',(34.981105270147,3.05079501715928,328.698924079665));
#71553=CARTESIAN_POINT('Ctrl Pts',(34.702867235873,-3.64774893060379,329.024647648059));
#71554=CARTESIAN_POINT('Ctrl Pts',(34.4246292015991,-6.99880752543772,334.833863873775));
#71555=CARTESIAN_POINT('Ctrl Pts',(34.1463911673251,-3.9271637564072,340.795540770361));
#71556=CARTESIAN_POINT('Ctrl Pts',(33.8681531330512,2.74838022703619,341.43873544403));
#71557=CARTESIAN_POINT('Ctrl Pts',(33.5899150987772,6.90177624215411,336.17319763629));
#71558=CARTESIAN_POINT('Ctrl Pts',(33.3116770645033,4.72151406989757,329.831033674098));
#71559=CARTESIAN_POINT('Ctrl Pts',(33.0334390302294,-1.79161187487054,328.232353815365));
#71560=CARTESIAN_POINT('Ctrl Pts',(32.7552009959554,-6.66060204621789,332.844242969981));
#71561=CARTESIAN_POINT('Ctrl Pts',(32.4769629616815,-5.41725603007612,339.43443853212));
#71562=CARTESIAN_POINT('Ctrl Pts',(32.1987249274076,0.79742588629856,341.955215305542));
#71563=CARTESIAN_POINT('Ctrl Pts',(31.9204868931336,6.28032183680384,338.093293651873));
#71564=CARTESIAN_POINT('Ctrl Pts',(31.6422488588597,5.9998591350726,331.392702070823));
#71565=CARTESIAN_POINT('Ctrl Pts',(31.3640108245857,0.213414262860903,328.002474555747));
#71566=CARTESIAN_POINT('Ctrl Pts',(31.0857727903118,-5.76887772838889,331.033772857557));
#71567=CARTESIAN_POINT('Ctrl Pts',(30.8075347560379,-6.4571557767919,337.704819266569));
#71568=CARTESIAN_POINT('Ctrl Pts',(30.5292967217639,-1.21979727629601,341.89369295772));
#71569=CARTESIAN_POINT('Ctrl Pts',(30.25105868749,5.13695118047843,339.756326372311));
#71570=CARTESIAN_POINT('Ctrl Pts',(29.9728206532161,6.77959536020297,333.254149278297));
#71571=CARTESIAN_POINT('Ctrl Pts',(29.6945826189421,2.20070494453272,328.354113622873));
#71572=CARTESIAN_POINT('Ctrl Pts',(29.4163445846682,-4.39773991638346,329.55290980262));
#71573=CARTESIAN_POINT('Ctrl Pts',(29.1381065503942,-6.9604437665693,335.75042025758));
#71574=CARTESIAN_POINT('Ctrl Pts',(28.8598685161203,-3.13565110815609,341.259281118346));
#71575=CARTESIAN_POINT('Ctrl Pts',(28.5816304818463,3.56668229007748,341.024092083642));
#71576=CARTESIAN_POINT('Ctrl Pts',(28.3033924475724,6.99592399485125,335.260682659234));
#71577=CARTESIAN_POINT('Ctrl Pts',(28.0251544132985,4.00510950921894,329.258048606115));
#71578=CARTESIAN_POINT('Ctrl Pts',(27.7469163790245,-2.66113485770415,328.524718596103));
#71579=CARTESIAN_POINT('Ctrl Pts',(27.4686783447506,-6.88529504399824,333.733658755447));
#71580=CARTESIAN_POINT('Ctrl Pts',(27.1904403104767,-4.79092159520341,340.104701583755));
#71581=CARTESIAN_POINT('Ctrl Pts',(26.9122022762027,1.70000988762276,341.79123511392));
#71582=CARTESIAN_POINT('Ctrl Pts',(26.6339642419288,6.63086738868234,337.245552418509));
#71583=CARTESIAN_POINT('Ctrl Pts',(26.3557262076548,5.47667575859036,330.639159412931));
#71584=CARTESIAN_POINT('Ctrl Pts',(26.077488173381,-0.7033803795583,328.034645448205));
#71585=CARTESIAN_POINT('Ctrl Pts',(25.7992501391069,-6.23795472526369,331.822134547197));
#71586=CARTESIAN_POINT('Ctrl Pts',(25.5210121048331,-6.04805009165541,338.525903867009));
#71587=CARTESIAN_POINT('Ctrl Pts',(25.2427740705591,-0.307939158007984,
341.994003250322));
#71588=CARTESIAN_POINT('Ctrl Pts',(24.9645360362852,5.71476299576885,339.043809082135));
#71589=CARTESIAN_POINT('Ctrl Pts',(24.6862980020112,6.49311149809216,332.382671005795));
#71590=CARTESIAN_POINT('Ctrl Pts',(24.4080599677373,1.31282741678491,328.123417115725));
#71591=CARTESIAN_POINT('Ctrl Pts',(24.1298219334633,-5.07221900760495,330.174701840357));
#71592=CARTESIAN_POINT('Ctrl Pts',(23.8515838991894,-6.80256491454558,336.654091464809));
#71593=CARTESIAN_POINT('Ctrl Pts',(23.5733458649154,-2.29029740510129,341.615545766355));
#71594=CARTESIAN_POINT('Ctrl Pts',(23.2951078306416,4.32374222827016,340.506011363414));
#71595=CARTESIAN_POINT('Ctrl Pts',(23.0168697963675,6.96994743708876,334.34369160086));
#71596=CARTESIAN_POINT('Ctrl Pts',(22.7386317620937,3.21993475914654,328.783656369104));
#71597=CARTESIAN_POINT('Ctrl Pts',(22.4603937278197,-3.48496452110532,328.928267934336));
#71598=CARTESIAN_POINT('Ctrl Pts',(22.1821556935458,-6.99176329833085,334.644818397613));
#71599=CARTESIAN_POINT('Ctrl Pts',(21.9039176592718,-4.08232409493527,340.687313774926));
#71600=CARTESIAN_POINT('Ctrl Pts',(21.6256796249979,2.57340367537753,341.510645245605));
#71601=CARTESIAN_POINT('Ctrl Pts',(21.3474415907239,6.86755687617236,336.359253671357));
#71602=CARTESIAN_POINT('Ctrl Pts',(21.06920355645,4.85945449667722,329.960495065457));
#71603=CARTESIAN_POINT('Ctrl Pts',(20.7909655221761,-1.6080975489873,328.186415755015));
#71604=CARTESIAN_POINT('Ctrl Pts',(20.5127274879022,-6.59992220942738,332.665062137858));
#71605=CARTESIAN_POINT('Ctrl Pts',(20.2344894536283,-5.53509567296828,339.286446533161));
#71606=CARTESIAN_POINT('Ctrl Pts',(19.9562514193543,0.609206464695599,341.974222212831));
#71607=CARTESIAN_POINT('Ctrl Pts',(19.6780133850804,6.19444882158101,338.261857107137));
#71608=CARTESIAN_POINT('Ctrl Pts',(19.3997753508064,6.09513692481626,331.556133879155));
#71609=CARTESIAN_POINT('Ctrl Pts',(19.1215373165325,0.40240783622117,328.010795758893));
#71610=CARTESIAN_POINT('Ctrl Pts',(18.8432992822585,-5.65960498414416,330.87934721021));
#71611=CARTESIAN_POINT('Ctrl Pts',(18.5650612479846,-6.52788184619303,337.529360905981));
#71612=CARTESIAN_POINT('Ctrl Pts',(18.2868232137106,-1.40561788936867,341.85821743164));
#71613=CARTESIAN_POINT('Ctrl Pts',(18.0085851794367,5.00656085764329,339.893389047406));
#71614=CARTESIAN_POINT('Ctrl Pts',(17.7303471451628,6.82429260231311,333.437969760673));
#71615=CARTESIAN_POINT('Ctrl Pts',(17.4521091108888,2.3794717522339,328.41600256904));
#71616=CARTESIAN_POINT('Ctrl Pts',(17.1738710766149,-4.24895520392486,329.436072640157));
#71617=CARTESIAN_POINT('Ctrl Pts',(16.895633042341,-6.97817868391783,335.562076725969));
#71618=CARTESIAN_POINT('Ctrl Pts',(16.617395008067,-3.30363058342786,341.172271296598));
#71619=CARTESIAN_POINT('Ctrl Pts',(16.3391569737931,3.40261054196623,341.118263600914));
#71620=CARTESIAN_POINT('Ctrl Pts',(16.0609189395192,6.98632619544743,335.449615704094));
#71621=CARTESIAN_POINT('Ctrl Pts',(15.7826809052452,4.15879341737169,329.368362111944));
#71622=CARTESIAN_POINT('Ctrl Pts',(15.5044428709713,-2.48520269613499,328.455179486824));
#71623=CARTESIAN_POINT('Ctrl Pts',(15.2262048366973,-6.84856497693183,333.548082045253));
#71624=CARTESIAN_POINT('Ctrl Pts',(14.9479668024234,-4.92710026304873,339.973388280481));
#71625=CARTESIAN_POINT('Ctrl Pts',(14.6697287681495,1.51589163834792,341.834689497799));
#71626=CARTESIAN_POINT('Ctrl Pts',(14.3914907338755,6.56777215776715,337.423897042843));
#71627=CARTESIAN_POINT('Ctrl Pts',(14.1132526996016,5.59250510814167,330.788730048326));
#71628=CARTESIAN_POINT('Ctrl Pts',(13.8350146653276,-0.514921333947683,
328.018183330228));
#71629=CARTESIAN_POINT('Ctrl Pts',(13.5567766310537,-6.14981206817078,331.654746718514));
#71630=CARTESIAN_POINT('Ctrl Pts',(13.2785385967797,-6.14111103837664,338.361199667403));
#71631=CARTESIAN_POINT('Ctrl Pts',(13.0003005625058,-0.496803051568086,
341.983129292665));
#71632=CARTESIAN_POINT('Ctrl Pts',(12.7220625282319,5.60341376334212,339.196744237014));
#71633=CARTESIAN_POINT('Ctrl Pts',(12.443824493958,6.56146047298106,332.559068938624));
#71634=CARTESIAN_POINT('Ctrl Pts',(12.165586459684,1.49815175526964,328.161400047695));
#71635=CARTESIAN_POINT('Ctrl Pts',(11.8873484254101,-4.93998871879135,330.039413394447));
#71636=CARTESIAN_POINT('Ctrl Pts',(11.6091103911361,-6.84477445364715,336.469683852826));
#71637=CARTESIAN_POINT('Ctrl Pts',(11.3308723568622,-2.46821171258475,341.551247128476));
#71638=CARTESIAN_POINT('Ctrl Pts',(11.0526343225883,4.17339250806404,340.620827617158));
#71639=CARTESIAN_POINT('Ctrl Pts',(10.7743962883143,6.98513598227502,334.532257552422));
#71640=CARTESIAN_POINT('Ctrl Pts',(10.4961582540404,3.3867233433309,328.872927851433));
#71641=CARTESIAN_POINT('Ctrl Pts',(10.2179202197665,-3.31963546586816,328.836321781429));
#71642=CARTESIAN_POINT('Ctrl Pts',(9.9396821854925,-6.97961353003579,334.456032320548));
#71643=CARTESIAN_POINT('Ctrl Pts',(9.66144415121862,-4.23450379727599,340.574933812142));
#71644=CARTESIAN_POINT('Ctrl Pts',(9.38320611694463,2.39654855218155,341.577801128574));
#71645=CARTESIAN_POINT('Ctrl Pts',(9.10496808267072,6.82832181198693,336.544316874147));
#71646=CARTESIAN_POINT('Ctrl Pts',(8.82673004839677,4.9938484358946,330.09363688212));
#71647=CARTESIAN_POINT('Ctrl Pts',(8.54849201412284,-1.4234125590739,328.145451897039));
#71648=CARTESIAN_POINT('Ctrl Pts',(8.2702539798489,-6.53441636134746,332.487588325599));
#71649=CARTESIAN_POINT('Ctrl Pts',(7.99201594557494,-5.64890631307911,339.135320703576));
#71650=CARTESIAN_POINT('Ctrl Pts',(7.71377791130103,0.420566235859593,341.988143830623));
#71651=CARTESIAN_POINT('Ctrl Pts',(7.43553987702708,6.1040072290099,338.428024977785));
#71652=CARTESIAN_POINT('Ctrl Pts',(7.15730184275314,6.18604973530199,331.722106408789));
#71653=CARTESIAN_POINT('Ctrl Pts',(6.8790638084792,0.590945759089165,328.024171379594));
#71654=CARTESIAN_POINT('Ctrl Pts',(6.60082577420527,-5.54589404922238,330.728023190032));
#71655=CARTESIAN_POINT('Ctrl Pts',(6.32258773993133,-6.59441823814528,337.351880525878));
#71656=CARTESIAN_POINT('Ctrl Pts',(6.04434970565737,-1.58932212683603,341.818064601347));
#71657=CARTESIAN_POINT('Ctrl Pts',(5.76611167138347,4.87045235443919,340.026254453026));
#71658=CARTESIAN_POINT('Ctrl Pts',(5.48787363710948,6.86793575564766,333.624108657021));
#71659=CARTESIAN_POINT('Ctrl Pts',(5.20963560283559,2.5487975662465,328.480480750959));
#71660=CARTESIAN_POINT('Ctrl Pts',(4.97777057427396,-2.97535607058049,329.186249754624));
#71661=CARTESIAN_POINT('Ctrl Pts',(4.79227855142465,-5.56135735959864,332.348719775238));
#71662=CARTESIAN_POINT('Ctrl Pts',(4.69953254000002,-5.96441153797609,334.331397335507));
#71663=CARTESIAN_POINT('Ctrl Pts',(4.65315953428771,-5.9118477353294,335.315703728026));
#71664=CARTESIAN_POINT('Ctrl Pts',(5.23167681249931,2.54972650148121,329.651773033606));
#71665=CARTESIAN_POINT('Ctrl Pts',(5.23167681249913,2.41800456025,329.600786237743));
#71666=CARTESIAN_POINT('Ctrl Pts',(5.23167681249913,2.28466063361559,329.554959909234));
#71667=CARTESIAN_POINT('Ctrl Pts',(5.23167681249924,2.14986992676735,329.514508295526));
#71668=CARTESIAN_POINT('Ctrl Pts',(5.23167681249934,1.9939798467528,329.467724615515));
#71669=CARTESIAN_POINT('Ctrl Pts',(5.23167681249914,1.83615434792712,329.428128731723));
#71670=CARTESIAN_POINT('Ctrl Pts',(5.23167681249919,1.67684153369454,329.39557219129));
#71671=CARTESIAN_POINT('Ctrl Pts',(5.23167681249925,1.51476829684993,329.362451541745));
#71672=CARTESIAN_POINT('Ctrl Pts',(5.23167681249897,1.3511549534905,329.336616380309));
#71673=CARTESIAN_POINT('Ctrl Pts',(5.23167681249917,1.18647141068386,329.317964639992));
#71674=CARTESIAN_POINT('Ctrl Pts',(5.23167681249938,1.02229982133636,329.299370882536));
#71675=CARTESIAN_POINT('Ctrl Pts',(5.23167681249934,0.857063874684294,329.287916213189));
#71676=CARTESIAN_POINT('Ctrl Pts',(5.23167681249924,0.69123933862632,329.283550047204));
#71677=CARTESIAN_POINT('Ctrl Pts',(5.23167681249917,0.60435650777413,329.28126241915));
#71678=CARTESIAN_POINT('Ctrl Pts',(5.23167681249934,0.517312342263204,329.280921526507));
#71679=CARTESIAN_POINT('Ctrl Pts',(5.23167681249914,0.430177521044325,329.282525300652));
#71680=CARTESIAN_POINT('Ctrl Pts',(5.23167681249905,0.404341844458899,329.283000823406));
#71681=CARTESIAN_POINT('Ctrl Pts',(5.23167681249918,0.378498210928564,329.283647332065));
#71682=CARTESIAN_POINT('Ctrl Pts',(5.23167681249927,0.352648497412946,329.28446483084));
#71683=CARTESIAN_POINT('Ctrl Pts',(5.23167681249934,0.333502347151716,329.285070329016));
#71684=CARTESIAN_POINT('Ctrl Pts',(5.23167681249895,0.314356581885818,329.285769540827));
#71685=CARTESIAN_POINT('Ctrl Pts',(5.23167681249896,0.29522010113727,329.286561951824));
#71686=CARTESIAN_POINT('Ctrl Pts',(5.23167681249928,0.132424129356062,329.293303072094));
#71687=CARTESIAN_POINT('Ctrl Pts',(5.23167681249911,-0.0298768216824351,
329.306790091531));
#71688=CARTESIAN_POINT('Ctrl Pts',(5.23167681249905,-0.191242176401267,
329.326890528971));
#71689=CARTESIAN_POINT('Ctrl Pts',(5.23167681249897,-0.352490232216596,
329.346976355101));
#71690=CARTESIAN_POINT('Ctrl Pts',(5.23167681249913,-0.512804836598123,
329.373666256176));
#71691=CARTESIAN_POINT('Ctrl Pts',(5.231676812499,-0.671735302422305,329.406878795084));
#71692=CARTESIAN_POINT('Ctrl Pts',(5.23167681249886,-0.829399809068293,
329.439826779817));
#71693=CARTESIAN_POINT('Ctrl Pts',(5.23167681249914,-0.985702858372395,
329.479194206026));
#71694=CARTESIAN_POINT('Ctrl Pts',(5.23167681249911,-1.14018237932099,329.524947201073));
#71695=CARTESIAN_POINT('Ctrl Pts',(5.23167681249913,-1.29176664913119,329.569842694685));
#71696=CARTESIAN_POINT('Ctrl Pts',(5.23167681249886,-1.44159568927443,329.620886982488));
#71697=CARTESIAN_POINT('Ctrl Pts',(5.23167681249887,-1.58920207264907,329.6780873439));
#71698=CARTESIAN_POINT('Ctrl Pts',(5.23167681249886,-1.63376575171165,329.695356641406));
#71699=CARTESIAN_POINT('Ctrl Pts',(5.23167681249898,-1.67812658882095,329.713187315508));
#71700=CARTESIAN_POINT('Ctrl Pts',(5.23167681249908,-1.72227103140139,329.731580219596));
#71701=CARTESIAN_POINT('Ctrl Pts',(5.23167681249914,-1.74269662266794,329.740090598687));
#71702=CARTESIAN_POINT('Ctrl Pts',(5.23167681249896,-1.76307588106098,329.748721349947));
#71703=CARTESIAN_POINT('Ctrl Pts',(5.23167681249893,-1.78340743812514,329.757472579012));
#71704=CARTESIAN_POINT('Ctrl Pts',(5.2316768124989,-1.80175923588897,329.765371668367));
#71705=CARTESIAN_POINT('Ctrl Pts',(5.23167681249882,-1.82006330253293,329.773365104279));
#71706=CARTESIAN_POINT('Ctrl Pts',(5.2316768124988,-1.83831746521071,329.781452110194));
#71707=CARTESIAN_POINT('Ctrl Pts',(5.23167681249883,-1.98233092296423,329.845253321194));
#71708=CARTESIAN_POINT('Ctrl Pts',(5.23167681249912,-2.12326805205457,329.914886745487));
#71709=CARTESIAN_POINT('Ctrl Pts',(5.23167681249902,-2.26071365305021,329.990282849218));
#71710=CARTESIAN_POINT('Ctrl Pts',(5.23167681249892,-2.39524127464768,330.064078288571));
#71711=CARTESIAN_POINT('Ctrl Pts',(5.23167681249882,-2.52642458879079,330.143394699649));
#71712=CARTESIAN_POINT('Ctrl Pts',(5.2316768124988,-2.65384554720594,330.228206595191));
#71713=CARTESIAN_POINT('Ctrl Pts',(5.23167681249879,-2.78009118683411,330.312236193885));
#71714=CARTESIAN_POINT('Ctrl Pts',(5.23167681249893,-2.90264409733492,330.401660629697));
#71715=CARTESIAN_POINT('Ctrl Pts',(5.23167681249907,-3.02106112099374,330.496489900504));
#71716=CARTESIAN_POINT('Ctrl Pts',(5.23167681249913,-3.06951763393609,330.535294251823));
#71717=CARTESIAN_POINT('Ctrl Pts',(5.23167681249888,-3.11728113419466,330.575004008348));
#71718=CARTESIAN_POINT('Ctrl Pts',(5.23167681249888,-3.16431914920114,330.615621404147));
#71719=CARTESIAN_POINT('Ctrl Pts',(5.23167681249886,-3.24767930945342,330.687603026296));
#71720=CARTESIAN_POINT('Ctrl Pts',(5.23167681249914,-3.32876163279295,330.762435095702));
#71721=CARTESIAN_POINT('Ctrl Pts',(5.23167681249899,-3.4074669648841,330.839968817051));
#71722=CARTESIAN_POINT('Ctrl Pts',(5.23167681249894,-3.43520704029975,330.867295952587));
#71723=CARTESIAN_POINT('Ctrl Pts',(5.23167681249884,-3.46265172518095,330.894958735291));
#71724=CARTESIAN_POINT('Ctrl Pts',(5.23167681249889,-3.48979631081915,330.92295075014));
#71725=CARTESIAN_POINT('Ctrl Pts',(5.23167681249892,-3.50731669470894,330.941018104438));
#71726=CARTESIAN_POINT('Ctrl Pts',(5.2316768124991,-3.52471423933795,330.959225054822));
#71727=CARTESIAN_POINT('Ctrl Pts',(5.23167681249907,-3.54197006666573,330.977550883116));
#71728=CARTESIAN_POINT('Ctrl Pts',(5.23167681249883,-3.64657636679153,331.088643620552));
#71729=CARTESIAN_POINT('Ctrl Pts',(5.23167681249895,-3.74611177326817,331.204237309737));
#71730=CARTESIAN_POINT('Ctrl Pts',(5.23167681249889,-3.84040442081676,331.323872703633));
#71731=CARTESIAN_POINT('Ctrl Pts',(5.23167681249883,-3.9352794679761,331.444247026901));
#71732=CARTESIAN_POINT('Ctrl Pts',(5.23167681249906,-4.02484714647093,331.568713946577));
#71733=CARTESIAN_POINT('Ctrl Pts',(5.23167681249906,-4.10888757179936,331.696834186031));
#71734=CARTESIAN_POINT('Ctrl Pts',(5.23167681249907,-4.19217159231138,331.823801280843));
#71735=CARTESIAN_POINT('Ctrl Pts',(5.23167681249912,-4.27002763524665,331.954357048025));
#71736=CARTESIAN_POINT('Ctrl Pts',(5.23167681249907,-4.34219365759432,332.08808963197));
#71737=CARTESIAN_POINT('Ctrl Pts',(5.23167681249902,-4.40188475268049,332.198704629509));
#71738=CARTESIAN_POINT('Ctrl Pts',(5.23167681249893,-4.45768221768303,332.311493540761));
#71739=CARTESIAN_POINT('Ctrl Pts',(5.23167681249896,-4.50941085668205,332.426225627016));
#71740=CARTESIAN_POINT('Ctrl Pts',(5.23167681249896,-4.53597814258197,332.485150821965));
#71741=CARTESIAN_POINT('Ctrl Pts',(5.23167681249895,-4.56147177056669,332.54458857805));
#71742=CARTESIAN_POINT('Ctrl Pts',(5.23167681249904,-4.58586534653017,332.604507433144));
#71743=CARTESIAN_POINT('Ctrl Pts',(5.23167681249908,-4.59440157528401,332.625475291834));
#71744=CARTESIAN_POINT('Ctrl Pts',(5.23167681249906,-4.60280385876661,332.646504055389));
#71745=CARTESIAN_POINT('Ctrl Pts',(5.23167681249904,-4.61106852320073,332.667586003979));
#71746=CARTESIAN_POINT('Ctrl Pts',(5.23167681249897,-4.62531373153314,332.703923444186));
#71747=CARTESIAN_POINT('Ctrl Pts',(5.23167681249907,-4.63914236795992,332.740398919073));
#71748=CARTESIAN_POINT('Ctrl Pts',(5.23167681249909,-4.65255058106541,332.77700510479));
#71749=CARTESIAN_POINT('Ctrl Pts',(5.23167681249902,-4.70421003064279,332.918042198278));
#71750=CARTESIAN_POINT('Ctrl Pts',(5.23167681249893,-4.74963264388488,333.061019116744));
#71751=CARTESIAN_POINT('Ctrl Pts',(5.23167681249899,-4.78874025475357,333.205562400287));
#71752=CARTESIAN_POINT('Ctrl Pts',(5.23167681249905,-4.82772255338508,333.349642524823));
#71753=CARTESIAN_POINT('Ctrl Pts',(5.23167681249904,-4.86043026958429,333.495279716321));
#71754=CARTESIAN_POINT('Ctrl Pts',(5.23167681249911,-4.88673444228786,333.642104028461));
#71755=CARTESIAN_POINT('Ctrl Pts',(5.2316768124991,-4.8986962336663,333.708872210487));
#71756=CARTESIAN_POINT('Ctrl Pts',(5.23167681249901,-4.90933308743962,333.775885817694));
#71757=CARTESIAN_POINT('Ctrl Pts',(5.23167681249898,-4.91862931835759,333.843109441235));
#71758=CARTESIAN_POINT('Ctrl Pts',(5.23167681249898,-4.92292145082778,333.874147041302));
#71759=CARTESIAN_POINT('Ctrl Pts',(5.23167681249906,-4.92692776730969,333.90522940348));
#71760=CARTESIAN_POINT('Ctrl Pts',(5.23167681249906,-4.9306465628392,333.936352997078));
#71761=CARTESIAN_POINT('Ctrl Pts',(5.23167681249907,-4.93342662939924,333.959620117064));
#71762=CARTESIAN_POINT('Ctrl Pts',(5.23167681249907,-4.93604591532386,333.98291004826));
#71763=CARTESIAN_POINT('Ctrl Pts',(5.23167681249907,-4.93850239243566,334.006207207835));
#71764=CARTESIAN_POINT('Ctrl Pts',(5.23167681249908,-4.95383544263047,334.151625422982));
#71765=CARTESIAN_POINT('Ctrl Pts',(5.23167681249901,-4.96284677660462,334.297465472424));
#71766=CARTESIAN_POINT('Ctrl Pts',(5.23167681249902,-4.96543576666754,334.44337495279));
#71767=CARTESIAN_POINT('Ctrl Pts',(5.23167681249896,-4.96798156936119,334.5868504931));
#71768=CARTESIAN_POINT('Ctrl Pts',(5.231676812499,-4.96431738792226,334.730393784283));
#71769=CARTESIAN_POINT('Ctrl Pts',(5.23167681249896,-4.95429886920134,334.873659727518));
#71770=CARTESIAN_POINT('Ctrl Pts',(5.23167681249894,-4.94521819965126,335.003514322247));
#71771=CARTESIAN_POINT('Ctrl Pts',(5.23167681249898,-4.93091661054929,335.133141271392));
#71772=CARTESIAN_POINT('Ctrl Pts',(5.23167681249902,-4.9112521298426,335.262270050933));
#71773=CARTESIAN_POINT('Ctrl Pts',(185.810302217248,3.4387199488324,339.81938086493));
#71774=CARTESIAN_POINT('Ctrl Pts',(185.763919407556,4.24130745050852,339.246723531428));
#71775=CARTESIAN_POINT('Ctrl Pts',(185.671163592151,5.54038606962475,337.695271231453));
#71776=CARTESIAN_POINT('Ctrl Pts',(185.485661765322,6.40062453626914,333.701383153881));
#71777=CARTESIAN_POINT('Ctrl Pts',(185.25379673676,3.50809689585563,328.942276555623));
#71778=CARTESIAN_POINT('Ctrl Pts',(184.975558702486,-3.20644657449587,328.772433974797));
#71779=CARTESIAN_POINT('Ctrl Pts',(184.697320668212,-6.96652177174833,334.325929885673));
#71780=CARTESIAN_POINT('Ctrl Pts',(184.419082633938,-4.33975135453482,340.493702333227));
#71781=CARTESIAN_POINT('Ctrl Pts',(184.140844599664,2.27283062225682,341.622249810224));
#71782=CARTESIAN_POINT('Ctrl Pts',(183.86260656539,6.79793088994909,336.672459105425));
#71783=CARTESIAN_POINT('Ctrl Pts',(183.584368531116,5.08559089065535,330.188511195752));
#71784=CARTESIAN_POINT('Ctrl Pts',(183.306130496843,-1.29420832154675,328.119659895712));
#71785=CARTESIAN_POINT('Ctrl Pts',(183.027892462568,-6.48607347215639,332.364972912782));
#71786=CARTESIAN_POINT('Ctrl Pts',(182.749654428295,-5.72590146837062,339.028317254472));
#71787=CARTESIAN_POINT('Ctrl Pts',(182.47141639402,0.288918215035514,341.994984166663));
#71788=CARTESIAN_POINT('Ctrl Pts',(182.193178359747,6.03856356499396,338.542430950412));
#71789=CARTESIAN_POINT('Ctrl Pts',(181.914940325473,6.24672857174619,331.839055121086));
#71790=CARTESIAN_POINT('Ctrl Pts',(181.636702291199,0.722352212805145,328.03642434573));
#71791=CARTESIAN_POINT('Ctrl Pts',(181.358464256925,-5.46491041299496,330.624168088303));
#71792=CARTESIAN_POINT('Ctrl Pts',(181.080226222651,-6.63710843185237,337.227546111849));
#71793=CARTESIAN_POINT('Ctrl Pts',(180.801988188377,-1.71852840848146,341.786739047181));
#71794=CARTESIAN_POINT('Ctrl Pts',(180.523750154103,4.77711892367299,340.1178411484));
#71795=CARTESIAN_POINT('Ctrl Pts',(180.245512119829,6.8888751779057,333.752376275502));
#71796=CARTESIAN_POINT('Ctrl Pts',(179.967274085555,2.67881212365101,328.531837116266));
#71797=CARTESIAN_POINT('Ctrl Pts',(179.689036051281,-3.98955715157227,329.24703565205));
#71798=CARTESIAN_POINT('Ctrl Pts',(179.410798017007,-6.99676878113797,335.241644610499));
#71799=CARTESIAN_POINT('Ctrl Pts',(179.132559982733,-3.58314893713384,341.014499900835));
#71800=CARTESIAN_POINT('Ctrl Pts',(178.854321948459,3.11867378061391,341.267937393193));
#71801=CARTESIAN_POINT('Ctrl Pts',(178.576083914186,6.95853561133084,335.769381261229));
#71802=CARTESIAN_POINT('Ctrl Pts',(178.297845879911,4.41265201410948,329.56477529828));
#71803=CARTESIAN_POINT('Ctrl Pts',(178.019607845638,-2.18265720304945,328.347994822222));
#71804=CARTESIAN_POINT('Ctrl Pts',(177.741369811363,-6.7749741224064,333.235661313365));
#71805=CARTESIAN_POINT('Ctrl Pts',(177.46313177709,-5.14999728730718,339.742435376173));
#71806=CARTESIAN_POINT('Ctrl Pts',(177.184893742816,1.20105604410647,341.897146492214));
#71807=CARTESIAN_POINT('Ctrl Pts',(176.906655708542,6.44991797161996,337.722448074217));
#71808=CARTESIAN_POINT('Ctrl Pts',(176.628417674268,5.77978537709548,331.0493992417));
#71809=CARTESIAN_POINT('Ctrl Pts',(176.350179639994,-0.194370948435958,
328.001758414345));
#71810=CARTESIAN_POINT('Ctrl Pts',(176.07194160572,-5.99015592353064,331.376300596248));
#71811=CARTESIAN_POINT('Ctrl Pts',(175.793703571446,-6.28886322214059,338.07625823527));
#71812=CARTESIAN_POINT('Ctrl Pts',(175.515465537172,-0.816373565270258,
341.953179097276));
#71813=CARTESIAN_POINT('Ctrl Pts',(175.237227502899,5.40529006279934,339.449270130471));
#71814=CARTESIAN_POINT('Ctrl Pts',(174.958989468624,6.666598782186,332.86233163605));
#71815=CARTESIAN_POINT('Ctrl Pts',(174.680751434351,1.81006819799868,328.237099847294));
#71816=CARTESIAN_POINT('Ctrl Pts',(174.402513400076,-4.70753525492994,329.818081708433));
#71817=CARTESIAN_POINT('Ctrl Pts',(174.124275365803,-6.90510308751545,336.154433500756));
#71818=CARTESIAN_POINT('Ctrl Pts',(173.846037331528,-2.76595973584276,341.431378708844));
#71819=CARTESIAN_POINT('Ctrl Pts',(173.567799297255,3.91146403991415,340.806342602822));
#71820=CARTESIAN_POINT('Ctrl Pts',(173.28956126298,6.99939499935638,334.852911591665));
#71821=CARTESIAN_POINT('Ctrl Pts',(173.011323228707,3.66408447879018,329.034461441817));
#71822=CARTESIAN_POINT('Ctrl Pts',(172.733085194433,-3.03370228616353,328.690497975607));
#71823=CARTESIAN_POINT('Ctrl Pts',(172.454847160159,-6.94750524047731,334.136671389087));
#71824=CARTESIAN_POINT('Ctrl Pts',(172.176609125885,-4.48568518061436,340.375108726091));
#71825=CARTESIAN_POINT('Ctrl Pts',(171.898371091611,2.09258196089365,341.680888121637));
#71826=CARTESIAN_POINT('Ctrl Pts',(171.620133057337,6.75051752334867,336.855715097703));
#71827=CARTESIAN_POINT('Ctrl Pts',(171.341895023063,5.21360279210196,330.327579718918));
#71828=CARTESIAN_POINT('Ctrl Pts',(171.063656988789,-1.1077582688056,328.087255467271));
#71829=CARTESIAN_POINT('Ctrl Pts',(170.785418954515,-6.41254591691553,332.190654841367));
#71830=CARTESIAN_POINT('Ctrl Pts',(170.507180920241,-5.83263482609468,338.872148801675));
#71831=CARTESIAN_POINT('Ctrl Pts',(170.228942885967,0.0997991550843282,
342.000228959508));
#71832=CARTESIAN_POINT('Ctrl Pts',(169.950704851693,5.94064892467557,338.704302324411));
#71833=CARTESIAN_POINT('Ctrl Pts',(169.672466817419,6.32985285992645,332.008992121615));
#71834=CARTESIAN_POINT('Ctrl Pts',(169.394228783146,0.910244254097873,328.058485701609));
#71835=CARTESIAN_POINT('Ctrl Pts',(169.115990748871,-5.34468206853313,330.478104496654));
#71836=CARTESIAN_POINT('Ctrl Pts',(168.837752714598,-6.69487254424932,337.047400052051));
#71837=CARTESIAN_POINT('Ctrl Pts',(168.559514680324,-1.90127730226469,341.737826799257));
#71838=CARTESIAN_POINT('Ctrl Pts',(168.28127664605,4.63709205720122,340.245049342945));
#71839=CARTESIAN_POINT('Ctrl Pts',(168.003038611776,6.92007047914019,333.938967521414));
#71840=CARTESIAN_POINT('Ctrl Pts',(167.724800577502,2.85260236244514,328.606579544669));
#71841=CARTESIAN_POINT('Ctrl Pts',(167.446562543228,-3.83265683792397,329.141339153049));
#71842=CARTESIAN_POINT('Ctrl Pts',(167.168324508954,-7.00074342805247,335.052505346985));
#71843=CARTESIAN_POINT('Ctrl Pts',(166.89008647468,-3.74435110506085,340.915488158969));
#71844=CARTESIAN_POINT('Ctrl Pts',(166.611848440406,2.9481769605134,341.349914799931));
#71845=CARTESIAN_POINT('Ctrl Pts',(166.333610406132,6.9352065444451,335.957118353584));
#71846=CARTESIAN_POINT('Ctrl Pts',(166.055372371858,4.55789944602034,329.685988521198));
#71847=CARTESIAN_POINT('Ctrl Pts',(165.777134337584,-2.00212469953175,328.291448588227));
#71848=CARTESIAN_POINT('Ctrl Pts',(165.498896303311,-6.72482855963568,333.053247267784));
#71849=CARTESIAN_POINT('Ctrl Pts',(165.220658269036,-5.27625650886877,339.601552195673));
#71850=CARTESIAN_POINT('Ctrl Pts',(164.942420234763,1.01425826266857,341.927080592391));
#71851=CARTESIAN_POINT('Ctrl Pts',(164.664182200489,6.3740031969824,337.895729373015));
#71852=CARTESIAN_POINT('Ctrl Pts',(164.385944166214,5.88441947755844,331.207010048917));
#71853=CARTESIAN_POINT('Ctrl Pts',(164.107706131941,-0.00520914253163273,
327.999061618489));
#71854=CARTESIAN_POINT('Ctrl Pts',(163.829468097667,-5.8900574094073,331.215771007091));
#71855=CARTESIAN_POINT('Ctrl Pts',(163.551230063393,-6.36968692877479,337.905211487359));
#71856=CARTESIAN_POINT('Ctrl Pts',(163.272992029119,-1.00394877003062,341.928582266528));
#71857=CARTESIAN_POINT('Ctrl Pts',(162.994753994845,5.28309835671109,339.593695365411));
#71858=CARTESIAN_POINT('Ctrl Pts',(162.716515960571,6.72192409990297,333.04324203029));
#71859=CARTESIAN_POINT('Ctrl Pts',(162.438277926297,1.99213931205097,328.288476602271));
#71860=CARTESIAN_POINT('Ctrl Pts',(162.160039892023,-4.56580231854216,329.692777134426));
#71861=CARTESIAN_POINT('Ctrl Pts',(161.881801857749,-6.9337745525409,335.967437755836));
#71862=CARTESIAN_POINT('Ctrl Pts',(161.603563823475,-2.93872422201748,341.354295028075));
#71863=CARTESIAN_POINT('Ctrl Pts',(161.325325789201,3.75314995155296,340.909909542289));
#71864=CARTESIAN_POINT('Ctrl Pts',(161.047087754927,7.00081381098573,335.042087299667));
#71865=CARTESIAN_POINT('Ctrl Pts',(160.768849720653,3.8239341679194,329.135642163348));
#71866=CARTESIAN_POINT('Ctrl Pts',(160.490611686379,-2.86211341987065,328.610831655945));
#71867=CARTESIAN_POINT('Ctrl Pts',(160.212373652106,-6.92164176697034,333.949266633911));
#71868=CARTESIAN_POINT('Ctrl Pts',(159.934135617832,-4.62928162778639,340.251944113139));
#71869=CARTESIAN_POINT('Ctrl Pts',(159.655897583558,1.91130193313229,341.734989998306));
#71870=CARTESIAN_POINT('Ctrl Pts',(159.377659549284,6.69791192078577,337.03743497032));
#71871=CARTESIAN_POINT('Ctrl Pts',(159.09942151501,5.33794699975203,330.47015594256));
#71872=CARTESIAN_POINT('Ctrl Pts',(158.821183480736,-0.920573094985571,
328.059847945927));
#71873=CARTESIAN_POINT('Ctrl Pts',(158.542945446462,-6.33429684809153,332.018415052839));
#71874=CARTESIAN_POINT('Ctrl Pts',(158.264707412188,-5.9351298777721,338.713138657639));
#71875=CARTESIAN_POINT('Ctrl Pts',(157.986469377914,-0.0893818209946288,
342.000369722162));
#71876=CARTESIAN_POINT('Ctrl Pts',(157.70823134364,5.83839061363612,338.863464817943));
#71877=CARTESIAN_POINT('Ctrl Pts',(157.429993309366,6.40835815663718,332.181115274946));
#71878=CARTESIAN_POINT('Ctrl Pts',(157.151755275092,1.09747000650366,328.08561463746));
#71879=CARTESIAN_POINT('Ctrl Pts',(156.873517240818,-5.22055016996747,330.335343391017));
#71880=CARTESIAN_POINT('Ctrl Pts',(156.595279206544,-6.74774851065374,336.865758664419));
#71881=CARTESIAN_POINT('Ctrl Pts',(156.31704117227,-2.08263763971794,341.683994750036));
#71882=CARTESIAN_POINT('Ctrl Pts',(156.038803137996,4.49367905350588,340.368427509146));
#71883=CARTESIAN_POINT('Ctrl Pts',(155.760565103723,6.94621280592146,334.126333580974));
#71884=CARTESIAN_POINT('Ctrl Pts',(155.482327069449,3.02430959227587,328.685990430246));
#71885=CARTESIAN_POINT('Ctrl Pts',(155.204089035175,-3.67295789546487,329.039920667053));
#71886=CARTESIAN_POINT('Ctrl Pts',(154.925851000901,-6.99960613530717,334.863327737078));
#71887=CARTESIAN_POINT('Ctrl Pts',(154.647612966627,-3.90281913879529,340.812156925509));
#71888=CARTESIAN_POINT('Ctrl Pts',(154.369374932353,2.77552737587297,341.427255490694));
#71889=CARTESIAN_POINT('Ctrl Pts',(154.091136898079,6.90681338441952,336.144156558206));
#71890=CARTESIAN_POINT('Ctrl Pts',(153.812898863805,4.69981869448273,329.811082039975));
#71891=CARTESIAN_POINT('Ctrl Pts',(153.534660829531,-1.82013024217066,328.239800945355));
#71892=CARTESIAN_POINT('Ctrl Pts',(153.256422795257,-6.6697725206623,332.872254742809));
#71893=CARTESIAN_POINT('Ctrl Pts',(152.978184760983,-5.39866300262332,339.457308957317));
#71894=CARTESIAN_POINT('Ctrl Pts',(152.699946726709,0.826719868787715,341.95195653147));
#71895=CARTESIAN_POINT('Ctrl Pts',(152.421708692435,6.29343411897757,338.0668962074));
#71896=CARTESIAN_POINT('Ctrl Pts',(152.143470658161,5.98475676911705,331.367390501116));
#71897=CARTESIAN_POINT('Ctrl Pts',(151.865232623887,0.183956467102918,328.001476914727));
#71898=CARTESIAN_POINT('Ctrl Pts',(151.586994589613,-5.78565796957856,331.058004665663));
#71899=CARTESIAN_POINT('Ctrl Pts',(151.30875655534,-6.44585948374944,337.732043351164));
#71900=CARTESIAN_POINT('Ctrl Pts',(151.030518521066,-1.19079089041349,341.898926178196));
#71901=CARTESIAN_POINT('Ctrl Pts',(150.752280486792,5.15704892701019,339.73476627948));
#71902=CARTESIAN_POINT('Ctrl Pts',(150.474042452518,6.77234106203401,333.225581251122));
#71903=CARTESIAN_POINT('Ctrl Pts',(150.195804418244,2.17275576401948,328.344754118231));
#71904=CARTESIAN_POINT('Ctrl Pts',(149.91756638397,-4.42073542881313,329.571347899771));
#71905=CARTESIAN_POINT('Ctrl Pts',(149.639328349696,-6.95738296857203,335.779735586917));
#71906=CARTESIAN_POINT('Ctrl Pts',(149.361090315422,-3.10934284887668,341.272571434828));
#71907=CARTESIAN_POINT('Ctrl Pts',(149.082852281148,3.59209530940757,341.009161059999));
#71908=CARTESIAN_POINT('Ctrl Pts',(148.804614246874,6.99712062148836,335.231232275482));
#71909=CARTESIAN_POINT('Ctrl Pts',(148.5263762126,3.98099161656035,329.241105044737));
#71910=CARTESIAN_POINT('Ctrl Pts',(148.248138178326,-2.68843463554514,328.535830713288));
#71911=CARTESIAN_POINT('Ctrl Pts',(147.969900144052,-6.89072410384103,333.762629125271));
#71912=CARTESIAN_POINT('Ctrl Pts',(147.691662109779,-4.76949776896307,340.124944525431));
#71913=CARTESIAN_POINT('Ctrl Pts',(147.413424075504,1.72862627082064,341.784173978658));
#71914=CARTESIAN_POINT('Ctrl Pts',(147.135186041231,6.64041549635417,337.217667105916));
#71915=CARTESIAN_POINT('Ctrl Pts',(146.856948006956,5.45839343325556,330.616039862787));
#71916=CARTESIAN_POINT('Ctrl Pts',(146.578709972683,-0.732715717786626,
328.037508130433));
#71917=CARTESIAN_POINT('Ctrl Pts',(146.300471938409,-6.25142246948224,331.84835242057));
#71918=CARTESIAN_POINT('Ctrl Pts',(146.022233904135,-6.03329109177857,338.551417176107));
#71919=CARTESIAN_POINT('Ctrl Pts',(145.743995869861,-0.278497530380219,
341.995398807964));
#71920=CARTESIAN_POINT('Ctrl Pts',(145.465757835587,5.73186910403123,339.019806205669));
#71921=CARTESIAN_POINT('Ctrl Pts',(145.187519801313,6.48218406392253,332.355296780674));
#71922=CARTESIAN_POINT('Ctrl Pts',(144.909281767039,1.28389438523206,328.1177924643));
#71923=CARTESIAN_POINT('Ctrl Pts',(144.631043732765,-5.09260622053579,330.19598842222));
#71924=CARTESIAN_POINT('Ctrl Pts',(144.352805698491,-6.79569726446257,336.682754897975));
#71925=CARTESIAN_POINT('Ctrl Pts',(144.074567664217,-2.26247723311923,341.62528204128));
#71926=CARTESIAN_POINT('Ctrl Pts',(143.796329629943,4.34698476094839,340.487885644304));
#71927=CARTESIAN_POINT('Ctrl Pts',(143.518091595669,6.96728300128357,334.314337592611));
#71928=CARTESIAN_POINT('Ctrl Pts',(143.239853561395,3.19380846826935,328.770011811818));
#71929=CARTESIAN_POINT('Ctrl Pts',(142.961615527121,-3.51057695553987,328.942854236844));
#71930=CARTESIAN_POINT('Ctrl Pts',(142.683377492847,-6.99335772328111,334.674249925394));
#71931=CARTESIAN_POINT('Ctrl Pts',(142.405139458574,-4.05843733015822,340.704581649346));
#71932=CARTESIAN_POINT('Ctrl Pts',(142.126901424299,2.60085109841411,341.499902993181));
#71933=CARTESIAN_POINT('Ctrl Pts',(141.848663390026,6.87337686247108,336.330359298584));
#71934=CARTESIAN_POINT('Ctrl Pts',(141.570425355752,4.83830613071455,329.939964511748));
#71935=CARTESIAN_POINT('Ctrl Pts',(141.292187321478,-1.63680672391732,328.193089606479));
#71936=CARTESIAN_POINT('Ctrl Pts',(141.013949287204,-6.60984620723789,332.692815899512));
#71937=CARTESIAN_POINT('Ctrl Pts',(140.73571125293,-5.51712738734636,339.309810987581));
#71938=CARTESIAN_POINT('Ctrl Pts',(140.457473218656,0.638577803246183,341.971756145054));
#71939=CARTESIAN_POINT('Ctrl Pts',(140.179235184382,6.20826956919261,338.235823591161));
#71940=CARTESIAN_POINT('Ctrl Pts',(139.900997150108,6.08072398539963,331.530423488339));
#71941=CARTESIAN_POINT('Ctrl Pts',(139.622759115834,0.372987751544304,328.009002539402));
#71942=CARTESIAN_POINT('Ctrl Pts',(139.34452108156,-5.67703383661305,330.903116773103));
#71943=CARTESIAN_POINT('Ctrl Pts',(139.066283047286,-6.51732526579266,337.556880274229));
#71944=CARTESIAN_POINT('Ctrl Pts',(138.788045013012,-1.37676349411775,341.864232487187));
#71945=CARTESIAN_POINT('Ctrl Pts',(138.509806978738,5.02723381511318,339.872379862558));
#71946=CARTESIAN_POINT('Ctrl Pts',(138.231568944464,6.81781285406428,333.40921615427));
#71947=CARTESIAN_POINT('Ctrl Pts',(137.953330910191,2.35178566759336,328.405891301276));
#71948=CARTESIAN_POINT('Ctrl Pts',(137.675092875917,-4.27244051372844,329.453882672218));
#71949=CARTESIAN_POINT('Ctrl Pts',(137.396854841643,-6.97591109672025,335.591464054306));
#71950=CARTESIAN_POINT('Ctrl Pts',(137.118616807369,-3.2776910305309,341.186267603754));
#71951=CARTESIAN_POINT('Ctrl Pts',(136.840378773095,3.42841771573635,341.104024682397));
#71952=CARTESIAN_POINT('Ctrl Pts',(136.562140738821,6.9883181276349,335.42020840526));
#71953=CARTESIAN_POINT('Ctrl Pts',(136.283902704547,4.13514214120938,329.350773076882));
#71954=CARTESIAN_POINT('Ctrl Pts',(136.005664670273,-2.51279275360601,328.465549913397));
#71955=CARTESIAN_POINT('Ctrl Pts',(135.727426635999,-6.85477482719744,333.576895146063));
#71956=CARTESIAN_POINT('Ctrl Pts',(135.449188601725,-4.90623121818037,339.994202698192));
#71957=CARTESIAN_POINT('Ctrl Pts',(135.170950567451,1.54468836390661,341.828404148504));
#71958=CARTESIAN_POINT('Ctrl Pts',(134.892712533177,6.57807023399944,337.396279898812));
#71959=CARTESIAN_POINT('Ctrl Pts',(134.614474498903,5.57485414250854,330.765124955016));
#71960=CARTESIAN_POINT('Ctrl Pts',(134.336236464629,-0.544323310850194,
328.020252333347));
#71961=CARTESIAN_POINT('Ctrl Pts',(134.057998430355,-6.1639832960406,331.680591124461));
#71962=CARTESIAN_POINT('Ctrl Pts',(133.779760396081,-6.12704679069886,338.387102446261));
#71963=CARTESIAN_POINT('Ctrl Pts',(133.501522361807,-0.467409880595166,
341.985319846679));
#71964=CARTESIAN_POINT('Ctrl Pts',(133.223284327534,5.62116217797218,339.173212326951));
#71965=CARTESIAN_POINT('Ctrl Pts',(132.94504629326,6.55127667403222,332.531409451293));
#71966=CARTESIAN_POINT('Ctrl Pts',(132.666808258985,1.46938126301808,328.154995685847));
#71967=CARTESIAN_POINT('Ctrl Pts',(132.388570224712,-4.96094364503585,330.060141347401));
#71968=CARTESIAN_POINT('Ctrl Pts',(132.110332190438,-6.83868379344855,336.49852238225));
#71969=CARTESIAN_POINT('Ctrl Pts',(131.832094156164,-2.44066476342085,341.561731545064));
#71970=CARTESIAN_POINT('Ctrl Pts',(131.55385612189,4.19711629584524,340.60333651997));
#71971=CARTESIAN_POINT('Ctrl Pts',(131.275618087616,6.98326567974919,334.502842275613));
#71972=CARTESIAN_POINT('Ctrl Pts',(130.997380053342,3.36097522217991,328.858582336889));
#71973=CARTESIAN_POINT('Ctrl Pts',(130.719142019068,-3.34563258887094,328.850210740427));
#71974=CARTESIAN_POINT('Ctrl Pts',(130.440903984794,-6.98200275457099,334.485409976734));
#71975=CARTESIAN_POINT('Ctrl Pts',(130.16266595052,-4.21109204659298,340.592840882057));
#71976=CARTESIAN_POINT('Ctrl Pts',(129.884427916246,2.42427567692669,341.567804260112));
#71977=CARTESIAN_POINT('Ctrl Pts',(129.606189881972,6.83492139398107,336.515590609294));
#71978=CARTESIAN_POINT('Ctrl Pts',(129.327951847698,4.97326063105343,330.072541826409));
#71979=CARTESIAN_POINT('Ctrl Pts',(129.049713813425,-1.45228800778535,328.151348680264));
#71980=CARTESIAN_POINT('Ctrl Pts',(128.771475779151,-6.54509337761538,332.515061764314));
#71981=CARTESIAN_POINT('Ctrl Pts',(128.493237744877,-5.63156316022767,339.159165989624));
#71982=CARTESIAN_POINT('Ctrl Pts',(128.214999710603,0.449969447564982,341.986464975446));
#71983=CARTESIAN_POINT('Ctrl Pts',(127.936761676329,6.11857173486536,338.402388173355));
#71984=CARTESIAN_POINT('Ctrl Pts',(127.658523642055,6.17225105105066,331.695989963744));
#71985=CARTESIAN_POINT('Ctrl Pts',(127.380285607781,0.561746679963059,328.021632997296));
#71986=CARTESIAN_POINT('Ctrl Pts',(127.102047573507,-5.5642643279593,330.751220428702));
#71987=CARTESIAN_POINT('Ctrl Pts',(126.823809539233,-6.58403209052025,337.379850160804));
#71988=CARTESIAN_POINT('Ctrl Pts',(126.545571504959,-1.56173078376513,341.824526526868));
#71989=CARTESIAN_POINT('Ctrl Pts',(126.267333470685,4.89374781214267,340.006435629071));
#71990=CARTESIAN_POINT('Ctrl Pts',(125.989095436411,6.85830627244645,333.594012649345));
#71991=CARTESIAN_POINT('Ctrl Pts',(125.710857402137,2.52909829496077,328.471843508975));
#71992=CARTESIAN_POINT('Ctrl Pts',(125.432619367863,-4.12102585838077,329.340467224988));
#71993=CARTESIAN_POINT('Ctrl Pts',(125.154381333589,-6.98934540772823,335.402760634062));
#71994=CARTESIAN_POINT('Ctrl Pts',(124.876143299315,-3.44364583897262,341.095446553995));
#71995=CARTESIAN_POINT('Ctrl Pts',(124.597905265041,3.2622366880789,341.194431139971));
#71996=CARTESIAN_POINT('Ctrl Pts',(124.319667230768,6.97441275701501,335.608877698449));
#71997=CARTESIAN_POINT('Ctrl Pts',(124.041429196494,4.28627318100201,329.464566180081));
#71998=CARTESIAN_POINT('Ctrl Pts',(123.76319116222,-2.33531602792795,328.400040575383));
#71999=CARTESIAN_POINT('Ctrl Pts',(123.484953127946,-6.8138201872366,333.392200319416));
#72000=CARTESIAN_POINT('Ctrl Pts',(123.206715093672,-5.03938213253937,339.859814099235));
#72001=CARTESIAN_POINT('Ctrl Pts',(122.928477059398,1.3596225240309,341.867648210926));
#72002=CARTESIAN_POINT('Ctrl Pts',(122.650239025124,6.51092165829356,337.573142925771));
#72003=CARTESIAN_POINT('Ctrl Pts',(122.37200099085,5.68724408778636,330.917302357164));
#72004=CARTESIAN_POINT('Ctrl Pts',(122.093762956576,-0.355533438497236,
328.008093154869));
#72005=CARTESIAN_POINT('Ctrl Pts',(121.815524922302,-6.07204317593688,331.515253663975));
#72006=CARTESIAN_POINT('Ctrl Pts',(121.537286888028,-6.21632851402961,338.220314450879));
#72007=CARTESIAN_POINT('Ctrl Pts',(121.259048853754,-0.655980927655841,
341.970140197976));
#72008=CARTESIAN_POINT('Ctrl Pts',(120.98081081948,5.50635067376508,339.32357116449));
#72009=CARTESIAN_POINT('Ctrl Pts',(120.702572785207,6.6155855354745,332.709324689158));
#72010=CARTESIAN_POINT('Ctrl Pts',(120.424334750932,1.65379519716147,328.197197136273));
#72011=CARTESIAN_POINT('Ctrl Pts',(120.146096716659,-4.82565858360948,329.927901362226));
#72012=CARTESIAN_POINT('Ctrl Pts',(119.867858682384,-6.87667670880607,336.31319564401));
#72013=CARTESIAN_POINT('Ctrl Pts',(119.589620648111,-2.61707011791319,341.493389666023));
#72014=CARTESIAN_POINT('Ctrl Pts',(119.311382613837,4.044183092297,340.714695833801));
#72015=CARTESIAN_POINT('Ctrl Pts',(119.033144579563,6.99414917075083,334.691709983673));
#72016=CARTESIAN_POINT('Ctrl Pts',(118.754906545289,3.52568778867917,328.951637331174));
#72017=CARTESIAN_POINT('Ctrl Pts',(118.476668511015,-3.17824523799691,328.762057826172));
#72018=CARTESIAN_POINT('Ctrl Pts',(118.198430476741,-6.96554952058604,334.296945782214));
#72019=CARTESIAN_POINT('Ctrl Pts',(117.920192442467,-4.36067181947576,340.477016216857));
#72020=CARTESIAN_POINT('Ctrl Pts',(117.641954408193,2.24593004695689,341.630909709916));
#72021=CARTESIAN_POINT('Ctrl Pts',(117.363716373919,6.79147505917034,336.699715234253));
#72022=CARTESIAN_POINT('Ctrl Pts',(117.085478339645,5.10458365159074,330.208717175871));
#72023=CARTESIAN_POINT('Ctrl Pts',(116.807240305371,-1.26670882952249,328.114608645974));
#72024=CARTESIAN_POINT('Ctrl Pts',(116.529002271097,-6.4755613143746,332.339122133457));
#72025=CARTESIAN_POINT('Ctrl Pts',(116.250764236823,-5.74188676015347,339.005483964574));
#72026=CARTESIAN_POINT('Ctrl Pts',(115.97252620255,0.26103252375085,341.996072282246));
#72027=CARTESIAN_POINT('Ctrl Pts',(115.694288168275,6.02440611344274,338.566468328361));
#72028=CARTESIAN_POINT('Ctrl Pts',(115.416050134002,6.25927113291671,331.863969030523));
#72029=CARTESIAN_POINT('Ctrl Pts',(115.137812099727,0.7500954204035,328.039359065635));
#72030=CARTESIAN_POINT('Ctrl Pts',(114.859574065454,-5.44743178802376,330.602426547321));
#72031=CARTESIAN_POINT('Ctrl Pts',(114.58133603118,-6.64593124854297,337.201082278453));
#72032=CARTESIAN_POINT('Ctrl Pts',(114.303097996906,-1.74555769605902,341.77983729057));
#72033=CARTESIAN_POINT('Ctrl Pts',(114.024859962632,4.75668838970893,340.136835691367));
#72034=CARTESIAN_POINT('Ctrl Pts',(113.746621928358,6.89379174884668,333.779835797765));
#72035=CARTESIAN_POINT('Ctrl Pts',(113.468383894084,2.70456417226724,328.542562582962));
#72036=CARTESIAN_POINT('Ctrl Pts',(113.19014585981,-3.9666020259001,329.231184374154));
#72037=CARTESIAN_POINT('Ctrl Pts',(112.911907825536,-6.99767609184886,335.213763117606));
#72038=CARTESIAN_POINT('Ctrl Pts',(112.633669791262,-3.60708609383773,341.00017460317));
#72039=CARTESIAN_POINT('Ctrl Pts',(112.355431756988,3.09367357198481,341.280314417837));
#72040=CARTESIAN_POINT('Ctrl Pts',(112.077193722714,6.95541466334396,335.797102388544));
#72041=CARTESIAN_POINT('Ctrl Pts',(111.79895568844,4.43427437990451,329.582401262496));
#72042=CARTESIAN_POINT('Ctrl Pts',(111.520717654166,-2.15613405219075,328.33935053423));
#72043=CARTESIAN_POINT('Ctrl Pts',(111.242479619892,-6.767890089077,333.208679509676));
#72044=CARTESIAN_POINT('Ctrl Pts',(110.964241585619,-5.16885328511126,339.721876859245));
#72045=CARTESIAN_POINT('Ctrl Pts',(110.686003551344,1.17356388645166,341.901877509873));
#72046=CARTESIAN_POINT('Ctrl Pts',(110.407765517071,6.43901880119245,337.748127041236));
#72047=CARTESIAN_POINT('Ctrl Pts',(110.129527482797,5.79548120184066,331.072460949145));
#72048=CARTESIAN_POINT('Ctrl Pts',(109.851289448523,-0.166483955278002,
328.001039473642));
#72049=CARTESIAN_POINT('Ctrl Pts',(109.573051414249,-5.97566924393718,331.35246076869));
#72050=CARTESIAN_POINT('Ctrl Pts',(109.294813379975,-6.30107106816867,338.051174978721));
#72051=CARTESIAN_POINT('Ctrl Pts',(109.016575345701,-0.844072976798288,
341.949870946048));
#72052=CARTESIAN_POINT('Ctrl Pts',(108.738337311427,5.38751842688317,339.470772926115));
#72053=CARTESIAN_POINT('Ctrl Pts',(108.460099277153,6.67506368985558,332.888912580385));
#72054=CARTESIAN_POINT('Ctrl Pts',(108.181861242879,1.83700152842608,328.244366000038));
#72055=CARTESIAN_POINT('Ctrl Pts',(107.903623208605,-4.6868498215419,329.799365028462));
#72056=CARTESIAN_POINT('Ctrl Pts',(107.625385174331,-6.90964826807086,336.126910009019));
#72057=CARTESIAN_POINT('Ctrl Pts',(107.347147140057,-2.79156448523252,341.420306307465));
#72058=CARTESIAN_POINT('Ctrl Pts',(107.068909105783,3.88829682227926,340.821882271116));
#72059=CARTESIAN_POINT('Ctrl Pts',(106.790671071509,6.99992552715261,334.880802805406));
#72060=CARTESIAN_POINT('Ctrl Pts',(106.512433037235,3.68782589448949,329.049108845827));
#72061=CARTESIAN_POINT('Ctrl Pts',(106.234195002962,-3.00853712932565,328.678459863423));
#72062=CARTESIAN_POINT('Ctrl Pts',(105.955956968688,-6.94401003549388,334.108994958577));
#72063=CARTESIAN_POINT('Ctrl Pts',(105.677718934414,-4.50706742550949,340.357192229032));
#72064=CARTESIAN_POINT('Ctrl Pts',(105.39948090014,2.0659444366588,341.689173262932));
#72065=CARTESIAN_POINT('Ctrl Pts',(105.121242865866,6.74306958259522,336.882598725476));
#72066=CARTESIAN_POINT('Ctrl Pts',(104.843004831592,5.2321793001279,330.348391124762));
#72067=CARTESIAN_POINT('Ctrl Pts',(104.564766797318,-1.08020469922692,328.082896331221));
#72068=CARTESIAN_POINT('Ctrl Pts',(104.286528763044,-6.40130078989642,332.165125478235));
#72069=CARTESIAN_POINT('Ctrl Pts',(104.00829072877,-5.84801762872275,338.848877131195));
#72070=CARTESIAN_POINT('Ctrl Pts',(103.730052694496,0.0719049937310667,
342.00057105019));
#72071=CARTESIAN_POINT('Ctrl Pts',(103.451814660222,5.92584146475386,338.727944244686));
#72072=CARTESIAN_POINT('Ctrl Pts',(103.173576625948,6.34172068884867,332.0342380302));
#72073=CARTESIAN_POINT('Ctrl Pts',(102.895338591674,0.937896440430998,328.062167800825));
#72074=CARTESIAN_POINT('Ctrl Pts',(102.6171005574,-5.32662152804144,330.456843778397));
#72075=CARTESIAN_POINT('Ctrl Pts',(102.338862523126,-6.70297754103513,337.020707163659));
#72076=CARTESIAN_POINT('Ctrl Pts',(102.060624488853,-1.9281100004072,341.730197410419));
#72077=CARTESIAN_POINT('Ctrl Pts',(101.782386454578,4.61615562873744,340.263484831189));
#72078=CARTESIAN_POINT('Ctrl Pts',(101.504148420305,6.92424337173514,333.966549911286));
#72079=CARTESIAN_POINT('Ctrl Pts',(101.225910386031,2.87805517415613,328.617996884097));
#72080=CARTESIAN_POINT('Ctrl Pts',(100.947672351757,-3.80928177672123,329.126113918161));
#72081=CARTESIAN_POINT('Ctrl Pts',(100.669434317483,-7.00089706600837,335.024609511113));
#72082=CARTESIAN_POINT('Ctrl Pts',(100.391196283209,-3.76789245089095,340.900521318951));
#72083=CARTESIAN_POINT('Ctrl Pts',(100.112958248935,2.92285145240769,341.361611803942));
#72084=CARTESIAN_POINT('Ctrl Pts',(99.8347202146609,6.93133771904842,335.98474503369));
#72085=CARTESIAN_POINT('Ctrl Pts',(99.5564821803873,4.57903766729572,329.704192280836));
#72086=CARTESIAN_POINT('Ctrl Pts',(99.2782441461129,-1.97537766524897,328.283524105863));
#72087=CARTESIAN_POINT('Ctrl Pts',(99.0000061118395,-6.71701807092136,333.026466723919));
#72088=CARTESIAN_POINT('Ctrl Pts',(98.7217680775651,-5.29455013593342,339.580491700131));
#72089=CARTESIAN_POINT('Ctrl Pts',(98.4435300432915,0.986648311368706,341.931067051079));
#72090=CARTESIAN_POINT('Ctrl Pts',(98.1652920090174,6.36241416623298,337.921104471635));
#72091=CARTESIAN_POINT('Ctrl Pts',(97.8870539747435,5.8994864498244,331.230487434001));
#72092=CARTESIAN_POINT('Ctrl Pts',(97.6088159404696,0.0226870946892429,
327.999096440272));
#72093=CARTESIAN_POINT('Ctrl Pts',(97.3305779061955,-5.87493187238127,331.192331310138));
#72094=CARTESIAN_POINT('Ctrl Pts',(97.0523398719218,-6.38121257401978,337.879807535592));
#72095=CARTESIAN_POINT('Ctrl Pts',(96.7741018376478,-1.03154868302355,341.924526891523));
#72096=CARTESIAN_POINT('Ctrl Pts',(96.4958638033737,5.2647522087498,339.614710124953));
#72097=CARTESIAN_POINT('Ctrl Pts',(96.2176257691,6.72966770616867,333.070041989723));
#72098=CARTESIAN_POINT('Ctrl Pts',(95.9393877348259,2.01886647936908,328.296467834391));
#72099=CARTESIAN_POINT('Ctrl Pts',(95.661149700552,-4.54461871712713,329.674626203466));
#72100=CARTESIAN_POINT('Ctrl Pts',(95.3829116662781,-6.93757439537808,335.939801503232));
#72101=CARTESIAN_POINT('Ctrl Pts',(95.104673632004,-2.96402044942079,341.342534834931));
#72102=CARTESIAN_POINT('Ctrl Pts',(94.8264355977303,3.72957131409984,340.924817564273));
#72103=CARTESIAN_POINT('Ctrl Pts',(94.5481975634562,7.00059053105341,335.069982665048));
#72104=CARTESIAN_POINT('Ctrl Pts',(94.2699595291823,3.84727114620612,329.15092570705));
#72105=CARTESIAN_POINT('Ctrl Pts',(93.9917214949084,-2.83663218388548,328.599477895498));
#72106=CARTESIAN_POINT('Ctrl Pts',(93.7134834606343,-6.91740002744779,333.921694747696));
#72107=CARTESIAN_POINT('Ctrl Pts',(93.4352454263607,-4.6501719664783,340.233456414174));
#72108=CARTESIAN_POINT('Ctrl Pts',(93.1570073920864,1.88445027170261,341.742552375055));
#72109=CARTESIAN_POINT('Ctrl Pts',(92.8787693578127,6.68974030998245,337.064107541259));
#72110=CARTESIAN_POINT('Ctrl Pts',(92.6005313235387,5.35595440619652,330.491461683025));
#72111=CARTESIAN_POINT('Ctrl Pts',(92.3222932892648,-0.892911802398389,
328.056234892364));
#72112=CARTESIAN_POINT('Ctrl Pts',(92.0440552549908,-6.32236602928883,331.993198851175));
#72113=CARTESIAN_POINT('Ctrl Pts',(91.7658172207168,-5.94987826907084,338.68945984395));
#72114=CARTESIAN_POINT('Ctrl Pts',(91.487579186443,-0.117275041385807,341.99995799427));
#72115=CARTESIAN_POINT('Ctrl Pts',(91.2093411521688,5.82294976080219,338.88669801246));
#72116=CARTESIAN_POINT('Ctrl Pts',(90.9311031178951,6.41953951409962,332.206672632183));
#72117=CARTESIAN_POINT('Ctrl Pts',(90.6528650836211,1.12501260755572,328.090042547907));
#72118=CARTESIAN_POINT('Ctrl Pts',(90.3746270493473,-5.20192176378319,330.314578426613));
#72119=CARTESIAN_POINT('Ctrl Pts',(90.0963890150731,-6.75512931273765,336.838856526506));
#72120=CARTESIAN_POINT('Ctrl Pts',(89.8181509807993,-2.10925439693799,341.675643133503));
#72121=CARTESIAN_POINT('Ctrl Pts',(89.5399129465253,4.47225214638779,340.386290569215));
#72122=CARTESIAN_POINT('Ctrl Pts',(89.2616749122515,6.94963890530698,334.154018651077));
#72123=CARTESIAN_POINT('Ctrl Pts',(88.9834368779774,3.04944461732804,328.698091330182));
#72124=CARTESIAN_POINT('Ctrl Pts',(88.7051988437036,-3.64917998624406,329.025332579559));
#72125=CARTESIAN_POINT('Ctrl Pts',(88.4269608094296,-6.9990059782483,334.835437934729));
#72126=CARTESIAN_POINT('Ctrl Pts',(88.1487227751557,-3.92594748917296,340.796559468266));
#72127=CARTESIAN_POINT('Ctrl Pts',(87.8704847408817,2.74989506382644,341.438263934852));
#72128=CARTESIAN_POINT('Ctrl Pts',(87.5922467066078,6.90219950513693,336.171668617046));
#72129=CARTESIAN_POINT('Ctrl Pts',(87.3140086723338,4.72045733688097,329.829850303176));
#72130=CARTESIAN_POINT('Ctrl Pts',(87.03577063806,-1.79317885559459,328.232602054798));
#72131=CARTESIAN_POINT('Ctrl Pts',(86.7575326037859,-6.6612412795675,332.845695014101));
#72132=CARTESIAN_POINT('Ctrl Pts',(86.4792945695121,-5.41638090104145,339.435761861475));
#72133=CARTESIAN_POINT('Ctrl Pts',(86.201056535238,0.799012284719287,341.95519552031));
#72134=CARTESIAN_POINT('Ctrl Pts',(85.9228185009643,6.28116369019514,338.091948908675));
#72135=CARTESIAN_POINT('Ctrl Pts',(85.6445804666901,5.99918388700299,331.391266420639));
#72136=CARTESIAN_POINT('Ctrl Pts',(85.3663424324163,0.211841578517241,328.002265473563));
#72137=CARTESIAN_POINT('Ctrl Pts',(85.0881043981423,-5.76990461979722,331.034982215006));
#72138=CARTESIAN_POINT('Ctrl Pts',(84.8098663638684,-6.45669451217634,337.70633725417));
#72139=CARTESIAN_POINT('Ctrl Pts',(84.5316283295946,-1.21827115138629,341.894126540657));
#72140=CARTESIAN_POINT('Ctrl Pts',(84.2533902953204,5.13814166337825,339.755277657923));
#72141=CARTESIAN_POINT('Ctrl Pts',(83.9751522610467,6.77935771250735,333.252580656297));
#72142=CARTESIAN_POINT('Ctrl Pts',(83.6969142267727,2.19925725202426,328.35346459452));
#72143=CARTESIAN_POINT('Ctrl Pts',(83.4186761924987,-4.39906912765766,329.553775971651));
#72144=CARTESIAN_POINT('Ctrl Pts',(83.1404381582248,-6.96043469904204,335.752006753462));
#72145=CARTESIAN_POINT('Ctrl Pts',(82.8622001239508,-3.13431208296329,341.260132037224));
#72146=CARTESIAN_POINT('Ctrl Pts',(82.583962089677,3.56812246928036,341.023426549822));
#72147=CARTESIAN_POINT('Ctrl Pts',(82.3057240554029,6.99614369686675,335.259111423279));
#72148=CARTESIAN_POINT('Ctrl Pts',(82.0274860211291,4.00390711675021,329.257013568072));
#72149=CARTESIAN_POINT('Ctrl Pts',(81.749247986855,-2.66265592683582,328.525169595103));
#72150=CARTESIAN_POINT('Ctrl Pts',(81.4710099525813,-6.88573892710168,333.73518191637));
#72151=CARTESIAN_POINT('Ctrl Pts',(81.1927719183071,-4.78988094730629,340.105899124299));
#72152=CARTESIAN_POINT('Ctrl Pts',(80.9145338840334,1.70158007930518,341.791008068806));
#72153=CARTESIAN_POINT('Ctrl Pts',(80.6362958497593,6.63152618241909,337.244109143685));
#72154=CARTESIAN_POINT('Ctrl Pts',(80.3580578154855,5.475818589093,330.637824380401));
#72155=CARTESIAN_POINT('Ctrl Pts',(80.0798197812114,-0.704966900493841,
328.034643797615));
#72156=CARTESIAN_POINT('Ctrl Pts',(79.8015817469376,-6.23881467079188,331.82346779327));
#72157=CARTESIAN_POINT('Ctrl Pts',(79.5233437126635,-6.04739430245781,338.527348509502));
#72158=CARTESIAN_POINT('Ctrl Pts',(79.2451056783897,-0.306369442151794,
341.994233562142));
#72159=CARTESIAN_POINT('Ctrl Pts',(78.9668676441157,5.71580613321137,339.042613709523));
#72160=CARTESIAN_POINT('Ctrl Pts',(78.6886296098418,6.4926707852867,332.381146924556));
#72161=CARTESIAN_POINT('Ctrl Pts',(78.4103915755678,1.31130728936813,328.122962952715));
#72162=CARTESIAN_POINT('Ctrl Pts',(78.1321535412939,-5.07342355113972,330.175734374268));
#72163=CARTESIAN_POINT('Ctrl Pts',(77.8539155070199,-6.8023484823755,336.655663154511));
#72164=CARTESIAN_POINT('Ctrl Pts',(77.575677472746,-2.28885861383431,341.616214295407));
#72165=CARTESIAN_POINT('Ctrl Pts',(77.2974394384722,4.32508302112474,340.505163232572));
#72166=CARTESIAN_POINT('Ctrl Pts',(77.0192014041981,6.96995980571845,334.342105127281));
#72167=CARTESIAN_POINT('Ctrl Pts',(76.7409633699243,3.21860735304273,328.782787436172));
#72168=CARTESIAN_POINT('Ctrl Pts',(76.4627253356503,-3.48641356095375,328.928913948982));
#72169=CARTESIAN_POINT('Ctrl Pts',(76.1844873013764,-6.99200420944275,334.646386521726));
#72170=CARTESIAN_POINT('Ctrl Pts',(75.9062492671024,-4.08113579673913,340.688364964158));
#72171=CARTESIAN_POINT('Ctrl Pts',(75.6280112328284,2.5749306991664,341.51021483911));
#72172=CARTESIAN_POINT('Ctrl Pts',(75.3497731985546,6.86802129836172,336.357736646825));
#72173=CARTESIAN_POINT('Ctrl Pts',(75.0715351642804,4.85843012387871,329.959283573908));
#72174=CARTESIAN_POINT('Ctrl Pts',(74.7932971300068,-1.60967066497673,328.186621564364));
#72175=CARTESIAN_POINT('Ctrl Pts',(74.5150590957326,-6.60060044328308,332.666496379903));
#72176=CARTESIAN_POINT('Ctrl Pts',(74.2368210614589,-5.5342566194914,339.287793025146));
#72177=CARTESIAN_POINT('Ctrl Pts',(73.9585830271847,0.61079281851374,341.974245298937));
#72178=CARTESIAN_POINT('Ctrl Pts',(73.680344992911,6.19532670225604,338.260535601584));
#72179=CARTESIAN_POINT('Ctrl Pts',(73.4021069586369,6.09450071421021,331.554680508085));
#72180=CARTESIAN_POINT('Ctrl Pts',(73.1238689243631,0.400841375416753,328.010544259484));
#72181=CARTESIAN_POINT('Ctrl Pts',(72.845630890089,-5.66066417718765,330.880528379757));
#72182=CARTESIAN_POINT('Ctrl Pts',(72.5673928558152,-6.52746176565324,337.530890802626));
#72183=CARTESIAN_POINT('Ctrl Pts',(72.2891548215411,-1.40410403695659,341.858692091811));
#72184=CARTESIAN_POINT('Ctrl Pts',(72.0109167872673,5.00777924191351,339.892372882472));
#72185=CARTESIAN_POINT('Ctrl Pts',(71.7326787529933,6.82409742518003,333.436395290192));
#72186=CARTESIAN_POINT('Ctrl Pts',(71.4544407187194,2.37804212487173,328.415314661337));
#72187=CARTESIAN_POINT('Ctrl Pts',(71.1762026844454,-4.25030733358714,329.436902577975));
#72188=CARTESIAN_POINT('Ctrl Pts',(70.8979646501716,-6.9782124864465,335.563662887623));
#72189=CARTESIAN_POINT('Ctrl Pts',(70.6197266158975,-3.30231503874137,341.17315808495));
#72190=CARTESIAN_POINT('Ctrl Pts',(70.3414885816236,3.40406817792663,341.117637223382));
#72191=CARTESIAN_POINT('Ctrl Pts',(70.0632505473498,6.98658827167532,335.448050978093));
#72192=CARTESIAN_POINT('Ctrl Pts',(69.7850125130757,4.15761943038146,329.367294963431));
#72193=CARTESIAN_POINT('Ctrl Pts',(69.5067744788019,-2.48673539581103,328.455589222237));
#72194=CARTESIAN_POINT('Ctrl Pts',(69.2285364445278,-6.84904985342219,333.549592656451));
#72195=CARTESIAN_POINT('Ctrl Pts',(68.950298410254,-4.92609235235802,339.974613501864));
#72196=CARTESIAN_POINT('Ctrl Pts',(68.67206037598,1.51746739146117,341.83450496179));
#72197=CARTESIAN_POINT('Ctrl Pts',(68.3938223417061,6.56846970791843,337.422472095411));
#72198=CARTESIAN_POINT('Ctrl Pts',(68.1155843074321,5.59168432387292,330.787372342702));
#72199=CARTESIAN_POINT('Ctrl Pts',(67.8373462731582,-0.516507231065439,
328.018138812814));
#72200=CARTESIAN_POINT('Ctrl Pts',(67.5591082388843,-6.15070772368928,331.656056242305));
#72201=CARTESIAN_POINT('Ctrl Pts',(67.2808702046103,-6.14049452258065,338.362661501703));
#72202=CARTESIAN_POINT('Ctrl Pts',(67.0026321703365,-0.495240131650347,
341.983401933791));
#72203=CARTESIAN_POINT('Ctrl Pts',(66.7243941360623,5.60448881836311,339.195577486083));
#72204=CARTESIAN_POINT('Ctrl Pts',(66.4461561017886,6.56106110188412,332.557533506018));
#72205=CARTESIAN_POINT('Ctrl Pts',(66.1679180675145,1.49664445330917,328.160904976734));
#72206=CARTESIAN_POINT('Ctrl Pts',(65.8896800332407,-4.94122071963166,330.040413005424));
#72207=CARTESIAN_POINT('Ctrl Pts',(65.6114419989667,-6.84460057046481,336.471260815653));
#72208=CARTESIAN_POINT('Ctrl Pts',(65.3332039646927,-2.4667915039212,341.55195429113));
#72209=CARTESIAN_POINT('Ctrl Pts',(65.0549659304188,4.17475571598797,340.620016020326));
#72210=CARTESIAN_POINT('Ctrl Pts',(64.7767278961449,6.98519123462835,334.530671998967));
#72211=CARTESIAN_POINT('Ctrl Pts',(64.4984898618709,3.38541985850391,328.872023356889));
#72212=CARTESIAN_POINT('Ctrl Pts',(64.220251827597,-3.32110135305436,328.836928431404));
#72213=CARTESIAN_POINT('Ctrl Pts',(63.942013793323,-6.97989687229026,334.457593317636));
#72214=CARTESIAN_POINT('Ctrl Pts',(63.6637757590492,-4.23334405493435,340.576016810361));
#72215=CARTESIAN_POINT('Ctrl Pts',(63.3855377247751,2.39808611757899,341.577411978093));
#72216=CARTESIAN_POINT('Ctrl Pts',(63.1072996905013,6.82882805568316,336.54281325597));
#72217=CARTESIAN_POINT('Ctrl Pts',(62.8290616562273,4.99285528042379,330.09239758073));
#72218=CARTESIAN_POINT('Ctrl Pts',(62.5508236219534,-1.42498709125737,328.145616209561));
#72219=CARTESIAN_POINT('Ctrl Pts',(62.2725855876794,-6.53513984206652,332.489001672339));
#72220=CARTESIAN_POINT('Ctrl Pts',(61.9943475534055,-5.6480912183174,339.136693238137));
#72221=CARTESIAN_POINT('Ctrl Pts',(61.7161095191316,0.422127350791677,341.988202476788));
#72222=CARTESIAN_POINT('Ctrl Pts',(61.4378714848576,6.10496588066887,338.426741448192));
#72223=CARTESIAN_POINT('Ctrl Pts',(61.1596334505837,6.1853673310049,331.720610371209));
#72224=CARTESIAN_POINT('Ctrl Pts',(60.8813954163097,0.589548477549911,328.023926752858));
#72225=CARTESIAN_POINT('Ctrl Pts',(60.6031573820358,-5.54729031203137,330.729082586735));
#72226=CARTESIAN_POINT('Ctrl Pts',(60.3249193477619,-6.59346266013225,337.35359629213));
#72227=CARTESIAN_POINT('Ctrl Pts',(60.046681313488,-1.58891164437911,341.81824941926));
#72228=CARTESIAN_POINT('Ctrl Pts',(59.768443279214,4.87376013512332,340.025895691533));
#72229=CARTESIAN_POINT('Ctrl Pts',(59.49020524494,6.86385417520475,333.621351669785));
#72230=CARTESIAN_POINT('Ctrl Pts',(59.2119672106661,2.55509054902234,328.48197287186));
#72231=CARTESIAN_POINT('Ctrl Pts',(58.9337291763922,-4.09844196092319,329.324091363506));
#72232=CARTESIAN_POINT('Ctrl Pts',(58.6554911421182,-6.99089477623369,335.374907434589));
#72233=CARTESIAN_POINT('Ctrl Pts',(58.3772531078443,-3.46790664083229,341.081676486574));
#72234=CARTESIAN_POINT('Ctrl Pts',(58.0990150735703,3.23752823264279,341.207380792228));
#72235=CARTESIAN_POINT('Ctrl Pts',(57.8207770392965,6.97193123285997,335.636663365645));
#72236=CARTESIAN_POINT('Ctrl Pts',(57.5425390050225,4.30829584621786,329.481689365544));
#72237=CARTESIAN_POINT('Ctrl Pts',(57.2643009707486,-2.30899904815591,328.390787584553));
#72238=CARTESIAN_POINT('Ctrl Pts',(56.9860629364746,-6.80735959680711,333.365062485402));
#72239=CARTESIAN_POINT('Ctrl Pts',(56.7078249022006,-5.05870671993135,339.839695411759));
#72240=CARTESIAN_POINT('Ctrl Pts',(56.4295868679267,1.3322466474366,341.873011292532));
#72241=CARTESIAN_POINT('Ctrl Pts',(56.1513488336528,6.50061693038027,337.599066155629));
#72242=CARTESIAN_POINT('Ctrl Pts',(55.8731107993788,5.70346700526257,330.939996369858));
#72243=CARTESIAN_POINT('Ctrl Pts',(55.5948727651049,-0.327670407549574,
328.006731989914));
#72244=CARTESIAN_POINT('Ctrl Pts',(55.316634730831,-6.05810952376078,331.491086442358));
#72245=CARTESIAN_POINT('Ctrl Pts',(55.0383966965571,-6.2291109475667,338.195519075173));
#72246=CARTESIAN_POINT('Ctrl Pts',(54.760158662283,-0.683749196317659,341.967471018484));
#72247=CARTESIAN_POINT('Ctrl Pts',(54.4819206280093,5.4890791002704,339.345477647838));
#72248=CARTESIAN_POINT('Ctrl Pts',(54.2036825937351,6.62466052521529,332.735703578915));
#72249=CARTESIAN_POINT('Ctrl Pts',(53.9254445594614,1.6808887659992,328.203840914663));
#72250=CARTESIAN_POINT('Ctrl Pts',(53.6472065251873,-4.80540980389684,329.90871313188));
#72251=CARTESIAN_POINT('Ctrl Pts',(53.3689684909135,-6.8818547244892,336.285784160701));
#72252=CARTESIAN_POINT('Ctrl Pts',(53.0907304566394,-2.64292314042703,341.482910043389));
#72253=CARTESIAN_POINT('Ctrl Pts',(52.8124924223656,4.02138000012339,340.730765066856));
#72254=CARTESIAN_POINT('Ctrl Pts',(52.5342543880916,6.99532207003211,334.719581574422));
#72255=CARTESIAN_POINT('Ctrl Pts',(52.2560163538177,3.54976032705684,328.965733932173));
#72256=CARTESIAN_POINT('Ctrl Pts',(51.9777783195437,-3.15336407368193,328.749443194747));
#72257=CARTESIAN_POINT('Ctrl Pts',(51.6995402852698,-6.96269280758023,334.269196179436));
#72258=CARTESIAN_POINT('Ctrl Pts',(51.4213022509958,-4.38246112113954,340.459597043608));
#72259=CARTESIAN_POINT('Ctrl Pts',(51.1430642167219,2.21949045115079,341.639806284384));
#72260=CARTESIAN_POINT('Ctrl Pts',(50.8648261824479,6.78464839604541,336.726763301359));
#72261=CARTESIAN_POINT('Ctrl Pts',(50.5865881481741,5.12363464913532,330.229095123663));
#72262=CARTESIAN_POINT('Ctrl Pts',(50.3083501139,-1.23926299056279,328.109615932539));
#72263=CARTESIAN_POINT('Ctrl Pts',(50.0301120796262,-6.46490727531319,332.313340498224));
#72264=CARTESIAN_POINT('Ctrl Pts',(49.7518740453522,-5.75780157538363,338.982572833658));
#72265=CARTESIAN_POINT('Ctrl Pts',(49.4736360110783,0.233153645263526,341.997056862324));
#72266=CARTESIAN_POINT('Ctrl Pts',(49.1953979768044,6.01014720699452,338.590445084824));
#72267=CARTESIAN_POINT('Ctrl Pts',(48.9171599425304,6.27171738649399,331.888934847865));
#72268=CARTESIAN_POINT('Ctrl Pts',(48.6389219082565,0.777825090804829,328.042403181773));
#72269=CARTESIAN_POINT('Ctrl Pts',(48.3606838739825,-5.42986581003643,330.580755421808));
#72270=CARTESIAN_POINT('Ctrl Pts',(48.0824458397086,-6.65464900169521,337.174583183307));
#72271=CARTESIAN_POINT('Ctrl Pts',(47.8042078054346,-1.7725590269566,341.772828054279));
#72272=CARTESIAN_POINT('Ctrl Pts',(47.5259697711608,4.73618220389178,340.155748586619));
#72273=CARTESIAN_POINT('Ctrl Pts',(47.2477317368866,6.89859893216333,333.807314739742));
#72274=CARTESIAN_POINT('Ctrl Pts',(46.9694937026129,2.73027324354223,328.553390552198));
#72275=CARTESIAN_POINT('Ctrl Pts',(46.6912556683389,-3.94358390191066,329.215424703103));
#72276=CARTESIAN_POINT('Ctrl Pts',(46.413017634065,-6.99847230778318,335.185878223779));
#72277=CARTESIAN_POINT('Ctrl Pts',(46.134779599791,-3.63096597408471,340.98575404205));
#72278=CARTESIAN_POINT('Ctrl Pts',(45.856541565517,3.06862424106128,341.292591725518));
#72279=CARTESIAN_POINT('Ctrl Pts',(45.5783035312431,6.9521832830049,335.824810860979));
#72280=CARTESIAN_POINT('Ctrl Pts',(45.3000654969693,4.45582634019197,329.600113243508));
#72281=CARTESIAN_POINT('Ctrl Pts',(45.0218274626953,-2.12957666712615,328.330812000272));
#72282=CARTESIAN_POINT('Ctrl Pts',(44.7435894284213,-6.76069859952268,333.181726147332));
#72283=CARTESIAN_POINT('Ctrl Pts',(44.4653513941474,-5.187627214885,339.701243371309));
#72284=CARTESIAN_POINT('Ctrl Pts',(44.1871133598734,1.14605309560046,341.906498943672));
#72285=CARTESIAN_POINT('Ctrl Pts',(43.9088753255995,6.42801739596936,337.773762375186));
#72286=CARTESIAN_POINT('Ctrl Pts',(43.6306372913256,5.81108500943841,331.095585015657));
#72287=CARTESIAN_POINT('Ctrl Pts',(43.3523992570517,-0.138594318779784,
328.000431658189));
#72288=CARTESIAN_POINT('Ctrl Pts',(43.0741612227777,-5.9610876863024,331.328678854542));
#72289=CARTESIAN_POINT('Ctrl Pts',(42.7959231885038,-6.3131788696159,338.026043277469));
#72290=CARTESIAN_POINT('Ctrl Pts',(42.5176851542299,-0.87175898665024,341.946452448991));
#72291=CARTESIAN_POINT('Ctrl Pts',(42.2394471199557,5.36966125122276,339.492204737542));
#72292=CARTESIAN_POINT('Ctrl Pts',(41.961209085682,6.68342261491881,332.915527043287));
#72293=CARTESIAN_POINT('Ctrl Pts',(41.6829710514079,1.86390569205994,328.251739414634));
#72294=CARTESIAN_POINT('Ctrl Pts',(41.4047330171342,-4.6660899731994,329.780730921012));
#72295=CARTESIAN_POINT('Ctrl Pts',(41.1264949828601,-6.91408374142877,336.099368624889));
#72296=CARTESIAN_POINT('Ctrl Pts',(40.8482569485863,-2.8171249118577,341.409131968363));
#72297=CARTESIAN_POINT('Ctrl Pts',(40.5700189143122,3.86506786862965,340.8373295031));
#72298=CARTESIAN_POINT('Ctrl Pts',(40.2917808800384,7.00034491438379,334.908695911688));
#72299=CARTESIAN_POINT('Ctrl Pts',(40.0135428457643,3.7115087571295,329.063850734471));
#72300=CARTESIAN_POINT('Ctrl Pts',(39.7353048114905,-2.98332420476309,328.666522120813));
#72301=CARTESIAN_POINT('Ctrl Pts',(39.4570667772165,-6.94040457773766,334.081332674903));
#72302=CARTESIAN_POINT('Ctrl Pts',(39.1788287429426,-4.52837810992604,340.339190673728));
#72303=CARTESIAN_POINT('Ctrl Pts',(38.9005907086686,2.03927411061338,341.697352197598));
#72304=CARTESIAN_POINT('Ctrl Pts',(38.6223526743947,6.73551457947943,336.909452462488));
#72305=CARTESIAN_POINT('Ctrl Pts',(38.3441146401207,5.25067273478944,330.369276386027));
#72306=CARTESIAN_POINT('Ctrl Pts',(38.0658766058468,-1.05263397881429,328.078647020738));
#72307=CARTESIAN_POINT('Ctrl Pts',(37.7876385715729,-6.38995402691219,332.139641125518));
#72308=CARTESIAN_POINT('Ctrl Pts',(37.509400537299,-5.86330758007963,338.825544350581));
#72309=CARTESIAN_POINT('Ctrl Pts',(37.2311625030249,0.0440096907140084,
342.000801990059));
#72310=CARTESIAN_POINT('Ctrl Pts',(36.9529244687511,5.91093991792135,338.751526974927));
#72311=CARTESIAN_POINT('Ctrl Pts',(36.6746864344771,6.35348782778246,332.059531027352));
#72312=CARTESIAN_POINT('Ctrl Pts',(36.3964484002031,0.965533735414213,328.065960054726));
#72313=CARTESIAN_POINT('Ctrl Pts',(36.1182103659293,-5.30847641468909,330.435655193615));
#72314=CARTESIAN_POINT('Ctrl Pts',(35.8399723316553,-6.71097611201565,336.993982191705));
#72315=CARTESIAN_POINT('Ctrl Pts',(35.5617342973813,-1.95491208519051,341.722461163596));
#72316=CARTESIAN_POINT('Ctrl Pts',(35.2834962631074,4.5951459077589,340.281836749019));
#72317=CARTESIAN_POINT('Ctrl Pts',(35.0052582288335,6.92830632540037,333.994148709649));
#72318=CARTESIAN_POINT('Ctrl Pts',(34.7270201945596,2.90346228985566,328.629515553095));
#72319=CARTESIAN_POINT('Ctrl Pts',(34.4487821602856,-3.78584623405643,329.110981945268));
#72320=CARTESIAN_POINT('Ctrl Pts',(34.1705441260117,-7.00093954797376,334.996713284505));
#72321=CARTESIAN_POINT('Ctrl Pts',(33.8923060917377,-3.79137397241392,340.88546079404));
#72322=CARTESIAN_POINT('Ctrl Pts',(33.6140680574638,2.89747953704209,341.373207802144));
#72323=CARTESIAN_POINT('Ctrl Pts',(33.3358300231898,6.92735884208241,336.012356078614));
#72324=CARTESIAN_POINT('Ctrl Pts',(33.057591988916,4.60010318539263,329.72248012409));
#72325=CARTESIAN_POINT('Ctrl Pts',(32.779353954642,-1.94859926712026,328.275706263624));
#72326=CARTESIAN_POINT('Ctrl Pts',(32.5011159203681,-6.70910093347492,332.999717514618));
#72327=CARTESIAN_POINT('Ctrl Pts',(32.2228778860941,-5.31275969934711,339.559358478325));
#72328=CARTESIAN_POINT('Ctrl Pts',(31.9446398518202,0.959022694666936,341.934943462494));
#72329=CARTESIAN_POINT('Ctrl Pts',(31.6664018175462,6.35072411693689,337.946433190731));
#72330=CARTESIAN_POINT('Ctrl Pts',(31.3881637832723,5.91445975362818,331.254024669115));
#72331=CARTESIAN_POINT('Ctrl Pts',(31.1099257489983,0.050582971697756,327.999242418148));
#72332=CARTESIAN_POINT('Ctrl Pts',(30.8316877147243,-5.85971305675627,331.168952069034));
#72333=CARTESIAN_POINT('Ctrl Pts',(30.5534496804505,-6.392636902248,337.854357859992));
#72334=CARTESIAN_POINT('Ctrl Pts',(30.2752116461766,-1.05913221771276,341.920361573089));
#72335=CARTESIAN_POINT('Ctrl Pts',(29.9969736119026,5.24632247025157,339.63565161493));
#72336=CARTESIAN_POINT('Ctrl Pts',(29.7187355776287,6.73730446285876,333.096872591859));
#72337=CARTESIAN_POINT('Ctrl Pts',(29.4404975433547,2.04556159235134,328.30456550112));
#72338=CARTESIAN_POINT('Ctrl Pts',(29.1622595090808,-4.52336295901732,329.656559825556));
#72339=CARTESIAN_POINT('Ctrl Pts',(28.8840214748068,-6.94126408762359,335.912150329029));
#72340=CARTESIAN_POINT('Ctrl Pts',(28.6057834405329,-2.98926961590786,341.330673938871));
#72341=CARTESIAN_POINT('Ctrl Pts',(28.327545406259,3.70593346077893,340.939631515604));
#72342=CARTESIAN_POINT('Ctrl Pts',(28.0493073719851,7.00025609999755,335.097876919286));
#72343=CARTESIAN_POINT('Ctrl Pts',(27.7710693377112,3.8705470398592,329.1663021188));
#72344=CARTESIAN_POINT('Ctrl Pts',(27.4928313034371,-2.81110590957726,328.588225758652));
#72345=CARTESIAN_POINT('Ctrl Pts',(27.2145932691633,-6.9130484576499,333.894139982156));
#72346=CARTESIAN_POINT('Ctrl Pts',(26.9363552348893,-4.67098847256519,340.214885621569));
#72347=CARTESIAN_POINT('Ctrl Pts',(26.6581172006154,1.85756869011575,341.750007697653));
#72348=CARTESIAN_POINT('Ctrl Pts',(26.3798791663414,6.68146248354638,337.090747339552));
#72349=CARTESIAN_POINT('Ctrl Pts',(26.1016411320675,5.37387677405111,330.512839007323));
#72350=CARTESIAN_POINT('Ctrl Pts',(25.8234030977935,-0.865236332699702,
328.052732087688));
#72351=CARTESIAN_POINT('Ctrl Pts',(25.5451650635196,-6.31033482779934,331.968030389673));
#72352=CARTESIAN_POINT('Ctrl Pts',(25.2669270292457,-5.9645321918169,338.665722451259));
#72353=CARTESIAN_POINT('Ctrl Pts',(24.9886889949716,-0.145166399754938,
341.999435125299));
#72354=CARTESIAN_POINT('Ctrl Pts',(24.7104509606978,5.80741645470958,338.909869496345));
#72355=CARTESIAN_POINT('Ctrl Pts',(24.4322129264239,6.43061894601348,332.232274340175));
#72356=CARTESIAN_POINT('Ctrl Pts',(24.1539748921499,1.15253734634087,328.094580170463));
#72357=CARTESIAN_POINT('Ctrl Pts',(23.875736857876,-5.18321076464542,330.293887854488));
#72358=CARTESIAN_POINT('Ctrl Pts',(23.5974988236019,-6.76240286098208,336.811925192347));
#72359=CARTESIAN_POINT('Ctrl Pts',(23.319260789328,-2.1358376646981,341.667185525164));
#72360=CARTESIAN_POINT('Ctrl Pts',(23.0410227550542,4.45075423156706,340.404068109033));
#72361=CARTESIAN_POINT('Ctrl Pts',(22.7627847207802,6.95295466254791,334.18171715316));
#72362=CARTESIAN_POINT('Ctrl Pts',(22.4845466865063,3.07453122515114,328.710292287995));
#72363=CARTESIAN_POINT('Ctrl Pts',(22.2063086522324,-3.62534413756034,329.010839354206));
#72364=CARTESIAN_POINT('Ctrl Pts',(21.9280706179584,-6.99829469522445,334.807550745195));
#72365=CARTESIAN_POINT('Ctrl Pts',(21.6498325836845,-3.94901350574146,340.780869976773));
#72366=CARTESIAN_POINT('Ctrl Pts',(21.3715945494105,2.72421909061666,341.449170156168));
#72367=CARTESIAN_POINT('Ctrl Pts',(21.0933565151366,6.89747603692375,336.199162072843));
#72368=CARTESIAN_POINT('Ctrl Pts',(20.8151184808627,4.74102103072533,329.848700654873));
#72369=CARTESIAN_POINT('Ctrl Pts',(20.5368804465887,-1.76619899801402,328.225510612874));
#72370=CARTESIAN_POINT('Ctrl Pts',(20.2586424123147,-6.65260427533037,332.81916949014));
#72371=CARTESIAN_POINT('Ctrl Pts',(19.9804043780408,-5.4340128014542,339.4141443373));
#72372=CARTESIAN_POINT('Ctrl Pts',(19.7021663437669,0.771292014419021,341.958324078784));
#72373=CARTESIAN_POINT('Ctrl Pts',(19.423928309493,6.26879353291137,338.116952517862));
#72374=CARTESIAN_POINT('Ctrl Pts',(19.145690275219,6.01351575349184,331.415199637444));
#72375=CARTESIAN_POINT('Ctrl Pts',(18.8674522409451,0.239723326439865,328.003165138176));
#72376=CARTESIAN_POINT('Ctrl Pts',(18.5892142066711,-5.75405965897546,331.01202271849));
#72377=CARTESIAN_POINT('Ctrl Pts',(18.3109761723972,-6.46742702513038,337.6805881876));
#72378=CARTESIAN_POINT('Ctrl Pts',(18.0327381381232,-1.24573206938954,341.889217442364));
#72379=CARTESIAN_POINT('Ctrl Pts',(17.7545001038494,5.11915281945485,339.775713534955));
#72380=CARTESIAN_POINT('Ctrl Pts',(17.4762620695754,6.78626672445732,333.279607805933));
#72381=CARTESIAN_POINT('Ctrl Pts',(17.1980240353015,2.2257238215579,328.36228060046));
#72382=CARTESIAN_POINT('Ctrl Pts',(16.9197860010275,-4.37733298075532,329.536290515367));
#72383=CARTESIAN_POINT('Ctrl Pts',(16.6415479667536,-6.96337591595852,335.724265980102));
#72384=CARTESIAN_POINT('Ctrl Pts',(16.3633099324796,-3.15923155234616,341.247593245045));
#72385=CARTESIAN_POINT('Ctrl Pts',(16.0850718982057,3.54409297667212,341.037596403337));
#72386=CARTESIAN_POINT('Ctrl Pts',(15.8068338639318,6.99505569172662,335.286986457062));
#72387=CARTESIAN_POINT('Ctrl Pts',(15.5285958296578,4.02675904533329,329.273013275055));
#72388=CARTESIAN_POINT('Ctrl Pts',(15.2503577953839,-2.63683494209051,328.514611280344));
#72389=CARTESIAN_POINT('Ctrl Pts',(14.9721197611099,-6.88064442278876,333.707754789481));
#72390=CARTESIAN_POINT('Ctrl Pts',(14.693881726836,-4.81018807481828,340.086772654803));
#72391=CARTESIAN_POINT('Ctrl Pts',(14.4156436925621,1.67450687111428,341.797734335452));
#72392=CARTESIAN_POINT('Ctrl Pts',(14.1374056582881,6.62253157717988,337.270515550857));
#72393=CARTESIAN_POINT('Ctrl Pts',(13.8591676240142,5.49315680313418,330.65967815798));
#72394=CARTESIAN_POINT('Ctrl Pts',(13.5809295897403,-0.677206890023213,
328.031890056511));
#72395=CARTESIAN_POINT('Ctrl Pts',(13.3026915554662,-6.22610781625971,331.798633600986));
#72396=CARTESIAN_POINT('Ctrl Pts',(13.0244535211924,-6.06140149577904,338.503223837862));
#72397=CARTESIAN_POINT('Ctrl Pts',(12.7462154869185,-0.334236490530462,
341.992957266009));
#72398=CARTESIAN_POINT('Ctrl Pts',(12.4679774526445,5.69965241209585,339.065357027443));
#72399=CARTESIAN_POINT('Ctrl Pts',(12.1897394183706,6.50305441656604,332.407038648561));
#72400=CARTESIAN_POINT('Ctrl Pts',(11.9115013840966,1.33869937978922,328.128242631365));
#72401=CARTESIAN_POINT('Ctrl Pts',(11.6332633498227,-5.05416034113784,330.155556921528));
#72402=CARTESIAN_POINT('Ctrl Pts',(11.3550253155488,-6.80889167382486,336.628545126353));
#72403=CARTESIAN_POINT('Ctrl Pts',(11.0767872812748,-2.31520369669645,341.607041495793));
#72404=CARTESIAN_POINT('Ctrl Pts',(10.7985492470008,4.30311269193076,340.52235342361));
#72405=CARTESIAN_POINT('Ctrl Pts',(10.5203112127269,6.97252579115532,334.369883087956));
#72406=CARTESIAN_POINT('Ctrl Pts',(10.242073178453,3.2433554259048,328.795661810754));
#72407=CARTESIAN_POINT('Ctrl Pts',(9.96383514417902,-3.46219536102038,328.915069984074));
#72408=CARTESIAN_POINT('Ctrl Pts',(9.6855971099051,-6.99053864265773,334.618528864805));
#72409=CARTESIAN_POINT('Ctrl Pts',(9.40735907563116,-4.10377142576636,340.672057712784));
#72410=CARTESIAN_POINT('Ctrl Pts',(9.12912104135721,2.54897311806734,341.520423791441));
#72411=CARTESIAN_POINT('Ctrl Pts',(8.85088300708329,6.86254969911119,336.385091547203));
#72412=CARTESIAN_POINT('Ctrl Pts',(8.57264497280934,4.87849017425162,329.978684351033));
#72413=CARTESIAN_POINT('Ctrl Pts',(8.29440693853538,-1.58253396617214,328.180258525862));
#72414=CARTESIAN_POINT('Ctrl Pts',(8.01616890426149,-6.59120282966596,332.640219905419));
#72415=CARTESIAN_POINT('Ctrl Pts',(7.7379308699875,-5.55138682090592,339.265695663652));
#72416=CARTESIAN_POINT('Ctrl Pts',(7.45969283571361,0.583165882706493,341.976645094441));
#72417=CARTESIAN_POINT('Ctrl Pts',(7.18145480143964,6.18196872210066,338.285155485332));
#72418=CARTESIAN_POINT('Ctrl Pts',(6.90321676716572,6.10877882471154,331.579068422606));
#72419=CARTESIAN_POINT('Ctrl Pts',(6.62497873289175,0.427558700872944,328.012053184046));
#72420=CARTESIAN_POINT('Ctrl Pts',(6.34674069861787,-5.64206691036484,330.858276072185));
#72421=CARTESIAN_POINT('Ctrl Pts',(6.06850266434387,-6.5415653170953,337.504356491304));
#72422=CARTESIAN_POINT('Ctrl Pts',(5.79026463006997,-1.42345620119259,341.853942631986));
#72423=CARTESIAN_POINT('Ctrl Pts',(5.55839960150834,3.905186457329,340.234875251695));
#72424=CARTESIAN_POINT('Ctrl Pts',(5.37290757865905,5.92636084688762,336.684629902852));
#72425=CARTESIAN_POINT('Ctrl Pts',(5.2801615672344,5.99240691187019,334.662430744869));
#72426=CARTESIAN_POINT('Ctrl Pts',(5.23378856152207,5.77608186237172,333.700728996892));
#72427=CARTESIAN_POINT('Ctrl Pts',(185.616456506696,3.24370764223164,339.546070274699));
#72428=CARTESIAN_POINT('Ctrl Pts',(185.570073697003,4.00077982359114,339.005888754628));
#72429=CARTESIAN_POINT('Ctrl Pts',(185.477317881598,5.22618675040964,337.542420441747));
#72430=CARTESIAN_POINT('Ctrl Pts',(185.291816054769,6.03764046862974,333.775028658698));
#72431=CARTESIAN_POINT('Ctrl Pts',(185.059951026208,3.30915017218641,329.285814453217));
#72432=CARTESIAN_POINT('Ctrl Pts',(184.781712991934,-3.02460665970507,329.125603768544));
#72433=CARTESIAN_POINT('Ctrl Pts',(184.50347495766,-6.57144526074855,334.364156891581));
#72434=CARTESIAN_POINT('Ctrl Pts',(184.225236923386,-4.09364090229947,340.182150482619));
#72435=CARTESIAN_POINT('Ctrl Pts',(183.946998889112,2.14393674640899,341.246697212283));
#72436=CARTESIAN_POINT('Ctrl Pts',(183.668760854838,6.41241529034084,336.577612734481));
#72437=CARTESIAN_POINT('Ctrl Pts',(183.390522820564,4.79718333645851,330.461374221489));
#72438=CARTESIAN_POINT('Ctrl Pts',(183.11228478629,-1.22081282736175,328.509848981737));
#72439=CARTESIAN_POINT('Ctrl Pts',(182.834046752016,-6.11824353328202,332.514407213301));
#72440=CARTESIAN_POINT('Ctrl Pts',(182.555808717742,-5.40118143611244,338.799868456314));
#72441=CARTESIAN_POINT('Ctrl Pts',(182.277570683468,0.272533453155054,341.598293532569));
#72442=CARTESIAN_POINT('Ctrl Pts',(181.999332649194,5.69611223808,338.341537117564));
#72443=CARTESIAN_POINT('Ctrl Pts',(181.72109461492,5.89247205606371,332.018314601662));
#72444=CARTESIAN_POINT('Ctrl Pts',(181.442856580647,0.681387094013621,328.431333780266));
#72445=CARTESIAN_POINT('Ctrl Pts',(181.164618546372,-5.1549913731018,330.872324695149));
#72446=CARTESIAN_POINT('Ctrl Pts',(180.886380512099,-6.26071319068405,337.101220353486));
#72447=CARTESIAN_POINT('Ctrl Pts',(180.608142477824,-1.62106941389026,341.401858145107));
#72448=CARTESIAN_POINT('Ctrl Pts',(180.329904443551,4.50620503883413,339.827604658656));
#72449=CARTESIAN_POINT('Ctrl Pts',(180.051666409277,6.49820206165478,333.823129923343));
#72450=CARTESIAN_POINT('Ctrl Pts',(179.773428375003,2.5268947419063,328.898651332658));
#72451=CARTESIAN_POINT('Ctrl Pts',(179.495190340729,-3.7633064670093,329.573290439871));
#72452=CARTESIAN_POINT('Ctrl Pts',(179.216952306455,-6.59997694026069,335.227940769077));
#72453=CARTESIAN_POINT('Ctrl Pts',(178.938714272181,-3.37994595767685,340.673413241798));
#72454=CARTESIAN_POINT('Ctrl Pts',(178.660476237907,2.94181152473292,340.912478109838));
#72455=CARTESIAN_POINT('Ctrl Pts',(178.382238203633,6.56391200129043,335.725749090934));
#72456=CARTESIAN_POINT('Ctrl Pts',(178.104000169359,4.1624073125058,329.873010839919));
#72457=CARTESIAN_POINT('Ctrl Pts',(177.825762135086,-2.05887712731774,328.725234868675));
#72458=CARTESIAN_POINT('Ctrl Pts',(177.547524100811,-6.39076041776407,333.335718242113));
#72459=CARTESIAN_POINT('Ctrl Pts',(177.269286066538,-4.85793719956362,339.47348842051));
#72460=CARTESIAN_POINT('Ctrl Pts',(176.991048032263,1.13294328325218,341.506004303719));
#72461=CARTESIAN_POINT('Ctrl Pts',(176.71280999799,6.08413843744873,337.568056066012));
#72462=CARTESIAN_POINT('Ctrl Pts',(176.434571963715,5.45200954922573,331.273440680897));
#72463=CARTESIAN_POINT('Ctrl Pts',(176.156333929442,-0.183348030734939,
328.398633779037));
#72464=CARTESIAN_POINT('Ctrl Pts',(175.878095895168,-5.65044982913321,331.581803222127));
#72465=CARTESIAN_POINT('Ctrl Pts',(175.599857860894,-5.93221721982255,337.901801395782));
#72466=CARTESIAN_POINT('Ctrl Pts',(175.32161982662,-0.770076427271954,341.558859259039));
#72467=CARTESIAN_POINT('Ctrl Pts',(175.043381792346,5.0987521362812,339.196948788884));
#72468=CARTESIAN_POINT('Ctrl Pts',(174.765143758072,6.28853112182489,332.983560362031));
#72469=CARTESIAN_POINT('Ctrl Pts',(174.486905723798,1.70741791543838,328.620628828343));
#72470=CARTESIAN_POINT('Ctrl Pts',(174.208667689524,-4.44056751049949,330.111952059519));
#72471=CARTESIAN_POINT('Ctrl Pts',(173.93042965525,-6.51350967472065,336.088964738207));
#72472=CARTESIAN_POINT('Ctrl Pts',(173.652191620976,-2.60910014969608,341.066650549734));
#72473=CARTESIAN_POINT('Ctrl Pts',(173.373953586702,3.68964207244958,340.477060695386));
#72474=CARTESIAN_POINT('Ctrl Pts',(173.095715552428,6.60245422373594,334.861253082165));
#72475=CARTESIAN_POINT('Ctrl Pts',(172.817477518154,3.45629158596449,329.372771467541));
#72476=CARTESIAN_POINT('Ctrl Pts',(172.53923948388,-2.86165882546639,329.048314419396));
#72477=CARTESIAN_POINT('Ctrl Pts',(172.261001449607,-6.5535071707818,334.185631381837));
#72478=CARTESIAN_POINT('Ctrl Pts',(171.982763415333,-4.23129871507806,340.070282405105));
#72479=CARTESIAN_POINT('Ctrl Pts',(171.704525381059,1.97391011758615,341.302010102454));
#72480=CARTESIAN_POINT('Ctrl Pts',(171.426287346785,6.36769077020714,336.750476146298));
#72481=CARTESIAN_POINT('Ctrl Pts',(171.148049312511,4.91793558997074,330.59255606767));
#72482=CARTESIAN_POINT('Ctrl Pts',(170.869811278237,-1.0449364925714,328.479282231975));
#72483=CARTESIAN_POINT('Ctrl Pts',(170.591573243963,-6.04888577911817,332.349974846361));
#72484=CARTESIAN_POINT('Ctrl Pts',(170.313335209689,-5.50186186757595,338.652556429933));
#72485=CARTESIAN_POINT('Ctrl Pts',(170.035097175415,0.0941394724926572,
341.603240889401));
#72486=CARTESIAN_POINT('Ctrl Pts',(169.756859141141,5.60375040815109,338.49422864834));
#72487=CARTESIAN_POINT('Ctrl Pts',(169.478621106867,5.97088230546971,332.178614351428));
#72488=CARTESIAN_POINT('Ctrl Pts',(169.200383072593,0.858623641137144,328.452144020627));
#72489=CARTESIAN_POINT('Ctrl Pts',(168.922145038319,-5.04158126540281,330.7345444759));
#72490=CARTESIAN_POINT('Ctrl Pts',(168.643907004046,-6.31520145830011,336.931290507619));
#72491=CARTESIAN_POINT('Ctrl Pts',(168.365668969771,-1.79345448513614,341.355719746299));
#72492=CARTESIAN_POINT('Ctrl Pts',(168.087430935498,4.37411919769241,339.947598784068));
#72493=CARTESIAN_POINT('Ctrl Pts',(167.809192901223,6.52762825469221,333.999139444138));
#72494=CARTESIAN_POINT('Ctrl Pts',(167.53095486695,2.69082920999616,328.969155063644));
#72495=CARTESIAN_POINT('Ctrl Pts',(167.252716832675,-3.61530408413933,329.473588066119));
#72496=CARTESIAN_POINT('Ctrl Pts',(166.974478798402,-6.60372618206099,335.04952773061));
#72497=CARTESIAN_POINT('Ctrl Pts',(166.696240764128,-3.53200623354396,340.580016527749));
#72498=CARTESIAN_POINT('Ctrl Pts',(166.418002729854,2.78098370316982,340.989806518281));
#72499=CARTESIAN_POINT('Ctrl Pts',(166.13976469558,6.54190594273683,335.902839476387));
#72500=CARTESIAN_POINT('Ctrl Pts',(165.861526661306,4.2994176570277,329.987349972901));
#72501=CARTESIAN_POINT('Ctrl Pts',(165.583288627032,-1.88858275323517,328.671895412691));
#72502=CARTESIAN_POINT('Ctrl Pts',(165.305050592758,-6.34345864628985,333.163649029584));
#72503=CARTESIAN_POINT('Ctrl Pts',(165.026812558484,-4.97703616894048,339.340594827532));
#72504=CARTESIAN_POINT('Ctrl Pts',(164.74857452421,0.956738939712131,341.534240819328));
#72505=CARTESIAN_POINT('Ctrl Pts',(164.470336489937,6.01252884483452,337.731510456463));
#72506=CARTESIAN_POINT('Ctrl Pts',(164.192098455662,5.55070977383256,331.422113264731));
#72507=CARTESIAN_POINT('Ctrl Pts',(163.913860421389,-0.00491372827345363,
328.396089920433));
#72508=CARTESIAN_POINT('Ctrl Pts',(163.635622387114,-5.55602797446947,331.430377382601));
#72509=CARTESIAN_POINT('Ctrl Pts',(163.357384352841,-6.00845735533339,337.740454833212));
#72510=CARTESIAN_POINT('Ctrl Pts',(163.079146318566,-0.947014105893046,
341.535657332433));
#72511=CARTESIAN_POINT('Ctrl Pts',(162.800908284293,4.98349001062004,339.333183563823));
#72512=CARTESIAN_POINT('Ctrl Pts',(162.522670250019,6.34071890057911,333.154211196378));
#72513=CARTESIAN_POINT('Ctrl Pts',(162.244432215745,1.87916364433428,328.669091970219));
#72514=CARTESIAN_POINT('Ctrl Pts',(161.966194181471,-4.30687235190619,329.99375359894));
#72515=CARTESIAN_POINT('Ctrl Pts',(161.687956147197,-6.54055516013407,335.912573657838));
#72516=CARTESIAN_POINT('Ctrl Pts',(161.409718112923,-2.77206703634281,340.993938340504));
#72517=CARTESIAN_POINT('Ctrl Pts',(161.131480078649,3.54030609105783,340.574754278473));
#72518=CARTESIAN_POINT('Ctrl Pts',(160.853242044375,6.60379257352697,335.039700498327));
#72519=CARTESIAN_POINT('Ctrl Pts',(160.575004010101,3.60707608308904,329.468214156844));
#72520=CARTESIAN_POINT('Ctrl Pts',(160.296765975827,-2.69980088844387,328.9731660346));
#72521=CARTESIAN_POINT('Ctrl Pts',(160.018527941553,-6.52911043364773,334.008854486481));
#72522=CARTESIAN_POINT('Ctrl Pts',(159.740289907279,-4.36675170340512,339.954102546833));
#72523=CARTESIAN_POINT('Ctrl Pts',(159.462051873005,1.80291061190286,341.353043822392));
#72524=CARTESIAN_POINT('Ctrl Pts',(159.183813838731,6.31806846958463,336.921890552913));
#72525=CARTESIAN_POINT('Ctrl Pts',(158.905575804457,5.0352281472663,330.727046690085));
#72526=CARTESIAN_POINT('Ctrl Pts',(158.627337770184,-0.868366725952659,
328.453429011078));
#72527=CARTESIAN_POINT('Ctrl Pts',(158.34909973591,-5.97507427183675,332.187502901376));
#72528=CARTESIAN_POINT('Ctrl Pts',(158.070861701636,-5.59854435040793,338.502563866691));
#72529=CARTESIAN_POINT('Ctrl Pts',(157.792623667362,-0.0843129129889187,
341.603373669303));
#72530=CARTESIAN_POINT('Ctrl Pts',(157.514385633088,5.50729124022346,338.64436492123));
#72531=CARTESIAN_POINT('Ctrl Pts',(157.236147598814,6.04493550976823,332.340976275684));
#72532=CARTESIAN_POINT('Ctrl Pts',(156.95790956454,1.03523168510056,328.477734454815));
#72533=CARTESIAN_POINT('Ctrl Pts',(156.679671530266,-4.92448897698921,330.599879456282));
#72534=CARTESIAN_POINT('Ctrl Pts',(156.401433495992,-6.36507879023421,336.759950135045));
#72535=CARTESIAN_POINT('Ctrl Pts',(156.123195461718,-1.96452974609034,341.3049405517));
#72536=CARTESIAN_POINT('Ctrl Pts',(155.844957427444,4.23883924962917,340.063980084828));
#72537=CARTESIAN_POINT('Ctrl Pts',(155.56671939317,6.55228803112875,334.175879838335));
#72538=CARTESIAN_POINT('Ctrl Pts',(155.288481358896,2.85279879807429,329.044062500207));
#72539=CARTESIAN_POINT('Ctrl Pts',(155.010243324622,-3.46466178473171,329.377921096147));
#72540=CARTESIAN_POINT('Ctrl Pts',(154.732005290348,-6.60265338601353,334.871078520404));
#72541=CARTESIAN_POINT('Ctrl Pts',(154.453767256075,-3.68148742995497,340.482545283609));
#72542=CARTESIAN_POINT('Ctrl Pts',(154.1755292218,2.61812520190787,341.062761162283));
#72543=CARTESIAN_POINT('Ctrl Pts',(153.897291187527,6.5151229794445,336.079270608537));
#72544=CARTESIAN_POINT('Ctrl Pts',(153.619053153253,4.43328856180245,330.105349347346));
#72545=CARTESIAN_POINT('Ctrl Pts',(153.340815118979,-1.7169093337738,328.62317674517));
#72546=CARTESIAN_POINT('Ctrl Pts',(153.062577084705,-6.29152487528601,332.992920722196));
#72547=CARTESIAN_POINT('Ctrl Pts',(152.784339050431,-5.0925009015033,339.204531728019));
#72548=CARTESIAN_POINT('Ctrl Pts',(152.506101016157,0.779835984398815,341.557706025828));
#72549=CARTESIAN_POINT('Ctrl Pts',(152.227862981883,5.93652889777846,337.892970295316));
#72550=CARTESIAN_POINT('Ctrl Pts',(151.949624947609,5.64535686468971,331.573398424964));
#72551=CARTESIAN_POINT('Ctrl Pts',(151.671386913335,0.173524162205951,328.398368243467));
#72552=CARTESIAN_POINT('Ctrl Pts',(151.393148879061,-5.45754910272178,331.281558085015));
#72553=CARTESIAN_POINT('Ctrl Pts',(151.114910844787,-6.08031010937444,337.577107187832));
#72554=CARTESIAN_POINT('Ctrl Pts',(150.836672810513,-1.12326027388429,341.507683062416));
#72555=CARTESIAN_POINT('Ctrl Pts',(150.558434776239,4.86458893565501,339.466254243865));
#72556=CARTESIAN_POINT('Ctrl Pts',(150.280196741966,6.38827668015871,333.326209827524));
#72557=CARTESIAN_POINT('Ctrl Pts',(150.001958707691,2.04953720609002,328.722177947362));
#72558=CARTESIAN_POINT('Ctrl Pts',(149.723720673418,-4.17003231088781,329.879210704404));
#72559=CARTESIAN_POINT('Ctrl Pts',(149.445482639144,-6.56282472574003,335.735516215289));
#72560=CARTESIAN_POINT('Ctrl Pts',(149.16724460487,-2.93300975691482,340.916849351605));
#72561=CARTESIAN_POINT('Ctrl Pts',(148.889006570596,3.38838497467808,340.668377170506));
#72562=CARTESIAN_POINT('Ctrl Pts',(148.610768536322,6.60030882748914,335.218118925144));
#72563=CARTESIAN_POINT('Ctrl Pts',(148.332530502048,3.75522668971203,329.567696161608));
#72564=CARTESIAN_POINT('Ctrl Pts',(148.054292467774,-2.53597155415873,328.90241844989));
#72565=CARTESIAN_POINT('Ctrl Pts',(147.7760544335,-6.49994613365681,333.832801326553));
#72566=CARTESIAN_POINT('Ctrl Pts',(147.497816399226,-4.4990160853457,339.834305198013));
#72567=CARTESIAN_POINT('Ctrl Pts',(147.219578364952,1.63059461911859,341.399438543485));
#72568=CARTESIAN_POINT('Ctrl Pts',(146.941340330678,6.26383270915488,337.091901593159));
#72569=CARTESIAN_POINT('Ctrl Pts',(146.663102296404,5.14884397601897,330.864657427207));
#72570=CARTESIAN_POINT('Ctrl Pts',(146.38486426213,-0.691162877096977,328.432356102752));
#72571=CARTESIAN_POINT('Ctrl Pts',(146.106626227856,-5.89689975944835,332.027084644536));
#72572=CARTESIAN_POINT('Ctrl Pts',(145.828388193583,-5.69113877065188,338.350013727871));
#72573=CARTESIAN_POINT('Ctrl Pts',(145.550150159308,-0.26270373309874,341.59868465926));
#72574=CARTESIAN_POINT('Ctrl Pts',(145.271912125034,5.40681064281838,338.791840075272));
#72575=CARTESIAN_POINT('Ctrl Pts',(144.993674090761,6.11457469621534,332.505279821676));
#72576=CARTESIAN_POINT('Ctrl Pts',(144.715436056487,1.21108380187007,328.508087453717));
#72577=CARTESIAN_POINT('Ctrl Pts',(144.437198022213,-4.80380082188375,330.468427409011));
#72578=CARTESIAN_POINT('Ctrl Pts',(144.158959987939,-6.41030833537875,336.587324645153));
#72579=CARTESIAN_POINT('Ctrl Pts',(143.880721953665,-2.13417050549261,341.249557483312));
#72580=CARTESIAN_POINT('Ctrl Pts',(143.602483919391,4.10046409697908,340.176663662353));
#72581=CARTESIAN_POINT('Ctrl Pts',(143.324245885117,6.57216332040393,334.353222005882));
#72582=CARTESIAN_POINT('Ctrl Pts',(143.046007850843,3.01268526966569,329.123318968187));
#72583=CARTESIAN_POINT('Ctrl Pts',(142.767769816569,-3.31148958588299,329.286359373715));
#72584=CARTESIAN_POINT('Ctrl Pts',(142.489531782295,-6.59675932597306,334.692723448789));
#72585=CARTESIAN_POINT('Ctrl Pts',(142.211293748021,-3.82828040062582,340.381070679513));
#72586=CARTESIAN_POINT('Ctrl Pts',(141.933055713747,2.45335494304968,341.131288772122));
#72587=CARTESIAN_POINT('Ctrl Pts',(141.654817679474,6.48358266694808,336.254913656228));
#72588=CARTESIAN_POINT('Ctrl Pts',(141.376579645199,4.56392227491153,330.226922800509));
#72589=CARTESIAN_POINT('Ctrl Pts',(141.098341610926,-1.54398222542898,328.579114440258));
#72590=CARTESIAN_POINT('Ctrl Pts',(140.820103576652,-6.2349970266336,332.823657986068));
#72591=CARTESIAN_POINT('Ctrl Pts',(140.541865542377,-5.20424708490183,339.065398475307));
#72592=CARTESIAN_POINT('Ctrl Pts',(140.263627508104,0.602363592083287,341.57638278894));
#72593=CARTESIAN_POINT('Ctrl Pts',(139.98538947383,5.85619409148563,338.052317684414));
#72594=CARTESIAN_POINT('Ctrl Pts',(139.707151439556,5.7358817104147,331.727185693036));
#72595=CARTESIAN_POINT('Ctrl Pts',(139.428913405282,0.351835345171481,328.405467084499));
#72596=CARTESIAN_POINT('Ctrl Pts',(139.150675371008,-5.35508512325443,331.135453997371));
#72597=CARTESIAN_POINT('Ctrl Pts',(138.872437336734,-6.14772301499658,337.41187773625));
#72598=CARTESIAN_POINT('Ctrl Pts',(138.59419930246,-1.29868623611949,341.47495687583));
#72599=CARTESIAN_POINT('Ctrl Pts',(138.315961268186,4.74213573306708,339.596063660667));
#72600=CARTESIAN_POINT('Ctrl Pts',(138.037723233912,6.43116973382671,333.499430661899));
#72601=CARTESIAN_POINT('Ctrl Pts',(137.759485199638,2.21841419376326,328.779847996339));
#72602=CARTESIAN_POINT('Ctrl Pts',(137.481247165364,-4.03014730817692,329.768407015246));
#72603=CARTESIAN_POINT('Ctrl Pts',(137.203009131091,-6.58030211027989,335.557921698075));
#72604=CARTESIAN_POINT('Ctrl Pts',(136.924771096816,-3.09181079087896,340.835439873493));
#72605=CARTESIAN_POINT('Ctrl Pts',(136.646533062543,3.23398965625914,340.757861007957));
#72606=CARTESIAN_POINT('Ctrl Pts',(136.368295028268,6.59200552945729,335.396378081309));
#72607=CARTESIAN_POINT('Ctrl Pts',(136.090056993995,3.90063522611462,329.671144839975));
#72608=CARTESIAN_POINT('Ctrl Pts',(135.811818959721,-2.37029045095188,328.836123325223));
#72609=CARTESIAN_POINT('Ctrl Pts',(135.533580925447,-6.46603556660954,333.657600456243));
#72610=CARTESIAN_POINT('Ctrl Pts',(135.255342891173,-4.62799528131817,339.710977834784));
#72611=CARTESIAN_POINT('Ctrl Pts',(134.977104856899,1.45708796454039,341.441160388263));
#72612=CARTESIAN_POINT('Ctrl Pts',(134.698866822625,6.20502309192341,337.260385124804));
#72613=CARTESIAN_POINT('Ctrl Pts',(134.420628788351,5.25870011383906,331.005287795542));
#72614=CARTESIAN_POINT('Ctrl Pts',(134.142390754077,-0.513454340428938,
328.416078894456));
#72615=CARTESIAN_POINT('Ctrl Pts',(133.864152719803,-5.81441932505895,331.868837213412));
#72616=CARTESIAN_POINT('Ctrl Pts',(133.585914685529,-5.77957751577092,338.195017405732));
#72617=CARTESIAN_POINT('Ctrl Pts',(133.307676651255,-0.440902726684218,
341.589177283193));
#72618=CARTESIAN_POINT('Ctrl Pts',(133.029438616981,5.30238198696701,338.936546423964));
#72619=CARTESIAN_POINT('Ctrl Pts',(132.751200582707,6.17974901420846,332.671405014795));
#72620=CARTESIAN_POINT('Ctrl Pts',(132.472962548433,1.38605158405674,328.543180853541));
#72621=CARTESIAN_POINT('Ctrl Pts',(132.194724514159,-4.67960492669601,330.3402843205));
#72622=CARTESIAN_POINT('Ctrl Pts',(131.916486479886,-6.45085706707532,336.413540089245));
#72623=CARTESIAN_POINT('Ctrl Pts',(131.638248445611,-2.30225289149384,341.189610981908));
#72624=CARTESIAN_POINT('Ctrl Pts',(131.360010411338,3.9590947814145,340.285567234982));
#72625=CARTESIAN_POINT('Ctrl Pts',(131.081772377064,6.58723960956198,334.531036451358));
#72626=CARTESIAN_POINT('Ctrl Pts',(130.80353434279,3.17037187551183,329.206866594432));
#72627=CARTESIAN_POINT('Ctrl Pts',(130.525296308516,-3.1558993340834,329.198969757288));
#72628=CARTESIAN_POINT('Ctrl Pts',(130.247058274242,-6.58604830578809,334.514592750813));
#72629=CARTESIAN_POINT('Ctrl Pts',(129.968820239968,-3.97227795718472,340.275666812319));
#72630=CARTESIAN_POINT('Ctrl Pts',(129.690582205694,2.28679324200054,341.195339308874));
#72631=CARTESIAN_POINT('Ctrl Pts',(129.41234417142,6.44730803601481,336.429640364734));
#72632=CARTESIAN_POINT('Ctrl Pts',(129.134106137146,4.69122340748892,330.351981559335));
#72633=CARTESIAN_POINT('Ctrl Pts',(128.855868102872,-1.36992769974558,328.539740672295));
#72634=CARTESIAN_POINT('Ctrl Pts',(128.577630068598,-6.17391637702325,332.655984417018));
#72635=CARTESIAN_POINT('Ctrl Pts',(128.299392034324,-5.31219312196306,338.923296664632));
#72636=CARTESIAN_POINT('Ctrl Pts',(128.021154000051,0.424451353280695,341.590257470875));
#72637=CARTESIAN_POINT('Ctrl Pts',(127.742915965776,5.77158308651039,338.209436268139));
#72638=CARTESIAN_POINT('Ctrl Pts',(127.464677931503,5.82221820967631,331.883362773332));
#72639=CARTESIAN_POINT('Ctrl Pts',(127.186439897228,0.529889617622296,328.417381259949));
#72640=CARTESIAN_POINT('Ctrl Pts',(126.908201862955,-5.24871085536584,330.992171805017));
#72641=CARTESIAN_POINT('Ctrl Pts',(126.629963828681,-6.21064684722995,337.244887129174));
#72642=CARTESIAN_POINT('Ctrl Pts',(126.351725794407,-1.47316389638836,341.437502669367));
#72643=CARTESIAN_POINT('Ctrl Pts',(126.073487760133,4.61621981830537,339.722517027267));
#72644=CARTESIAN_POINT('Ctrl Pts',(125.795249725859,6.46936674103309,333.67374721348));
#72645=CARTESIAN_POINT('Ctrl Pts',(125.517011691585,2.38567129321132,328.842060006424));
#72646=CARTESIAN_POINT('Ctrl Pts',(125.238773657311,-3.88731948793991,329.661423440427));
#72647=CARTESIAN_POINT('Ctrl Pts',(124.960535623037,-6.59297455175028,335.37991978589));
#72648=CARTESIAN_POINT('Ctrl Pts',(124.682297588763,-3.24835418156428,340.749769351449));
#72649=CARTESIAN_POINT('Ctrl Pts',(124.404059554489,3.07723287541413,340.843140449638));
#72650=CARTESIAN_POINT('Ctrl Pts',(124.125821520215,6.57888874250778,335.574347801809));
#72651=CARTESIAN_POINT('Ctrl Pts',(123.847583485941,4.04319551484074,329.778484653617));
#72652=CARTESIAN_POINT('Ctrl Pts',(123.569345451667,-2.20287855932757,328.774329069363));
#72653=CARTESIAN_POINT('Ctrl Pts',(123.291107417393,-6.42740349403529,333.4833798074));
#72654=CARTESIAN_POINT('Ctrl Pts',(123.012869383119,-4.75359511058692,339.584210510911));
#72655=CARTESIAN_POINT('Ctrl Pts',(122.734631348846,1.28251734289823,341.478178891393));
#72656=CARTESIAN_POINT('Ctrl Pts',(122.456393314572,6.14168256073063,337.427218121009));
#72657=CARTESIAN_POINT('Ctrl Pts',(122.178155280298,5.36471634366653,331.148835106654));
#72658=CARTESIAN_POINT('Ctrl Pts',(121.899917246024,-0.335370878896913,
328.404609271823));
#72659=CARTESIAN_POINT('Ctrl Pts',(121.62167921175,-5.72769319596271,331.712876160432));
#72660=CARTESIAN_POINT('Ctrl Pts',(121.343441177476,-5.86379600770653,338.037688078744));
#72661=CARTESIAN_POINT('Ctrl Pts',(121.065203143202,-0.61877977266526,341.574858483396));
#72662=CARTESIAN_POINT('Ctrl Pts',(120.786965108928,5.19408152657644,339.078378302588));
#72663=CARTESIAN_POINT('Ctrl Pts',(120.508727074654,6.24041087339662,332.83923055026));
#72664=CARTESIAN_POINT('Ctrl Pts',(120.23048904038,1.56000727001425,328.582989029054));
#72665=CARTESIAN_POINT('Ctrl Pts',(119.952251006106,-4.55199197939054,330.215543760959));
#72666=CARTESIAN_POINT('Ctrl Pts',(119.674012971832,-6.48669537660025,336.238723364973));
#72667=CARTESIAN_POINT('Ctrl Pts',(119.395774937558,-2.46865417017073,341.125144820479));
#72668=CARTESIAN_POINT('Ctrl Pts',(119.117536903284,3.81483453094864,340.39061128122));
#72669=CARTESIAN_POINT('Ctrl Pts',(118.83929886901,6.59750588988183,334.709193334478));
#72670=CARTESIAN_POINT('Ctrl Pts',(118.561060834736,3.32574347269777,329.294644372386));
#72671=CARTESIAN_POINT('Ctrl Pts',(118.282822800463,-2.99800464148784,329.115816058845));
#72672=CARTESIAN_POINT('Ctrl Pts',(118.004584766188,-6.57052814665602,334.336816497688));
#72673=CARTESIAN_POINT('Ctrl Pts',(117.726346731915,-4.11337495247446,340.166410648031));
#72674=CARTESIAN_POINT('Ctrl Pts',(117.448108697641,2.11856172227814,341.254866002772));
#72675=CARTESIAN_POINT('Ctrl Pts',(117.169870663367,6.40632557441585,336.603323148441));
#72676=CARTESIAN_POINT('Ctrl Pts',(116.891632629093,4.81509900412262,330.480434305795));
#72677=CARTESIAN_POINT('Ctrl Pts',(116.613394594819,-1.19487285150915,328.505084192042));
#72678=CARTESIAN_POINT('Ctrl Pts',(116.335156560545,-6.10832752760533,332.490022450452));
#72679=CARTESIAN_POINT('Ctrl Pts',(116.056918526271,-5.41626019038464,338.778330058875));
#72680=CARTESIAN_POINT('Ctrl Pts',(115.778680491997,0.246229179682688,341.599319940328));
#72681=CARTESIAN_POINT('Ctrl Pts',(115.500442457723,5.68275766589193,338.364211318346));
#72682=CARTESIAN_POINT('Ctrl Pts',(115.222204423449,5.90430331947782,332.041815625194));
#72683=CARTESIAN_POINT('Ctrl Pts',(114.943966389175,0.707556964153051,328.434102070073));
#72684=CARTESIAN_POINT('Ctrl Pts',(114.665728354901,-5.13850397365131,330.851816132751));
#72685=CARTESIAN_POINT('Ctrl Pts',(114.387490320627,-6.26903565903015,337.076257303309));
#72686=CARTESIAN_POINT('Ctrl Pts',(114.109252286354,-1.64656585093195,341.395347792128));
#72687=CARTESIAN_POINT('Ctrl Pts',(113.831014252079,4.48693313529438,339.84552200729));
#72688=CARTESIAN_POINT('Ctrl Pts',(113.552776217806,6.50283981028572,333.849032196149));
#72689=CARTESIAN_POINT('Ctrl Pts',(113.274538183532,2.55118637313611,328.908768550345));
#72690=CARTESIAN_POINT('Ctrl Pts',(112.996300149258,-3.74165314319136,329.558338099461));
#72691=CARTESIAN_POINT('Ctrl Pts',(112.718062114984,-6.60083279672198,335.201640455903));
#72692=CARTESIAN_POINT('Ctrl Pts',(112.43982408071,-3.40252562083322,340.659900342171));
#72693=CARTESIAN_POINT('Ctrl Pts',(112.161586046436,2.91822909609835,340.924153224421));
#72694=CARTESIAN_POINT('Ctrl Pts',(111.883348012162,6.56096804453132,335.751898132978));
#72695=CARTESIAN_POINT('Ctrl Pts',(111.605109977888,4.18280345822748,329.8896372229));
#72696=CARTESIAN_POINT('Ctrl Pts',(111.326871943614,-2.03385812361386,328.717080804535));
#72697=CARTESIAN_POINT('Ctrl Pts',(111.04863390934,-6.38407812511147,333.310266596113));
#72698=CARTESIAN_POINT('Ctrl Pts',(110.770395875066,-4.87572386003294,339.454095792015));
#72699=CARTESIAN_POINT('Ctrl Pts',(110.492157840792,1.10701022583161,341.51046702193));
#72700=CARTESIAN_POINT('Ctrl Pts',(110.213919806518,6.07385736689464,337.592278760157));
#72701=CARTESIAN_POINT('Ctrl Pts',(109.935681772244,5.46681525234625,331.295194542159));
#72702=CARTESIAN_POINT('Ctrl Pts',(109.657443737971,-0.157042529219445,
328.397955609983));
#72703=CARTESIAN_POINT('Ctrl Pts',(109.379205703697,-5.63678469966438,331.559315368511));
#72704=CARTESIAN_POINT('Ctrl Pts',(109.100967669423,-5.94373275003311,337.878140628934));
#72705=CARTESIAN_POINT('Ctrl Pts',(108.822729635149,-0.796204985048034,
341.555738715471));
#72706=CARTESIAN_POINT('Ctrl Pts',(108.544491600875,5.08198834274931,339.217232145364));
#72707=CARTESIAN_POINT('Ctrl Pts',(108.266253566601,6.29651597843058,333.008633881702));
#72708=CARTESIAN_POINT('Ctrl Pts',(107.988015532327,1.73282383712962,328.627482912285));
#72709=CARTESIAN_POINT('Ctrl Pts',(107.709777498053,-4.42105516306729,330.094296816067));
#72710=CARTESIAN_POINT('Ctrl Pts',(107.431539463779,-6.51779709478459,336.063002123683));
#72711=CARTESIAN_POINT('Ctrl Pts',(107.153301429505,-2.63325283514557,341.056206072282));
#72712=CARTESIAN_POINT('Ctrl Pts',(106.875063395231,3.66778868455823,340.491719097801));
#72713=CARTESIAN_POINT('Ctrl Pts',(106.596825360957,6.60295466491539,334.887562564912));
#72714=CARTESIAN_POINT('Ctrl Pts',(106.318587326683,3.47868660873086,329.386588206628));
#72715=CARTESIAN_POINT('Ctrl Pts',(106.040349292409,-2.8379208029558,329.036958997299));
#72716=CARTESIAN_POINT('Ctrl Pts',(105.762111258135,-6.55021018141231,334.159524501809));
#72717=CARTESIAN_POINT('Ctrl Pts',(105.483873223861,-4.25146835733054,340.05338196561));
#72718=CARTESIAN_POINT('Ctrl Pts',(105.205635189587,1.94878322670338,341.309825387367));
#72719=CARTESIAN_POINT('Ctrl Pts',(104.927397155314,6.36066520758488,336.775835184007));
#72720=CARTESIAN_POINT('Ctrl Pts',(104.649159121039,4.93545861073031,330.612187243568));
#72721=CARTESIAN_POINT('Ctrl Pts',(104.370921086766,-1.01894550594178,328.475170305697));
#72722=CARTESIAN_POINT('Ctrl Pts',(104.092683052492,-6.03827837142212,332.325893271959));
#72723=CARTESIAN_POINT('Ctrl Pts',(103.814445018218,-5.51637230029104,338.630604512794));
#72724=CARTESIAN_POINT('Ctrl Pts',(103.536206983944,0.0678272092954339,
341.603563579873));
#72725=CARTESIAN_POINT('Ctrl Pts',(103.25796894967,5.58978269003947,338.51652981814));
#72726=CARTESIAN_POINT('Ctrl Pts',(102.979730915396,5.98207710119154,332.202428546197));
#72727=CARTESIAN_POINT('Ctrl Pts',(102.701492881122,0.884707651893417,328.45561730532));
#72728=CARTESIAN_POINT('Ctrl Pts',(102.423254846848,-5.02454495128375,330.714489468422));
#72729=CARTESIAN_POINT('Ctrl Pts',(102.145016812574,-6.32284681482974,336.906111392321));
#72730=CARTESIAN_POINT('Ctrl Pts',(101.8667787783,-1.81876548147248,341.348523025644));
#72731=CARTESIAN_POINT('Ctrl Pts',(101.588540744026,4.35437008929757,339.964988782382));
#72732=CARTESIAN_POINT('Ctrl Pts',(101.310302709752,6.5315644995164,334.02515761664));
#72733=CARTESIAN_POINT('Ctrl Pts',(101.032064675478,2.71483857426302,328.979924917459));
#72734=CARTESIAN_POINT('Ctrl Pts',(100.753826641205,-3.59325463963987,329.459226265363));
#72735=CARTESIAN_POINT('Ctrl Pts',(100.47558860693,-6.60387110709679,335.023213887857));
#72736=CARTESIAN_POINT('Ctrl Pts',(100.197350572657,-3.55421253254876,340.565898468101));
#72737=CARTESIAN_POINT('Ctrl Pts',(99.9191125383824,2.7570944230283,341.000840176695));
#72738=CARTESIAN_POINT('Ctrl Pts',(99.640874504109,6.53825652123917,335.928899427393));
#72739=CARTESIAN_POINT('Ctrl Pts',(99.3626364698346,4.31935711441718,330.004521384104));
#72740=CARTESIAN_POINT('Ctrl Pts',(99.0843984355609,-1.86335256269885,328.664420333481));
#72741=CARTESIAN_POINT('Ctrl Pts',(98.8061604012869,-6.336091096065,333.138387229819));
#72742=CARTESIAN_POINT('Ctrl Pts',(98.527922367013,-4.99429235112359,339.320728687994));
#72743=CARTESIAN_POINT('Ctrl Pts',(98.2496843327389,0.930694768809688,341.538001203048));
#72744=CARTESIAN_POINT('Ctrl Pts',(97.9714462984651,6.00159703643856,337.755446514805));
#72745=CARTESIAN_POINT('Ctrl Pts',(97.6932082641911,5.56492228715485,331.44425923025));
#72746=CARTESIAN_POINT('Ctrl Pts',(97.4149702299172,0.0214004930674214,
328.396122767447));
#72747=CARTESIAN_POINT('Ctrl Pts',(97.1367321956432,-5.5417602176372,331.40826696789));
#72748=CARTESIAN_POINT('Ctrl Pts',(96.8584941613693,-6.01932937286292,337.716491558008));
#72749=CARTESIAN_POINT('Ctrl Pts',(96.5802561270954,-0.973048807768221,
341.531831940691));
#72750=CARTESIAN_POINT('Ctrl Pts',(96.3020180928214,4.96618428603849,339.353006561085));
#72751=CARTESIAN_POINT('Ctrl Pts',(96.0237800585475,6.34802336130759,333.179491310641));
#72752=CARTESIAN_POINT('Ctrl Pts',(95.7455420242736,1.90437509457594,328.676630013759));
#72753=CARTESIAN_POINT('Ctrl Pts',(95.4673039899995,-4.28689008791774,329.976632020462));
#72754=CARTESIAN_POINT('Ctrl Pts',(95.1890659557258,-6.54413951112327,335.886504677198));
#72755=CARTESIAN_POINT('Ctrl Pts',(94.9108279214516,-2.79592869631185,340.982845076456));
#72756=CARTESIAN_POINT('Ctrl Pts',(94.6325898871779,3.51806461526506,340.588816855701));
#72757=CARTESIAN_POINT('Ctrl Pts',(94.3543518529038,6.60358195596182,335.066013897269));
#72758=CARTESIAN_POINT('Ctrl Pts',(94.0761138186299,3.62908960438232,329.482630959679));
#72759=CARTESIAN_POINT('Ctrl Pts',(93.797875784356,-2.67576471186408,328.962456154156));
#72760=CARTESIAN_POINT('Ctrl Pts',(93.519637750082,-6.52510924625522,333.982846221964));
#72761=CARTESIAN_POINT('Ctrl Pts',(93.2413997158082,-4.38645733581255,339.93666329871));
#72762=CARTESIAN_POINT('Ctrl Pts',(92.9631616815341,1.77758172770115,341.360177331261));
#72763=CARTESIAN_POINT('Ctrl Pts',(92.6849236472602,6.3103602767668,336.947050502976));
#72764=CARTESIAN_POINT('Ctrl Pts',(92.4066856129864,5.05221434060857,330.747144166529));
#72765=CARTESIAN_POINT('Ctrl Pts',(92.1284475787124,-0.842274125364607,
328.450020856409));
#72766=CARTESIAN_POINT('Ctrl Pts',(91.8502095444384,-5.96382005843634,332.163716728827));
#72767=CARTESIAN_POINT('Ctrl Pts',(91.5719715101645,-5.61245634972109,338.48022789573));
#72768=CARTESIAN_POINT('Ctrl Pts',(91.2937334758905,-0.110624288586713,
341.602985290799));
#72769=CARTESIAN_POINT('Ctrl Pts',(91.0154954416166,5.49272604937187,338.666280544406));
#72770=CARTESIAN_POINT('Ctrl Pts',(90.7372574073426,6.05548276432548,332.365084256623));
#72771=CARTESIAN_POINT('Ctrl Pts',(90.4590193730688,1.0612123252367,328.481911255245));
#72772=CARTESIAN_POINT('Ctrl Pts',(90.1807813387946,-4.90691700125357,330.580292088096));
#72773=CARTESIAN_POINT('Ctrl Pts',(89.902543304521,-6.37204102166964,336.734573636919));
#72774=CARTESIAN_POINT('Ctrl Pts',(89.6243052702468,-1.9896370476708,341.297062561407));
#72775=CARTESIAN_POINT('Ctrl Pts',(89.346067235973,4.21862747798084,340.080830117783));
#72776=CARTESIAN_POINT('Ctrl Pts',(89.067829201699,6.55551983392898,334.201994867998));
#72777=CARTESIAN_POINT('Ctrl Pts',(88.7895911674251,2.87650839759463,329.055477149316));
#72778=CARTESIAN_POINT('Ctrl Pts',(88.5113531331511,-3.44223233801797,329.364160309692));
#72779=CARTESIAN_POINT('Ctrl Pts',(88.2331150988773,-6.60208726429748,334.844770369007));
#72780=CARTESIAN_POINT('Ctrl Pts',(87.9548770646033,-3.7033041547795,340.467832369498));
#72781=CARTESIAN_POINT('Ctrl Pts',(87.6766390303294,2.59394651689991,341.073145309574));
#72782=CARTESIAN_POINT('Ctrl Pts',(87.3984009960554,6.5107707566081,336.105222438532));
#72783=CARTESIAN_POINT('Ctrl Pts',(87.1201629617815,4.45275677179588,330.123053248705));
#72784=CARTESIAN_POINT('Ctrl Pts',(86.8419249275075,-1.6914863799112,328.616386108926));
#72785=CARTESIAN_POINT('Ctrl Pts',(86.5636868932336,-6.28347744707182,332.967867214998));
#72786=CARTESIAN_POINT('Ctrl Pts',(86.2854488589596,-5.10921400502972,339.184206583637));
#72787=CARTESIAN_POINT('Ctrl Pts',(86.0072108246857,0.753699717553054,341.560761329258));
#72788=CARTESIAN_POINT('Ctrl Pts',(85.7289727904118,5.92495433392699,337.916602239699));
#72789=CARTESIAN_POINT('Ctrl Pts',(85.4507347561379,5.65896581023874,331.595920323747));
#72790=CARTESIAN_POINT('Ctrl Pts',(85.1724967218639,0.199827888692849,328.399112082556));
#72791=CARTESIAN_POINT('Ctrl Pts',(84.89425868759,-5.44268913685168,331.25984125426));
#72792=CARTESIAN_POINT('Ctrl Pts',(84.616020653316,-6.09053067546736,337.552858902275));
#72793=CARTESIAN_POINT('Ctrl Pts',(84.3377826190421,-1.14918210929235,341.503155615808));
#72794=CARTESIAN_POINT('Ctrl Pts',(84.0595445847682,4.84675391668017,339.485602407134));
#72795=CARTESIAN_POINT('Ctrl Pts',(83.7813065504942,6.39489541128596,333.351678076816));
#72796=CARTESIAN_POINT('Ctrl Pts',(83.5030685162203,2.07453577545617,328.730394446212));
#72797=CARTESIAN_POINT('Ctrl Pts',(83.2248304819463,-4.14959472141189,329.862635293094));
#72798=CARTESIAN_POINT('Ctrl Pts',(82.9465924476724,-6.56570339035795,335.709359904124));
#72799=CARTESIAN_POINT('Ctrl Pts',(82.6683544133985,-2.95656296759571,340.905115401276));
#72800=CARTESIAN_POINT('Ctrl Pts',(82.3901163791245,3.36577165173125,340.681833654036));
#72801=CARTESIAN_POINT('Ctrl Pts',(82.1118783448506,6.59938730497258,335.244417026216));
#72802=CARTESIAN_POINT('Ctrl Pts',(81.8336403105766,3.77684263523753,329.582702501026));
#72803=CARTESIAN_POINT('Ctrl Pts',(81.5554022763027,-2.51165477474909,328.892361931465));
#72804=CARTESIAN_POINT('Ctrl Pts',(81.2771642420287,-6.49524366991217,333.806910668809));
#72805=CARTESIAN_POINT('Ctrl Pts',(80.9989262077549,-4.51824331883628,339.816339875417));
#72806=CARTESIAN_POINT('Ctrl Pts',(80.7206881734808,1.6050822367736,341.405885067415));
#72807=CARTESIAN_POINT('Ctrl Pts',(80.442450139207,6.25544751467132,337.116844083755));
#72808=CARTESIAN_POINT('Ctrl Pts',(80.164212104933,5.16528093860915,330.885206529001));
#72809=CARTESIAN_POINT('Ctrl Pts',(79.8859740706591,-0.66498771539297,328.42965420833));
#72810=CARTESIAN_POINT('Ctrl Pts',(79.6077360363851,-5.88500695818154,332.00361124253));
#72811=CARTESIAN_POINT('Ctrl Pts',(79.3294980021113,-5.70444217800723,338.327310012835));
#72812=CARTESIAN_POINT('Ctrl Pts',(79.0512599678372,-0.288995008504218,
341.597585495376));
#72813=CARTESIAN_POINT('Ctrl Pts',(78.7730219335634,5.39165861474379,338.813354149013));
#72814=CARTESIAN_POINT('Ctrl Pts',(78.4947838992893,6.12446670799212,332.529663985116));
#72815=CARTESIAN_POINT('Ctrl Pts',(78.2165458650155,1.23694210029652,328.512964719977));
#72816=CARTESIAN_POINT('Ctrl Pts',(77.9383078307416,-4.78570601560572,330.449321982833));
#72817=CARTESIAN_POINT('Ctrl Pts',(77.6600697964675,-6.41658235789159,336.561769294144));
#72818=CARTESIAN_POINT('Ctrl Pts',(77.3818317621937,-2.1590557789407,341.241003975897));
#72819=CARTESIAN_POINT('Ctrl Pts',(77.1035937279197,4.07980442073289,340.192961426037));
#72820=CARTESIAN_POINT('Ctrl Pts',(76.8253556936458,6.57468832131455,334.379414823488));
#72821=CARTESIAN_POINT('Ctrl Pts',(76.5471176593719,3.03607779166665,329.135370077603));
#72822=CARTESIAN_POINT('Ctrl Pts',(76.2688796250979,-3.28869651495906,329.273209649705));
#72823=CARTESIAN_POINT('Ctrl Pts',(75.990641590824,-6.59548257088784,334.666440198987));
#72824=CARTESIAN_POINT('Ctrl Pts',(75.7124035565499,-3.849691620676,340.365773654324));
#72825=CARTESIAN_POINT('Ctrl Pts',(75.4341655222762,2.428904508475,341.141015825777));
#72826=CARTESIAN_POINT('Ctrl Pts',(75.155927488002,6.47853082077028,336.280738415161));
#72827=CARTESIAN_POINT('Ctrl Pts',(74.8776894537284,4.58290502180284,330.245146264618));
#72828=CARTESIAN_POINT('Ctrl Pts',(74.5994514194541,-1.51838507210583,328.573013205511));
#72829=CARTESIAN_POINT('Ctrl Pts',(74.3212133851804,-6.22627559666991,332.798831065535));
#72830=CARTESIAN_POINT('Ctrl Pts',(74.0429753509063,-5.22040490584718,339.044629167519));
#72831=CARTESIAN_POINT('Ctrl Pts',(73.7647373166325,0.576154314021396,341.578730781099));
#72832=CARTESIAN_POINT('Ctrl Pts',(73.4864992823585,5.84398522393628,338.075628258771));
#72833=CARTESIAN_POINT('Ctrl Pts',(73.2082612480845,5.74887715092534,331.750067079568));
#72834=CARTESIAN_POINT('Ctrl Pts',(72.9300232138107,0.378109369797882,328.406921372514));
#72835=CARTESIAN_POINT('Ctrl Pts',(72.6517851795367,-5.33964379910795,331.114146608223));
#72836=CARTESIAN_POINT('Ctrl Pts',(72.3735471452627,-6.1572846665857,337.387362146464));
#72837=CARTESIAN_POINT('Ctrl Pts',(72.0953091109889,-1.32447627691046,341.469730680301));
#72838=CARTESIAN_POINT('Ctrl Pts',(71.8170710767148,4.72378444284771,339.614922861896));
#72839=CARTESIAN_POINT('Ctrl Pts',(71.5388330424411,6.43709790234862,333.525068449278));
#72840=CARTESIAN_POINT('Ctrl Pts',(71.2605950081669,2.24318162827351,328.788736950804));
#72841=CARTESIAN_POINT('Ctrl Pts',(70.9823569738931,-4.00926931676166,329.752389874485));
#72842=CARTESIAN_POINT('Ctrl Pts',(70.7041189396191,-6.58247298652274,335.531697155753));
#72843=CARTESIAN_POINT('Ctrl Pts',(70.4258809053453,-3.11503835369394,340.823073805024));
#72844=CARTESIAN_POINT('Ctrl Pts',(70.1476428710712,3.21102099842906,340.770701571853));
#72845=CARTESIAN_POINT('Ctrl Pts',(69.8694048367974,6.59037377488596,335.422641681609));
#72846=CARTESIAN_POINT('Ctrl Pts',(69.5911668025233,3.92183781188753,329.686729758333));
#72847=CARTESIAN_POINT('Ctrl Pts',(69.3129287682495,-2.34571082484865,328.826727512095));
#72848=CARTESIAN_POINT('Ctrl Pts',(69.0346907339755,-6.46063526025642,333.631846310655));
#72849=CARTESIAN_POINT('Ctrl Pts',(68.7564526997015,-4.64673007614707,339.692499556012));
#72850=CARTESIAN_POINT('Ctrl Pts',(68.4782146654277,1.43141071321893,341.446915219996));
#72851=CARTESIAN_POINT('Ctrl Pts',(68.1999766311536,6.19596701865144,337.285091942903));
#72852=CARTESIAN_POINT('Ctrl Pts',(67.9217385968798,5.27457584339078,331.026273517709));
#72853=CARTESIAN_POINT('Ctrl Pts',(67.6435005626058,-0.487215730737746,
328.414085233207));
#72854=CARTESIAN_POINT('Ctrl Pts',(67.3652625283319,-5.80189662006064,331.845693722248));
#72855=CARTESIAN_POINT('Ctrl Pts',(67.0870244940579,-5.79226261700764,338.171962524897));
#72856=CARTESIAN_POINT('Ctrl Pts',(66.808786459784,-0.467154703982791,341.587368136539));
#72857=CARTESIAN_POINT('Ctrl Pts',(66.5305484255101,5.28665418569491,338.957643238672));
#72858=CARTESIAN_POINT('Ctrl Pts',(66.2523103912362,6.18897856004828,332.696047555395));
#72859=CARTESIAN_POINT('Ctrl Pts',(65.9740723569621,1.41176865901914,328.548755024249));
#72860=CARTESIAN_POINT('Ctrl Pts',(65.6958343226883,-4.66100050272061,330.32167478713));
#72861=CARTESIAN_POINT('Ctrl Pts',(65.4175962884143,-6.45643829936832,336.387824545895));
#72862=CARTESIAN_POINT('Ctrl Pts',(65.1393582541404,-2.32689796555879,341.180388203148));
#72863=CARTESIAN_POINT('Ctrl Pts',(64.8611202198664,3.93800228628635,340.301300828754));
#72864=CARTESIAN_POINT('Ctrl Pts',(64.5828821855925,6.58905596482498,334.557287930882));
#72865=CARTESIAN_POINT('Ctrl Pts',(64.3046441513185,3.19343023875035,329.219545364423));
#72866=CARTESIAN_POINT('Ctrl Pts',(64.0264061170447,-3.13275928247242,329.18644069766));
#72867=CARTESIAN_POINT('Ctrl Pts',(63.7481680827706,-6.58406184962146,334.488353594661));
#72868=CARTESIAN_POINT('Ctrl Pts',(63.4699300484969,-3.99326803796649,340.259796845953));
#72869=CARTESIAN_POINT('Ctrl Pts',(63.1916920142227,2.2620889115907,341.204402166188));
#72870=CARTESIAN_POINT('Ctrl Pts',(62.9134539799489,6.44156025535872,336.455319195338));
#72871=CARTESIAN_POINT('Ctrl Pts',(62.6352159456749,4.70970683005755,330.370711279404));
#72872=CARTESIAN_POINT('Ctrl Pts',(62.356977911401,-1.34417503802856,328.53433329417));
#72873=CARTESIAN_POINT('Ctrl Pts',(62.0787398771271,-6.16452731370681,332.631402211794));
#72874=CARTESIAN_POINT('Ctrl Pts',(61.8005018428531,-5.32778386187053,338.902098359207));
#72875=CARTESIAN_POINT('Ctrl Pts',(61.5222638085792,0.39818820204327,341.591896437255));
#72876=CARTESIAN_POINT('Ctrl Pts',(61.2440257743053,5.75874883019031,338.232408451065));
#72877=CARTESIAN_POINT('Ctrl Pts',(60.9657877400313,5.8345906558651,331.906586939604));
#72878=CARTESIAN_POINT('Ctrl Pts',(60.6875497057574,0.556114755069404,328.419544934966));
#72879=CARTESIAN_POINT('Ctrl Pts',(60.4093116714834,-5.23269944821315,330.971289416152));
#72880=CARTESIAN_POINT('Ctrl Pts',(60.1310736372095,-6.21954260238776,337.220122136465));
#72881=CARTESIAN_POINT('Ctrl Pts',(59.8528356029356,-1.49880331064944,341.431581541093));
#72882=CARTESIAN_POINT('Ctrl Pts',(59.5745975686616,4.59736565697126,339.740873495448));
#72883=CARTESIAN_POINT('Ctrl Pts',(59.2963595343877,6.47460001819531,333.699535818209));
#72884=CARTESIAN_POINT('Ctrl Pts',(59.0181215001138,2.41018950766113,328.85161492578));
#72885=CARTESIAN_POINT('Ctrl Pts',(58.7398834658397,-3.86601633971484,329.645976265948));
#72886=CARTESIAN_POINT('Ctrl Pts',(58.461645431566,-6.59443605444214,335.353646161595));
#72887=CARTESIAN_POINT('Ctrl Pts',(58.1834073972918,-3.27123913572451,340.736780194555));
#72888=CARTESIAN_POINT('Ctrl Pts',(57.9051693630181,3.05392565443701,340.855355717709));
#72889=CARTESIAN_POINT('Ctrl Pts',(57.626931328744,6.57654794739045,335.60055772363));
#72890=CARTESIAN_POINT('Ctrl Pts',(57.3486932944702,4.06396925871226,329.794636770793));
#72891=CARTESIAN_POINT('Ctrl Pts',(57.0704552601961,-2.17805403459824,328.765600822364));
#72892=CARTESIAN_POINT('Ctrl Pts',(56.7922172259222,-6.42130928838279,333.457780979671));
#72893=CARTESIAN_POINT('Ctrl Pts',(56.5139791916483,-4.7718237865882,339.565232768818));
#72894=CARTESIAN_POINT('Ctrl Pts',(56.2357411573743,1.25669397215475,341.483237828746));
#72895=CARTESIAN_POINT('Ctrl Pts',(55.9575031231004,6.13196222142391,337.451671225668));
#72896=CARTESIAN_POINT('Ctrl Pts',(55.6792650888265,5.38001924770637,331.170242125401));
#72897=CARTESIAN_POINT('Ctrl Pts',(55.4010270545525,-0.309087980677374,
328.403325299521));
#72898=CARTESIAN_POINT('Ctrl Pts',(55.1227890202786,-5.7145497313246,331.690079479511));
#72899=CARTESIAN_POINT('Ctrl Pts',(54.8445509860047,-5.87585354015102,338.014298866807));
#72900=CARTESIAN_POINT('Ctrl Pts',(54.5663129517307,-0.644973282637039,
341.572340675012));
#72901=CARTESIAN_POINT('Ctrl Pts',(54.2880749174568,5.17778943656281,339.099042453349));
#72902=CARTESIAN_POINT('Ctrl Pts',(54.0098368831829,6.24897121387603,332.864113474015));
#72903=CARTESIAN_POINT('Ctrl Pts',(53.7315988489089,1.58556434287916,328.589256033944));
#72904=CARTESIAN_POINT('Ctrl Pts',(53.453360814635,-4.53289152268657,330.197443709097));
#72905=CARTESIAN_POINT('Ctrl Pts',(53.175122780361,-6.49157974325204,336.212866406798));
#72906=CARTESIAN_POINT('Ctrl Pts',(52.8968847460871,-2.49304104899505,341.115259504858));
#72907=CARTESIAN_POINT('Ctrl Pts',(52.6186467118132,3.79332461869913,340.405769216394));
#72908=CARTESIAN_POINT('Ctrl Pts',(52.3404086775392,6.59861227319271,334.735484307067));
#72909=CARTESIAN_POINT('Ctrl Pts',(52.0621706432654,3.34845083993485,329.307941544899));
#72910=CARTESIAN_POINT('Ctrl Pts',(51.7839326089913,-2.97453450607784,329.103916812333));
#72911=CARTESIAN_POINT('Ctrl Pts',(51.5056945747175,-6.56783343992024,334.310640595043));
#72912=CARTESIAN_POINT('Ctrl Pts',(51.2274565404434,-4.13392856701051,340.149979328754));
#72913=CARTESIAN_POINT('Ctrl Pts',(50.9492185061695,2.09362153515914,341.263258046037));
#72914=CARTESIAN_POINT('Ctrl Pts',(50.6709804718956,6.39988605631644,336.62883730001));
#72915=CARTESIAN_POINT('Ctrl Pts',(50.3927424376217,4.8330696057555,330.499656605363));
#72916=CARTESIAN_POINT('Ctrl Pts',(50.1145044033477,-1.16898348601682,328.500374619014));
#72917=CARTESIAN_POINT('Ctrl Pts',(49.8362663690738,-6.09827768683947,332.465702910484));
#72918=CARTESIAN_POINT('Ctrl Pts',(49.5580283347998,-5.43127246488066,338.756718234838));
#72919=CARTESIAN_POINT('Ctrl Pts',(49.279790300526,0.21993133264897,341.600248684153));
#72920=CARTESIAN_POINT('Ctrl Pts',(49.0015522662519,5.66930739238778,338.386828335532));
#72921=CARTESIAN_POINT('Ctrl Pts',(48.7233142319781,5.91604373697227,332.065365612896));
#72922=CARTESIAN_POINT('Ctrl Pts',(48.445076197704,0.73371406479973,328.436973552176));
#72923=CARTESIAN_POINT('Ctrl Pts',(48.1668381634302,-5.12193417503768,330.83137399251));
#72924=CARTESIAN_POINT('Ctrl Pts',(47.8886001291562,-6.27725902206752,337.051260991101));
#72925=CARTESIAN_POINT('Ctrl Pts',(47.6103620948823,-1.67203591673728,341.388736054719));
#72926=CARTESIAN_POINT('Ctrl Pts',(47.3321240606083,4.46758987017308,339.863362338513));
#72927=CARTESIAN_POINT('Ctrl Pts',(47.0538860263344,6.50737437474395,333.874952787363));
#72928=CARTESIAN_POINT('Ctrl Pts',(46.7756479920604,2.57543746430089,328.918982457581));
#72929=CARTESIAN_POINT('Ctrl Pts',(46.4974099577865,-3.71994039373653,329.543472170804));
#72930=CARTESIAN_POINT('Ctrl Pts',(46.2191719235126,-6.6015838586722,335.175336934662));
#72931=CARTESIAN_POINT('Ctrl Pts',(45.9409338892386,-3.42505125572216,340.64629758155));
#72932=CARTESIAN_POINT('Ctrl Pts',(45.6626958549647,2.89460033093036,340.935734277064));
#72933=CARTESIAN_POINT('Ctrl Pts',(45.3844578206908,6.55791991811895,335.778035237812));
#72934=CARTESIAN_POINT('Ctrl Pts',(45.1062197864168,4.2031331911891,329.9063447446));
#72935=CARTESIAN_POINT('Ctrl Pts',(44.8279817521429,-2.00880682715078,328.709026497041));
#72936=CARTESIAN_POINT('Ctrl Pts',(44.5497437178689,-6.37729447015455,333.284841778531));
#72937=CARTESIAN_POINT('Ctrl Pts',(44.2715056835951,-4.89343310660957,339.434632444168));
#72938=CARTESIAN_POINT('Ctrl Pts',(43.993267649321,1.08105959191674,341.514826370861));
#72939=CARTESIAN_POINT('Ctrl Pts',(43.7150296150472,6.06347985935449,337.616460295694));
#72940=CARTESIAN_POINT('Ctrl Pts',(43.4367915807731,5.48153415667863,331.317007226059));
#72941=CARTESIAN_POINT('Ctrl Pts',(43.1585535464993,-0.130734534269442,
328.397382264187));
#72942=CARTESIAN_POINT('Ctrl Pts',(42.8803155122253,-5.62303007275688,331.536882143992));
#72943=CARTESIAN_POINT('Ctrl Pts',(42.6020774779514,-5.95515390926368,337.854434164719));
#72944=CARTESIAN_POINT('Ctrl Pts',(42.3238394436775,-0.822320901166817,
341.552514083865));
#72945=CARTESIAN_POINT('Ctrl Pts',(42.0456014094035,5.06514386049422,339.237448543196));
#72946=CARTESIAN_POINT('Ctrl Pts',(41.7673633751296,6.30440086278054,333.033739019075));
#72947=CARTESIAN_POINT('Ctrl Pts',(41.4891253408556,1.75820224609737,328.634438175184));
#72948=CARTESIAN_POINT('Ctrl Pts',(41.2108873065818,-4.40147262080676,330.076719462388));
#72949=CARTESIAN_POINT('Ctrl Pts',(40.9326492723077,-6.5219810292259,336.037022631457));
#72950=CARTESIAN_POINT('Ctrl Pts',(40.6544112380339,-2.65736371140664,341.045665438067));
#72951=CARTESIAN_POINT('Ctrl Pts',(40.3761732037599,3.64587706174641,340.506290306038));
#72952=CARTESIAN_POINT('Ctrl Pts',(40.097935169486,6.603350268392,334.91387383287));
#72953=CARTESIAN_POINT('Ctrl Pts',(39.819697135212,3.50102639902445,329.400494072056));
#72954=CARTESIAN_POINT('Ctrl Pts',(39.5414591009381,-2.8141377216629,329.025698252745));
#72955=CARTESIAN_POINT('Ctrl Pts',(39.2632210666642,-6.54680919178488,334.13343096634));
#72956=CARTESIAN_POINT('Ctrl Pts',(38.9849830323901,-4.27157049735116,340.036401291587));
#72957=CARTESIAN_POINT('Ctrl Pts',(38.7067449981163,1.92362539422454,341.317540488706));
#72958=CARTESIAN_POINT('Ctrl Pts',(38.4285069638423,6.35353865418465,336.801166026084));
#72959=CARTESIAN_POINT('Ctrl Pts',(38.1502689295684,4.95290326927633,330.631888086492));
#72960=CARTESIAN_POINT('Ctrl Pts',(37.8720308952944,-0.99293834111446,328.471161976701));
#72961=CARTESIAN_POINT('Ctrl Pts',(37.5937928610205,-6.0275750916104,332.301854155399));
#72962=CARTESIAN_POINT('Ctrl Pts',(37.3155548267466,-5.530795147398,338.608594951121));
#72963=CARTESIAN_POINT('Ctrl Pts',(37.0373167924726,0.0415138691789895,
341.603781422973));
#72964=CARTESIAN_POINT('Ctrl Pts',(36.7590787581987,5.57572622075412,338.538775154617));
#72965=CARTESIAN_POINT('Ctrl Pts',(36.4808407239247,5.99317691712731,332.226287159104));
#72966=CARTESIAN_POINT('Ctrl Pts',(36.2026026896508,0.910777615799064,328.459194497748));
#72967=CARTESIAN_POINT('Ctrl Pts',(35.9243646553769,-5.00742886049242,330.694502503677));
#72968=CARTESIAN_POINT('Ctrl Pts',(35.646126621103,-6.33039178103882,336.880902012943));
#72969=CARTESIAN_POINT('Ctrl Pts',(35.367888586829,-1.84404760055544,341.341225507));
#72970=CARTESIAN_POINT('Ctrl Pts',(35.0896505525551,4.3345518448597,339.982299949618));
#72971=CARTESIAN_POINT('Ctrl Pts',(34.8114125182811,6.53539704012746,334.051191267098));
#72972=CARTESIAN_POINT('Ctrl Pts',(34.5331744840072,2.73880483397243,328.990790354369));
#72973=CARTESIAN_POINT('Ctrl Pts',(34.2549364497332,-3.571148143626,329.444952437646));
#72974=CARTESIAN_POINT('Ctrl Pts',(33.9766984154593,-6.60391117987907,334.996899676528));
#72975=CARTESIAN_POINT('Ctrl Pts',(33.6984603811854,-3.57636239992634,340.5516920365));
#72976=CARTESIAN_POINT('Ctrl Pts',(33.4202223469114,2.73316136741629,341.011778557416));
#72977=CARTESIAN_POINT('Ctrl Pts',(33.1419843126375,6.53450328927665,335.954944629898));
#72978=CARTESIAN_POINT('Ctrl Pts',(32.8637462783636,4.33922799167826,330.021772110482));
#72979=CARTESIAN_POINT('Ctrl Pts',(32.5855082440896,-1.83809278698308,328.657045846753));
#72980=CARTESIAN_POINT('Ctrl Pts',(32.3072702098157,-6.32862294523512,333.113154987611));
#72981=CARTESIAN_POINT('Ctrl Pts',(32.0290321755417,-5.01146923696644,339.300793946549));
#72982=CARTESIAN_POINT('Ctrl Pts',(31.7507941412678,0.904635820901655,341.541657780355));
#72983=CARTESIAN_POINT('Ctrl Pts',(31.4725561069938,5.99056993833113,337.779338823839));
#72984=CARTESIAN_POINT('Ctrl Pts',(31.19431807272,5.57904644402149,331.46646165166));
#72985=CARTESIAN_POINT('Ctrl Pts',(30.9160800384459,0.047714374623849,328.396260466811));
#72986=CARTESIAN_POINT('Ctrl Pts',(30.6378420041721,-5.52740447210307,331.386213580536));
#72987=CARTESIAN_POINT('Ctrl Pts',(30.359603969898,-6.03010581913728,337.692485152001));
#72988=CARTESIAN_POINT('Ctrl Pts',(30.0813659356242,-0.999068060165199,
341.527902840492));
#72989=CARTESIAN_POINT('Ctrl Pts',(29.8031279013501,4.94879971140008,339.372760443951));
#72990=CARTESIAN_POINT('Ctrl Pts',(29.5248898670764,6.35522703197753,333.204800329835));
#72991=CARTESIAN_POINT('Ctrl Pts',(29.2466518328023,1.92955630830642,328.684268455926));
#72992=CARTESIAN_POINT('Ctrl Pts',(28.9684137985284,-4.26683975929307,329.959590199969));
#72993=CARTESIAN_POINT('Ctrl Pts',(28.6901757642544,-6.54761995824091,335.860421621174));
#72994=CARTESIAN_POINT('Ctrl Pts',(28.4119377299806,-2.81974596422338,340.971656820429));
#72995=CARTESIAN_POINT('Ctrl Pts',(28.1336996957066,3.49576728177937,340.602790697088));
#72996=CARTESIAN_POINT('Ctrl Pts',(27.8554616614327,6.60326649073411,335.092326248084));
#72997=CARTESIAN_POINT('Ctrl Pts',(27.5772236271588,3.6510455051959,329.497135363947));
#72998=CARTESIAN_POINT('Ctrl Pts',(27.2989855928848,-2.65168605111725,328.951842134166));
#72999=CARTESIAN_POINT('Ctrl Pts',(27.0207475586109,-6.52100445714207,333.956854107198));
#73000=CARTESIAN_POINT('Ctrl Pts',(26.7425095243369,-4.40609332271562,339.919145669246));
#73001=CARTESIAN_POINT('Ctrl Pts',(26.464271490063,1.75222462013611,341.367209857098));
#73002=CARTESIAN_POINT('Ctrl Pts',(26.1860334557891,6.30255189188194,336.972179538955));
#73003=CARTESIAN_POINT('Ctrl Pts',(25.9077954215151,5.06912031796114,330.767309167235));
#73004=CARTESIAN_POINT('Ctrl Pts',(25.6295573872412,-0.816168151659336,
328.446716698329));
#73005=CARTESIAN_POINT('Ctrl Pts',(25.3513193529672,-5.95247115512422,332.139975589065));
#73006=CARTESIAN_POINT('Ctrl Pts',(25.0730813186933,-5.62627923786184,338.457836667822));
#73007=CARTESIAN_POINT('Ctrl Pts',(24.7948432844193,-0.136933907759072,
341.602492074107));
#73008=CARTESIAN_POINT('Ctrl Pts',(24.5166052501454,5.47807364835303,338.688137956606));
#73009=CARTESIAN_POINT('Ctrl Pts',(24.2383672158715,6.06593387360606,332.389234073155));
#73010=CARTESIAN_POINT('Ctrl Pts',(23.9601291815975,1.08717611608803,328.486191545927));
#73011=CARTESIAN_POINT('Ctrl Pts',(23.6818911473236,-4.88926711647082,330.560774893348));
#73012=CARTESIAN_POINT('Ctrl Pts',(23.4036531130496,-6.37890208170874,336.709169598286));
#73013=CARTESIAN_POINT('Ctrl Pts',(23.1254150787758,-2.01471275900294,341.289084590182));
#73014=CARTESIAN_POINT('Ctrl Pts',(22.8471770445018,4.19834872552828,340.097599480402));
#73015=CARTESIAN_POINT('Ctrl Pts',(22.5689390102279,6.55864755216782,334.228122567904));
#73016=CARTESIAN_POINT('Ctrl Pts',(22.2907009759539,2.90017232566213,329.066986181947));
#73017=CARTESIAN_POINT('Ctrl Pts',(22.01246294168,-3.41974823763033,329.350489005678));
#73018=CARTESIAN_POINT('Ctrl Pts',(21.734224907406,-6.60141631865069,334.818464682252));
#73019=CARTESIAN_POINT('Ctrl Pts',(21.4559868731321,-3.72506208079045,340.453032640467));
#73020=CARTESIAN_POINT('Ctrl Pts',(21.1777488388582,2.56972664678499,341.083433031154));
#73021=CARTESIAN_POINT('Ctrl Pts',(20.8995108045842,6.50631515970899,336.131156720477));
#73022=CARTESIAN_POINT('Ctrl Pts',(20.6212727703103,4.47215428362238,330.140834583263));
#73023=CARTESIAN_POINT('Ctrl Pts',(20.3430347360363,-1.66603656965545,328.609696827826));
#73024=CARTESIAN_POINT('Ctrl Pts',(20.0647967017624,-6.27533025361995,332.942845972772));
#73025=CARTESIAN_POINT('Ctrl Pts',(19.7865586674884,-5.12584598756012,339.163815004963));
#73026=CARTESIAN_POINT('Ctrl Pts',(19.5083206332146,0.727551483920866,341.563712464907));
#73027=CARTESIAN_POINT('Ctrl Pts',(19.2300825989406,5.91328569724997,337.940187876045));
#73028=CARTESIAN_POINT('Ctrl Pts',(18.9518445646666,5.6724849061666,331.618496270436));
#73029=CARTESIAN_POINT('Ctrl Pts',(18.6736065303927,0.226128442434109,328.399960726537));
#73030=CARTESIAN_POINT('Ctrl Pts',(18.3953684961188,-5.42774275526982,331.238183807473));
#73031=CARTESIAN_POINT('Ctrl Pts',(18.1171304618448,-6.10065453981439,337.528570083977));
#73032=CARTESIAN_POINT('Ctrl Pts',(17.8388924275709,-1.17508569868469,341.498524916047));
#73033=CARTESIAN_POINT('Ctrl Pts',(17.560654393297,4.82884194389145,339.504879350732));
#73034=CARTESIAN_POINT('Ctrl Pts',(17.282416359023,6.4014126081487,333.377172497161));
#73035=CARTESIAN_POINT('Ctrl Pts',(17.0041783247491,2.09950140660303,328.73871049005));
#73036=CARTESIAN_POINT('Ctrl Pts',(16.7259402904752,-4.12909124719214,329.846141449739));
#73037=CARTESIAN_POINT('Ctrl Pts',(16.4477022562012,-6.56847780872623,335.683192330176));
#73038=CARTESIAN_POINT('Ctrl Pts',(16.1694642219273,-2.98006923576536,340.893287693111));
#73039=CARTESIAN_POINT('Ctrl Pts',(15.8912261876533,3.34310488910675,340.695199924864));
#73040=CARTESIAN_POINT('Ctrl Pts',(15.6129881533794,6.59836100139441,335.270711246581));
#73041=CARTESIAN_POINT('Ctrl Pts',(15.3347501191054,3.79839861434825,329.597794853003));
#73042=CARTESIAN_POINT('Ctrl Pts',(15.0565120848315,-2.48729811680818,328.882402386407));
#73043=CARTESIAN_POINT('Ctrl Pts',(14.7782740505576,-6.49043807864009,333.781038954212));
#73044=CARTESIAN_POINT('Ctrl Pts',(14.5000360162836,-4.5373988143935,339.798298081903));
#73045=CARTESIAN_POINT('Ctrl Pts',(14.2217979820097,1.57954436988845,341.412229882592));
#73046=CARTESIAN_POINT('Ctrl Pts',(13.9435599477357,6.24696300003001,337.141752964392));
#73047=CARTESIAN_POINT('Ctrl Pts',(13.6653219134619,5.18163588993546,330.905820962976));
#73048=CARTESIAN_POINT('Ctrl Pts',(13.3870838791879,-0.638801995284358,
328.427056633885));
#73049=CARTESIAN_POINT('Ctrl Pts',(13.108845844914,-5.87302071860168,331.980185415332));
#73050=CARTESIAN_POINT('Ctrl Pts',(12.83060781064,-5.71765501321869,338.304553468852));
#73051=CARTESIAN_POINT('Ctrl Pts',(12.5523697763661,-0.315281696323335,
341.596381578923));
#73052=CARTESIAN_POINT('Ctrl Pts',(12.2741317420922,5.37642098288874,338.83480767685));
#73053=CARTESIAN_POINT('Ctrl Pts',(11.9958937078182,6.13426147599768,332.554087370642));
#73054=CARTESIAN_POINT('Ctrl Pts',(11.7176556735443,1.26278076536891,328.517944984216));
#73055=CARTESIAN_POINT('Ctrl Pts',(11.4394176392703,-4.76753523623819,330.430288808096));
#73056=CARTESIAN_POINT('Ctrl Pts',(11.1611796049964,-6.4227544802001,336.536189149064));
#73057=CARTESIAN_POINT('Ctrl Pts',(10.8829415707225,-2.18390681301347,341.232351372412));
#73058=CARTESIAN_POINT('Ctrl Pts',(10.6047035364485,4.05908004486941,340.209176748852));
#73059=CARTESIAN_POINT('Ctrl Pts',(10.3264655021746,6.57710878785304,334.405617475831));
#73060=CARTESIAN_POINT('Ctrl Pts',(10.0482274679006,3.05942238333672,329.147514337048));
#73061=CARTESIAN_POINT('Ctrl Pts',(9.76998943362672,-3.26585174673895,329.260150786106));
#73062=CARTESIAN_POINT('Ctrl Pts',(9.49175139935276,-6.59410011745994,334.640162370028));
#73063=CARTESIAN_POINT('Ctrl Pts',(9.21351336507884,-3.87104356673585,340.350391199024));
#73064=CARTESIAN_POINT('Ctrl Pts',(8.9352753308049,2.4044190006588,341.150645821003));
#73065=CARTESIAN_POINT('Ctrl Pts',(8.65703729653096,6.47336951988847,336.306541999263));
#73066=CARTESIAN_POINT('Ctrl Pts',(8.37879926225703,4.60182745214506,330.263446809577));
#73067=CARTESIAN_POINT('Ctrl Pts',(8.10056122798305,-1.49278731520583,328.567011019545));
#73068=CARTESIAN_POINT('Ctrl Pts',(7.82232319370917,-6.21741092854858,332.774044749012));
#73069=CARTESIAN_POINT('Ctrl Pts',(7.54408515943517,-5.23656364109403,339.023784963449));
#73070=CARTESIAN_POINT('Ctrl Pts',(7.2658471251613,0.550094121815325,341.580994482456));
#73071=CARTESIAN_POINT('Ctrl Pts',(6.98760909088731,5.83138478454036,338.098851931026));
#73072=CARTESIAN_POINT('Ctrl Pts',(6.70937105661341,5.7623455394068,331.773071937739));
#73073=CARTESIAN_POINT('Ctrl Pts',(6.43113302233942,0.403311536316757,328.408344724868));
#73074=CARTESIAN_POINT('Ctrl Pts',(6.15289498806554,-5.32210119679797,331.09315624518));
#73075=CARTESIAN_POINT('Ctrl Pts',(5.87465695379156,-6.17058839537894,337.362332615213));
#73076=CARTESIAN_POINT('Ctrl Pts',(5.59641891951763,-1.3427309658529,341.465250565794));
#73077=CARTESIAN_POINT('Ctrl Pts',(5.36455389095603,3.6837204961337,339.938001672926));
#73078=CARTESIAN_POINT('Ctrl Pts',(5.17906186810672,5.59027261763526,336.589093317143));
#73079=CARTESIAN_POINT('Ctrl Pts',(5.08631585668207,5.65257316228901,334.68157454258));
#73080=CARTESIAN_POINT('Ctrl Pts',(5.03994285096975,5.44851606351237,333.774411599427));
#73081=CARTESIAN_POINT('Ctrl Pts',(185.422610796143,3.04869533563088,339.272759684468));
#73082=CARTESIAN_POINT('Ctrl Pts',(185.376227986451,3.76025219667377,338.765053977827));
#73083=CARTESIAN_POINT('Ctrl Pts',(185.283472171046,4.91198743119452,337.389569652041));
#73084=CARTESIAN_POINT('Ctrl Pts',(185.097970344217,5.67465640099036,333.848674163514));
#73085=CARTESIAN_POINT('Ctrl Pts',(184.866105315656,3.1102034485172,329.629352350811));
#73086=CARTESIAN_POINT('Ctrl Pts',(184.587867281381,-2.84276674491428,329.478773562289));
#73087=CARTESIAN_POINT('Ctrl Pts',(184.309629247108,-6.17636874974876,334.402383897492));
#73088=CARTESIAN_POINT('Ctrl Pts',(184.031391212834,-3.84753045006414,339.870598632012));
#73089=CARTESIAN_POINT('Ctrl Pts',(183.75315317856,2.01504287056116,340.871144614342));
#73090=CARTESIAN_POINT('Ctrl Pts',(183.474915144286,6.02689969073261,336.482766363536));
#73091=CARTESIAN_POINT('Ctrl Pts',(183.196677110012,4.50877578226168,330.734237247225));
#73092=CARTESIAN_POINT('Ctrl Pts',(182.918439075738,-1.14741733317675,328.900038067762));
#73093=CARTESIAN_POINT('Ctrl Pts',(182.640201041464,-5.75041359440766,332.663841513818));
#73094=CARTESIAN_POINT('Ctrl Pts',(182.36196300719,-5.07646140385426,338.571419658156));
#73095=CARTESIAN_POINT('Ctrl Pts',(182.083724972916,0.256148691274596,341.201602898475));
#73096=CARTESIAN_POINT('Ctrl Pts',(181.805486938642,5.35366091116605,338.140643284717));
#73097=CARTESIAN_POINT('Ctrl Pts',(181.527248904368,5.53821554038123,332.197574082239));
#73098=CARTESIAN_POINT('Ctrl Pts',(181.249010870094,0.640421975222099,328.826243214803));
#73099=CARTESIAN_POINT('Ctrl Pts',(180.97077283582,-4.84507233320865,331.120481301994));
#73100=CARTESIAN_POINT('Ctrl Pts',(180.692534801546,-5.88431794951573,336.974894595124));
#73101=CARTESIAN_POINT('Ctrl Pts',(180.414296767273,-1.52361041929907,341.016977243033));
#73102=CARTESIAN_POINT('Ctrl Pts',(180.136058732998,4.23529115399526,339.537368168912));
#73103=CARTESIAN_POINT('Ctrl Pts',(179.857820698725,6.10752894540388,333.893883571184));
#73104=CARTESIAN_POINT('Ctrl Pts',(179.579582664451,2.37497736016159,329.265465549051));
#73105=CARTESIAN_POINT('Ctrl Pts',(179.301344630176,-3.53705578244632,329.899545227691));
#73106=CARTESIAN_POINT('Ctrl Pts',(179.023106595903,-6.20318509938342,335.214236927654));
#73107=CARTESIAN_POINT('Ctrl Pts',(178.744868561628,-3.17674297821987,340.332326582762));
#73108=CARTESIAN_POINT('Ctrl Pts',(178.466630527355,2.76494926885195,340.557018826482));
#73109=CARTESIAN_POINT('Ctrl Pts',(178.188392493081,6.16928839125002,335.682116920639));
#73110=CARTESIAN_POINT('Ctrl Pts',(177.910154458807,3.91216261090214,330.181246381558));
#73111=CARTESIAN_POINT('Ctrl Pts',(177.631916424533,-1.93509705158604,329.102474915127));
#73112=CARTESIAN_POINT('Ctrl Pts',(177.353678390259,-6.00654671312173,333.43577517086));
#73113=CARTESIAN_POINT('Ctrl Pts',(177.075440355985,-4.56587711182005,339.204541464849));
#73114=CARTESIAN_POINT('Ctrl Pts',(176.797202321711,1.0648305223979,341.114862115224));
#73115=CARTESIAN_POINT('Ctrl Pts',(176.518964287437,5.71835890327751,337.41366405781));
#73116=CARTESIAN_POINT('Ctrl Pts',(176.240726253163,5.12423372135596,331.497482120095));
#73117=CARTESIAN_POINT('Ctrl Pts',(175.962488218889,-0.172325113033902,
328.795509143729));
#73118=CARTESIAN_POINT('Ctrl Pts',(175.684250184616,-5.31074373473581,331.787305848006));
#73119=CARTESIAN_POINT('Ctrl Pts',(175.406012150341,-5.57557121750448,337.727344556293));
#73120=CARTESIAN_POINT('Ctrl Pts',(175.127774116067,-0.723779289273663,
341.164539420802));
#73121=CARTESIAN_POINT('Ctrl Pts',(174.849536081794,4.79221420976308,338.944627447299));
#73122=CARTESIAN_POINT('Ctrl Pts',(174.571298047519,5.91046346146377,333.104789088012));
#73123=CARTESIAN_POINT('Ctrl Pts',(174.293060013246,1.6047676328781,329.004157809391));
#73124=CARTESIAN_POINT('Ctrl Pts',(174.014821978972,-4.17359976606904,330.405822410606));
#73125=CARTESIAN_POINT('Ctrl Pts',(173.736583944698,-6.12191626192584,336.023495975658));
#73126=CARTESIAN_POINT('Ctrl Pts',(173.458345910424,-2.45224056354941,340.701922390625));
#73127=CARTESIAN_POINT('Ctrl Pts',(173.18010787615,3.467820104985,340.147778787951));
#73128=CARTESIAN_POINT('Ctrl Pts',(172.901869841876,6.20551344811549,334.869594572666));
#73129=CARTESIAN_POINT('Ctrl Pts',(172.623631807602,3.24849869313879,329.711081493264));
#73130=CARTESIAN_POINT('Ctrl Pts',(172.345393773329,-2.68961536476926,329.406130863184));
#73131=CARTESIAN_POINT('Ctrl Pts',(172.067155739054,-6.15950910108628,334.234591374587));
#73132=CARTESIAN_POINT('Ctrl Pts',(171.788917704781,-3.97691224954176,339.76545608412));
#73133=CARTESIAN_POINT('Ctrl Pts',(171.510679670506,1.85523827427864,340.923132083271));
#73134=CARTESIAN_POINT('Ctrl Pts',(171.232441636233,5.98486401706558,336.645237194892));
#73135=CARTESIAN_POINT('Ctrl Pts',(170.954203601958,4.62226838783954,330.857532416421));
#73136=CARTESIAN_POINT('Ctrl Pts',(170.675965567685,-0.982114716337224,
328.87130899668));
#73137=CARTESIAN_POINT('Ctrl Pts',(170.397727533411,-5.6852256413208,332.509294851355));
#73138=CARTESIAN_POINT('Ctrl Pts',(170.119489499137,-5.17108890905721,338.432964058193));
#73139=CARTESIAN_POINT('Ctrl Pts',(169.841251464863,0.0884797899009875,
341.206252819294));
#73140=CARTESIAN_POINT('Ctrl Pts',(169.563013430589,5.26685189162661,338.284154972271));
#73141=CARTESIAN_POINT('Ctrl Pts',(169.284775396315,5.61191175101298,332.348236581241));
#73142=CARTESIAN_POINT('Ctrl Pts',(169.006537362041,0.807003028176409,328.845802339644));
#73143=CARTESIAN_POINT('Ctrl Pts',(168.728299327767,-4.73848046227249,330.990984455146));
#73144=CARTESIAN_POINT('Ctrl Pts',(168.450061293493,-5.93553037235089,336.815180963188));
#73145=CARTESIAN_POINT('Ctrl Pts',(168.171823259219,-1.6856316680076,340.97361269334));
#73146=CARTESIAN_POINT('Ctrl Pts',(167.893585224945,4.11114633818361,339.650148225192));
#73147=CARTESIAN_POINT('Ctrl Pts',(167.615347190671,6.13518603024423,334.059311366861));
#73148=CARTESIAN_POINT('Ctrl Pts',(167.337109156397,2.52905605754718,329.33173058262));
#73149=CARTESIAN_POINT('Ctrl Pts',(167.058871122123,-3.3979513303547,329.805836979189));
#73150=CARTESIAN_POINT('Ctrl Pts',(166.780633087849,-6.20670893606953,335.046550114236));
#73151=CARTESIAN_POINT('Ctrl Pts',(166.502395053576,-3.31966136202707,340.244544896527));
#73152=CARTESIAN_POINT('Ctrl Pts',(166.224157019301,2.61379044582624,340.629698236632));
#73153=CARTESIAN_POINT('Ctrl Pts',(165.945918985028,6.14860534102855,335.848560599189));
#73154=CARTESIAN_POINT('Ctrl Pts',(165.667680950753,4.04093586803504,330.288711424605));
#73155=CARTESIAN_POINT('Ctrl Pts',(165.38944291648,-1.77504080693859,329.052342237156));
#73156=CARTESIAN_POINT('Ctrl Pts',(165.111204882206,-5.96208873294403,333.274050791383));
#73157=CARTESIAN_POINT('Ctrl Pts',(164.832966847932,-4.67781582901218,339.079637459391));
#73158=CARTESIAN_POINT('Ctrl Pts',(164.554728813658,0.899219616755684,341.141401046264));
#73159=CARTESIAN_POINT('Ctrl Pts',(164.276490779384,5.65105449268665,337.567291539913));
#73160=CARTESIAN_POINT('Ctrl Pts',(163.99825274511,5.21700007010667,331.637216480543));
#73161=CARTESIAN_POINT('Ctrl Pts',(163.720014710836,-0.00461831401527035,
328.793118222377));
#73162=CARTESIAN_POINT('Ctrl Pts',(163.441776676562,-5.22199853953164,331.644983758109));
#73163=CARTESIAN_POINT('Ctrl Pts',(163.163538642288,-5.64722778189197,337.575698179067));
#73164=CARTESIAN_POINT('Ctrl Pts',(162.885300608014,-0.89007944175547,341.142732398337));
#73165=CARTESIAN_POINT('Ctrl Pts',(162.60706257374,4.68388166452899,339.072671762236));
#73166=CARTESIAN_POINT('Ctrl Pts',(162.328824539466,5.95951370125524,333.265180362466));
#73167=CARTESIAN_POINT('Ctrl Pts',(162.050586505192,1.7661879766176,329.049707338167));
#73168=CARTESIAN_POINT('Ctrl Pts',(161.772348470919,-4.04794238527021,330.294730063455));
#73169=CARTESIAN_POINT('Ctrl Pts',(161.494110436645,-6.14733576772723,335.857709559841));
#73170=CARTESIAN_POINT('Ctrl Pts',(161.215872402371,-2.60540985066816,340.633581652932));
#73171=CARTESIAN_POINT('Ctrl Pts',(160.937634368097,3.32746223056271,340.239599014658));
#73172=CARTESIAN_POINT('Ctrl Pts',(160.659396333823,6.20677133606821,335.037313696985));
#73173=CARTESIAN_POINT('Ctrl Pts',(160.381158299549,3.39021799825867,329.800786150339));
#73174=CARTESIAN_POINT('Ctrl Pts',(160.102920265275,-2.53748835701711,329.335500413256));
#73175=CARTESIAN_POINT('Ctrl Pts',(159.824682231001,-6.13657910032513,334.068442339051));
#73176=CARTESIAN_POINT('Ctrl Pts',(159.546444196727,-4.10422177902387,339.65626098053));
#73177=CARTESIAN_POINT('Ctrl Pts',(159.268206162453,1.69451929067344,340.971097646477));
#73178=CARTESIAN_POINT('Ctrl Pts',(158.989968128179,5.93822501838346,336.806346135508));
#73179=CARTESIAN_POINT('Ctrl Pts',(158.711730093905,4.73250929478059,330.983937437609));
#73180=CARTESIAN_POINT('Ctrl Pts',(158.433492059631,-0.816160356919756,
328.84701007623));
#73181=CARTESIAN_POINT('Ctrl Pts',(158.155254025357,-5.61585169558195,332.356590749912));
#73182=CARTESIAN_POINT('Ctrl Pts',(157.877015991083,-5.26195882304375,338.291989075743));
#73183=CARTESIAN_POINT('Ctrl Pts',(157.598777956809,-0.0792440049832126,
341.206377616444));
#73184=CARTESIAN_POINT('Ctrl Pts',(157.320539922536,5.17619186681082,338.425265024517));
#73185=CARTESIAN_POINT('Ctrl Pts',(157.042301888262,5.68151286289929,332.50083727642));
#73186=CARTESIAN_POINT('Ctrl Pts',(156.764063853988,0.972993363697465,328.869854272171));
#73187=CARTESIAN_POINT('Ctrl Pts',(156.485825819714,-4.62842778401096,330.864415521548));
#73188=CARTESIAN_POINT('Ctrl Pts',(156.20758778544,-5.9824090698147,336.654141605673));
#73189=CARTESIAN_POINT('Ctrl Pts',(155.929349751166,-1.84642185246274,340.925886353362));
#73190=CARTESIAN_POINT('Ctrl Pts',(155.651111716892,3.98399944575246,339.759532660511));
#73191=CARTESIAN_POINT('Ctrl Pts',(155.372873682618,6.15836325633603,334.225426095694));
#73192=CARTESIAN_POINT('Ctrl Pts',(155.094635648344,2.68128800387271,329.402134570168));
#73193=CARTESIAN_POINT('Ctrl Pts',(154.81639761407,-3.25636567399855,329.715921525239));
#73194=CARTESIAN_POINT('Ctrl Pts',(154.538159579796,-6.2057006367199,334.878829303729));
#73195=CARTESIAN_POINT('Ctrl Pts',(154.259921545522,-3.46015572111465,340.152933641709));
#73196=CARTESIAN_POINT('Ctrl Pts',(153.981683511248,2.46072302794279,340.69826683387));
#73197=CARTESIAN_POINT('Ctrl Pts',(153.703445476974,6.12343257446949,336.014384658867));
#73198=CARTESIAN_POINT('Ctrl Pts',(153.4252074427,4.16675842912217,330.399616654718));
#73199=CARTESIAN_POINT('Ctrl Pts',(153.146969408426,-1.61368842537694,329.006552544985));
#73200=CARTESIAN_POINT('Ctrl Pts',(152.868731374152,-5.91327722990972,333.113586701582));
#73201=CARTESIAN_POINT('Ctrl Pts',(152.590493339879,-4.7863388003833,338.951754498722));
#73202=CARTESIAN_POINT('Ctrl Pts',(152.312255305605,0.732952100009919,341.163455520186));
#73203=CARTESIAN_POINT('Ctrl Pts',(152.034017271331,5.57962367657935,337.71904438323));
#73204=CARTESIAN_POINT('Ctrl Pts',(151.755779237057,5.30595696026238,331.779406348814));
#73205=CARTESIAN_POINT('Ctrl Pts',(151.477541202783,0.163091857308978,328.795259572205));
#73206=CARTESIAN_POINT('Ctrl Pts',(151.199303168509,-5.12944023586499,331.505111504367));
#73207=CARTESIAN_POINT('Ctrl Pts',(150.921065134235,-5.71476073499945,337.4221710245));
#73208=CARTESIAN_POINT('Ctrl Pts',(150.642827099961,-1.05572965735508,341.116439946636));
#73209=CARTESIAN_POINT('Ctrl Pts',(150.364589065687,4.57212894429984,339.197742208249));
#73210=CARTESIAN_POINT('Ctrl Pts',(150.086351031413,6.0042122982834,333.426838403926));
#73211=CARTESIAN_POINT('Ctrl Pts',(149.808112997139,1.92631864816058,329.099601776493));
#73212=CARTESIAN_POINT('Ctrl Pts',(149.529874962865,-3.91932919296249,330.187073509037));
#73213=CARTESIAN_POINT('Ctrl Pts',(149.251636928591,-6.16826648290805,335.69129684366));
#73214=CARTESIAN_POINT('Ctrl Pts',(148.973398894317,-2.75667666495296,340.561127268381));
#73215=CARTESIAN_POINT('Ctrl Pts',(148.695160860043,3.18467463994858,340.327593281013));
#73216=CARTESIAN_POINT('Ctrl Pts',(148.41692282577,6.20349703348994,335.205005574807));
#73217=CARTESIAN_POINT('Ctrl Pts',(148.138684791495,3.52946176286371,329.894287278479));
#73218=CARTESIAN_POINT('Ctrl Pts',(147.860446757222,-2.38350847277232,329.269006186494));
#73219=CARTESIAN_POINT('Ctrl Pts',(147.582208722948,-6.10916816347259,333.902973527834));
#73220=CARTESIAN_POINT('Ctrl Pts',(147.303970688674,-4.22853440172834,339.543665870596));
#73221=CARTESIAN_POINT('Ctrl Pts',(147.0257326544,1.53256296741654,341.014703108311));
#73222=CARTESIAN_POINT('Ctrl Pts',(146.747494620126,5.88724992195559,336.966136080401));
#73223=CARTESIAN_POINT('Ctrl Pts',(146.469256585852,4.8392945187824,331.113274991628));
#73224=CARTESIAN_POINT('Ctrl Pts',(146.191018551578,-0.649610036407337,
328.827204075071));
#73225=CARTESIAN_POINT('Ctrl Pts',(145.912780517304,-5.54237704941444,332.205816868504));
#73226=CARTESIAN_POINT('Ctrl Pts',(145.63454248303,-5.3489864495252,338.148610279633));
#73227=CARTESIAN_POINT('Ctrl Pts',(145.356304448756,-0.246909935817251,
341.201970510557));
#73228=CARTESIAN_POINT('Ctrl Pts',(145.078066414482,5.08175218160551,338.563873944876));
#73229=CARTESIAN_POINT('Ctrl Pts',(144.799828380208,5.74696532850814,332.655262862677));
#73230=CARTESIAN_POINT('Ctrl Pts',(144.521590345935,1.13827321850806,328.898382443135));
#73231=CARTESIAN_POINT('Ctrl Pts',(144.24335231166,-4.51499542323171,330.740866395801));
#73232=CARTESIAN_POINT('Ctrl Pts',(143.965114277387,-6.02491940629494,336.491894392332));
#73233=CARTESIAN_POINT('Ctrl Pts',(143.686876243112,-2.00586377786598,340.873832925344));
#73234=CARTESIAN_POINT('Ctrl Pts',(143.408638208839,3.85394343300977,339.8654416804));
#73235=CARTESIAN_POINT('Ctrl Pts',(143.130400174565,6.17704363952428,334.392106419154));
#73236=CARTESIAN_POINT('Ctrl Pts',(142.852162140291,2.83156207106203,329.476626124556));
#73237=CARTESIAN_POINT('Ctrl Pts',(142.573924106017,-3.11240221622613,329.629864510587));
#73238=CARTESIAN_POINT('Ctrl Pts',(142.295686071743,-6.200160928665,334.711196972183));
#73239=CARTESIAN_POINT('Ctrl Pts',(142.017448037469,-3.59812347109343,340.057559709681));
#73240=CARTESIAN_POINT('Ctrl Pts',(141.739210003195,2.30585878768524,340.762674551063));
#73241=CARTESIAN_POINT('Ctrl Pts',(141.460971968921,6.09378847142506,336.179468013873));
#73242=CARTESIAN_POINT('Ctrl Pts',(141.182733934647,4.28953841910852,330.51388108927));
#73243=CARTESIAN_POINT('Ctrl Pts',(140.904495900373,-1.45115772694064,328.965139274038));
#73244=CARTESIAN_POINT('Ctrl Pts',(140.626257866099,-5.8601478460293,332.954500072623));
#73245=CARTESIAN_POINT('Ctrl Pts',(140.348019831825,-4.89136678245731,338.820985963033));
#73246=CARTESIAN_POINT('Ctrl Pts',(140.069781797551,0.5661493809204,341.181009432828));
#73247=CARTESIAN_POINT('Ctrl Pts',(139.791543763277,5.50411861377862,337.868811777666));
#73248=CARTESIAN_POINT('Ctrl Pts',(139.513305729004,5.39103943542977,331.923947897733));
#73249=CARTESIAN_POINT('Ctrl Pts',(139.23506769473,0.330682938798655,328.801931629596));
#73250=CARTESIAN_POINT('Ctrl Pts',(138.956829660456,-5.03313640989581,331.367791221638));
#73251=CARTESIAN_POINT('Ctrl Pts',(138.678591626182,-5.77812076420052,337.266875198271));
#73252=CARTESIAN_POINT('Ctrl Pts',(138.400353591908,-1.22060897812122,341.085681264472));
#73253=CARTESIAN_POINT('Ctrl Pts',(138.122115557634,4.45703765102095,339.319747458776));
#73254=CARTESIAN_POINT('Ctrl Pts',(137.84387752336,6.04452661358915,333.589645169529));
#73255=CARTESIAN_POINT('Ctrl Pts',(137.565639489086,2.08504271993315,329.153804691402));
#73256=CARTESIAN_POINT('Ctrl Pts',(137.287401454812,-3.7878541026254,330.082931358274));
#73257=CARTESIAN_POINT('Ctrl Pts',(137.009163420538,-6.18469312383953,335.524379341844));
#73258=CARTESIAN_POINT('Ctrl Pts',(136.730925386264,-2.90593055122699,340.48461214323));
#73259=CARTESIAN_POINT('Ctrl Pts',(136.45268735199,3.03956159678193,340.411697333516));
#73260=CARTESIAN_POINT('Ctrl Pts',(136.174449317716,6.1956929312797,335.372547757357));
#73261=CARTESIAN_POINT('Ctrl Pts',(135.896211283442,3.66612831101986,329.991516603066));
#73262=CARTESIAN_POINT('Ctrl Pts',(135.617973249168,-2.22778814829773,329.206696737048));
#73263=CARTESIAN_POINT('Ctrl Pts',(135.339735214895,-6.07729630602166,333.738305766426));
#73264=CARTESIAN_POINT('Ctrl Pts',(135.06149718062,-4.34975934445596,339.427752971376));
#73265=CARTESIAN_POINT('Ctrl Pts',(134.783259146347,1.36948756517418,341.053916628024));
#73266=CARTESIAN_POINT('Ctrl Pts',(134.505021112073,5.83197594984737,337.124490350795));
#73267=CARTESIAN_POINT('Ctrl Pts',(134.226783077799,4.94254608516959,331.24545063607));
#73268=CARTESIAN_POINT('Ctrl Pts',(133.948545043525,-0.482585370007687,
328.811905455564));
#73269=CARTESIAN_POINT('Ctrl Pts',(133.670307009251,-5.46485535407729,332.057083302363));
#73270=CARTESIAN_POINT('Ctrl Pts',(133.392068974977,-5.43210824084298,338.002932365204));
#73271=CARTESIAN_POINT('Ctrl Pts',(133.113830940703,-0.414395572773265,
341.193034719706));
#73272=CARTESIAN_POINT('Ctrl Pts',(132.835592906429,4.98360179596184,338.699880520978));
#73273=CARTESIAN_POINT('Ctrl Pts',(132.557354872155,5.8082213543847,332.811400578295));
#73274=CARTESIAN_POINT('Ctrl Pts',(132.279116837881,1.30272190509538,328.931366021237));
#73275=CARTESIAN_POINT('Ctrl Pts',(132.000878803607,-4.39826620835616,330.620427293599));
#73276=CARTESIAN_POINT('Ctrl Pts',(131.722640769333,-6.06303034070208,336.328557796239));
#73277=CARTESIAN_POINT('Ctrl Pts',(131.444402735059,-2.16384101956683,340.817490418751));
#73278=CARTESIAN_POINT('Ctrl Pts',(131.166164700785,3.72107326698374,339.967797949994));
#73279=CARTESIAN_POINT('Ctrl Pts',(130.887926666511,6.19121353937478,334.559230627104));
#73280=CARTESIAN_POINT('Ctrl Pts',(130.609688632238,2.97976852884374,329.555150851977));
#73281=CARTESIAN_POINT('Ctrl Pts',(130.331450597963,-2.96616607929583,329.547728774148));
#73282=CARTESIAN_POINT('Ctrl Pts',(130.05321256369,-6.1900938570052,334.543775524893));
#73283=CARTESIAN_POINT('Ctrl Pts',(129.774974529416,-3.73346386777644,339.958492742581));
#73284=CARTESIAN_POINT('Ctrl Pts',(129.496736495142,2.14931080707439,340.822874357635));
#73285=CARTESIAN_POINT('Ctrl Pts',(129.218498460868,6.05969467804856,336.343690120174));
#73286=CARTESIAN_POINT('Ctrl Pts',(128.940260426594,4.40918618392441,330.631421292261));
#73287=CARTESIAN_POINT('Ctrl Pts',(128.66202239232,-1.28756739170578,328.928132664326));
#73288=CARTESIAN_POINT('Ctrl Pts',(128.383784358046,-5.80273937643113,332.796907069723));
#73289=CARTESIAN_POINT('Ctrl Pts',(128.105546323772,-4.99282308369843,338.687427339638));
#73290=CARTESIAN_POINT('Ctrl Pts',(127.827308289498,0.398933258996397,341.194049966306));
#73291=CARTESIAN_POINT('Ctrl Pts',(127.549070255224,5.42459443815543,338.016484362922));
#73292=CARTESIAN_POINT('Ctrl Pts',(127.27083222095,5.47218536830197,332.070735582922));
#73293=CARTESIAN_POINT('Ctrl Pts',(126.992594186676,0.498032555281528,328.813129522603));
#73294=CARTESIAN_POINT('Ctrl Pts',(126.714356152402,-4.93315738277237,331.233123181331));
#73295=CARTESIAN_POINT('Ctrl Pts',(126.436118118129,-5.83726160393966,337.109924097544));
#73296=CARTESIAN_POINT('Ctrl Pts',(126.157880083854,-1.38459700901158,341.050478811867));
#73297=CARTESIAN_POINT('Ctrl Pts',(125.879642049581,4.33869182446808,339.438598425463));
#73298=CARTESIAN_POINT('Ctrl Pts',(125.601404015306,6.08042720961975,333.753481777615));
#73299=CARTESIAN_POINT('Ctrl Pts',(125.323165981033,2.24224429146187,329.212276503873));
#73300=CARTESIAN_POINT('Ctrl Pts',(125.044927946759,-3.65361311749906,329.982379655866));
#73301=CARTESIAN_POINT('Ctrl Pts',(124.766689912485,-6.19660369577232,335.357078937718));
#73302=CARTESIAN_POINT('Ctrl Pts',(124.488451878211,-3.05306252415595,340.404092148901));
#73303=CARTESIAN_POINT('Ctrl Pts',(124.210213843937,2.89222906274935,340.491849759308));
#73304=CARTESIAN_POINT('Ctrl Pts',(123.931975809663,6.18336472800057,335.539817905167));
#73305=CARTESIAN_POINT('Ctrl Pts',(123.653737775389,3.80011784867946,330.092403127154));
#73306=CARTESIAN_POINT('Ctrl Pts',(123.375499741115,-2.07044109072718,329.14861756334));
#73307=CARTESIAN_POINT('Ctrl Pts',(123.097261706841,-6.04098680083397,333.574559295386));
#73308=CARTESIAN_POINT('Ctrl Pts',(122.819023672567,-4.46780808863448,339.308606922586));
#73309=CARTESIAN_POINT('Ctrl Pts',(122.540785638293,1.20541216176558,341.088709571862));
#73310=CARTESIAN_POINT('Ctrl Pts',(122.26254760402,5.77244346316771,337.281293316247));
#73311=CARTESIAN_POINT('Ctrl Pts',(121.984309569745,5.04218859954669,331.380367856147));
#73312=CARTESIAN_POINT('Ctrl Pts',(121.706071535472,-0.315208319296592,
328.801125388777));
#73313=CARTESIAN_POINT('Ctrl Pts',(121.427833501198,-5.38334321598855,331.910498656888));
#73314=CARTESIAN_POINT('Ctrl Pts',(121.149595466924,-5.51126350138344,337.855061706608));
#73315=CARTESIAN_POINT('Ctrl Pts',(120.87135743265,-0.581578617674682,341.179576768816));
#73316=CARTESIAN_POINT('Ctrl Pts',(120.593119398376,4.8818123793878,338.833185440684));
#73317=CARTESIAN_POINT('Ctrl Pts',(120.314881364102,5.86523621131872,332.969136411362));
#73318=CARTESIAN_POINT('Ctrl Pts',(120.036643329828,1.46621934286705,328.968780921835));
#73319=CARTESIAN_POINT('Ctrl Pts',(119.758405295554,-4.27832537517161,330.503186159693));
#73320=CARTESIAN_POINT('Ctrl Pts',(119.48016726128,-6.09671404439443,336.164251085937));
#73321=CARTESIAN_POINT('Ctrl Pts',(119.201929227006,-2.32023822242827,340.756899974934));
#73322=CARTESIAN_POINT('Ctrl Pts',(118.923691192732,3.58548596960027,340.06652672864));
#73323=CARTESIAN_POINT('Ctrl Pts',(118.645453158458,6.20086260901282,334.726676685283));
#73324=CARTESIAN_POINT('Ctrl Pts',(118.367215124184,3.12579915671638,329.637651413598));
#73325=CARTESIAN_POINT('Ctrl Pts',(118.08897708991,-2.81776404497875,329.469574291517));
#73326=CARTESIAN_POINT('Ctrl Pts',(117.810739055636,-6.17550677272601,334.376687213162));
#73327=CARTESIAN_POINT('Ctrl Pts',(117.532501021362,-3.86607808547316,339.855805079206));
#73328=CARTESIAN_POINT('Ctrl Pts',(117.254262987089,1.9911933975994,340.878822295629));
#73329=CARTESIAN_POINT('Ctrl Pts',(116.976024952814,6.02117608966137,336.506931062627));
#73330=CARTESIAN_POINT('Ctrl Pts',(116.697786918541,4.5256143566545,330.752151435719));
#73331=CARTESIAN_POINT('Ctrl Pts',(116.419548884267,-1.12303687349579,328.895559738109));
#73332=CARTESIAN_POINT('Ctrl Pts',(116.141310849993,-5.74109374083608,332.640922767447));
#73333=CARTESIAN_POINT('Ctrl Pts',(115.863072815719,-5.09063362061581,338.551176153174));
#73334=CARTESIAN_POINT('Ctrl Pts',(115.584834781445,0.231425835614517,341.202567598409));
#73335=CARTESIAN_POINT('Ctrl Pts',(115.306596747171,5.34110921834113,338.161954308331));
#73336=CARTESIAN_POINT('Ctrl Pts',(115.028358712897,5.54933550603892,332.219662219867));
#73337=CARTESIAN_POINT('Ctrl Pts',(114.750120678623,0.665018507902607,328.828845074513));
#73338=CARTESIAN_POINT('Ctrl Pts',(114.471882644349,-4.82957615927886,331.101205718181));
#73339=CARTESIAN_POINT('Ctrl Pts',(114.193644610075,-5.89214006951734,336.951432328165));
#73340=CARTESIAN_POINT('Ctrl Pts',(113.915406575801,-1.54757400580489,341.010858293686));
#73341=CARTESIAN_POINT('Ctrl Pts',(113.637168541527,4.21717788087984,339.554208323215));
#73342=CARTESIAN_POINT('Ctrl Pts',(113.358930507253,6.11188787172474,333.918228594534));
#73343=CARTESIAN_POINT('Ctrl Pts',(113.080692472979,2.39780857400497,329.27497451773));
#73344=CARTESIAN_POINT('Ctrl Pts',(112.802454438706,-3.51670426048264,329.885491824767));
#73345=CARTESIAN_POINT('Ctrl Pts',(112.524216404431,-6.20398950159512,335.189517794199));
#73346=CARTESIAN_POINT('Ctrl Pts',(112.245978370158,-3.1979651478287,340.319626081173));
#73347=CARTESIAN_POINT('Ctrl Pts',(111.967740335884,2.74278462021191,340.567992031006));
#73348=CARTESIAN_POINT('Ctrl Pts',(111.68950230161,6.16652142571869,335.706693877412));
#73349=CARTESIAN_POINT('Ctrl Pts',(111.411264267336,3.93133253655047,330.196873183302));
#73350=CARTESIAN_POINT('Ctrl Pts',(111.133026233062,-1.91158219503698,329.09481107484));
#73351=CARTESIAN_POINT('Ctrl Pts',(110.854788198788,-6.00026616114596,333.41185368255));
#73352=CARTESIAN_POINT('Ctrl Pts',(110.576550164514,-4.58259443495464,339.186314724784));
#73353=CARTESIAN_POINT('Ctrl Pts',(110.29831213024,1.04045656521155,341.119056533987));
#73354=CARTESIAN_POINT('Ctrl Pts',(110.020074095966,5.70869593259684,337.436430479077));
#73355=CARTESIAN_POINT('Ctrl Pts',(109.741836061692,5.13814930285185,331.517928135172));
#73356=CARTESIAN_POINT('Ctrl Pts',(109.463598027418,-0.147601103160891,
328.794871746324));
#73357=CARTESIAN_POINT('Ctrl Pts',(109.185359993144,-5.29790015539158,331.766169968332));
#73358=CARTESIAN_POINT('Ctrl Pts',(108.90712195887,-5.58639443189754,337.705106279148));
#73359=CARTESIAN_POINT('Ctrl Pts',(108.628883924596,-0.748336993297773,
341.161606484894));
#73360=CARTESIAN_POINT('Ctrl Pts',(108.350645890323,4.77645825861544,338.963691364615));
#73361=CARTESIAN_POINT('Ctrl Pts',(108.072407856048,5.9179682670056,333.128355183018));
#73362=CARTESIAN_POINT('Ctrl Pts',(107.794169821775,1.62864614583315,329.010599824533));
#73363=CARTESIAN_POINT('Ctrl Pts',(107.515931787501,-4.15526050459266,330.389228603673));
#73364=CARTESIAN_POINT('Ctrl Pts',(107.237693753227,-6.12594592149832,335.999094238348));
#73365=CARTESIAN_POINT('Ctrl Pts',(106.959455718953,-2.47494118505861,340.692105837097));
#73366=CARTESIAN_POINT('Ctrl Pts',(106.681217684679,3.44728054683719,340.161555924489));
#73367=CARTESIAN_POINT('Ctrl Pts',(106.402979650405,6.20598380267818,334.894322324416));
#73368=CARTESIAN_POINT('Ctrl Pts',(106.124741616131,3.26954732297222,329.724067567429));
#73369=CARTESIAN_POINT('Ctrl Pts',(105.846503581857,-2.66730447658596,329.395458131174));
#73370=CARTESIAN_POINT('Ctrl Pts',(105.568265547583,-6.15641032733074,334.210054045042));
#73371=CARTESIAN_POINT('Ctrl Pts',(105.290027513309,-3.99586928915159,339.749571702188));
#73372=CARTESIAN_POINT('Ctrl Pts',(105.011789479035,1.83162201674796,340.930477511803));
#73373=CARTESIAN_POINT('Ctrl Pts',(104.733551444761,5.97826083257455,336.669071642537));
#73374=CARTESIAN_POINT('Ctrl Pts',(104.455313410487,4.63873792133273,330.875983362375));
#73375=CARTESIAN_POINT('Ctrl Pts',(104.177075376213,-0.957686312656652,
328.867444280173));
#73376=CARTESIAN_POINT('Ctrl Pts',(103.898837341939,-5.67525595294783,332.486661065683));
#73377=CARTESIAN_POINT('Ctrl Pts',(103.620599307666,-5.18472697185933,338.412331894394));
#73378=CARTESIAN_POINT('Ctrl Pts',(103.342361273392,0.0637494248598003,
341.206556109554));
#73379=CARTESIAN_POINT('Ctrl Pts',(103.064123239118,5.25372391532508,338.305115391596));
#73380=CARTESIAN_POINT('Ctrl Pts',(102.785885204844,5.62243351353439,332.370619062192));
#73381=CARTESIAN_POINT('Ctrl Pts',(102.50764717057,0.831518863355839,328.849066809817));
#73382=CARTESIAN_POINT('Ctrl Pts',(102.229409136296,-4.72246837452607,330.972135158446));
#73383=CARTESIAN_POINT('Ctrl Pts',(101.951171102022,-5.94271608862435,336.791515620983));
#73384=CARTESIAN_POINT('Ctrl Pts',(101.672933067748,-1.70942096253776,340.96684864087));
#73385=CARTESIAN_POINT('Ctrl Pts',(101.394695033474,4.0925845498577,339.666492733573));
#73386=CARTESIAN_POINT('Ctrl Pts',(101.1164569992,6.13888562729768,334.083765321995));
#73387=CARTESIAN_POINT('Ctrl Pts',(100.838218964926,2.55162197436991,329.341852950821));
#73388=CARTESIAN_POINT('Ctrl Pts',(100.559980930652,-3.37722750255852,329.792338612565));
#73389=CARTESIAN_POINT('Ctrl Pts',(100.281742896378,-6.20684514818521,335.021818264602));
#73390=CARTESIAN_POINT('Ctrl Pts',(100.003504862104,-3.34053261420657,340.231275617251));
#73391=CARTESIAN_POINT('Ctrl Pts',(99.7252668278303,2.59133739364889,340.64006854945));
#73392=CARTESIAN_POINT('Ctrl Pts',(99.4470287935565,6.14517532342992,335.873053821095));
#73393=CARTESIAN_POINT('Ctrl Pts',(99.1687907592825,4.05967656153864,330.304850487373));
#73394=CARTESIAN_POINT('Ctrl Pts',(98.8905527250086,-1.75132746014872,329.045316561097));
#73395=CARTESIAN_POINT('Ctrl Pts',(98.6123146907346,-5.95516412120866,333.250307735717));
#73396=CARTESIAN_POINT('Ctrl Pts',(98.3340766564607,-4.69403456631375,339.060965675855));
#73397=CARTESIAN_POINT('Ctrl Pts',(98.0558386221866,0.874741226250659,341.144935355016));
#73398=CARTESIAN_POINT('Ctrl Pts',(97.7776005879129,5.64077990664417,337.589788557975));
#73399=CARTESIAN_POINT('Ctrl Pts',(97.4993625536387,5.23035812448528,331.658031026498));
#73400=CARTESIAN_POINT('Ctrl Pts',(97.221124519365,0.0201138914456118,328.793149094622));
#73401=CARTESIAN_POINT('Ctrl Pts',(96.9428864850909,-5.20858856289313,331.624202625643));
#73402=CARTESIAN_POINT('Ctrl Pts',(96.6646484508171,-5.65744617170602,337.553175580424));
#73403=CARTESIAN_POINT('Ctrl Pts',(96.3864104165431,-0.914548932512907,
341.139136989859));
#73404=CARTESIAN_POINT('Ctrl Pts',(96.1081723822692,4.66761636332718,339.091302997216));
#73405=CARTESIAN_POINT('Ctrl Pts',(95.8299343479952,5.96637901644651,333.288940631558));
#73406=CARTESIAN_POINT('Ctrl Pts',(95.5516963137214,1.78988370978281,329.056792193128));
#73407=CARTESIAN_POINT('Ctrl Pts',(95.2734582794472,-4.02916145870834,330.278637837457));
#73408=CARTESIAN_POINT('Ctrl Pts',(94.9952202451736,-6.15070462686848,335.833207851163));
#73409=CARTESIAN_POINT('Ctrl Pts',(94.7169822108993,-2.62783694320291,340.623155317982));
#73410=CARTESIAN_POINT('Ctrl Pts',(94.4387441766256,3.30655791643028,340.252816147127));
#73411=CARTESIAN_POINT('Ctrl Pts',(94.1605061423516,6.20657338087024,335.062045129492));
#73412=CARTESIAN_POINT('Ctrl Pts',(93.8822681080776,3.41090806255851,329.814336212306));
#73413=CARTESIAN_POINT('Ctrl Pts',(93.6040300738037,-2.51489723984268,329.325434412816));
#73414=CARTESIAN_POINT('Ctrl Pts',(93.3257920395297,-6.13281846506266,334.043997696233));
#73415=CARTESIAN_POINT('Ctrl Pts',(93.0475540052558,-4.1227427051468,339.639870183246));
#73416=CARTESIAN_POINT('Ctrl Pts',(92.7693159709819,1.67071318369969,340.977802287466));
#73417=CARTESIAN_POINT('Ctrl Pts',(92.4910779367078,5.93098024355116,336.829993464695));
#73418=CARTESIAN_POINT('Ctrl Pts',(92.2128399024341,4.74847427502061,331.002826650033));
#73419=CARTESIAN_POINT('Ctrl Pts',(91.9346018681601,-0.79163644833082,328.843806820454));
#73420=CARTESIAN_POINT('Ctrl Pts',(91.6563638338862,-5.60527408758383,332.334234606481));
#73421=CARTESIAN_POINT('Ctrl Pts',(91.3781257996122,-5.27503443037134,338.270995947509));
#73422=CARTESIAN_POINT('Ctrl Pts',(91.0998877653383,-0.103973535787613,
341.206012587328));
#73423=CARTESIAN_POINT('Ctrl Pts',(90.8216497310643,5.16250233794153,338.445863076353));
#73424=CARTESIAN_POINT('Ctrl Pts',(90.5434116967905,5.69142601455134,332.523495881063));
#73425=CARTESIAN_POINT('Ctrl Pts',(90.2651736625165,0.997412042917653,328.873779962582));
#73426=CARTESIAN_POINT('Ctrl Pts',(89.9869356282425,-4.61191223872394,330.846005749579));
#73427=CARTESIAN_POINT('Ctrl Pts',(89.7086975939687,-5.98895273060163,336.630290747333));
#73428=CARTESIAN_POINT('Ctrl Pts',(89.4304595596946,-1.87001969840361,340.918481989311));
#73429=CARTESIAN_POINT('Ctrl Pts',(89.1522215254208,3.9650028095739,339.77536966635));
#73430=CARTESIAN_POINT('Ctrl Pts',(88.8739834911467,6.16140076255098,334.249971084919));
#73431=CARTESIAN_POINT('Ctrl Pts',(88.5957454568728,2.70357217786121,329.41286296845));
#73432=CARTESIAN_POINT('Ctrl Pts',(88.317507422599,-3.23528468979185,329.702988039827));
#73433=CARTESIAN_POINT('Ctrl Pts',(88.0392693883248,-6.20516855034669,334.854102803286));
#73434=CARTESIAN_POINT('Ctrl Pts',(87.7610313540511,-3.48066082038602,340.139105270731));
#73435=CARTESIAN_POINT('Ctrl Pts',(87.482793319777,2.43799796997338,340.708026684295));
#73436=CARTESIAN_POINT('Ctrl Pts',(87.2045552855032,6.11934200807928,336.038776260018));
#73437=CARTESIAN_POINT('Ctrl Pts',(86.9263172512292,4.1850562067108,330.416256194235));
#73438=CARTESIAN_POINT('Ctrl Pts',(86.6480792169553,-1.58979390422782,329.000170163055));
#73439=CARTESIAN_POINT('Ctrl Pts',(86.3698411826813,-5.90571361457614,333.090039415897));
#73440=CARTESIAN_POINT('Ctrl Pts',(86.0916031484074,-4.80204710901799,338.932651305798));
#73441=CARTESIAN_POINT('Ctrl Pts',(85.8133651141335,0.70838715038682,341.166327138207));
#73442=CARTESIAN_POINT('Ctrl Pts',(85.5351270798595,5.56874497765884,337.741255570723));
#73443=CARTESIAN_POINT('Ctrl Pts',(85.2568890455857,5.31874773347449,331.800574226852));
#73444=CARTESIAN_POINT('Ctrl Pts',(84.9786510113115,0.187814198868455,328.795958691553));
#73445=CARTESIAN_POINT('Ctrl Pts',(84.7004129770378,-5.11547365390613,331.484700293515));
#73446=CARTESIAN_POINT('Ctrl Pts',(84.4221749427637,-5.7243668387584,337.399380550381));
#73447=CARTESIAN_POINT('Ctrl Pts',(84.1439369084899,-1.08009306719839,341.11218469096));
#73448=CARTESIAN_POINT('Ctrl Pts',(83.865698874216,4.55536616998208,339.215927156345));
#73449=CARTESIAN_POINT('Ctrl Pts',(83.5874608399418,6.01043311006456,333.450775497334));
#73450=CARTESIAN_POINT('Ctrl Pts',(83.3092228056682,1.94981429888808,329.107324297904));
#73451=CARTESIAN_POINT('Ctrl Pts',(83.0309847713939,-3.90012031516611,330.171494614536));
#73452=CARTESIAN_POINT('Ctrl Pts',(82.7527467371202,-6.17097208167385,335.666713054786));
#73453=CARTESIAN_POINT('Ctrl Pts',(82.4745087028461,-2.77881385222812,340.550098765327));
#73454=CARTESIAN_POINT('Ctrl Pts',(82.1962706685723,3.16342083418214,340.340240758251));
#73455=CARTESIAN_POINT('Ctrl Pts',(81.9180326342983,6.20263091307842,335.229722629152));
#73456=CARTESIAN_POINT('Ctrl Pts',(81.6397946000243,3.54977815372484,329.908391433981));
#73457=CARTESIAN_POINT('Ctrl Pts',(81.3615565657505,-2.36065362266235,329.259554267826));
#73458=CARTESIAN_POINT('Ctrl Pts',(81.0833185314764,-6.10474841272267,333.878639421248));
#73459=CARTESIAN_POINT('Ctrl Pts',(80.8050804972027,-4.24660569036626,339.526780626535));
#73460=CARTESIAN_POINT('Ctrl Pts',(80.5268424629285,1.50858439424203,341.020762066024));
#73461=CARTESIAN_POINT('Ctrl Pts',(80.2486044286548,5.87936884692356,336.989579023824));
#73462=CARTESIAN_POINT('Ctrl Pts',(79.9703663943807,4.85474328812528,331.132588677602));
#73463=CARTESIAN_POINT('Ctrl Pts',(79.6921283601069,-0.625008530292098,
328.824664619043));
#73464=CARTESIAN_POINT('Ctrl Pts',(79.4138903258329,-5.5311992455712,332.183754691791));
#73465=CARTESIAN_POINT('Ctrl Pts',(79.1356522915589,-5.36149005355665,338.127271516167));
#73466=CARTESIAN_POINT('Ctrl Pts',(78.8574142572851,-0.271620574856635,
341.20093742861));
#73467=CARTESIAN_POINT('Ctrl Pts',(78.579176223011,5.0675110962762,338.584094588503));
#73468=CARTESIAN_POINT('Ctrl Pts',(78.3009381887372,5.75626263069755,332.678181045677));
#73469=CARTESIAN_POINT('Ctrl Pts',(78.0227001544631,1.16257691122491,328.902966487241));
#73470=CARTESIAN_POINT('Ctrl Pts',(77.7444621201893,-4.49798848007174,330.722909591397));
#73471=CARTESIAN_POINT('Ctrl Pts',(77.4662240859153,-6.0308162334077,336.467875433777));
#73472=CARTESIAN_POINT('Ctrl Pts',(77.1879860516414,-2.0292529440471,340.865793656386));
#73473=CARTESIAN_POINT('Ctrl Pts',(76.9097480173673,3.83452582034105,339.880759619502));
#73474=CARTESIAN_POINT('Ctrl Pts',(76.6315099830936,6.17941683691064,334.416724519695));
#73475=CARTESIAN_POINT('Ctrl Pts',(76.3532719488195,2.85354823029058,329.487952719032));
#73476=CARTESIAN_POINT('Ctrl Pts',(76.0750339145457,-3.09097946896438,329.617505350429));
#73477=CARTESIAN_POINT('Ctrl Pts',(75.7967958802716,-6.19896093233291,334.686493876246));
#73478=CARTESIAN_POINT('Ctrl Pts',(75.5185578459978,-3.6182474446129,340.04318234449));
#73479=CARTESIAN_POINT('Ctrl Pts',(75.2403198117237,2.28287831778362,340.771816812444));
#73480=CARTESIAN_POINT('Ctrl Pts',(74.9620817774499,6.08904034317885,336.203740183496));
#73481=CARTESIAN_POINT('Ctrl Pts',(74.6838437431759,4.30737991972699,330.531008955329));
#73482=CARTESIAN_POINT('Ctrl Pts',(74.4056057089021,-1.42709947923493,328.959404846657));
#73483=CARTESIAN_POINT('Ctrl Pts',(74.1273676746279,-5.85195075005674,332.93116575117));
#73484=CARTESIAN_POINT('Ctrl Pts',(73.8491296403542,-4.90655319220296,338.801465309891));
#73485=CARTESIAN_POINT('Ctrl Pts',(73.5708916060801,0.541515809529054,341.183216263261));
#73486=CARTESIAN_POINT('Ctrl Pts',(73.2926535718063,5.49264374561652,337.890720915959));
#73487=CARTESIAN_POINT('Ctrl Pts',(73.0144155375323,5.40325358764049,331.945453651052));
#73488=CARTESIAN_POINT('Ctrl Pts',(72.7361775032584,0.355377364179016,328.803298485545));
#73489=CARTESIAN_POINT('Ctrl Pts',(72.4579394689843,-5.01862342102826,331.347764836688));
#73490=CARTESIAN_POINT('Ctrl Pts',(72.1797014347105,-5.78710756751815,337.243833490301));
#73491=CARTESIAN_POINT('Ctrl Pts',(71.9014634004365,-1.24484851686434,341.080769268791));
#73492=CARTESIAN_POINT('Ctrl Pts',(71.6232253661627,4.4397896437819,339.33747284132));
#73493=CARTESIAN_POINT('Ctrl Pts',(71.3449873318886,6.05009837951721,333.613741608363));
#73494=CARTESIAN_POINT('Ctrl Pts',(71.0667492976148,2.10832113167528,329.16215924027));
#73495=CARTESIAN_POINT('Ctrl Pts',(70.7885112633407,-3.76823129993616,330.067877170995));
#73496=CARTESIAN_POINT('Ctrl Pts',(70.510273229067,-6.18673348659899,335.499731423882));
#73497=CARTESIAN_POINT('Ctrl Pts',(70.2320351947928,-2.92776166864652,340.472989525097));
#73498=CARTESIAN_POINT('Ctrl Pts',(69.953797160519,3.01797381893149,340.423765920324));
#73499=CARTESIAN_POINT('Ctrl Pts',(69.675559126245,6.19415927809661,335.397232385123));
#73500=CARTESIAN_POINT('Ctrl Pts',(69.3973210919711,3.68605619339361,330.006164553235));
#73501=CARTESIAN_POINT('Ctrl Pts',(69.1190830576973,-2.20468625388628,329.197865801953));
#73502=CARTESIAN_POINT('Ctrl Pts',(68.8408450234231,-6.07222066709064,333.714099964859));
#73503=CARTESIAN_POINT('Ctrl Pts',(68.5626069891494,-4.36736779993612,339.41038561016));
#73504=CARTESIAN_POINT('Ctrl Pts',(68.2843689548753,1.34535403497671,341.059325478203));
#73505=CARTESIAN_POINT('Ctrl Pts',(68.0061309206015,5.82346432938442,337.147711790396));
#73506=CARTESIAN_POINT('Ctrl Pts',(67.7278928863274,4.95746736290866,331.265174692718));
#73507=CARTESIAN_POINT('Ctrl Pts',(67.4496548520537,-0.457924230410055,
328.810031653601));
#73508=CARTESIAN_POINT('Ctrl Pts',(67.1714168177795,-5.45308551643202,332.035331202191));
#73509=CARTESIAN_POINT('Ctrl Pts',(66.8931787835057,-5.44403071143462,337.981263548091));
#73510=CARTESIAN_POINT('Ctrl Pts',(66.6149407492317,-0.439069276315245,
341.191334339285));
#73511=CARTESIAN_POINT('Ctrl Pts',(66.3367027149577,4.96881955302673,338.719708991262));
#73512=CARTESIAN_POINT('Ctrl Pts',(66.0584646806839,5.81689601821245,332.834561604773));
#73513=CARTESIAN_POINT('Ctrl Pts',(65.7802266464099,1.32689286472911,328.936605071765));
#73514=CARTESIAN_POINT('Ctrl Pts',(65.5019886121359,-4.38078028580957,330.602936568836));
#73515=CARTESIAN_POINT('Ctrl Pts',(65.2237505778621,-6.06827602827182,336.304388276137));
#73516=CARTESIAN_POINT('Ctrl Pts',(64.945512543588,-2.18700442719639,340.808822115166));
#73517=CARTESIAN_POINT('Ctrl Pts',(64.6672745093142,3.70124885658474,339.982585637181));
#73518=CARTESIAN_POINT('Ctrl Pts',(64.3890364750402,6.19292069502163,334.583903862799));
#73519=CARTESIAN_POINT('Ctrl Pts',(64.1107984407663,3.00144061899679,329.567067371956));
#73520=CARTESIAN_POINT('Ctrl Pts',(63.8325604064923,-2.94441721189048,329.535952963916));
#73521=CARTESIAN_POINT('Ctrl Pts',(63.5543223722184,-6.18822682695267,334.519113871686));
#73522=CARTESIAN_POINT('Ctrl Pts',(63.2760843379444,-3.75319202099864,339.943576881544));
#73523=CARTESIAN_POINT('Ctrl Pts',(62.9978463036705,2.12609170560242,340.831392354283));
#73524=CARTESIAN_POINT('Ctrl Pts',(62.7196082693966,6.05429245503427,336.367825134707));
#73525=CARTESIAN_POINT('Ctrl Pts',(62.4413702351226,4.42655837969133,330.649024978076));
#73526=CARTESIAN_POINT('Ctrl Pts',(62.1631322008487,-1.26336298479978,328.92305037878));
#73527=CARTESIAN_POINT('Ctrl Pts',(61.8848941665749,-5.7939147853471,332.773802751247));
#73528=CARTESIAN_POINT('Ctrl Pts',(61.6066561323007,-5.00747650542366,338.667503480278));
#73529=CARTESIAN_POINT('Ctrl Pts',(61.328418098027,0.37424905329486,341.195590397721));
#73530=CARTESIAN_POINT('Ctrl Pts',(61.0501800637529,5.41253177971177,338.038075453939));
#73531=CARTESIAN_POINT('Ctrl Pts',(60.771942029479,5.4838139807253,332.092563507999));
#73532=CARTESIAN_POINT('Ctrl Pts',(60.493703995205,0.522681032588899,328.815163117075));
#73533=CARTESIAN_POINT('Ctrl Pts',(60.2154659609312,-4.91810858439494,331.21349624557));
#73534=CARTESIAN_POINT('Ctrl Pts',(59.9372279266572,-5.84562254464326,337.0866479808));
#73535=CARTESIAN_POINT('Ctrl Pts',(59.6589898923833,-1.40869497691978,341.044913662926));
#73536=CARTESIAN_POINT('Ctrl Pts',(59.3807518581093,4.32097117881919,339.455851299363));
#73537=CARTESIAN_POINT('Ctrl Pts',(59.1025138238355,6.08534586118586,333.777719966632));
#73538=CARTESIAN_POINT('Ctrl Pts',(58.8242757895614,2.26528846629994,329.2212569797));
#73539=CARTESIAN_POINT('Ctrl Pts',(58.5460377552876,-3.63359071850647,329.967861168389));
#73540=CARTESIAN_POINT('Ctrl Pts',(58.2677997210135,-6.1979773326506,335.332384888601));
#73541=CARTESIAN_POINT('Ctrl Pts',(57.9895616867397,-3.07457163061672,340.391883902536));
#73542=CARTESIAN_POINT('Ctrl Pts',(57.7113236524656,2.87032307623123,340.50333064319));
#73543=CARTESIAN_POINT('Ctrl Pts',(57.4330856181918,6.18116466192095,335.564452081615));
#73544=CARTESIAN_POINT('Ctrl Pts',(57.1548475839177,3.81964267120667,330.107584176042));
#73545=CARTESIAN_POINT('Ctrl Pts',(56.876609549644,-2.04710902104055,329.140414060174));
#73546=CARTESIAN_POINT('Ctrl Pts',(56.5983715153699,-6.03525897995848,333.55049947394));
#73547=CARTESIAN_POINT('Ctrl Pts',(56.3201334810961,-4.48494085324504,339.290770125876));
#73548=CARTESIAN_POINT('Ctrl Pts',(56.041895446822,1.1811412968729,341.09346436496));
#73549=CARTESIAN_POINT('Ctrl Pts',(55.7636574125481,5.76330751246754,337.304276295707));
#73550=CARTESIAN_POINT('Ctrl Pts',(55.4854193782742,5.05657149015016,331.400487880946));
#73551=CARTESIAN_POINT('Ctrl Pts',(55.2071813440003,-0.290505553805166,
328.799918609128));
#73552=CARTESIAN_POINT('Ctrl Pts',(54.9289433097263,-5.37098993888844,331.889072516663));
#73553=CARTESIAN_POINT('Ctrl Pts',(54.6507052754524,-5.52259613273534,337.833078658442));
#73554=CARTESIAN_POINT('Ctrl Pts',(54.3724672411784,-0.606197368956423,
341.177210331541));
#73555=CARTESIAN_POINT('Ctrl Pts',(54.0942292069045,4.86649977285522,338.85260725886));
#73556=CARTESIAN_POINT('Ctrl Pts',(53.8159911726306,5.87328190253675,332.992523369114));
#73557=CARTESIAN_POINT('Ctrl Pts',(53.5377531383566,1.49023991975911,328.974671153226));
#73558=CARTESIAN_POINT('Ctrl Pts',(53.2595151040827,-4.2603732414763,330.486174286314));
#73559=CARTESIAN_POINT('Ctrl Pts',(52.9812770698088,-6.10130476201488,336.139948652894));
#73560=CARTESIAN_POINT('Ctrl Pts',(52.7030390355348,-2.34315895756308,340.747608966329));
#73561=CARTESIAN_POINT('Ctrl Pts',(52.4248010012609,3.56526923727485,340.080773365931));
#73562=CARTESIAN_POINT('Ctrl Pts',(52.146562966987,6.20190247635333,334.751387039712));
#73563=CARTESIAN_POINT('Ctrl Pts',(51.868324932713,3.14714135281286,329.650149157628));
#73564=CARTESIAN_POINT('Ctrl Pts',(51.5900868984391,-2.79570493847374,329.458390429919));
#73565=CARTESIAN_POINT('Ctrl Pts',(51.3118488641651,-6.17297407226025,334.35208501065));
#73566=CARTESIAN_POINT('Ctrl Pts',(51.0336108298912,-3.88539601288147,339.840361613899));
#73567=CARTESIAN_POINT('Ctrl Pts',(50.7553727956172,1.96775261916748,340.886709807693));
#73568=CARTESIAN_POINT('Ctrl Pts',(50.4771347613433,6.01512371658749,336.53091129866));
#73569=CARTESIAN_POINT('Ctrl Pts',(50.1988967270694,4.54250456237568,330.770218087062));
#73570=CARTESIAN_POINT('Ctrl Pts',(49.9206586927955,-1.09870398147085,328.891133305488));
#73571=CARTESIAN_POINT('Ctrl Pts',(49.6424206585215,-5.73164809836577,332.618065322743));
#73572=CARTESIAN_POINT('Ctrl Pts',(49.3641826242476,-5.10474335437767,338.530863636018));
#73573=CARTESIAN_POINT('Ctrl Pts',(49.0859445899735,0.206709020034407,341.203440505983));
#73574=CARTESIAN_POINT('Ctrl Pts',(48.8077065556997,5.32846757778105,338.183211586237));
#73575=CARTESIAN_POINT('Ctrl Pts',(48.5294685214257,5.56037008745055,332.24179637793));
#73576=CARTESIAN_POINT('Ctrl Pts',(48.2512304871518,0.689603038794641,328.831543922576));
#73577=CARTESIAN_POINT('Ctrl Pts',(47.9729924528778,-4.81400254003894,331.081992563213));
#73578=CARTESIAN_POINT('Ctrl Pts',(47.694754418604,-5.8998690424398,336.927938798894));
#73579=CARTESIAN_POINT('Ctrl Pts',(47.4165163843299,-1.57151280651798,341.00464405516));
#73580=CARTESIAN_POINT('Ctrl Pts',(47.1382783500561,4.19899753645439,339.570976090407));
#73581=CARTESIAN_POINT('Ctrl Pts',(46.8600403157821,6.11614981732458,333.942590834985));
#73582=CARTESIAN_POINT('Ctrl Pts',(46.5818022815083,2.42060168505957,329.284574362962));
#73583=CARTESIAN_POINT('Ctrl Pts',(46.3035642472342,-3.49629688556238,329.871519638507));
#73584=CARTESIAN_POINT('Ctrl Pts',(46.0253262129604,-6.20469540956123,335.164795645547));
#73585=CARTESIAN_POINT('Ctrl Pts',(45.7470881786863,-3.21913653735961,340.306841121049));
#73586=CARTESIAN_POINT('Ctrl Pts',(45.4688501444124,2.72057642079944,340.578876828611));
#73587=CARTESIAN_POINT('Ctrl Pts',(45.1906121101385,6.163656553233,335.731259614644));
#73588=CARTESIAN_POINT('Ctrl Pts',(44.9123740758645,3.95044004218623,330.212576245691));
#73589=CARTESIAN_POINT('Ctrl Pts',(44.6341360415906,-1.8880369871754,329.087240993811));
#73590=CARTESIAN_POINT('Ctrl Pts',(44.3558980073167,-5.99389034078641,333.387957409729));
#73591=CARTESIAN_POINT('Ctrl Pts',(44.0776599730428,-4.59923899833415,339.168021517031));
#73592=CARTESIAN_POINT('Ctrl Pts',(43.7994219387688,1.01606608823303,341.123153798048));
#73593=CARTESIAN_POINT('Ctrl Pts',(43.5211839044949,5.69894232273963,337.459158216201));
#73594=CARTESIAN_POINT('Ctrl Pts',(43.2429458702208,5.15198330391888,331.53842943646));
#73595=CARTESIAN_POINT('Ctrl Pts',(42.9647078359471,-0.122874749759113,
328.794332870184));
#73596=CARTESIAN_POINT('Ctrl Pts',(42.686469801673,-5.28497245921135,331.745085433442));
#73597=CARTESIAN_POINT('Ctrl Pts',(42.4082317673992,-5.59712894891147,337.68282505197));
#73598=CARTESIAN_POINT('Ctrl Pts',(42.1299937331252,-0.772882815683387,
341.158575718739));
#73599=CARTESIAN_POINT('Ctrl Pts',(41.8517556988512,4.76062646976567,338.98269234885));
#73600=CARTESIAN_POINT('Ctrl Pts',(41.5735176645774,5.92537911064229,333.151950994864));
#73601=CARTESIAN_POINT('Ctrl Pts',(41.2952796303033,1.65249880013479,329.017136935732));
#73602=CARTESIAN_POINT('Ctrl Pts',(41.0170415960296,-4.13685526841409,330.372708003766));
#73603=CARTESIAN_POINT('Ctrl Pts',(40.7388035617553,-6.12987831702303,335.974676638024));
#73604=CARTESIAN_POINT('Ctrl Pts',(40.4605655274817,-2.49760251095559,340.682198907772));
#73605=CARTESIAN_POINT('Ctrl Pts',(40.1823274932075,3.42668625486317,340.175251108975));
#73606=CARTESIAN_POINT('Ctrl Pts',(39.9040894589337,6.20635562240021,334.919051754053));
#73607=CARTESIAN_POINT('Ctrl Pts',(39.6258514246597,3.2905440409194,329.737137409643));
#73608=CARTESIAN_POINT('Ctrl Pts',(39.3476133903858,-2.64495123856271,329.384874384678));
#73609=CARTESIAN_POINT('Ctrl Pts',(39.0693753561119,-6.15321380583211,334.185529257777));
#73610=CARTESIAN_POINT('Ctrl Pts',(38.7911373218379,-4.01476288477629,339.733611909445));
#73611=CARTESIAN_POINT('Ctrl Pts',(38.512899287564,1.80797667783569,340.937728779813));
#73612=CARTESIAN_POINT('Ctrl Pts',(38.23466125329,5.97156272888989,336.69287958968));
#73613=CARTESIAN_POINT('Ctrl Pts',(37.9564232190161,4.65513380376322,330.894499786959));
#73614=CARTESIAN_POINT('Ctrl Pts',(37.6781851847422,-0.93324270341463,328.863676932662));
#73615=CARTESIAN_POINT('Ctrl Pts',(37.3999471504682,-5.6651961563086,332.464067185281));
#73616=CARTESIAN_POINT('Ctrl Pts',(37.1217091161943,-5.19828271471637,338.391645551662));
#73617=CARTESIAN_POINT('Ctrl Pts',(36.8434710819203,0.0390180476439763,
341.206760855887));
#73618=CARTESIAN_POINT('Ctrl Pts',(36.5652330476464,5.24051252358688,338.326023334307));
#73619=CARTESIAN_POINT('Ctrl Pts',(36.2869950133724,5.63286600647216,332.393043290855));
#73620=CARTESIAN_POINT('Ctrl Pts',(36.0087569790986,0.856021496183908,328.85242894077));
#73621=CARTESIAN_POINT('Ctrl Pts',(35.7305189448245,-4.70638130629574,330.953349813738));
#73622=CARTESIAN_POINT('Ctrl Pts',(35.4522809105507,-5.94980745006201,336.767821834182));
#73623=CARTESIAN_POINT('Ctrl Pts',(35.1740428762767,-1.73318311592037,340.959989850402));
#73624=CARTESIAN_POINT('Ctrl Pts',(34.8958048420028,4.07395778196053,339.682763150217));
#73625=CARTESIAN_POINT('Ctrl Pts',(34.6175668077288,6.14248775485454,334.108233824547));
#73626=CARTESIAN_POINT('Ctrl Pts',(34.3393287734549,2.5741473780892,329.352065155644));
#73627=CARTESIAN_POINT('Ctrl Pts',(34.0610907391809,-3.35645005319558,329.778922930024));
#73628=CARTESIAN_POINT('Ctrl Pts',(33.7828527049071,-6.20688281178436,334.997086068551));
#73629=CARTESIAN_POINT('Ctrl Pts',(33.504614670633,-3.36135082743875,340.217923278958));
#73630=CARTESIAN_POINT('Ctrl Pts',(33.2263766363592,2.56884319779051,340.650349312687));
#73631=CARTESIAN_POINT('Ctrl Pts',(32.9481386020852,6.14164773647087,335.897533181182));
#73632=CARTESIAN_POINT('Ctrl Pts',(32.6699005678113,4.07835279796391,330.321064096874));
#73633=CARTESIAN_POINT('Ctrl Pts',(32.3916625335373,-1.7275863068459,329.038385429884));
#73634=CARTESIAN_POINT('Ctrl Pts',(32.1134244992634,-5.94814495699532,333.226592460602));
#73635=CARTESIAN_POINT('Ctrl Pts',(31.8351864649894,-4.71017877458579,339.042229414774));
#73636=CARTESIAN_POINT('Ctrl Pts',(31.5569484307155,0.85024894713638,341.148372098216));
#73637=CARTESIAN_POINT('Ctrl Pts',(31.2787103964415,5.63041575972536,337.612244456948));
#73638=CARTESIAN_POINT('Ctrl Pts',(31.0004723621677,5.24363313441479,331.678898634205));
#73639=CARTESIAN_POINT('Ctrl Pts',(30.7222343278936,0.0448457775499455,
328.793278515476));
#73640=CARTESIAN_POINT('Ctrl Pts',(30.4439962936198,-5.1950958874499,331.603475092036));
#73641=CARTESIAN_POINT('Ctrl Pts',(30.1657582593458,-5.66757473602656,337.530612444009));
#73642=CARTESIAN_POINT('Ctrl Pts',(29.8875202250719,-0.939003902617646,
341.135444107894));
#73643=CARTESIAN_POINT('Ctrl Pts',(29.6092821907979,4.65127695254862,339.10986927297));
#73644=CARTESIAN_POINT('Ctrl Pts',(29.331044156524,5.97314960109628,333.312728067814));
#73645=CARTESIAN_POINT('Ctrl Pts',(29.05280612225,1.81355102426149,329.06397141073));
#73646=CARTESIAN_POINT('Ctrl Pts',(28.7745680879761,-4.01031655956884,330.262620574382));
#73647=CARTESIAN_POINT('Ctrl Pts',(28.4963300537022,-6.15397582885823,335.808692913317));
#73648=CARTESIAN_POINT('Ctrl Pts',(28.2180920194283,-2.6502223125389,340.612639701989));
#73649=CARTESIAN_POINT('Ctrl Pts',(27.9398539851543,3.28560110277981,340.265949878572));
#73650=CARTESIAN_POINT('Ctrl Pts',(27.6616159508804,6.20627688147068,335.086775576883));
#73651=CARTESIAN_POINT('Ctrl Pts',(27.3833779166065,3.43154397053261,329.827968609094));
#73652=CARTESIAN_POINT('Ctrl Pts',(27.1051398823325,-2.49226619265724,329.315458509681));
#73653=CARTESIAN_POINT('Ctrl Pts',(26.8269018480586,-6.12896045663425,334.01956823224));
#73654=CARTESIAN_POINT('Ctrl Pts',(26.5486638137846,-4.14119817286605,339.623405716922));
#73655=CARTESIAN_POINT('Ctrl Pts',(26.2704257795108,1.64688055015648,340.984412016543));
#73656=CARTESIAN_POINT('Ctrl Pts',(25.9921877452367,5.92364130021749,336.853611738357));
#73657=CARTESIAN_POINT('Ctrl Pts',(25.7139497109629,4.76436386187118,331.021779327147));
#73658=CARTESIAN_POINT('Ctrl Pts',(25.4357116766889,-0.767099970618971,
328.840701308971));
#73659=CARTESIAN_POINT('Ctrl Pts',(25.157473642415,-5.59460748244911,332.311920788455));
#73660=CARTESIAN_POINT('Ctrl Pts',(24.879235608141,-5.28802628390677,338.249950884387));
#73661=CARTESIAN_POINT('Ctrl Pts',(24.6009975738671,-0.128701415763207,
341.205549022917));
#73662=CARTESIAN_POINT('Ctrl Pts',(24.3227595395931,5.14873084199648,338.466406416866));
#73663=CARTESIAN_POINT('Ctrl Pts',(24.0445215053192,5.70124880119865,332.546193806135));
#73664=CARTESIAN_POINT('Ctrl Pts',(23.7662834710453,1.02181488583519,328.877802921394));
#73665=CARTESIAN_POINT('Ctrl Pts',(23.4880454367713,-4.59532346829624,330.827661932208));
#73666=CARTESIAN_POINT('Ctrl Pts',(23.2098074024974,-5.9954013024354,336.606414004227));
#73667=CARTESIAN_POINT('Ctrl Pts',(22.9315693682235,-1.89358785330778,340.910983655199));
#73668=CARTESIAN_POINT('Ctrl Pts',(22.6533313339495,3.9459432194895,339.79113085177));
#73669=CARTESIAN_POINT('Ctrl Pts',(22.3750932996756,6.16434044178771,334.274527982648));
#73670=CARTESIAN_POINT('Ctrl Pts',(22.0968552654016,2.72581342617312,329.4236800759));
#73671=CARTESIAN_POINT('Ctrl Pts',(21.8186172311277,-3.21415233770034,329.690138657152));
#73672=CARTESIAN_POINT('Ctrl Pts',(21.5403791968537,-6.20453794207692,334.82937861931));
#73673=CARTESIAN_POINT('Ctrl Pts',(21.2621411625798,-3.50111065583944,340.125195304161));
#73674=CARTESIAN_POINT('Ctrl Pts',(20.9839031283059,2.41523420295332,340.717695906141));
#73675=CARTESIAN_POINT('Ctrl Pts',(20.705665094032,6.11515428249423,336.063151368109));
#73676=CARTESIAN_POINT('Ctrl Pts',(20.427427059758,4.20328753651943,330.432968511652));
#73677=CARTESIAN_POINT('Ctrl Pts',(20.1491890254841,-1.56587414129691,328.993883042778));
#73678=CARTESIAN_POINT('Ctrl Pts',(19.8709509912101,-5.89805623190951,333.066522455404));
#73679=CARTESIAN_POINT('Ctrl Pts',(19.5927129569362,-4.81767917366603,338.913485672627));
#73680=CARTESIAN_POINT('Ctrl Pts',(19.3144749226622,0.683810953422714,341.16910085103));
#73681=CARTESIAN_POINT('Ctrl Pts',(19.0362368883883,5.55777786158857,337.763423234226));
#73682=CARTESIAN_POINT('Ctrl Pts',(18.7579988541143,5.33145405884136,331.82179290343));
#73683=CARTESIAN_POINT('Ctrl Pts',(18.4797608198405,0.212533558428351,328.796756314898));
#73684=CARTESIAN_POINT('Ctrl Pts',(18.2015227855665,-5.10142585156417,331.464344896456));
#73685=CARTESIAN_POINT('Ctrl Pts',(17.9232847512926,-5.73388205449841,337.376551980354));
#73686=CARTESIAN_POINT('Ctrl Pts',(17.6450467170186,-1.10443932797984,341.10783238973));
#73687=CARTESIAN_POINT('Ctrl Pts',(17.3668086827447,4.53853106832805,339.23404516651));
#73688=CARTESIAN_POINT('Ctrl Pts',(17.0885706484707,6.01655849184008,333.474737188387));
#73689=CARTESIAN_POINT('Ctrl Pts',(16.8103326141968,1.97327899164818,329.115140379641));
#73690=CARTESIAN_POINT('Ctrl Pts',(16.5320945799228,-3.88084951362897,330.155992384111));
#73691=CARTESIAN_POINT('Ctrl Pts',(16.2538565456489,-6.17357970149395,335.642118680249));
#73692=CARTESIAN_POINT('Ctrl Pts',(15.975618511375,-2.80090691918455,340.538982141178));
#73693=CARTESIAN_POINT('Ctrl Pts',(15.697380477101,3.14211680154138,340.352803446391));
#73694=CARTESIAN_POINT('Ctrl Pts',(15.4191424428271,6.2016663110622,335.254436036101));
#73695=CARTESIAN_POINT('Ctrl Pts',(15.1409044085532,3.57003818336322,329.92257643095));
#73696=CARTESIAN_POINT('Ctrl Pts',(14.8626663742792,-2.33776129152583,329.250193492469));
#73697=CARTESIAN_POINT('Ctrl Pts',(14.5844283400053,-6.10023173449145,333.854323118942));
#73698=CARTESIAN_POINT('Ctrl Pts',(14.3061903057313,-4.26460955396873,339.509823509002));
#73699=CARTESIAN_POINT('Ctrl Pts',(14.0279522714575,1.48458186866264,341.026725429732));
#73700=CARTESIAN_POINT('Ctrl Pts',(13.7497142371834,5.87139442288012,337.012990377927));
#73701=CARTESIAN_POINT('Ctrl Pts',(13.4714762029096,4.87011497673675,331.151963767972));
#73702=CARTESIAN_POINT('Ctrl Pts',(13.1932381686356,-0.600397100545508,
328.822223211257));
#73703=CARTESIAN_POINT('Ctrl Pts',(12.9150001343617,-5.51993362094364,332.161737229679));
#73704=CARTESIAN_POINT('Ctrl Pts',(12.6367621000877,-5.37390853065834,338.105883099841));
#73705=CARTESIAN_POINT('Ctrl Pts',(12.3585240658138,-0.296326902116208,
341.199805891837));
#73706=CARTESIAN_POINT('Ctrl Pts',(12.0802860315399,5.05318955368163,338.604258326258));
#73707=CARTESIAN_POINT('Ctrl Pts',(11.8020479972659,5.76546853542933,332.701136092723));
#73708=CARTESIAN_POINT('Ctrl Pts',(11.523809962992,1.18686215094859,328.907647337068));
#73709=CARTESIAN_POINT('Ctrl Pts',(11.245571928718,-4.48091013133853,330.705020694665));
#73710=CARTESIAN_POINT('Ctrl Pts',(10.9673338944441,-6.03661728657534,336.443833171777));
#73711=CARTESIAN_POINT('Ctrl Pts',(10.6890958601702,-2.0526099293305,340.857661249031));
#73712=CARTESIAN_POINT('Ctrl Pts',(10.4108578258962,3.81504739780807,339.896000074094));
#73713=CARTESIAN_POINT('Ctrl Pts',(10.1326197916223,6.18169178455076,334.441351863707));
#73714=CARTESIAN_POINT('Ctrl Pts',(9.85438175734834,2.87548934076866,329.499366863342));
#73715=CARTESIAN_POINT('Ctrl Pts',(9.5761437230744,-3.06950813245751,329.605231588139));
#73716=CARTESIAN_POINT('Ctrl Pts',(9.29790568880045,-6.19766159226215,334.661795875251));
#73717=CARTESIAN_POINT('Ctrl Pts',(9.01966765452654,-3.63831570770535,340.028724685263));
#73718=CARTESIAN_POINT('Ctrl Pts',(8.74142962025257,2.25986488325026,340.780867850567));
#73719=CARTESIAN_POINT('Ctrl Pts',(8.46319158597866,6.08418934066576,336.227992451325));
#73720=CARTESIAN_POINT('Ctrl Pts',(8.18495355170471,4.32516473003851,330.548209268121));
#73721=CARTESIAN_POINT('Ctrl Pts',(7.90671551743075,-1.40304066423951,328.953763513228));
#73722=CARTESIAN_POINT('Ctrl Pts',(7.62847748315686,-5.84361902743119,332.907869592604));
#73723=CARTESIAN_POINT('Ctrl Pts',(7.35023944888287,-4.92174046128214,338.781874263245));
#73724=CARTESIAN_POINT('Ctrl Pts',(7.07200141460898,0.517022360924158,341.185343870472));
#73725=CARTESIAN_POINT('Ctrl Pts',(6.79376338033501,5.48080084698006,337.91254837672));
#73726=CARTESIAN_POINT('Ctrl Pts',(6.51552534606109,5.41591225410207,331.967075452871));
#73727=CARTESIAN_POINT('Ctrl Pts',(6.23728731178713,0.37906437176057,328.804636265691));
#73728=CARTESIAN_POINT('Ctrl Pts',(5.95904927751322,-5.00213548323109,331.328036418174));
#73729=CARTESIAN_POINT('Ctrl Pts',(5.68081124323926,-5.79961147366261,337.220308739124));
#73730=CARTESIAN_POINT('Ctrl Pts',(5.40257320896532,-1.26200573051318,341.0765584996));
#73731=CARTESIAN_POINT('Ctrl Pts',(5.17070818040372,3.46225453493836,339.641128094155));
#73732=CARTESIAN_POINT('Ctrl Pts',(4.98521615755441,5.25418438838292,336.493556731435));
#73733=CARTESIAN_POINT('Ctrl Pts',(4.89247014612976,5.31273941270785,334.700718340289));
#73734=CARTESIAN_POINT('Ctrl Pts',(4.84609714041744,5.12095026465303,333.848094201961));
#73735=CARTESIAN_POINT('Ctrl Pts',(185.228765085591,2.85368302903013,338.999449094237));
#73736=CARTESIAN_POINT('Ctrl Pts',(185.182382275899,3.51972456975641,338.524219201027));
#73737=CARTESIAN_POINT('Ctrl Pts',(185.089626460494,4.59778811197941,337.236718862335));
#73738=CARTESIAN_POINT('Ctrl Pts',(184.904124633665,5.31167233335097,333.92231966833));
#73739=CARTESIAN_POINT('Ctrl Pts',(184.672259605103,2.91125672484798,329.972890248405));
#73740=CARTESIAN_POINT('Ctrl Pts',(184.394021570829,-2.66092683012348,329.831943356036));
#73741=CARTESIAN_POINT('Ctrl Pts',(184.115783536555,-5.78129223874898,334.4406109034));
#73742=CARTESIAN_POINT('Ctrl Pts',(183.837545502281,-3.60141999782881,339.559046781404));
#73743=CARTESIAN_POINT('Ctrl Pts',(183.559307468008,1.88614899471333,340.495592016401));
#73744=CARTESIAN_POINT('Ctrl Pts',(183.281069433733,5.64138409112437,336.387919992591));
#73745=CARTESIAN_POINT('Ctrl Pts',(183.00283139946,4.22036822806485,331.007100272962));
#73746=CARTESIAN_POINT('Ctrl Pts',(182.724593365185,-1.07402183899175,329.290227153788));
#73747=CARTESIAN_POINT('Ctrl Pts',(182.446355330911,-5.38258365553329,332.813275814337));
#73748=CARTESIAN_POINT('Ctrl Pts',(182.168117296638,-4.75174137159609,338.342970859998));
#73749=CARTESIAN_POINT('Ctrl Pts',(181.889879262364,0.239763929394143,340.804912264382));
#73750=CARTESIAN_POINT('Ctrl Pts',(181.61164122809,5.01120958425209,337.939749451869));
#73751=CARTESIAN_POINT('Ctrl Pts',(181.333403193816,5.18395902469876,332.376833562816));
#73752=CARTESIAN_POINT('Ctrl Pts',(181.055165159542,0.599456856430579,329.22115264934));
#73753=CARTESIAN_POINT('Ctrl Pts',(180.776927125268,-4.5351532933155,331.36863790884));
#73754=CARTESIAN_POINT('Ctrl Pts',(180.498689090994,-5.50792270834741,336.848568836761));
#73755=CARTESIAN_POINT('Ctrl Pts',(180.22045105672,-1.42615142470787,340.63209634096));
#73756=CARTESIAN_POINT('Ctrl Pts',(179.942213022446,3.96437726915641,339.247131679169));
#73757=CARTESIAN_POINT('Ctrl Pts',(179.663974988173,5.71685582915296,333.964637219027));
#73758=CARTESIAN_POINT('Ctrl Pts',(179.385736953898,2.22305997841688,329.632279765444));
#73759=CARTESIAN_POINT('Ctrl Pts',(179.107498919624,-3.31080509788334,330.225800015512));
#73760=CARTESIAN_POINT('Ctrl Pts',(178.82926088535,-5.80639325850615,335.200533086233));
#73761=CARTESIAN_POINT('Ctrl Pts',(178.551022851076,-2.97353999876288,339.991239923725));
#73762=CARTESIAN_POINT('Ctrl Pts',(178.272784816803,2.58808701297097,340.201559543127));
#73763=CARTESIAN_POINT('Ctrl Pts',(177.994546782528,5.77466478120961,335.638484750344));
#73764=CARTESIAN_POINT('Ctrl Pts',(177.716308748255,3.66191790929846,330.489481923198));
#73765=CARTESIAN_POINT('Ctrl Pts',(177.43807071398,-1.81131697585433,329.47971496158));
#73766=CARTESIAN_POINT('Ctrl Pts',(177.159832679707,-5.62233300847941,333.535832099607));
#73767=CARTESIAN_POINT('Ctrl Pts',(176.881594645433,-4.2738170240765,338.935594509187));
#73768=CARTESIAN_POINT('Ctrl Pts',(176.603356611159,0.996717761543614,340.723719926729));
#73769=CARTESIAN_POINT('Ctrl Pts',(176.325118576885,5.35257936910628,337.259272049606));
#73770=CARTESIAN_POINT('Ctrl Pts',(176.046880542611,4.79645789348621,331.721523559292));
#73771=CARTESIAN_POINT('Ctrl Pts',(175.768642508337,-0.161302195332879,
329.192384508421));
#73772=CARTESIAN_POINT('Ctrl Pts',(175.490404474063,-4.97103764033839,331.992808473886));
#73773=CARTESIAN_POINT('Ctrl Pts',(175.212166439789,-5.21892521518643,337.552887716805));
#73774=CARTESIAN_POINT('Ctrl Pts',(174.933928405515,-0.677482151275358,
340.770219582566));
#73775=CARTESIAN_POINT('Ctrl Pts',(174.655690371242,4.48567628324494,338.692306105712));
#73776=CARTESIAN_POINT('Ctrl Pts',(174.377452336967,5.53239580110267,333.226017813993));
#73777=CARTESIAN_POINT('Ctrl Pts',(174.099214302694,1.50211735031779,329.38768679044));
#73778=CARTESIAN_POINT('Ctrl Pts',(173.820976268419,-3.90663202163858,330.699692761692));
#73779=CARTESIAN_POINT('Ctrl Pts',(173.542738234146,-5.73032284913103,335.95802721311));
#73780=CARTESIAN_POINT('Ctrl Pts',(173.264500199872,-2.29538097740274,340.337194231514));
#73781=CARTESIAN_POINT('Ctrl Pts',(172.986262165598,3.24599813752044,339.818496880517));
#73782=CARTESIAN_POINT('Ctrl Pts',(172.708024131324,5.80857267249504,334.877936063166));
#73783=CARTESIAN_POINT('Ctrl Pts',(172.42978609705,3.04070580031311,330.049391518987));
#73784=CARTESIAN_POINT('Ctrl Pts',(172.151548062776,-2.51757190407213,329.763947306973));
#73785=CARTESIAN_POINT('Ctrl Pts',(171.873310028502,-5.76551103139077,334.283551367338));
#73786=CARTESIAN_POINT('Ctrl Pts',(171.595071994228,-3.72252578400546,339.460629763133));
#73787=CARTESIAN_POINT('Ctrl Pts',(171.316833959954,1.73656643097114,340.544254064088));
#73788=CARTESIAN_POINT('Ctrl Pts',(171.03859592568,5.60203726392403,336.539998243486));
#73789=CARTESIAN_POINT('Ctrl Pts',(170.760357891406,4.32660118570833,331.122508765173));
#73790=CARTESIAN_POINT('Ctrl Pts',(170.482119857132,-0.919292940103036,
329.263335761385));
#73791=CARTESIAN_POINT('Ctrl Pts',(170.203881822858,-5.32156550352343,332.668614856348));
#73792=CARTESIAN_POINT('Ctrl Pts',(169.925643788584,-4.84031595053847,338.213371686453));
#73793=CARTESIAN_POINT('Ctrl Pts',(169.64740575431,0.0828201073093179,340.809264749189));
#73794=CARTESIAN_POINT('Ctrl Pts',(169.369167720037,4.92995337510213,338.0740812962));
#73795=CARTESIAN_POINT('Ctrl Pts',(169.090929685762,5.25294119655625,332.517858811056));
#73796=CARTESIAN_POINT('Ctrl Pts',(168.812691651489,0.755382415215671,329.23946065866));
#73797=CARTESIAN_POINT('Ctrl Pts',(168.534453617214,-4.43537965914216,331.247424434392));
#73798=CARTESIAN_POINT('Ctrl Pts',(168.256215582941,-5.55585928640169,336.699071418756));
#73799=CARTESIAN_POINT('Ctrl Pts',(167.977977548667,-1.57780885087906,340.591505640382));
#73800=CARTESIAN_POINT('Ctrl Pts',(167.699739514393,3.8481734786748,339.352697666316));
#73801=CARTESIAN_POINT('Ctrl Pts',(167.421501480119,5.74274380579626,334.119483289585));
#73802=CARTESIAN_POINT('Ctrl Pts',(167.143263445845,2.3672829050982,329.694306101596));
#73803=CARTESIAN_POINT('Ctrl Pts',(166.865025411571,-3.18059857657007,330.138085892259));
#73804=CARTESIAN_POINT('Ctrl Pts',(166.586787377297,-5.80969169007805,335.043572497861));
#73805=CARTESIAN_POINT('Ctrl Pts',(166.308549343023,-3.10731649051019,339.909073265305));
#73806=CARTESIAN_POINT('Ctrl Pts',(166.030311308749,2.44659718848265,340.269589954981));
#73807=CARTESIAN_POINT('Ctrl Pts',(165.752073274475,5.75530473932027,335.794281721991));
#73808=CARTESIAN_POINT('Ctrl Pts',(165.473835240201,3.78245407904238,330.590072876309));
#73809=CARTESIAN_POINT('Ctrl Pts',(165.195597205928,-1.66149886064201,329.43278906162));
#73810=CARTESIAN_POINT('Ctrl Pts',(164.917359171654,-5.58071881959822,333.384452553184));
#73811=CARTESIAN_POINT('Ctrl Pts',(164.63912113738,-4.37859548908389,338.81868009125));
#73812=CARTESIAN_POINT('Ctrl Pts',(164.360883103105,0.841700293799237,340.748561273202));
#73813=CARTESIAN_POINT('Ctrl Pts',(164.082645068832,5.28958014053878,337.403072623362));
#73814=CARTESIAN_POINT('Ctrl Pts',(163.804407034558,4.88329036638077,331.852319696357));
#73815=CARTESIAN_POINT('Ctrl Pts',(163.526169000284,-0.00432289975708849,
329.19014652432));
#73816=CARTESIAN_POINT('Ctrl Pts',(163.24793096601,-4.8879691045938,331.859590133619));
#73817=CARTESIAN_POINT('Ctrl Pts',(162.969692931736,-5.28599820845056,337.410941524921));
#73818=CARTESIAN_POINT('Ctrl Pts',(162.691454897462,-0.833144777617896,
340.749807464242));
#73819=CARTESIAN_POINT('Ctrl Pts',(162.413216863188,4.38427331843794,338.812159960648));
#73820=CARTESIAN_POINT('Ctrl Pts',(162.134978828914,5.5783085019314,333.376149528555));
#73821=CARTESIAN_POINT('Ctrl Pts',(161.85674079464,1.65321230890092,329.430322706114));
#73822=CARTESIAN_POINT('Ctrl Pts',(161.578502760366,-3.78901241863424,330.59570652797));
#73823=CARTESIAN_POINT('Ctrl Pts',(161.300264726092,-5.75411637532039,335.802845461843));
#73824=CARTESIAN_POINT('Ctrl Pts',(161.022026691818,-2.43875266499349,340.273224965362));
#73825=CARTESIAN_POINT('Ctrl Pts',(160.743788657544,3.1146183700676,339.904443750842));
#73826=CARTESIAN_POINT('Ctrl Pts',(160.465550623271,5.80975009860945,335.034926895645));
#73827=CARTESIAN_POINT('Ctrl Pts',(160.187312588997,3.17335991342832,330.133358143835));
#73828=CARTESIAN_POINT('Ctrl Pts',(159.909074554723,-2.37517582559034,329.697834791912));
#73829=CARTESIAN_POINT('Ctrl Pts',(159.630836520449,-5.74404776700253,334.128030191621));
#73830=CARTESIAN_POINT('Ctrl Pts',(159.352598486175,-3.84169185464261,339.358419414226));
#73831=CARTESIAN_POINT('Ctrl Pts',(159.074360451901,1.58612796944403,340.589151470561));
#73832=CARTESIAN_POINT('Ctrl Pts',(158.796122417627,5.55838156718232,336.690801718102));
#73833=CARTESIAN_POINT('Ctrl Pts',(158.517884383353,4.42979044229486,331.240828185134));
#73834=CARTESIAN_POINT('Ctrl Pts',(158.239646349079,-0.763953987886848,
329.240591141382));
#73835=CARTESIAN_POINT('Ctrl Pts',(157.961408314805,-5.25662911932717,332.525678598449));
#73836=CARTESIAN_POINT('Ctrl Pts',(157.683170280531,-4.92537329567956,338.081414284795));
#73837=CARTESIAN_POINT('Ctrl Pts',(157.404932246257,-0.0741750969775079,
340.809381563585));
#73838=CARTESIAN_POINT('Ctrl Pts',(157.126694211983,4.84509249339818,338.206165127804));
#73839=CARTESIAN_POINT('Ctrl Pts',(156.848456177709,5.31809021603033,332.660698277158));
#73840=CARTESIAN_POINT('Ctrl Pts',(156.570218143435,0.910755042294368,329.261974089526));
#73841=CARTESIAN_POINT('Ctrl Pts',(156.291980109161,-4.33236659103269,331.128951586813));
#73842=CARTESIAN_POINT('Ctrl Pts',(156.013742074888,-5.59973934939517,336.548333076301));
#73843=CARTESIAN_POINT('Ctrl Pts',(155.735504040614,-1.72831395883512,340.546832155026));
#73844=CARTESIAN_POINT('Ctrl Pts',(155.457266006339,3.72915964187575,339.455085236193));
#73845=CARTESIAN_POINT('Ctrl Pts',(155.179027972066,5.76443848154334,334.274972353055));
#73846=CARTESIAN_POINT('Ctrl Pts',(154.900789937792,2.50977720967112,329.760206640129));
#73847=CARTESIAN_POINT('Ctrl Pts',(154.622551903518,-3.04806956326539,330.053921954334));
#73848=CARTESIAN_POINT('Ctrl Pts',(154.344313869244,-5.80874788742625,334.886580087053));
#73849=CARTESIAN_POINT('Ctrl Pts',(154.06607583497,-3.23882401227433,339.82332199981));
#73850=CARTESIAN_POINT('Ctrl Pts',(153.787837800696,2.3033208539777,340.333772505456));
#73851=CARTESIAN_POINT('Ctrl Pts',(153.509599766422,5.73174216949446,335.949498709199));
#73852=CARTESIAN_POINT('Ctrl Pts',(153.231361732148,3.90022829644191,330.693883962088));
#73853=CARTESIAN_POINT('Ctrl Pts',(152.953123697874,-1.5104675169801,329.3899283448));
#73854=CARTESIAN_POINT('Ctrl Pts',(152.6748856636,-5.53502958453341,333.234252680968));
#73855=CARTESIAN_POINT('Ctrl Pts',(152.396647629326,-4.48017669926329,338.698977269423));
#73856=CARTESIAN_POINT('Ctrl Pts',(152.118409595052,0.686068215621029,340.769205014545));
#73857=CARTESIAN_POINT('Ctrl Pts',(151.840171560778,5.22271845538023,337.545118471145));
#73858=CARTESIAN_POINT('Ctrl Pts',(151.561933526504,4.96655705583505,331.985414272663));
#73859=CARTESIAN_POINT('Ctrl Pts',(151.283695492231,0.152659552412012,329.192150900945));
#73860=CARTESIAN_POINT('Ctrl Pts',(151.005457457957,-4.80133136900823,331.728664923719));
#73861=CARTESIAN_POINT('Ctrl Pts',(150.727219423682,-5.34921136062445,337.267234861169));
#73862=CARTESIAN_POINT('Ctrl Pts',(150.448981389409,-0.988199040825888,
340.725196830856));
#73863=CARTESIAN_POINT('Ctrl Pts',(150.170743355135,4.27966895294467,338.929230172633));
#73864=CARTESIAN_POINT('Ctrl Pts',(149.892505320861,5.62014791640809,333.527466980328));
#73865=CARTESIAN_POINT('Ctrl Pts',(149.614267286587,1.80310009023112,329.477025605624));
#73866=CARTESIAN_POINT('Ctrl Pts',(149.336029252313,-3.66862607503718,330.49493631367));
#73867=CARTESIAN_POINT('Ctrl Pts',(149.057791218039,-5.77370824007606,335.647077472031));
#73868=CARTESIAN_POINT('Ctrl Pts',(148.779553183765,-2.5803435729911,340.205405185156));
#73869=CARTESIAN_POINT('Ctrl Pts',(148.501315149491,2.98096430521908,339.986809391519));
#73870=CARTESIAN_POINT('Ctrl Pts',(148.223077115217,5.80668523949074,335.191892224471));
#73871=CARTESIAN_POINT('Ctrl Pts',(147.944839080943,3.30369683601538,330.22087839535));
#73872=CARTESIAN_POINT('Ctrl Pts',(147.666601046669,-2.23104539138592,329.635593923097));
#73873=CARTESIAN_POINT('Ctrl Pts',(147.388363012396,-5.71839019328836,333.973145729115));
#73874=CARTESIAN_POINT('Ctrl Pts',(147.110124978121,-3.95805271811097,339.25302654318));
#73875=CARTESIAN_POINT('Ctrl Pts',(146.831886943848,1.43453131571451,340.629967673136));
#73876=CARTESIAN_POINT('Ctrl Pts',(146.553648909573,5.5106671347563,336.840370567645));
#73877=CARTESIAN_POINT('Ctrl Pts',(146.2754108753,4.52974506154582,331.361892556048));
#73878=CARTESIAN_POINT('Ctrl Pts',(145.997172841026,-0.608057195717691,
329.222052047391));
#73879=CARTESIAN_POINT('Ctrl Pts',(145.718934806752,-5.18785433938055,332.38454909247));
#73880=CARTESIAN_POINT('Ctrl Pts',(145.440696772478,-5.00683412839853,337.947206831397));
#73881=CARTESIAN_POINT('Ctrl Pts',(145.162458738204,-0.231116138535769,
340.805256361854));
#73882=CARTESIAN_POINT('Ctrl Pts',(144.88422070393,4.75669372039265,338.33590781448));
#73883=CARTESIAN_POINT('Ctrl Pts',(144.605982669656,5.37935596080095,332.805245903677));
#73884=CARTESIAN_POINT('Ctrl Pts',(144.327744635382,1.06546263514606,329.288677432552));
#73885=CARTESIAN_POINT('Ctrl Pts',(144.049506601108,-4.22619002457966,331.013305382591));
#73886=CARTESIAN_POINT('Ctrl Pts',(143.771268566834,-5.63953047721114,336.396464139511));
#73887=CARTESIAN_POINT('Ctrl Pts',(143.49303053256,-1.87755705023934,340.498108367378));
#73888=CARTESIAN_POINT('Ctrl Pts',(143.214792498286,3.60742276904044,339.554219698449));
#73889=CARTESIAN_POINT('Ctrl Pts',(142.936554464012,5.78192395864463,334.430990832426));
#73890=CARTESIAN_POINT('Ctrl Pts',(142.658316429739,2.65043887245836,329.829933280924));
#73891=CARTESIAN_POINT('Ctrl Pts',(142.380078395464,-2.91331484656925,329.973369647459));
#73892=CARTESIAN_POINT('Ctrl Pts',(142.101840361191,-5.80356253135695,334.729670495578));
#73893=CARTESIAN_POINT('Ctrl Pts',(141.823602326917,-3.36796654156104,339.734048739849));
#73894=CARTESIAN_POINT('Ctrl Pts',(141.545364292643,2.1583626323208,340.394060330005));
#73895=CARTESIAN_POINT('Ctrl Pts',(141.267126258369,5.70399427590206,336.104022371516));
#73896=CARTESIAN_POINT('Ctrl Pts',(140.988888224095,4.0151545633055,330.80083937803));
#73897=CARTESIAN_POINT('Ctrl Pts',(140.710650189821,-1.3583332284523,329.351164107817));
#73898=CARTESIAN_POINT('Ctrl Pts',(140.432412155547,-5.48529866542502,333.085342159178));
#73899=CARTESIAN_POINT('Ctrl Pts',(140.154174121273,-4.57848648001278,338.576573450759));
#73900=CARTESIAN_POINT('Ctrl Pts',(139.875936086999,0.529935169757505,340.785636076714));
#73901=CARTESIAN_POINT('Ctrl Pts',(139.597698052725,5.15204313607163,337.685305870919));
#73902=CARTESIAN_POINT('Ctrl Pts',(139.319460018451,5.04619716044484,332.120710102429));
#73903=CARTESIAN_POINT('Ctrl Pts',(139.041221984177,0.309530532425838,329.198396174692));
#73904=CARTESIAN_POINT('Ctrl Pts',(138.762983949904,-4.71118769653721,331.600128445908));
#73905=CARTESIAN_POINT('Ctrl Pts',(138.484745915629,-5.40851851340445,337.121872660291));
#73906=CARTESIAN_POINT('Ctrl Pts',(138.206507881356,-1.14253172012296,340.696405653115));
#73907=CARTESIAN_POINT('Ctrl Pts',(137.928269847081,4.17193956897484,339.043431256885));
#73908=CARTESIAN_POINT('Ctrl Pts',(137.650031812808,5.65788349335158,333.679859677159));
#73909=CARTESIAN_POINT('Ctrl Pts',(137.371793778534,1.95167124610305,329.527761386465));
#73910=CARTESIAN_POINT('Ctrl Pts',(137.09355574426,-3.54556089707387,330.397455701302));
#73911=CARTESIAN_POINT('Ctrl Pts',(136.815317709986,-5.78908413739917,335.490836985613));
#73912=CARTESIAN_POINT('Ctrl Pts',(136.537079675712,-2.72005031157503,340.133784412968));
#73913=CARTESIAN_POINT('Ctrl Pts',(136.258841641438,2.84513353730471,340.065533659077));
#73914=CARTESIAN_POINT('Ctrl Pts',(135.980603607164,5.7993803331021,335.348717433405));
#73915=CARTESIAN_POINT('Ctrl Pts',(135.70236557289,3.4316213959251,330.311888366159));
#73916=CARTESIAN_POINT('Ctrl Pts',(135.424127538616,-2.08528584564359,329.577270148875));
#73917=CARTESIAN_POINT('Ctrl Pts',(135.145889504342,-5.68855704543379,333.819011076606));
#73918=CARTESIAN_POINT('Ctrl Pts',(134.867651470068,-4.07152340759375,339.14452810797));
#73919=CARTESIAN_POINT('Ctrl Pts',(134.589413435794,1.28188716580795,340.666672867782));
#73920=CARTESIAN_POINT('Ctrl Pts',(134.31117540152,5.45892880777134,336.988595576787));
#73921=CARTESIAN_POINT('Ctrl Pts',(134.032937367246,4.62639205650012,331.485613476596));
#73922=CARTESIAN_POINT('Ctrl Pts',(133.754699332972,-0.451716399586434,
329.207732016673));
#73923=CARTESIAN_POINT('Ctrl Pts',(133.476461298699,-5.11529138309565,332.245329391314));
#73924=CARTESIAN_POINT('Ctrl Pts',(133.198223264425,-5.08463896591503,337.810847324675));
#73925=CARTESIAN_POINT('Ctrl Pts',(132.919985230151,-0.38788841886232,340.79689215622));
#73926=CARTESIAN_POINT('Ctrl Pts',(132.641747195877,4.66482160495669,338.46321461799));
#73927=CARTESIAN_POINT('Ctrl Pts',(132.363509161603,5.43669369456094,332.951396141795));
#73928=CARTESIAN_POINT('Ctrl Pts',(132.085271127329,1.21939222613404,329.319551188931));
#73929=CARTESIAN_POINT('Ctrl Pts',(131.807033093055,-4.11692749001633,330.900570266698));
#73930=CARTESIAN_POINT('Ctrl Pts',(131.528795058781,-5.67520361432885,336.243575503233));
#73931=CARTESIAN_POINT('Ctrl Pts',(131.250557024507,-2.02542914763983,340.445369855595));
#73932=CARTESIAN_POINT('Ctrl Pts',(130.972318990233,3.483051752553,339.650028665005));
#73933=CARTESIAN_POINT('Ctrl Pts',(130.694080955959,5.79518746918758,334.587424802851));
#73934=CARTESIAN_POINT('Ctrl Pts',(130.415842921685,2.78916518217566,329.903435109521));
#73935=CARTESIAN_POINT('Ctrl Pts',(130.137604887411,-2.77643282450829,329.896487791008));
#73936=CARTESIAN_POINT('Ctrl Pts',(129.859366853137,-5.7941394082223,334.572958298972));
#73937=CARTESIAN_POINT('Ctrl Pts',(129.581128818863,-3.49464977836818,339.641318672843));
#73938=CARTESIAN_POINT('Ctrl Pts',(129.302890784589,2.01182837214824,340.450409406398));
#73939=CARTESIAN_POINT('Ctrl Pts',(129.024652750315,5.67208132008231,336.257739875612));
#73940=CARTESIAN_POINT('Ctrl Pts',(128.746414716042,4.1271489603599,330.910861025188));
#73941=CARTESIAN_POINT('Ctrl Pts',(128.468176681768,-1.20520708366599,329.316524656355));
#73942=CARTESIAN_POINT('Ctrl Pts',(128.189938647494,-5.43156237583899,332.937829722429));
#73943=CARTESIAN_POINT('Ctrl Pts',(127.91170061322,-4.67345304543382,338.451558014644));
#73944=CARTESIAN_POINT('Ctrl Pts',(127.633462578946,0.373415164712107,340.797842461735));
#73945=CARTESIAN_POINT('Ctrl Pts',(127.355224544672,5.07760578980047,337.823532457706));
#73946=CARTESIAN_POINT('Ctrl Pts',(127.076986510398,5.12215252692763,332.258108392511));
#73947=CARTESIAN_POINT('Ctrl Pts',(126.798748476124,0.466175492940766,329.208877785255));
#73948=CARTESIAN_POINT('Ctrl Pts',(126.52051044185,-4.61760391017891,331.474074557648));
#73949=CARTESIAN_POINT('Ctrl Pts',(126.242272407576,-5.46387636064937,336.974961065912));
#73950=CARTESIAN_POINT('Ctrl Pts',(125.964034373302,-1.29603012163481,340.663454954368));
#73951=CARTESIAN_POINT('Ctrl Pts',(125.685796339028,4.06116383063079,339.154679823657));
#73952=CARTESIAN_POINT('Ctrl Pts',(125.407558304754,5.69148767820639,333.833216341752));
#73953=CARTESIAN_POINT('Ctrl Pts',(125.12932027048,2.09881728971241,329.58249300132));
#73954=CARTESIAN_POINT('Ctrl Pts',(124.851082236206,-3.41990674705822,330.303335871306));
#73955=CARTESIAN_POINT('Ctrl Pts',(124.572844201933,-5.80023283979438,335.334238089545));
#73956=CARTESIAN_POINT('Ctrl Pts',(124.294606167658,-2.85777086674761,340.058414946355));
#73957=CARTESIAN_POINT('Ctrl Pts',(124.016368133385,2.70722525008458,340.140559068977));
#73958=CARTESIAN_POINT('Ctrl Pts',(123.738130099111,5.78784071349336,335.505288008526));
#73959=CARTESIAN_POINT('Ctrl Pts',(123.459892064837,3.55704018251817,330.406321600691));
#73960=CARTESIAN_POINT('Ctrl Pts',(123.181654030563,-1.93800362212678,329.522906057319));
#73961=CARTESIAN_POINT('Ctrl Pts',(122.903415996289,-5.65457010763266,333.665738783371));
#73962=CARTESIAN_POINT('Ctrl Pts',(122.625177962015,-4.18202106668204,339.033003334261));
#73963=CARTESIAN_POINT('Ctrl Pts',(122.346939927741,1.12830698063291,340.699240252331));
#73964=CARTESIAN_POINT('Ctrl Pts',(122.068701893467,5.40320436560478,337.135368511485));
#73965=CARTESIAN_POINT('Ctrl Pts',(121.790463859193,4.71966085542685,331.611900605637));
#73966=CARTESIAN_POINT('Ctrl Pts',(121.512225824919,-0.295045759696265,
329.197641505731));
#73967=CARTESIAN_POINT('Ctrl Pts',(121.233987790645,-5.03899323601439,332.108121153345));
#73968=CARTESIAN_POINT('Ctrl Pts',(120.955749756371,-5.15873099506036,337.672435334473));
#73969=CARTESIAN_POINT('Ctrl Pts',(120.677511722097,-0.544377462684104,
340.784295054235));
#73970=CARTESIAN_POINT('Ctrl Pts',(120.399273687823,4.56954323219917,338.587992578782));
#73971=CARTESIAN_POINT('Ctrl Pts',(120.12103565355,5.49006154924083,333.099042272464));
#73972=CARTESIAN_POINT('Ctrl Pts',(119.842797619276,1.37243141571984,329.354572814616));
#73973=CARTESIAN_POINT('Ctrl Pts',(119.564559585002,-4.00465877095267,330.790828558426));
#73974=CARTESIAN_POINT('Ctrl Pts',(119.286321550728,-5.7067327121886,336.089778806901));
#73975=CARTESIAN_POINT('Ctrl Pts',(119.008083516454,-2.17182227468582,340.388655129391));
#73976=CARTESIAN_POINT('Ctrl Pts',(118.72984548218,3.35613740825191,339.742442176059));
#73977=CARTESIAN_POINT('Ctrl Pts',(118.451607447906,5.80421932814381,334.744160036089));
#73978=CARTESIAN_POINT('Ctrl Pts',(118.173369413632,2.92585484073498,329.980658454809));
#73979=CARTESIAN_POINT('Ctrl Pts',(117.895131379358,-2.63752344846967,329.823332524191));
#73980=CARTESIAN_POINT('Ctrl Pts',(117.616893345084,-5.780485398796,334.416557928635));
#73981=CARTESIAN_POINT('Ctrl Pts',(117.33865531081,-3.61878121847186,339.545199510381));
#73982=CARTESIAN_POINT('Ctrl Pts',(117.060417276536,1.86382507292066,340.502778588485));
#73983=CARTESIAN_POINT('Ctrl Pts',(116.782179242262,5.63602660490689,336.410538976814));
#73984=CARTESIAN_POINT('Ctrl Pts',(116.503941207988,4.23612970918638,331.023868565644));
#73985=CARTESIAN_POINT('Ctrl Pts',(116.225703173714,-1.05120089548245,329.286035284177));
#73986=CARTESIAN_POINT('Ctrl Pts',(115.94746513944,-5.37385995406682,332.791823084441));
#73987=CARTESIAN_POINT('Ctrl Pts',(115.669227105167,-4.76500705084698,338.324022247475));
#73988=CARTESIAN_POINT('Ctrl Pts',(115.390989070892,0.216622491546355,340.80581525649));
#73989=CARTESIAN_POINT('Ctrl Pts',(115.112751036619,4.99946077079033,337.959697298317));
#73990=CARTESIAN_POINT('Ctrl Pts',(114.834513002344,5.19436769260004,332.397508814538));
#73991=CARTESIAN_POINT('Ctrl Pts',(114.556274968071,0.622480051652159,329.223588078952));
#73992=CARTESIAN_POINT('Ctrl Pts',(114.278036933797,-4.52064834490641,331.350595303611));
#73993=CARTESIAN_POINT('Ctrl Pts',(113.999798899523,-5.51524448000453,336.826607353021));
#73994=CARTESIAN_POINT('Ctrl Pts',(113.721560865249,-1.44858216067782,340.626368795244));
#73995=CARTESIAN_POINT('Ctrl Pts',(113.443322830975,3.94742262646529,339.26289463914));
#73996=CARTESIAN_POINT('Ctrl Pts',(113.165084796701,5.72093593316378,333.987424992917));
#73997=CARTESIAN_POINT('Ctrl Pts',(112.886846762427,2.24443077487382,329.641180485114));
#73998=CARTESIAN_POINT('Ctrl Pts',(112.608608728153,-3.2917553777739,330.212645550074));
#73999=CARTESIAN_POINT('Ctrl Pts',(112.330370693879,-5.80714620646826,335.177395132495));
#74000=CARTESIAN_POINT('Ctrl Pts',(112.052132659606,-2.99340467482419,339.979351820174));
#74001=CARTESIAN_POINT('Ctrl Pts',(111.773894625331,2.56734014432545,340.211830837592));
#74002=CARTESIAN_POINT('Ctrl Pts',(111.495656591058,5.77207480690603,335.661489621848));
#74003=CARTESIAN_POINT('Ctrl Pts',(111.217418556783,3.67986161487345,330.504109143706));
#74004=CARTESIAN_POINT('Ctrl Pts',(110.93918052251,-1.78930626646011,329.472541345144));
#74005=CARTESIAN_POINT('Ctrl Pts',(110.660942488236,-5.61645419718042,333.513440768989));
#74006=CARTESIAN_POINT('Ctrl Pts',(110.382704453962,-4.28946500987634,338.918533657553));
#74007=CARTESIAN_POINT('Ctrl Pts',(110.104466419688,0.973902904591502,340.727646046044));
#74008=CARTESIAN_POINT('Ctrl Pts',(109.826228385414,5.34353449829903,337.280582197997));
#74009=CARTESIAN_POINT('Ctrl Pts',(109.54799035114,4.80948335335744,331.740661728187));
#74010=CARTESIAN_POINT('Ctrl Pts',(109.269752316866,-0.138159677102331,
329.191787882665));
#74011=CARTESIAN_POINT('Ctrl Pts',(108.991514282592,-4.95901561111879,331.973024568152));
#74012=CARTESIAN_POINT('Ctrl Pts',(108.713276248318,-5.22905611376197,337.532071929362));
#74013=CARTESIAN_POINT('Ctrl Pts',(108.435038214044,-0.700469001547521,
340.767474254316));
#74014=CARTESIAN_POINT('Ctrl Pts',(108.15680017977,4.47092817448158,338.710150583865));
#74015=CARTESIAN_POINT('Ctrl Pts',(107.878562145496,5.53942055558062,333.248076484335));
#74016=CARTESIAN_POINT('Ctrl Pts',(107.600324111222,1.52446845453669,329.39371673678));
#74017=CARTESIAN_POINT('Ctrl Pts',(107.322086076948,-3.88946584611805,330.684160391279));
#74018=CARTESIAN_POINT('Ctrl Pts',(107.043848042674,-5.73409474821204,335.935186353011));
#74019=CARTESIAN_POINT('Ctrl Pts',(106.7656100084,-2.31662953497166,340.328005601914));
#74020=CARTESIAN_POINT('Ctrl Pts',(106.487371974127,3.22677240911617,339.831392751173));
#74021=CARTESIAN_POINT('Ctrl Pts',(106.209133939853,5.80901294044096,334.901082083922));
#74022=CARTESIAN_POINT('Ctrl Pts',(105.930895905579,3.06040803721359,330.061546928227));
#74023=CARTESIAN_POINT('Ctrl Pts',(105.652657871305,-2.49668815021611,329.753957265053));
#74024=CARTESIAN_POINT('Ctrl Pts',(105.374419837031,-5.76261047324917,334.260583588273));
#74025=CARTESIAN_POINT('Ctrl Pts',(105.096181802757,-3.74027022097263,339.445761438768));
#74026=CARTESIAN_POINT('Ctrl Pts',(104.817943768483,1.71446080679252,340.551129636237));
#74027=CARTESIAN_POINT('Ctrl Pts',(104.539705734209,5.59585645756422,336.56230810107));
#74028=CARTESIAN_POINT('Ctrl Pts',(104.261467699935,4.34201723193514,331.139779481181));
#74029=CARTESIAN_POINT('Ctrl Pts',(103.983229665661,-0.896427119371509,
329.259718254652));
#74030=CARTESIAN_POINT('Ctrl Pts',(103.704991631387,-5.31223353447353,332.647428859408));
#74031=CARTESIAN_POINT('Ctrl Pts',(103.426753597113,-4.85308164342763,338.194059275994));
#74032=CARTESIAN_POINT('Ctrl Pts',(103.148515562839,0.0596716404241646,
340.809548639237));
#74033=CARTESIAN_POINT('Ctrl Pts',(102.870277528565,4.91766514061068,338.093700965052));
#74034=CARTESIAN_POINT('Ctrl Pts',(102.592039494291,5.26278992587726,332.538809578187));
#74035=CARTESIAN_POINT('Ctrl Pts',(102.313801460018,0.778330074818259,329.242516314312));
#74036=CARTESIAN_POINT('Ctrl Pts',(102.035563425744,-4.42039179776838,331.22978084847));
#74037=CARTESIAN_POINT('Ctrl Pts',(101.75732539147,-5.56258536241897,336.676919849645));
#74038=CARTESIAN_POINT('Ctrl Pts',(101.479087357196,-1.60007644360303,340.585174256096));
#74039=CARTESIAN_POINT('Ctrl Pts',(101.200849322922,3.83079901041782,339.367996684764));
#74040=CARTESIAN_POINT('Ctrl Pts',(100.922611288648,5.74620675507894,334.14237302735));
#74041=CARTESIAN_POINT('Ctrl Pts',(100.644373254374,2.3884053744768,329.703780984183));
#74042=CARTESIAN_POINT('Ctrl Pts',(100.3661352201,-3.16120036547716,330.125450959766));
#74043=CARTESIAN_POINT('Ctrl Pts',(100.087897185826,-5.80981918927364,335.020422641347));
#74044=CARTESIAN_POINT('Ctrl Pts',(99.809659151552,-3.12685269586437,339.8966527664));
#74045=CARTESIAN_POINT('Ctrl Pts',(99.531421117278,2.4255803642695,340.279296922205));
#74046=CARTESIAN_POINT('Ctrl Pts',(99.2531830830042,5.75209412562066,335.817208214797));
#74047=CARTESIAN_POINT('Ctrl Pts',(98.9749450487301,3.79999600866009,330.605179590644));
#74048=CARTESIAN_POINT('Ctrl Pts',(98.6967070144562,-1.6393023575986,329.426212788713));
#74049=CARTESIAN_POINT('Ctrl Pts',(98.4184689801823,-5.57423714635231,333.362228241617));
#74050=CARTESIAN_POINT('Ctrl Pts',(98.1402309459082,-4.39377678150391,338.801202663717));
#74051=CARTESIAN_POINT('Ctrl Pts',(97.8619929116345,0.818787683691637,340.751869506984));
#74052=CARTESIAN_POINT('Ctrl Pts',(97.5837548773604,5.27996277684976,337.424130601146));
#74053=CARTESIAN_POINT('Ctrl Pts',(97.3055168430865,4.89579396181571,331.871802822746));
#74054=CARTESIAN_POINT('Ctrl Pts',(97.0272788088127,0.0188272898237993,
329.190175421797));
#74055=CARTESIAN_POINT('Ctrl Pts',(96.7490407745384,-4.87541690814907,331.840138283395));
#74056=CARTESIAN_POINT('Ctrl Pts',(96.4708027402649,-5.29556297054915,337.389859602839));
#74057=CARTESIAN_POINT('Ctrl Pts',(96.1925647059907,-0.856049057257586,
340.746442039027));
#74058=CARTESIAN_POINT('Ctrl Pts',(95.9143266717167,4.36904844061587,338.829599433346));
#74059=CARTESIAN_POINT('Ctrl Pts',(95.636088637443,5.58473467158543,333.398389952479));
#74060=CARTESIAN_POINT('Ctrl Pts',(95.3578506031688,1.67539232498966,329.436954372495));
#74061=CARTESIAN_POINT('Ctrl Pts',(95.0796125688951,-3.77143282949893,330.580643654456));
#74062=CARTESIAN_POINT('Ctrl Pts',(94.8013745346211,-5.75726974261368,335.779911025129));
#74063=CARTESIAN_POINT('Ctrl Pts',(94.5231365003471,-2.45974519009395,340.263465559509));
#74064=CARTESIAN_POINT('Ctrl Pts',(94.2448984660733,3.0950512175955,339.916815438554));
#74065=CARTESIAN_POINT('Ctrl Pts',(93.9666604317991,5.80956480577865,335.058076361713));
#74066=CARTESIAN_POINT('Ctrl Pts',(93.6884223975253,3.19272652073472,330.146041464936));
#74067=CARTESIAN_POINT('Ctrl Pts',(93.4101843632514,-2.35402976782128,329.688412671475));
#74068=CARTESIAN_POINT('Ctrl Pts',(93.1319463289774,-5.7405276838701,334.105149170503));
#74069=CARTESIAN_POINT('Ctrl Pts',(92.8537082947034,-3.85902807448106,339.343077067782));
#74070=CARTESIAN_POINT('Ctrl Pts',(92.5754702604298,1.56384463969824,340.595427243672));
#74071=CARTESIAN_POINT('Ctrl Pts',(92.2972322261555,5.55160021033551,336.712936426414));
#74072=CARTESIAN_POINT('Ctrl Pts',(92.0189941918818,4.44473420943266,331.258509133536));
#74073=CARTESIAN_POINT('Ctrl Pts',(91.7407561576076,-0.740998771297037,
329.237592784498));
#74074=CARTESIAN_POINT('Ctrl Pts',(91.4625181233339,-5.24672811673134,332.504752484135));
#74075=CARTESIAN_POINT('Ctrl Pts',(91.18428008906,-4.93761251102159,338.061763999288));
#74076=CARTESIAN_POINT('Ctrl Pts',(90.9060420547858,-0.0973227829885132,
340.809039883857));
#74077=CARTESIAN_POINT('Ctrl Pts',(90.6278040205122,4.83227862651119,338.225445608299));
#74078=CARTESIAN_POINT('Ctrl Pts',(90.3495659862381,5.3273692647772,332.681907505503));
#74079=CARTESIAN_POINT('Ctrl Pts',(90.0713279519642,0.933611760598616,329.26564866992));
#74080=CARTESIAN_POINT('Ctrl Pts',(89.7930899176902,-4.31690747619431,331.111719411062));
#74081=CARTESIAN_POINT('Ctrl Pts',(89.5148518834163,-5.60586443953363,336.526007857746));
#74082=CARTESIAN_POINT('Ctrl Pts',(89.2366138491423,-1.75040234913642,340.539901417215));
#74083=CARTESIAN_POINT('Ctrl Pts',(88.9583758148684,3.71137814116694,339.469909214918));
#74084=CARTESIAN_POINT('Ctrl Pts',(88.6801377805944,5.767281691173,334.29794730184));
#74085=CARTESIAN_POINT('Ctrl Pts',(88.4018997463205,2.5306359581278,329.770248787585));
#74086=CARTESIAN_POINT('Ctrl Pts',(88.1236617120466,-3.02833704156575,330.041815769961));
#74087=CARTESIAN_POINT('Ctrl Pts',(87.8454236777727,-5.80824983639588,334.863435237565));
#74088=CARTESIAN_POINT('Ctrl Pts',(87.5671856434985,-3.25801748599256,339.810378171963));
#74089=CARTESIAN_POINT('Ctrl Pts',(87.2889476092249,2.28204942304687,340.342908059017));
#74090=CARTESIAN_POINT('Ctrl Pts',(87.0107095749507,5.72791325955045,335.972330081504));
#74091=CARTESIAN_POINT('Ctrl Pts',(86.732471540677,3.91735564162572,330.709459139764));
#74092=CARTESIAN_POINT('Ctrl Pts',(86.4542335064028,-1.48810142854445,329.383954217183));
#74093=CARTESIAN_POINT('Ctrl Pts',(86.1759954721289,-5.52794978208046,333.212211616794));
#74094=CARTESIAN_POINT('Ctrl Pts',(85.8977574378551,-4.49488021300627,338.681096027959));
#74095=CARTESIAN_POINT('Ctrl Pts',(85.6195194035811,0.66307458322058,340.771892947156));
#74096=CARTESIAN_POINT('Ctrl Pts',(85.3412813693072,5.2125356213907,337.565908901747));
#74097=CARTESIAN_POINT('Ctrl Pts',(85.0630433350333,4.97852965671024,332.005228129959));
#74098=CARTESIAN_POINT('Ctrl Pts',(84.7848053007592,0.175800509044065,329.192805300547));
#74099=CARTESIAN_POINT('Ctrl Pts',(84.5065672664855,-4.78825817096059,331.70955933277));
#74100=CARTESIAN_POINT('Ctrl Pts',(84.2283292322114,-5.35820300204945,337.245902198485));
#74101=CARTESIAN_POINT('Ctrl Pts',(83.9500911979375,-1.01100402510444,340.721213766112));
#74102=CARTESIAN_POINT('Ctrl Pts',(83.6718531636636,4.26397842328399,338.946251905556));
#74103=CARTESIAN_POINT('Ctrl Pts',(83.3936151293895,5.62597080884317,333.549872917852));
#74104=CARTESIAN_POINT('Ctrl Pts',(83.1153770951157,1.82509282231999,329.484254149597));
#74105=CARTESIAN_POINT('Ctrl Pts',(82.8371390608417,-3.65064590892035,330.480353935979));
#74106=CARTESIAN_POINT('Ctrl Pts',(82.5589010265678,-5.77624077298977,335.624066205448));
#74107=CARTESIAN_POINT('Ctrl Pts',(82.2806629922939,-2.60106473686054,340.195082129379));
#74108=CARTESIAN_POINT('Ctrl Pts',(82.0024249580199,2.96107001663303,339.998647862465));
#74109=CARTESIAN_POINT('Ctrl Pts',(81.7241869237459,5.80587452118426,335.215028232089));
#74110=CARTESIAN_POINT('Ctrl Pts',(81.4459488894722,3.32271367221217,330.234080366935));
#74111=CARTESIAN_POINT('Ctrl Pts',(81.167710855198,-2.20965247057562,329.626746604187));
#74112=CARTESIAN_POINT('Ctrl Pts',(80.8894728209243,-5.71425315553317,333.950368173687));
#74113=CARTESIAN_POINT('Ctrl Pts',(80.6112347866501,-3.97496806189624,339.237221377653));
#74114=CARTESIAN_POINT('Ctrl Pts',(80.3329967523764,1.41208655171044,340.635639064632));
#74115=CARTESIAN_POINT('Ctrl Pts',(80.0547587181022,5.5032901791758,336.862313963896));
#74116=CARTESIAN_POINT('Ctrl Pts',(79.7765206838285,4.54420563764141,331.3799708262));
#74117=CARTESIAN_POINT('Ctrl Pts',(79.4982826495544,-0.58502934519122,329.219675029759));
#74118=CARTESIAN_POINT('Ctrl Pts',(79.2200446152804,-5.17739153296086,332.36389814105));
#74119=CARTESIAN_POINT('Ctrl Pts',(78.9418065810067,-5.01853792910607,337.927233019501));
#74120=CARTESIAN_POINT('Ctrl Pts',(78.6635685467325,-0.25424614120906,340.804289361844));
#74121=CARTESIAN_POINT('Ctrl Pts',(78.3853305124589,4.74336357780861,338.354835027994));
#74122=CARTESIAN_POINT('Ctrl Pts',(78.1070924781846,5.38805855340297,332.826698106237));
#74123=CARTESIAN_POINT('Ctrl Pts',(77.828854443911,1.0882117221533,329.292968254504));
#74124=CARTESIAN_POINT('Ctrl Pts',(77.5506164096369,-4.21027094453775,330.996497199962));
#74125=CARTESIAN_POINT('Ctrl Pts',(77.272378375363,-5.6450501089238,336.373981573411));
#74126=CARTESIAN_POINT('Ctrl Pts',(76.994140341089,-1.89945010915349,340.490583336875));
#74127=CARTESIAN_POINT('Ctrl Pts',(76.7159023068151,3.5892472199492,339.568557812966));
#74128=CARTESIAN_POINT('Ctrl Pts',(76.4376642725411,5.78414535250674,334.454034215902));
#74129=CARTESIAN_POINT('Ctrl Pts',(76.1594262382672,2.6710186689145,329.840535360462));
#74130=CARTESIAN_POINT('Ctrl Pts',(75.8811882039932,-2.89326242296969,329.961801051152));
#74131=CARTESIAN_POINT('Ctrl Pts',(75.6029501697193,-5.80243929377797,334.706547553507));
#74132=CARTESIAN_POINT('Ctrl Pts',(75.3247121354454,-3.38680326854979,339.720591034656));
#74133=CARTESIAN_POINT('Ctrl Pts',(75.0464741011714,2.13685212709222,340.402617799111));
#74134=CARTESIAN_POINT('Ctrl Pts',(74.7682360668975,5.69954986558741,336.126741951831));
#74135=CARTESIAN_POINT('Ctrl Pts',(74.4899980326236,4.03185481765114,330.816871646039));
#74136=CARTESIAN_POINT('Ctrl Pts',(74.2117599983496,-1.33581388636402,329.345796487804));
#74137=CARTESIAN_POINT('Ctrl Pts',(73.9335219640757,-5.47762590344356,333.063500436805));
#74138=CARTESIAN_POINT('Ctrl Pts',(73.6552839298017,-4.59270147855875,338.558301452263));
#74139=CARTESIAN_POINT('Ctrl Pts',(73.3770458955278,0.506877305036717,340.787701745422));
#74140=CARTESIAN_POINT('Ctrl Pts',(73.0988078612539,5.14130226729675,337.705813573146));
#74141=CARTESIAN_POINT('Ctrl Pts',(72.8205698269799,5.05763002435563,332.140840222535));
#74142=CARTESIAN_POINT('Ctrl Pts',(72.542331792706,0.33264535856014,329.199675598576));
#74143=CARTESIAN_POINT('Ctrl Pts',(72.264093758432,-4.69760304294855,331.581383065154));
#74144=CARTESIAN_POINT('Ctrl Pts',(71.9858557241581,-5.41693046845061,337.100304834139));
#74145=CARTESIAN_POINT('Ctrl Pts',(71.7076176898843,-1.1652207568182,340.691807857282));
#74146=CARTESIAN_POINT('Ctrl Pts',(71.4293796556102,4.15579484471609,339.060022820744));
#74147=CARTESIAN_POINT('Ctrl Pts',(71.1511416213363,5.66309885668578,333.702414767449));
#74148=CARTESIAN_POINT('Ctrl Pts',(70.8729035870623,1.97346063507705,329.535581529739));
#74149=CARTESIAN_POINT('Ctrl Pts',(70.5946655527883,-3.52719328311067,330.383364467503));
#74150=CARTESIAN_POINT('Ctrl Pts',(70.3164275185145,-5.79099398667525,335.467765692012));
#74151=CARTESIAN_POINT('Ctrl Pts',(70.0381894842405,-2.74048498359907,340.122905245171));
#74152=CARTESIAN_POINT('Ctrl Pts',(69.7599514499667,2.8249266394339,340.076830268795));
#74153=CARTESIAN_POINT('Ctrl Pts',(69.4817134156927,5.79794478130726,335.371823088637));
#74154=CARTESIAN_POINT('Ctrl Pts',(69.2034753814187,3.45027457489966,330.325599348138));
#74155=CARTESIAN_POINT('Ctrl Pts',(68.9252373471448,-2.0636616829239,329.569004091811));
#74156=CARTESIAN_POINT('Ctrl Pts',(68.6469993128709,-5.68380607392486,333.796353619061));
#74157=CARTESIAN_POINT('Ctrl Pts',(68.3687612785969,-4.08800552372517,339.128271664307));
#74158=CARTESIAN_POINT('Ctrl Pts',(68.090523244323,1.25929735673448,340.671735736408));
#74159=CARTESIAN_POINT('Ctrl Pts',(67.8122852100489,5.45096164011743,337.01033163789));
#74160=CARTESIAN_POINT('Ctrl Pts',(67.5340471757753,4.64035888242653,331.504075867726));
#74161=CARTESIAN_POINT('Ctrl Pts',(67.255809141501,-0.428632730082352,329.205978073994));
#74162=CARTESIAN_POINT('Ctrl Pts',(66.9775711072273,-5.1042744128034,332.224968682135));
#74163=CARTESIAN_POINT('Ctrl Pts',(66.6993330729532,-5.09579880586159,337.790564571285));
#74164=CARTESIAN_POINT('Ctrl Pts',(66.4210950386793,-0.410983848647697,
340.795300542033));
#74165=CARTESIAN_POINT('Ctrl Pts',(66.1428570044054,4.65098492035853,338.481774743852));
#74166=CARTESIAN_POINT('Ctrl Pts',(65.8646189701315,5.44481347637662,332.97307565415));
#74167=CARTESIAN_POINT('Ctrl Pts',(65.5863809358575,1.24201707043907,329.324455119279));
#74168=CARTESIAN_POINT('Ctrl Pts',(65.3081429015836,-4.10056006889851,330.884198350542));
#74169=CARTESIAN_POINT('Ctrl Pts',(65.0299048673096,-5.68011375717534,336.220952006379));
#74170=CARTESIAN_POINT('Ctrl Pts',(64.7516668330357,-2.04711088883399,340.437256027184));
#74171=CARTESIAN_POINT('Ctrl Pts',(64.4734287987619,3.46449542688313,339.66387044561));
#74172=CARTESIAN_POINT('Ctrl Pts',(64.1951907644879,5.79678542521827,334.610519794715));
#74173=CARTESIAN_POINT('Ctrl Pts',(63.9169527302139,2.80945099924323,329.914589379491));
#74174=CARTESIAN_POINT('Ctrl Pts',(63.6387146959399,-2.75607514130854,329.885465230171));
#74175=CARTESIAN_POINT('Ctrl Pts',(63.360476661666,-5.79239180428386,334.549874148714));
#74176=CARTESIAN_POINT('Ctrl Pts',(63.0822386273922,-3.51311600403078,339.627356917135));
#74177=CARTESIAN_POINT('Ctrl Pts',(62.8040005931181,1.99009449961415,340.458382542378));
#74178=CARTESIAN_POINT('Ctrl Pts',(62.5257625588441,5.66702465470982,336.280331074075));
#74179=CARTESIAN_POINT('Ctrl Pts',(62.2475245245704,4.14340992932511,330.92733867675));
#74180=CARTESIAN_POINT('Ctrl Pts',(61.9692864902963,-1.18255093157096,329.311767463388));
#74181=CARTESIAN_POINT('Ctrl Pts',(61.6910484560225,-5.4233022569874,332.916203290701));
#74182=CARTESIAN_POINT('Ctrl Pts',(61.4128104217484,-4.68716914897679,338.432908601349));
#74183=CARTESIAN_POINT('Ctrl Pts',(61.1345723874745,0.350309904546443,340.799284358187));
#74184=CARTESIAN_POINT('Ctrl Pts',(60.8563343532007,5.06631472923324,337.843742456814));
#74185=CARTESIAN_POINT('Ctrl Pts',(60.5780963189266,5.1330373055855,332.278540076393));
#74186=CARTESIAN_POINT('Ctrl Pts',(60.2998582846528,0.489247310108402,329.210781299184));
#74187=CARTESIAN_POINT('Ctrl Pts',(60.0216202503787,-4.60351772057673,331.455703074986));
#74188=CARTESIAN_POINT('Ctrl Pts',(59.743382216105,-5.47170248689875,336.953173825136));
#74189=CARTESIAN_POINT('Ctrl Pts',(59.4651441818308,-1.31858664319012,340.658245784758));
#74190=CARTESIAN_POINT('Ctrl Pts',(59.186906147557,4.04457670066713,339.170829103278));
#74191=CARTESIAN_POINT('Ctrl Pts',(58.9086681132829,5.69609170417641,333.855904115056));
#74192=CARTESIAN_POINT('Ctrl Pts',(58.6304300790092,2.12038742493874,329.59089903362));
#74193=CARTESIAN_POINT('Ctrl Pts',(58.3521920447351,-3.40116509729812,330.289746070831));
#74194=CARTESIAN_POINT('Ctrl Pts',(58.0739540104613,-5.80151861085904,335.311123615607));
#74195=CARTESIAN_POINT('Ctrl Pts',(57.7957159761872,-2.87790412550895,340.046987610516));
#74196=CARTESIAN_POINT('Ctrl Pts',(57.5174779419134,2.68672049802545,340.151305568671));
#74197=CARTESIAN_POINT('Ctrl Pts',(57.2392399076394,5.78578137645143,335.528346439601));
#74198=CARTESIAN_POINT('Ctrl Pts',(56.9610018733654,3.57531608370108,330.42053158129));
#74199=CARTESIAN_POINT('Ctrl Pts',(56.6827638390915,-1.91616400748287,329.515227297986));
#74200=CARTESIAN_POINT('Ctrl Pts',(56.4045258048175,-5.64920867153418,333.643217968208));
#74201=CARTESIAN_POINT('Ctrl Pts',(56.1262877705437,-4.19805791990187,339.016307482935));
#74202=CARTESIAN_POINT('Ctrl Pts',(55.8480497362697,1.10558862159104,340.703690901174));
#74203=CARTESIAN_POINT('Ctrl Pts',(55.5698117019958,5.39465280351117,337.156881365746));
#74204=CARTESIAN_POINT('Ctrl Pts',(55.2915736677218,4.73312373259396,331.630733636489));
#74205=CARTESIAN_POINT('Ctrl Pts',(55.013335633448,-0.271923126932959,329.196511918736));
#74206=CARTESIAN_POINT('Ctrl Pts',(54.7350975991739,-5.02743014645227,332.088065553816));
#74207=CARTESIAN_POINT('Ctrl Pts',(54.4568595649,-5.16933872531966,337.651858450077));
#74208=CARTESIAN_POINT('Ctrl Pts',(54.1786215306261,-0.567421455275803,
340.782079988069));
#74209=CARTESIAN_POINT('Ctrl Pts',(53.9003834963521,4.55521010914761,338.606172064372));
#74210=CARTESIAN_POINT('Ctrl Pts',(53.6221454620782,5.49759259119749,333.120933264213));
#74211=CARTESIAN_POINT('Ctrl Pts',(53.3439074278042,1.39491549663908,329.360086272507));
#74212=CARTESIAN_POINT('Ctrl Pts',(53.0656693935303,-3.98785496026603,330.774904863531));
#74213=CARTESIAN_POINT('Ctrl Pts',(52.7874313592564,-5.71102978077773,336.067030898991));
#74214=CARTESIAN_POINT('Ctrl Pts',(52.5091933249824,-2.1932768661311,340.379958427797));
#74215=CARTESIAN_POINT('Ctrl Pts',(52.2309552907086,3.33721385585057,339.75577751547));
#74216=CARTESIAN_POINT('Ctrl Pts',(51.9527172564345,5.80519267951394,334.767289772358));
#74217=CARTESIAN_POINT('Ctrl Pts',(51.6744792221607,2.94583186569086,329.992356770355));
#74218=CARTESIAN_POINT('Ctrl Pts',(51.3962411878866,-2.61687537086965,329.812864047505));
#74219=CARTESIAN_POINT('Ctrl Pts',(51.1180031536129,-5.77811470460025,334.393529426259));
#74220=CARTESIAN_POINT('Ctrl Pts',(50.8397651193388,-3.63686345875244,339.530743899044));
#74221=CARTESIAN_POINT('Ctrl Pts',(50.561527085065,1.84188370317583,340.510161569346));
#74222=CARTESIAN_POINT('Ctrl Pts',(50.283289050791,5.63036137685853,336.432985297313));
#74223=CARTESIAN_POINT('Ctrl Pts',(50.005051016517,4.25193951899586,331.040779568762));
#74224=CARTESIAN_POINT('Ctrl Pts',(49.726812982243,-1.02842447692488,329.281891991962));
#74225=CARTESIAN_POINT('Ctrl Pts',(49.4485749479692,-5.36501850989206,332.770427735001));
#74226=CARTESIAN_POINT('Ctrl Pts',(49.1703369136951,-4.77821424387469,338.305009037199));
#74227=CARTESIAN_POINT('Ctrl Pts',(48.8920988794214,0.193486707419849,340.806632327811));
#74228=CARTESIAN_POINT('Ctrl Pts',(48.6138608451472,4.98762776317431,337.979594836945));
#74229=CARTESIAN_POINT('Ctrl Pts',(48.3356228108734,5.20469643792882,332.418227142961));
#74230=CARTESIAN_POINT('Ctrl Pts',(48.0573847765994,0.645492012789552,329.226114292978));
#74231=CARTESIAN_POINT('Ctrl Pts',(47.7791467423257,-4.50607090504021,331.332611133916));
#74232=CARTESIAN_POINT('Ctrl Pts',(47.5009087080515,-5.52247906281209,336.804616606687));
#74233=CARTESIAN_POINT('Ctrl Pts',(47.2226706737776,-1.47098969629869,340.620552055601));
#74234=CARTESIAN_POINT('Ctrl Pts',(46.9444326395036,3.93040520273572,339.2785898423));
#74235=CARTESIAN_POINT('Ctrl Pts',(46.6661946052298,5.72492525990519,334.010228882605));
#74236=CARTESIAN_POINT('Ctrl Pts',(46.3879565709557,2.26576590581826,329.650166268343));
#74237=CARTESIAN_POINT('Ctrl Pts',(46.1097185366819,-3.27265337738824,330.199567106209));
#74238=CARTESIAN_POINT('Ctrl Pts',(45.8314805024079,-5.80780696045024,335.154254356432));
#74239=CARTESIAN_POINT('Ctrl Pts',(45.5532424681341,-3.01322181899706,339.967384660549));
#74240=CARTESIAN_POINT('Ctrl Pts',(45.27500443386,2.54655251066853,340.222019380158));
#74241=CARTESIAN_POINT('Ctrl Pts',(44.9967663995862,5.76939318834706,335.684483991476));
#74242=CARTESIAN_POINT('Ctrl Pts',(44.7185283653121,3.69774689318336,330.518807746783));
#74243=CARTESIAN_POINT('Ctrl Pts',(44.4402903310382,-1.76726714720003,329.46545549058));
#74244=CARTESIAN_POINT('Ctrl Pts',(44.1620522967642,-5.61048621141828,333.491073040927));
#74245=CARTESIAN_POINT('Ctrl Pts',(43.8838142624904,-4.30504489005872,338.901410589891));
#74246=CARTESIAN_POINT('Ctrl Pts',(43.6055762282163,0.951072584549313,340.731481225237));
#74247=CARTESIAN_POINT('Ctrl Pts',(43.3273381939426,5.33440478612478,337.301856136709));
#74248=CARTESIAN_POINT('Ctrl Pts',(43.0491001596685,4.82243245115911,331.759851646862));
#74249=CARTESIAN_POINT('Ctrl Pts',(42.7708621253947,-0.115014965248771,
329.191283476181));
#74250=CARTESIAN_POINT('Ctrl Pts',(42.4926240911207,-4.94691484566584,331.95328872289));
#74251=CARTESIAN_POINT('Ctrl Pts',(42.2143860568467,-5.23910398855925,337.511215939221));
#74252=CARTESIAN_POINT('Ctrl Pts',(41.9361480225728,-0.723444730199963,
340.764637353613));
#74253=CARTESIAN_POINT('Ctrl Pts',(41.6579099882988,4.45610907903712,338.727936154504));
#74254=CARTESIAN_POINT('Ctrl Pts',(41.379671954025,5.54635735850404,333.270162970653));
#74255=CARTESIAN_POINT('Ctrl Pts',(41.1014339197509,1.5467953541722,329.399835696282));
#74256=CARTESIAN_POINT('Ctrl Pts',(40.8231958854771,-3.87223791602144,330.668696545143));
#74257=CARTESIAN_POINT('Ctrl Pts',(40.5449578512032,-5.73777560482017,335.912330644593));
#74258=CARTESIAN_POINT('Ctrl Pts',(40.2667198169292,-2.33784131050453,340.318732377478));
#74259=CARTESIAN_POINT('Ctrl Pts',(39.9884817826552,3.20749544797993,339.844211911913));
#74260=CARTESIAN_POINT('Ctrl Pts',(39.7102437483813,5.80936097640842,334.924229675237));
#74261=CARTESIAN_POINT('Ctrl Pts',(39.4320057141073,3.08006168281437,330.073780747227));
#74262=CARTESIAN_POINT('Ctrl Pts',(39.1537676798335,-2.47576475546252,329.74405051661));
#74263=CARTESIAN_POINT('Ctrl Pts',(38.8755296455594,-5.75961841987933,334.237627549214));
#74264=CARTESIAN_POINT('Ctrl Pts',(38.5972916112856,-3.75795527220141,339.430822527304));
#74265=CARTESIAN_POINT('Ctrl Pts',(38.3190535770116,1.69232796144685,340.557917070921));
#74266=CARTESIAN_POINT('Ctrl Pts',(38.0408155427377,5.58958680359511,336.584593153275));
#74267=CARTESIAN_POINT('Ctrl Pts',(37.7625775084637,4.35736433825011,331.157111487425));
#74268=CARTESIAN_POINT('Ctrl Pts',(37.4843394741898,-0.873547065714799,
329.256191888624));
#74269=CARTESIAN_POINT('Ctrl Pts',(37.2061014399158,-5.3028172210068,332.626280215163));
#74270=CARTESIAN_POINT('Ctrl Pts',(36.9278634056419,-4.86577028203474,338.174696152201));
#74271=CARTESIAN_POINT('Ctrl Pts',(36.649625371368,0.0365222261089616,340.809740288802));
#74272=CARTESIAN_POINT('Ctrl Pts',(36.3713873370941,4.90529882641964,338.113271513996));
#74273=CARTESIAN_POINT('Ctrl Pts',(36.0931493028201,5.27255509581702,332.559799422608));
#74274=CARTESIAN_POINT('Ctrl Pts',(35.8149112685462,0.801265376568756,329.245663383792));
#74275=CARTESIAN_POINT('Ctrl Pts',(35.5366732342722,-4.40533375209907,331.2121971238));
#74276=CARTESIAN_POINT('Ctrl Pts',(35.2584351999983,-5.56922311908519,336.654741655419));
#74277=CARTESIAN_POINT('Ctrl Pts',(34.9801971657244,-1.62231863128531,340.578754193806));
#74278=CARTESIAN_POINT('Ctrl Pts',(34.7019591314504,3.81336371906134,339.383226350815));
#74279=CARTESIAN_POINT('Ctrl Pts',(34.4237210971765,5.74957846958163,334.165276381994));
#74280=CARTESIAN_POINT('Ctrl Pts',(34.1454830629025,2.40948992220596,329.713339956918));
#74281=CARTESIAN_POINT('Ctrl Pts',(33.8672450286286,-3.14175196276516,330.112893422403));
#74282=CARTESIAN_POINT('Ctrl Pts',(33.5890069943546,-5.80985444368967,334.997272460574));
#74283=CARTESIAN_POINT('Ctrl Pts',(33.3107689600807,-3.14633925495117,339.884154521417));
#74284=CARTESIAN_POINT('Ctrl Pts',(33.0325309258068,2.40452502816473,340.28892006796));
#74285=CARTESIAN_POINT('Ctrl Pts',(32.7542928915328,5.74879218366509,335.840121732466));
#74286=CARTESIAN_POINT('Ctrl Pts',(32.4760548572589,3.81747760424955,330.620356083268));
#74287=CARTESIAN_POINT('Ctrl Pts',(32.1978168229849,-1.61707982670873,329.419725013012));
#74288=CARTESIAN_POINT('Ctrl Pts',(31.919578788711,-5.56766696875553,333.340029933596));
#74289=CARTESIAN_POINT('Ctrl Pts',(31.6413407544371,-4.40888831220513,338.783664882997));
#74290=CARTESIAN_POINT('Ctrl Pts',(31.3631027201632,0.795862073371101,340.755086416076));
#74291=CARTESIAN_POINT('Ctrl Pts',(31.0848646858892,5.27026158111962,337.445150090057));
#74292=CARTESIAN_POINT('Ctrl Pts',(30.8066266516153,4.90821982480809,331.89133561675));
#74293=CARTESIAN_POINT('Ctrl Pts',(30.5283886173413,0.0419771804760357,
329.190296564138));
#74294=CARTESIAN_POINT('Ctrl Pts',(30.2501505830674,-4.8627873027967,331.820736603537));
#74295=CARTESIAN_POINT('Ctrl Pts',(29.9719125487934,-5.30504365291584,337.368739736017));
#74296=CARTESIAN_POINT('Ctrl Pts',(29.6936745145195,-0.87893974507008,340.742985375297));
#74297=CARTESIAN_POINT('Ctrl Pts',(29.4154364802456,4.35375419369712,338.84697810199));
#74298=CARTESIAN_POINT('Ctrl Pts',(29.1371984459716,5.59107217021504,333.420655805792));
#74299=CARTESIAN_POINT('Ctrl Pts',(28.8589604116977,1.69754574021657,329.443674365535));
#74300=CARTESIAN_POINT('Ctrl Pts',(28.5807223774237,-3.75379335984459,330.565650948796));
#74301=CARTESIAN_POINT('Ctrl Pts',(28.3024843431498,-5.76033169947554,335.75696420546));
#74302=CARTESIAN_POINT('Ctrl Pts',(28.0242463088759,-2.48069866085444,340.253622583549));
#74303=CARTESIAN_POINT('Ctrl Pts',(27.746008274602,3.07543492378025,339.929109060055));
#74304=CARTESIAN_POINT('Ctrl Pts',(27.467770240328,5.80928727220723,335.081224905682));
#74305=CARTESIAN_POINT('Ctrl Pts',(27.1895322060541,3.21204243586931,330.15880185424));
#74306=CARTESIAN_POINT('Ctrl Pts',(26.9112941717801,-2.33284633419722,329.679074885196));
#74307=CARTESIAN_POINT('Ctrl Pts',(26.6330561375062,-5.73691645612644,334.082282357281));
#74308=CARTESIAN_POINT('Ctrl Pts',(26.3548181032323,-3.87630302301649,339.3276657646));
#74309=CARTESIAN_POINT('Ctrl Pts',(26.0765800689583,1.54153648017683,340.601614175988));
#74310=CARTESIAN_POINT('Ctrl Pts',(25.7983420346844,5.54473070855304,336.73504393776));
#74311=CARTESIAN_POINT('Ctrl Pts',(25.5201040004104,4.45960740578122,331.276249487059));
#74312=CARTESIAN_POINT('Ctrl Pts',(25.2418659661365,-0.718031789578611,
329.234685919615));
#74313=CARTESIAN_POINT('Ctrl Pts',(24.9636279318626,-5.236743809774,332.483865987845));
#74314=CARTESIAN_POINT('Ctrl Pts',(24.6853898975886,-4.9497733299517,338.042065100952));
#74315=CARTESIAN_POINT('Ctrl Pts',(24.4071518633147,-0.120468923767338,
340.808605971724));
#74316=CARTESIAN_POINT('Ctrl Pts',(24.1289138290407,4.81938803563992,338.244674877127));
#74317=CARTESIAN_POINT('Ctrl Pts',(23.8506757947668,5.33656372879123,332.703153539115));
#74318=CARTESIAN_POINT('Ctrl Pts',(23.5724377604928,0.956453655582346,329.269414296857));
#74319=CARTESIAN_POINT('Ctrl Pts',(23.294199726219,-4.30137982012164,331.094548971069));
#74320=CARTESIAN_POINT('Ctrl Pts',(23.0159616919449,-5.61190052316207,336.503658410166));
#74321=CARTESIAN_POINT('Ctrl Pts',(22.7377236576712,-1.77246294761261,340.532882720216));
#74322=CARTESIAN_POINT('Ctrl Pts',(22.4594856233971,3.69353771345072,339.484662223139));
#74323=CARTESIAN_POINT('Ctrl Pts',(22.1812475891232,5.77003333140761,334.320933397392));
#74324=CARTESIAN_POINT('Ctrl Pts',(21.9030095548492,2.55145452668411,329.780373969853));
#74325=CARTESIAN_POINT('Ctrl Pts',(21.6247715205754,-3.00855643777032,330.029788308625));
#74326=CARTESIAN_POINT('Ctrl Pts',(21.3465334863014,-5.80765956550315,334.840292556368));
#74327=CARTESIAN_POINT('Ctrl Pts',(21.0682954520274,-3.27715923088842,339.797357967855));
#74328=CARTESIAN_POINT('Ctrl Pts',(20.7900574177535,2.26074175912166,340.351958781128));
#74329=CARTESIAN_POINT('Ctrl Pts',(20.5118193834796,5.72399340527947,335.995146015743));
#74330=CARTESIAN_POINT('Ctrl Pts',(20.2335813492056,3.93442078941648,330.725102440042));
#74331=CARTESIAN_POINT('Ctrl Pts',(19.9553433149317,-1.46571171293835,329.37806925773));
#74332=CARTESIAN_POINT('Ctrl Pts',(19.6771052806577,-5.52078221019907,333.190198938037));
#74333=CARTESIAN_POINT('Ctrl Pts',(19.3988672463838,-4.50951235977196,338.663156340289));
#74334=CARTESIAN_POINT('Ctrl Pts',(19.1206292121098,0.640070422924563,340.774489237156));
#74335=CARTESIAN_POINT('Ctrl Pts',(18.842391177836,5.20227002592717,337.586658592407));
#74336=CARTESIAN_POINT('Ctrl Pts',(18.5641531435619,4.99042321151613,332.025089536424));
#74337=CARTESIAN_POINT('Ctrl Pts',(18.2859151092881,0.198938674422592,329.193551903259));
#74338=CARTESIAN_POINT('Ctrl Pts',(18.0076770750141,-4.77510894785852,331.690505985439));
#74339=CARTESIAN_POINT('Ctrl Pts',(17.7294390407402,-5.36710956918242,337.224533876731));
#74340=CARTESIAN_POINT('Ctrl Pts',(17.4512010064662,-1.03379295727499,340.717139863413));
#74341=CARTESIAN_POINT('Ctrl Pts',(17.1729629721923,4.24822019276465,338.963210982287));
#74342=CARTESIAN_POINT('Ctrl Pts',(16.8947249379183,5.63170437553145,333.572301879615));
#74343=CARTESIAN_POINT('Ctrl Pts',(16.6164869036444,1.84705657669332,329.49157026923));
#74344=CARTESIAN_POINT('Ctrl Pts',(16.3382488693705,-3.63260778006579,330.465843318484));
#74345=CARTESIAN_POINT('Ctrl Pts',(16.0600108350965,-5.77868159426167,335.601045030322));
#74346=CARTESIAN_POINT('Ctrl Pts',(15.7817728008226,-2.62174460260375,340.184676589243));
#74347=CARTESIAN_POINT('Ctrl Pts',(15.5035347665486,2.94112871397601,340.010406967918));
#74348=CARTESIAN_POINT('Ctrl Pts',(15.2252967322747,5.80497162072999,335.238160825619));
#74349=CARTESIAN_POINT('Ctrl Pts',(14.9470586980008,3.34167775237819,330.247358008898));
#74350=CARTESIAN_POINT('Ctrl Pts',(14.6688206637269,-2.18822446624349,329.617984598531));
#74351=CARTESIAN_POINT('Ctrl Pts',(14.3905826294529,-5.71002539034279,333.927607283674));
#74352=CARTESIAN_POINT('Ctrl Pts',(14.1123445951789,-3.99182029354395,339.221348936101));
#74353=CARTESIAN_POINT('Ctrl Pts',(13.834106560905,1.38961936743681,340.641220976873));
#74354=CARTESIAN_POINT('Ctrl Pts',(13.5558685266311,5.49582584573023,336.884227791461));
#74355=CARTESIAN_POINT('Ctrl Pts',(13.2776304923572,4.55859406353803,331.398106572968));
#74356=CARTESIAN_POINT('Ctrl Pts',(12.9993924580832,-0.561992205806647,
329.217389788631));
#74357=CARTESIAN_POINT('Ctrl Pts',(12.7211544238093,-5.16684652328562,332.343289044026));
#74358=CARTESIAN_POINT('Ctrl Pts',(12.4429163895354,-5.03016204809799,337.90721273083));
#74359=CARTESIAN_POINT('Ctrl Pts',(12.1646783552614,-0.277372107909085,
340.803230204752));
#74360=CARTESIAN_POINT('Ctrl Pts',(11.8864403209875,4.72995812447452,338.373708975665));
#74361=CARTESIAN_POINT('Ctrl Pts',(11.6082022867135,5.39667559486097,332.848184814806));
#74362=CARTESIAN_POINT('Ctrl Pts',(11.3299642524396,1.11094353652828,329.297349689919));
#74363=CARTESIAN_POINT('Ctrl Pts',(11.0517262181657,-4.19428502643889,330.979752581234));
#74364=CARTESIAN_POINT('Ctrl Pts',(10.7734881838918,-5.65048009295057,336.351477194488));
#74365=CARTESIAN_POINT('Ctrl Pts',(10.4952501496178,-1.92131304564754,340.482971125652));
#74366=CARTESIAN_POINT('Ctrl Pts',(10.2170121153439,3.57101475074672,339.582823399336));
#74367=CARTESIAN_POINT('Ctrl Pts',(9.93877408106996,5.78627478124848,334.477086251583));
#74368=CARTESIAN_POINT('Ctrl Pts',(9.66053604679602,2.69155629820058,329.851219389636));
#74369=CARTESIAN_POINT('Ctrl Pts',(9.38229801252208,-2.87316451817608,329.95031239017));
#74370=CARTESIAN_POINT('Ctrl Pts',(9.10405997824813,-5.80122306706437,334.683429380474));
#74371=CARTESIAN_POINT('Ctrl Pts',(8.82582194397421,-3.40558784867484,339.707058171501));
#74372=CARTESIAN_POINT('Ctrl Pts',(8.54758390970025,2.11531076584172,340.41108988013));
#74373=CARTESIAN_POINT('Ctrl Pts',(8.26934587542634,5.69500916144305,336.149442903385));
#74374=CARTESIAN_POINT('Ctrl Pts',(7.9911078411524,4.04850200793196,330.832971726666));
#74375=CARTESIAN_POINT('Ctrl Pts',(7.71286980687842,-1.31329401327319,329.340516006911));
#74376=CARTESIAN_POINT('Ctrl Pts',(7.43463177260454,-5.46982712631381,333.041694436197));
#74377=CARTESIAN_POINT('Ctrl Pts',(7.15639373833055,-4.60691728147025,338.539963563042));
#74378=CARTESIAN_POINT('Ctrl Pts',(6.87815570405667,0.483950600032991,340.789693258488));
#74379=CARTESIAN_POINT('Ctrl Pts',(6.59991766978268,5.13021690941976,337.726244822412));
#74380=CARTESIAN_POINT('Ctrl Pts',(6.32167963550878,5.06947896879733,332.161078968005));
#74381=CARTESIAN_POINT('Ctrl Pts',(6.0434416012348,0.354817207204381,329.200927806512));
#74382=CARTESIAN_POINT('Ctrl Pts',(5.7652035669609,-4.68216976966421,331.56291659117));
#74383=CARTESIAN_POINT('Ctrl Pts',(5.48696553268694,-5.42863455194625,337.078284863033));
#74384=CARTESIAN_POINT('Ctrl Pts',(5.208727498413,-1.18128049517348,340.687866433408));
#74385=CARTESIAN_POINT('Ctrl Pts',(4.9768624698514,3.24078857374305,339.344254515386));
#74386=CARTESIAN_POINT('Ctrl Pts',(4.79137044700209,4.91809615913057,336.398020145725));
#74387=CARTESIAN_POINT('Ctrl Pts',(4.69862443557744,4.97290566312669,334.719862138));
#74388=CARTESIAN_POINT('Ctrl Pts',(4.65225142986512,4.79338446579369,333.921776804495));
#74389=CARTESIAN_POINT('Ctrl Pts',(5.23167681249901,-1.34668115311846,339.737346666877));
#74390=CARTESIAN_POINT('Ctrl Pts',(5.23167681249889,-1.23675483698737,339.781456312384));
#74391=CARTESIAN_POINT('Ctrl Pts',(5.23167681249914,-1.12542425527317,339.821231768089));
#74392=CARTESIAN_POINT('Ctrl Pts',(5.2316768124991,-1.01288792298132,339.85652298731));
#74393=CARTESIAN_POINT('Ctrl Pts',(5.23167681249901,-0.877572330351241,
339.898957747234));
#74394=CARTESIAN_POINT('Ctrl Pts',(5.23167681249896,-0.740514058238084,
339.934911453407));
#74395=CARTESIAN_POINT('Ctrl Pts',(5.23167681249902,-0.602118655133099,
339.96460111858));
#74396=CARTESIAN_POINT('Ctrl Pts',(5.23167681249908,-0.463723252028115,
339.994290783752));
#74397=CARTESIAN_POINT('Ctrl Pts',(5.23167681249919,-0.323990096019264,
340.017716363323));
#74398=CARTESIAN_POINT('Ctrl Pts',(5.23167681249908,-0.183299247619329,
340.035048214569));
#74399=CARTESIAN_POINT('Ctrl Pts',(5.23167681249896,-0.0386841920429301,
340.05286349296));
#74400=CARTESIAN_POINT('Ctrl Pts',(5.23167681249883,0.106943343603134,340.06424054752));
#74401=CARTESIAN_POINT('Ctrl Pts',(5.23167681249904,0.253188220578269,340.069313737644));
#74402=CARTESIAN_POINT('Ctrl Pts',(5.23167681249916,0.334525544479147,340.072135304572));
#74403=CARTESIAN_POINT('Ctrl Pts',(5.23167681249893,0.416054086959694,340.073006003226));
#74404=CARTESIAN_POINT('Ctrl Pts',(5.23167681249885,0.49770699289044,340.071942155002));
#74405=CARTESIAN_POINT('Ctrl Pts',(5.23167681249882,0.526903163358536,340.071561760774));
#74406=CARTESIAN_POINT('Ctrl Pts',(5.23167681249909,0.556122147452936,340.070933686722));
#74407=CARTESIAN_POINT('Ctrl Pts',(5.23167681249904,0.585323801418764,340.070059915179));
#74408=CARTESIAN_POINT('Ctrl Pts',(5.23167681249883,0.734801547718469,340.06558724383));
#74409=CARTESIAN_POINT('Ctrl Pts',(5.23167681249919,0.883962607076913,340.0546820683));
#74410=CARTESIAN_POINT('Ctrl Pts',(5.23167681249915,1.0323778451602,340.037563106176));
#74411=CARTESIAN_POINT('Ctrl Pts',(5.23167681249911,1.18269721686223,340.020224511677));
#74412=CARTESIAN_POINT('Ctrl Pts',(5.23167681249882,1.33225222875417,339.996511689538));
#74413=CARTESIAN_POINT('Ctrl Pts',(5.23167681249888,1.48061471242626,339.966599919862));
#74414=CARTESIAN_POINT('Ctrl Pts',(5.23167681249894,1.63042017296366,339.936397227639));
#74415=CARTESIAN_POINT('Ctrl Pts',(5.2316768124989,1.77901059605625,339.899874418231));
#74416=CARTESIAN_POINT('Ctrl Pts',(5.23167681249895,1.9259515555415,339.857159153423));
#74417=CARTESIAN_POINT('Ctrl Pts',(5.231676812499,2.07258551961732,339.814533131194));
#74418=CARTESIAN_POINT('Ctrl Pts',(5.23167681249901,2.21757773979494,339.765740402025));
#74419=CARTESIAN_POINT('Ctrl Pts',(5.23167681249909,2.36049050053187,339.710856434616));
#74420=CARTESIAN_POINT('Ctrl Pts',(5.23167681249913,2.40223249230077,339.694825912891));
#74421=CARTESIAN_POINT('Ctrl Pts',(5.23167681249891,2.44379699939896,339.678275412879));
#74422=CARTESIAN_POINT('Ctrl Pts',(5.23167681249902,2.48517285780773,339.661206003771));
#74423=CARTESIAN_POINT('Ctrl Pts',(5.23167681249904,2.50433078795608,339.653302492885));
#74424=CARTESIAN_POINT('Ctrl Pts',(5.23167681249916,2.52344916383466,339.645287290512));
#74425=CARTESIAN_POINT('Ctrl Pts',(5.23167681249915,2.54251135007745,339.637167259143));
#74426=CARTESIAN_POINT('Ctrl Pts',(5.2316768124989,2.68705304330757,339.575595985614));
#74427=CARTESIAN_POINT('Ctrl Pts',(5.23167681249902,2.82857221596661,339.50791689713));
#74428=CARTESIAN_POINT('Ctrl Pts',(5.23167681249907,2.96662330249087,339.434312734319));
#74429=CARTESIAN_POINT('Ctrl Pts',(5.23167681249911,3.10460481213973,339.360745667541));
#74430=CARTESIAN_POINT('Ctrl Pts',(5.23167681249916,3.23912257405703,339.281259374025));
#74431=CARTESIAN_POINT('Ctrl Pts',(5.23167681249917,3.36972909595313,339.195984735696));
#74432=CARTESIAN_POINT('Ctrl Pts',(5.23167681249917,3.49947681772413,339.111270818753));
#74433=CARTESIAN_POINT('Ctrl Pts',(5.23167681249904,3.62536538725959,339.02084426393));
#74434=CARTESIAN_POINT('Ctrl Pts',(5.23167681249888,3.74694111839647,338.924784699129));
#74435=CARTESIAN_POINT('Ctrl Pts',(5.23167681249882,3.79095071680503,338.890011781618));
#74436=CARTESIAN_POINT('Ctrl Pts',(5.23167681249915,3.83439496160363,338.854500266954));
#74437=CARTESIAN_POINT('Ctrl Pts',(5.23167681249907,3.87725152194784,338.818252407266));
#74438=CARTESIAN_POINT('Ctrl Pts',(5.23167681249883,3.98972601993342,338.723122051758));
#74439=CARTESIAN_POINT('Ctrl Pts',(5.23167681249901,4.09815478095222,338.622922413815));
#74440=CARTESIAN_POINT('Ctrl Pts',(5.2316768124991,4.20239332039485,338.518019138625));
#74441=CARTESIAN_POINT('Ctrl Pts',(5.23167681249906,4.22019037122658,338.500108594876));
#74442=CARTESIAN_POINT('Ctrl Pts',(5.23167681249891,4.23786747898358,338.482058400429));
#74443=CARTESIAN_POINT('Ctrl Pts',(5.23167681249894,4.2554061724232,338.463888906878));
#74444=CARTESIAN_POINT('Ctrl Pts',(5.23167681249913,4.36250722519882,338.352935836487));
#74445=CARTESIAN_POINT('Ctrl Pts',(5.23167681249885,4.46458172457174,338.237406884179));
#74446=CARTESIAN_POINT('Ctrl Pts',(5.23167681249892,4.56153344475904,338.117806877089));
#74447=CARTESIAN_POINT('Ctrl Pts',(5.23167681249899,4.66017670753057,337.996120176697));
#74448=CARTESIAN_POINT('Ctrl Pts',(5.23167681249898,4.75351731967113,337.870218648565));
#74449=CARTESIAN_POINT('Ctrl Pts',(5.23167681249897,4.8414280052284,337.740585136994));
#74450=CARTESIAN_POINT('Ctrl Pts',(5.23167681249896,4.93094693812344,337.608580096313));
#74451=CARTESIAN_POINT('Ctrl Pts',(5.23167681249902,5.01483597188807,337.472704727081));
#74452=CARTESIAN_POINT('Ctrl Pts',(5.23167681249905,5.09292670865521,337.333426458399));
#74453=CARTESIAN_POINT('Ctrl Pts',(5.23167681249908,5.16249416850671,337.209349829519));
#74454=CARTESIAN_POINT('Ctrl Pts',(5.23167681249896,5.22745971835016,337.082571668943));
#74455=CARTESIAN_POINT('Ctrl Pts',(5.231676812499,5.28767719560329,336.953400592671));
#74456=CARTESIAN_POINT('Ctrl Pts',(5.231676812499,5.31803717586098,336.888276122096));
#74457=CARTESIAN_POINT('Ctrl Pts',(5.23167681249893,5.34718981662582,336.822543112078));
#74458=CARTESIAN_POINT('Ctrl Pts',(5.23167681249895,5.37511360302354,336.756239639658));
#74459=CARTESIAN_POINT('Ctrl Pts',(5.23167681249897,5.38387786312344,336.735429393169));
#74460=CARTESIAN_POINT('Ctrl Pts',(5.23167681249899,5.3925210537521,336.714562944136));
#74461=CARTESIAN_POINT('Ctrl Pts',(5.23167681249894,5.40104246900692,336.693641454162));
#74462=CARTESIAN_POINT('Ctrl Pts',(5.23167681249891,5.40897664218581,336.674161741032));
#74463=CARTESIAN_POINT('Ctrl Pts',(5.231676812499,5.41680164871212,336.654643136502));
#74464=CARTESIAN_POINT('Ctrl Pts',(5.23167681249898,5.42451698628412,336.635087237854));
#74465=CARTESIAN_POINT('Ctrl Pts',(5.23167681249897,5.43491648844008,336.608727845506));
#74466=CARTESIAN_POINT('Ctrl Pts',(5.23167681249902,5.44511686297811,336.582300399227));
#74467=CARTESIAN_POINT('Ctrl Pts',(5.23167681249901,5.45511734450837,336.555807568461));
#74468=CARTESIAN_POINT('Ctrl Pts',(5.23167681249897,5.51276118082839,336.403100081758));
#74469=CARTESIAN_POINT('Ctrl Pts',(5.231676812499,5.56376708959899,336.248222805456));
#74470=CARTESIAN_POINT('Ctrl Pts',(5.23167681249898,5.60813990494374,336.091593888462));
#74471=CARTESIAN_POINT('Ctrl Pts',(5.23167681249896,5.65251272028848,335.934964971469));
#74472=CARTESIAN_POINT('Ctrl Pts',(5.23167681249898,5.69025265554719,335.776583766993));
#74473=CARTESIAN_POINT('Ctrl Pts',(5.231676812499,5.72131952430206,335.616841802708));
#74474=CARTESIAN_POINT('Ctrl Pts',(5.23167681249901,5.73662548264904,335.538140473941));
#74475=CARTESIAN_POINT('Ctrl Pts',(5.23167681249891,5.75031096821763,335.459108498761));
#74476=CARTESIAN_POINT('Ctrl Pts',(5.23167681249892,5.76236691005121,335.379791061143));
#74477=CARTESIAN_POINT('Ctrl Pts',(5.23167681249892,5.76818605760889,335.341506215399));
#74478=CARTESIAN_POINT('Ctrl Pts',(5.23167681249898,5.77362551299829,335.303154849943));
#74479=CARTESIAN_POINT('Ctrl Pts',(5.23167681249898,5.77868401197528,335.264741983279));
#74480=CARTESIAN_POINT('Ctrl Pts',(5.231676812499,5.78204651990671,335.239208011756));
#74481=CARTESIAN_POINT('Ctrl Pts',(5.23167681249895,5.78524069104185,335.213646366837));
#74482=CARTESIAN_POINT('Ctrl Pts',(5.23167681249898,5.78826445021777,335.188074200246));
#74483=CARTESIAN_POINT('Ctrl Pts',(5.231676812499,5.80778662166987,335.022973677496));
#74484=CARTESIAN_POINT('Ctrl Pts',(5.231676812499,5.82023072297851,334.857279926282));
#74485=CARTESIAN_POINT('Ctrl Pts',(5.231676812499,5.82557797797662,334.691409186639));
#74486=CARTESIAN_POINT('Ctrl Pts',(5.23167681249897,5.83090854965785,334.526055960018));
#74487=CARTESIAN_POINT('Ctrl Pts',(5.23167681249901,5.82918667389409,334.360526158613));
#74488=CARTESIAN_POINT('Ctrl Pts',(5.23167681249899,5.82034517345234,334.195215344822));
#74489=CARTESIAN_POINT('Ctrl Pts',(5.23167681249896,5.81152526086727,334.030308162313));
#74490=CARTESIAN_POINT('Ctrl Pts',(5.23167681249899,5.79562064591606,333.865618214986));
#74491=CARTESIAN_POINT('Ctrl Pts',(5.23167681249902,5.77251337094751,333.701531692827));
#74492=CARTESIAN_POINT('Origin',(5.23167681249902,0.,335.));
#74493=CARTESIAN_POINT('',(0.,0.,0.));
#74494=CARTESIAN_POINT('',(0.,0.,0.));
#74495=CARTESIAN_POINT('',(0.,0.,0.));
#74496=CARTESIAN_POINT('',(0.,0.,0.));
#74497=CARTESIAN_POINT('',(0.,0.,0.));
#74498=CARTESIAN_POINT('',(0.,0.,0.));
#74499=CARTESIAN_POINT('',(0.,0.,0.));
#74500=CARTESIAN_POINT('',(0.,0.,0.));
#74501=CARTESIAN_POINT('',(0.,0.,0.));
#74502=UNCERTAINTY_MEASURE_WITH_UNIT(LENGTH_MEASURE(0.01),#74524,
'DISTANCE_ACCURACY_VALUE',
'Maximum model space distance between geometric entities at asserted c
onnectivities');
#74503=UNCERTAINTY_MEASURE_WITH_UNIT(LENGTH_MEASURE(0.01),#74524,
'DISTANCE_ACCURACY_VALUE',
'Maximum model space distance between geometric entities at asserted c
onnectivities');
#74504=UNCERTAINTY_MEASURE_WITH_UNIT(LENGTH_MEASURE(0.01),#74524,
'DISTANCE_ACCURACY_VALUE',
'Maximum model space distance between geometric entities at asserted c
onnectivities');
#74505=UNCERTAINTY_MEASURE_WITH_UNIT(LENGTH_MEASURE(0.01),#74524,
'DISTANCE_ACCURACY_VALUE',
'Maximum model space distance between geometric entities at asserted c
onnectivities');
#74506=UNCERTAINTY_MEASURE_WITH_UNIT(LENGTH_MEASURE(0.01),#74524,
'DISTANCE_ACCURACY_VALUE',
'Maximum model space distance between geometric entities at asserted c
onnectivities');
#74507=UNCERTAINTY_MEASURE_WITH_UNIT(LENGTH_MEASURE(0.01),#74524,
'DISTANCE_ACCURACY_VALUE',
'Maximum model space distance between geometric entities at asserted c
onnectivities');
#74508=UNCERTAINTY_MEASURE_WITH_UNIT(LENGTH_MEASURE(0.01),#74524,
'DISTANCE_ACCURACY_VALUE',
'Maximum model space distance between geometric entities at asserted c
onnectivities');
#74509=UNCERTAINTY_MEASURE_WITH_UNIT(LENGTH_MEASURE(0.01),#74524,
'DISTANCE_ACCURACY_VALUE',
'Maximum model space distance between geometric entities at asserted c
onnectivities');
#74510=UNCERTAINTY_MEASURE_WITH_UNIT(LENGTH_MEASURE(0.01),#74524,
'DISTANCE_ACCURACY_VALUE',
'Maximum model space distance between geometric entities at asserted c
onnectivities');
#74511=UNCERTAINTY_MEASURE_WITH_UNIT(LENGTH_MEASURE(0.01),#74524,
'DISTANCE_ACCURACY_VALUE',
'Maximum model space distance between geometric entities at asserted c
onnectivities');
#74512=UNCERTAINTY_MEASURE_WITH_UNIT(LENGTH_MEASURE(0.01),#74524,
'DISTANCE_ACCURACY_VALUE',
'Maximum model space distance between geometric entities at asserted c
onnectivities');
#74513=(
GEOMETRIC_REPRESENTATION_CONTEXT(3)
GLOBAL_UNCERTAINTY_ASSIGNED_CONTEXT((#74502))
GLOBAL_UNIT_ASSIGNED_CONTEXT((#74524,#74526,#74527))
REPRESENTATION_CONTEXT('','3D')
);
#74514=(
GEOMETRIC_REPRESENTATION_CONTEXT(3)
GLOBAL_UNCERTAINTY_ASSIGNED_CONTEXT((#74503))
GLOBAL_UNIT_ASSIGNED_CONTEXT((#74524,#74526,#74527))
REPRESENTATION_CONTEXT('','3D')
);
#74515=(
GEOMETRIC_REPRESENTATION_CONTEXT(3)
GLOBAL_UNCERTAINTY_ASSIGNED_CONTEXT((#74504))
GLOBAL_UNIT_ASSIGNED_CONTEXT((#74524,#74526,#74527))
REPRESENTATION_CONTEXT('','3D')
);
#74516=(
GEOMETRIC_REPRESENTATION_CONTEXT(3)
GLOBAL_UNCERTAINTY_ASSIGNED_CONTEXT((#74505))
GLOBAL_UNIT_ASSIGNED_CONTEXT((#74524,#74526,#74527))
REPRESENTATION_CONTEXT('','3D')
);
#74517=(
GEOMETRIC_REPRESENTATION_CONTEXT(3)
GLOBAL_UNCERTAINTY_ASSIGNED_CONTEXT((#74506))
GLOBAL_UNIT_ASSIGNED_CONTEXT((#74524,#74526,#74527))
REPRESENTATION_CONTEXT('','3D')
);
#74518=(
GEOMETRIC_REPRESENTATION_CONTEXT(3)
GLOBAL_UNCERTAINTY_ASSIGNED_CONTEXT((#74507))
GLOBAL_UNIT_ASSIGNED_CONTEXT((#74524,#74526,#74527))
REPRESENTATION_CONTEXT('','3D')
);
#74519=(
GEOMETRIC_REPRESENTATION_CONTEXT(3)
GLOBAL_UNCERTAINTY_ASSIGNED_CONTEXT((#74508))
GLOBAL_UNIT_ASSIGNED_CONTEXT((#74524,#74526,#74527))
REPRESENTATION_CONTEXT('','3D')
);
#74520=(
GEOMETRIC_REPRESENTATION_CONTEXT(3)
GLOBAL_UNCERTAINTY_ASSIGNED_CONTEXT((#74509))
GLOBAL_UNIT_ASSIGNED_CONTEXT((#74524,#74526,#74527))
REPRESENTATION_CONTEXT('','3D')
);
#74521=(
GEOMETRIC_REPRESENTATION_CONTEXT(3)
GLOBAL_UNCERTAINTY_ASSIGNED_CONTEXT((#74510))
GLOBAL_UNIT_ASSIGNED_CONTEXT((#74524,#74526,#74527))
REPRESENTATION_CONTEXT('','3D')
);
#74522=(
GEOMETRIC_REPRESENTATION_CONTEXT(3)
GLOBAL_UNCERTAINTY_ASSIGNED_CONTEXT((#74511))
GLOBAL_UNIT_ASSIGNED_CONTEXT((#74524,#74526,#74527))
REPRESENTATION_CONTEXT('','3D')
);
#74523=(
GEOMETRIC_REPRESENTATION_CONTEXT(3)
GLOBAL_UNCERTAINTY_ASSIGNED_CONTEXT((#74512))
GLOBAL_UNIT_ASSIGNED_CONTEXT((#74524,#74526,#74527))
REPRESENTATION_CONTEXT('','3D')
);
#74524=(
LENGTH_UNIT()
NAMED_UNIT(*)
SI_UNIT(.MILLI.,.METRE.)
);
#74525=(
LENGTH_UNIT()
NAMED_UNIT(*)
SI_UNIT($,.METRE.)
);
#74526=(
NAMED_UNIT(*)
PLANE_ANGLE_UNIT()
SI_UNIT($,.RADIAN.)
);
#74527=(
NAMED_UNIT(*)
SI_UNIT($,.STERADIAN.)
SOLID_ANGLE_UNIT()
);
#74528=SHAPE_DEFINITION_REPRESENTATION(#74538,#74557);
#74529=SHAPE_DEFINITION_REPRESENTATION(#74539,#74558);
#74530=SHAPE_DEFINITION_REPRESENTATION(#74540,#74559);
#74531=SHAPE_DEFINITION_REPRESENTATION(#74541,#74560);
#74532=SHAPE_DEFINITION_REPRESENTATION(#74542,#74561);
#74533=SHAPE_DEFINITION_REPRESENTATION(#74543,#74562);
#74534=SHAPE_DEFINITION_REPRESENTATION(#74544,#74563);
#74535=SHAPE_DEFINITION_REPRESENTATION(#74545,#74564);
#74536=SHAPE_DEFINITION_REPRESENTATION(#74546,#74565);
#74537=SHAPE_DEFINITION_REPRESENTATION(#74547,#74566);
#74538=PRODUCT_DEFINITION_SHAPE('',$,#74568);
#74539=PRODUCT_DEFINITION_SHAPE('',$,#74569);
#74540=PRODUCT_DEFINITION_SHAPE('',$,#74570);
#74541=PRODUCT_DEFINITION_SHAPE('',$,#74571);
#74542=PRODUCT_DEFINITION_SHAPE('',$,#74572);
#74543=PRODUCT_DEFINITION_SHAPE('',$,#74573);
#74544=PRODUCT_DEFINITION_SHAPE('',$,#74574);
#74545=PRODUCT_DEFINITION_SHAPE('',$,#74575);
#74546=PRODUCT_DEFINITION_SHAPE('',$,#74576);
#74547=PRODUCT_DEFINITION_SHAPE('',$,#74577);
#74548=PRODUCT_DEFINITION_SHAPE($,$,#38);
#74549=PRODUCT_DEFINITION_SHAPE($,$,#39);
#74550=PRODUCT_DEFINITION_SHAPE($,$,#40);
#74551=PRODUCT_DEFINITION_SHAPE($,$,#41);
#74552=PRODUCT_DEFINITION_SHAPE($,$,#42);
#74553=PRODUCT_DEFINITION_SHAPE($,$,#43);
#74554=PRODUCT_DEFINITION_SHAPE($,$,#44);
#74555=PRODUCT_DEFINITION_SHAPE($,$,#45);
#74556=PRODUCT_DEFINITION_SHAPE($,$,#46);
#74557=SHAPE_REPRESENTATION('',(#4831,#5089,#5090,#5091,#5092,#5093,#5094,
#5095,#5096,#5097),#74513);
#74558=SHAPE_REPRESENTATION('',(#4832),#74514);
#74559=SHAPE_REPRESENTATION('',(#4883),#74515);
#74560=SHAPE_REPRESENTATION('',(#4929),#74516);
#74561=SHAPE_REPRESENTATION('',(#4935),#74517);
#74562=SHAPE_REPRESENTATION('',(#4960),#74518);
#74563=SHAPE_REPRESENTATION('',(#4986),#74519);
#74564=SHAPE_REPRESENTATION('',(#5037),#74520);
#74565=SHAPE_REPRESENTATION('',(#5063),#74521);
#74566=SHAPE_REPRESENTATION('',(#5069),#74522);
#74567=PRODUCT_DEFINITION_CONTEXT('part definition',#74599,'design');
#74568=PRODUCT_DEFINITION('BR-202','BR-202',#74578,#74567);
#74569=PRODUCT_DEFINITION('Bottom_Base','Bottom_Base',#74579,#74567);
#74570=PRODUCT_DEFINITION('Clamp_03','Clamp_03',#74580,#74567);
#74571=PRODUCT_DEFINITION('Rod_02','Rod_02',#74581,#74567);
#74572=PRODUCT_DEFINITION('Clamp_01','Clamp_01',#74582,#74567);
#74573=PRODUCT_DEFINITION('Clamp_02','Clamp_02',#74583,#74567);
#74574=PRODUCT_DEFINITION('Top_Base','Top_Base',#74584,#74567);
#74575=PRODUCT_DEFINITION('Nut','Nut',#74585,#74567);
#74576=PRODUCT_DEFINITION('Rod','Rod',#74586,#74567);
#74577=PRODUCT_DEFINITION('Screw','Screw',#74587,#74567);
#74578=PRODUCT_DEFINITION_FORMATION('',$,#74601);
#74579=PRODUCT_DEFINITION_FORMATION('',$,#74602);
#74580=PRODUCT_DEFINITION_FORMATION('',$,#74603);
#74581=PRODUCT_DEFINITION_FORMATION('',$,#74604);
#74582=PRODUCT_DEFINITION_FORMATION('',$,#74605);
#74583=PRODUCT_DEFINITION_FORMATION('',$,#74606);
#74584=PRODUCT_DEFINITION_FORMATION('',$,#74607);
#74585=PRODUCT_DEFINITION_FORMATION('',$,#74608);
#74586=PRODUCT_DEFINITION_FORMATION('',$,#74609);
#74587=PRODUCT_DEFINITION_FORMATION('',$,#74610);
#74588=PRODUCT_RELATED_PRODUCT_CATEGORY('BR-202','BR-202',(#74601));
#74589=PRODUCT_RELATED_PRODUCT_CATEGORY('Bottom_Base','Bottom_Base',(#74602));
#74590=PRODUCT_RELATED_PRODUCT_CATEGORY('Clamp_03','Clamp_03',(#74603));
#74591=PRODUCT_RELATED_PRODUCT_CATEGORY('Rod_02','Rod_02',(#74604));
#74592=PRODUCT_RELATED_PRODUCT_CATEGORY('Clamp_01','Clamp_01',(#74605));
#74593=PRODUCT_RELATED_PRODUCT_CATEGORY('Clamp_02','Clamp_02',(#74606));
#74594=PRODUCT_RELATED_PRODUCT_CATEGORY('Top_Base','Top_Base',(#74607));
#74595=PRODUCT_RELATED_PRODUCT_CATEGORY('Nut','Nut',(#74608));
#74596=PRODUCT_RELATED_PRODUCT_CATEGORY('Rod','Rod',(#74609));
#74597=PRODUCT_RELATED_PRODUCT_CATEGORY('Screw','Screw',(#74610));
#74598=APPLICATION_PROTOCOL_DEFINITION('international standard',
'automotive_design',2009,#74599);
#74599=APPLICATION_CONTEXT(
'Core Data for Automotive Mechanical Design Process');
#74600=PRODUCT_CONTEXT('part definition',#74599,'mechanical');
#74601=PRODUCT('BR-202','BR-202',$,(#74600));
#74602=PRODUCT('Bottom_Base','Bottom_Base',$,(#74600));
#74603=PRODUCT('Clamp_03','Clamp_03',$,(#74600));
#74604=PRODUCT('Rod_02','Rod_02',$,(#74600));
#74605=PRODUCT('Clamp_01','Clamp_01',$,(#74600));
#74606=PRODUCT('Clamp_02','Clamp_02',$,(#74600));
#74607=PRODUCT('Top_Base','Top_Base',$,(#74600));
#74608=PRODUCT('Nut','Nut',$,(#74600));
#74609=PRODUCT('Rod','Rod',$,(#74600));
#74610=PRODUCT('Screw','Screw',$,(#74600));
#74611=PRESENTATION_STYLE_ASSIGNMENT((#74614));
#74612=PRESENTATION_STYLE_ASSIGNMENT((#74615));
#74613=PRESENTATION_STYLE_ASSIGNMENT((#74616));
#74614=SURFACE_STYLE_USAGE(.BOTH.,#74617);
#74615=SURFACE_STYLE_USAGE(.BOTH.,#74618);
#74616=SURFACE_STYLE_USAGE(.BOTH.,#74619);
#74617=SURFACE_SIDE_STYLE('',(#74620));
#74618=SURFACE_SIDE_STYLE('',(#74621));
#74619=SURFACE_SIDE_STYLE('',(#74622));
#74620=SURFACE_STYLE_FILL_AREA(#74623);
#74621=SURFACE_STYLE_FILL_AREA(#74624);
#74622=SURFACE_STYLE_FILL_AREA(#74625);
#74623=FILL_AREA_STYLE('Steel - Satin',(#74626));
#74624=FILL_AREA_STYLE('Opaque(215,0,0)',(#74627));
#74625=FILL_AREA_STYLE('Opaque(255,255,255)',(#74628));
#74626=FILL_AREA_STYLE_COLOUR('Steel - Satin',#74629);
#74627=FILL_AREA_STYLE_COLOUR('Opaque(215,0,0)',#74630);
#74628=FILL_AREA_STYLE_COLOUR('Opaque(255,255,255)',#74631);
#74629=COLOUR_RGB('Steel - Satin', 0.09019608, 0.27058824, 0.51372549);
#74630=COLOUR_RGB('Opaque(215,0,0)', 0.09019608, 0.27058824, 0.51372549);
#74631=COLOUR_RGB('Opaque(255,255,255)', 0.31764706, 0.68627451, 0.89019608);
ENDSEC;
END-ISO-10303-21;
